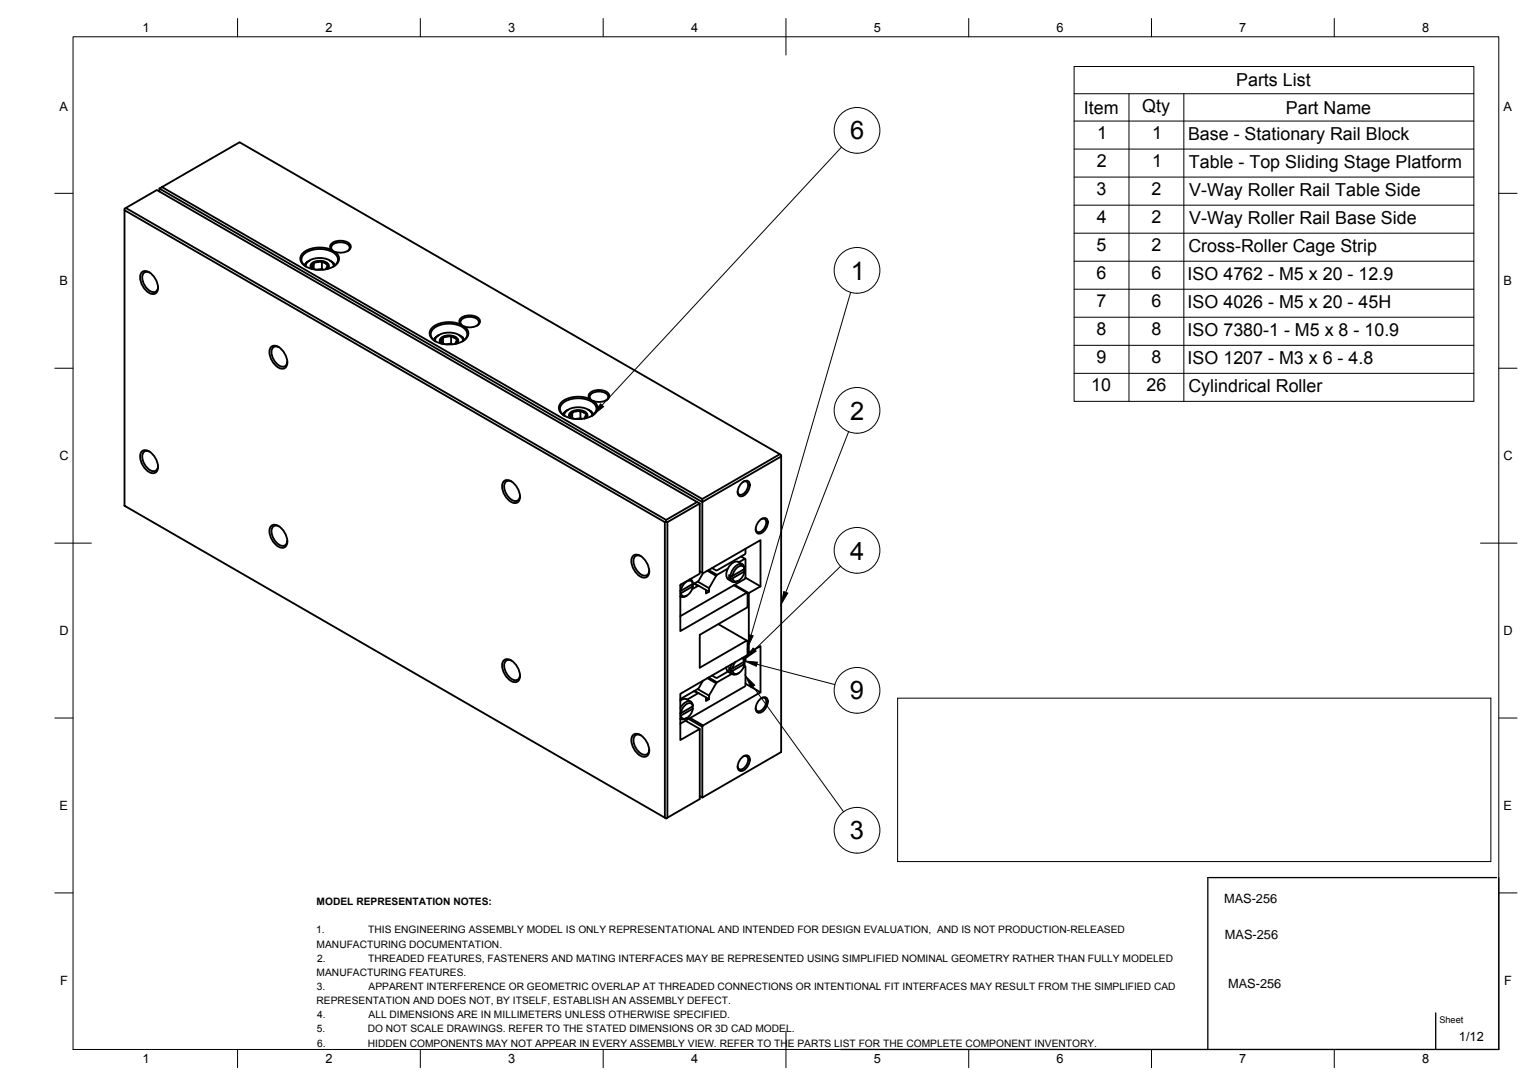
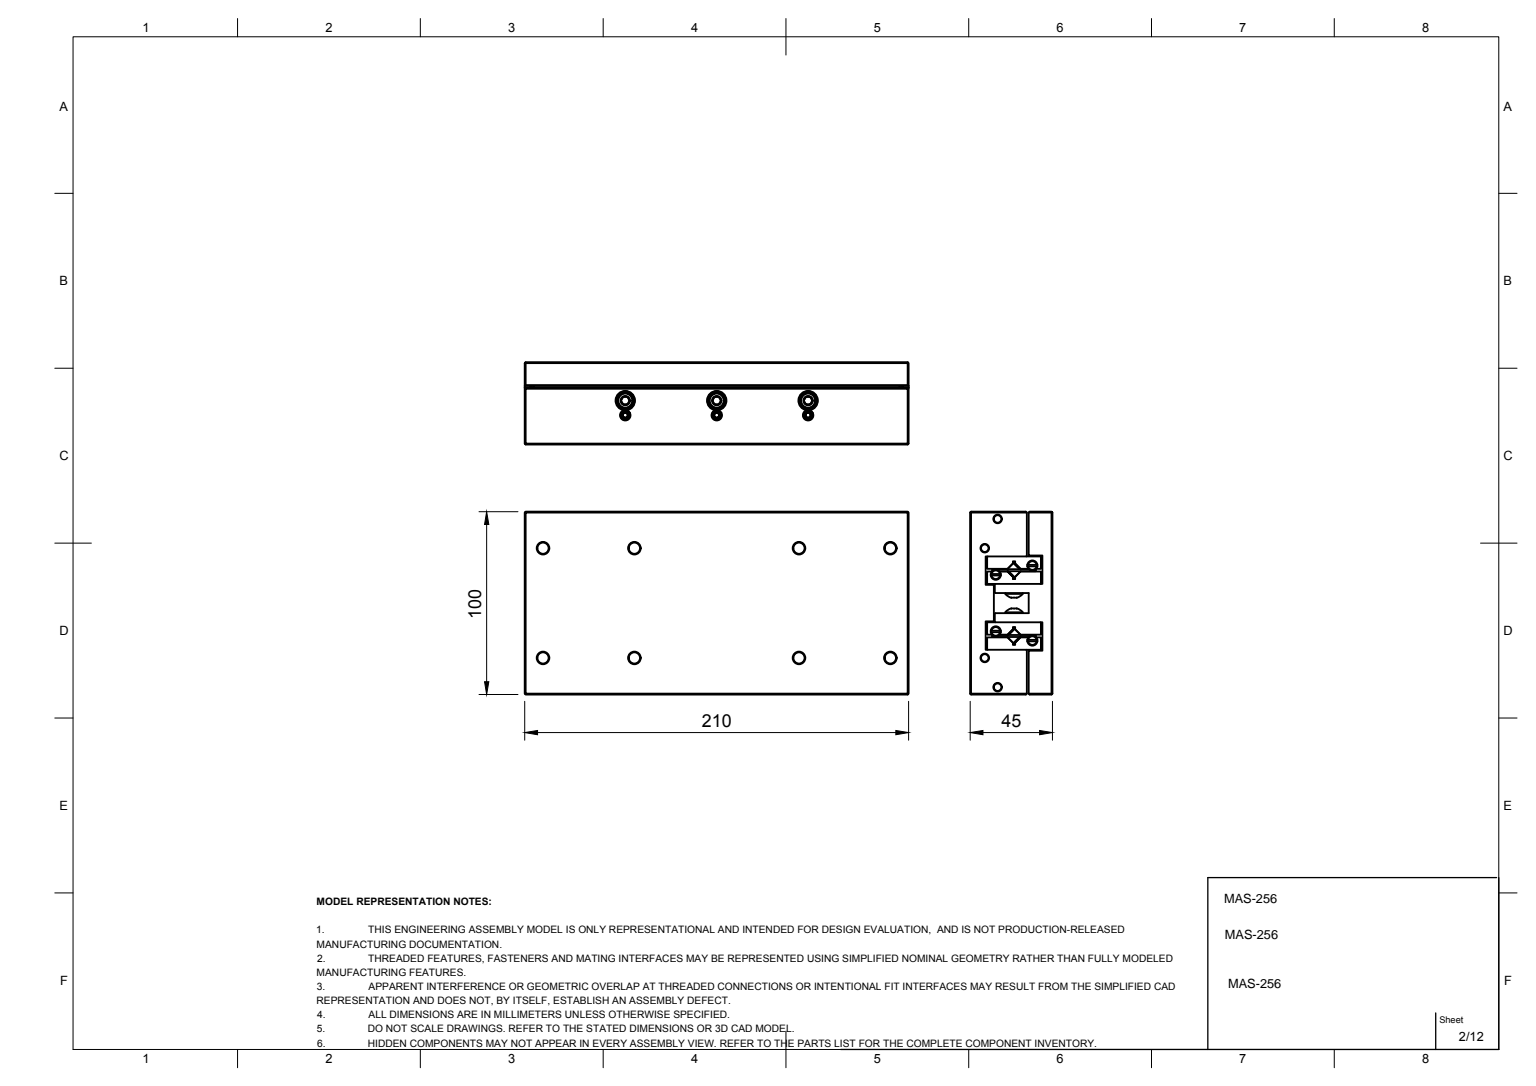
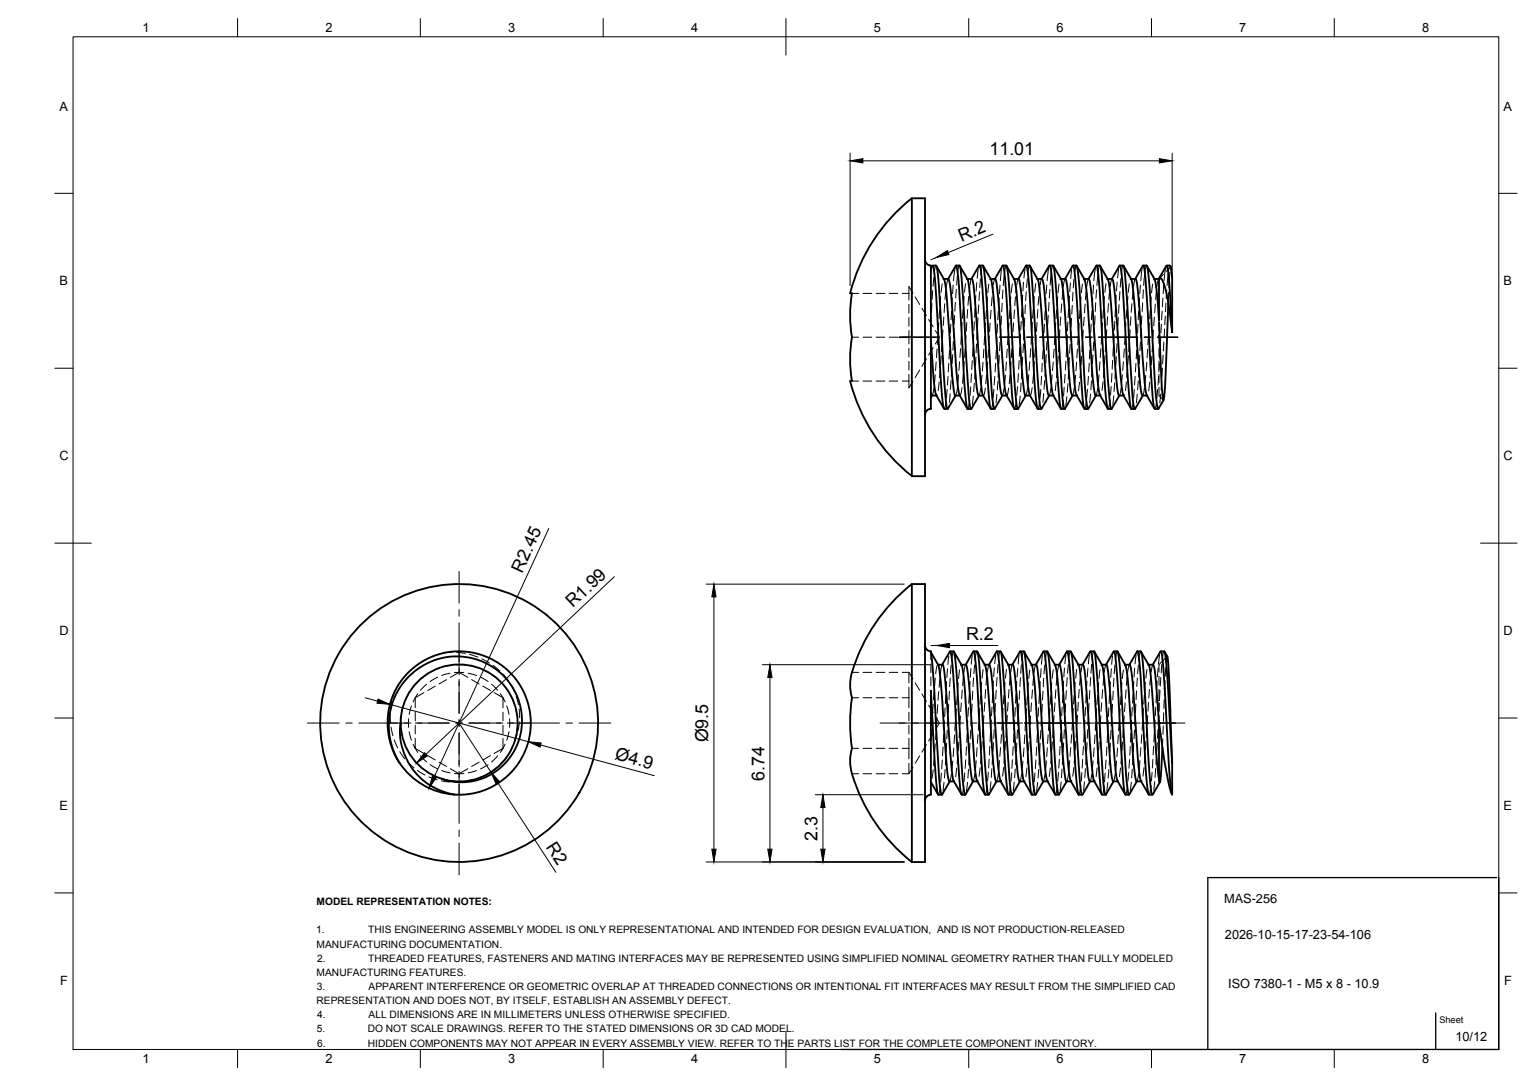
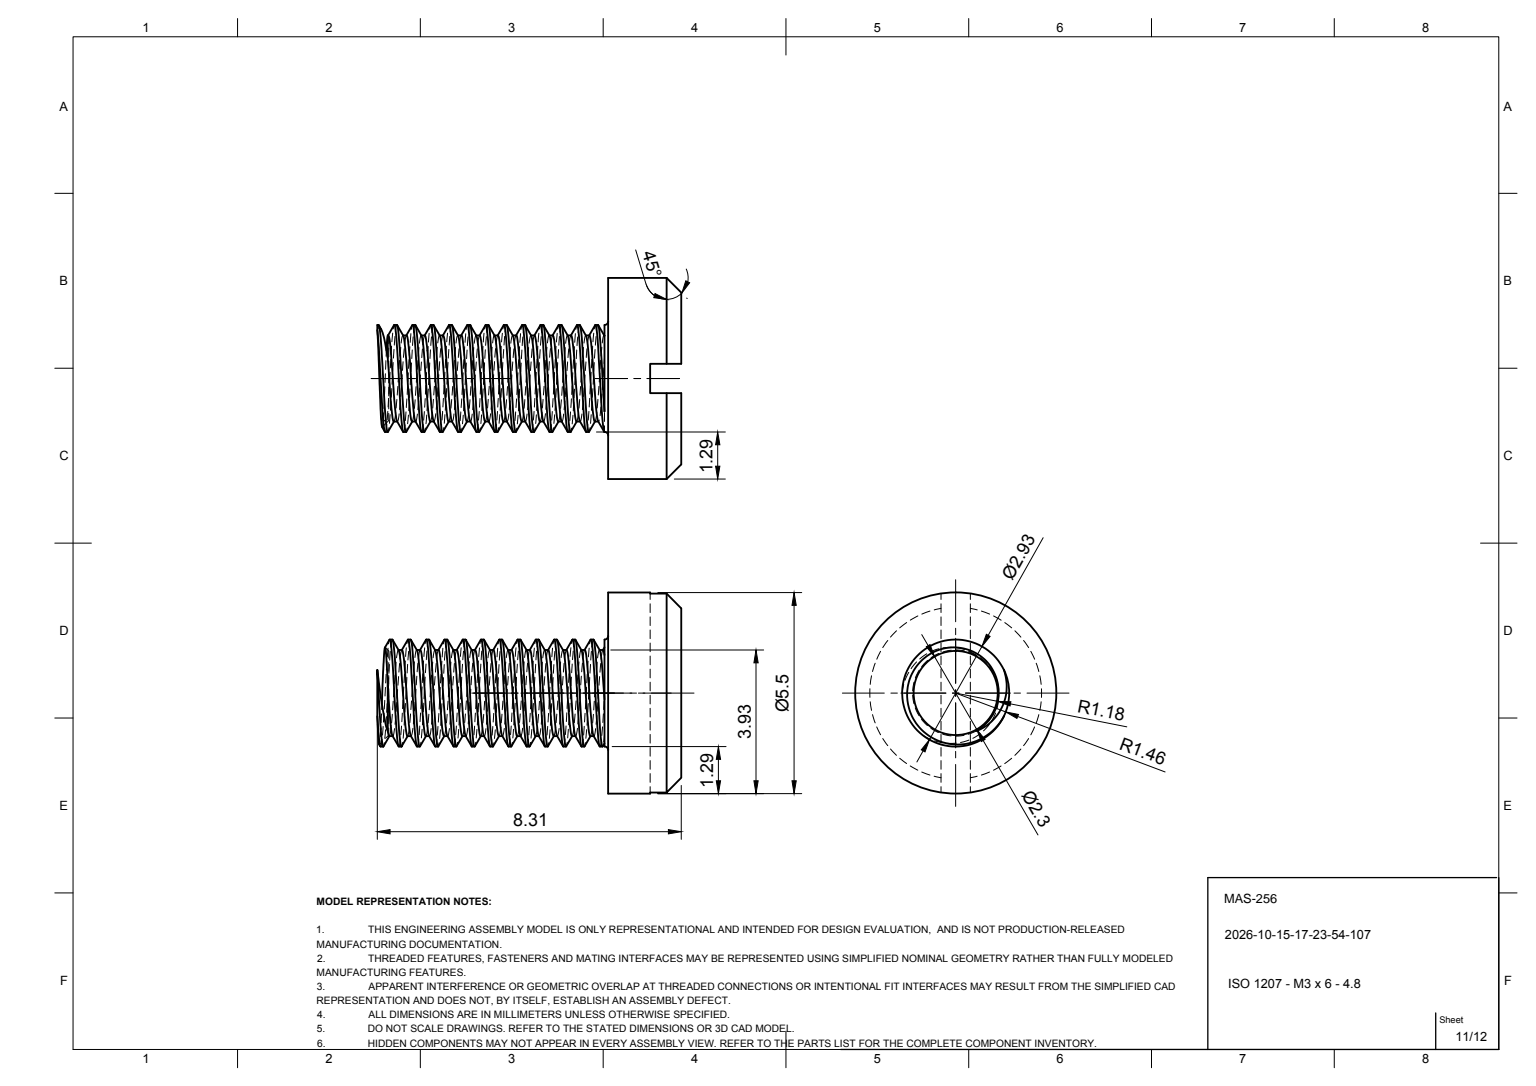
ISO-10303-21;
HEADER;
/* Generated by software containing ST-Developer
 * from STEP Tools, Inc. (www.steptools.com) 
 */

FILE_DESCRIPTION(
/* description */ (''),
/* implementation_level */ '2;1');

FILE_NAME(
/* name */ 'MAS-256',
/* time_stamp */ '2026-10-14T18:40:07-07:00',
/* author */ (''),
/* organization */ (''),
/* preprocessor_version */ 'ST-DEVELOPER v20.2',
/* originating_system */ 'Autodesk Translation Framework v15.15.0.0',
/* authorisation */ '');

FILE_SCHEMA (('AUTOMOTIVE_DESIGN { 1 0 10303 214 3 1 1 }'));
ENDSEC;

DATA;
#10=MECHANICAL_DESIGN_GEOMETRIC_PRESENTATION_REPRESENTATION('',(#831,#832,
#833,#834,#835,#836,#837,#838,#839,#840),#81040);
#11=ITEM_DEFINED_TRANSFORMATION($,$,#15206,#16558);
#12=ITEM_DEFINED_TRANSFORMATION($,$,#15327,#16559);
#13=ITEM_DEFINED_TRANSFORMATION($,$,#15614,#16560);
#14=ITEM_DEFINED_TRANSFORMATION($,$,#15705,#16561);
#15=ITEM_DEFINED_TRANSFORMATION($,$,#15816,#16562);
#16=ITEM_DEFINED_TRANSFORMATION($,$,#16085,#16563);
#17=ITEM_DEFINED_TRANSFORMATION($,$,#16363,#16564);
#18=ITEM_DEFINED_TRANSFORMATION($,$,#16450,#16565);
#19=ITEM_DEFINED_TRANSFORMATION($,$,#16512,#16566);
#20=ITEM_DEFINED_TRANSFORMATION($,$,#16075,#16567);
#21=ITEM_DEFINED_TRANSFORMATION($,$,#15614,#16568);
#22=ITEM_DEFINED_TRANSFORMATION($,$,#15705,#16569);
#23=ITEM_DEFINED_TRANSFORMATION($,$,#15816,#16570);
#24=ITEM_DEFINED_TRANSFORMATION($,$,#16075,#16571);
#25=ITEM_DEFINED_TRANSFORMATION($,$,#16075,#16572);
#26=ITEM_DEFINED_TRANSFORMATION($,$,#16075,#16573);
#27=ITEM_DEFINED_TRANSFORMATION($,$,#16075,#16574);
#28=ITEM_DEFINED_TRANSFORMATION($,$,#16075,#16575);
#29=ITEM_DEFINED_TRANSFORMATION($,$,#16075,#16576);
#30=ITEM_DEFINED_TRANSFORMATION($,$,#16075,#16577);
#31=ITEM_DEFINED_TRANSFORMATION($,$,#16075,#16578);
#32=ITEM_DEFINED_TRANSFORMATION($,$,#16075,#16579);
#33=ITEM_DEFINED_TRANSFORMATION($,$,#16075,#16580);
#34=ITEM_DEFINED_TRANSFORMATION($,$,#16075,#16581);
#35=ITEM_DEFINED_TRANSFORMATION($,$,#16075,#16582);
#36=ITEM_DEFINED_TRANSFORMATION($,$,#16075,#16583);
#37=ITEM_DEFINED_TRANSFORMATION($,$,#16075,#16584);
#38=ITEM_DEFINED_TRANSFORMATION($,$,#16075,#16585);
#39=ITEM_DEFINED_TRANSFORMATION($,$,#16075,#16586);
#40=ITEM_DEFINED_TRANSFORMATION($,$,#16075,#16587);
#41=ITEM_DEFINED_TRANSFORMATION($,$,#16075,#16588);
#42=ITEM_DEFINED_TRANSFORMATION($,$,#16075,#16589);
#43=ITEM_DEFINED_TRANSFORMATION($,$,#16075,#16590);
#44=ITEM_DEFINED_TRANSFORMATION($,$,#16075,#16591);
#45=ITEM_DEFINED_TRANSFORMATION($,$,#16075,#16592);
#46=ITEM_DEFINED_TRANSFORMATION($,$,#16075,#16593);
#47=ITEM_DEFINED_TRANSFORMATION($,$,#16075,#16594);
#48=ITEM_DEFINED_TRANSFORMATION($,$,#16075,#16595);
#49=ITEM_DEFINED_TRANSFORMATION($,$,#16085,#16596);
#50=ITEM_DEFINED_TRANSFORMATION($,$,#16085,#16597);
#51=ITEM_DEFINED_TRANSFORMATION($,$,#16085,#16598);
#52=ITEM_DEFINED_TRANSFORMATION($,$,#16085,#16599);
#53=ITEM_DEFINED_TRANSFORMATION($,$,#16085,#16600);
#54=ITEM_DEFINED_TRANSFORMATION($,$,#16363,#16601);
#55=ITEM_DEFINED_TRANSFORMATION($,$,#16363,#16602);
#56=ITEM_DEFINED_TRANSFORMATION($,$,#16363,#16603);
#57=ITEM_DEFINED_TRANSFORMATION($,$,#16363,#16604);
#58=ITEM_DEFINED_TRANSFORMATION($,$,#16363,#16605);
#59=ITEM_DEFINED_TRANSFORMATION($,$,#16450,#16606);
#60=ITEM_DEFINED_TRANSFORMATION($,$,#16450,#16607);
#61=ITEM_DEFINED_TRANSFORMATION($,$,#16450,#16608);
#62=ITEM_DEFINED_TRANSFORMATION($,$,#16450,#16609);
#63=ITEM_DEFINED_TRANSFORMATION($,$,#16450,#16610);
#64=ITEM_DEFINED_TRANSFORMATION($,$,#16450,#16611);
#65=ITEM_DEFINED_TRANSFORMATION($,$,#16450,#16612);
#66=ITEM_DEFINED_TRANSFORMATION($,$,#16512,#16613);
#67=ITEM_DEFINED_TRANSFORMATION($,$,#16512,#16614);
#68=ITEM_DEFINED_TRANSFORMATION($,$,#16512,#16615);
#69=ITEM_DEFINED_TRANSFORMATION($,$,#16512,#16616);
#70=ITEM_DEFINED_TRANSFORMATION($,$,#16512,#16617);
#71=ITEM_DEFINED_TRANSFORMATION($,$,#16512,#16618);
#72=ITEM_DEFINED_TRANSFORMATION($,$,#16512,#16619);
#73=(
REPRESENTATION_RELATIONSHIP($,$,#81130,#81129)
REPRESENTATION_RELATIONSHIP_WITH_TRANSFORMATION(#11)
SHAPE_REPRESENTATION_RELATIONSHIP()
);
#74=(
REPRESENTATION_RELATIONSHIP($,$,#81131,#81129)
REPRESENTATION_RELATIONSHIP_WITH_TRANSFORMATION(#12)
SHAPE_REPRESENTATION_RELATIONSHIP()
);
#75=(
REPRESENTATION_RELATIONSHIP($,$,#81132,#81129)
REPRESENTATION_RELATIONSHIP_WITH_TRANSFORMATION(#13)
SHAPE_REPRESENTATION_RELATIONSHIP()
);
#76=(
REPRESENTATION_RELATIONSHIP($,$,#81133,#81129)
REPRESENTATION_RELATIONSHIP_WITH_TRANSFORMATION(#14)
SHAPE_REPRESENTATION_RELATIONSHIP()
);
#77=(
REPRESENTATION_RELATIONSHIP($,$,#81134,#81129)
REPRESENTATION_RELATIONSHIP_WITH_TRANSFORMATION(#15)
SHAPE_REPRESENTATION_RELATIONSHIP()
);
#78=(
REPRESENTATION_RELATIONSHIP($,$,#81136,#81129)
REPRESENTATION_RELATIONSHIP_WITH_TRANSFORMATION(#16)
SHAPE_REPRESENTATION_RELATIONSHIP()
);
#79=(
REPRESENTATION_RELATIONSHIP($,$,#81137,#81129)
REPRESENTATION_RELATIONSHIP_WITH_TRANSFORMATION(#17)
SHAPE_REPRESENTATION_RELATIONSHIP()
);
#80=(
REPRESENTATION_RELATIONSHIP($,$,#81138,#81129)
REPRESENTATION_RELATIONSHIP_WITH_TRANSFORMATION(#18)
SHAPE_REPRESENTATION_RELATIONSHIP()
);
#81=(
REPRESENTATION_RELATIONSHIP($,$,#81139,#81129)
REPRESENTATION_RELATIONSHIP_WITH_TRANSFORMATION(#19)
SHAPE_REPRESENTATION_RELATIONSHIP()
);
#82=(
REPRESENTATION_RELATIONSHIP($,$,#81135,#81129)
REPRESENTATION_RELATIONSHIP_WITH_TRANSFORMATION(#20)
SHAPE_REPRESENTATION_RELATIONSHIP()
);
#83=(
REPRESENTATION_RELATIONSHIP($,$,#81132,#81129)
REPRESENTATION_RELATIONSHIP_WITH_TRANSFORMATION(#21)
SHAPE_REPRESENTATION_RELATIONSHIP()
);
#84=(
REPRESENTATION_RELATIONSHIP($,$,#81133,#81129)
REPRESENTATION_RELATIONSHIP_WITH_TRANSFORMATION(#22)
SHAPE_REPRESENTATION_RELATIONSHIP()
);
#85=(
REPRESENTATION_RELATIONSHIP($,$,#81134,#81129)
REPRESENTATION_RELATIONSHIP_WITH_TRANSFORMATION(#23)
SHAPE_REPRESENTATION_RELATIONSHIP()
);
#86=(
REPRESENTATION_RELATIONSHIP($,$,#81135,#81129)
REPRESENTATION_RELATIONSHIP_WITH_TRANSFORMATION(#24)
SHAPE_REPRESENTATION_RELATIONSHIP()
);
#87=(
REPRESENTATION_RELATIONSHIP($,$,#81135,#81129)
REPRESENTATION_RELATIONSHIP_WITH_TRANSFORMATION(#25)
SHAPE_REPRESENTATION_RELATIONSHIP()
);
#88=(
REPRESENTATION_RELATIONSHIP($,$,#81135,#81129)
REPRESENTATION_RELATIONSHIP_WITH_TRANSFORMATION(#26)
SHAPE_REPRESENTATION_RELATIONSHIP()
);
#89=(
REPRESENTATION_RELATIONSHIP($,$,#81135,#81129)
REPRESENTATION_RELATIONSHIP_WITH_TRANSFORMATION(#27)
SHAPE_REPRESENTATION_RELATIONSHIP()
);
#90=(
REPRESENTATION_RELATIONSHIP($,$,#81135,#81129)
REPRESENTATION_RELATIONSHIP_WITH_TRANSFORMATION(#28)
SHAPE_REPRESENTATION_RELATIONSHIP()
);
#91=(
REPRESENTATION_RELATIONSHIP($,$,#81135,#81129)
REPRESENTATION_RELATIONSHIP_WITH_TRANSFORMATION(#29)
SHAPE_REPRESENTATION_RELATIONSHIP()
);
#92=(
REPRESENTATION_RELATIONSHIP($,$,#81135,#81129)
REPRESENTATION_RELATIONSHIP_WITH_TRANSFORMATION(#30)
SHAPE_REPRESENTATION_RELATIONSHIP()
);
#93=(
REPRESENTATION_RELATIONSHIP($,$,#81135,#81129)
REPRESENTATION_RELATIONSHIP_WITH_TRANSFORMATION(#31)
SHAPE_REPRESENTATION_RELATIONSHIP()
);
#94=(
REPRESENTATION_RELATIONSHIP($,$,#81135,#81129)
REPRESENTATION_RELATIONSHIP_WITH_TRANSFORMATION(#32)
SHAPE_REPRESENTATION_RELATIONSHIP()
);
#95=(
REPRESENTATION_RELATIONSHIP($,$,#81135,#81129)
REPRESENTATION_RELATIONSHIP_WITH_TRANSFORMATION(#33)
SHAPE_REPRESENTATION_RELATIONSHIP()
);
#96=(
REPRESENTATION_RELATIONSHIP($,$,#81135,#81129)
REPRESENTATION_RELATIONSHIP_WITH_TRANSFORMATION(#34)
SHAPE_REPRESENTATION_RELATIONSHIP()
);
#97=(
REPRESENTATION_RELATIONSHIP($,$,#81135,#81129)
REPRESENTATION_RELATIONSHIP_WITH_TRANSFORMATION(#35)
SHAPE_REPRESENTATION_RELATIONSHIP()
);
#98=(
REPRESENTATION_RELATIONSHIP($,$,#81135,#81129)
REPRESENTATION_RELATIONSHIP_WITH_TRANSFORMATION(#36)
SHAPE_REPRESENTATION_RELATIONSHIP()
);
#99=(
REPRESENTATION_RELATIONSHIP($,$,#81135,#81129)
REPRESENTATION_RELATIONSHIP_WITH_TRANSFORMATION(#37)
SHAPE_REPRESENTATION_RELATIONSHIP()
);
#100=(
REPRESENTATION_RELATIONSHIP($,$,#81135,#81129)
REPRESENTATION_RELATIONSHIP_WITH_TRANSFORMATION(#38)
SHAPE_REPRESENTATION_RELATIONSHIP()
);
#101=(
REPRESENTATION_RELATIONSHIP($,$,#81135,#81129)
REPRESENTATION_RELATIONSHIP_WITH_TRANSFORMATION(#39)
SHAPE_REPRESENTATION_RELATIONSHIP()
);
#102=(
REPRESENTATION_RELATIONSHIP($,$,#81135,#81129)
REPRESENTATION_RELATIONSHIP_WITH_TRANSFORMATION(#40)
SHAPE_REPRESENTATION_RELATIONSHIP()
);
#103=(
REPRESENTATION_RELATIONSHIP($,$,#81135,#81129)
REPRESENTATION_RELATIONSHIP_WITH_TRANSFORMATION(#41)
SHAPE_REPRESENTATION_RELATIONSHIP()
);
#104=(
REPRESENTATION_RELATIONSHIP($,$,#81135,#81129)
REPRESENTATION_RELATIONSHIP_WITH_TRANSFORMATION(#42)
SHAPE_REPRESENTATION_RELATIONSHIP()
);
#105=(
REPRESENTATION_RELATIONSHIP($,$,#81135,#81129)
REPRESENTATION_RELATIONSHIP_WITH_TRANSFORMATION(#43)
SHAPE_REPRESENTATION_RELATIONSHIP()
);
#106=(
REPRESENTATION_RELATIONSHIP($,$,#81135,#81129)
REPRESENTATION_RELATIONSHIP_WITH_TRANSFORMATION(#44)
SHAPE_REPRESENTATION_RELATIONSHIP()
);
#107=(
REPRESENTATION_RELATIONSHIP($,$,#81135,#81129)
REPRESENTATION_RELATIONSHIP_WITH_TRANSFORMATION(#45)
SHAPE_REPRESENTATION_RELATIONSHIP()
);
#108=(
REPRESENTATION_RELATIONSHIP($,$,#81135,#81129)
REPRESENTATION_RELATIONSHIP_WITH_TRANSFORMATION(#46)
SHAPE_REPRESENTATION_RELATIONSHIP()
);
#109=(
REPRESENTATION_RELATIONSHIP($,$,#81135,#81129)
REPRESENTATION_RELATIONSHIP_WITH_TRANSFORMATION(#47)
SHAPE_REPRESENTATION_RELATIONSHIP()
);
#110=(
REPRESENTATION_RELATIONSHIP($,$,#81135,#81129)
REPRESENTATION_RELATIONSHIP_WITH_TRANSFORMATION(#48)
SHAPE_REPRESENTATION_RELATIONSHIP()
);
#111=(
REPRESENTATION_RELATIONSHIP($,$,#81136,#81129)
REPRESENTATION_RELATIONSHIP_WITH_TRANSFORMATION(#49)
SHAPE_REPRESENTATION_RELATIONSHIP()
);
#112=(
REPRESENTATION_RELATIONSHIP($,$,#81136,#81129)
REPRESENTATION_RELATIONSHIP_WITH_TRANSFORMATION(#50)
SHAPE_REPRESENTATION_RELATIONSHIP()
);
#113=(
REPRESENTATION_RELATIONSHIP($,$,#81136,#81129)
REPRESENTATION_RELATIONSHIP_WITH_TRANSFORMATION(#51)
SHAPE_REPRESENTATION_RELATIONSHIP()
);
#114=(
REPRESENTATION_RELATIONSHIP($,$,#81136,#81129)
REPRESENTATION_RELATIONSHIP_WITH_TRANSFORMATION(#52)
SHAPE_REPRESENTATION_RELATIONSHIP()
);
#115=(
REPRESENTATION_RELATIONSHIP($,$,#81136,#81129)
REPRESENTATION_RELATIONSHIP_WITH_TRANSFORMATION(#53)
SHAPE_REPRESENTATION_RELATIONSHIP()
);
#116=(
REPRESENTATION_RELATIONSHIP($,$,#81137,#81129)
REPRESENTATION_RELATIONSHIP_WITH_TRANSFORMATION(#54)
SHAPE_REPRESENTATION_RELATIONSHIP()
);
#117=(
REPRESENTATION_RELATIONSHIP($,$,#81137,#81129)
REPRESENTATION_RELATIONSHIP_WITH_TRANSFORMATION(#55)
SHAPE_REPRESENTATION_RELATIONSHIP()
);
#118=(
REPRESENTATION_RELATIONSHIP($,$,#81137,#81129)
REPRESENTATION_RELATIONSHIP_WITH_TRANSFORMATION(#56)
SHAPE_REPRESENTATION_RELATIONSHIP()
);
#119=(
REPRESENTATION_RELATIONSHIP($,$,#81137,#81129)
REPRESENTATION_RELATIONSHIP_WITH_TRANSFORMATION(#57)
SHAPE_REPRESENTATION_RELATIONSHIP()
);
#120=(
REPRESENTATION_RELATIONSHIP($,$,#81137,#81129)
REPRESENTATION_RELATIONSHIP_WITH_TRANSFORMATION(#58)
SHAPE_REPRESENTATION_RELATIONSHIP()
);
#121=(
REPRESENTATION_RELATIONSHIP($,$,#81138,#81129)
REPRESENTATION_RELATIONSHIP_WITH_TRANSFORMATION(#59)
SHAPE_REPRESENTATION_RELATIONSHIP()
);
#122=(
REPRESENTATION_RELATIONSHIP($,$,#81138,#81129)
REPRESENTATION_RELATIONSHIP_WITH_TRANSFORMATION(#60)
SHAPE_REPRESENTATION_RELATIONSHIP()
);
#123=(
REPRESENTATION_RELATIONSHIP($,$,#81138,#81129)
REPRESENTATION_RELATIONSHIP_WITH_TRANSFORMATION(#61)
SHAPE_REPRESENTATION_RELATIONSHIP()
);
#124=(
REPRESENTATION_RELATIONSHIP($,$,#81138,#81129)
REPRESENTATION_RELATIONSHIP_WITH_TRANSFORMATION(#62)
SHAPE_REPRESENTATION_RELATIONSHIP()
);
#125=(
REPRESENTATION_RELATIONSHIP($,$,#81138,#81129)
REPRESENTATION_RELATIONSHIP_WITH_TRANSFORMATION(#63)
SHAPE_REPRESENTATION_RELATIONSHIP()
);
#126=(
REPRESENTATION_RELATIONSHIP($,$,#81138,#81129)
REPRESENTATION_RELATIONSHIP_WITH_TRANSFORMATION(#64)
SHAPE_REPRESENTATION_RELATIONSHIP()
);
#127=(
REPRESENTATION_RELATIONSHIP($,$,#81138,#81129)
REPRESENTATION_RELATIONSHIP_WITH_TRANSFORMATION(#65)
SHAPE_REPRESENTATION_RELATIONSHIP()
);
#128=(
REPRESENTATION_RELATIONSHIP($,$,#81139,#81129)
REPRESENTATION_RELATIONSHIP_WITH_TRANSFORMATION(#66)
SHAPE_REPRESENTATION_RELATIONSHIP()
);
#129=(
REPRESENTATION_RELATIONSHIP($,$,#81139,#81129)
REPRESENTATION_RELATIONSHIP_WITH_TRANSFORMATION(#67)
SHAPE_REPRESENTATION_RELATIONSHIP()
);
#130=(
REPRESENTATION_RELATIONSHIP($,$,#81139,#81129)
REPRESENTATION_RELATIONSHIP_WITH_TRANSFORMATION(#68)
SHAPE_REPRESENTATION_RELATIONSHIP()
);
#131=(
REPRESENTATION_RELATIONSHIP($,$,#81139,#81129)
REPRESENTATION_RELATIONSHIP_WITH_TRANSFORMATION(#69)
SHAPE_REPRESENTATION_RELATIONSHIP()
);
#132=(
REPRESENTATION_RELATIONSHIP($,$,#81139,#81129)
REPRESENTATION_RELATIONSHIP_WITH_TRANSFORMATION(#70)
SHAPE_REPRESENTATION_RELATIONSHIP()
);
#133=(
REPRESENTATION_RELATIONSHIP($,$,#81139,#81129)
REPRESENTATION_RELATIONSHIP_WITH_TRANSFORMATION(#71)
SHAPE_REPRESENTATION_RELATIONSHIP()
);
#134=(
REPRESENTATION_RELATIONSHIP($,$,#81139,#81129)
REPRESENTATION_RELATIONSHIP_WITH_TRANSFORMATION(#72)
SHAPE_REPRESENTATION_RELATIONSHIP()
);
#135=CONTEXT_DEPENDENT_SHAPE_REPRESENTATION(#73,#81067);
#136=CONTEXT_DEPENDENT_SHAPE_REPRESENTATION(#74,#81068);
#137=CONTEXT_DEPENDENT_SHAPE_REPRESENTATION(#75,#81069);
#138=CONTEXT_DEPENDENT_SHAPE_REPRESENTATION(#76,#81070);
#139=CONTEXT_DEPENDENT_SHAPE_REPRESENTATION(#77,#81071);
#140=CONTEXT_DEPENDENT_SHAPE_REPRESENTATION(#78,#81072);
#141=CONTEXT_DEPENDENT_SHAPE_REPRESENTATION(#79,#81073);
#142=CONTEXT_DEPENDENT_SHAPE_REPRESENTATION(#80,#81074);
#143=CONTEXT_DEPENDENT_SHAPE_REPRESENTATION(#81,#81075);
#144=CONTEXT_DEPENDENT_SHAPE_REPRESENTATION(#82,#81076);
#145=CONTEXT_DEPENDENT_SHAPE_REPRESENTATION(#83,#81077);
#146=CONTEXT_DEPENDENT_SHAPE_REPRESENTATION(#84,#81078);
#147=CONTEXT_DEPENDENT_SHAPE_REPRESENTATION(#85,#81079);
#148=CONTEXT_DEPENDENT_SHAPE_REPRESENTATION(#86,#81080);
#149=CONTEXT_DEPENDENT_SHAPE_REPRESENTATION(#87,#81081);
#150=CONTEXT_DEPENDENT_SHAPE_REPRESENTATION(#88,#81082);
#151=CONTEXT_DEPENDENT_SHAPE_REPRESENTATION(#89,#81083);
#152=CONTEXT_DEPENDENT_SHAPE_REPRESENTATION(#90,#81084);
#153=CONTEXT_DEPENDENT_SHAPE_REPRESENTATION(#91,#81085);
#154=CONTEXT_DEPENDENT_SHAPE_REPRESENTATION(#92,#81086);
#155=CONTEXT_DEPENDENT_SHAPE_REPRESENTATION(#93,#81087);
#156=CONTEXT_DEPENDENT_SHAPE_REPRESENTATION(#94,#81088);
#157=CONTEXT_DEPENDENT_SHAPE_REPRESENTATION(#95,#81089);
#158=CONTEXT_DEPENDENT_SHAPE_REPRESENTATION(#96,#81090);
#159=CONTEXT_DEPENDENT_SHAPE_REPRESENTATION(#97,#81091);
#160=CONTEXT_DEPENDENT_SHAPE_REPRESENTATION(#98,#81092);
#161=CONTEXT_DEPENDENT_SHAPE_REPRESENTATION(#99,#81093);
#162=CONTEXT_DEPENDENT_SHAPE_REPRESENTATION(#100,#81094);
#163=CONTEXT_DEPENDENT_SHAPE_REPRESENTATION(#101,#81095);
#164=CONTEXT_DEPENDENT_SHAPE_REPRESENTATION(#102,#81096);
#165=CONTEXT_DEPENDENT_SHAPE_REPRESENTATION(#103,#81097);
#166=CONTEXT_DEPENDENT_SHAPE_REPRESENTATION(#104,#81098);
#167=CONTEXT_DEPENDENT_SHAPE_REPRESENTATION(#105,#81099);
#168=CONTEXT_DEPENDENT_SHAPE_REPRESENTATION(#106,#81100);
#169=CONTEXT_DEPENDENT_SHAPE_REPRESENTATION(#107,#81101);
#170=CONTEXT_DEPENDENT_SHAPE_REPRESENTATION(#108,#81102);
#171=CONTEXT_DEPENDENT_SHAPE_REPRESENTATION(#109,#81103);
#172=CONTEXT_DEPENDENT_SHAPE_REPRESENTATION(#110,#81104);
#173=CONTEXT_DEPENDENT_SHAPE_REPRESENTATION(#111,#81105);
#174=CONTEXT_DEPENDENT_SHAPE_REPRESENTATION(#112,#81106);
#175=CONTEXT_DEPENDENT_SHAPE_REPRESENTATION(#113,#81107);
#176=CONTEXT_DEPENDENT_SHAPE_REPRESENTATION(#114,#81108);
#177=CONTEXT_DEPENDENT_SHAPE_REPRESENTATION(#115,#81109);
#178=CONTEXT_DEPENDENT_SHAPE_REPRESENTATION(#116,#81110);
#179=CONTEXT_DEPENDENT_SHAPE_REPRESENTATION(#117,#81111);
#180=CONTEXT_DEPENDENT_SHAPE_REPRESENTATION(#118,#81112);
#181=CONTEXT_DEPENDENT_SHAPE_REPRESENTATION(#119,#81113);
#182=CONTEXT_DEPENDENT_SHAPE_REPRESENTATION(#120,#81114);
#183=CONTEXT_DEPENDENT_SHAPE_REPRESENTATION(#121,#81115);
#184=CONTEXT_DEPENDENT_SHAPE_REPRESENTATION(#122,#81116);
#185=CONTEXT_DEPENDENT_SHAPE_REPRESENTATION(#123,#81117);
#186=CONTEXT_DEPENDENT_SHAPE_REPRESENTATION(#124,#81118);
#187=CONTEXT_DEPENDENT_SHAPE_REPRESENTATION(#125,#81119);
#188=CONTEXT_DEPENDENT_SHAPE_REPRESENTATION(#126,#81120);
#189=CONTEXT_DEPENDENT_SHAPE_REPRESENTATION(#127,#81121);
#190=CONTEXT_DEPENDENT_SHAPE_REPRESENTATION(#128,#81122);
#191=CONTEXT_DEPENDENT_SHAPE_REPRESENTATION(#129,#81123);
#192=CONTEXT_DEPENDENT_SHAPE_REPRESENTATION(#130,#81124);
#193=CONTEXT_DEPENDENT_SHAPE_REPRESENTATION(#131,#81125);
#194=CONTEXT_DEPENDENT_SHAPE_REPRESENTATION(#132,#81126);
#195=CONTEXT_DEPENDENT_SHAPE_REPRESENTATION(#133,#81127);
#196=CONTEXT_DEPENDENT_SHAPE_REPRESENTATION(#134,#81128);
#197=NEXT_ASSEMBLY_USAGE_OCCURRENCE('Base - Stationary Rail Block:1',
'Base - Stationary Rail Block:1','Base - Stationary Rail Block:1',#81141,
#81142,'Base - Stationary Rail Block:1');
#198=NEXT_ASSEMBLY_USAGE_OCCURRENCE(
'Table - Top Sliding Stage Platform:1',
'Table - Top Sliding Stage Platform:1',
'Table - Top Sliding Stage Platform:1',#81141,#81143,
'Table - Top Sliding Stage Platform:1');
#199=NEXT_ASSEMBLY_USAGE_OCCURRENCE('V-Way Roller Rail Table Side:1',
'V-Way Roller Rail Table Side:1','V-Way Roller Rail Table Side:1',#81141,
#81144,'V-Way Roller Rail Table Side:1');
#200=NEXT_ASSEMBLY_USAGE_OCCURRENCE('V-Way Roller Rail Base Side:1',
'V-Way Roller Rail Base Side:1','V-Way Roller Rail Base Side:1',#81141,
#81145,'V-Way Roller Rail Base Side:1');
#201=NEXT_ASSEMBLY_USAGE_OCCURRENCE('Cross-Roller Cage Strip:1',
'Cross-Roller Cage Strip:1','Cross-Roller Cage Strip:1',#81141,#81146,
'Cross-Roller Cage Strip:1');
#202=NEXT_ASSEMBLY_USAGE_OCCURRENCE('ISO 4762 - M5 x 20 - 12.9:1',
'ISO 4762 - M5 x 20 - 12.9:1','ISO 4762 - M5 x 20 - 12.9:1',#81141,#81148,
'ISO 4762 - M5 x 20 - 12.9:1');
#203=NEXT_ASSEMBLY_USAGE_OCCURRENCE('ISO 4026 - M5 x 20 - 45H:1',
'ISO 4026 - M5 x 20 - 45H:1','ISO 4026 - M5 x 20 - 45H:1',#81141,#81149,
'ISO 4026 - M5 x 20 - 45H:1');
#204=NEXT_ASSEMBLY_USAGE_OCCURRENCE('ISO 7380-1 - M5 x 8 - 10.9:1',
'ISO 7380-1 - M5 x 8 - 10.9:1','ISO 7380-1 - M5 x 8 - 10.9:1',#81141,#81150,
'ISO 7380-1 - M5 x 8 - 10.9:1');
#205=NEXT_ASSEMBLY_USAGE_OCCURRENCE('ISO 1207 - M3 x 6 - 4.8:1',
'ISO 1207 - M3 x 6 - 4.8:1','ISO 1207 - M3 x 6 - 4.8:1',#81141,#81151,
'ISO 1207 - M3 x 6 - 4.8:1');
#206=NEXT_ASSEMBLY_USAGE_OCCURRENCE('Cylindrical Roller:1',
'Cylindrical Roller:1','Cylindrical Roller:1',#81141,#81147,
'Cylindrical Roller:1');
#207=NEXT_ASSEMBLY_USAGE_OCCURRENCE('V-Way Roller Rail Table Side:2',
'V-Way Roller Rail Table Side:2','V-Way Roller Rail Table Side:2',#81141,
#81144,'V-Way Roller Rail Table Side:2');
#208=NEXT_ASSEMBLY_USAGE_OCCURRENCE('V-Way Roller Rail Base Side:2',
'V-Way Roller Rail Base Side:2','V-Way Roller Rail Base Side:2',#81141,
#81145,'V-Way Roller Rail Base Side:2');
#209=NEXT_ASSEMBLY_USAGE_OCCURRENCE('Cross-Roller Cage Strip:2',
'Cross-Roller Cage Strip:2','Cross-Roller Cage Strip:2',#81141,#81146,
'Cross-Roller Cage Strip:2');
#210=NEXT_ASSEMBLY_USAGE_OCCURRENCE('Cylindrical Roller:2',
'Cylindrical Roller:2','Cylindrical Roller:2',#81141,#81147,
'Cylindrical Roller:2');
#211=NEXT_ASSEMBLY_USAGE_OCCURRENCE('Cylindrical Roller:3',
'Cylindrical Roller:3','Cylindrical Roller:3',#81141,#81147,
'Cylindrical Roller:3');
#212=NEXT_ASSEMBLY_USAGE_OCCURRENCE('Cylindrical Roller:4',
'Cylindrical Roller:4','Cylindrical Roller:4',#81141,#81147,
'Cylindrical Roller:4');
#213=NEXT_ASSEMBLY_USAGE_OCCURRENCE('Cylindrical Roller:5',
'Cylindrical Roller:5','Cylindrical Roller:5',#81141,#81147,
'Cylindrical Roller:5');
#214=NEXT_ASSEMBLY_USAGE_OCCURRENCE('Cylindrical Roller:6',
'Cylindrical Roller:6','Cylindrical Roller:6',#81141,#81147,
'Cylindrical Roller:6');
#215=NEXT_ASSEMBLY_USAGE_OCCURRENCE('Cylindrical Roller:7',
'Cylindrical Roller:7','Cylindrical Roller:7',#81141,#81147,
'Cylindrical Roller:7');
#216=NEXT_ASSEMBLY_USAGE_OCCURRENCE('Cylindrical Roller:8',
'Cylindrical Roller:8','Cylindrical Roller:8',#81141,#81147,
'Cylindrical Roller:8');
#217=NEXT_ASSEMBLY_USAGE_OCCURRENCE('Cylindrical Roller:9',
'Cylindrical Roller:9','Cylindrical Roller:9',#81141,#81147,
'Cylindrical Roller:9');
#218=NEXT_ASSEMBLY_USAGE_OCCURRENCE('Cylindrical Roller:10',
'Cylindrical Roller:10','Cylindrical Roller:10',#81141,#81147,
'Cylindrical Roller:10');
#219=NEXT_ASSEMBLY_USAGE_OCCURRENCE('Cylindrical Roller:11',
'Cylindrical Roller:11','Cylindrical Roller:11',#81141,#81147,
'Cylindrical Roller:11');
#220=NEXT_ASSEMBLY_USAGE_OCCURRENCE('Cylindrical Roller:12',
'Cylindrical Roller:12','Cylindrical Roller:12',#81141,#81147,
'Cylindrical Roller:12');
#221=NEXT_ASSEMBLY_USAGE_OCCURRENCE('Cylindrical Roller:13',
'Cylindrical Roller:13','Cylindrical Roller:13',#81141,#81147,
'Cylindrical Roller:13');
#222=NEXT_ASSEMBLY_USAGE_OCCURRENCE('Cylindrical Roller:14',
'Cylindrical Roller:14','Cylindrical Roller:14',#81141,#81147,
'Cylindrical Roller:14');
#223=NEXT_ASSEMBLY_USAGE_OCCURRENCE('Cylindrical Roller:15',
'Cylindrical Roller:15','Cylindrical Roller:15',#81141,#81147,
'Cylindrical Roller:15');
#224=NEXT_ASSEMBLY_USAGE_OCCURRENCE('Cylindrical Roller:16',
'Cylindrical Roller:16','Cylindrical Roller:16',#81141,#81147,
'Cylindrical Roller:16');
#225=NEXT_ASSEMBLY_USAGE_OCCURRENCE('Cylindrical Roller:17',
'Cylindrical Roller:17','Cylindrical Roller:17',#81141,#81147,
'Cylindrical Roller:17');
#226=NEXT_ASSEMBLY_USAGE_OCCURRENCE('Cylindrical Roller:18',
'Cylindrical Roller:18','Cylindrical Roller:18',#81141,#81147,
'Cylindrical Roller:18');
#227=NEXT_ASSEMBLY_USAGE_OCCURRENCE('Cylindrical Roller:19',
'Cylindrical Roller:19','Cylindrical Roller:19',#81141,#81147,
'Cylindrical Roller:19');
#228=NEXT_ASSEMBLY_USAGE_OCCURRENCE('Cylindrical Roller:20',
'Cylindrical Roller:20','Cylindrical Roller:20',#81141,#81147,
'Cylindrical Roller:20');
#229=NEXT_ASSEMBLY_USAGE_OCCURRENCE('Cylindrical Roller:21',
'Cylindrical Roller:21','Cylindrical Roller:21',#81141,#81147,
'Cylindrical Roller:21');
#230=NEXT_ASSEMBLY_USAGE_OCCURRENCE('Cylindrical Roller:22',
'Cylindrical Roller:22','Cylindrical Roller:22',#81141,#81147,
'Cylindrical Roller:22');
#231=NEXT_ASSEMBLY_USAGE_OCCURRENCE('Cylindrical Roller:23',
'Cylindrical Roller:23','Cylindrical Roller:23',#81141,#81147,
'Cylindrical Roller:23');
#232=NEXT_ASSEMBLY_USAGE_OCCURRENCE('Cylindrical Roller:24',
'Cylindrical Roller:24','Cylindrical Roller:24',#81141,#81147,
'Cylindrical Roller:24');
#233=NEXT_ASSEMBLY_USAGE_OCCURRENCE('Cylindrical Roller:25',
'Cylindrical Roller:25','Cylindrical Roller:25',#81141,#81147,
'Cylindrical Roller:25');
#234=NEXT_ASSEMBLY_USAGE_OCCURRENCE('Cylindrical Roller:26',
'Cylindrical Roller:26','Cylindrical Roller:26',#81141,#81147,
'Cylindrical Roller:26');
#235=NEXT_ASSEMBLY_USAGE_OCCURRENCE('ISO 4762 - M5 x 20 - 12.9:2',
'ISO 4762 - M5 x 20 - 12.9:2','ISO 4762 - M5 x 20 - 12.9:2',#81141,#81148,
'ISO 4762 - M5 x 20 - 12.9:2');
#236=NEXT_ASSEMBLY_USAGE_OCCURRENCE('ISO 4762 - M5 x 20 - 12.9:3',
'ISO 4762 - M5 x 20 - 12.9:3','ISO 4762 - M5 x 20 - 12.9:3',#81141,#81148,
'ISO 4762 - M5 x 20 - 12.9:3');
#237=NEXT_ASSEMBLY_USAGE_OCCURRENCE('ISO 4762 - M5 x 20 - 12.9:4',
'ISO 4762 - M5 x 20 - 12.9:4','ISO 4762 - M5 x 20 - 12.9:4',#81141,#81148,
'ISO 4762 - M5 x 20 - 12.9:4');
#238=NEXT_ASSEMBLY_USAGE_OCCURRENCE('ISO 4762 - M5 x 20 - 12.9:5',
'ISO 4762 - M5 x 20 - 12.9:5','ISO 4762 - M5 x 20 - 12.9:5',#81141,#81148,
'ISO 4762 - M5 x 20 - 12.9:5');
#239=NEXT_ASSEMBLY_USAGE_OCCURRENCE('ISO 4762 - M5 x 20 - 12.9:6',
'ISO 4762 - M5 x 20 - 12.9:6','ISO 4762 - M5 x 20 - 12.9:6',#81141,#81148,
'ISO 4762 - M5 x 20 - 12.9:6');
#240=NEXT_ASSEMBLY_USAGE_OCCURRENCE('ISO 4026 - M5 x 20 - 45H:2',
'ISO 4026 - M5 x 20 - 45H:2','ISO 4026 - M5 x 20 - 45H:2',#81141,#81149,
'ISO 4026 - M5 x 20 - 45H:2');
#241=NEXT_ASSEMBLY_USAGE_OCCURRENCE('ISO 4026 - M5 x 20 - 45H:3',
'ISO 4026 - M5 x 20 - 45H:3','ISO 4026 - M5 x 20 - 45H:3',#81141,#81149,
'ISO 4026 - M5 x 20 - 45H:3');
#242=NEXT_ASSEMBLY_USAGE_OCCURRENCE('ISO 4026 - M5 x 20 - 45H:4',
'ISO 4026 - M5 x 20 - 45H:4','ISO 4026 - M5 x 20 - 45H:4',#81141,#81149,
'ISO 4026 - M5 x 20 - 45H:4');
#243=NEXT_ASSEMBLY_USAGE_OCCURRENCE('ISO 4026 - M5 x 20 - 45H:5',
'ISO 4026 - M5 x 20 - 45H:5','ISO 4026 - M5 x 20 - 45H:5',#81141,#81149,
'ISO 4026 - M5 x 20 - 45H:5');
#244=NEXT_ASSEMBLY_USAGE_OCCURRENCE('ISO 4026 - M5 x 20 - 45H:6',
'ISO 4026 - M5 x 20 - 45H:6','ISO 4026 - M5 x 20 - 45H:6',#81141,#81149,
'ISO 4026 - M5 x 20 - 45H:6');
#245=NEXT_ASSEMBLY_USAGE_OCCURRENCE('ISO 7380-1 - M5 x 8 - 10.9:2',
'ISO 7380-1 - M5 x 8 - 10.9:2','ISO 7380-1 - M5 x 8 - 10.9:2',#81141,#81150,
'ISO 7380-1 - M5 x 8 - 10.9:2');
#246=NEXT_ASSEMBLY_USAGE_OCCURRENCE('ISO 7380-1 - M5 x 8 - 10.9:3',
'ISO 7380-1 - M5 x 8 - 10.9:3','ISO 7380-1 - M5 x 8 - 10.9:3',#81141,#81150,
'ISO 7380-1 - M5 x 8 - 10.9:3');
#247=NEXT_ASSEMBLY_USAGE_OCCURRENCE('ISO 7380-1 - M5 x 8 - 10.9:4',
'ISO 7380-1 - M5 x 8 - 10.9:4','ISO 7380-1 - M5 x 8 - 10.9:4',#81141,#81150,
'ISO 7380-1 - M5 x 8 - 10.9:4');
#248=NEXT_ASSEMBLY_USAGE_OCCURRENCE('ISO 7380-1 - M5 x 8 - 10.9:5',
'ISO 7380-1 - M5 x 8 - 10.9:5','ISO 7380-1 - M5 x 8 - 10.9:5',#81141,#81150,
'ISO 7380-1 - M5 x 8 - 10.9:5');
#249=NEXT_ASSEMBLY_USAGE_OCCURRENCE('ISO 7380-1 - M5 x 8 - 10.9:6',
'ISO 7380-1 - M5 x 8 - 10.9:6','ISO 7380-1 - M5 x 8 - 10.9:6',#81141,#81150,
'ISO 7380-1 - M5 x 8 - 10.9:6');
#250=NEXT_ASSEMBLY_USAGE_OCCURRENCE('ISO 7380-1 - M5 x 8 - 10.9:7',
'ISO 7380-1 - M5 x 8 - 10.9:7','ISO 7380-1 - M5 x 8 - 10.9:7',#81141,#81150,
'ISO 7380-1 - M5 x 8 - 10.9:7');
#251=NEXT_ASSEMBLY_USAGE_OCCURRENCE('ISO 7380-1 - M5 x 8 - 10.9:8',
'ISO 7380-1 - M5 x 8 - 10.9:8','ISO 7380-1 - M5 x 8 - 10.9:8',#81141,#81150,
'ISO 7380-1 - M5 x 8 - 10.9:8');
#252=NEXT_ASSEMBLY_USAGE_OCCURRENCE('ISO 1207 - M3 x 6 - 4.8:2',
'ISO 1207 - M3 x 6 - 4.8:2','ISO 1207 - M3 x 6 - 4.8:2',#81141,#81151,
'ISO 1207 - M3 x 6 - 4.8:2');
#253=NEXT_ASSEMBLY_USAGE_OCCURRENCE('ISO 1207 - M3 x 6 - 4.8:3',
'ISO 1207 - M3 x 6 - 4.8:3','ISO 1207 - M3 x 6 - 4.8:3',#81141,#81151,
'ISO 1207 - M3 x 6 - 4.8:3');
#254=NEXT_ASSEMBLY_USAGE_OCCURRENCE('ISO 1207 - M3 x 6 - 4.8:4',
'ISO 1207 - M3 x 6 - 4.8:4','ISO 1207 - M3 x 6 - 4.8:4',#81141,#81151,
'ISO 1207 - M3 x 6 - 4.8:4');
#255=NEXT_ASSEMBLY_USAGE_OCCURRENCE('ISO 1207 - M3 x 6 - 4.8:5',
'ISO 1207 - M3 x 6 - 4.8:5','ISO 1207 - M3 x 6 - 4.8:5',#81141,#81151,
'ISO 1207 - M3 x 6 - 4.8:5');
#256=NEXT_ASSEMBLY_USAGE_OCCURRENCE('ISO 1207 - M3 x 6 - 4.8:6',
'ISO 1207 - M3 x 6 - 4.8:6','ISO 1207 - M3 x 6 - 4.8:6',#81141,#81151,
'ISO 1207 - M3 x 6 - 4.8:6');
#257=NEXT_ASSEMBLY_USAGE_OCCURRENCE('ISO 1207 - M3 x 6 - 4.8:7',
'ISO 1207 - M3 x 6 - 4.8:7','ISO 1207 - M3 x 6 - 4.8:7',#81141,#81151,
'ISO 1207 - M3 x 6 - 4.8:7');
#258=NEXT_ASSEMBLY_USAGE_OCCURRENCE('ISO 1207 - M3 x 6 - 4.8:8',
'ISO 1207 - M3 x 6 - 4.8:8','ISO 1207 - M3 x 6 - 4.8:8',#81141,#81151,
'ISO 1207 - M3 x 6 - 4.8:8');
#259=SPHERICAL_SURFACE('',#16510,6.05489130434781);
#260=(
BOUNDED_CURVE()
B_SPLINE_CURVE(2,(#42262,#42263,#42264),.UNSPECIFIED.,.F.,.F.)
B_SPLINE_CURVE_WITH_KNOTS((3,3),(0.,0.0216285523885327),.UNSPECIFIED.)
CURVE()
GEOMETRIC_REPRESENTATION_ITEM()
RATIONAL_B_SPLINE_CURVE((1.,1.000549833114,1.00070303138813))
REPRESENTATION_ITEM('')
);
#261=(
BOUNDED_CURVE()
B_SPLINE_CURVE(2,(#42268,#42269,#42270),.UNSPECIFIED.,.F.,.F.)
B_SPLINE_CURVE_WITH_KNOTS((3,3),(0.0383363983196538,0.0599649507081082),
 .UNSPECIFIED.)
CURVE()
GEOMETRIC_REPRESENTATION_ITEM()
RATIONAL_B_SPLINE_CURVE((1.00070303139789,1.00054983312164,1.))
REPRESENTATION_ITEM('')
);
#262=(
BOUNDED_CURVE()
B_SPLINE_CURVE(2,(#42563,#42564,#42565),.UNSPECIFIED.,.F.,.F.)
B_SPLINE_CURVE_WITH_KNOTS((3,3),(0.,0.0216285523885616),.UNSPECIFIED.)
CURVE()
GEOMETRIC_REPRESENTATION_ITEM()
RATIONAL_B_SPLINE_CURVE((1.,1.00054983311705,1.00070303139203))
REPRESENTATION_ITEM('')
);
#263=(
BOUNDED_CURVE()
B_SPLINE_CURVE(2,(#42567,#42568,#42569),.UNSPECIFIED.,.F.,.F.)
B_SPLINE_CURVE_WITH_KNOTS((3,3),(0.0383363983195465,0.0599649507081086),
 .UNSPECIFIED.)
CURVE()
GEOMETRIC_REPRESENTATION_ITEM()
RATIONAL_B_SPLINE_CURVE((1.00070303139079,1.00054983311608,1.))
REPRESENTATION_ITEM('')
);
#264=(
BOUNDED_CURVE()
B_SPLINE_CURVE(2,(#42574,#42575,#42576),.UNSPECIFIED.,.F.,.F.)
B_SPLINE_CURVE_WITH_KNOTS((3,3),(0.0383363983195738,0.0599649507081061),
 .UNSPECIFIED.)
CURVE()
GEOMETRIC_REPRESENTATION_ITEM()
RATIONAL_B_SPLINE_CURVE((1.00070303139411,1.00054983311868,1.))
REPRESENTATION_ITEM('')
);
#265=(
BOUNDED_CURVE()
B_SPLINE_CURVE(2,(#42578,#42579,#42580),.UNSPECIFIED.,.F.,.F.)
B_SPLINE_CURVE_WITH_KNOTS((3,3),(0.,0.0216285523884906),.UNSPECIFIED.)
CURVE()
GEOMETRIC_REPRESENTATION_ITEM()
RATIONAL_B_SPLINE_CURVE((1.,1.00054983311838,1.00070303139373))
REPRESENTATION_ITEM('')
);
#266=(
BOUNDED_CURVE()
B_SPLINE_CURVE(2,(#42581,#42582,#42583),.UNSPECIFIED.,.F.,.F.)
B_SPLINE_CURVE_WITH_KNOTS((3,3),(0.0383363983195406,0.0599649507081063),
 .UNSPECIFIED.)
CURVE()
GEOMETRIC_REPRESENTATION_ITEM()
RATIONAL_B_SPLINE_CURVE((1.00070303138964,1.00054983311518,1.))
REPRESENTATION_ITEM('')
);
#267=(
BOUNDED_CURVE()
B_SPLINE_CURVE(2,(#42585,#42586,#42587),.UNSPECIFIED.,.F.,.F.)
B_SPLINE_CURVE_WITH_KNOTS((3,3),(0.,0.0216285523884772),.UNSPECIFIED.)
CURVE()
GEOMETRIC_REPRESENTATION_ITEM()
RATIONAL_B_SPLINE_CURVE((1.,1.00054983312122,1.00070303139736))
REPRESENTATION_ITEM('')
);
#268=(
BOUNDED_CURVE()
B_SPLINE_CURVE(2,(#42588,#42589,#42590),.UNSPECIFIED.,.F.,.F.)
B_SPLINE_CURVE_WITH_KNOTS((3,3),(0.0383363983195954,0.0599649507081057),
 .UNSPECIFIED.)
CURVE()
GEOMETRIC_REPRESENTATION_ITEM()
RATIONAL_B_SPLINE_CURVE((1.00070303139538,1.00054983311967,1.))
REPRESENTATION_ITEM('')
);
#269=(
BOUNDED_CURVE()
B_SPLINE_CURVE(2,(#42592,#42593,#42594),.UNSPECIFIED.,.F.,.F.)
B_SPLINE_CURVE_WITH_KNOTS((3,3),(0.,0.0216285523885691),.UNSPECIFIED.)
CURVE()
GEOMETRIC_REPRESENTATION_ITEM()
RATIONAL_B_SPLINE_CURVE((1.,1.00054983311357,1.00070303138758))
REPRESENTATION_ITEM('')
);
#270=(
BOUNDED_CURVE()
B_SPLINE_CURVE(2,(#42595,#42596,#42597),.UNSPECIFIED.,.F.,.F.)
B_SPLINE_CURVE_WITH_KNOTS((3,3),(0.0383363983195734,0.0599649507081057),
 .UNSPECIFIED.)
CURVE()
GEOMETRIC_REPRESENTATION_ITEM()
RATIONAL_B_SPLINE_CURVE((1.00070303138924,1.00054983311487,1.))
REPRESENTATION_ITEM('')
);
#271=(
BOUNDED_CURVE()
B_SPLINE_CURVE(2,(#42599,#42600,#42601),.UNSPECIFIED.,.F.,.F.)
B_SPLINE_CURVE_WITH_KNOTS((3,3),(0.,0.021628552388544),.UNSPECIFIED.)
CURVE()
GEOMETRIC_REPRESENTATION_ITEM()
RATIONAL_B_SPLINE_CURVE((1.,1.00054983311579,1.00070303139042))
REPRESENTATION_ITEM('')
);
#272=(
BOUNDED_CURVE()
B_SPLINE_CURVE(2,(#42602,#42603,#42604),.UNSPECIFIED.,.F.,.F.)
B_SPLINE_CURVE_WITH_KNOTS((3,3),(0.0383363983195219,0.0599649507081056),
 .UNSPECIFIED.)
CURVE()
GEOMETRIC_REPRESENTATION_ITEM()
RATIONAL_B_SPLINE_CURVE((1.00070303138672,1.0005498331129,1.))
REPRESENTATION_ITEM('')
);
#273=(
BOUNDED_CURVE()
B_SPLINE_CURVE(2,(#42606,#42607,#42608),.UNSPECIFIED.,.F.,.F.)
B_SPLINE_CURVE_WITH_KNOTS((3,3),(0.,0.0216285523886276),.UNSPECIFIED.)
CURVE()
GEOMETRIC_REPRESENTATION_ITEM()
RATIONAL_B_SPLINE_CURVE((1.,1.00054983311002,1.00070303138303))
REPRESENTATION_ITEM('')
);
#274=(
BOUNDED_CURVE()
B_SPLINE_CURVE(2,(#42609,#42610,#42611),.UNSPECIFIED.,.F.,.F.)
B_SPLINE_CURVE_WITH_KNOTS((3,3),(0.0383363983195948,0.0599649507081057),
 .UNSPECIFIED.)
CURVE()
GEOMETRIC_REPRESENTATION_ITEM()
RATIONAL_B_SPLINE_CURVE((1.00070303139332,1.00054983311806,1.))
REPRESENTATION_ITEM('')
);
#275=(
BOUNDED_CURVE()
B_SPLINE_CURVE(2,(#42613,#42614,#42615),.UNSPECIFIED.,.F.,.F.)
B_SPLINE_CURVE_WITH_KNOTS((3,3),(0.,0.0216285523885387),.UNSPECIFIED.)
CURVE()
GEOMETRIC_REPRESENTATION_ITEM()
RATIONAL_B_SPLINE_CURVE((1.,1.00054983311459,1.00070303138888))
REPRESENTATION_ITEM('')
);
#276=(
BOUNDED_CURVE()
B_SPLINE_CURVE(2,(#42616,#42617,#42618),.UNSPECIFIED.,.F.,.F.)
B_SPLINE_CURVE_WITH_KNOTS((3,3),(0.0383363983195453,0.0599649507081048),
 .UNSPECIFIED.)
CURVE()
GEOMETRIC_REPRESENTATION_ITEM()
RATIONAL_B_SPLINE_CURVE((1.00070303138923,1.00054983311486,1.))
REPRESENTATION_ITEM('')
);
#277=(
BOUNDED_CURVE()
B_SPLINE_CURVE(2,(#42620,#42621,#42622),.UNSPECIFIED.,.F.,.F.)
B_SPLINE_CURVE_WITH_KNOTS((3,3),(0.,0.0216285523885327),.UNSPECIFIED.)
CURVE()
GEOMETRIC_REPRESENTATION_ITEM()
RATIONAL_B_SPLINE_CURVE((1.,1.000549833118,1.00070303139324))
REPRESENTATION_ITEM('')
);
#278=(
BOUNDED_CURVE()
B_SPLINE_CURVE(2,(#42623,#42624,#42625),.UNSPECIFIED.,.F.,.F.)
B_SPLINE_CURVE_WITH_KNOTS((3,3),(0.038336398319501,0.0599649507081059),
 .UNSPECIFIED.)
CURVE()
GEOMETRIC_REPRESENTATION_ITEM()
RATIONAL_B_SPLINE_CURVE((1.00070303138577,1.00054983311216,1.))
REPRESENTATION_ITEM('')
);
#279=(
BOUNDED_CURVE()
B_SPLINE_CURVE(2,(#42627,#42628,#42629),.UNSPECIFIED.,.F.,.F.)
B_SPLINE_CURVE_WITH_KNOTS((3,3),(0.,0.0216285523885216),.UNSPECIFIED.)
CURVE()
GEOMETRIC_REPRESENTATION_ITEM()
RATIONAL_B_SPLINE_CURVE((1.,1.0005498331148,1.00070303138915))
REPRESENTATION_ITEM('')
);
#280=(
BOUNDED_CURVE()
B_SPLINE_CURVE(2,(#42630,#42631,#42632),.UNSPECIFIED.,.F.,.F.)
B_SPLINE_CURVE_WITH_KNOTS((3,3),(0.0383363983195421,0.0599649507081054),
 .UNSPECIFIED.)
CURVE()
GEOMETRIC_REPRESENTATION_ITEM()
RATIONAL_B_SPLINE_CURVE((1.00070303139029,1.00054983311569,1.))
REPRESENTATION_ITEM('')
);
#281=(
BOUNDED_CURVE()
B_SPLINE_CURVE(2,(#42634,#42635,#42636),.UNSPECIFIED.,.F.,.F.)
B_SPLINE_CURVE_WITH_KNOTS((3,3),(0.,0.0216285523885795),.UNSPECIFIED.)
CURVE()
GEOMETRIC_REPRESENTATION_ITEM()
RATIONAL_B_SPLINE_CURVE((1.,1.0005498331127,1.00070303138646))
REPRESENTATION_ITEM('')
);
#282=(
BOUNDED_CURVE()
B_SPLINE_CURVE(2,(#42637,#42638,#42639),.UNSPECIFIED.,.F.,.F.)
B_SPLINE_CURVE_WITH_KNOTS((3,3),(0.0383363983195796,0.0599649507081049),
 .UNSPECIFIED.)
CURVE()
GEOMETRIC_REPRESENTATION_ITEM()
RATIONAL_B_SPLINE_CURVE((1.00070303139298,1.00054983311779,1.))
REPRESENTATION_ITEM('')
);
#283=(
BOUNDED_CURVE()
B_SPLINE_CURVE(2,(#42641,#42642,#42643),.UNSPECIFIED.,.F.,.F.)
B_SPLINE_CURVE_WITH_KNOTS((3,3),(0.,0.0216285523885516),.UNSPECIFIED.)
CURVE()
GEOMETRIC_REPRESENTATION_ITEM()
RATIONAL_B_SPLINE_CURVE((1.,1.00054983311626,1.00070303139102))
REPRESENTATION_ITEM('')
);
#284=(
BOUNDED_CURVE()
B_SPLINE_CURVE(2,(#42644,#42645,#42646),.UNSPECIFIED.,.F.,.F.)
B_SPLINE_CURVE_WITH_KNOTS((3,3),(0.0383363983195596,0.059964950708105),
 .UNSPECIFIED.)
CURVE()
GEOMETRIC_REPRESENTATION_ITEM()
RATIONAL_B_SPLINE_CURVE((1.00070303138868,1.00054983311444,1.))
REPRESENTATION_ITEM('')
);
#285=(
BOUNDED_CURVE()
B_SPLINE_CURVE(2,(#42648,#42649,#42650),.UNSPECIFIED.,.F.,.F.)
B_SPLINE_CURVE_WITH_KNOTS((3,3),(0.,0.0216285523885783),.UNSPECIFIED.)
CURVE()
GEOMETRIC_REPRESENTATION_ITEM()
RATIONAL_B_SPLINE_CURVE((1.,1.00054983311312,1.000703031387))
REPRESENTATION_ITEM('')
);
#286=(
BOUNDED_CURVE()
B_SPLINE_CURVE(2,(#42651,#42652,#42653),.UNSPECIFIED.,.F.,.F.)
B_SPLINE_CURVE_WITH_KNOTS((3,3),(0.0383363983195159,0.0599649507081054),
 .UNSPECIFIED.)
CURVE()
GEOMETRIC_REPRESENTATION_ITEM()
RATIONAL_B_SPLINE_CURVE((1.00070303138659,1.0005498331128,1.))
REPRESENTATION_ITEM('')
);
#287=(
BOUNDED_CURVE()
B_SPLINE_CURVE(2,(#42655,#42656,#42657),.UNSPECIFIED.,.F.,.F.)
B_SPLINE_CURVE_WITH_KNOTS((3,3),(0.,0.0216285523885604),.UNSPECIFIED.)
CURVE()
GEOMETRIC_REPRESENTATION_ITEM()
RATIONAL_B_SPLINE_CURVE((1.,1.00054983311293,1.00070303138676))
REPRESENTATION_ITEM('')
);
#288=(
BOUNDED_CURVE()
B_SPLINE_CURVE(2,(#42658,#42659,#42660),.UNSPECIFIED.,.F.,.F.)
B_SPLINE_CURVE_WITH_KNOTS((3,3),(0.0383363983195082,0.0599649507081046),
 .UNSPECIFIED.)
CURVE()
GEOMETRIC_REPRESENTATION_ITEM()
RATIONAL_B_SPLINE_CURVE((1.00070303138548,1.00054983311193,1.))
REPRESENTATION_ITEM('')
);
#289=(
BOUNDED_CURVE()
B_SPLINE_CURVE(2,(#42662,#42663,#42664),.UNSPECIFIED.,.F.,.F.)
B_SPLINE_CURVE_WITH_KNOTS((3,3),(0.,0.0216285523886338),.UNSPECIFIED.)
CURVE()
GEOMETRIC_REPRESENTATION_ITEM()
RATIONAL_B_SPLINE_CURVE((1.,1.00054983310968,1.00070303138259))
REPRESENTATION_ITEM('')
);
#290=(
BOUNDED_CURVE()
B_SPLINE_CURVE(2,(#42665,#42666,#42667),.UNSPECIFIED.,.F.,.F.)
B_SPLINE_CURVE_WITH_KNOTS((3,3),(0.0383363983196053,0.0599649507081053),
 .UNSPECIFIED.)
CURVE()
GEOMETRIC_REPRESENTATION_ITEM()
RATIONAL_B_SPLINE_CURVE((1.00070303139687,1.00054983312084,1.))
REPRESENTATION_ITEM('')
);
#291=(
BOUNDED_CURVE()
B_SPLINE_CURVE(2,(#42669,#42670,#42671),.UNSPECIFIED.,.F.,.F.)
B_SPLINE_CURVE_WITH_KNOTS((3,3),(0.,0.0216285523885115),.UNSPECIFIED.)
CURVE()
GEOMETRIC_REPRESENTATION_ITEM()
RATIONAL_B_SPLINE_CURVE((1.,1.00054983312007,1.00070303139589))
REPRESENTATION_ITEM('')
);
#292=(
BOUNDED_CURVE()
B_SPLINE_CURVE(2,(#42672,#42673,#42674),.UNSPECIFIED.,.F.,.F.)
B_SPLINE_CURVE_WITH_KNOTS((3,3),(0.0383363983195966,0.0599649507081041),
 .UNSPECIFIED.)
CURVE()
GEOMETRIC_REPRESENTATION_ITEM()
RATIONAL_B_SPLINE_CURVE((1.00070303139314,1.00054983311792,1.))
REPRESENTATION_ITEM('')
);
#293=(
BOUNDED_CURVE()
B_SPLINE_CURVE(2,(#42676,#42677,#42678),.UNSPECIFIED.,.F.,.F.)
B_SPLINE_CURVE_WITH_KNOTS((3,3),(0.,0.0216285523885745),.UNSPECIFIED.)
CURVE()
GEOMETRIC_REPRESENTATION_ITEM()
RATIONAL_B_SPLINE_CURVE((1.,1.00054983311169,1.00070303138517))
REPRESENTATION_ITEM('')
);
#294=(
BOUNDED_CURVE()
B_SPLINE_CURVE(2,(#42679,#42680,#42681),.UNSPECIFIED.,.F.,.F.)
B_SPLINE_CURVE_WITH_KNOTS((3,3),(0.0383363983195842,0.0599649507081042),
 .UNSPECIFIED.)
CURVE()
GEOMETRIC_REPRESENTATION_ITEM()
RATIONAL_B_SPLINE_CURVE((1.00070303139113,1.00054983311635,1.))
REPRESENTATION_ITEM('')
);
#295=(
BOUNDED_CURVE()
B_SPLINE_CURVE(2,(#42683,#42684,#42685),.UNSPECIFIED.,.F.,.F.)
B_SPLINE_CURVE_WITH_KNOTS((3,3),(0.,0.0216285523885027),.UNSPECIFIED.)
CURVE()
GEOMETRIC_REPRESENTATION_ITEM()
RATIONAL_B_SPLINE_CURVE((1.,1.00054983311917,1.00070303139474))
REPRESENTATION_ITEM('')
);
#296=(
BOUNDED_CURVE()
B_SPLINE_CURVE(2,(#42686,#42687,#42688),.UNSPECIFIED.,.F.,.F.)
B_SPLINE_CURVE_WITH_KNOTS((3,3),(0.0383363983195908,0.0599649507081052),
 .UNSPECIFIED.)
CURVE()
GEOMETRIC_REPRESENTATION_ITEM()
RATIONAL_B_SPLINE_CURVE((1.00070303139353,1.00054983311823,1.))
REPRESENTATION_ITEM('')
);
#297=(
BOUNDED_CURVE()
B_SPLINE_CURVE(2,(#42690,#42691,#42692),.UNSPECIFIED.,.F.,.F.)
B_SPLINE_CURVE_WITH_KNOTS((3,3),(0.,0.0216285523885997),.UNSPECIFIED.)
CURVE()
GEOMETRIC_REPRESENTATION_ITEM()
RATIONAL_B_SPLINE_CURVE((1.,1.00054983311374,1.00070303138779))
REPRESENTATION_ITEM('')
);
#298=(
BOUNDED_CURVE()
B_SPLINE_CURVE(2,(#42693,#42694,#42695),.UNSPECIFIED.,.F.,.F.)
B_SPLINE_CURVE_WITH_KNOTS((3,3),(0.0383363983195373,0.0599649507081046),
 .UNSPECIFIED.)
CURVE()
GEOMETRIC_REPRESENTATION_ITEM()
RATIONAL_B_SPLINE_CURVE((1.00070303138796,1.00054983311387,1.))
REPRESENTATION_ITEM('')
);
#299=(
BOUNDED_CURVE()
B_SPLINE_CURVE(2,(#42697,#42698,#42699),.UNSPECIFIED.,.F.,.F.)
B_SPLINE_CURVE_WITH_KNOTS((3,3),(0.,0.0216285523885614),.UNSPECIFIED.)
CURVE()
GEOMETRIC_REPRESENTATION_ITEM()
RATIONAL_B_SPLINE_CURVE((1.,1.00054983311414,1.00070303138831))
REPRESENTATION_ITEM('')
);
#300=(
BOUNDED_CURVE()
B_SPLINE_CURVE(2,(#42700,#42701,#42702),.UNSPECIFIED.,.F.,.F.)
B_SPLINE_CURVE_WITH_KNOTS((3,3),(0.0383363983195286,0.0599649507081044),
 .UNSPECIFIED.)
CURVE()
GEOMETRIC_REPRESENTATION_ITEM()
RATIONAL_B_SPLINE_CURVE((1.00070303139035,1.00054983311574,1.))
REPRESENTATION_ITEM('')
);
#301=(
BOUNDED_CURVE()
B_SPLINE_CURVE(2,(#42704,#42705,#42706),.UNSPECIFIED.,.F.,.F.)
B_SPLINE_CURVE_WITH_KNOTS((3,3),(0.,0.0216285523885108),.UNSPECIFIED.)
CURVE()
GEOMETRIC_REPRESENTATION_ITEM()
RATIONAL_B_SPLINE_CURVE((1.,1.00054983311702,1.00070303139198))
REPRESENTATION_ITEM('')
);
#302=(
BOUNDED_CURVE()
B_SPLINE_CURVE(2,(#42707,#42708,#42709),.UNSPECIFIED.,.F.,.F.)
B_SPLINE_CURVE_WITH_KNOTS((3,3),(0.0383363983195893,0.0599649507081084),
 .UNSPECIFIED.)
CURVE()
GEOMETRIC_REPRESENTATION_ITEM()
RATIONAL_B_SPLINE_CURVE((1.00070303139496,1.00054983311935,1.))
REPRESENTATION_ITEM('')
);
#303=(
BOUNDED_CURVE()
B_SPLINE_CURVE(2,(#42711,#42712,#42713),.UNSPECIFIED.,.F.,.F.)
B_SPLINE_CURVE_WITH_KNOTS((3,3),(0.,0.021628552388581),.UNSPECIFIED.)
CURVE()
GEOMETRIC_REPRESENTATION_ITEM()
RATIONAL_B_SPLINE_CURVE((1.,1.00054983311652,1.00070303139135))
REPRESENTATION_ITEM('')
);
#304=(
BOUNDED_CURVE()
B_SPLINE_CURVE(2,(#42714,#42715,#42716),.UNSPECIFIED.,.F.,.F.)
B_SPLINE_CURVE_WITH_KNOTS((3,3),(0.0383363983195303,0.059964950708108),
 .UNSPECIFIED.)
CURVE()
GEOMETRIC_REPRESENTATION_ITEM()
RATIONAL_B_SPLINE_CURVE((1.00070303138822,1.00054983311407,1.))
REPRESENTATION_ITEM('')
);
#305=(
BOUNDED_CURVE()
B_SPLINE_CURVE(2,(#42718,#42719,#42720),.UNSPECIFIED.,.F.,.F.)
B_SPLINE_CURVE_WITH_KNOTS((3,3),(0.,0.0216285523886002),.UNSPECIFIED.)
CURVE()
GEOMETRIC_REPRESENTATION_ITEM()
RATIONAL_B_SPLINE_CURVE((1.,1.00054983311286,1.00070303138666))
REPRESENTATION_ITEM('')
);
#306=(
BOUNDED_CURVE()
B_SPLINE_CURVE(2,(#42721,#42722,#42723),.UNSPECIFIED.,.F.,.F.)
B_SPLINE_CURVE_WITH_KNOTS((3,3),(0.0383363983195208,0.059964950708108),
 .UNSPECIFIED.)
CURVE()
GEOMETRIC_REPRESENTATION_ITEM()
RATIONAL_B_SPLINE_CURVE((1.00070303138903,1.00054983311471,1.))
REPRESENTATION_ITEM('')
);
#307=(
BOUNDED_CURVE()
B_SPLINE_CURVE(2,(#42725,#42726,#42727),.UNSPECIFIED.,.F.,.F.)
B_SPLINE_CURVE_WITH_KNOTS((3,3),(0.,0.0216285523885397),.UNSPECIFIED.)
CURVE()
GEOMETRIC_REPRESENTATION_ITEM()
RATIONAL_B_SPLINE_CURVE((1.,1.00054983311497,1.00070303138936))
REPRESENTATION_ITEM('')
);
#308=(
BOUNDED_CURVE()
B_SPLINE_CURVE(2,(#42728,#42729,#42730),.UNSPECIFIED.,.F.,.F.)
B_SPLINE_CURVE_WITH_KNOTS((3,3),(0.0383363983195002,0.0599649507081073),
 .UNSPECIFIED.)
CURVE()
GEOMETRIC_REPRESENTATION_ITEM()
RATIONAL_B_SPLINE_CURVE((1.00070303138446,1.00054983311114,1.))
REPRESENTATION_ITEM('')
);
#309=(
BOUNDED_CURVE()
B_SPLINE_CURVE(2,(#42732,#42733,#42734),.UNSPECIFIED.,.F.,.F.)
B_SPLINE_CURVE_WITH_KNOTS((3,3),(0.,0.0216285523885717),.UNSPECIFIED.)
CURVE()
GEOMETRIC_REPRESENTATION_ITEM()
RATIONAL_B_SPLINE_CURVE((1.,1.00054983311286,1.00070303138667))
REPRESENTATION_ITEM('')
);
#310=(
BOUNDED_CURVE()
B_SPLINE_CURVE(2,(#42735,#42736,#42737),.UNSPECIFIED.,.F.,.F.)
B_SPLINE_CURVE_WITH_KNOTS((3,3),(0.0383363983195212,0.0599649507081082),
 .UNSPECIFIED.)
CURVE()
GEOMETRIC_REPRESENTATION_ITEM()
RATIONAL_B_SPLINE_CURVE((1.00070303138591,1.00054983311226,1.))
REPRESENTATION_ITEM('')
);
#311=(
BOUNDED_CURVE()
B_SPLINE_CURVE(2,(#42739,#42740,#42741),.UNSPECIFIED.,.F.,.F.)
B_SPLINE_CURVE_WITH_KNOTS((3,3),(0.,0.0216285523885764),.UNSPECIFIED.)
CURVE()
GEOMETRIC_REPRESENTATION_ITEM()
RATIONAL_B_SPLINE_CURVE((1.,1.0005498331135,1.00070303138749))
REPRESENTATION_ITEM('')
);
#312=(
BOUNDED_CURVE()
B_SPLINE_CURVE(2,(#42742,#42743,#42744),.UNSPECIFIED.,.F.,.F.)
B_SPLINE_CURVE_WITH_KNOTS((3,3),(0.0383363983195505,0.059964950708108),
 .UNSPECIFIED.)
CURVE()
GEOMETRIC_REPRESENTATION_ITEM()
RATIONAL_B_SPLINE_CURVE((1.00070303138856,1.00054983311434,1.))
REPRESENTATION_ITEM('')
);
#313=(
BOUNDED_CURVE()
B_SPLINE_CURVE(2,(#42746,#42747,#42748),.UNSPECIFIED.,.F.,.F.)
B_SPLINE_CURVE_WITH_KNOTS((3,3),(0.,0.0216285523885379),.UNSPECIFIED.)
CURVE()
GEOMETRIC_REPRESENTATION_ITEM()
RATIONAL_B_SPLINE_CURVE((1.,1.00054983311513,1.00070303138957))
REPRESENTATION_ITEM('')
);
#314=(
BOUNDED_CURVE()
B_SPLINE_CURVE(2,(#42749,#42750,#42751),.UNSPECIFIED.,.F.,.F.)
B_SPLINE_CURVE_WITH_KNOTS((3,3),(0.0383363983195525,0.0599649507081075),
 .UNSPECIFIED.)
CURVE()
GEOMETRIC_REPRESENTATION_ITEM()
RATIONAL_B_SPLINE_CURVE((1.00070303138821,1.00054983311407,1.))
REPRESENTATION_ITEM('')
);
#315=(
BOUNDED_CURVE()
B_SPLINE_CURVE(2,(#42753,#42754,#42755),.UNSPECIFIED.,.F.,.F.)
B_SPLINE_CURVE_WITH_KNOTS((3,3),(0.,0.0216285523885421),.UNSPECIFIED.)
CURVE()
GEOMETRIC_REPRESENTATION_ITEM()
RATIONAL_B_SPLINE_CURVE((1.,1.00054983311399,1.00070303138812))
REPRESENTATION_ITEM('')
);
#316=(
BOUNDED_CURVE()
B_SPLINE_CURVE(2,(#42756,#42757,#42758),.UNSPECIFIED.,.F.,.F.)
B_SPLINE_CURVE_WITH_KNOTS((3,3),(0.0383363983195263,0.0599649507081077),
 .UNSPECIFIED.)
CURVE()
GEOMETRIC_REPRESENTATION_ITEM()
RATIONAL_B_SPLINE_CURVE((1.00070303138823,1.00054983311409,1.))
REPRESENTATION_ITEM('')
);
#317=(
BOUNDED_CURVE()
B_SPLINE_CURVE(2,(#42760,#42761,#42762),.UNSPECIFIED.,.F.,.F.)
B_SPLINE_CURVE_WITH_KNOTS((3,3),(0.,0.0216285523886281),.UNSPECIFIED.)
CURVE()
GEOMETRIC_REPRESENTATION_ITEM()
RATIONAL_B_SPLINE_CURVE((1.,1.00054983311262,1.00070303138635))
REPRESENTATION_ITEM('')
);
#318=(
BOUNDED_CURVE()
B_SPLINE_CURVE(2,(#42763,#42764,#42765),.UNSPECIFIED.,.F.,.F.)
B_SPLINE_CURVE_WITH_KNOTS((3,3),(0.0383363983195607,0.0599649507081075),
 .UNSPECIFIED.)
CURVE()
GEOMETRIC_REPRESENTATION_ITEM()
RATIONAL_B_SPLINE_CURVE((1.00070303139002,1.00054983311548,1.))
REPRESENTATION_ITEM('')
);
#319=(
BOUNDED_CURVE()
B_SPLINE_CURVE(2,(#42767,#42768,#42769),.UNSPECIFIED.,.F.,.F.)
B_SPLINE_CURVE_WITH_KNOTS((3,3),(0.,0.0216285523885411),.UNSPECIFIED.)
CURVE()
GEOMETRIC_REPRESENTATION_ITEM()
RATIONAL_B_SPLINE_CURVE((1.,1.00054983311589,1.00070303139054))
REPRESENTATION_ITEM('')
);
#320=(
BOUNDED_CURVE()
B_SPLINE_CURVE(2,(#42770,#42771,#42772),.UNSPECIFIED.,.F.,.F.)
B_SPLINE_CURVE_WITH_KNOTS((3,3),(0.0383363983195253,0.0599649507081071),
 .UNSPECIFIED.)
CURVE()
GEOMETRIC_REPRESENTATION_ITEM()
RATIONAL_B_SPLINE_CURVE((1.0007030313902,1.00054983311562,1.))
REPRESENTATION_ITEM('')
);
#321=(
BOUNDED_CURVE()
B_SPLINE_CURVE(2,(#42774,#42775,#42776),.UNSPECIFIED.,.F.,.F.)
B_SPLINE_CURVE_WITH_KNOTS((3,3),(0.,0.0216285523886145),.UNSPECIFIED.)
CURVE()
GEOMETRIC_REPRESENTATION_ITEM()
RATIONAL_B_SPLINE_CURVE((1.,1.00054983311291,1.00070303138673))
REPRESENTATION_ITEM('')
);
#322=(
BOUNDED_CURVE()
B_SPLINE_CURVE(2,(#42777,#42778,#42779),.UNSPECIFIED.,.F.,.F.)
B_SPLINE_CURVE_WITH_KNOTS((3,3),(0.0383363983195111,0.0599649507081069),
 .UNSPECIFIED.)
CURVE()
GEOMETRIC_REPRESENTATION_ITEM()
RATIONAL_B_SPLINE_CURVE((1.00070303138553,1.00054983311197,1.))
REPRESENTATION_ITEM('')
);
#323=(
BOUNDED_CURVE()
B_SPLINE_CURVE(2,(#42781,#42782,#42783),.UNSPECIFIED.,.F.,.F.)
B_SPLINE_CURVE_WITH_KNOTS((3,3),(0.,0.0216285523885865),.UNSPECIFIED.)
CURVE()
GEOMETRIC_REPRESENTATION_ITEM()
RATIONAL_B_SPLINE_CURVE((1.,1.00054983311348,1.00070303138746))
REPRESENTATION_ITEM('')
);
#324=(
BOUNDED_CURVE()
B_SPLINE_CURVE(2,(#42784,#42785,#42786),.UNSPECIFIED.,.F.,.F.)
B_SPLINE_CURVE_WITH_KNOTS((3,3),(0.0383363983194927,0.0599649507081069),
 .UNSPECIFIED.)
CURVE()
GEOMETRIC_REPRESENTATION_ITEM()
RATIONAL_B_SPLINE_CURVE((1.00070303138451,1.00054983311118,1.))
REPRESENTATION_ITEM('')
);
#325=(
BOUNDED_CURVE()
B_SPLINE_CURVE(2,(#42788,#42789,#42790),.UNSPECIFIED.,.F.,.F.)
B_SPLINE_CURVE_WITH_KNOTS((3,3),(0.,0.0216285523884905),.UNSPECIFIED.)
CURVE()
GEOMETRIC_REPRESENTATION_ITEM()
RATIONAL_B_SPLINE_CURVE((1.,1.00054983311838,1.00070303139373))
REPRESENTATION_ITEM('')
);
#326=(
BOUNDED_CURVE()
B_SPLINE_CURVE(2,(#42791,#42792,#42793),.UNSPECIFIED.,.F.,.F.)
B_SPLINE_CURVE_WITH_KNOTS((3,3),(0.0383363983196131,0.0599649507081062),
 .UNSPECIFIED.)
CURVE()
GEOMETRIC_REPRESENTATION_ITEM()
RATIONAL_B_SPLINE_CURVE((1.00070303139756,1.00054983312138,1.))
REPRESENTATION_ITEM('')
);
#327=(
BOUNDED_CURVE()
B_SPLINE_CURVE(2,(#42795,#42796,#42797),.UNSPECIFIED.,.F.,.F.)
B_SPLINE_CURVE_WITH_KNOTS((3,3),(0.,0.0216285523886255),.UNSPECIFIED.)
CURVE()
GEOMETRIC_REPRESENTATION_ITEM()
RATIONAL_B_SPLINE_CURVE((1.,1.00054983311094,1.00070303138421))
REPRESENTATION_ITEM('')
);
#328=(
BOUNDED_CURVE()
B_SPLINE_CURVE(2,(#42798,#42799,#42800),.UNSPECIFIED.,.F.,.F.)
B_SPLINE_CURVE_WITH_KNOTS((3,3),(0.0383363983195603,0.0599649507081068),
 .UNSPECIFIED.)
CURVE()
GEOMETRIC_REPRESENTATION_ITEM()
RATIONAL_B_SPLINE_CURVE((1.0007030313936,1.00054983311828,1.))
REPRESENTATION_ITEM('')
);
#329=(
BOUNDED_CURVE()
B_SPLINE_CURVE(2,(#42802,#42803,#42804),.UNSPECIFIED.,.F.,.F.)
B_SPLINE_CURVE_WITH_KNOTS((3,3),(0.,0.021628552388625),.UNSPECIFIED.)
CURVE()
GEOMETRIC_REPRESENTATION_ITEM()
RATIONAL_B_SPLINE_CURVE((1.,1.00054983311264,1.00070303138639))
REPRESENTATION_ITEM('')
);
#330=(
BOUNDED_CURVE()
B_SPLINE_CURVE(2,(#42805,#42806,#42807),.UNSPECIFIED.,.F.,.F.)
B_SPLINE_CURVE_WITH_KNOTS((3,3),(0.0383363983195806,0.059964950708106),
 .UNSPECIFIED.)
CURVE()
GEOMETRIC_REPRESENTATION_ITEM()
RATIONAL_B_SPLINE_CURVE((1.00070303139255,1.00054983311746,1.))
REPRESENTATION_ITEM('')
);
#331=(
BOUNDED_CURVE()
B_SPLINE_CURVE(2,(#42808,#42809,#42810),.UNSPECIFIED.,.F.,.F.)
B_SPLINE_CURVE_WITH_KNOTS((3,3),(0.,0.0216285523884755),.UNSPECIFIED.)
CURVE()
GEOMETRIC_REPRESENTATION_ITEM()
RATIONAL_B_SPLINE_CURVE((1.,1.00054983312103,1.00070303139712))
REPRESENTATION_ITEM('')
);
#332=(
BOUNDED_CURVE()
B_SPLINE_CURVE(2,(#43060,#43061,#43062),.UNSPECIFIED.,.F.,.F.)
B_SPLINE_CURVE_WITH_KNOTS((3,3),(0.,0.0124050518656677),.UNSPECIFIED.)
CURVE()
GEOMETRIC_REPRESENTATION_ITEM()
RATIONAL_B_SPLINE_CURVE((1.,1.00128973373368,1.00206600698525))
REPRESENTATION_ITEM('')
);
#333=(
BOUNDED_CURVE()
B_SPLINE_CURVE(2,(#43066,#43067,#43068),.UNSPECIFIED.,.F.,.F.)
B_SPLINE_CURVE_WITH_KNOTS((3,3),(0.0499141116010052,0.0623191634666637),
 .UNSPECIFIED.)
CURVE()
GEOMETRIC_REPRESENTATION_ITEM()
RATIONAL_B_SPLINE_CURVE((1.00206600698578,1.00128973373401,1.))
REPRESENTATION_ITEM('')
);
#334=(
BOUNDED_CURVE()
B_SPLINE_CURVE(2,(#43070,#43071,#43072),.UNSPECIFIED.,.F.,.F.)
B_SPLINE_CURVE_WITH_KNOTS((3,3),(0.,0.0124050518656597),.UNSPECIFIED.)
CURVE()
GEOMETRIC_REPRESENTATION_ITEM()
RATIONAL_B_SPLINE_CURVE((1.,1.00128973373396,1.00206600698569))
REPRESENTATION_ITEM('')
);
#335=(
BOUNDED_CURVE()
B_SPLINE_CURVE(2,(#43076,#43077,#43078),.UNSPECIFIED.,.F.,.F.)
B_SPLINE_CURVE_WITH_KNOTS((3,3),(0.049914111601003,0.0623191634666626),
 .UNSPECIFIED.)
CURVE()
GEOMETRIC_REPRESENTATION_ITEM()
RATIONAL_B_SPLINE_CURVE((1.00206600698569,1.00128973373396,1.))
REPRESENTATION_ITEM('')
);
#336=(
BOUNDED_CURVE()
B_SPLINE_CURVE(2,(#43080,#43081,#43082),.UNSPECIFIED.,.F.,.F.)
B_SPLINE_CURVE_WITH_KNOTS((3,3),(0.,0.0124050518656559),.UNSPECIFIED.)
CURVE()
GEOMETRIC_REPRESENTATION_ITEM()
RATIONAL_B_SPLINE_CURVE((1.,1.00128973373402,1.0020660069858))
REPRESENTATION_ITEM('')
);
#337=(
BOUNDED_CURVE()
B_SPLINE_CURVE(2,(#43086,#43087,#43088),.UNSPECIFIED.,.F.,.F.)
B_SPLINE_CURVE_WITH_KNOTS((3,3),(0.0499141116009975,0.062319163466664),
 .UNSPECIFIED.)
CURVE()
GEOMETRIC_REPRESENTATION_ITEM()
RATIONAL_B_SPLINE_CURVE((1.00206600698527,1.0012897337337,1.))
REPRESENTATION_ITEM('')
);
#338=(
BOUNDED_CURVE()
B_SPLINE_CURVE(2,(#43090,#43091,#43092),.UNSPECIFIED.,.F.,.F.)
B_SPLINE_CURVE_WITH_KNOTS((3,3),(0.,0.0124050518656685),.UNSPECIFIED.)
CURVE()
GEOMETRIC_REPRESENTATION_ITEM()
RATIONAL_B_SPLINE_CURVE((1.,1.00128973373364,1.00206600698518))
REPRESENTATION_ITEM('')
);
#339=(
BOUNDED_CURVE()
B_SPLINE_CURVE(2,(#43096,#43097,#43098),.UNSPECIFIED.,.F.,.F.)
B_SPLINE_CURVE_WITH_KNOTS((3,3),(0.049914111600997,0.0623191634666649),
 .UNSPECIFIED.)
CURVE()
GEOMETRIC_REPRESENTATION_ITEM()
RATIONAL_B_SPLINE_CURVE((1.00206600698519,1.00128973373364,1.))
REPRESENTATION_ITEM('')
);
#340=(
BOUNDED_CURVE()
B_SPLINE_CURVE(2,(#43100,#43101,#43102),.UNSPECIFIED.,.F.,.F.)
B_SPLINE_CURVE_WITH_KNOTS((3,3),(0.,0.0124050518656616),.UNSPECIFIED.)
CURVE()
GEOMETRIC_REPRESENTATION_ITEM()
RATIONAL_B_SPLINE_CURVE((1.,1.0012897337338,1.00206600698545))
REPRESENTATION_ITEM('')
);
#341=(
BOUNDED_CURVE()
B_SPLINE_CURVE(2,(#43106,#43107,#43108),.UNSPECIFIED.,.F.,.F.)
B_SPLINE_CURVE_WITH_KNOTS((3,3),(0.049914111601002,0.0623191634666634),
 .UNSPECIFIED.)
CURVE()
GEOMETRIC_REPRESENTATION_ITEM()
RATIONAL_B_SPLINE_CURVE((1.00206600698545,1.0012897337338,1.))
REPRESENTATION_ITEM('')
);
#342=(
BOUNDED_CURVE()
B_SPLINE_CURVE(2,(#43110,#43111,#43112),.UNSPECIFIED.,.F.,.F.)
B_SPLINE_CURVE_WITH_KNOTS((3,3),(0.,0.0124050518656481),.UNSPECIFIED.)
CURVE()
GEOMETRIC_REPRESENTATION_ITEM()
RATIONAL_B_SPLINE_CURVE((1.,1.00128973373427,1.0020660069862))
REPRESENTATION_ITEM('')
);
#343=(
BOUNDED_CURVE()
B_SPLINE_CURVE(2,(#43115,#43116,#43117),.UNSPECIFIED.,.F.,.F.)
B_SPLINE_CURVE_WITH_KNOTS((3,3),(0.0499141116009961,0.0623191634666644),
 .UNSPECIFIED.)
CURVE()
GEOMETRIC_REPRESENTATION_ITEM()
RATIONAL_B_SPLINE_CURVE((1.0020660069852,1.00128973373365,1.))
REPRESENTATION_ITEM('')
);
#344=(
BOUNDED_CURVE()
B_SPLINE_CURVE(2,(#63186,#63187,#63188),.UNSPECIFIED.,.F.,.F.)
B_SPLINE_CURVE_WITH_KNOTS((3,3),(0.,0.0126130588257634),.UNSPECIFIED.)
CURVE()
GEOMETRIC_REPRESENTATION_ITEM()
RATIONAL_B_SPLINE_CURVE((1.,1.00234596681246,1.00329298027559))
REPRESENTATION_ITEM('')
);
#345=(
BOUNDED_CURVE()
B_SPLINE_CURVE(2,(#63192,#63193,#63194),.UNSPECIFIED.,.F.,.F.)
B_SPLINE_CURVE_WITH_KNOTS((3,3),(0.0296897347922137,0.0423027936179765),
 .UNSPECIFIED.)
CURVE()
GEOMETRIC_REPRESENTATION_ITEM()
RATIONAL_B_SPLINE_CURVE((1.00329298027598,1.00234596681273,1.))
REPRESENTATION_ITEM('')
);
#346=(
BOUNDED_CURVE()
B_SPLINE_CURVE(2,(#63196,#63197,#63198),.UNSPECIFIED.,.F.,.F.)
B_SPLINE_CURVE_WITH_KNOTS((3,3),(0.,0.0126130588257622),.UNSPECIFIED.)
CURVE()
GEOMETRIC_REPRESENTATION_ITEM()
RATIONAL_B_SPLINE_CURVE((1.,1.00234596681263,1.00329298027583))
REPRESENTATION_ITEM('')
);
#347=(
BOUNDED_CURVE()
B_SPLINE_CURVE(2,(#63202,#63203,#63204),.UNSPECIFIED.,.F.,.F.)
B_SPLINE_CURVE_WITH_KNOTS((3,3),(0.0296897347922138,0.0423027936179762),
 .UNSPECIFIED.)
CURVE()
GEOMETRIC_REPRESENTATION_ITEM()
RATIONAL_B_SPLINE_CURVE((1.00329298027583,1.00234596681263,1.))
REPRESENTATION_ITEM('')
);
#348=(
BOUNDED_CURVE()
B_SPLINE_CURVE(2,(#63206,#63207,#63208),.UNSPECIFIED.,.F.,.F.)
B_SPLINE_CURVE_WITH_KNOTS((3,3),(0.,0.0126130588257628),.UNSPECIFIED.)
CURVE()
GEOMETRIC_REPRESENTATION_ITEM()
RATIONAL_B_SPLINE_CURVE((1.,1.00234596681273,1.00329298027598))
REPRESENTATION_ITEM('')
);
#349=(
BOUNDED_CURVE()
B_SPLINE_CURVE(2,(#63212,#63213,#63214),.UNSPECIFIED.,.F.,.F.)
B_SPLINE_CURVE_WITH_KNOTS((3,3),(0.0296897347922133,0.0423027936179766),
 .UNSPECIFIED.)
CURVE()
GEOMETRIC_REPRESENTATION_ITEM()
RATIONAL_B_SPLINE_CURVE((1.00329298027559,1.00234596681246,1.))
REPRESENTATION_ITEM('')
);
#350=(
BOUNDED_CURVE()
B_SPLINE_CURVE(2,(#63216,#63217,#63218),.UNSPECIFIED.,.F.,.F.)
B_SPLINE_CURVE_WITH_KNOTS((3,3),(0.,0.0126130588257654),.UNSPECIFIED.)
CURVE()
GEOMETRIC_REPRESENTATION_ITEM()
RATIONAL_B_SPLINE_CURVE((1.,1.00234596681226,1.00329298027532))
REPRESENTATION_ITEM('')
);
#351=(
BOUNDED_CURVE()
B_SPLINE_CURVE(2,(#63222,#63223,#63224),.UNSPECIFIED.,.F.,.F.)
B_SPLINE_CURVE_WITH_KNOTS((3,3),(0.029689734792212,0.0423027936179753),
 .UNSPECIFIED.)
CURVE()
GEOMETRIC_REPRESENTATION_ITEM()
RATIONAL_B_SPLINE_CURVE((1.00329298027571,1.00234596681254,1.))
REPRESENTATION_ITEM('')
);
#352=(
BOUNDED_CURVE()
B_SPLINE_CURVE(2,(#63226,#63227,#63228),.UNSPECIFIED.,.F.,.F.)
B_SPLINE_CURVE_WITH_KNOTS((3,3),(0.,0.0126130588257619),.UNSPECIFIED.)
CURVE()
GEOMETRIC_REPRESENTATION_ITEM()
RATIONAL_B_SPLINE_CURVE((1.,1.00234596681263,1.00329298027583))
REPRESENTATION_ITEM('')
);
#353=(
BOUNDED_CURVE()
B_SPLINE_CURVE(2,(#63232,#63233,#63234),.UNSPECIFIED.,.F.,.F.)
B_SPLINE_CURVE_WITH_KNOTS((3,3),(0.0296897347922146,0.0423027936179762),
 .UNSPECIFIED.)
CURVE()
GEOMETRIC_REPRESENTATION_ITEM()
RATIONAL_B_SPLINE_CURVE((1.00329298027583,1.00234596681263,1.))
REPRESENTATION_ITEM('')
);
#354=(
BOUNDED_CURVE()
B_SPLINE_CURVE(2,(#63236,#63237,#63238),.UNSPECIFIED.,.F.,.F.)
B_SPLINE_CURVE_WITH_KNOTS((3,3),(0.,0.0126130588257574),.UNSPECIFIED.)
CURVE()
GEOMETRIC_REPRESENTATION_ITEM()
RATIONAL_B_SPLINE_CURVE((1.,1.002345966813,1.00329298027635))
REPRESENTATION_ITEM('')
);
#355=(
BOUNDED_CURVE()
B_SPLINE_CURVE(2,(#63241,#63242,#63243),.UNSPECIFIED.,.F.,.F.)
B_SPLINE_CURVE_WITH_KNOTS((3,3),(0.029689734792213,0.0423027936179761),
 .UNSPECIFIED.)
CURVE()
GEOMETRIC_REPRESENTATION_ITEM()
RATIONAL_B_SPLINE_CURVE((1.00329298027557,1.00234596681244,1.))
REPRESENTATION_ITEM('')
);
#356=(
BOUNDED_CURVE()
B_SPLINE_CURVE(2,(#80918,#80919,#80920),.UNSPECIFIED.,.F.,.F.)
B_SPLINE_CURVE_WITH_KNOTS((3,3),(0.,0.0569264978342637),.UNSPECIFIED.)
CURVE()
GEOMETRIC_REPRESENTATION_ITEM()
RATIONAL_B_SPLINE_CURVE((1.,1.00316883460161,1.))
REPRESENTATION_ITEM('')
);
#357=(
BOUNDED_CURVE()
B_SPLINE_CURVE(2,(#80923,#80924,#80925),.UNSPECIFIED.,.F.,.F.)
B_SPLINE_CURVE_WITH_KNOTS((3,3),(0.,0.0569264978342636),.UNSPECIFIED.)
CURVE()
GEOMETRIC_REPRESENTATION_ITEM()
RATIONAL_B_SPLINE_CURVE((1.,1.00316883454694,1.))
REPRESENTATION_ITEM('')
);
#358=(
BOUNDED_CURVE()
B_SPLINE_CURVE(2,(#80930,#80931,#80932),.UNSPECIFIED.,.F.,.F.)
B_SPLINE_CURVE_WITH_KNOTS((3,3),(0.,0.0569264978342637),.UNSPECIFIED.)
CURVE()
GEOMETRIC_REPRESENTATION_ITEM()
RATIONAL_B_SPLINE_CURVE((1.,1.00316883459387,1.))
REPRESENTATION_ITEM('')
);
#359=(
BOUNDED_CURVE()
B_SPLINE_CURVE(2,(#80936,#80937,#80938),.UNSPECIFIED.,.F.,.F.)
B_SPLINE_CURVE_WITH_KNOTS((3,3),(0.,0.0569264978342637),.UNSPECIFIED.)
CURVE()
GEOMETRIC_REPRESENTATION_ITEM()
RATIONAL_B_SPLINE_CURVE((1.,1.00316883460998,1.))
REPRESENTATION_ITEM('')
);
#360=TOROIDAL_SURFACE('',#16122,2.6505,0.2);
#361=TOROIDAL_SURFACE('',#16315,4.05,0.2);
#362=TOROIDAL_SURFACE('',#16478,2.6505,0.2);
#363=TOROIDAL_SURFACE('',#16535,1.5635,0.1);
#364=B_SPLINE_SURFACE_WITH_KNOTS('',3,3,((#40791,#40792,#40793,#40794,#40795,
#40796,#40797,#40798,#40799,#40800,#40801,#40802,#40803,#40804,#40805,#40806,
#40807,#40808,#40809,#40810,#40811,#40812,#40813,#40814,#40815,#40816,#40817,
#40818,#40819,#40820,#40821,#40822,#40823,#40824,#40825,#40826,#40827,#40828,
#40829,#40830,#40831,#40832,#40833,#40834,#40835,#40836,#40837,#40838,#40839,
#40840,#40841,#40842,#40843,#40844,#40845,#40846,#40847,#40848,#40849,#40850,
#40851,#40852,#40853,#40854,#40855,#40856,#40857,#40858,#40859,#40860,#40861,
#40862,#40863,#40864,#40865,#40866,#40867,#40868,#40869,#40870,#40871,#40872,
#40873,#40874,#40875,#40876,#40877,#40878,#40879,#40880,#40881,#40882,#40883,
#40884,#40885,#40886,#40887,#40888,#40889,#40890,#40891,#40892,#40893,#40894,
#40895,#40896,#40897,#40898,#40899,#40900,#40901,#40902,#40903,#40904,#40905,
#40906,#40907,#40908,#40909,#40910,#40911,#40912,#40913,#40914,#40915,#40916,
#40917,#40918,#40919,#40920,#40921,#40922,#40923,#40924,#40925,#40926,#40927,
#40928,#40929,#40930,#40931,#40932,#40933,#40934,#40935,#40936,#40937,#40938,
#40939,#40940,#40941,#40942,#40943,#40944,#40945,#40946,#40947),(#40948,
#40949,#40950,#40951,#40952,#40953,#40954,#40955,#40956,#40957,#40958,#40959,
#40960,#40961,#40962,#40963,#40964,#40965,#40966,#40967,#40968,#40969,#40970,
#40971,#40972,#40973,#40974,#40975,#40976,#40977,#40978,#40979,#40980,#40981,
#40982,#40983,#40984,#40985,#40986,#40987,#40988,#40989,#40990,#40991,#40992,
#40993,#40994,#40995,#40996,#40997,#40998,#40999,#41000,#41001,#41002,#41003,
#41004,#41005,#41006,#41007,#41008,#41009,#41010,#41011,#41012,#41013,#41014,
#41015,#41016,#41017,#41018,#41019,#41020,#41021,#41022,#41023,#41024,#41025,
#41026,#41027,#41028,#41029,#41030,#41031,#41032,#41033,#41034,#41035,#41036,
#41037,#41038,#41039,#41040,#41041,#41042,#41043,#41044,#41045,#41046,#41047,
#41048,#41049,#41050,#41051,#41052,#41053,#41054,#41055,#41056,#41057,#41058,
#41059,#41060,#41061,#41062,#41063,#41064,#41065,#41066,#41067,#41068,#41069,
#41070,#41071,#41072,#41073,#41074,#41075,#41076,#41077,#41078,#41079,#41080,
#41081,#41082,#41083,#41084,#41085,#41086,#41087,#41088,#41089,#41090,#41091,
#41092,#41093,#41094,#41095,#41096,#41097,#41098,#41099,#41100,#41101,#41102,
#41103,#41104),(#41105,#41106,#41107,#41108,#41109,#41110,#41111,#41112,
#41113,#41114,#41115,#41116,#41117,#41118,#41119,#41120,#41121,#41122,#41123,
#41124,#41125,#41126,#41127,#41128,#41129,#41130,#41131,#41132,#41133,#41134,
#41135,#41136,#41137,#41138,#41139,#41140,#41141,#41142,#41143,#41144,#41145,
#41146,#41147,#41148,#41149,#41150,#41151,#41152,#41153,#41154,#41155,#41156,
#41157,#41158,#41159,#41160,#41161,#41162,#41163,#41164,#41165,#41166,#41167,
#41168,#41169,#41170,#41171,#41172,#41173,#41174,#41175,#41176,#41177,#41178,
#41179,#41180,#41181,#41182,#41183,#41184,#41185,#41186,#41187,#41188,#41189,
#41190,#41191,#41192,#41193,#41194,#41195,#41196,#41197,#41198,#41199,#41200,
#41201,#41202,#41203,#41204,#41205,#41206,#41207,#41208,#41209,#41210,#41211,
#41212,#41213,#41214,#41215,#41216,#41217,#41218,#41219,#41220,#41221,#41222,
#41223,#41224,#41225,#41226,#41227,#41228,#41229,#41230,#41231,#41232,#41233,
#41234,#41235,#41236,#41237,#41238,#41239,#41240,#41241,#41242,#41243,#41244,
#41245,#41246,#41247,#41248,#41249,#41250,#41251,#41252,#41253,#41254,#41255,
#41256,#41257,#41258,#41259,#41260,#41261),(#41262,#41263,#41264,#41265,
#41266,#41267,#41268,#41269,#41270,#41271,#41272,#41273,#41274,#41275,#41276,
#41277,#41278,#41279,#41280,#41281,#41282,#41283,#41284,#41285,#41286,#41287,
#41288,#41289,#41290,#41291,#41292,#41293,#41294,#41295,#41296,#41297,#41298,
#41299,#41300,#41301,#41302,#41303,#41304,#41305,#41306,#41307,#41308,#41309,
#41310,#41311,#41312,#41313,#41314,#41315,#41316,#41317,#41318,#41319,#41320,
#41321,#41322,#41323,#41324,#41325,#41326,#41327,#41328,#41329,#41330,#41331,
#41332,#41333,#41334,#41335,#41336,#41337,#41338,#41339,#41340,#41341,#41342,
#41343,#41344,#41345,#41346,#41347,#41348,#41349,#41350,#41351,#41352,#41353,
#41354,#41355,#41356,#41357,#41358,#41359,#41360,#41361,#41362,#41363,#41364,
#41365,#41366,#41367,#41368,#41369,#41370,#41371,#41372,#41373,#41374,#41375,
#41376,#41377,#41378,#41379,#41380,#41381,#41382,#41383,#41384,#41385,#41386,
#41387,#41388,#41389,#41390,#41391,#41392,#41393,#41394,#41395,#41396,#41397,
#41398,#41399,#41400,#41401,#41402,#41403,#41404,#41405,#41406,#41407,#41408,
#41409,#41410,#41411,#41412,#41413,#41414,#41415,#41416,#41417,#41418)),
 .UNSPECIFIED.,.F.,.F.,.F.,(4,4),(4,1,1,1,1,1,1,1,1,1,1,1,1,1,1,1,1,1,1,
1,1,1,1,1,1,1,1,1,1,1,1,1,1,1,1,1,1,1,1,1,1,1,1,1,1,1,1,1,1,1,1,1,1,1,1,
1,1,1,1,1,1,1,1,1,1,1,1,1,1,1,1,1,1,1,1,1,1,1,1,1,1,1,1,1,1,1,1,1,1,1,1,
1,1,1,1,1,1,1,1,1,1,1,1,1,1,1,1,1,1,1,1,1,1,1,1,1,1,1,1,1,1,1,1,1,1,1,1,
1,1,1,1,1,1,1,1,1,1,1,1,1,1,1,1,1,1,1,1,1,1,1,1,1,1,1,4),(-0.000414828532079457,
0.0529939397069977),(8.30815772716272,9.30587489071033,10.3035920542579,
11.3013092178055,12.2990263813532,13.2967435449008,14.2944607084484,15.292177871996,
16.2898950355436,17.2876121990912,18.2853293626388,19.2830465261864,20.280763689734,
21.2784808532816,22.2761980168293,23.2739151803769,24.2716323439245,25.2693495074721,
26.2670666710197,27.2647838345673,28.2625009981149,29.2602181616625,30.2579353252101,
31.2556524887577,32.2533696523054,33.251086815853,34.2488039794006,35.2465211429482,
36.2442383064958,37.2419554700434,38.239672633591,39.2373897971386,40.2351069606862,
41.2328241242338,42.2305412877814,43.2282584513291,44.2259756148767,45.2236927784243,
46.2214099419719,47.2191271055195,48.2168442690671,49.2145614326147,50.2122785961623,
51.2099957597099,52.2077129232575,53.2054300868052,54.2031472503528,55.2008644139004,
56.198581577448,57.1962987409956,58.1940159045432,59.1917330680908,60.1894502316384,
61.187167395186,62.1848845587336,63.1826017222812,64.1803188858289,65.1780360493765,
66.1757532129241,67.1734703764717,68.1711875400193,69.1689047035669,70.1666218671145,
71.1643390306621,72.1620561942097,73.1597733577573,74.157490521305,75.1552076848526,
76.1529248484002,77.1506420119478,78.1483591754954,79.146076339043,80.1437935025906,
81.1415106661382,82.1392278296858,83.1369449932334,84.1346621567811,85.1323793203287,
86.1300964838763,87.1278136474239,88.1255308109715,89.1232479745191,90.1209651380667,
91.1186823016143,92.1163994651619,93.1141166287095,94.1118337922572,95.1095509558048,
96.1072681193524,97.1049852829,98.1027024464476,99.1004196099952,100.098136773543,
101.09585393709,102.093571100638,103.091288264186,104.089005427733,105.086722591281,
106.084439754828,107.082156918376,108.079874081924,109.077591245471,110.075308409019,
111.073025572567,112.070742736114,113.068459899662,114.066177063209,115.063894226757,
116.061611390305,117.059328553852,118.0570457174,119.054762880947,120.052480044495,
121.050197208043,122.04791437159,123.045631535138,124.043348698685,125.041065862233,
126.038783025781,127.036500189328,128.034217352876,129.031934516423,130.029651679971,
131.027368843519,132.025086007066,133.022803170614,134.020520334162,135.018237497709,
136.015954661257,137.013671824804,138.011388988352,139.0091061519,140.006823315447,
141.004540478995,142.002257642542,142.99997480609,143.997691969638,144.995409133185,
145.993126296733,146.99084346028,147.988560623828,148.986277787376,149.983994950923,
150.981712114471,151.979429278019,152.977146441566,153.974863605114,154.972580768661,
155.970297932209,156.968015095757,157.965732259304,158.963449422852,159.961166586399,
160.958883749947,161.957015742027),.UNSPECIFIED.);
#365=B_SPLINE_SURFACE_WITH_KNOTS('',3,3,((#41606,#41607,#41608,#41609,#41610,
#41611,#41612,#41613,#41614,#41615,#41616,#41617,#41618,#41619,#41620,#41621,
#41622,#41623,#41624,#41625,#41626,#41627,#41628,#41629,#41630,#41631,#41632,
#41633,#41634,#41635,#41636,#41637,#41638,#41639,#41640,#41641,#41642,#41643,
#41644,#41645,#41646,#41647,#41648,#41649,#41650,#41651,#41652,#41653,#41654,
#41655,#41656,#41657,#41658,#41659,#41660,#41661,#41662,#41663,#41664,#41665,
#41666,#41667,#41668,#41669,#41670,#41671,#41672,#41673,#41674,#41675,#41676,
#41677,#41678,#41679,#41680,#41681,#41682,#41683,#41684,#41685,#41686,#41687,
#41688,#41689,#41690,#41691,#41692,#41693,#41694,#41695,#41696,#41697,#41698,
#41699,#41700,#41701,#41702,#41703,#41704,#41705,#41706,#41707,#41708,#41709,
#41710,#41711,#41712,#41713,#41714,#41715,#41716,#41717,#41718,#41719,#41720,
#41721,#41722,#41723,#41724,#41725,#41726,#41727,#41728,#41729,#41730,#41731,
#41732,#41733,#41734,#41735,#41736,#41737,#41738,#41739,#41740,#41741,#41742,
#41743,#41744,#41745,#41746,#41747,#41748,#41749,#41750,#41751,#41752,#41753,
#41754,#41755,#41756,#41757,#41758,#41759,#41760,#41761,#41762),(#41763,
#41764,#41765,#41766,#41767,#41768,#41769,#41770,#41771,#41772,#41773,#41774,
#41775,#41776,#41777,#41778,#41779,#41780,#41781,#41782,#41783,#41784,#41785,
#41786,#41787,#41788,#41789,#41790,#41791,#41792,#41793,#41794,#41795,#41796,
#41797,#41798,#41799,#41800,#41801,#41802,#41803,#41804,#41805,#41806,#41807,
#41808,#41809,#41810,#41811,#41812,#41813,#41814,#41815,#41816,#41817,#41818,
#41819,#41820,#41821,#41822,#41823,#41824,#41825,#41826,#41827,#41828,#41829,
#41830,#41831,#41832,#41833,#41834,#41835,#41836,#41837,#41838,#41839,#41840,
#41841,#41842,#41843,#41844,#41845,#41846,#41847,#41848,#41849,#41850,#41851,
#41852,#41853,#41854,#41855,#41856,#41857,#41858,#41859,#41860,#41861,#41862,
#41863,#41864,#41865,#41866,#41867,#41868,#41869,#41870,#41871,#41872,#41873,
#41874,#41875,#41876,#41877,#41878,#41879,#41880,#41881,#41882,#41883,#41884,
#41885,#41886,#41887,#41888,#41889,#41890,#41891,#41892,#41893,#41894,#41895,
#41896,#41897,#41898,#41899,#41900,#41901,#41902,#41903,#41904,#41905,#41906,
#41907,#41908,#41909,#41910,#41911,#41912,#41913,#41914,#41915,#41916,#41917,
#41918,#41919),(#41920,#41921,#41922,#41923,#41924,#41925,#41926,#41927,
#41928,#41929,#41930,#41931,#41932,#41933,#41934,#41935,#41936,#41937,#41938,
#41939,#41940,#41941,#41942,#41943,#41944,#41945,#41946,#41947,#41948,#41949,
#41950,#41951,#41952,#41953,#41954,#41955,#41956,#41957,#41958,#41959,#41960,
#41961,#41962,#41963,#41964,#41965,#41966,#41967,#41968,#41969,#41970,#41971,
#41972,#41973,#41974,#41975,#41976,#41977,#41978,#41979,#41980,#41981,#41982,
#41983,#41984,#41985,#41986,#41987,#41988,#41989,#41990,#41991,#41992,#41993,
#41994,#41995,#41996,#41997,#41998,#41999,#42000,#42001,#42002,#42003,#42004,
#42005,#42006,#42007,#42008,#42009,#42010,#42011,#42012,#42013,#42014,#42015,
#42016,#42017,#42018,#42019,#42020,#42021,#42022,#42023,#42024,#42025,#42026,
#42027,#42028,#42029,#42030,#42031,#42032,#42033,#42034,#42035,#42036,#42037,
#42038,#42039,#42040,#42041,#42042,#42043,#42044,#42045,#42046,#42047,#42048,
#42049,#42050,#42051,#42052,#42053,#42054,#42055,#42056,#42057,#42058,#42059,
#42060,#42061,#42062,#42063,#42064,#42065,#42066,#42067,#42068,#42069,#42070,
#42071,#42072,#42073,#42074,#42075,#42076),(#42077,#42078,#42079,#42080,
#42081,#42082,#42083,#42084,#42085,#42086,#42087,#42088,#42089,#42090,#42091,
#42092,#42093,#42094,#42095,#42096,#42097,#42098,#42099,#42100,#42101,#42102,
#42103,#42104,#42105,#42106,#42107,#42108,#42109,#42110,#42111,#42112,#42113,
#42114,#42115,#42116,#42117,#42118,#42119,#42120,#42121,#42122,#42123,#42124,
#42125,#42126,#42127,#42128,#42129,#42130,#42131,#42132,#42133,#42134,#42135,
#42136,#42137,#42138,#42139,#42140,#42141,#42142,#42143,#42144,#42145,#42146,
#42147,#42148,#42149,#42150,#42151,#42152,#42153,#42154,#42155,#42156,#42157,
#42158,#42159,#42160,#42161,#42162,#42163,#42164,#42165,#42166,#42167,#42168,
#42169,#42170,#42171,#42172,#42173,#42174,#42175,#42176,#42177,#42178,#42179,
#42180,#42181,#42182,#42183,#42184,#42185,#42186,#42187,#42188,#42189,#42190,
#42191,#42192,#42193,#42194,#42195,#42196,#42197,#42198,#42199,#42200,#42201,
#42202,#42203,#42204,#42205,#42206,#42207,#42208,#42209,#42210,#42211,#42212,
#42213,#42214,#42215,#42216,#42217,#42218,#42219,#42220,#42221,#42222,#42223,
#42224,#42225,#42226,#42227,#42228,#42229,#42230,#42231,#42232,#42233)),
 .UNSPECIFIED.,.F.,.F.,.F.,(4,4),(4,1,1,1,1,1,1,1,1,1,1,1,1,1,1,1,1,1,1,
1,1,1,1,1,1,1,1,1,1,1,1,1,1,1,1,1,1,1,1,1,1,1,1,1,1,1,1,1,1,1,1,1,1,1,1,
1,1,1,1,1,1,1,1,1,1,1,1,1,1,1,1,1,1,1,1,1,1,1,1,1,1,1,1,1,1,1,1,1,1,1,1,
1,1,1,1,1,1,1,1,1,1,1,1,1,1,1,1,1,1,1,1,1,1,1,1,1,1,1,1,1,1,1,1,1,1,1,1,
1,1,1,1,1,1,1,1,1,1,1,1,1,1,1,1,1,1,1,1,1,1,1,1,1,1,1,4),(-0.000352467397055627,
0.053040310820889),(11.6159783635572,12.6141103608891,13.6118275244367,
14.6095446879844,15.607261851532,16.6049790150796,17.6026961786272,18.6004133421748,
19.5981305057224,20.59584766927,21.5935648328176,22.5912819963652,23.5889991599128,
24.5867163234605,25.5844334870081,26.5821506505557,27.5798678141033,28.5775849776509,
29.5753021411985,30.5730193047461,31.5707364682937,32.5684536318413,33.5661707953889,
34.5638879589366,35.5616051224842,36.5593222860318,37.5570394495794,38.554756613127,
39.5524737766746,40.5501909402222,41.5479081037698,42.5456252673174,43.543342430865,
44.5410595944127,45.5387767579603,46.5364939215079,47.5342110850555,48.5319282486031,
49.5296454121507,50.5273625756983,51.5250797392459,52.5227969027935,53.5205140663411,
54.5182312298887,55.5159483934364,56.513665556984,57.5113827205316,58.5090998840792,
59.5068170476268,60.5045342111744,61.502251374722,62.4999685382696,63.4976857018172,
64.4954028653649,65.4931200289125,66.4908371924601,67.4885543560077,68.4862715195553,
69.4839886831029,70.4817058466505,71.4794230101981,72.4771401737457,73.4748573372933,
74.4725745008409,75.4702916643886,76.4680088279362,77.4657259914838,78.4634431550314,
79.461160318579,80.4588774821266,81.4565946456742,82.4543118092218,83.4520289727694,
84.449746136317,85.4474632998647,86.4451804634123,87.4428976269599,88.4406147905075,
89.4383319540551,90.4360491176027,91.4337662811503,92.4314834446979,93.4292006082455,
94.4269177717931,95.4246349353407,96.4223520988884,97.420069262436,98.4177864259836,
99.4155035895312,100.413220753079,101.410937916626,102.408655080174,103.406372243722,
104.404089407269,105.401806570817,106.399523734364,107.397240897912,108.39495806146,
109.392675225007,110.390392388555,111.388109552103,112.38582671565,113.383543879198,
114.381261042745,115.378978206293,116.376695369841,117.374412533388,118.372129696936,
119.369846860483,120.367564024031,121.365281187579,122.362998351126,123.360715514674,
124.358432678221,125.356149841769,126.353867005317,127.351584168864,128.349301332412,
129.34701849596,130.344735659507,131.342452823055,132.340169986602,133.33788715015,
134.335604313698,135.333321477245,136.331038640793,137.32875580434,138.326472967888,
139.324190131436,140.321907294983,141.319624458531,142.317341622078,143.315058785626,
144.312775949174,145.310493112721,146.308210276269,147.305927439816,148.303644603364,
149.301361766912,150.299078930459,151.296796094007,152.294513257555,153.292230421102,
154.28994758465,155.287664748197,156.285381911745,157.283099075293,158.28081623884,
159.278533402388,160.276250565935,161.273967729483,162.271684893031,163.269402056578,
164.267119220126,165.264836383673),.UNSPECIFIED.);
#366=B_SPLINE_SURFACE_WITH_KNOTS('',3,3,((#61760,#61761,#61762,#61763,#61764,
#61765,#61766,#61767,#61768,#61769,#61770,#61771,#61772,#61773,#61774,#61775,
#61776,#61777,#61778,#61779,#61780,#61781,#61782,#61783,#61784,#61785,#61786,
#61787,#61788,#61789,#61790,#61791,#61792,#61793,#61794,#61795,#61796,#61797,
#61798,#61799,#61800,#61801,#61802,#61803,#61804,#61805,#61806,#61807,#61808,
#61809,#61810,#61811,#61812,#61813,#61814,#61815,#61816,#61817,#61818,#61819,
#61820,#61821,#61822,#61823,#61824,#61825,#61826,#61827,#61828,#61829,#61830,
#61831,#61832,#61833,#61834,#61835,#61836,#61837,#61838,#61839,#61840,#61841,
#61842,#61843,#61844,#61845,#61846,#61847,#61848,#61849,#61850,#61851,#61852,
#61853,#61854,#61855,#61856,#61857,#61858,#61859,#61860,#61861,#61862,#61863,
#61864,#61865,#61866,#61867,#61868,#61869,#61870,#61871,#61872,#61873,#61874,
#61875,#61876,#61877,#61878,#61879,#61880,#61881,#61882,#61883,#61884,#61885,
#61886,#61887,#61888,#61889,#61890,#61891,#61892,#61893,#61894,#61895,#61896,
#61897,#61898,#61899,#61900,#61901,#61902,#61903,#61904,#61905,#61906,#61907,
#61908,#61909,#61910,#61911,#61912,#61913),(#61914,#61915,#61916,#61917,
#61918,#61919,#61920,#61921,#61922,#61923,#61924,#61925,#61926,#61927,#61928,
#61929,#61930,#61931,#61932,#61933,#61934,#61935,#61936,#61937,#61938,#61939,
#61940,#61941,#61942,#61943,#61944,#61945,#61946,#61947,#61948,#61949,#61950,
#61951,#61952,#61953,#61954,#61955,#61956,#61957,#61958,#61959,#61960,#61961,
#61962,#61963,#61964,#61965,#61966,#61967,#61968,#61969,#61970,#61971,#61972,
#61973,#61974,#61975,#61976,#61977,#61978,#61979,#61980,#61981,#61982,#61983,
#61984,#61985,#61986,#61987,#61988,#61989,#61990,#61991,#61992,#61993,#61994,
#61995,#61996,#61997,#61998,#61999,#62000,#62001,#62002,#62003,#62004,#62005,
#62006,#62007,#62008,#62009,#62010,#62011,#62012,#62013,#62014,#62015,#62016,
#62017,#62018,#62019,#62020,#62021,#62022,#62023,#62024,#62025,#62026,#62027,
#62028,#62029,#62030,#62031,#62032,#62033,#62034,#62035,#62036,#62037,#62038,
#62039,#62040,#62041,#62042,#62043,#62044,#62045,#62046,#62047,#62048,#62049,
#62050,#62051,#62052,#62053,#62054,#62055,#62056,#62057,#62058,#62059,#62060,
#62061,#62062,#62063,#62064,#62065,#62066,#62067),(#62068,#62069,#62070,
#62071,#62072,#62073,#62074,#62075,#62076,#62077,#62078,#62079,#62080,#62081,
#62082,#62083,#62084,#62085,#62086,#62087,#62088,#62089,#62090,#62091,#62092,
#62093,#62094,#62095,#62096,#62097,#62098,#62099,#62100,#62101,#62102,#62103,
#62104,#62105,#62106,#62107,#62108,#62109,#62110,#62111,#62112,#62113,#62114,
#62115,#62116,#62117,#62118,#62119,#62120,#62121,#62122,#62123,#62124,#62125,
#62126,#62127,#62128,#62129,#62130,#62131,#62132,#62133,#62134,#62135,#62136,
#62137,#62138,#62139,#62140,#62141,#62142,#62143,#62144,#62145,#62146,#62147,
#62148,#62149,#62150,#62151,#62152,#62153,#62154,#62155,#62156,#62157,#62158,
#62159,#62160,#62161,#62162,#62163,#62164,#62165,#62166,#62167,#62168,#62169,
#62170,#62171,#62172,#62173,#62174,#62175,#62176,#62177,#62178,#62179,#62180,
#62181,#62182,#62183,#62184,#62185,#62186,#62187,#62188,#62189,#62190,#62191,
#62192,#62193,#62194,#62195,#62196,#62197,#62198,#62199,#62200,#62201,#62202,
#62203,#62204,#62205,#62206,#62207,#62208,#62209,#62210,#62211,#62212,#62213,
#62214,#62215,#62216,#62217,#62218,#62219,#62220,#62221),(#62222,#62223,
#62224,#62225,#62226,#62227,#62228,#62229,#62230,#62231,#62232,#62233,#62234,
#62235,#62236,#62237,#62238,#62239,#62240,#62241,#62242,#62243,#62244,#62245,
#62246,#62247,#62248,#62249,#62250,#62251,#62252,#62253,#62254,#62255,#62256,
#62257,#62258,#62259,#62260,#62261,#62262,#62263,#62264,#62265,#62266,#62267,
#62268,#62269,#62270,#62271,#62272,#62273,#62274,#62275,#62276,#62277,#62278,
#62279,#62280,#62281,#62282,#62283,#62284,#62285,#62286,#62287,#62288,#62289,
#62290,#62291,#62292,#62293,#62294,#62295,#62296,#62297,#62298,#62299,#62300,
#62301,#62302,#62303,#62304,#62305,#62306,#62307,#62308,#62309,#62310,#62311,
#62312,#62313,#62314,#62315,#62316,#62317,#62318,#62319,#62320,#62321,#62322,
#62323,#62324,#62325,#62326,#62327,#62328,#62329,#62330,#62331,#62332,#62333,
#62334,#62335,#62336,#62337,#62338,#62339,#62340,#62341,#62342,#62343,#62344,
#62345,#62346,#62347,#62348,#62349,#62350,#62351,#62352,#62353,#62354,#62355,
#62356,#62357,#62358,#62359,#62360,#62361,#62362,#62363,#62364,#62365,#62366,
#62367,#62368,#62369,#62370,#62371,#62372,#62373,#62374,#62375)),
 .UNSPECIFIED.,.F.,.F.,.F.,(4,4),(4,1,1,1,1,1,1,1,1,1,1,1,1,1,1,1,1,1,1,
1,1,1,1,1,1,1,1,1,1,1,1,1,1,1,1,1,1,1,1,1,1,1,1,1,1,1,1,1,1,1,1,1,1,1,1,
1,1,1,1,1,1,1,1,1,1,1,1,1,1,1,1,1,1,1,1,1,1,1,1,1,1,1,1,1,1,1,1,1,1,1,1,
1,1,1,1,1,1,1,1,1,1,1,1,1,1,1,1,1,1,1,1,1,1,1,1,1,1,1,1,1,1,1,1,1,1,1,1,
1,1,1,1,1,1,1,1,1,1,1,1,1,1,1,1,1,1,1,1,1,1,1,1,4),(-0.000410693813861421,
0.0529897430905959),(8.30815772716268,9.30327942982552,10.2984011324884,
11.2935228351512,12.288644537814,13.2837662404769,14.2788879431397,15.2740096458026,
16.2691313484654,17.2642530511282,18.2593747537911,19.2544964564539,20.2496181591168,
21.2447398617796,22.2398615644424,23.2349832671053,24.2301049697681,25.225226672431,
26.2203483750938,27.2154700777567,28.2105917804195,29.2057134830823,30.2008351857452,
31.195956888408,32.1910785910709,33.1862002937337,34.1813219963965,35.1764436990594,
36.1715654017222,37.1666871043851,38.1618088070479,39.1569305097107,40.1520522123736,
41.1471739150364,42.1422956176993,43.1374173203621,44.132539023025,45.1276607256878,
46.1227824283506,47.1179041310135,48.1130258336763,49.1081475363392,50.103269239002,
51.0983909416648,52.0935126443277,53.0886343469905,54.0837560496534,55.0788777523162,
56.073999454979,57.0691211576419,58.0642428603047,59.0593645629676,60.0544862656304,
61.0496079682933,62.0447296709561,63.0398513736189,64.0349730762818,65.0300947789446,
66.0252164816075,67.0203381842703,68.0154598869331,69.010581589596,70.0057032922588,
71.0008249949217,71.9959466975845,72.9910684002473,73.9861901029102,74.981311805573,
75.9764335082359,76.9715552108987,77.9666769135615,78.9617986162244,79.9569203188872,
80.9520420215501,81.9471637242129,82.9422854268758,83.9374071295386,84.9325288322014,
85.9276505348643,86.9227722375271,87.91789394019,88.9130156428528,89.9081373455156,
90.9032590481785,91.8983807508413,92.8935024535042,93.888624156167,94.8837458588298,
95.8788675614927,96.8739892641555,97.8691109668184,98.8642326694812,99.859354372144,
100.854476074807,101.84959777747,102.844719480133,103.839841182795,104.834962885458,
105.830084588121,106.825206290784,107.820327993447,108.81544969611,109.810571398772,
110.805693101435,111.800814804098,112.795936506761,113.791058209424,114.786179912087,
115.781301614749,116.776423317412,117.771545020075,118.766666722738,119.761788425401,
120.756910128064,121.752031830727,122.747153533389,123.742275236052,124.737396938715,
125.732518641378,126.727640344041,127.722762046704,128.717883749366,129.713005452029,
130.708127154692,131.703248857355,132.698370560018,133.693492262681,134.688613965343,
135.683735668006,136.678857370669,137.673979073332,138.669100775995,139.664222478658,
140.659344181321,141.654465883983,142.649587586646,143.644709289309,144.639830991972,
145.634952694635,146.630074397298,147.62519609996,148.620317802623,149.615439505286,
150.610561207949,151.605682910612,152.600804613275,153.595926315937,154.5910480186,
155.586169721263,156.581291423926,157.576413126589,158.571945523066),
 .UNSPECIFIED.);
#367=B_SPLINE_SURFACE_WITH_KNOTS('',3,3,((#62563,#62564,#62565,#62566,#62567,
#62568,#62569,#62570,#62571,#62572,#62573,#62574,#62575,#62576,#62577,#62578,
#62579,#62580,#62581,#62582,#62583,#62584,#62585,#62586,#62587,#62588,#62589,
#62590,#62591,#62592,#62593,#62594,#62595,#62596,#62597,#62598,#62599,#62600,
#62601,#62602,#62603,#62604,#62605,#62606,#62607,#62608,#62609,#62610,#62611,
#62612,#62613,#62614,#62615,#62616,#62617,#62618,#62619,#62620,#62621,#62622,
#62623,#62624,#62625,#62626,#62627,#62628,#62629,#62630,#62631,#62632,#62633,
#62634,#62635,#62636,#62637,#62638,#62639,#62640,#62641,#62642,#62643,#62644,
#62645,#62646,#62647,#62648,#62649,#62650,#62651,#62652,#62653,#62654,#62655,
#62656,#62657,#62658,#62659,#62660,#62661,#62662,#62663,#62664,#62665,#62666,
#62667,#62668,#62669,#62670,#62671,#62672,#62673,#62674,#62675,#62676,#62677,
#62678,#62679,#62680,#62681,#62682,#62683,#62684,#62685,#62686,#62687,#62688,
#62689,#62690,#62691,#62692,#62693,#62694,#62695,#62696,#62697,#62698,#62699,
#62700,#62701,#62702,#62703,#62704,#62705,#62706,#62707,#62708,#62709,#62710,
#62711,#62712,#62713,#62714,#62715,#62716),(#62717,#62718,#62719,#62720,
#62721,#62722,#62723,#62724,#62725,#62726,#62727,#62728,#62729,#62730,#62731,
#62732,#62733,#62734,#62735,#62736,#62737,#62738,#62739,#62740,#62741,#62742,
#62743,#62744,#62745,#62746,#62747,#62748,#62749,#62750,#62751,#62752,#62753,
#62754,#62755,#62756,#62757,#62758,#62759,#62760,#62761,#62762,#62763,#62764,
#62765,#62766,#62767,#62768,#62769,#62770,#62771,#62772,#62773,#62774,#62775,
#62776,#62777,#62778,#62779,#62780,#62781,#62782,#62783,#62784,#62785,#62786,
#62787,#62788,#62789,#62790,#62791,#62792,#62793,#62794,#62795,#62796,#62797,
#62798,#62799,#62800,#62801,#62802,#62803,#62804,#62805,#62806,#62807,#62808,
#62809,#62810,#62811,#62812,#62813,#62814,#62815,#62816,#62817,#62818,#62819,
#62820,#62821,#62822,#62823,#62824,#62825,#62826,#62827,#62828,#62829,#62830,
#62831,#62832,#62833,#62834,#62835,#62836,#62837,#62838,#62839,#62840,#62841,
#62842,#62843,#62844,#62845,#62846,#62847,#62848,#62849,#62850,#62851,#62852,
#62853,#62854,#62855,#62856,#62857,#62858,#62859,#62860,#62861,#62862,#62863,
#62864,#62865,#62866,#62867,#62868,#62869,#62870),(#62871,#62872,#62873,
#62874,#62875,#62876,#62877,#62878,#62879,#62880,#62881,#62882,#62883,#62884,
#62885,#62886,#62887,#62888,#62889,#62890,#62891,#62892,#62893,#62894,#62895,
#62896,#62897,#62898,#62899,#62900,#62901,#62902,#62903,#62904,#62905,#62906,
#62907,#62908,#62909,#62910,#62911,#62912,#62913,#62914,#62915,#62916,#62917,
#62918,#62919,#62920,#62921,#62922,#62923,#62924,#62925,#62926,#62927,#62928,
#62929,#62930,#62931,#62932,#62933,#62934,#62935,#62936,#62937,#62938,#62939,
#62940,#62941,#62942,#62943,#62944,#62945,#62946,#62947,#62948,#62949,#62950,
#62951,#62952,#62953,#62954,#62955,#62956,#62957,#62958,#62959,#62960,#62961,
#62962,#62963,#62964,#62965,#62966,#62967,#62968,#62969,#62970,#62971,#62972,
#62973,#62974,#62975,#62976,#62977,#62978,#62979,#62980,#62981,#62982,#62983,
#62984,#62985,#62986,#62987,#62988,#62989,#62990,#62991,#62992,#62993,#62994,
#62995,#62996,#62997,#62998,#62999,#63000,#63001,#63002,#63003,#63004,#63005,
#63006,#63007,#63008,#63009,#63010,#63011,#63012,#63013,#63014,#63015,#63016,
#63017,#63018,#63019,#63020,#63021,#63022,#63023,#63024),(#63025,#63026,
#63027,#63028,#63029,#63030,#63031,#63032,#63033,#63034,#63035,#63036,#63037,
#63038,#63039,#63040,#63041,#63042,#63043,#63044,#63045,#63046,#63047,#63048,
#63049,#63050,#63051,#63052,#63053,#63054,#63055,#63056,#63057,#63058,#63059,
#63060,#63061,#63062,#63063,#63064,#63065,#63066,#63067,#63068,#63069,#63070,
#63071,#63072,#63073,#63074,#63075,#63076,#63077,#63078,#63079,#63080,#63081,
#63082,#63083,#63084,#63085,#63086,#63087,#63088,#63089,#63090,#63091,#63092,
#63093,#63094,#63095,#63096,#63097,#63098,#63099,#63100,#63101,#63102,#63103,
#63104,#63105,#63106,#63107,#63108,#63109,#63110,#63111,#63112,#63113,#63114,
#63115,#63116,#63117,#63118,#63119,#63120,#63121,#63122,#63123,#63124,#63125,
#63126,#63127,#63128,#63129,#63130,#63131,#63132,#63133,#63134,#63135,#63136,
#63137,#63138,#63139,#63140,#63141,#63142,#63143,#63144,#63145,#63146,#63147,
#63148,#63149,#63150,#63151,#63152,#63153,#63154,#63155,#63156,#63157,#63158,
#63159,#63160,#63161,#63162,#63163,#63164,#63165,#63166,#63167,#63168,#63169,
#63170,#63171,#63172,#63173,#63174,#63175,#63176,#63177,#63178)),
 .UNSPECIFIED.,.F.,.F.,.F.,(4,4),(4,1,1,1,1,1,1,1,1,1,1,1,1,1,1,1,1,1,1,
1,1,1,1,1,1,1,1,1,1,1,1,1,1,1,1,1,1,1,1,1,1,1,1,1,1,1,1,1,1,1,1,1,1,1,1,
1,1,1,1,1,1,1,1,1,1,1,1,1,1,1,1,1,1,1,1,1,1,1,1,1,1,1,1,1,1,1,1,1,1,1,1,
1,1,1,1,1,1,1,1,1,1,1,1,1,1,1,1,1,1,1,1,1,1,1,1,1,1,1,1,1,1,1,1,1,1,1,1,
1,1,1,1,1,1,1,1,1,1,1,1,1,1,1,1,1,1,1,1,1,1,1,1,4),(-0.000364258179702487,
0.0530361410367657),(11.6159825333414,12.6115149000043,13.6066366026672,
14.60175830533,15.5968800079929,16.5920017106557,17.5871234133185,18.5822451159814,
19.5773668186442,20.5724885213071,21.5676102239699,22.5627319266327,23.5578536292956,
24.5529753319584,25.5480970346213,26.5432187372841,27.5383404399469,28.5334621426098,
29.5285838452726,30.5237055479355,31.5188272505983,32.5139489532611,33.509070655924,
34.5041923585868,35.4993140612497,36.4944357639125,37.4895574665754,38.4846791692382,
39.479800871901,40.4749225745639,41.4700442772267,42.4651659798896,43.4602876825524,
44.4554093852152,45.4505310878781,46.4456527905409,47.4407744932038,48.4358961958666,
49.4310178985294,50.4261396011923,51.4212613038551,52.416383006518,53.4115047091808,
54.4066264118436,55.4017481145065,56.3968698171693,57.3919915198322,58.387113222495,
59.3822349251579,60.3773566278207,61.3724783304835,62.3676000331464,63.3627217358092,
64.3578434384721,65.3529651411349,66.3480868437977,67.3432085464606,68.3383302491234,
69.3334519517863,70.3285736544491,71.3236953571119,72.3188170597748,73.3139387624376,
74.3090604651005,75.3041821677633,76.2993038704262,77.294425573089,78.2895472757518,
79.2846689784147,80.2797906810775,81.2749123837404,82.2700340864032,83.265155789066,
84.2602774917289,85.2553991943917,86.2505208970546,87.2456425997174,88.2407643023802,
89.2358860050431,90.2310077077059,91.2261294103688,92.2212511130316,93.2163728156945,
94.2114945183573,95.2066162210201,96.201737923683,97.1968596263458,98.1919813290087,
99.1871030316715,100.182224734334,101.177346436997,102.17246813966,103.167589842323,
104.162711544986,105.157833247649,106.152954950311,107.148076652974,108.143198355637,
109.1383200583,110.133441760963,111.128563463626,112.123685166288,113.118806868951,
114.113928571614,115.109050274277,116.10417197694,117.099293679603,118.094415382265,
119.089537084928,120.084658787591,121.079780490254,122.074902192917,123.07002389558,
124.065145598243,125.060267300905,126.055389003568,127.050510706231,128.045632408894,
129.040754111557,130.03587581422,131.030997516882,132.026119219545,133.021240922208,
134.016362624871,135.011484327534,136.006606030197,137.001727732859,137.996849435522,
138.991971138185,139.987092840848,140.982214543511,141.977336246174,142.972457948837,
143.967579651499,144.962701354162,145.957823056825,146.952944759488,147.948066462151,
148.943188164814,149.938309867476,150.933431570139,151.928553272802,152.923674975465,
153.918796678128,154.913918380791,155.909040083453,156.904161786116,157.899283488779,
158.894405191442,159.889526894105,160.884648596768,161.87977029943),
 .UNSPECIFIED.);
#368=B_SPLINE_SURFACE_WITH_KNOTS('',3,3,((#70659,#70660,#70661,#70662,#70663,
#70664,#70665,#70666,#70667,#70668,#70669,#70670,#70671,#70672,#70673,#70674,
#70675,#70676,#70677,#70678,#70679,#70680,#70681,#70682,#70683,#70684,#70685,
#70686,#70687,#70688,#70689,#70690,#70691,#70692,#70693,#70694,#70695,#70696,
#70697,#70698,#70699,#70700,#70701,#70702,#70703,#70704,#70705,#70706,#70707,
#70708,#70709,#70710,#70711,#70712,#70713,#70714,#70715,#70716,#70717,#70718,
#70719,#70720,#70721,#70722,#70723,#70724,#70725,#70726),(#70727,#70728,
#70729,#70730,#70731,#70732,#70733,#70734,#70735,#70736,#70737,#70738,#70739,
#70740,#70741,#70742,#70743,#70744,#70745,#70746,#70747,#70748,#70749,#70750,
#70751,#70752,#70753,#70754,#70755,#70756,#70757,#70758,#70759,#70760,#70761,
#70762,#70763,#70764,#70765,#70766,#70767,#70768,#70769,#70770,#70771,#70772,
#70773,#70774,#70775,#70776,#70777,#70778,#70779,#70780,#70781,#70782,#70783,
#70784,#70785,#70786,#70787,#70788,#70789,#70790,#70791,#70792,#70793,#70794),
(#70795,#70796,#70797,#70798,#70799,#70800,#70801,#70802,#70803,#70804,
#70805,#70806,#70807,#70808,#70809,#70810,#70811,#70812,#70813,#70814,#70815,
#70816,#70817,#70818,#70819,#70820,#70821,#70822,#70823,#70824,#70825,#70826,
#70827,#70828,#70829,#70830,#70831,#70832,#70833,#70834,#70835,#70836,#70837,
#70838,#70839,#70840,#70841,#70842,#70843,#70844,#70845,#70846,#70847,#70848,
#70849,#70850,#70851,#70852,#70853,#70854,#70855,#70856,#70857,#70858,#70859,
#70860,#70861,#70862),(#70863,#70864,#70865,#70866,#70867,#70868,#70869,
#70870,#70871,#70872,#70873,#70874,#70875,#70876,#70877,#70878,#70879,#70880,
#70881,#70882,#70883,#70884,#70885,#70886,#70887,#70888,#70889,#70890,#70891,
#70892,#70893,#70894,#70895,#70896,#70897,#70898,#70899,#70900,#70901,#70902,
#70903,#70904,#70905,#70906,#70907,#70908,#70909,#70910,#70911,#70912,#70913,
#70914,#70915,#70916,#70917,#70918,#70919,#70920,#70921,#70922,#70923,#70924,
#70925,#70926,#70927,#70928,#70929,#70930)),.UNSPECIFIED.,.F.,.F.,.F.,(4,
4),(4,1,1,1,1,1,1,1,1,1,1,1,1,1,1,1,1,1,1,1,1,1,1,1,1,1,1,1,1,1,1,1,1,1,
1,1,1,1,1,1,1,1,1,1,1,1,1,1,1,1,1,1,1,1,1,1,1,1,1,1,1,1,1,1,1,4),(-0.000353530926813993,
0.0529178421063444),(13.6829908479658,14.6799027782905,15.6768147086152,
16.67372663894,17.6706385692647,18.6675504995894,19.6644624299141,20.6613743602388,
21.6582862905635,22.6551982208882,23.652110151213,24.6490220815377,25.6459340118624,
26.6428459421871,27.6397578725118,28.6366698028365,29.6335817331613,30.630493663486,
31.6274055938107,32.6243175241354,33.6212294544601,34.6181413847848,35.6150533151095,
36.6119652454343,37.608877175759,38.6057891060837,39.6027010364084,40.5996129667331,
41.5965248970578,42.5934368273825,43.5903487577073,44.587260688032,45.5841726183567,
46.5810845486814,47.5779964790061,48.5749084093308,49.5718203396556,50.5687322699803,
51.565644200305,52.5625561306297,53.5594680609544,54.5563799912791,55.5532919216039,
56.5502038519286,57.5471157822533,58.544027712578,59.5409396429027,60.5378515732274,
61.5347635035521,62.5316754338769,63.5285873642016,64.5254992945263,65.522411224851,
66.5193231551757,67.5162350855004,68.5131470158251,69.5100589461499,70.5069708764746,
71.5038828067993,72.500794737124,73.4977066674487,74.4946185977734,75.4915305280982,
76.4884424584229,77.4853543887476,78.4822663190723),.UNSPECIFIED.);
#369=B_SPLINE_SURFACE_WITH_KNOTS('',3,3,((#71108,#71109,#71110,#71111,#71112,
#71113,#71114,#71115,#71116,#71117,#71118,#71119,#71120,#71121,#71122,#71123,
#71124,#71125,#71126,#71127,#71128,#71129,#71130,#71131,#71132,#71133,#71134,
#71135,#71136,#71137,#71138,#71139,#71140,#71141,#71142,#71143,#71144,#71145,
#71146,#71147,#71148,#71149,#71150,#71151,#71152,#71153,#71154,#71155,#71156,
#71157,#71158,#71159,#71160,#71161,#71162,#71163,#71164,#71165,#71166,#71167,
#71168,#71169,#71170,#71171,#71172,#71173,#71174,#71175,#71176,#71177),
(#71178,#71179,#71180,#71181,#71182,#71183,#71184,#71185,#71186,#71187,
#71188,#71189,#71190,#71191,#71192,#71193,#71194,#71195,#71196,#71197,#71198,
#71199,#71200,#71201,#71202,#71203,#71204,#71205,#71206,#71207,#71208,#71209,
#71210,#71211,#71212,#71213,#71214,#71215,#71216,#71217,#71218,#71219,#71220,
#71221,#71222,#71223,#71224,#71225,#71226,#71227,#71228,#71229,#71230,#71231,
#71232,#71233,#71234,#71235,#71236,#71237,#71238,#71239,#71240,#71241,#71242,
#71243,#71244,#71245,#71246,#71247),(#71248,#71249,#71250,#71251,#71252,
#71253,#71254,#71255,#71256,#71257,#71258,#71259,#71260,#71261,#71262,#71263,
#71264,#71265,#71266,#71267,#71268,#71269,#71270,#71271,#71272,#71273,#71274,
#71275,#71276,#71277,#71278,#71279,#71280,#71281,#71282,#71283,#71284,#71285,
#71286,#71287,#71288,#71289,#71290,#71291,#71292,#71293,#71294,#71295,#71296,
#71297,#71298,#71299,#71300,#71301,#71302,#71303,#71304,#71305,#71306,#71307,
#71308,#71309,#71310,#71311,#71312,#71313,#71314,#71315,#71316,#71317),
(#71318,#71319,#71320,#71321,#71322,#71323,#71324,#71325,#71326,#71327,
#71328,#71329,#71330,#71331,#71332,#71333,#71334,#71335,#71336,#71337,#71338,
#71339,#71340,#71341,#71342,#71343,#71344,#71345,#71346,#71347,#71348,#71349,
#71350,#71351,#71352,#71353,#71354,#71355,#71356,#71357,#71358,#71359,#71360,
#71361,#71362,#71363,#71364,#71365,#71366,#71367,#71368,#71369,#71370,#71371,
#71372,#71373,#71374,#71375,#71376,#71377,#71378,#71379,#71380,#71381,#71382,
#71383,#71384,#71385,#71386,#71387)),.UNSPECIFIED.,.F.,.F.,.F.,(4,4),(4,
1,1,1,1,1,1,1,1,1,1,1,1,1,1,1,1,1,1,1,1,1,1,1,1,1,1,1,1,1,1,1,1,1,1,1,1,
1,1,1,1,1,1,1,1,1,1,1,1,1,1,1,1,1,1,1,1,1,1,1,1,1,1,1,1,1,1,4),(-0.000420248331794808,
0.0529960453941712),(8.30815772716266,9.30615583345715,10.3041539397516,
11.3021520460461,12.3001501523406,13.2981482586351,14.2961463649296,15.2941444712241,
16.2921425775186,17.2901406838131,18.2881387901076,19.286136896402,20.2841350026965,
21.282133108991,22.2801312152855,23.27812932158,24.2761274278745,25.274125534169,
26.2721236404635,27.270121746758,28.2681198530525,29.2661179593469,30.2641160656414,
31.2621141719359,32.2601122782304,33.2581103845249,34.2561084908194,35.2541065971139,
36.2521047034084,37.2501028097029,38.2481009159974,39.2460990222918,40.2440971285863,
41.2420952348808,42.2400933411753,43.2380914474698,44.2360895537643,45.2340876600588,
46.2320857663533,47.2300838726478,48.2280819789423,49.2260800852367,50.2240781915312,
51.2220762978257,52.2200744041202,53.2180725104147,54.2160706167092,55.2140687230037,
56.2120668292982,57.2100649355927,58.2080630418872,59.2060611481816,60.2040592544761,
61.2020573607706,62.2000554670651,63.1980535733596,64.1960516796541,65.1940497859486,
66.1920478922431,67.1900459985376,68.188044104832,69.1860422111265,70.184040317421,
71.1820384237155,72.18003653001,73.1780346363045,74.176032742599,75.1744510972253),
 .UNSPECIFIED.);
#370=B_SPLINE_SURFACE_WITH_KNOTS('',3,3,((#80001,#80002,#80003,#80004,#80005,
#80006,#80007,#80008,#80009,#80010,#80011,#80012,#80013,#80014,#80015,#80016,
#80017,#80018,#80019,#80020,#80021,#80022,#80023,#80024,#80025,#80026,#80027,
#80028,#80029,#80030,#80031,#80032,#80033,#80034,#80035,#80036,#80037,#80038,
#80039,#80040,#80041,#80042,#80043,#80044,#80045,#80046,#80047,#80048,#80049,
#80050,#80051,#80052,#80053,#80054,#80055,#80056,#80057,#80058,#80059,#80060,
#80061,#80062,#80063,#80064,#80065,#80066,#80067,#80068,#80069,#80070,#80071,
#80072,#80073,#80074,#80075,#80076,#80077,#80078,#80079,#80080,#80081,#80082,
#80083,#80084),(#80085,#80086,#80087,#80088,#80089,#80090,#80091,#80092,
#80093,#80094,#80095,#80096,#80097,#80098,#80099,#80100,#80101,#80102,#80103,
#80104,#80105,#80106,#80107,#80108,#80109,#80110,#80111,#80112,#80113,#80114,
#80115,#80116,#80117,#80118,#80119,#80120,#80121,#80122,#80123,#80124,#80125,
#80126,#80127,#80128,#80129,#80130,#80131,#80132,#80133,#80134,#80135,#80136,
#80137,#80138,#80139,#80140,#80141,#80142,#80143,#80144,#80145,#80146,#80147,
#80148,#80149,#80150,#80151,#80152,#80153,#80154,#80155,#80156,#80157,#80158,
#80159,#80160,#80161,#80162,#80163,#80164,#80165,#80166,#80167,#80168),
(#80169,#80170,#80171,#80172,#80173,#80174,#80175,#80176,#80177,#80178,
#80179,#80180,#80181,#80182,#80183,#80184,#80185,#80186,#80187,#80188,#80189,
#80190,#80191,#80192,#80193,#80194,#80195,#80196,#80197,#80198,#80199,#80200,
#80201,#80202,#80203,#80204,#80205,#80206,#80207,#80208,#80209,#80210,#80211,
#80212,#80213,#80214,#80215,#80216,#80217,#80218,#80219,#80220,#80221,#80222,
#80223,#80224,#80225,#80226,#80227,#80228,#80229,#80230,#80231,#80232,#80233,
#80234,#80235,#80236,#80237,#80238,#80239,#80240,#80241,#80242,#80243,#80244,
#80245,#80246,#80247,#80248,#80249,#80250,#80251,#80252),(#80253,#80254,
#80255,#80256,#80257,#80258,#80259,#80260,#80261,#80262,#80263,#80264,#80265,
#80266,#80267,#80268,#80269,#80270,#80271,#80272,#80273,#80274,#80275,#80276,
#80277,#80278,#80279,#80280,#80281,#80282,#80283,#80284,#80285,#80286,#80287,
#80288,#80289,#80290,#80291,#80292,#80293,#80294,#80295,#80296,#80297,#80298,
#80299,#80300,#80301,#80302,#80303,#80304,#80305,#80306,#80307,#80308,#80309,
#80310,#80311,#80312,#80313,#80314,#80315,#80316,#80317,#80318,#80319,#80320,
#80321,#80322,#80323,#80324,#80325,#80326,#80327,#80328,#80329,#80330,#80331,
#80332,#80333,#80334,#80335,#80336)),.UNSPECIFIED.,.F.,.F.,.F.,(4,4),(4,
1,1,1,1,1,1,1,1,1,1,1,1,1,1,1,1,1,1,1,1,1,1,1,1,1,1,1,1,1,1,1,1,1,1,1,1,
1,1,1,1,1,1,1,1,1,1,1,1,1,1,1,1,1,1,1,1,1,1,1,1,1,1,1,1,1,1,1,1,1,1,1,1,
1,1,1,1,1,1,1,1,4),(-0.000243720225400152,0.0332111771674427),(8.30203615430888,
9.29159561709456,10.2811550798802,11.2707145426659,12.2602740054516,13.2498334682373,
14.2393929310229,15.2289523938086,16.2185118565943,17.20807131938,18.1976307821657,
19.1871902449513,20.176749707737,21.1663091705227,22.1558686333084,23.145428096094,
24.1349875588797,25.1245470216654,26.1141064844511,27.1036659472367,28.0932254100224,
29.0827848728081,30.0723443355938,31.0619037983795,32.0514632611651,33.0410227239508,
34.0305821867365,35.0201416495222,36.0097011123078,36.9992605750935,37.9888200378792,
38.9783795006649,39.9679389634505,40.9574984262362,41.9470578890219,42.9366173518076,
43.9261768145933,44.9157362773789,45.9052957401646,46.8948552029503,47.884414665736,
48.8739741285216,49.8635335913073,50.853093054093,51.8426525168787,52.8322119796644,
53.82177144245,54.8113309052357,55.8008903680214,56.7904498308071,57.7800092935927,
58.7695687563784,59.7591282191641,60.7486876819498,61.7382471447354,62.7278066075211,
63.7173660703068,64.7069255330925,65.6964849958782,66.6860444586638,67.6756039214495,
68.6651633842352,69.6547228470209,70.6442823098065,71.6338417725922,72.6234012353779,
73.6129606981636,74.6025201609492,75.5920796237349,76.5816390865206,77.5711985493063,
78.560758012092,79.5503174748776,80.5398769376633,81.529436400449,82.5189958632347,
83.5085553260203,84.498114788806,85.4876742515917,86.4772337143774,87.466793177163,
88.4565963601741),.UNSPECIFIED.);
#371=B_SPLINE_SURFACE_WITH_KNOTS('',3,3,((#80552,#80553,#80554,#80555,#80556,
#80557,#80558,#80559,#80560,#80561,#80562,#80563,#80564,#80565,#80566,#80567,
#80568,#80569,#80570,#80571,#80572,#80573,#80574,#80575,#80576,#80577,#80578,
#80579,#80580,#80581,#80582,#80583,#80584,#80585,#80586,#80587,#80588,#80589,
#80590,#80591,#80592,#80593,#80594,#80595,#80596,#80597,#80598,#80599,#80600,
#80601,#80602,#80603,#80604,#80605,#80606,#80607,#80608,#80609,#80610,#80611,
#80612,#80613,#80614,#80615,#80616,#80617,#80618,#80619,#80620,#80621,#80622,
#80623,#80624,#80625,#80626,#80627,#80628,#80629,#80630,#80631,#80632,#80633),
(#80634,#80635,#80636,#80637,#80638,#80639,#80640,#80641,#80642,#80643,
#80644,#80645,#80646,#80647,#80648,#80649,#80650,#80651,#80652,#80653,#80654,
#80655,#80656,#80657,#80658,#80659,#80660,#80661,#80662,#80663,#80664,#80665,
#80666,#80667,#80668,#80669,#80670,#80671,#80672,#80673,#80674,#80675,#80676,
#80677,#80678,#80679,#80680,#80681,#80682,#80683,#80684,#80685,#80686,#80687,
#80688,#80689,#80690,#80691,#80692,#80693,#80694,#80695,#80696,#80697,#80698,
#80699,#80700,#80701,#80702,#80703,#80704,#80705,#80706,#80707,#80708,#80709,
#80710,#80711,#80712,#80713,#80714,#80715),(#80716,#80717,#80718,#80719,
#80720,#80721,#80722,#80723,#80724,#80725,#80726,#80727,#80728,#80729,#80730,
#80731,#80732,#80733,#80734,#80735,#80736,#80737,#80738,#80739,#80740,#80741,
#80742,#80743,#80744,#80745,#80746,#80747,#80748,#80749,#80750,#80751,#80752,
#80753,#80754,#80755,#80756,#80757,#80758,#80759,#80760,#80761,#80762,#80763,
#80764,#80765,#80766,#80767,#80768,#80769,#80770,#80771,#80772,#80773,#80774,
#80775,#80776,#80777,#80778,#80779,#80780,#80781,#80782,#80783,#80784,#80785,
#80786,#80787,#80788,#80789,#80790,#80791,#80792,#80793,#80794,#80795,#80796,
#80797),(#80798,#80799,#80800,#80801,#80802,#80803,#80804,#80805,#80806,
#80807,#80808,#80809,#80810,#80811,#80812,#80813,#80814,#80815,#80816,#80817,
#80818,#80819,#80820,#80821,#80822,#80823,#80824,#80825,#80826,#80827,#80828,
#80829,#80830,#80831,#80832,#80833,#80834,#80835,#80836,#80837,#80838,#80839,
#80840,#80841,#80842,#80843,#80844,#80845,#80846,#80847,#80848,#80849,#80850,
#80851,#80852,#80853,#80854,#80855,#80856,#80857,#80858,#80859,#80860,#80861,
#80862,#80863,#80864,#80865,#80866,#80867,#80868,#80869,#80870,#80871,#80872,
#80873,#80874,#80875,#80876,#80877,#80878,#80879)),.UNSPECIFIED.,.F.,.F.,
 .F.,(4,4),(4,1,1,1,1,1,1,1,1,1,1,1,1,1,1,1,1,1,1,1,1,1,1,1,1,1,1,1,1,1,
1,1,1,1,1,1,1,1,1,1,1,1,1,1,1,1,1,1,1,1,1,1,1,1,1,1,1,1,1,1,1,1,1,1,1,1,
1,1,1,1,1,1,1,1,1,1,1,1,1,4),(-0.000214583729420464,0.0331596015900255),
(13.6891124208198,14.6774813298366,15.6658502388533,16.65421914787,17.6425880568867,
18.6309569659034,19.6193258749201,20.6076947839369,21.5960636929536,22.5844326019703,
23.572801510987,24.5611704200037,25.5495393290204,26.5379082380372,27.5262771470539,
28.5146460560706,29.5030149650873,30.491383874104,31.4797527831207,32.4681216921375,
33.4564906011542,34.4448595101709,35.4332284191876,36.4215973282043,37.409966237221,
38.3983351462378,39.3867040552545,40.3750729642712,41.3634418732879,42.3518107823046,
43.3401796913213,44.3285486003381,45.3169175093548,46.3052864183715,47.2936553273882,
48.2820242364049,49.2703931454216,50.2587620544383,51.2471309634551,52.2354998724718,
53.2238687814885,54.2122376905052,55.2006065995219,56.1889755085386,57.1773444175554,
58.1657133265721,59.1540822355888,60.1424511446055,61.1308200536222,62.119188962639,
63.1075578716557,64.0959267806724,65.0842956896891,66.0726645987058,67.0610335077225,
68.0494024167392,69.037771325756,70.0261402347727,71.0145091437894,72.0028780528061,
72.9912469618228,73.9796158708395,74.9679847798563,75.956353688873,76.9447225978897,
77.9330915069064,78.9214604159231,79.9098293249398,80.8981982339565,81.8865671429733,
82.87493605199,83.8633049610067,84.8516738700234,85.8400427790401,86.8284116880568,
87.8167805970736,88.8051495060903,89.793518415107,90.7818873241237,91.7702562331404),
 .UNSPECIFIED.);
#372=ELLIPSE('',#15639,3.6062445840514,2.55000000000001);
#373=ELLIPSE('',#15641,3.6062445840514,2.55000000000001);
#374=ELLIPSE('',#15643,3.6062445840514,2.55000000000001);
#375=ELLIPSE('',#15645,3.6062445840514,2.55000000000001);
#376=ELLIPSE('',#15651,3.6062445840514,2.55000000000001);
#377=ELLIPSE('',#15653,3.6062445840514,2.55000000000001);
#378=ELLIPSE('',#15655,3.6062445840514,2.55000000000001);
#379=ELLIPSE('',#15657,3.6062445840514,2.55000000000001);
#380=ELLIPSE('',#15663,3.60624458405139,2.55);
#381=ELLIPSE('',#15665,3.60624458405139,2.55);
#382=ELLIPSE('',#15667,3.60624458405139,2.55);
#383=ELLIPSE('',#15669,3.60624458405139,2.55);
#384=ELLIPSE('',#15733,3.60624458405138,2.54999999999999);
#385=ELLIPSE('',#15735,3.60624458405138,2.54999999999999);
#386=ELLIPSE('',#15737,3.60624458405138,2.54999999999999);
#387=ELLIPSE('',#15739,3.60624458405138,2.54999999999999);
#388=ELLIPSE('',#15745,3.60624458405139,2.55);
#389=ELLIPSE('',#15747,3.60624458405139,2.55);
#390=ELLIPSE('',#15749,3.60624458405139,2.55);
#391=ELLIPSE('',#15751,3.60624458405139,2.55);
#392=ELLIPSE('',#15757,3.60624458405141,2.55000000000001);
#393=ELLIPSE('',#15759,3.60624458405141,2.55000000000001);
#394=ELLIPSE('',#15761,3.6062445840514,2.55000000000001);
#395=ELLIPSE('',#15763,3.6062445840514,2.55000000000001);
#396=ELLIPSE('',#15769,3.60624458405141,2.55000000000001);
#397=ELLIPSE('',#15771,3.60624458405141,2.55000000000001);
#398=ELLIPSE('',#15773,3.6062445840514,2.55000000000001);
#399=ELLIPSE('',#15775,3.6062445840514,2.55000000000001);
#400=ELLIPSE('',#16473,1.70248048578179,1.37104286127159);
#401=ELLIPSE('',#16476,1.73906534450511,1.41773226323344);
#402=B_SPLINE_CURVE_WITH_KNOTS('',3,(#20931,#20932,#20933,#20934,#20935,
#20936),.UNSPECIFIED.,.F.,.F.,(4,2,4),(1.66095691430957,1.73342009736541,
1.80588328042126),.UNSPECIFIED.);
#403=B_SPLINE_CURVE_WITH_KNOTS('',3,(#20957,#20958,#20959,#20960,#20961,
#20962),.UNSPECIFIED.,.F.,.F.,(4,2,4),(1.66095691430954,1.73342009736538,
1.80588328042123),.UNSPECIFIED.);
#404=B_SPLINE_CURVE_WITH_KNOTS('',3,(#20983,#20984,#20985,#20986,#20987,
#20988),.UNSPECIFIED.,.F.,.F.,(4,2,4),(1.66095691430954,1.73342009736541,
1.80588328042128),.UNSPECIFIED.);
#405=B_SPLINE_CURVE_WITH_KNOTS('',3,(#21051,#21052,#21053,#21054,#21055,
#21056),.UNSPECIFIED.,.F.,.F.,(4,2,4),(1.66095691430955,1.73342009736539,
1.80588328042123),.UNSPECIFIED.);
#406=B_SPLINE_CURVE_WITH_KNOTS('',3,(#21077,#21078,#21079,#21080,#21081,
#21082),.UNSPECIFIED.,.F.,.F.,(4,2,4),(1.66095691430953,1.73342009736537,
1.80588328042121),.UNSPECIFIED.);
#407=B_SPLINE_CURVE_WITH_KNOTS('',3,(#21103,#21104,#21105,#21106,#21107,
#21108),.UNSPECIFIED.,.F.,.F.,(4,2,4),(1.66095691430952,1.73342009736539,
1.80588328042126),.UNSPECIFIED.);
#408=B_SPLINE_CURVE_WITH_KNOTS('',3,(#23040,#23041,#23042,#23043,#23044,
#23045,#23046,#23047,#23048,#23049,#23050,#23051,#23052,#23053,#23054,#23055,
#23056,#23057,#23058,#23059,#23060,#23061,#23062,#23063,#23064,#23065,#23066,
#23067,#23068,#23069,#23070,#23071,#23072,#23073,#23074,#23075,#23076,#23077,
#23078,#23079,#23080,#23081,#23082,#23083,#23084,#23085,#23086,#23087,#23088,
#23089,#23090,#23091,#23092,#23093,#23094,#23095,#23096,#23097,#23098,#23099,
#23100,#23101,#23102,#23103,#23104,#23105,#23106,#23107,#23108,#23109,#23110,
#23111,#23112,#23113,#23114,#23115,#23116,#23117,#23118,#23119,#23120,#23121,
#23122,#23123,#23124,#23125,#23126,#23127,#23128,#23129,#23130,#23131,#23132,
#23133,#23134,#23135,#23136,#23137,#23138,#23139,#23140,#23141,#23142,#23143,
#23144,#23145,#23146,#23147,#23148,#23149,#23150,#23151,#23152,#23153,#23154,
#23155,#23156,#23157,#23158,#23159,#23160,#23161,#23162,#23163,#23164,#23165,
#23166,#23167,#23168,#23169,#23170,#23171,#23172,#23173,#23174,#23175,#23176,
#23177,#23178,#23179,#23180,#23181,#23182,#23183,#23184,#23185,#23186,#23187,
#23188,#23189,#23190,#23191,#23192,#23193,#23194,#23195,#23196,#23197),
 .UNSPECIFIED.,.F.,.F.,(4,2,2,2,2,2,2,2,2,2,2,2,2,2,2,2,2,2,2,2,2,2,2,2,
2,2,2,2,2,2,2,2,2,2,2,2,2,2,2,2,2,2,2,2,2,2,2,2,2,2,2,2,2,2,2,2,2,2,2,2,
2,2,2,2,2,2,2,2,2,2,2,2,2,2,2,2,2,2,4),(-0.736675210638058,-0.733821596808743,
-0.694292033914328,-0.689636306082269,-0.686738441869285,-0.684478224512377,
-0.68197459732431,-0.677843159020972,-0.662315926433236,-0.609673816667036,
-0.60542480610492,-0.590249017300808,-0.587646734993429,-0.58603249381003,
-0.584775927897407,-0.583320803513858,-0.580700810859027,-0.567619048230907,
-0.498749414458695,-0.490687875993121,-0.487355526501576,-0.485269466399629,
-0.482983111861107,-0.47981466001079,-0.472190340759041,-0.461503343415649,
-0.402687458406344,-0.390008334220899,-0.387544858158691,-0.385977168728162,
-0.38472244088543,-0.383223865036566,-0.380442637090082,-0.364403892819621,
-0.310894446169308,-0.293090695693202,-0.288631625129639,-0.286024966281755,
-0.283770737027648,-0.281009047858853,-0.27569948623136,-0.268986738050613,
-0.253669224173961,-0.215639415702403,-0.191097914207698,-0.187984675517241,
-0.186403617887784,-0.185150735660367,-0.185140371720751,-0.185130377235419,
-0.185120735762252,-0.185111431649632,-0.185102450266112,-0.185093777770031,
-0.185085401014474,-0.185077307521438,-0.185069485549634,-0.185061923946848,
-0.185054612044751,-0.185047539936342,-0.1850406980958,-0.185032579111707,
-0.185024517471098,-0.185016512188063,-0.185008562278368,-0.185000666664865,
-0.184992824418986,-0.183459446820892,-0.180515474988828,-0.161220776772221,
-0.119046916699663,-0.0967044542819805,-0.0923424843568188,-0.0895154180428306,
-0.087237298885081,-0.0846349927311359,-0.0801453807302738,-0.0602832274206637,
-0.00330615950253142),.UNSPECIFIED.);
#409=B_SPLINE_CURVE_WITH_KNOTS('',3,(#23200,#23201,#23202,#23203,#23204,
#23205,#23206,#23207,#23208,#23209,#23210,#23211,#23212,#23213,#23214,#23215,
#23216,#23217,#23218,#23219,#23220,#23221,#23222,#23223,#23224,#23225,#23226,
#23227,#23228,#23229,#23230,#23231,#23232,#23233,#23234,#23235,#23236,#23237,
#23238,#23239,#23240,#23241,#23242,#23243,#23244,#23245,#23246,#23247,#23248,
#23249,#23250,#23251,#23252,#23253,#23254,#23255,#23256,#23257,#23258,#23259,
#23260,#23261,#23262,#23263,#23264,#23265,#23266,#23267,#23268,#23269,#23270,
#23271,#23272,#23273,#23274,#23275),.UNSPECIFIED.,.F.,.F.,(4,3,3,3,3,3,
3,3,3,3,3,3,3,3,3,3,3,3,3,3,3,3,3,3,3,4),(11.6163931973415,11.7237492295633,
11.835044370979,11.9423196466468,12.049596139851,12.156902775469,12.2642685060456,
12.371800331433,12.4794284226994,12.5872559860832,12.6141103608891,12.7180831030621,
12.8218829433769,12.9255411761381,13.0291226045906,13.1326641607794,13.2362027194087,
13.3398462288228,13.4435459699825,13.5474312704339,13.6118275244367,13.7169098947458,
13.8218092643123,13.9266035018259,14.0313222763496,14.054777935193),
 .UNSPECIFIED.);
#410=B_SPLINE_CURVE_WITH_KNOTS('',3,(#23280,#23281,#23282,#23283,#23284,
#23285,#23286,#23287,#23288,#23289,#23290,#23291,#23292,#23293,#23294,#23295,
#23296,#23297,#23298,#23299,#23300,#23301,#23302,#23303,#23304,#23305,#23306,
#23307,#23308,#23309,#23310,#23311,#23312,#23313,#23314,#23315,#23316,#23317,
#23318,#23319,#23320,#23321,#23322,#23323,#23324,#23325,#23326,#23327,#23328,
#23329,#23330,#23331,#23332,#23333,#23334,#23335,#23336,#23337,#23338,#23339,
#23340,#23341,#23342,#23343,#23344,#23345,#23346,#23347,#23348,#23349,#23350,
#23351,#23352,#23353,#23354,#23355,#23356,#23357,#23358,#23359,#23360,#23361,
#23362,#23363,#23364,#23365,#23366,#23367,#23368,#23369,#23370,#23371,#23372,
#23373,#23374,#23375,#23376,#23377,#23378,#23379,#23380,#23381,#23382,#23383,
#23384,#23385,#23386,#23387,#23388,#23389,#23390,#23391,#23392,#23393,#23394,
#23395,#23396,#23397,#23398,#23399,#23400,#23401,#23402,#23403,#23404,#23405,
#23406,#23407,#23408,#23409,#23410,#23411,#23412,#23413,#23414,#23415,#23416,
#23417,#23418,#23419,#23420,#23421,#23422,#23423,#23424,#23425,#23426,#23427,
#23428,#23429,#23430,#23431,#23432,#23433,#23434,#23435,#23436,#23437,#23438,
#23439,#23440,#23441,#23442,#23443,#23444,#23445,#23446,#23447,#23448,#23449,
#23450,#23451,#23452,#23453,#23454,#23455,#23456,#23457,#23458,#23459,#23460,
#23461,#23462,#23463,#23464,#23465,#23466,#23467,#23468,#23469,#23470,#23471,
#23472,#23473,#23474,#23475,#23476,#23477,#23478,#23479,#23480,#23481,#23482,
#23483,#23484,#23485,#23486,#23487,#23488,#23489,#23490,#23491,#23492,#23493,
#23494,#23495,#23496,#23497,#23498,#23499,#23500,#23501),.UNSPECIFIED.,
 .F.,.F.,(4,2,2,2,2,2,2,2,2,2,2,2,2,2,2,2,2,2,2,2,2,2,2,2,2,2,2,2,2,2,2,
2,2,2,2,2,2,2,2,2,2,2,2,2,2,2,2,2,2,2,2,2,2,2,2,2,2,2,2,2,2,2,2,2,2,2,2,
2,2,2,2,2,2,2,2,2,2,2,2,2,2,2,2,2,2,2,2,2,2,2,2,2,2,2,2,2,2,2,2,2,2,2,2,
2,2,2,2,2,2,2,4),(-1.99319254965038,-1.98653737002634,-1.98379876219187,
-1.98231127336989,-1.98105390575671,-1.97946774020603,-1.97695764114924,
-1.96358609747753,-1.95947365261895,-1.91009979267965,-1.88997447752518,
-1.8855124399241,-1.88293983892923,-1.88069627497894,-1.87792368335606,
-1.87366964594137,-1.85263256574772,-1.80271668913237,-1.79220829787831,
-1.7878977864728,-1.78462777973597,-1.78303063756752,-1.78177262317214,
-1.78029379898174,-1.77766847778042,-1.76624504842418,-1.72805574524784,
-1.69152579643256,-1.68645760565609,-1.68375522131271,-1.68173376564286,
-1.67918575318431,-1.67483532908617,-1.65877935779111,-1.6037048732393,
-1.58756341620945,-1.5847825791044,-1.583286052845,-1.58202929210908,-1.58045430170204,
-1.57798093406084,-1.56527370394193,-1.55688098194784,-1.50556565384859,
-1.49022978933833,-1.48612066592295,-1.48362540409227,-1.48136947813647,
-1.47847265369504,-1.47380975113612,-1.44015465221223,-1.41430436279017,
-1.3907709908021,-1.38618570486933,-1.38435473181944,-1.383063591166,-1.38186692765178,
-1.38018734647392,-1.37572966665698,-1.33404109191877,-1.29299639046651,
-1.28762830059024,-1.28486300891597,-1.28261920610225,-1.28003953442239,
-1.27566305997605,-1.25870238180554,-1.20068310336964,-1.18819100667183,
-1.18559107374171,-1.18413335063411,-1.18287330707974,-1.18124711843356,
-1.17860182329707,-1.16243375888946,-1.10376929772002,-1.09093020651619,
-1.08691406550062,-1.08444070426442,-1.08218190750236,-1.07924926338534,
-1.07302093646664,-1.03972953816717,-1.0098835930594,-1.00216406863422,
-0.988916655393418,-0.986414427156384,-0.984831290152103,-0.983574602856247,
-0.982085784279071,-0.979340969979418,-0.964033763220833,-0.917227233395081,
-0.892981609427976,-0.888570353940284,-0.885748892048188,-0.883500284903431,
-0.880958973937785,-0.876643557614502,-0.858725039011845,-0.8120316403843,
-0.810317698066935,-0.80146037094138,-0.789266527434246,-0.786821851193486,
-0.785254625932403,-0.783995157677338,-0.782484136198523,-0.779651271266861,
-0.762365581868955,-0.736675210638058),.UNSPECIFIED.);
#411=B_SPLINE_CURVE_WITH_KNOTS('',3,(#23503,#23504,#23505,#23506,#23507,
#23508,#23509,#23510,#23511,#23512,#23513,#23514,#23515,#23516,#23517,#23518,
#23519,#23520,#23521,#23522,#23523,#23524,#23525,#23526,#23527,#23528,#23529,
#23530,#23531,#23532,#23533,#23534,#23535,#23536,#23537,#23538,#23539,#23540,
#23541,#23542,#23543,#23544,#23545,#23546,#23547,#23548,#23549,#23550,#23551,
#23552,#23553,#23554),.UNSPECIFIED.,.F.,.F.,(4,3,3,3,3,3,3,3,3,3,3,3,3,
3,3,3,3,4),(14.054777935193,14.1594700099767,14.2641741224379,14.3689912503651,
14.4738754371146,14.5789317449399,14.6095446879844,14.7146790594763,14.8196597064566,
14.9245217842077,15.0293208169872,15.1340920802013,15.2388708079724,15.3437622025241,
15.4487162544608,15.5538525389373,15.607261851532,15.707963267949),
 .UNSPECIFIED.);
#412=B_SPLINE_CURVE_WITH_KNOTS('',3,(#23555,#23556,#23557,#23558,#23559,
#23560,#23561,#23562,#23563,#23564,#23565,#23566,#23567,#23568,#23569,#23570,
#23571,#23572,#23573,#23574,#23575,#23576,#23577,#23578,#23579,#23580,#23581,
#23582,#23583,#23584,#23585,#23586,#23587,#23588,#23589,#23590,#23591,#23592,
#23593,#23594,#23595,#23596,#23597,#23598,#23599,#23600,#23601,#23602,#23603,
#23604,#23605,#23606,#23607,#23608,#23609,#23610,#23611,#23612,#23613,#23614,
#23615,#23616,#23617,#23618,#23619,#23620,#23621,#23622,#23623,#23624,#23625,
#23626,#23627,#23628,#23629,#23630,#23631,#23632,#23633,#23634,#23635,#23636,
#23637,#23638,#23639,#23640,#23641,#23642,#23643,#23644,#23645,#23646,#23647,
#23648,#23649,#23650,#23651,#23652,#23653,#23654,#23655,#23656,#23657,#23658,
#23659,#23660,#23661,#23662,#23663,#23664,#23665,#23666,#23667,#23668,#23669,
#23670,#23671,#23672,#23673,#23674,#23675,#23676,#23677,#23678,#23679,#23680,
#23681,#23682,#23683,#23684,#23685,#23686,#23687,#23688,#23689,#23690,#23691,
#23692,#23693,#23694,#23695,#23696,#23697,#23698,#23699,#23700,#23701,#23702,
#23703,#23704,#23705,#23706,#23707,#23708,#23709,#23710,#23711,#23712,#23713,
#23714),.UNSPECIFIED.,.F.,.F.,(4,2,2,2,2,2,2,2,2,2,2,2,2,2,2,2,2,2,2,2,
2,2,2,2,2,2,2,2,2,2,2,2,2,2,2,2,2,2,2,2,2,2,2,2,2,2,2,2,2,2,2,2,2,2,2,2,
2,2,2,2,2,2,2,2,2,2,2,2,2,2,2,2,2,2,2,2,2,2,2,4),(-2.51428340140175,-2.5075761767229,
-2.45683770840886,-2.44694558480235,-2.43976138139802,-2.43666717087808,
-2.43439424280313,-2.43229232245576,-2.42942596561606,-2.42222426557208,
-2.37875002873089,-2.35254832993181,-2.34360277058353,-2.33975515706998,
-2.33763316598838,-2.33579391733833,-2.33452171846559,-2.33334371170081,
-2.33142428110962,-2.32662747627728,-2.29536552386702,-2.26894776642379,
-2.24547788033084,-2.23934453969068,-2.23642506127349,-2.23416264487136,
-2.23167141480239,-2.22759445232846,-2.21427158911533,-2.1564453148252,
-2.14010421221288,-2.13730832658454,-2.13580526270536,-2.13454558661861,
-2.13296942338265,-2.12990975131705,-2.10887285789977,-2.05788040819895,
-2.04275310843614,-2.03866156407082,-2.03616971049145,-2.03391216218611,
-2.03100666744326,-2.02631629293022,-1.98971337666585,-1.95395538417286,
-1.94029352616069,-1.93762888225658,-1.93615744135929,-1.93489938813596,
-1.93329387424094,-1.93071738003684,-1.9161173043658,-1.8943178333712,-1.86074202471722,
-1.84349754275835,-1.83923594398317,-1.83670871473161,-1.83446173565513,
-1.83162783997351,-1.82716877083037,-1.8015579920678,-1.76511576577924,
-1.74342876761541,-1.73902692727964,-1.73722685757312,-1.73594237209019,
-1.73457089489806,-1.7323601738389,-1.72554131716868,-1.68365381660965,
-1.66232755257428,-1.64407877699645,-1.63974031220367,-1.63719430830286,
-1.63494695966009,-1.63213425033871,-1.62775052475623,-1.60421127678611,
-1.58825468741526),.UNSPECIFIED.);
#413=B_SPLINE_CURVE_WITH_KNOTS('',3,(#23720,#23721,#23722,#23723,#23724,
#23725,#23726,#23727,#23728,#23729,#23730,#23731,#23732,#23733,#23734,#23735,
#23736,#23737,#23738,#23739,#23740,#23741,#23742,#23743,#23744,#23745,#23746,
#23747,#23748,#23749,#23750,#23751,#23752,#23753,#23754,#23755,#23756,#23757,
#23758,#23759,#23760,#23761,#23762,#23763,#23764,#23765,#23766,#23767,#23768,
#23769,#23770,#23771,#23772,#23773,#23774,#23775,#23776,#23777,#23778,#23779,
#23780,#23781,#23782,#23783,#23784,#23785,#23786,#23787,#23788,#23789,#23790,
#23791,#23792,#23793,#23794,#23795,#23796,#23797,#23798,#23799,#23800,#23801,
#23802,#23803,#23804,#23805,#23806,#23807,#23808,#23809,#23810,#23811,#23812,
#23813,#23814,#23815,#23816,#23817,#23818,#23819,#23820,#23821,#23822,#23823,
#23824,#23825,#23826,#23827,#23828,#23829,#23830,#23831,#23832,#23833,#23834,
#23835,#23836,#23837,#23838,#23839,#23840,#23841,#23842,#23843,#23844,#23845,
#23846,#23847,#23848,#23849,#23850,#23851,#23852,#23853,#23854,#23855,#23856,
#23857,#23858,#23859,#23860,#23861,#23862,#23863,#23864,#23865,#23866,#23867,
#23868,#23869,#23870,#23871,#23872,#23873,#23874,#23875,#23876,#23877,#23878,
#23879),.UNSPECIFIED.,.F.,.F.,(4,2,2,2,2,2,2,2,2,2,2,2,2,2,2,2,2,2,2,2,
2,2,2,2,2,2,2,2,2,2,2,2,2,2,2,2,2,2,2,2,2,2,2,2,2,2,2,2,2,2,2,2,2,2,2,2,
2,2,2,2,2,2,2,2,2,2,2,2,2,2,2,2,2,2,2,2,2,2,2,4),(-0.926471073029744,-0.901398759294761,
-0.863449560271604,-0.8587761697636,-0.856877258545011,-0.85570281277469,
-0.854390777529996,-0.852453661213017,-0.847162662369924,-0.839085288849207,
-0.785971877562881,-0.777057598575648,-0.763193976411606,-0.75906279309083,
-0.75656269366143,-0.75430788109391,-0.751420113184561,-0.745434473064014,
-0.701439480574167,-0.663919966451118,-0.65922739160026,-0.657325276204849,
-0.656150248169787,-0.654838926037188,-0.652905234628083,-0.647638216958983,
-0.639610055216725,-0.58732950151616,-0.578277266020182,-0.563770046930224,
-0.559571489157056,-0.557056546905337,-0.555029930440796,-0.552279559627591,
-0.546982047577972,-0.540281886959943,-0.524985634153146,-0.487492707266087,
-0.462041993179969,-0.458914167666053,-0.45732445647121,-0.456066807200957,
-0.45458193471129,-0.451855905147516,-0.436961198923767,-0.393353239812336,
-0.365760600957839,-0.361234075326173,-0.358378298953241,-0.356127120693537,
-0.353608895514417,-0.349395326665183,-0.332804041632327,-0.269379222595975,
-0.261094679575136,-0.258714976427778,-0.257305711512071,-0.256034303932594,
-0.254320957608614,-0.250434290240936,-0.245054712240226,-0.230482217332864,
-0.180040824463748,-0.164788409045415,-0.160515653588025,-0.157984118036114,
-0.155959670457389,-0.153814290875608,-0.149684335246355,-0.132747892627418,
-0.104663709423388,-0.0651145466777724,-0.0605245248097448,-0.0586393776065246,
-0.0573507265026836,-0.0560085391993869,-0.0539314083632888,-0.0514996293803942,
-0.046843274153505,-0.000589973186885262),.UNSPECIFIED.);
#414=B_SPLINE_CURVE_WITH_KNOTS('',3,(#23880,#23881,#23882,#23883,#23884,
#23885,#23886,#23887,#23888,#23889,#23890,#23891,#23892,#23893,#23894,#23895,
#23896,#23897,#23898,#23899,#23900,#23901,#23902,#23903,#23904,#23905,#23906,
#23907,#23908,#23909,#23910,#23911,#23912,#23913,#23914,#23915,#23916,#23917,
#23918,#23919,#23920,#23921,#23922,#23923,#23924,#23925,#23926,#23927,#23928,
#23929,#23930,#23931,#23932,#23933,#23934,#23935,#23936,#23937,#23938,#23939),
 .UNSPECIFIED.,.F.,.F.,(4,2,2,2,2,2,2,2,2,2,2,2,2,2,2,2,2,2,2,2,2,2,2,2,
2,2,2,2,2,4),(-2.32386902743845,-2.30024041246414,-2.28982706294607,-2.28626771725673,
-2.28379755546917,-2.28169323369155,-2.27944215589424,-2.27658444578319,
-2.27205069880471,-2.24420995510776,-2.22185146770358,-2.20084557525772,
-2.18598778828631,-2.18325338576836,-2.18176690229588,-2.18050966000605,
-2.17892272561299,-2.17580707699489,-2.15134499037956,-2.1195743325545,
-2.1000265239033,-2.08816509482076,-2.0844248315671,-2.08231862587725,-2.0800700710637,
-2.07723710407267,-2.07278513444405,-2.04741796436327,-2.00170747490439,
-1.99319254965038),.UNSPECIFIED.);
#415=B_SPLINE_CURVE_WITH_KNOTS('',3,(#23940,#23941,#23942,#23943,#23944,
#23945,#23946,#23947,#23948,#23949,#23950,#23951,#23952,#23953,#23954,#23955,
#23956,#23957,#23958,#23959,#23960,#23961,#23962,#23963,#23964,#23965,#23966,
#23967,#23968,#23969,#23970,#23971,#23972,#23973,#23974,#23975,#23976,#23977,
#23978,#23979,#23980,#23981,#23982,#23983,#23984,#23985,#23986,#23987,#23988,
#23989,#23990,#23991,#23992,#23993,#23994,#23995,#23996,#23997,#23998,#23999,
#24000,#24001,#24002,#24003,#24004,#24005,#24006,#24007,#24008,#24009,#24010,
#24011,#24012,#24013,#24014,#24015,#24016,#24017,#24018,#24019,#24020,#24021,
#24022,#24023,#24024,#24025,#24026,#24027,#24028,#24029,#24030,#24031,#24032,
#24033,#24034,#24035,#24036,#24037,#24038,#24039,#24040,#24041,#24042,#24043,
#24044,#24045,#24046,#24047,#24048,#24049,#24050,#24051,#24052,#24053,#24054,
#24055,#24056,#24057,#24058,#24059,#24060,#24061,#24062,#24063,#24064,#24065,
#24066,#24067,#24068,#24069,#24070,#24071,#24072,#24073,#24074,#24075,#24076,
#24077,#24078,#24079,#24080,#24081,#24082,#24083,#24084,#24085,#24086,#24087,
#24088,#24089,#24090,#24091,#24092,#24093,#24094,#24095,#24096,#24097,#24098,
#24099,#24100,#24101,#24102,#24103,#24104,#24105,#24106,#24107,#24108,#24109,
#24110,#24111,#24112,#24113,#24114,#24115,#24116,#24117,#24118,#24119,#24120,
#24121,#24122,#24123,#24124,#24125,#24126,#24127,#24128,#24129,#24130,#24131,
#24132,#24133,#24134,#24135,#24136,#24137,#24138,#24139,#24140,#24141,#24142,
#24143,#24144,#24145,#24146,#24147,#24148,#24149,#24150,#24151),
 .UNSPECIFIED.,.F.,.F.,(4,2,2,2,2,2,2,2,2,2,2,2,2,2,2,2,2,2,2,2,2,2,2,2,
2,2,2,2,2,2,2,2,2,2,2,2,2,2,2,2,2,2,2,2,2,2,2,2,2,2,2,2,2,2,2,2,2,2,2,2,
2,2,2,2,2,2,2,2,2,2,2,2,2,2,2,2,2,2,2,2,2,2,2,2,2,2,2,2,2,2,2,2,2,2,2,2,
2,2,2,2,2,2,2,2,2,4),(-1.58825468741526,-1.55677506762686,-1.54139479875759,
-1.53864569877202,-1.53715547627514,-1.53589789844193,-1.53431399719557,
-1.53181158703341,-1.51858553333341,-1.46036439035829,-1.44421639674659,
-1.44003904369588,-1.43752901255672,-1.4352766705218,-1.43240780443973,
-1.42783719397291,-1.39873623119091,-1.35645497139845,-1.34174254908841,
-1.33902537677097,-1.33754258912259,-1.33628509220085,-1.33469355133465,
-1.33155601228223,-1.30476527817291,-1.25760534437154,-1.24442306199696,
-1.24036672110512,-1.23788355567592,-1.23562557886839,-1.23270783868223,
-1.22656355135345,-1.2029636011212,-1.17666026239359,-1.1454594412336,-1.14066498106173,
-1.13874619950042,-1.13756839240883,-1.13626106863574,-1.13434584666061,
-1.12920515949249,-1.099335148626,-1.04964048219559,-1.04338318364314,-1.04003650932242,
-1.03793804377308,-1.03563519696388,-1.0324382829047,-1.02471587082062,
-1.01386799284532,-0.952496209407458,-0.942316435553413,-0.939786839112411,
-0.938329715197559,-0.937080962753366,-0.935459307712926,-0.932064270962055,
-0.902850075623865,-0.851083944835811,-0.843539045504256,-0.840604468987905,
-0.838475751765444,-0.836195552509475,-0.833129397117509,-0.826177351757518,
-0.796164195035236,-0.765251952016309,-0.743697803607661,-0.740614769775796,
-0.739034717233685,-0.737777777429725,-0.736285594195263,-0.733524951392105,
-0.717856561959718,-0.667803722517626,-0.646912657506546,-0.642668709759187,
-0.639899310754679,-0.63765612011023,-0.63508152058239,-0.630609816994546,
-0.610327666667982,-0.559925052734969,-0.543811958200507,-0.541167496046246,
-0.539540907412971,-0.53828042250701,-0.536822407231302,-0.534220187814012,
-0.521681642425395,-0.462957025843696,-0.446684494953387,-0.442359922472271,
-0.439792878570727,-0.437548984029459,-0.434769297797808,-0.429327067146504,
-0.39206335072283,-0.3510844558689,-0.343160369793844,-0.340819935367345,
-0.339419677534822,-0.3381459957407,-0.33641512250523,-0.332427443485893,
-0.331363008767816),.UNSPECIFIED.);
#416=B_SPLINE_CURVE_WITH_KNOTS('',3,(#24156,#24157,#24158,#24159,#24160,
#24161,#24162,#24163,#24164,#24165,#24166,#24167,#24168,#24169,#24170,#24171,
#24172,#24173,#24174,#24175,#24176,#24177,#24178,#24179,#24180,#24181,#24182,
#24183,#24184,#24185,#24186,#24187,#24188,#24189,#24190,#24191,#24192,#24193,
#24194,#24195,#24196,#24197,#24198,#24199,#24200,#24201,#24202,#24203,#24204,
#24205,#24206,#24207,#24208,#24209,#24210,#24211,#24212,#24213,#24214,#24215,
#24216,#24217,#24218,#24219,#24220,#24221,#24222,#24223,#24224,#24225,#24226,
#24227,#24228,#24229,#24230,#24231,#24232,#24233,#24234,#24235,#24236,#24237,
#24238,#24239,#24240,#24241,#24242,#24243,#24244,#24245,#24246,#24247,#24248,
#24249,#24250,#24251,#24252,#24253,#24254,#24255,#24256,#24257,#24258,#24259,
#24260,#24261,#24262,#24263,#24264,#24265,#24266,#24267,#24268,#24269,#24270,
#24271,#24272,#24273,#24274,#24275,#24276,#24277,#24278,#24279,#24280,#24281,
#24282,#24283,#24284,#24285,#24286,#24287,#24288,#24289,#24290,#24291,#24292,
#24293,#24294,#24295,#24296,#24297,#24298,#24299,#24300,#24301,#24302,#24303,
#24304,#24305,#24306,#24307,#24308,#24309,#24310,#24311,#24312,#24313,#24314,
#24315,#24316,#24317,#24318,#24319,#24320,#24321,#24322,#24323,#24324,#24325,
#24326,#24327,#24328,#24329,#24330,#24331,#24332,#24333,#24334,#24335,#24336,
#24337,#24338,#24339,#24340,#24341,#24342,#24343,#24344,#24345,#24346,#24347,
#24348,#24349,#24350,#24351,#24352,#24353,#24354,#24355,#24356,#24357,#24358,
#24359,#24360,#24361,#24362,#24363,#24364,#24365,#24366,#24367,#24368,#24369,
#24370,#24371),.UNSPECIFIED.,.F.,.F.,(4,2,2,2,2,2,2,2,2,2,2,2,2,2,2,2,2,
2,2,2,2,2,2,2,2,2,2,2,2,2,2,2,2,2,2,2,2,2,2,2,2,2,2,2,2,2,2,2,2,2,2,2,2,
2,2,2,2,2,2,2,2,2,2,2,2,2,2,2,2,2,2,2,2,2,2,2,2,2,2,2,2,2,2,2,2,2,2,2,2,
2,2,2,2,2,2,2,2,2,2,2,2,2,2,2,2,2,2,4),(-2.18288930522275,-2.17834301383946,
-2.16020040172271,-2.15587072988079,-2.15332731439035,-2.1510806879597,
-2.14826681747001,-2.14387730153829,-2.1201523076371,-2.07288484499641,
-2.05752614137735,-2.05477918087068,-2.05328996736556,-2.05203287237048,
-2.05044923516515,-2.04794710130817,-2.03471863569996,-1.97652329525705,
-1.96038039200939,-1.95620379391468,-1.95369409432431,-1.9514419666657,
-1.94857325213857,-1.94400261283041,-1.91487487853451,-1.87265683400618,
-1.85795633725304,-1.85523983324506,-1.85375720853212,-1.85249967531851,
-1.85090784074904,-1.84776905670891,-1.82053844454068,-1.80702176300512,
-1.762770457098,-1.75754620130744,-1.75481133108086,-1.75278677223426,-1.75026235437542,
-1.74601912725718,-1.73107638943766,-1.72277035561684,-1.67406462991704,
-1.6585415000374,-1.65578724851468,-1.65429647179162,-1.65303948404066,
-1.65145778811473,-1.64836688534275,-1.61499255657007,-1.6073174439316,
-1.56316058746397,-1.55800618092379,-1.55528573064452,-1.55326253842361,
-1.55072773351432,-1.54643765807058,-1.53099284876732,-1.52359312990677,
-1.47079345239254,-1.46273356700672,-1.45745170533687,-1.4555160347539,
-1.45420441800844,-1.45302991697515,-1.45113012579219,-1.44645060936936,
-1.40879652980982,-1.37789096259205,-1.36733124129625,-1.35976588672558,
-1.35659469999181,-1.35429635296919,-1.35219233198252,-1.34935546633975,
-1.34239240660485,-1.29454086604358,-1.26039285948415,-1.25710430676926,
-1.25550345953941,-1.2542450605592,-1.2527686867682,-1.25008208414243,-1.23599879538802,
-1.20020177073284,-1.16420873192039,-1.15953052808974,-1.15662915048781,
-1.15437271942564,-1.15187998748226,-1.14778215559761,-1.13257488419503,
-1.08167177164236,-1.06058446385204,-1.05751334261323,-1.055935687434,-1.05467867073207,
-1.05318402170262,-1.05041255344463,-1.03449880251862,-0.981965032847736,
-0.963518796284954,-0.959029969321492,-0.956424982584346,-0.954183684597177,
-0.951452370623684,-0.946247010678033,-0.926471073029744),.UNSPECIFIED.);
#417=B_SPLINE_CURVE_WITH_KNOTS('',3,(#24373,#24374,#24375,#24376,#24377,
#24378,#24379,#24380,#24381,#24382,#24383,#24384,#24385,#24386,#24387,#24388,
#24389,#24390,#24391,#24392,#24393,#24394,#24395,#24396,#24397,#24398,#24399,
#24400,#24401,#24402,#24403,#24404,#24405,#24406,#24407,#24408,#24409,#24410,
#24411,#24412,#24413,#24414,#24415,#24416,#24417,#24418,#24419,#24420,#24421,
#24422,#24423,#24424,#24425,#24426,#24427,#24428,#24429,#24430,#24431,#24432),
 .UNSPECIFIED.,.F.,.F.,(4,2,2,2,2,2,2,2,2,2,2,2,2,2,2,2,2,2,2,2,2,2,2,2,
2,2,2,2,2,4),(-0.331363008767816,-0.314613325869936,-0.263867340288622,
-0.247176462282809,-0.242822084074471,-0.240248181884976,-0.238004959710724,
-0.235289894837674,-0.230105687478555,-0.223506425722653,-0.208541152356611,
-0.174691666715924,-0.145069412420928,-0.141929844389683,-0.140337806477531,
-0.139080220156367,-0.137597676101777,-0.13488172883738,-0.120193948897179,
-0.102666300485983,-0.0745907170427717,-0.0667114523857546,-0.0479811673334748,
-0.0434728312697193,-0.0408636002469527,-0.0386228621979387,-0.0364783822061139,
-0.0338123195932177,-0.0297771153707352,-0.000589579587611316),
 .UNSPECIFIED.);
#418=B_SPLINE_CURVE_WITH_KNOTS('',3,(#24433,#24434,#24435,#24436,#24437,
#24438,#24439,#24440,#24441,#24442,#24443,#24444,#24445,#24446,#24447,#24448,
#24449,#24450,#24451,#24452,#24453,#24454,#24455,#24456,#24457,#24458,#24459,
#24460,#24461,#24462,#24463,#24464,#24465,#24466,#24467,#24468,#24469,#24470,
#24471,#24472,#24473,#24474,#24475,#24476,#24477,#24478,#24479,#24480,#24481,
#24482,#24483,#24484,#24485,#24486,#24487,#24488,#24489,#24490,#24491,#24492,
#24493,#24494,#24495,#24496,#24497,#24498,#24499,#24500,#24501,#24502,#24503,
#24504,#24505,#24506,#24507,#24508,#24509,#24510,#24511,#24512,#24513,#24514,
#24515,#24516,#24517,#24518,#24519,#24520,#24521,#24522,#24523,#24524,#24525,
#24526,#24527,#24528,#24529,#24530,#24531,#24532,#24533,#24534,#24535,#24536,
#24537,#24538,#24539,#24540,#24541,#24542,#24543,#24544,#24545,#24546,#24547,
#24548,#24549,#24550,#24551,#24552,#24553,#24554,#24555,#24556,#24557,#24558,
#24559,#24560,#24561,#24562,#24563,#24564,#24565,#24566,#24567,#24568,#24569,
#24570,#24571,#24572,#24573,#24574,#24575,#24576,#24577,#24578,#24579,#24580,
#24581,#24582,#24583,#24584,#24585,#24586,#24587,#24588,#24589,#24590,#24591,
#24592),.UNSPECIFIED.,.F.,.F.,(4,2,2,2,2,2,2,2,2,2,2,2,2,2,2,2,2,2,2,2,
2,2,2,2,2,2,2,2,2,2,2,2,2,2,2,2,2,2,2,2,2,2,2,2,2,2,2,2,2,2,2,2,2,2,2,2,
2,2,2,2,2,2,2,2,2,2,2,2,2,2,2,2,2,2,2,2,2,2,2,4),(-2.51358401917516,-2.46703860870495,
-2.46051812019456,-2.45601462776875,-2.45419725742886,-2.45290914450858,
-2.45171041740422,-2.45002073159288,-2.44548318021959,-2.40464700529405,
-2.37779981793696,-2.36090169562812,-2.35677388468954,-2.35462965872032,
-2.35238935779344,-2.3497816367392,-2.34527840742169,-2.32661282921734,
-2.29323509950433,-2.26204653145543,-2.25680265662964,-2.25487274654001,
-2.25356258071575,-2.25238753313668,-2.25048344397783,-2.24577632722571,
-2.20858866072298,-2.17736326057625,-2.16674123678549,-2.15914203105175,
-2.15596576186363,-2.15366699020086,-2.15156482532594,-2.14873385523847,
-2.14180236408896,-2.09357101040751,-2.06252505115547,-2.05729207703341,
-2.05536366441566,-2.05405375605734,-2.05287836137734,-2.05097263444841,
-2.04625610368035,-2.00958269215844,-2.00827377236082,-1.96357062935181,
-1.95836210175496,-1.95563066737396,-1.95360665753113,-1.95108035445126,
-1.94682777536967,-1.93178326394824,-1.92412774371613,-1.87492927438097,
-1.85935091895692,-1.85659442034959,-1.85510325700639,-1.85384644525813,
-1.85226563405835,-1.84917842462162,-1.82743592732228,-1.7933232899625,
-1.7734818379219,-1.76145754600471,-1.75767679399282,-1.75525400601117,
-1.75297560363687,-1.74997200248425,-1.74318546755197,-1.69190450788205,
-1.66983204042916,-1.66282779437516,-1.65807321130845,-1.65621599499858,
-1.65492022064735,-1.65373063107379,-1.65174984896922,-1.64657571147666,
-1.60316397744653,-1.58790776972358),.UNSPECIFIED.);
#419=B_SPLINE_CURVE_WITH_KNOTS('',3,(#24598,#24599,#24600,#24601,#24602,
#24603,#24604,#24605,#24606,#24607,#24608,#24609,#24610,#24611,#24612,#24613,
#24614,#24615,#24616,#24617,#24618,#24619,#24620,#24621,#24622,#24623,#24624,
#24625,#24626,#24627,#24628,#24629,#24630,#24631,#24632,#24633,#24634,#24635,
#24636,#24637,#24638,#24639,#24640,#24641,#24642,#24643,#24644,#24645,#24646,
#24647,#24648,#24649,#24650,#24651,#24652,#24653,#24654,#24655,#24656,#24657,
#24658,#24659,#24660,#24661,#24662,#24663,#24664,#24665,#24666,#24667,#24668,
#24669,#24670,#24671,#24672,#24673,#24674,#24675,#24676,#24677,#24678,#24679,
#24680,#24681,#24682,#24683,#24684,#24685,#24686,#24687,#24688,#24689,#24690,
#24691,#24692,#24693,#24694,#24695,#24696,#24697,#24698,#24699,#24700,#24701,
#24702,#24703,#24704,#24705,#24706,#24707,#24708,#24709,#24710,#24711,#24712,
#24713,#24714,#24715,#24716,#24717,#24718,#24719,#24720,#24721,#24722,#24723,
#24724,#24725,#24726,#24727,#24728,#24729,#24730,#24731,#24732,#24733,#24734,
#24735,#24736,#24737,#24738,#24739,#24740,#24741,#24742,#24743,#24744,#24745,
#24746,#24747,#24748,#24749,#24750,#24751,#24752,#24753,#24754,#24755,#24756,
#24757,#24758,#24759,#24760,#24761,#24762,#24763,#24764,#24765,#24766,#24767,
#24768,#24769,#24770,#24771,#24772,#24773,#24774,#24775,#24776,#24777,#24778,
#24779,#24780,#24781,#24782,#24783,#24784,#24785,#24786,#24787,#24788,#24789,
#24790,#24791,#24792,#24793,#24794,#24795,#24796,#24797,#24798,#24799),
 .UNSPECIFIED.,.F.,.F.,(4,2,2,2,2,2,2,2,2,2,2,2,2,2,2,2,2,2,2,2,2,2,2,2,
2,2,2,2,2,2,2,2,2,2,2,2,2,2,2,2,2,2,2,2,2,2,2,2,2,2,2,2,2,2,2,2,2,2,2,2,
2,2,2,2,2,2,2,2,2,2,2,2,2,2,2,2,2,2,2,2,2,2,2,2,2,2,2,2,2,2,2,2,2,2,2,2,
2,2,2,2,4),(-0.926590849584021,-0.895705628617206,-0.849097035878392,-0.84205238580067,
-0.839201487858656,-0.837093933251416,-0.834798394542621,-0.831643261401205,
-0.824174518738562,-0.813788802669523,-0.7837535010908,-0.777232071165272,
-0.774946725784697,-0.756916936181162,-0.742064214596665,-0.739479374222173,
-0.737870647314892,-0.736611704772934,-0.735141235364103,-0.732481715790049,
-0.718919058633716,-0.685782092130831,-0.646498652233088,-0.641855846977377,
-0.638965158103643,-0.636710135130437,-0.634211917532468,-0.630088762293131,
-0.614588451309749,-0.562036459205467,-0.557273586525968,-0.542536259699213,
-0.539956820168759,-0.53834966162718,-0.537090765311508,-0.535618981590008,
-0.532953677846819,-0.519284180896549,-0.483463864555616,-0.479834864333695,
-0.447003099826601,-0.442349011651426,-0.43945481891684,-0.437199219675766,
-0.434702563613216,-0.430587084483246,-0.415178318239458,-0.363324761820432,
-0.356756312954078,-0.342930448248988,-0.340396089552481,-0.338802484965043,
-0.337544493127627,-0.336062417776771,-0.333349724848171,-0.318740074634343,
-0.287948673622923,-0.247447086897912,-0.242803199030523,-0.239911966447855,
-0.237656599298613,-0.2376061950838,-0.237560501009073,-0.237519066148853,
-0.237481482031868,-0.237447381287586,-0.237416432763583,-0.237388337869124,
-0.237362827247346,-0.237339657852027,-0.237318610250785,-0.237299486247105,
-0.237272793681814,-0.237246662466461,-0.237221077810542,-0.237196025360201,
-0.237171491207558,-0.237147461813345,-0.237123924063153,-0.234481204273956,
-0.229639135778107,-0.223576755855529,-0.172049741676069,-0.143982609666729,
-0.140842202158548,-0.139249695289737,-0.137991710515435,-0.136508637639563,
-0.13379154507168,-0.1190922253451,-0.0836875128642156,-0.0677007568617229,
-0.0578862961661651,-0.045709236361506,-0.0417684314047173,-0.0393099850987222,
-0.0370436444585214,-0.0348306661534586,-0.0319439022230871,-0.0273777962145406,
-0.000589178997369609),.UNSPECIFIED.);
#420=B_SPLINE_CURVE_WITH_KNOTS('',3,(#24800,#24801,#24802,#24803,#24804,
#24805,#24806,#24807,#24808,#24809,#24810,#24811,#24812,#24813,#24814,#24815,
#24816,#24817,#24818,#24819,#24820,#24821,#24822,#24823,#24824,#24825,#24826,
#24827,#24828,#24829,#24830,#24831,#24832,#24833,#24834,#24835,#24836,#24837,
#24838,#24839,#24840,#24841,#24842,#24843,#24844,#24845,#24846,#24847,#24848,
#24849,#24850,#24851,#24852,#24853),.UNSPECIFIED.,.F.,.F.,(4,2,2,2,2,2,
2,2,2,2,2,2,2,2,2,2,2,2,2,2,2,2,2,2,2,2,4),(-2.51327171715581,-2.48216238508032,
-2.45919088034406,-2.45466062409862,-2.45283886646618,-2.4515498705018,
-2.45035209269732,-2.44866616191491,-2.44415559962663,-2.40283336804128,
-2.37572130933742,-2.35946289330924,-2.35538592518744,-2.35324585131935,
-2.35102717896767,-2.34841220047479,-2.34387768404516,-2.32476294411026,
-2.27290024661368,-2.25704996916575,-2.25428163299295,-2.25278787855367,
-2.25153113879486,-2.24995323829489,-2.24687991493532,-2.22570759015456,
-2.18288930522275),.UNSPECIFIED.);
#421=B_SPLINE_CURVE_WITH_KNOTS('',3,(#24854,#24855,#24856,#24857,#24858,
#24859,#24860,#24861,#24862,#24863,#24864,#24865,#24866,#24867,#24868,#24869,
#24870,#24871,#24872,#24873,#24874,#24875,#24876,#24877,#24878,#24879,#24880,
#24881,#24882,#24883,#24884,#24885,#24886,#24887,#24888,#24889,#24890,#24891,
#24892,#24893,#24894,#24895,#24896,#24897,#24898,#24899,#24900,#24901,#24902,
#24903,#24904,#24905,#24906,#24907,#24908,#24909,#24910,#24911,#24912,#24913,
#24914,#24915,#24916,#24917,#24918,#24919,#24920,#24921,#24922,#24923,#24924,
#24925,#24926,#24927,#24928,#24929,#24930,#24931,#24932,#24933,#24934,#24935,
#24936,#24937,#24938,#24939,#24940,#24941,#24942,#24943,#24944,#24945,#24946,
#24947,#24948,#24949,#24950,#24951,#24952,#24953,#24954,#24955,#24956,#24957,
#24958,#24959,#24960,#24961,#24962,#24963,#24964,#24965,#24966,#24967,#24968,
#24969,#24970,#24971,#24972,#24973,#24974,#24975,#24976,#24977,#24978,#24979,
#24980,#24981,#24982,#24983,#24984,#24985,#24986,#24987,#24988,#24989,#24990,
#24991,#24992,#24993,#24994,#24995,#24996,#24997,#24998,#24999,#25000,#25001,
#25002,#25003,#25004,#25005,#25006,#25007,#25008,#25009,#25010,#25011,#25012,
#25013,#25014,#25015,#25016,#25017,#25018,#25019,#25020,#25021,#25022,#25023,
#25024,#25025,#25026,#25027,#25028,#25029,#25030,#25031,#25032,#25033,#25034,
#25035,#25036,#25037,#25038,#25039,#25040,#25041,#25042,#25043,#25044,#25045,
#25046,#25047,#25048,#25049,#25050,#25051,#25052,#25053,#25054,#25055,#25056,
#25057,#25058,#25059,#25060,#25061,#25062,#25063,#25064,#25065,#25066,#25067,
#25068,#25069,#25070,#25071,#25072,#25073,#25074,#25075),.UNSPECIFIED.,
 .F.,.F.,(4,2,2,2,2,2,2,2,2,2,2,2,2,2,2,2,2,2,2,2,2,2,2,2,2,2,2,2,2,2,2,
2,2,2,2,2,2,2,2,2,2,2,2,2,2,2,2,2,2,2,2,2,2,2,2,2,2,2,2,2,2,2,2,2,2,2,2,
2,2,2,2,2,2,2,2,2,2,2,2,2,2,2,2,2,2,2,2,2,2,2,2,2,2,2,2,2,2,2,2,2,2,2,2,
2,2,2,2,2,2,2,4),(-1.58790776972358,-1.56433038537726,-1.55922552834473,
-1.55651550855986,-1.55429663836922,-1.55168292212814,-1.54715436724346,
-1.52813037922064,-1.47614614877465,-1.46028109451036,-1.45751195575631,
-1.45601797405431,-1.45476117260214,-1.45318338617889,-1.4501108637531,
-1.42896988838759,-1.37803958926502,-1.36805226866343,-1.36080496724478,
-1.3576876652133,-1.35539902472085,-1.35328333181485,-1.35039917994523,
-1.34315648021733,-1.30169838395921,-1.27269464144579,-1.26449670339422,
-1.25914786400453,-1.25720279984552,-1.25601998818139,-1.25471780634858,
-1.25282809331194,-1.24786016457302,-1.24043607544603,-1.21609426764117,
-1.16831833072192,-1.16135110661376,-1.15851372473321,-1.15640974861023,
-1.15411187187234,-1.15094212745578,-1.14338416094597,-1.13283645927949,
-1.10199248833042,-1.06418610726124,-1.05951055055522,-1.05761151373998,
-1.05643722499709,-1.05512561058081,-1.05318956827674,-1.04790434174775,
-1.03983840816093,-0.986921597734203,-0.979849263367743,-0.96424914910678,
-0.959944356115374,-0.957406397205592,-0.955383753702977,-0.952667993201792,
-0.947535709764712,-0.906442000049919,-0.864311606286453,-0.859854417102353,
-0.858175525700282,-0.856979535409336,-0.855688908569718,-0.853859037279309,
-0.849278918784948,-0.825798522273947,-0.799834300346273,-0.766250011593278,
-0.761588242008963,-0.758691938877223,-0.756436334221659,-0.753941347516222,
-0.74983251145566,-0.73449664720544,-0.683187480161499,-0.674762776190746,
-0.662035645267422,-0.659561113628769,-0.657985800836894,-0.656729035787356,
-0.655232800303313,-0.652453434985366,-0.636347181587834,-0.581669316826979,
-0.565263035664434,-0.560927233560201,-0.558357533134028,-0.556113792558436,
-0.553337497964581,-0.547912321027593,-0.504863377490104,-0.465348547109447,
-0.460756767152621,-0.458871617368697,-0.457583207893888,-0.456241511823363,
-0.454165620251658,-0.447820358056242,-0.437464068155186,-0.389527692327158,
-0.366507039381414,-0.362143755338416,-0.35933772025724,-0.357091582241529,
-0.354542529520285,-0.35018792614072,-0.331697579609663,-0.331164696783045),
 .UNSPECIFIED.);
#422=B_SPLINE_CURVE_WITH_KNOTS('',3,(#25080,#25081,#25082,#25083,#25084,
#25085,#25086,#25087,#25088,#25089,#25090,#25091,#25092,#25093,#25094,#25095,
#25096,#25097,#25098,#25099,#25100,#25101,#25102,#25103,#25104,#25105,#25106,
#25107,#25108,#25109,#25110,#25111,#25112,#25113,#25114,#25115,#25116,#25117,
#25118,#25119,#25120,#25121,#25122,#25123,#25124,#25125,#25126,#25127,#25128,
#25129,#25130,#25131,#25132,#25133,#25134,#25135,#25136,#25137,#25138,#25139,
#25140,#25141,#25142,#25143,#25144,#25145,#25146,#25147,#25148,#25149,#25150,
#25151,#25152,#25153,#25154,#25155,#25156,#25157,#25158,#25159,#25160,#25161,
#25162,#25163,#25164,#25165,#25166,#25167,#25168,#25169,#25170,#25171,#25172,
#25173,#25174,#25175,#25176,#25177,#25178,#25179,#25180,#25181,#25182,#25183,
#25184,#25185,#25186,#25187,#25188,#25189,#25190,#25191,#25192,#25193,#25194,
#25195,#25196,#25197,#25198,#25199,#25200,#25201,#25202,#25203,#25204,#25205,
#25206,#25207,#25208,#25209,#25210,#25211,#25212,#25213,#25214,#25215,#25216,
#25217,#25218,#25219,#25220,#25221,#25222,#25223,#25224,#25225,#25226,#25227,
#25228,#25229,#25230,#25231,#25232,#25233,#25234,#25235,#25236,#25237,#25238,
#25239,#25240,#25241,#25242,#25243,#25244,#25245,#25246,#25247,#25248,#25249,
#25250,#25251,#25252,#25253,#25254,#25255,#25256,#25257,#25258,#25259,#25260,
#25261,#25262,#25263,#25264,#25265,#25266,#25267,#25268,#25269,#25270,#25271,
#25272,#25273,#25274,#25275,#25276,#25277,#25278,#25279,#25280,#25281,#25282,
#25283,#25284,#25285,#25286,#25287,#25288,#25289,#25290,#25291,#25292,#25293),
 .UNSPECIFIED.,.F.,.F.,(4,2,2,2,2,2,2,2,2,2,2,2,2,2,2,2,2,2,2,2,2,2,2,2,
2,2,2,2,2,2,2,2,2,2,2,2,2,2,2,2,2,2,2,2,2,2,2,2,2,2,2,2,2,2,2,2,2,2,2,2,
2,2,2,2,2,2,2,2,2,2,2,2,2,2,2,2,2,2,2,2,2,2,2,2,2,2,2,2,2,2,2,2,2,2,2,2,
2,2,2,2,2,2,2,2,2,2,4),(-2.18303470285366,-2.15323070742354,-2.13838275441974,
-2.13565920080161,-2.13417502276345,-2.13291756089068,-2.13132758505621,
-2.12819774145529,-2.09732430128089,-2.05947037596656,-2.04158971387745,
-2.03727871475553,-2.03473931492364,-2.03249198606179,-2.02967158806749,
-2.02526089969832,-2.00098170680169,-1.95423868863094,-1.9389419007886,
-1.93619761165177,-1.93470892585,-1.93345172481894,-1.93186725469224,-1.92936251419912,
-1.91608774371415,-1.8579349067261,-1.84179569422143,-1.83761925732135,
-1.83510951416174,-1.83285725855118,-1.8299882590998,-1.82541692029795,
-1.79627084060417,-1.75406610782806,-1.73936708878227,-1.73665055484494,
-1.73516787905997,-1.73391028142891,-1.73231833842737,-1.72917926022242,
-1.70187761255867,-1.68842486591373,-1.65811051600642,-1.64766888773947,
-1.64016876818698,-1.63700858717922,-1.6347123316985,-1.6326061581937,-1.62976022503272,
-1.62274365673674,-1.57566490710204,-1.54073000057352,-1.5375055302525,
-1.53591745204772,-1.53465999739472,-1.53317406646495,-1.5305178873319,
-1.51865850714293,-1.45907989559261,-1.44280473715374,-1.43861714468706,
-1.43610491853278,-1.4338530992537,-1.43098830552653,-1.42643100233579,
-1.39778419182389,-1.35512210007525,-1.34035792101552,-1.33763825993884,
-1.33615489535833,-1.33489733058598,-1.33330621547456,-1.33017111859939,
-1.30379552089089,-1.25734096698368,-1.24325615154456,-1.23910203776784,
-1.23659716011384,-1.23434383637724,-1.23146598879311,-1.22552999347426,
-1.18770298528498,-1.14331160636109,-1.13908645869486,-1.13744080414567,
-1.13625357555316,-1.13495547125603,-1.13308668699463,-1.12825750268597,
-1.12110796042993,-1.09826765738807,-1.04825527587019,-1.04134067265296,
-1.03858686777589,-1.03629453433488,-1.03393894020954,-1.0304741371515,
-1.0209779822248,-1.0067028198717,-0.950036471996001,-0.940858628873664,
-0.938389628295971,-0.936960772696591,-0.935821787841959,-0.934218751633752,
-0.930919155436449,-0.926590849584021),.UNSPECIFIED.);
#423=B_SPLINE_CURVE_WITH_KNOTS('',3,(#25295,#25296,#25297,#25298,#25299,
#25300,#25301,#25302,#25303,#25304,#25305,#25306,#25307,#25308,#25309,#25310,
#25311,#25312,#25313,#25314,#25315,#25316,#25317,#25318,#25319,#25320,#25321,
#25322,#25323,#25324,#25325,#25326,#25327,#25328,#25329,#25330,#25331,#25332,
#25333,#25334,#25335,#25336,#25337,#25338,#25339,#25340,#25341,#25342,#25343,
#25344,#25345,#25346),.UNSPECIFIED.,.F.,.F.,(4,2,2,2,2,2,2,2,2,2,2,2,2,
2,2,2,2,2,2,2,2,2,2,2,2,4),(-0.331164696783045,-0.284340024328848,-0.263458405458446,
-0.260394021052475,-0.258817921732811,-0.25756113203129,-0.256065580756608,
-0.253289371421596,-0.237388738728392,-0.184912682781884,-0.166395205030571,
-0.161901670623027,-0.159295798848285,-0.157054846381753,-0.154909335325312,
-0.150771729368069,-0.13373600435653,-0.106159192349091,-0.0661893748728856,
-0.061617829780471,-0.0597360883543101,-0.0584483707546459,-0.0571057808163933,
-0.0550256913502012,-0.0486456322016143,-0.00058995120662514),
 .UNSPECIFIED.);
#424=B_SPLINE_CURVE_WITH_KNOTS('',3,(#25347,#25348,#25349,#25350,#25351,
#25352,#25353,#25354,#25355,#25356,#25357,#25358,#25359,#25360,#25361,#25362,
#25363,#25364,#25365,#25366,#25367,#25368,#25369,#25370,#25371,#25372,#25373,
#25374,#25375,#25376,#25377,#25378,#25379,#25380,#25381,#25382,#25383,#25384,
#25385,#25386,#25387,#25388,#25389,#25390,#25391,#25392,#25393,#25394,#25395,
#25396,#25397,#25398,#25399,#25400,#25401,#25402,#25403,#25404,#25405,#25406,
#25407,#25408,#25409,#25410,#25411,#25412,#25413,#25414,#25415,#25416,#25417,
#25418,#25419,#25420,#25421,#25422,#25423,#25424,#25425,#25426,#25427,#25428,
#25429,#25430,#25431,#25432,#25433,#25434,#25435,#25436,#25437,#25438,#25439,
#25440,#25441,#25442,#25443,#25444,#25445,#25446,#25447,#25448,#25449,#25450,
#25451,#25452,#25453,#25454,#25455,#25456,#25457,#25458,#25459,#25460,#25461,
#25462,#25463,#25464,#25465,#25466,#25467,#25468,#25469,#25470,#25471,#25472,
#25473,#25474,#25475,#25476,#25477,#25478,#25479,#25480,#25481,#25482,#25483,
#25484,#25485,#25486,#25487,#25488,#25489,#25490,#25491,#25492,#25493,#25494,
#25495,#25496,#25497,#25498,#25499,#25500,#25501,#25502,#25503,#25504,#25505,
#25506),.UNSPECIFIED.,.F.,.F.,(4,2,2,2,2,2,2,2,2,2,2,2,2,2,2,2,2,2,2,2,
2,2,2,2,2,2,2,2,2,2,2,2,2,2,2,2,2,2,2,2,2,2,2,2,2,2,2,2,2,2,2,2,2,2,2,2,
2,2,2,2,2,2,2,2,2,2,2,2,2,2,2,2,2,2,2,2,2,2,2,4),(-2.51410445116209,-2.48115962050804,
-2.4775909854511,-2.47511710807547,-2.47301244678002,-2.47076222930669,
-2.46791145153916,-2.46340035413433,-2.43629515448796,-2.41345917543091,
-2.3918711866273,-2.37725269550936,-2.37452995355423,-2.37304602537111,
-2.37178866658817,-2.37019871104166,-2.36706860085179,-2.34130238490027,
-2.28778461265617,-2.28158674873041,-2.27666077349263,-2.27399903801622,
-2.27197657063979,-2.26943915158629,-2.26513604710984,-2.24955080300122,
-2.2424050734882,-2.20341756298698,-2.18046744818344,-2.17593920896639,
-2.1741178163007,-2.17282892763191,-2.17163114411436,-2.16994507729867,
-2.16543325549935,-2.12410635948414,-2.08265470442655,-2.07733252077868,
-2.07457767069645,-2.07255116461594,-2.07004071453089,-2.06585997657549,
-2.05151614598836,-2.04212252185987,-1.99373447131584,-1.98334167469653,
-1.97698131906251,-1.97490385701313,-1.97356201090889,-1.97227418791932,
-1.97039103713779,-1.96580976647041,-1.92614628363177,-1.88300627035365,
-1.87775431228586,-1.87501386675412,-1.87298888623818,-1.87046871175628,
-1.86624407825216,-1.85147730278375,-1.84284309777178,-1.79042690555159,
-1.78238945657257,-1.7771186455345,-1.77518472927491,-1.77387361724298,
-1.77269906382288,-1.77079827600718,-1.76611178981052,-1.72855070920642,
-1.6844844865033,-1.67858935215021,-1.67571960484346,-1.67346737213277,
-1.67095829089961,-1.66678447810119,-1.652509791412,-1.64298838599048,-1.59084016524227,
-1.58799807313078),.UNSPECIFIED.);
#425=B_SPLINE_CURVE_WITH_KNOTS('',3,(#25512,#25513,#25514,#25515,#25516,
#25517,#25518,#25519,#25520),.UNSPECIFIED.,.F.,.F.,(4,1,1,1,1,1,4),(47.1238898038469,
47.2191271055195,48.2168442690671,49.2145614326147,50.2122785961623,51.2099957597099,
51.753505798748),.UNSPECIFIED.);
#426=B_SPLINE_CURVE_WITH_KNOTS('',3,(#25521,#25522,#25523,#25524,#25525,
#25526,#25527,#25528,#25529,#25530,#25531,#25532,#25533,#25534,#25535,#25536,
#25537,#25538,#25539,#25540,#25541,#25542,#25543,#25544,#25545,#25546,#25547,
#25548,#25549,#25550,#25551,#25552,#25553,#25554,#25555,#25556,#25557,#25558,
#25559,#25560,#25561,#25562,#25563,#25564,#25565,#25566,#25567,#25568,#25569,
#25570,#25571,#25572,#25573,#25574),.UNSPECIFIED.,.F.,.F.,(4,2,2,2,2,2,
2,2,2,2,2,2,2,2,2,2,2,2,2,2,2,2,2,2,2,2,4),(-2.51382926221767,-2.45903949326626,
-2.44068235929343,-2.43633727043439,-2.4337903419711,-2.43154397812033,
-2.42873488528968,-2.42436142953249,-2.40107333404785,-2.35338312683811,
-2.34304546170578,-2.33878344098341,-2.33559364184831,-2.33400554447704,
-2.33278162207138,-2.33133353937978,-2.32884275385845,-2.31910991204386,
-2.25731393916809,-2.24084993657796,-2.23664717385184,-2.23413165225028,
-2.23188053067103,-2.22902160968702,-2.22448363042851,-2.19649575545307,
-2.18303470285366),.UNSPECIFIED.);
#427=B_SPLINE_CURVE_WITH_KNOTS('',3,(#25575,#25576,#25577,#25578,#25579,
#25580,#25581,#25582,#25583,#25584,#25585,#25586,#25587,#25588,#25589,#25590,
#25591,#25592,#25593,#25594,#25595,#25596,#25597,#25598,#25599,#25600,#25601,
#25602,#25603,#25604,#25605,#25606,#25607,#25608,#25609,#25610,#25611,#25612,
#25613,#25614,#25615,#25616,#25617,#25618,#25619,#25620,#25621,#25622,#25623,
#25624,#25625,#25626,#25627,#25628,#25629,#25630,#25631,#25632,#25633,#25634,
#25635,#25636,#25637,#25638,#25639,#25640,#25641,#25642,#25643,#25644,#25645,
#25646,#25647,#25648,#25649,#25650,#25651,#25652,#25653,#25654,#25655,#25656,
#25657,#25658,#25659,#25660,#25661,#25662,#25663,#25664,#25665,#25666,#25667,
#25668,#25669,#25670,#25671,#25672,#25673,#25674,#25675,#25676,#25677,#25678,
#25679,#25680,#25681,#25682,#25683,#25684,#25685,#25686,#25687,#25688,#25689,
#25690,#25691,#25692,#25693,#25694,#25695,#25696,#25697,#25698,#25699,#25700,
#25701,#25702,#25703,#25704,#25705,#25706,#25707,#25708,#25709,#25710,#25711,
#25712,#25713,#25714,#25715,#25716,#25717,#25718,#25719,#25720,#25721,#25722,
#25723,#25724,#25725,#25726,#25727,#25728,#25729,#25730,#25731,#25732,#25733,
#25734,#25735,#25736,#25737,#25738,#25739,#25740,#25741,#25742,#25743,#25744,
#25745,#25746,#25747,#25748,#25749,#25750,#25751,#25752,#25753,#25754,#25755,
#25756,#25757,#25758,#25759,#25760,#25761,#25762,#25763,#25764,#25765,#25766,
#25767,#25768,#25769,#25770,#25771,#25772,#25773,#25774,#25775,#25776,#25777,
#25778,#25779,#25780,#25781,#25782,#25783,#25784,#25785,#25786,#25787,#25788,
#25789,#25790,#25791,#25792,#25793,#25794),.UNSPECIFIED.,.F.,.F.,(4,2,2,
2,2,2,2,2,2,2,2,2,2,2,2,2,2,2,2,2,2,2,2,2,2,2,2,2,2,2,2,2,2,2,2,2,2,2,2,
2,2,2,2,2,2,2,2,2,2,2,2,2,2,2,2,2,2,2,2,2,2,2,2,2,2,2,2,2,2,2,2,2,2,2,2,
2,2,2,2,2,2,2,2,2,2,2,2,2,2,2,2,2,2,2,2,2,2,2,2,2,2,2,2,2,2,2,2,2,2,4),
(-1.58799807313078,-1.58281854779097,-1.57755537961493,-1.5756224874594,
-1.57431153510487,-1.57313671950623,-1.57123475362205,-1.56654160087626,
-1.52906351136109,-1.49802699439358,-1.48199304797864,-1.47782511396363,
-1.47531717555945,-1.47306445112747,-1.47019199152731,-1.46560938630689,
-1.43669924933499,-1.39428106696778,-1.37954944304334,-1.37683123410999,
-1.37534815887241,-1.37409054249698,-1.3724990119409,-1.36936207201397,
-1.34274183254778,-1.28674100229136,-1.27993345901643,-1.27689317464382,
-1.27461735267793,-1.2721882306633,-1.26837862871245,-1.25723710660705,
-1.23894332830876,-1.21377157079921,-1.20269944921508,-1.20183196487044,
-1.1806593824426,-1.17758610323861,-1.17600826057003,-1.174751591428,-1.17325796937191,
-1.17049004405378,-1.15464591426987,-1.10283366266568,-1.08368075910792,
-1.0791439567425,-1.07652848512044,-1.07430988584095,-1.07160236463613,
-1.06650883198453,-1.02845631994496,-0.98703199366014,-0.979653981653059,
-0.977375689492475,-0.975989358952021,-0.974710736414749,-0.972948252382905,
-0.968776938777643,-0.949308591445746,-0.898213513488314,-0.883458187345647,
-0.879234678108117,-0.876714705181225,-0.874689625715152,-0.871948694274047,
-0.866694631378739,-0.823439680357804,-0.783858298084751,-0.779271076918284,
-0.777386865775199,-0.776098786118058,-0.774757126591892,-0.772680757375622,
-0.766329880626308,-0.755960188204414,-0.707840955538581,-0.697561859977648,
-0.683732683711984,-0.679605829781044,-0.677107111653054,-0.674852757496159,
-0.671964490956605,-0.665973890678441,-0.62125639897922,-0.584495431343864,
-0.579779286833981,-0.577873528946357,-0.576698059128757,-0.575388009606254,
-0.57345929734738,-0.568224880184591,-0.537165905962623,-0.488987914889991,
-0.482052090544821,-0.479220220913931,-0.477117698220485,-0.474818838034934,
-0.471643015508458,-0.464047682685806,-0.453431819894759,-0.42224030535768,
-0.384950837732984,-0.380245214903167,-0.378341230681134,-0.377166096588368,
-0.375855686179772,-0.373925163426813,-0.368678008366101,-0.360689937409051,
-0.331376765677369),.UNSPECIFIED.);
#428=B_SPLINE_CURVE_WITH_KNOTS('',3,(#25800,#25801,#25802,#25803,#25804,
#25805,#25806,#25807,#25808,#25809,#25810,#25811,#25812,#25813,#25814,#25815,
#25816,#25817,#25818,#25819,#25820,#25821,#25822,#25823,#25824,#25825,#25826,
#25827,#25828,#25829,#25830,#25831,#25832,#25833,#25834,#25835,#25836,#25837,
#25838,#25839,#25840,#25841,#25842,#25843,#25844,#25845,#25846,#25847,#25848,
#25849,#25850,#25851,#25852,#25853,#25854,#25855,#25856,#25857,#25858,#25859,
#25860,#25861,#25862,#25863,#25864,#25865,#25866,#25867,#25868,#25869,#25870,
#25871,#25872,#25873,#25874,#25875,#25876,#25877,#25878,#25879,#25880,#25881,
#25882,#25883,#25884,#25885,#25886,#25887,#25888,#25889,#25890,#25891,#25892,
#25893,#25894,#25895,#25896,#25897,#25898,#25899,#25900,#25901,#25902,#25903,
#25904,#25905,#25906,#25907,#25908,#25909,#25910,#25911,#25912,#25913,#25914,
#25915,#25916,#25917,#25918,#25919,#25920,#25921,#25922,#25923,#25924,#25925,
#25926,#25927,#25928,#25929,#25930,#25931,#25932,#25933,#25934,#25935,#25936,
#25937,#25938,#25939,#25940,#25941,#25942,#25943,#25944,#25945,#25946,#25947,
#25948,#25949,#25950,#25951,#25952,#25953),.UNSPECIFIED.,.F.,.F.,(4,2,2,
2,2,2,2,2,2,2,2,2,2,2,2,2,2,2,2,2,2,2,2,2,2,2,2,2,2,2,2,2,2,2,2,2,2,2,2,
2,2,2,2,2,2,2,2,2,2,2,2,2,2,2,2,2,2,2,2,2,2,2,2,2,2,2,2,2,2,2,2,2,2,2,2,
2,4),(-0.926782221294469,-0.896569100631809,-0.867447118673057,-0.862876094611461,
-0.860006951553309,-0.857754387215146,-0.855244096965053,-0.851066274682072,
-0.834916065147125,-0.776686390209619,-0.763443585714247,-0.760940167704961,
-0.759355947067707,-0.758098536432829,-0.756609114835076,-0.753862217391411,
-0.738514391918759,-0.691339421288076,-0.667534478572589,-0.663141365188601,
-0.660325983629374,-0.658078676370874,-0.655535052155691,-0.651206417428453,
-0.6330909157989,-0.585626792600053,-0.564456624116818,-0.561382686323562,
-0.559804384165768,-0.558547278484847,-0.557053027733001,-0.554283624801016,
-0.53842083286486,-0.486429462491141,-0.467451549432601,-0.46292553704893,
-0.460311979787076,-0.458092471214793,-0.455380709575718,-0.450269616839376,
-0.411074460894452,-0.366679149602077,-0.362463768482037,-0.360819511930875,
-0.359632481435553,-0.358333666825421,-0.356462303850262,-0.351617877119955,
-0.344438872658291,-0.32144410179083,-0.271648037273247,-0.264711303041573,
-0.261953609145812,-0.25965992714859,-0.257304879895282,-0.253844487590635,
-0.244586799371763,-0.23069623817164,-0.182930715482505,-0.179584128800173,
-0.164918984744038,-0.162342767911905,-0.160736473467934,-0.159477499261556,
-0.158004749467612,-0.155523551248057,-0.143761124602971,-0.116923019618865,
-0.0726531924634352,-0.0654919159067642,-0.0626209873586662,-0.0605082243338179,
-0.0582162528217251,-0.0550827265177684,-0.0516124903134288,-0.0403488636777721,
-0.000589815695671829),.UNSPECIFIED.);
#429=B_SPLINE_CURVE_WITH_KNOTS('',3,(#25954,#25955,#25956,#25957,#25958,
#25959),.UNSPECIFIED.,.F.,.F.,(4,1,1,4),(51.753505798748,52.2077129232575,
53.2054300868052,53.4070751110265),.UNSPECIFIED.);
#430=B_SPLINE_CURVE_WITH_KNOTS('',3,(#25961,#25962,#25963,#25964,#25965,
#25966,#25967,#25968,#25969,#25970,#25971,#25972,#25973,#25974,#25975,#25976,
#25977,#25978,#25979,#25980,#25981,#25982,#25983,#25984,#25985,#25986,#25987,
#25988,#25989,#25990,#25991,#25992,#25993,#25994,#25995,#25996,#25997,#25998,
#25999,#26000,#26001,#26002,#26003,#26004,#26005,#26006,#26007,#26008,#26009,
#26010,#26011,#26012,#26013,#26014,#26015,#26016,#26017,#26018,#26019,#26020,
#26021,#26022,#26023,#26024,#26025,#26026,#26027,#26028,#26029,#26030,#26031,
#26032),.UNSPECIFIED.,.F.,.F.,(4,2,2,2,2,2,2,2,2,2,2,2,2,2,2,2,2,2,2,2,
2,2,2,2,2,2,2,2,2,2,2,2,2,2,2,4),(-0.331376765677369,-0.309063892239683,
-0.285958208367855,-0.281592278087566,-0.278785677343909,-0.276539819396871,
-0.273991872497997,-0.269641116675965,-0.251198764775781,-0.210921638042901,
-0.183051994460163,-0.179916331687803,-0.178325200630787,-0.177067771202634,
-0.177060482826282,-0.177053263815713,-0.177046112922922,-0.177039028893918,
-0.177032010767957,-0.177025057373861,-0.177018167626151,-0.177011340628512,
-0.175534301229271,-0.172876503285918,-0.169474827828848,-0.16198886748036,
-0.137296419888448,-0.0900392263524134,-0.0830363294569277,-0.0801930047857767,
-0.0780877085930016,-0.0757913910703241,-0.0726292855006604,-0.0651159049661456,
-0.0546487482589572,-0.000590208984640202),.UNSPECIFIED.);
#431=B_SPLINE_CURVE_WITH_KNOTS('',3,(#26033,#26034,#26035,#26036,#26037,
#26038,#26039,#26040,#26041,#26042,#26043,#26044,#26045,#26046,#26047,#26048,
#26049,#26050,#26051,#26052,#26053,#26054,#26055,#26056,#26057,#26058,#26059,
#26060,#26061,#26062,#26063,#26064,#26065,#26066,#26067,#26068,#26069,#26070,
#26071,#26072,#26073,#26074,#26075,#26076,#26077,#26078,#26079,#26080,#26081,
#26082,#26083,#26084,#26085,#26086,#26087,#26088,#26089,#26090,#26091,#26092,
#26093,#26094,#26095,#26096,#26097,#26098,#26099,#26100,#26101,#26102,#26103,
#26104,#26105,#26106,#26107,#26108,#26109,#26110,#26111,#26112,#26113,#26114,
#26115,#26116,#26117,#26118,#26119,#26120,#26121,#26122,#26123,#26124,#26125,
#26126,#26127,#26128,#26129,#26130,#26131,#26132,#26133,#26134,#26135,#26136,
#26137,#26138,#26139,#26140,#26141,#26142,#26143,#26144,#26145,#26146,#26147,
#26148,#26149,#26150,#26151,#26152,#26153,#26154,#26155,#26156,#26157,#26158,
#26159,#26160,#26161,#26162,#26163,#26164,#26165,#26166,#26167,#26168,#26169,
#26170,#26171,#26172,#26173,#26174,#26175,#26176,#26177,#26178,#26179,#26180,
#26181,#26182,#26183,#26184,#26185,#26186,#26187,#26188,#26189,#26190,#26191,
#26192,#26193,#26194,#26195,#26196,#26197,#26198,#26199,#26200,#26201,#26202,
#26203,#26204,#26205,#26206,#26207,#26208,#26209,#26210,#26211,#26212,#26213,
#26214,#26215,#26216,#26217,#26218,#26219,#26220,#26221,#26222,#26223,#26224,
#26225,#26226,#26227,#26228,#26229,#26230,#26231,#26232,#26233,#26234,#26235,
#26236,#26237,#26238,#26239,#26240,#26241,#26242,#26243,#26244,#26245,#26246,
#26247,#26248,#26249,#26250,#26251,#26252,#26253,#26254,#26255,#26256,#26257,
#26258,#26259,#26260,#26261,#26262),.UNSPECIFIED.,.F.,.F.,(4,2,2,2,2,2,
2,2,2,2,2,2,2,2,2,2,2,2,2,2,2,2,2,2,2,2,2,2,2,2,2,2,2,2,2,2,2,2,2,2,2,2,
2,2,2,2,2,2,2,2,2,2,2,2,2,2,2,2,2,2,2,2,2,2,2,2,2,2,2,2,2,2,2,2,2,2,2,2,
2,2,2,2,2,2,2,2,2,2,2,2,2,2,2,2,2,2,2,2,2,2,2,2,2,2,2,2,2,2,2,2,2,2,2,2,
4),(-2.51346753526968,-2.49656179228236,-2.49424723594855,-2.49273616890078,
-2.49153253300303,-2.4904003041141,-2.48891890748557,-2.48628092833495,
-2.47467461223247,-2.46438953224031,-2.41344210935815,-2.40349461615151,
-2.39627032435406,-2.39315773071129,-2.39087061291293,-2.38875496529178,
-2.38586876956187,-2.37860980224731,-2.34044838303393,-2.30883856078443,
-2.3002571234992,-2.29651339291565,-2.29361521200013,-2.29210067622909,
-2.29209676840992,-2.29209284763182,-2.29208891390529,-2.29208496724888,
-2.292081007472,-2.29207703453806,-2.29207304832167,-2.29206904876174,-2.2920650358846,
-2.29206100947057,-2.29205696947747,-2.29205291583333,-2.29204884855905,
-2.29204476735244,-2.29204067231708,-2.29203656334953,-2.29203244024959,
-2.29202830317416,-2.29202415190499,-2.29201998627501,-2.2920158061623,
-2.29201161171023,-2.29200735585989,-2.29200303220012,-2.29199863949181,
-2.29199417644603,-2.29198964205109,-2.29198503500484,-2.29198035405605,
-2.29072396623304,-2.28914406122872,-2.28605971234948,-2.25313701549437,
-2.22819669415689,-2.20033728864931,-2.19550277604362,-2.19285044322371,
-2.19083341211432,-2.18824620332314,-2.18383126039513,-2.16634169349974,
-2.11751650752112,-2.10362146207841,-2.09841081189956,-2.0946197886711,
-2.09292436995261,-2.09165624682317,-2.09023965806498,-2.08782411721593,
-2.07918227157483,-2.06467469556245,-2.03652651853766,-2.00123953520626,
-1.99619631574526,-1.99349966870737,-1.99128187958603,-1.98865784365498,
-1.98408208799893,-1.9643599454585,-1.9131083739074,-1.89731800110081,-1.89455263350775,
-1.89305970821891,-1.89180321516825,-1.89022508306611,-1.88714975356278,
-1.86590431340644,-1.81848083834169,-1.8004494510167,-1.79612832339647,
-1.79358712837836,-1.7913407632741,-1.78852497205372,-1.78412811281269,
-1.7601943684581,-1.71311724953864,-1.69778110606826,-1.69503556125834,
-1.69354684698124,-1.69229002049101,-1.69070655582423,-1.68760642285652,
-1.66434293455431,-1.62354861643047,-1.60893761960786,-1.60244718966934,
-1.59728205236897,-1.59455970113808,-1.59231958379201,-1.58970895658841,
-1.58797213626332),.UNSPECIFIED.);
#432=B_SPLINE_CURVE_WITH_KNOTS('',3,(#26267,#26268,#26269,#26270,#26271,
#26272,#26273,#26274,#26275,#26276,#26277,#26278,#26279,#26280,#26281,#26282,
#26283,#26284,#26285,#26286,#26287,#26288,#26289,#26290,#26291,#26292,#26293,
#26294,#26295,#26296,#26297,#26298,#26299,#26300,#26301,#26302,#26303,#26304,
#26305,#26306,#26307,#26308,#26309,#26310,#26311,#26312,#26313,#26314,#26315,
#26316,#26317,#26318,#26319,#26320,#26321,#26322,#26323,#26324,#26325,#26326,
#26327,#26328,#26329,#26330,#26331,#26332,#26333,#26334,#26335,#26336,#26337,
#26338,#26339,#26340,#26341,#26342,#26343,#26344,#26345,#26346,#26347,#26348,
#26349,#26350,#26351,#26352,#26353,#26354,#26355,#26356,#26357,#26358,#26359,
#26360,#26361,#26362,#26363,#26364,#26365,#26366,#26367,#26368,#26369,#26370,
#26371,#26372,#26373,#26374,#26375,#26376,#26377,#26378,#26379,#26380,#26381,
#26382,#26383,#26384,#26385,#26386,#26387,#26388,#26389,#26390,#26391,#26392,
#26393,#26394,#26395,#26396,#26397,#26398,#26399,#26400,#26401,#26402,#26403,
#26404,#26405,#26406,#26407,#26408,#26409,#26410,#26411,#26412,#26413,#26414,
#26415,#26416,#26417,#26418,#26419,#26420,#26421,#26422,#26423,#26424,#26425,
#26426,#26427,#26428,#26429,#26430,#26431,#26432,#26433,#26434,#26435,#26436,
#26437,#26438,#26439,#26440,#26441,#26442,#26443,#26444,#26445,#26446,#26447,
#26448,#26449,#26450,#26451,#26452,#26453,#26454,#26455,#26456,#26457,#26458,
#26459,#26460,#26461,#26462,#26463,#26464,#26465,#26466,#26467,#26468,#26469,
#26470,#26471,#26472,#26473,#26474,#26475,#26476,#26477,#26478,#26479,#26480,
#26481,#26482,#26483,#26484,#26485,#26486),.UNSPECIFIED.,.F.,.F.,(4,2,2,
2,2,2,2,2,2,2,2,2,2,2,2,2,2,2,2,2,2,2,2,2,2,2,2,2,2,2,2,2,2,2,2,2,2,2,2,
2,2,2,2,2,2,2,2,2,2,2,2,2,2,2,2,2,2,2,2,2,2,2,2,2,2,2,2,2,2,2,2,2,2,2,2,
2,2,2,2,2,2,2,2,2,2,2,2,2,2,2,2,2,2,2,2,2,2,2,2,2,2,2,2,2,2,2,2,2,2,4),
(-2.18319200174337,-2.16359838216707,-2.1584116001934,-2.15648969410656,
-2.15518100271013,-2.15400424566726,-2.15209168910771,-2.14733515781527,
-2.1117026065375,-2.06598685646796,-2.05998912749124,-2.05709937449685,
-2.05484471035047,-2.05234651101395,-2.04822250514987,-2.03442145243029,
-2.02543629577283,-1.97610993079422,-1.96051859735302,-1.95776130709681,
-1.95626985859612,-1.95501288431121,-1.95343193894711,-1.95093872828567,
-1.93786949853894,-1.93007531197245,-1.87860936625802,-1.86846603671781,
-1.86113158605661,-1.85799942688707,-1.85570820926452,-1.85359596284519,
-1.85072546270073,-1.84356386857095,-1.79931583588026,-1.76201427868664,
-1.75863540324206,-1.75701699140117,-1.75575730520372,-1.75429383070465,
-1.75173592666085,-1.74120938965973,-1.68599124027133,-1.67182058774856,
-1.66237510029339,-1.65891752477938,-1.65656353706547,-1.65427022678671,
-1.65151217240877,-1.64457021923226,-1.59480995628112,-1.56498014999898,
-1.55984312005975,-1.55792842001342,-1.55662118878533,-1.55544310789001,
-1.55352343947155,-1.54872459774506,-1.51607767614575,-1.48675320837772,
-1.47243778484153,-1.4629208941717,-1.45945320627041,-1.45709700459764,
-1.45480511416044,-1.45205307667352,-1.44514971648253,-1.39499021934369,
-1.37221643280129,-1.36507931473656,-1.36025683228186,-1.35838905648669,
-1.35709114121835,-1.35590368006945,-1.35425717660693,-1.35002685272821,
-1.3057114569128,-1.27140333647857,-1.26302142366455,-1.25971968882476,
-1.25739687609636,-1.25504560822842,-1.25160198491647,-1.24225736039381,
-1.22828929603157,-1.17569161707384,-1.16249594593501,-1.1599952910368,
-1.1584119989668,-1.15715476730923,-1.15566490053829,-1.15291547138757,
-1.13750586590118,-1.08979268683339,-1.06655946222934,-1.06218820417152,
-1.05937965125502,-1.05713317268694,-1.05458552700571,-1.05023776279689,
-1.03184699280381,-0.991802722515877,-0.963657384518453,-0.96051761509897,
-0.958925407794182,-0.957667647150966,-0.956184823873192,-0.953468151099108,
-0.938770136960093,-0.926782221294469),.UNSPECIFIED.);
#433=B_SPLINE_CURVE_WITH_KNOTS('',3,(#26487,#26488,#26489,#26490,#26491,
#26492,#26493,#26494,#26495,#26496,#26497,#26498,#26499,#26500,#26501,#26502,
#26503,#26504,#26505,#26506,#26507,#26508,#26509,#26510,#26511,#26512,#26513,
#26514,#26515,#26516,#26517,#26518,#26519,#26520,#26521,#26522,#26523,#26524,
#26525,#26526,#26527,#26528,#26529,#26530,#26531,#26532,#26533,#26534,#26535,
#26536,#26537,#26538,#26539,#26540,#26541,#26542,#26543,#26544,#26545,#26546,
#26547,#26548,#26549,#26550,#26551,#26552,#26553,#26554,#26555,#26556,#26557,
#26558,#26559,#26560,#26561,#26562,#26563,#26564,#26565,#26566,#26567,#26568,
#26569,#26570,#26571,#26572,#26573,#26574,#26575,#26576,#26577,#26578,#26579,
#26580,#26581,#26582,#26583,#26584,#26585,#26586,#26587,#26588,#26589,#26590,
#26591,#26592,#26593,#26594,#26595,#26596,#26597,#26598,#26599,#26600,#26601,
#26602,#26603,#26604,#26605,#26606,#26607,#26608,#26609,#26610,#26611,#26612,
#26613,#26614,#26615,#26616,#26617,#26618,#26619,#26620,#26621,#26622,#26623,
#26624,#26625,#26626,#26627,#26628,#26629,#26630,#26631,#26632,#26633,#26634,
#26635,#26636,#26637,#26638,#26639,#26640,#26641,#26642,#26643,#26644,#26645,
#26646,#26647,#26648,#26649,#26650,#26651,#26652,#26653,#26654,#26655,#26656,
#26657,#26658,#26659,#26660,#26661,#26662,#26663,#26664,#26665,#26666,#26667,
#26668,#26669,#26670,#26671,#26672,#26673,#26674,#26675,#26676,#26677,#26678,
#26679,#26680,#26681,#26682,#26683,#26684,#26685,#26686,#26687,#26688,#26689,
#26690,#26691,#26692,#26693,#26694,#26695,#26696),.UNSPECIFIED.,.F.,.F.,
(4,2,2,2,2,2,2,2,2,2,2,2,2,2,2,2,2,2,2,2,2,2,2,2,2,2,2,2,2,2,2,2,2,2,2,
2,2,2,2,2,2,2,2,2,2,2,2,2,2,2,2,2,2,2,2,2,2,2,2,2,2,2,2,2,2,2,2,2,2,2,2,
2,2,2,2,2,2,2,2,2,2,2,2,2,2,2,2,2,2,2,2,2,2,2,2,2,2,2,2,2,2,2,2,2,4),(-1.58797213626332,
-1.5851929007491,-1.5663422844173,-1.51419113504517,-1.49831169608799,-1.49554225745563,
-1.49404834616904,-1.49279174156747,-1.49121437593086,-1.48814317787937,
-1.46703177656211,-1.41614769494923,-1.40097955905269,-1.39688603160707,
-1.39439474632506,-1.39213887207933,-1.38923716471809,-1.38455625656101,
-1.34767100094664,-1.31220497116264,-1.29859999805051,-1.2959386080392,
-1.29446795206325,-1.29320937908204,-1.29160184711831,-1.28902033922292,
-1.27422728704706,-1.2704075810326,-1.25750066205839,-1.20583112652477,
-1.19976368995687,-1.19646809061598,-1.19417002883725,-1.19182259665336,
-1.18839578697113,-1.17916635650738,-1.12562321929112,-1.09988575134419,
-1.09675565798519,-1.09516571459432,-1.09390836805184,-1.09242444874957,
-1.08970172541419,-1.07486675030426,-1.03169035384809,-1.00362467498763,
-0.999084627258315,-0.996225166722573,-0.993974121173912,-0.991459211339525,
-0.98725874516619,-0.970822265571422,-0.909425777807314,-0.899269227848342,
-0.896741808908697,-0.895285306637434,-0.894036620311793,-0.892414479487631,
-0.889016543084278,-0.859688219414146,-0.806342908280219,-0.79989390930073,
-0.796904624741144,-0.794628474582261,-0.792199789842373,-0.788392523505356,
-0.776131794161726,-0.755719113906674,-0.723641362493661,-0.717161664297247,
-0.710306326389501,-0.699775968838783,-0.697217776842032,-0.695754280985651,
-0.694494670686153,-0.692876520728066,-0.689498760586868,-0.65523219478018,
-0.607696342518147,-0.600711970852484,-0.597871687747316,-0.595767030877307,
-0.59346984196221,-0.590303667014539,-0.582766833567633,-0.572257412688759,
-0.5416056563801,-0.52126461190133,-0.514076782525264,-0.500608793142929,
-0.498093774263695,-0.496506300997038,-0.495249084389736,-0.493763178101448,
-0.491031291730914,-0.476000215818838,-0.431365170330414,-0.404886988352848,
-0.400388542027565,-0.397541633132385,-0.395291889687219,-0.39276946027005,
-0.388534951295831,-0.371669015387297,-0.331262636501411),.UNSPECIFIED.);
#434=B_SPLINE_CURVE_WITH_KNOTS('',3,(#26702,#26703,#26704,#26705,#26706,
#26707,#26708,#26709,#26710),.UNSPECIFIED.,.F.,.F.,(4,1,1,1,1,1,4),(65.9734457253857,
66.1757532129241,67.1734703764717,68.1711875400193,69.1689047035669,70.1666218671145,
70.6036277493768),.UNSPECIFIED.);
#435=B_SPLINE_CURVE_WITH_KNOTS('',3,(#26711,#26712,#26713,#26714,#26715,
#26716,#26717,#26718,#26719,#26720,#26721,#26722,#26723,#26724,#26725,#26726,
#26727,#26728,#26729,#26730,#26731,#26732,#26733,#26734,#26735,#26736,#26737,
#26738,#26739,#26740,#26741,#26742,#26743,#26744,#26745,#26746,#26747,#26748,
#26749,#26750,#26751,#26752,#26753,#26754,#26755,#26756,#26757,#26758,#26759,
#26760,#26761,#26762,#26763,#26764,#26765,#26766),.UNSPECIFIED.,.F.,.F.,
(4,2,2,2,2,2,2,2,2,2,2,2,2,2,2,2,2,2,2,2,2,2,2,2,2,2,2,4),(-2.51394155306699,
-2.466637600994,-2.4617427397929,-2.45762045848769,-2.45512266136964,-2.45286794636516,
-2.44997755319159,-2.44533497805284,-2.40601539242209,-2.38392710713627,
-2.36049431156025,-2.35724775535317,-2.35593199396106,-2.3546288135796,
-2.35344713167725,-2.35150779911278,-2.34659141335136,-2.30853132004468,
-2.27817622236129,-2.26772679171622,-2.2602956332158,-2.25710544234426,
-2.25480391126825,-2.25270422506788,-2.24988409942968,-2.2430165150615,
-2.19405343286759,-2.18319200174337),.UNSPECIFIED.);
#436=B_SPLINE_CURVE_WITH_KNOTS('',3,(#26768,#26769,#26770,#26771,#26772,
#26773,#26774,#26775,#26776,#26777,#26778,#26779,#26780,#26781,#26782,#26783,
#26784,#26785,#26786,#26787,#26788,#26789,#26790,#26791,#26792,#26793,#26794,
#26795,#26796,#26797,#26798,#26799,#26800,#26801,#26802,#26803,#26804,#26805,
#26806,#26807,#26808,#26809,#26810,#26811,#26812,#26813,#26814,#26815,#26816,
#26817,#26818,#26819,#26820,#26821,#26822,#26823,#26824,#26825,#26826,#26827,
#26828,#26829,#26830,#26831,#26832,#26833,#26834,#26835,#26836,#26837,#26838,
#26839,#26840,#26841,#26842,#26843,#26844,#26845,#26846,#26847,#26848,#26849,
#26850,#26851,#26852,#26853,#26854,#26855,#26856,#26857,#26858,#26859),
 .UNSPECIFIED.,.F.,.F.,(4,2,2,2,2,2,2,2,2,2,2,2,2,2,2,2,2,2,2,2,2,2,2,2,
2,2,2,2,2,2,2,2,2,2,2,2,2,2,2,2,2,2,2,2,2,4),(-0.331262636501411,-0.312537078033625,
-0.300832996363419,-0.298187411773189,-0.296703916745071,-0.295446313583396,
-0.293855270118835,-0.290615749906918,-0.286356679162698,-0.276030209491528,
-0.228465125088051,-0.205056141648706,-0.200292075512775,-0.197657880779281,
-0.195582052980325,-0.195490067650667,-0.195407293701803,-0.195331674364844,
-0.195261724972701,-0.195196335329914,-0.195134650617439,-0.195075995992206,
-0.195019826822999,-0.194965694784247,-0.194913223937621,-0.194862093538244,
-0.194812025352817,-0.194762774111738,-0.19471412011704,-0.194665863532038,
-0.191834663234259,-0.185628295894901,-0.161570327181278,-0.120953101159568,
-0.116450037651974,-0.101616979484438,-0.099033135339379,-0.0974247572295934,
-0.096165915090873,-0.0946953889985359,-0.0920353584835478,-0.0784614972025078,
-0.0467598687421659,-0.00940609176814624,-0.00362882690152282,-0.000621359024833994),
 .UNSPECIFIED.);
#437=B_SPLINE_CURVE_WITH_KNOTS('',3,(#26860,#26861,#26862,#26863,#26864,
#26865,#26866,#26867,#26868),.UNSPECIFIED.,.F.,.F.,(4,1,1,1,1,1,4),(65.9734457253857,
66.4908371924601,67.4885543560077,68.4862715195553,69.4839886831029,70.4817058466505,
70.6039745846252),.UNSPECIFIED.);
#438=B_SPLINE_CURVE_WITH_KNOTS('',3,(#26874,#26875,#26876,#26877,#26878,
#26879,#26880,#26881,#26882,#26883,#26884,#26885,#26886,#26887,#26888,#26889,
#26890,#26891,#26892,#26893,#26894,#26895,#26896,#26897,#26898,#26899,#26900,
#26901,#26902,#26903,#26904,#26905,#26906,#26907,#26908,#26909,#26910,#26911,
#26912,#26913,#26914,#26915,#26916,#26917,#26918,#26919,#26920,#26921,#26922,
#26923,#26924,#26925,#26926,#26927,#26928,#26929,#26930,#26931,#26932,#26933,
#26934,#26935,#26936,#26937,#26938,#26939,#26940,#26941,#26942,#26943,#26944,
#26945,#26946,#26947,#26948,#26949,#26950,#26951,#26952,#26953,#26954,#26955,
#26956,#26957,#26958,#26959,#26960,#26961,#26962,#26963,#26964,#26965,#26966,
#26967,#26968,#26969,#26970,#26971,#26972,#26973,#26974,#26975,#26976,#26977,
#26978,#26979,#26980,#26981,#26982,#26983,#26984,#26985,#26986,#26987,#26988,
#26989,#26990,#26991,#26992,#26993,#26994,#26995,#26996,#26997,#26998,#26999,
#27000,#27001,#27002,#27003,#27004,#27005,#27006,#27007,#27008,#27009,#27010,
#27011,#27012),.UNSPECIFIED.,.F.,.F.,(4,3,3,3,3,3,3,3,3,3,3,3,3,3,3,3,3,
3,3,3,3,3,3,3,3,3,3,3,3,3,3,3,3,3,3,3,3,3,3,3,3,3,3,3,3,3,4),(72.2566313142932,
72.3602645627545,72.4637412961988,72.567131952733,72.670473758299,72.7738038687084,
72.8772298862312,72.9807049395385,73.0843641198611,73.1597733577573,73.2647320310558,
73.3695332432659,73.474211236588,73.5788234142111,73.6834053394952,73.7879925318276,
73.8926903737461,73.9974494450646,74.1023905972613,74.157490521305,74.2624491946034,
74.3672504068134,74.4719284001355,74.5765405777585,74.6811225030425,74.7857096953747,
74.8904075372932,74.9951666086117,75.1001077608083,75.1552076848526,75.2601663581511,
75.3649675703609,75.469645563683,75.5742577413061,75.6788396665902,75.783426858922,
75.8881247008404,75.9928837721588,76.0978249243555,76.1529248484002,76.2578569199746,
76.3626439379309,76.4673216974341,76.5719713509118,76.6765579426452,76.7812391269951,
76.8859203113449),.UNSPECIFIED.);
#439=B_SPLINE_CURVE_WITH_KNOTS('',3,(#27013,#27014,#27015,#27016,#27017,
#27018),.UNSPECIFIED.,.F.,.F.,(4,1,1,4),(70.6036277493768,71.1643390306621,
72.1620561942097,72.2566310325653),.UNSPECIFIED.);
#440=B_SPLINE_CURVE_WITH_KNOTS('',3,(#27020,#27021,#27022,#27023,#27024),
 .UNSPECIFIED.,.F.,.F.,(4,1,4),(70.6039745846252,71.4794230101981,72.2566298138773),
 .UNSPECIFIED.);
#441=B_SPLINE_CURVE_WITH_KNOTS('',3,(#27025,#27026,#27027,#27028,#27029,
#27030,#27031,#27032,#27033,#27034,#27035,#27036,#27037,#27038,#27039,#27040,
#27041,#27042,#27043,#27044,#27045,#27046,#27047,#27048,#27049,#27050,#27051,
#27052,#27053,#27054,#27055,#27056,#27057,#27058,#27059,#27060,#27061,#27062,
#27063,#27064,#27065,#27066,#27067,#27068,#27069,#27070,#27071,#27072,#27073,
#27074,#27075,#27076,#27077,#27078,#27079,#27080,#27081,#27082,#27083,#27084,
#27085,#27086,#27087,#27088,#27089,#27090,#27091,#27092,#27093,#27094,#27095,
#27096,#27097,#27098,#27099,#27100,#27101,#27102,#27103,#27104,#27105,#27106,
#27107,#27108,#27109,#27110,#27111,#27112,#27113,#27114,#27115,#27116,#27117,
#27118,#27119,#27120,#27121,#27122,#27123,#27124,#27125,#27126,#27127,#27128,
#27129,#27130,#27131,#27132,#27133,#27134,#27135,#27136,#27137,#27138,#27139,
#27140,#27141,#27142,#27143,#27144,#27145,#27146,#27147,#27148,#27149,#27150,
#27151,#27152,#27153,#27154,#27155,#27156,#27157,#27158,#27159,#27160,#27161,
#27162,#27163,#27164,#27165,#27166,#27167,#27168,#27169,#27170,#27171,#27172,
#27173,#27174,#27175,#27176,#27177,#27178,#27179,#27180,#27181,#27182,#27183,
#27184,#27185,#27186,#27187,#27188,#27189,#27190),.UNSPECIFIED.,.F.,.F.,
(4,2,2,2,2,2,2,2,2,2,2,2,2,2,2,2,2,2,2,2,2,2,2,2,2,2,2,2,2,2,2,2,2,2,2,
2,2,2,2,2,2,2,2,2,2,2,2,2,2,2,2,2,2,2,2,2,2,2,2,2,2,2,2,2,2,2,2,2,2,2,2,
2,2,2,2,2,2,2,2,2,2,2,4),(-2.51330016705752,-2.47991256274182,-2.47529421864695,
-2.4728770419069,-2.47132370811844,-2.4698596046738,-2.46860064517186,-2.4669848530403,
-2.46437511981821,-2.44905909909445,-2.43145075979571,-2.40980862070163,
-2.38441020802264,-2.37554419845501,-2.37294406094825,-2.37043126395865,
-2.36818048880956,-2.36531915807952,-2.36077166539362,-2.33242979206749,
-2.29028115258029,-2.27985543836915,-2.27556886743201,-2.27238212011941,
-2.27076428981524,-2.26951646673672,-2.26805808971772,-2.26552097690678,
-2.25524029574819,-2.19403330477267,-2.18319928172661,-2.17548453064293,
-2.17228976555339,-2.16998810430565,-2.16789046670598,-2.16454458651877,
-2.15828727472907,-2.10862815690352,-2.07872439634806,-2.07358234294318,
-2.07166740114468,-2.07036050990824,-2.06918313579971,-2.06726539847066,
-2.0624752654823,-2.03120494517,-2.00474676260167,-1.98139779817127,-1.97528812501293,
-1.97237746645103,-1.97012089964132,-1.96763517933785,-1.96356529556603,
-1.95025468714898,-1.94074376402126,-1.89135754142829,-1.87576111808876,
-1.8730042864536,-1.87151325004914,-1.87025672840254,-1.86867651365306,
-1.86559114622134,-1.84390124485284,-1.80799875526818,-1.78930432285737,
-1.78162123549416,-1.77571718100365,-1.77284603762069,-1.77059403159059,
-1.76808656862234,-1.76391866536552,-1.74969554545172,-1.74008836109247,
-1.69176924791012,-1.68138250321778,-1.67502498943512,-1.67294800552402,
-1.67160635405697,-1.67031862047412,-1.66843544979252,-1.66385338009683,
-1.62422138514652,-1.58784062522319),.UNSPECIFIED.);
#442=B_SPLINE_CURVE_WITH_KNOTS('',3,(#27196,#27197,#27198,#27199,#27200,
#27201,#27202,#27203,#27204,#27205,#27206,#27207,#27208,#27209,#27210,#27211,
#27212,#27213,#27214,#27215,#27216,#27217,#27218,#27219,#27220,#27221,#27222,
#27223,#27224,#27225,#27226,#27227,#27228,#27229,#27230,#27231,#27232,#27233,
#27234,#27235,#27236,#27237,#27238,#27239,#27240,#27241,#27242,#27243,#27244,
#27245,#27246,#27247,#27248,#27249,#27250,#27251,#27252,#27253,#27254,#27255,
#27256,#27257,#27258,#27259,#27260,#27261,#27262,#27263,#27264,#27265,#27266,
#27267,#27268,#27269,#27270,#27271,#27272,#27273,#27274,#27275,#27276,#27277,
#27278,#27279,#27280,#27281,#27282,#27283,#27284,#27285,#27286,#27287,#27288,
#27289,#27290,#27291,#27292,#27293,#27294,#27295,#27296,#27297,#27298,#27299,
#27300,#27301,#27302,#27303,#27304,#27305,#27306,#27307,#27308,#27309,#27310,
#27311,#27312,#27313,#27314,#27315,#27316,#27317,#27318,#27319,#27320,#27321,
#27322,#27323,#27324,#27325,#27326,#27327,#27328,#27329,#27330,#27331,#27332,
#27333,#27334,#27335,#27336,#27337,#27338,#27339,#27340,#27341,#27342,#27343,
#27344,#27345,#27346,#27347,#27348,#27349,#27350,#27351,#27352,#27353,#27354,
#27355,#27356,#27357,#27358,#27359,#27360,#27361,#27362,#27363,#27364,#27365,
#27366,#27367),.UNSPECIFIED.,.F.,.F.,(4,2,2,2,2,2,2,2,2,2,2,2,2,2,2,2,2,
2,2,2,2,2,2,2,2,2,2,2,2,2,2,2,2,2,2,2,2,2,2,2,2,2,2,2,2,2,2,2,2,2,2,2,2,
2,2,2,2,2,2,2,2,2,2,2,2,2,2,2,2,2,2,2,2,2,2,2,2,2,2,2,2,2,2,2,2,4),(-0.926807318156856,
-0.925373376894712,-0.922713571027084,-0.921082197429211,-0.919820983452259,
-0.918365503869921,-0.915775850211289,-0.90345491509868,-0.874298322310961,
-0.833079534301998,-0.825834080675445,-0.822948939119945,-0.820832544766051,
-0.818543164258394,-0.815424891538882,-0.80817547098942,-0.798184089328335,
-0.747211001922924,-0.726077872881513,-0.723004874505717,-0.721426667831066,
-0.720169431854571,-0.718674782275535,-0.715903998226448,-0.700014398287469,
-0.647755460227258,-0.6290304993301,-0.624521689505782,-0.621911878994728,
-0.619670455078301,-0.61694400867495,-0.611763386103654,-0.566763233892935,
-0.528911052604525,-0.524235744475249,-0.522336329847796,-0.521161656910474,
-0.519849451286753,-0.517912226725937,-0.512621818685951,-0.504546114369096,
-0.451475453742175,-0.443037867787702,-0.428727097014748,-0.424548478078506,
-0.422037670582143,-0.419784616041472,-0.416914813247638,-0.41102309633798,
-0.369520376990956,-0.329162402132365,-0.324603233221116,-0.322909765846531,
-0.32170959020882,-0.320421249380948,-0.318605707999499,-0.314117460590152,
-0.291589075693152,-0.282497019545978,-0.233799987062063,-0.226907837373905,
-0.22408277986961,-0.221981296203417,-0.219725598053063,-0.21664096372067,
-0.213179056558184,-0.207203429930074,-0.1942258004651,-0.147710486661316,
-0.139797729375172,-0.126759667223844,-0.124267477631899,-0.122686546961463,
-0.121429143446021,-0.119936657983165,-0.117176084710195,-0.101525116676944,
-0.0480775700168125,-0.0330517577391862,-0.0268002465373971,-0.0238929708442883,
-0.0216289297483238,-0.019528173283468,-0.0171074106056456,-0.0136712472908266,
-0.000589101730667486),.UNSPECIFIED.);
#443=B_SPLINE_CURVE_WITH_KNOTS('',3,(#27368,#27369,#27370,#27371,#27372,
#27373,#27374,#27375,#27376,#27377,#27378,#27379,#27380,#27381,#27382,#27383,
#27384,#27385,#27386,#27387,#27388,#27389,#27390,#27391,#27392,#27393,#27394,
#27395,#27396,#27397,#27398,#27399,#27400,#27401,#27402,#27403,#27404,#27405,
#27406,#27407,#27408,#27409,#27410,#27411,#27412,#27413,#27414,#27415,#27416,
#27417,#27418,#27419),.UNSPECIFIED.,.F.,.F.,(4,3,3,3,3,3,3,3,3,3,3,3,3,
3,3,3,3,4),(76.8859203113449,76.9906794404996,77.095620626684,77.1506420119478,
77.2556006852461,77.3604018974561,77.4650798907783,77.5696920684015,77.6742739936856,
77.7788611860176,77.8835590279362,77.9883180992548,78.0932592514514,78.1483591754954,
78.2655869204099,78.382405937241,78.4985506711647,78.5398163393789),
 .UNSPECIFIED.);
#444=B_SPLINE_CURVE_WITH_KNOTS('',3,(#27420,#27421,#27422,#27423,#27424,
#27425,#27426,#27427,#27428,#27429,#27430,#27431,#27432,#27433,#27434,#27435,
#27436,#27437,#27438,#27439,#27440,#27441,#27442,#27443,#27444,#27445,#27446,
#27447,#27448,#27449,#27450,#27451,#27452,#27453,#27454,#27455,#27456,#27457,
#27458,#27459,#27460,#27461,#27462,#27463,#27464,#27465,#27466,#27467,#27468,
#27469,#27470,#27471,#27472,#27473,#27474,#27475,#27476,#27477,#27478,#27479,
#27480,#27481,#27482,#27483,#27484,#27485,#27486,#27487,#27488,#27489,#27490,
#27491,#27492,#27493,#27494,#27495,#27496,#27497,#27498,#27499,#27500,#27501,
#27502,#27503,#27504,#27505,#27506,#27507,#27508,#27509,#27510,#27511,#27512,
#27513,#27514,#27515,#27516,#27517,#27518,#27519,#27520,#27521,#27522,#27523,
#27524,#27525,#27526,#27527,#27528,#27529,#27530,#27531,#27532,#27533,#27534,
#27535,#27536,#27537,#27538,#27539,#27540,#27541,#27542,#27543,#27544,#27545,
#27546,#27547,#27548,#27549,#27550,#27551,#27552,#27553,#27554,#27555,#27556,
#27557,#27558,#27559,#27560,#27561,#27562,#27563,#27564,#27565,#27566,#27567,
#27568,#27569,#27570,#27571,#27572,#27573,#27574,#27575,#27576,#27577,#27578,
#27579,#27580,#27581,#27582,#27583,#27584,#27585,#27586,#27587,#27588,#27589,
#27590,#27591,#27592,#27593,#27594,#27595,#27596,#27597,#27598,#27599,#27600,
#27601,#27602,#27603,#27604,#27605,#27606,#27607,#27608,#27609,#27610,#27611,
#27612,#27613,#27614,#27615,#27616,#27617,#27618,#27619,#27620,#27621,#27622,
#27623,#27624,#27625,#27626,#27627,#27628,#27629,#27630,#27631,#27632,#27633,
#27634,#27635,#27636,#27637,#27638,#27639,#27640,#27641,#27642,#27643),
 .UNSPECIFIED.,.F.,.F.,(4,2,2,2,2,2,2,2,2,2,2,2,2,2,2,2,2,2,2,2,2,2,2,2,
2,2,2,2,2,2,2,2,2,2,2,2,2,2,2,2,2,2,2,2,2,2,2,2,2,2,2,2,2,2,2,2,2,2,2,2,
2,2,2,2,2,2,2,2,2,2,2,2,2,2,2,2,2,2,2,2,2,2,2,2,2,2,2,2,2,2,2,2,2,2,2,2,
2,2,2,2,2,2,2,2,2,2,2,2,2,2,2,4),(-1.58784062522319,-1.58221103954342,-1.57624379253658,
-1.57336030004944,-1.57110678889273,-1.5686060511992,-1.56446898299355,
-1.55054031333842,-1.5403996123742,-1.48844940522033,-1.48044057016584,
-1.47518385362657,-1.47325207147764,-1.47194149333888,-1.47076672597767,
-1.4688643037845,-1.46416735823224,-1.42685748453031,-1.39571037012948,
-1.3796441492217,-1.37547399866116,-1.37296582418165,-1.3707135833922,-1.36784269676348,
-1.36326452976911,-1.3338661568848,-1.28269358222039,-1.27823077797614,
-1.27487063935757,-1.2732559658949,-1.27199671755082,-1.27053092911233,
-1.26796255187546,-1.25730409551706,-1.23402934605179,-1.18466678326279,
-1.17768802828592,-1.17492424917217,-1.1726295664007,-1.17027763960127,
-1.16682955455234,-1.15745100760379,-1.14341407555502,-1.09000305083113,
-1.07762655782137,-1.07517309973763,-1.07360431720513,-1.07234799098609,
-1.07084660405032,-1.06804254251476,-1.05131907054971,-1.02219495066418,
-0.9823059764507,-0.977656020347348,-0.974763331421145,-0.972508259456574,
-0.970011535578737,-0.965894451670222,-0.950461926067842,-0.898434063152091,
-0.892358085407629,-0.878254646857698,-0.875706396014921,-0.874108733593552,
-0.872850670815167,-0.871372190868561,-0.868675453697037,-0.854386645095842,
-0.83379807270375,-0.785706357108745,-0.77876249055942,-0.775929036702919,
-0.773825952992545,-0.771527079904415,-0.768352342853144,-0.760764958496427,
-0.750163951228377,-0.71905093550358,-0.681637270713771,-0.676937307973491,
-0.67503413336087,-0.673859046308614,-0.672548249224625,-0.670616392034461,
-0.665360920851439,-0.657356160705935,-0.605467264792169,-0.595107241660825,
-0.581320178577621,-0.577197514745334,-0.574699536054711,-0.572444695775254,
-0.569554203330038,-0.563553117135836,-0.519029241755175,-0.482077028959812,
-0.477362993831511,-0.475457459290951,-0.474281934789479,-0.472971637895728,
-0.471042237212878,-0.465803971318245,-0.434699629213652,-0.386567694011509,
-0.379627406296936,-0.376794578242346,-0.374691656841344,-0.372392666182983,
-0.369217224770673,-0.361625527917048,-0.351016654667816,-0.331163854026367),
 .UNSPECIFIED.);
#445=B_SPLINE_CURVE_WITH_KNOTS('',3,(#27648,#27649,#27650,#27651,#27652,
#27653,#27654,#27655,#27656,#27657,#27658,#27659,#27660,#27661,#27662,#27663,
#27664,#27665,#27666,#27667,#27668,#27669,#27670,#27671,#27672,#27673,#27674,
#27675,#27676,#27677,#27678,#27679,#27680,#27681,#27682,#27683,#27684,#27685,
#27686,#27687,#27688,#27689,#27690,#27691,#27692,#27693,#27694,#27695,#27696,
#27697,#27698,#27699,#27700,#27701,#27702,#27703,#27704,#27705,#27706,#27707,
#27708,#27709,#27710,#27711,#27712,#27713,#27714,#27715,#27716,#27717,#27718,
#27719,#27720,#27721,#27722,#27723,#27724,#27725,#27726,#27727,#27728,#27729,
#27730,#27731,#27732,#27733,#27734,#27735,#27736,#27737,#27738,#27739,#27740,
#27741,#27742,#27743,#27744,#27745,#27746,#27747,#27748,#27749,#27750,#27751,
#27752,#27753,#27754,#27755,#27756,#27757,#27758,#27759,#27760,#27761,#27762,
#27763,#27764,#27765,#27766,#27767,#27768,#27769,#27770,#27771,#27772,#27773,
#27774,#27775,#27776,#27777,#27778,#27779,#27780,#27781,#27782,#27783,#27784,
#27785,#27786,#27787,#27788,#27789,#27790,#27791,#27792,#27793,#27794,#27795,
#27796,#27797,#27798,#27799,#27800,#27801,#27802,#27803,#27804,#27805,#27806,
#27807,#27808,#27809,#27810,#27811,#27812,#27813,#27814,#27815,#27816,#27817,
#27818,#27819,#27820,#27821,#27822,#27823,#27824,#27825,#27826,#27827,#27828,
#27829,#27830,#27831,#27832,#27833,#27834,#27835,#27836,#27837,#27838,#27839,
#27840,#27841,#27842,#27843,#27844,#27845,#27846,#27847,#27848,#27849,#27850,
#27851),.UNSPECIFIED.,.F.,.F.,(4,2,2,2,2,2,2,2,2,2,2,2,2,2,2,2,2,2,2,2,
2,2,2,2,2,2,2,2,2,2,2,2,2,2,2,2,2,2,2,2,2,2,2,2,2,2,2,2,2,2,2,2,2,2,2,2,
2,2,2,2,2,2,2,2,2,2,2,2,2,2,2,2,2,2,2,2,2,2,2,2,2,2,2,2,2,2,2,2,2,2,2,2,
2,2,2,2,2,2,2,2,2,4),(-2.18351281682041,-2.18101681610237,-2.1372290852562,
-2.12230855412162,-2.11958131522797,-2.11809621566542,-2.11683862965526,
-2.11524933235074,-2.11212331065142,-2.08108951867406,-2.04334702308628,
-2.02549204063445,-2.02118247014029,-2.01864315334134,-2.01639543379035,
-2.01357392767378,-2.00916030230868,-1.98481735473266,-1.94652470527624,
-1.92531954767722,-1.9209651494158,-1.91917173531293,-1.91788759929618,
-1.91668201002598,-1.9146197520273,-1.90890717017128,-1.86602816708059,
-1.82738618997019,-1.82228356652633,-1.81957374242647,-1.81735452457443,
-1.81473979965965,-1.81020797347806,-1.79114276621091,-1.73921311664175,
-1.723353900045,-1.720584705783,-1.7190905623037,-1.7178335390829,-1.71625533803371,
-1.71318159035454,-1.69201279303018,-1.64100155323564,-1.63108288676515,
-1.62387392809614,-1.62076290641904,-1.61847505178503,-1.61635738373742,
-1.61290670811308,-1.6042227764439,-1.54679198967744,-1.5313036791489,-1.52570400233818,
-1.5216955570262,-1.51996082054256,-1.51868632399239,-1.51728732222685,
-1.51495338261783,-1.5070907376698,-1.44322790731788,-1.42660968236939,
-1.42239416762734,-1.41987559198117,-1.41762460781561,-1.41476976814698,
-1.41024606415742,-1.38274738846111,-1.33902026916804,-1.32410781823506,
-1.32138092997059,-1.31989589425515,-1.31863828554251,-1.3170488618652,
-1.31452805404872,-1.30095653388421,-1.294006931938,-1.25769731442286,-1.22865277151619,
-1.22408373627076,-1.22121511994126,-1.2189625206458,-1.21645172735011,
-1.21227197191485,-1.19609988066308,-1.13765288145582,-1.12462434190597,
-1.12213286299651,-1.12055223188168,-1.11929496323575,-1.11780251585233,
-1.1150416935152,-1.0993801385356,-1.04939480462388,-1.02844500712769,-1.02419649919778,
-1.02142533428652,-1.0191815040607,-1.016607034876,-1.0121377570243,-0.991906648634121,
-0.941860362376527,-0.926807318156856),.UNSPECIFIED.);
#446=B_SPLINE_CURVE_WITH_KNOTS('',3,(#27853,#27854,#27855,#27856,#27857,
#27858,#27859,#27860,#27861,#27862,#27863,#27864,#27865,#27866,#27867,#27868,
#27869,#27870,#27871,#27872,#27873,#27874,#27875,#27876,#27877,#27878,#27879,
#27880,#27881,#27882,#27883,#27884,#27885,#27886,#27887,#27888,#27889,#27890,
#27891,#27892,#27893,#27894,#27895,#27896,#27897,#27898,#27899,#27900,#27901,
#27902,#27903,#27904,#27905,#27906,#27907,#27908,#27909,#27910),
 .UNSPECIFIED.,.F.,.F.,(4,2,2,2,2,2,2,2,2,2,2,2,2,2,2,2,2,2,2,2,2,2,2,2,
2,2,2,2,4),(-0.331163854026367,-0.319863441156325,-0.282506835646621,-0.277805204671239,
-0.275901757877679,-0.274726626002702,-0.273415898471444,-0.271484352001104,
-0.26623100329555,-0.258230573221689,-0.206412150061396,-0.183470942609572,
-0.179123961518021,-0.176322980558378,-0.174077374758578,-0.171620148404089,
-0.167481878800948,-0.162478015590372,-0.152386304442785,-0.125059925231917,
-0.0825698578329224,-0.0781441494796792,-0.0764693740893651,-0.0752744619194422,
-0.0739829355785006,-0.0721483906077727,-0.0675390301218784,-0.0437529782176269,
-0.000590121595483474),.UNSPECIFIED.);
#447=B_SPLINE_CURVE_WITH_KNOTS('',3,(#27911,#27912,#27913,#27914,#27915,
#27916,#27917,#27918,#27919,#27920,#27921,#27922,#27923,#27924,#27925,#27926,
#27927,#27928,#27929,#27930,#27931,#27932,#27933,#27934,#27935,#27936,#27937,
#27938,#27939,#27940,#27941,#27942,#27943,#27944,#27945,#27946,#27947,#27948,
#27949,#27950,#27951,#27952,#27953,#27954,#27955,#27956,#27957,#27958,#27959,
#27960,#27961,#27962,#27963,#27964,#27965,#27966,#27967,#27968,#27969,#27970,
#27971,#27972,#27973,#27974,#27975,#27976,#27977,#27978,#27979,#27980,#27981,
#27982,#27983,#27984,#27985,#27986,#27987,#27988,#27989,#27990,#27991,#27992,
#27993,#27994,#27995,#27996,#27997,#27998,#27999,#28000,#28001,#28002,#28003,
#28004,#28005,#28006,#28007,#28008,#28009,#28010,#28011,#28012,#28013,#28014,
#28015,#28016,#28017,#28018,#28019,#28020,#28021,#28022,#28023,#28024,#28025,
#28026,#28027,#28028,#28029,#28030,#28031,#28032,#28033,#28034,#28035,#28036,
#28037,#28038,#28039,#28040,#28041,#28042,#28043,#28044,#28045,#28046,#28047,
#28048,#28049,#28050,#28051,#28052,#28053,#28054,#28055,#28056,#28057,#28058,
#28059,#28060,#28061,#28062,#28063,#28064,#28065,#28066,#28067,#28068,#28069,
#28070,#28071,#28072,#28073,#28074,#28075,#28076,#28077,#28078,#28079,#28080,
#28081,#28082,#28083,#28084,#28085,#28086,#28087,#28088,#28089,#28090,#28091,
#28092),.UNSPECIFIED.,.F.,.F.,(4,2,2,2,2,2,2,2,2,2,2,2,2,2,2,2,2,2,2,2,
2,2,2,2,2,2,2,2,2,2,2,2,2,2,2,2,2,2,2,2,2,2,2,2,2,2,2,2,2,2,2,2,2,2,2,2,
2,2,2,2,2,2,2,2,2,2,2,2,2,2,2,2,2,2,2,2,2,2,2,2,2,2,2,2,2,2,2,2,2,2,4),
(-2.51353945094856,-2.50220186507432,-2.49527542065432,-2.4923592038255,
-2.4901372269883,-2.48799464166275,-2.48587512033717,-2.48240866365923,
-2.47361280374915,-2.45880492184982,-2.40618900205649,-2.39313758226095,
-2.3905069447287,-2.38904325567487,-2.38778433848214,-2.38616819344917,
-2.38355710255715,-2.36822767398951,-2.31716309211462,-2.30372540991668,
-2.2976034428148,-2.29271602857679,-2.29006856305797,-2.29004487329658,
-2.2900206881505,-2.28999599511909,-2.28997078131414,-2.28994503347818,
-2.28991873800238,-2.28789976666376,-2.28529951635349,-2.28082673225287,
-2.26259338861597,-2.20983409160828,-2.1939004978952,-2.19112940705993,
-2.18963541990004,-2.18837923418689,-2.18680300330163,-2.1837357838108,
-2.16272443384726,-2.11187846482913,-2.09661162278341,-2.09251027500257,
-2.0900177539398,-2.08776303461586,-2.08486599196874,-2.08019913913287,
-2.04067387747045,-2.00775269183138,-1.99423646712642,-1.99158039115654,
-1.99011116142325,-1.98885286758129,-1.98724447781428,-1.98465927006454,
-1.96977723397764,-1.9657112920977,-1.92484159572174,-1.90074633741755,
-1.89453602685366,-1.89160633467944,-1.88934741998761,-1.88687152921894,
-1.88284584064097,-1.86992814297236,-1.86106762445878,-1.81066778903153,
-1.79496500775627,-1.7922036682246,-1.79071171582063,-1.78945532751888,
-1.78787642461829,-1.78538884343792,-1.77240851787872,-1.7644681380549,
-1.71798280984101,-1.69832496422443,-1.6938938206752,-1.69132871223749,
-1.68908556850196,-1.68630559324293,-1.68202529533571,-1.66054121399684,
-1.61108208154023,-1.59547781481612,-1.59272064160989,-1.59122953241725,
-1.58997301610867,-1.58839289240738,-1.58779384257567),.UNSPECIFIED.);
#448=B_SPLINE_CURVE_WITH_KNOTS('',3,(#28098,#28099,#28100,#28101,#28102,
#28103,#28104,#28105,#28106,#28107,#28108,#28109,#28110,#28111,#28112,#28113,
#28114,#28115,#28116,#28117,#28118,#28119,#28120,#28121,#28122,#28123,#28124,
#28125,#28126,#28127,#28128,#28129,#28130,#28131,#28132,#28133,#28134,#28135,
#28136,#28137,#28138,#28139,#28140,#28141,#28142,#28143,#28144,#28145,#28146,
#28147,#28148,#28149,#28150,#28151,#28152,#28153,#28154,#28155,#28156,#28157,
#28158,#28159,#28160,#28161,#28162,#28163,#28164,#28165,#28166,#28167,#28168,
#28169,#28170,#28171,#28172,#28173,#28174,#28175,#28176,#28177,#28178,#28179,
#28180,#28181,#28182,#28183,#28184,#28185,#28186,#28187,#28188,#28189,#28190,
#28191,#28192,#28193,#28194,#28195,#28196,#28197,#28198,#28199,#28200,#28201,
#28202,#28203,#28204,#28205,#28206,#28207,#28208,#28209,#28210,#28211,#28212,
#28213,#28214,#28215,#28216,#28217,#28218,#28219,#28220,#28221,#28222,#28223,
#28224,#28225,#28226,#28227,#28228,#28229,#28230,#28231,#28232,#28233,#28234,
#28235,#28236,#28237,#28238,#28239,#28240,#28241,#28242,#28243,#28244,#28245,
#28246,#28247,#28248,#28249,#28250,#28251,#28252,#28253,#28254,#28255,#28256,
#28257,#28258,#28259,#28260,#28261,#28262,#28263,#28264,#28265,#28266,#28267),
 .UNSPECIFIED.,.F.,.F.,(4,2,2,2,2,2,2,2,2,2,2,2,2,2,2,2,2,2,2,2,2,2,2,2,
2,2,2,2,2,2,2,2,2,2,2,2,2,2,2,2,2,2,2,2,2,2,2,2,2,2,2,2,2,2,2,2,2,2,2,2,
2,2,2,2,2,2,2,2,2,2,2,2,2,2,2,2,2,2,2,2,2,2,2,2,4),(-0.926452780362809,
-0.909637390829123,-0.905229033347337,-0.902409538782332,-0.900162569554983,
-0.897623191808063,-0.893311291056809,-0.875413314360576,-0.828683561839237,
-0.826602189992789,-0.819658396293833,-0.806054498526084,-0.803532363268601,
-0.801942752075319,-0.800685424975685,-0.799201217319981,-0.796477140805644,
-0.781612357380261,-0.738205760173885,-0.71041582483058,-0.705884297560961,
-0.703027417811861,-0.700776653718294,-0.698260229705421,-0.69405286355535,
-0.67752947311056,-0.614988949722869,-0.605919794125388,-0.603461365362065,
-0.602034923473083,-0.600895576046197,-0.599289021167143,-0.595971085594238,
-0.562732826372065,-0.513945411207184,-0.507061002043918,-0.504237813121291,
-0.502137243919294,-0.499836115548513,-0.496649028056098,-0.488986935526028,
-0.478249535149239,-0.418807071527379,-0.4067760496548,-0.404108058120974,
-0.402619354801629,-0.401361957695237,-0.399777010521043,-0.396568755446391,
-0.392362061495167,-0.382219182975904,-0.336833320660837,-0.311146559031905,
-0.306682433989072,-0.303845509941163,-0.301596223973575,-0.29906647174904,
-0.294800719127599,-0.277538402984045,-0.243906241970156,-0.210539914062049,
-0.205761662800579,-0.203876827853335,-0.202607846560628,-0.20131699883905,
-0.199985948362352,-0.198115467943968,-0.185932207224183,-0.157374934046016,
-0.11539442927958,-0.108162898220615,-0.105280301336457,-0.103164725556191,
-0.100875228828571,-0.0977550038494009,-0.0904928011869399,-0.0804782340822814,
-0.0295372784663833,-0.0132637756828869,-0.00675812967874559,-0.00463040526874976,
-0.00325817851213518,-0.00205816246604583,-0.00108891780732919,-0.000589454289888855),
 .UNSPECIFIED.);
#449=B_SPLINE_CURVE_WITH_KNOTS('',3,(#28268,#28269,#28270,#28271,#28272,
#28273,#28274,#28275,#28276,#28277,#28278,#28279,#28280,#28281,#28282,#28283,
#28284,#28285,#28286,#28287,#28288,#28289,#28290,#28291,#28292,#28293,#28294,
#28295,#28296,#28297,#28298,#28299,#28300,#28301,#28302,#28303,#28304,#28305,
#28306,#28307,#28308,#28309,#28310,#28311,#28312,#28313,#28314,#28315,#28316,
#28317,#28318,#28319,#28320,#28321,#28322,#28323,#28324,#28325),
 .UNSPECIFIED.,.F.,.F.,(4,2,2,2,2,2,2,2,2,2,2,2,2,2,2,2,2,2,2,2,2,2,2,2,
2,2,2,2,4),(-2.51424347129331,-2.51298909616975,-2.50974297696382,-2.49086577269954,
-2.43953947552916,-2.42420230201702,-2.42009286305575,-2.41759741122848,
-2.41534131430693,-2.41244427175551,-2.40778102725624,-2.36861356833193,
-2.34088994770667,-2.32822021179079,-2.32332203447788,-2.31970836324781,
-2.3180661535042,-2.31684531340443,-2.31546990813453,-2.31321238005377,
-2.30562425205202,-2.24145067854674,-2.22481168872888,-2.22059456534028,
-2.21807565631282,-2.21582476734007,-2.21297058292729,-2.2084489828068,
-2.18351281682041),.UNSPECIFIED.);
#450=B_SPLINE_CURVE_WITH_KNOTS('',3,(#28326,#28327,#28328,#28329,#28330,
#28331,#28332,#28333,#28334,#28335,#28336,#28337,#28338,#28339,#28340,#28341,
#28342,#28343,#28344,#28345,#28346,#28347,#28348,#28349,#28350,#28351,#28352,
#28353,#28354,#28355,#28356,#28357,#28358,#28359,#28360,#28361,#28362,#28363,
#28364,#28365,#28366,#28367,#28368,#28369,#28370,#28371,#28372,#28373,#28374,
#28375,#28376,#28377,#28378,#28379,#28380,#28381,#28382,#28383,#28384,#28385,
#28386,#28387,#28388,#28389,#28390,#28391,#28392,#28393,#28394,#28395,#28396,
#28397,#28398,#28399,#28400,#28401,#28402,#28403,#28404,#28405,#28406,#28407,
#28408,#28409,#28410,#28411,#28412,#28413,#28414,#28415,#28416,#28417,#28418,
#28419,#28420,#28421,#28422,#28423,#28424,#28425,#28426,#28427,#28428,#28429,
#28430,#28431,#28432,#28433,#28434,#28435,#28436,#28437,#28438,#28439,#28440,
#28441,#28442,#28443,#28444,#28445,#28446,#28447,#28448,#28449,#28450,#28451,
#28452,#28453,#28454,#28455,#28456,#28457,#28458,#28459,#28460,#28461,#28462,
#28463,#28464,#28465,#28466,#28467,#28468,#28469,#28470,#28471,#28472,#28473,
#28474,#28475,#28476,#28477,#28478,#28479,#28480,#28481,#28482,#28483,#28484,
#28485,#28486,#28487,#28488,#28489,#28490,#28491,#28492,#28493,#28494,#28495,
#28496,#28497,#28498,#28499,#28500,#28501,#28502,#28503,#28504,#28505,#28506,
#28507,#28508,#28509,#28510,#28511,#28512,#28513,#28514,#28515,#28516,#28517,
#28518,#28519,#28520,#28521,#28522,#28523,#28524,#28525,#28526,#28527),
 .UNSPECIFIED.,.F.,.F.,(4,2,2,2,2,2,2,2,2,2,2,2,2,2,2,2,2,2,2,2,2,2,2,2,
2,2,2,2,2,2,2,2,2,2,2,2,2,2,2,2,2,2,2,2,2,2,2,2,2,2,2,2,2,2,2,2,2,2,2,2,
2,2,2,2,2,2,2,2,2,2,2,2,2,2,2,2,2,2,2,2,2,2,2,2,2,2,2,2,2,2,2,2,2,2,2,2,
2,2,2,2,4),(-1.58779384257567,-1.58530794947241,-1.56363531377009,-1.5277173334975,
-1.502108239085,-1.4956983741498,-1.49273101241254,-1.49046665410613,-1.48800798875912,
-1.48406165264793,-1.47182624559535,-1.42947772403734,-1.39953940009233,
-1.39439420386491,-1.39247864574392,-1.39117150395504,-1.38999403421244,
-1.38807638593596,-1.38328768519082,-1.35003123001768,-1.3163578787736,
-1.2990850221524,-1.29481979239473,-1.29229086757762,-1.2900426420838,-1.28720749980552,
-1.28274703433158,-1.25712946427265,-1.2309016158967,-1.19974792762863,
-1.19495386378932,-1.19303530967686,-1.19185766863045,-1.19055070335237,
-1.18863604401668,-1.1834970163045,-1.15363841567152,-1.10395251088246,
-1.0976974001608,-1.09435182250629,-1.09225401353284,-1.08995186341681,
-1.08675587422493,-1.07903550863753,-1.06819045349403,-1.00684065986656,
-0.996653163768813,-0.994123460804956,-0.992666602774408,-0.991418250122011,
-0.989797372338245,-0.986404993373701,-0.957262671062231,-0.905738153423709,
-0.897985897829439,-0.894690400011276,-0.892392346577639,-0.890044870833402,
-0.886617901687495,-0.87738745063311,-0.823843874675645,-0.798107568135285,
-0.794977466447497,-0.793387515135325,-0.792130160400013,-0.790646229167718,
-0.787923478132749,-0.773088200049362,-0.729910036825996,-0.70184577967035,
-0.69730574949192,-0.694446284358185,-0.692195225413299,-0.689680290444027,
-0.685479758113578,-0.669042693550401,-0.607639976093929,-0.597488851031956,
-0.594961878846494,-0.593505473381675,-0.592256763100708,-0.590634452145934,
-0.587235670757584,-0.557876756830801,-0.504570747755453,-0.498116529623879,
-0.495126226002401,-0.49284989523288,-0.490421592138919,-0.486616126413661,
-0.474371876822789,-0.453999217792585,-0.422879830155066,-0.398939084188236,
-0.395825093693884,-0.394238486223362,-0.392981235825957,-0.391494444456293,
-0.388758746054412,-0.373647931397671,-0.331223639443211),.UNSPECIFIED.);
#451=B_SPLINE_CURVE_WITH_KNOTS('',3,(#28532,#28533,#28534,#28535,#28536,
#28537,#28538,#28539,#28540,#28541,#28542,#28543,#28544,#28545,#28546,#28547,
#28548,#28549,#28550,#28551,#28552,#28553,#28554,#28555,#28556,#28557,#28558,
#28559,#28560,#28561,#28562,#28563,#28564,#28565,#28566,#28567,#28568,#28569,
#28570,#28571,#28572,#28573,#28574,#28575,#28576,#28577,#28578,#28579,#28580,
#28581,#28582,#28583,#28584,#28585,#28586,#28587,#28588,#28589,#28590,#28591,
#28592,#28593,#28594,#28595,#28596,#28597,#28598,#28599,#28600,#28601,#28602,
#28603,#28604,#28605,#28606,#28607,#28608,#28609,#28610,#28611,#28612,#28613,
#28614,#28615,#28616,#28617,#28618,#28619,#28620,#28621,#28622,#28623,#28624,
#28625,#28626,#28627,#28628,#28629,#28630,#28631,#28632,#28633,#28634,#28635,
#28636,#28637,#28638,#28639,#28640,#28641,#28642,#28643,#28644,#28645,#28646,
#28647,#28648,#28649,#28650,#28651,#28652,#28653,#28654,#28655,#28656,#28657,
#28658,#28659,#28660,#28661,#28662,#28663,#28664,#28665,#28666,#28667,#28668,
#28669,#28670,#28671,#28672,#28673,#28674,#28675,#28676,#28677,#28678,#28679,
#28680,#28681,#28682,#28683,#28684,#28685,#28686,#28687,#28688,#28689,#28690,
#28691,#28692,#28693,#28694,#28695,#28696,#28697,#28698,#28699,#28700,#28701,
#28702,#28703,#28704,#28705,#28706,#28707,#28708,#28709,#28710,#28711,#28712,
#28713,#28714,#28715,#28716,#28717,#28718,#28719,#28720,#28721,#28722,#28723,
#28724,#28725,#28726,#28727,#28728,#28729,#28730,#28731,#28732,#28733),
 .UNSPECIFIED.,.F.,.F.,(4,2,2,2,2,2,2,2,2,2,2,2,2,2,2,2,2,2,2,2,2,2,2,2,
2,2,2,2,2,2,2,2,2,2,2,2,2,2,2,2,2,2,2,2,2,2,2,2,2,2,2,2,2,2,2,2,2,2,2,2,
2,2,2,2,2,2,2,2,2,2,2,2,2,2,2,2,2,2,2,2,2,2,2,2,2,2,2,2,2,2,2,2,2,2,2,2,
2,2,2,2,4),(-2.18264003139251,-2.14598451708076,-2.10816324425232,-2.10222939614988,
-2.0993523865971,-2.09709962472545,-2.09459527428191,-2.09044181082173,
-2.07635722326331,-2.06768237234159,-2.01458815009102,-2.00651223311199,
-2.00122290088457,-1.99928645620989,-1.9979749021351,-1.99680090168871,
-1.99490274494027,-1.99023136912594,-1.95231774782686,-1.90753000941557,
-1.90231067993299,-1.89957704643358,-1.89733637115704,-1.8947349626996,
-1.89025938272062,-1.87198742392528,-1.81926721632703,-1.8033360604423,
-1.80056442705413,-1.79907002736022,-1.797813416199,-1.79623652430868,-1.79316762776359,
-1.7721257845726,-1.72130604146506,-1.70604383032626,-1.70194202418997,
-1.69944887860977,-1.69719336477275,-1.69429497280168,-1.68962524999063,
-1.65465448426018,-1.62954044403999,-1.60654603379918,-1.60201364758044,
-1.60019159491186,-1.59890258516541,-1.59770495083073,-1.59601943672233,
-1.59151154759564,-1.55015084884505,-1.50844831044497,-1.50331178188857,
-1.50059537565022,-1.49857291477652,-1.49603605541585,-1.49173523329185,
-1.47617214165339,-1.42057980179783,-1.40439869897935,-1.40161658903259,
-1.40011994170544,-1.39886344698385,-1.39728922798726,-1.39423284770309,
-1.37359207520142,-1.32240919203572,-1.30709484263055,-1.30298844807667,
-1.30049427226178,-1.29823895994862,-1.29534240983719,-1.29067890181161,
-1.25678765109242,-1.2202430768001,-1.20510121321782,-1.20250176290395,
-1.20088882445463,-1.19962978186435,-1.19816288368014,-1.19551894024778,
-1.18223748360061,-1.15043463924379,-1.10948361271134,-1.10486482500918,
-1.10198167533799,-1.09972796941844,-1.09722653510611,-1.09308717663254,
-1.07738987906207,-1.04744044205406,-1.00837454542915,-1.00375780977525,
-1.00186871928028,-1.00057971673414,-0.99923944727864,-0.997169282320156,
-0.990868671238765,-0.980612478789826,-0.933876250565931,-0.926452780362809),
 .UNSPECIFIED.);
#452=B_SPLINE_CURVE_WITH_KNOTS('',3,(#28735,#28736,#28737,#28738,#28739,
#28740,#28741,#28742,#28743,#28744,#28745,#28746,#28747,#28748,#28749,#28750,
#28751,#28752,#28753,#28754,#28755,#28756,#28757,#28758,#28759,#28760,#28761,
#28762,#28763,#28764,#28765,#28766,#28767,#28768,#28769,#28770,#28771,#28772,
#28773,#28774,#28775,#28776,#28777,#28778,#28779,#28780,#28781,#28782,#28783,
#28784,#28785,#28786,#28787,#28788,#28789,#28790,#28791,#28792,#28793,#28794,
#28795,#28796,#28797,#28798,#28799,#28800,#28801,#28802,#28803,#28804,#28805,
#28806,#28807,#28808,#28809,#28810,#28811,#28812,#28813,#28814,#28815,#28816,
#28817,#28818),.UNSPECIFIED.,.F.,.F.,(4,2,2,2,2,2,2,2,2,2,2,2,2,2,2,2,2,
2,2,2,2,2,2,2,2,2,2,2,2,2,2,2,2,2,2,2,2,2,2,2,2,4),(-0.331223639443211,
-0.328400283237573,-0.318230345971041,-0.301571799019314,-0.297219577159239,
-0.294646191467861,-0.29240295333943,-0.289632073593904,-0.284232991031098,
-0.277370440987669,-0.261533147621455,-0.221660235473837,-0.19938299995667,
-0.196293789654357,-0.194712475032134,-0.193490616217635,-0.193482886691718,
-0.193475217914417,-0.193467608531236,-0.1934600574321,-0.193452563300397,
-0.193445124781644,-0.19343774067915,-0.193430409979487,-0.19342313169482,
-0.193415904542959,-0.193408727497731,-0.1919276918568,-0.190320685315479,
-0.187773706910874,-0.18280122812995,-0.169845147164471,-0.128787708133948,
-0.103050212938598,-0.0985848410198022,-0.0957478779548156,-0.0934990459870276,
-0.0909703220249327,-0.0867075750181842,-0.0694766656570718,-0.0373212317703668,
-0.000589895100449732),.UNSPECIFIED.);
#453=B_SPLINE_CURVE_WITH_KNOTS('',3,(#28819,#28820,#28821,#28822,#28823,
#28824,#28825,#28826,#28827,#28828,#28829,#28830,#28831,#28832,#28833,#28834,
#28835,#28836,#28837,#28838,#28839,#28840,#28841,#28842,#28843,#28844,#28845,
#28846,#28847,#28848,#28849,#28850,#28851,#28852,#28853,#28854,#28855,#28856,
#28857,#28858,#28859,#28860,#28861,#28862,#28863,#28864,#28865,#28866,#28867,
#28868,#28869,#28870,#28871,#28872,#28873,#28874,#28875,#28876,#28877,#28878,
#28879,#28880,#28881,#28882,#28883,#28884,#28885,#28886,#28887,#28888,#28889,
#28890,#28891,#28892,#28893,#28894,#28895,#28896,#28897,#28898,#28899,#28900,
#28901,#28902,#28903,#28904,#28905,#28906,#28907,#28908,#28909,#28910,#28911,
#28912,#28913,#28914,#28915,#28916,#28917,#28918,#28919,#28920,#28921,#28922,
#28923,#28924,#28925,#28926,#28927,#28928,#28929,#28930,#28931,#28932,#28933,
#28934,#28935,#28936,#28937,#28938,#28939,#28940,#28941,#28942,#28943,#28944,
#28945,#28946,#28947,#28948,#28949,#28950,#28951,#28952,#28953,#28954,#28955,
#28956,#28957,#28958,#28959,#28960,#28961,#28962,#28963,#28964,#28965,#28966,
#28967,#28968,#28969,#28970,#28971,#28972,#28973,#28974,#28975,#28976,#28977,
#28978,#28979,#28980,#28981,#28982,#28983,#28984,#28985,#28986),
 .UNSPECIFIED.,.F.,.F.,(4,2,2,2,2,2,2,2,2,2,2,2,2,2,2,2,2,2,2,2,2,2,2,2,
2,2,2,2,2,2,2,2,2,2,2,2,2,2,2,2,2,2,2,2,2,2,2,2,2,2,2,2,2,2,2,2,2,2,2,2,
2,2,2,2,2,2,2,2,2,2,2,2,2,2,2,2,2,2,2,2,2,2,2,4),(-2.51455855929107,-2.51267182880103,
-2.51070992938911,-2.50944404317543,-2.50824341760209,-2.50686998312504,
-2.5046508170838,-2.49776268037399,-2.48328141238618,-2.43134975919785,
-2.41592979517343,-2.41181344669691,-2.40931665937358,-2.40706120102442,
-2.40416755859932,-2.399515090484,-2.35967307239754,-2.33087137330689,-2.31934138430718,
-2.31474724717373,-2.31233861907934,-2.31078850070573,-2.30934995365382,
-2.30813825193173,-2.3065556437761,-2.30346104587939,-2.27105233106817,
-2.23432188999498,-2.21671480519106,-2.212423325102,-2.20988796821129,-2.20763964562131,
-2.20481190507332,-2.20037783686281,-2.17550534314661,-2.12929179002068,
-2.11907402644167,-2.11279029264204,-2.1107217758433,-2.10938159027269,
-2.1080918321381,-2.10620037573726,-2.10157158395456,-2.06272787620119,
-2.01882008688869,-2.01355659330931,-2.01081321545647,-2.0087873446844,
-2.00626769959418,-2.00204787052256,-1.9873360563847,-1.93617665552517,
-1.9166595416907,-1.91248251071885,-1.91071870976273,-1.90943955011861,
-1.9080530718869,-1.90577541100855,-1.89840660830998,-1.85698225723775,
-1.83578842024898,-1.81760633237194,-1.81327287723171,-1.81072815510037,
-1.80848093849328,-1.80566708304984,-1.80127907173016,-1.77762856658772,
-1.73981116668979,-1.71684754745087,-1.71284628666751,-1.71111281516262,
-1.70983852640525,-1.7084390022998,-1.70610267362239,-1.6982184297288,-1.63435668719908,
-1.61773550055021,-1.61351972240989,-1.61100110385319,-1.60875015954643,
-1.60589548422185,-1.60137228783183,-1.58839498599662),.UNSPECIFIED.);
#454=B_SPLINE_CURVE_WITH_KNOTS('',3,(#28992,#28993,#28994,#28995,#28996,
#28997,#28998,#28999,#29000,#29001,#29002,#29003,#29004,#29005,#29006,#29007,
#29008,#29009,#29010,#29011,#29012,#29013,#29014,#29015,#29016,#29017,#29018,
#29019,#29020,#29021,#29022,#29023,#29024,#29025,#29026,#29027,#29028,#29029,
#29030,#29031,#29032,#29033,#29034,#29035,#29036,#29037,#29038,#29039,#29040,
#29041,#29042,#29043,#29044,#29045,#29046,#29047,#29048,#29049,#29050,#29051,
#29052,#29053,#29054,#29055,#29056,#29057,#29058,#29059,#29060,#29061,#29062,
#29063,#29064,#29065,#29066,#29067,#29068,#29069,#29070,#29071,#29072,#29073,
#29074,#29075,#29076,#29077,#29078,#29079,#29080,#29081,#29082,#29083,#29084,
#29085,#29086,#29087,#29088,#29089,#29090,#29091,#29092,#29093,#29094,#29095,
#29096,#29097,#29098,#29099,#29100,#29101,#29102,#29103,#29104,#29105,#29106,
#29107,#29108,#29109,#29110,#29111,#29112,#29113,#29114,#29115,#29116,#29117,
#29118,#29119,#29120,#29121,#29122,#29123,#29124,#29125,#29126,#29127,#29128,
#29129,#29130,#29131,#29132,#29133,#29134,#29135,#29136,#29137,#29138,#29139,
#29140,#29141,#29142,#29143,#29144,#29145,#29146,#29147,#29148,#29149,#29150,
#29151,#29152,#29153,#29154,#29155),.UNSPECIFIED.,.F.,.F.,(4,2,2,2,2,2,
2,2,2,2,2,2,2,2,2,2,2,2,2,2,2,2,2,2,2,2,2,2,2,2,2,2,2,2,2,2,2,2,2,2,2,2,
2,2,2,2,2,2,2,2,2,2,2,2,2,2,2,2,2,2,2,2,2,2,2,2,2,2,2,2,2,2,2,2,2,2,2,2,
2,2,2,4),(-0.92677959358465,-0.913956461130793,-0.887738891672986,-0.88460392692942,
-0.883012622282303,-0.88175477462299,-0.880270911707597,-0.877549931281789,
-0.862766394361419,-0.819969429023721,-0.79148963880891,-0.786936396563254,
-0.784072428199227,-0.78182019700041,-0.779306410335309,-0.775113611790413,
-0.758784126405556,-0.698657199786042,-0.687281807858335,-0.684659282558548,
-0.683180723310601,-0.681922185656012,-0.680323380708066,-0.67704636708009,
-0.672724771099001,-0.62415063732743,-0.592032702904539,-0.587387979671654,
-0.584496297058608,-0.582240621835037,-0.579741807221744,-0.575617958157782,
-0.560118639868694,-0.507592837897413,-0.502745404443118,-0.488037317593654,
-0.485458757510819,-0.48385163229742,-0.482592422724597,-0.481119879474698,
-0.478452219407395,-0.464748199372748,-0.428746998202478,-0.392514894443486,
-0.387837323526096,-0.384935697135191,-0.38267868134251,-0.380184906170556,
-0.37608444400125,-0.360856403997985,-0.30994950409805,-0.288863758069141,
-0.285791990872181,-0.284213929083897,-0.282956548399099,-0.281461419176586,
-0.278688936006906,-0.262765672654064,-0.210164493371885,-0.191771762761121,
-0.187280697736259,-0.184674739580836,-0.182516231652231,-0.182476324449123,
-0.182438033032951,-0.182401247586332,-0.182365867957033,-0.18233180268593,
-0.182298968078676,-0.179559949958377,-0.176588839186943,-0.171819231333473,
-0.162389840194946,-0.115810719314727,-0.089364706251363,-0.0862274145327824,
-0.0846353913761449,-0.0833772170991153,-0.081893251484031,-0.0791728076642042,
-0.0644110085413288,-0.000590038431533063),.UNSPECIFIED.);
#455=B_SPLINE_CURVE_WITH_KNOTS('',3,(#29156,#29157,#29158,#29159,#29160,
#29161,#29162,#29163,#29164,#29165,#29166,#29167,#29168,#29169,#29170,#29171,
#29172,#29173,#29174,#29175,#29176,#29177,#29178,#29179,#29180,#29181,#29182,
#29183,#29184,#29185,#29186,#29187,#29188,#29189,#29190,#29191,#29192,#29193,
#29194,#29195,#29196,#29197,#29198,#29199,#29200,#29201,#29202,#29203,#29204,
#29205,#29206,#29207,#29208,#29209,#29210,#29211,#29212,#29213,#29214,#29215,
#29216,#29217,#29218,#29219,#29220,#29221,#29222,#29223,#29224,#29225),
 .UNSPECIFIED.,.F.,.F.,(4,2,2,2,2,2,2,2,2,2,2,2,2,2,2,2,2,2,2,2,2,2,2,2,
2,2,2,2,2,2,2,2,2,2,4),(-2.51322710726194,-2.50306881125958,-2.500318325518,
-2.49815032271898,-2.4959489582546,-2.49342563129446,-2.48918475967013,
-2.47519140971142,-2.41681275051123,-2.40166680893969,-2.3989300207045,
-2.39744323970873,-2.39618634741625,-2.39460061606263,-2.39148957656057,
-2.36733357237162,-2.32989726596998,-2.31379660224984,-2.30685603765565,
-2.30301464286754,-2.29965910347358,-2.29735087919383,-2.29505941343393,
-2.29230722082498,-2.28539985991157,-2.23532504570624,-2.21251159976598,
-2.20536789146102,-2.20054240368459,-2.1986744984044,-2.19737683100111,
-2.19618986191896,-2.19454439272652,-2.1903186976033,-2.18264003139251),
 .UNSPECIFIED.);
#456=B_SPLINE_CURVE_WITH_KNOTS('',3,(#29226,#29227,#29228,#29229,#29230,
#29231,#29232,#29233,#29234,#29235,#29236,#29237,#29238,#29239,#29240,#29241,
#29242,#29243,#29244,#29245,#29246,#29247,#29248,#29249,#29250,#29251,#29252,
#29253,#29254,#29255,#29256,#29257,#29258,#29259,#29260,#29261,#29262,#29263,
#29264,#29265,#29266,#29267,#29268,#29269,#29270,#29271,#29272,#29273,#29274,
#29275,#29276,#29277,#29278,#29279,#29280,#29281,#29282,#29283,#29284,#29285,
#29286,#29287,#29288,#29289,#29290,#29291,#29292,#29293,#29294,#29295,#29296,
#29297,#29298,#29299,#29300,#29301,#29302,#29303,#29304,#29305,#29306,#29307,
#29308,#29309,#29310,#29311,#29312,#29313,#29314,#29315,#29316,#29317,#29318,
#29319,#29320,#29321,#29322,#29323,#29324,#29325,#29326,#29327,#29328,#29329,
#29330,#29331,#29332,#29333,#29334,#29335,#29336,#29337,#29338,#29339,#29340,
#29341,#29342,#29343,#29344,#29345,#29346,#29347,#29348,#29349,#29350,#29351,
#29352,#29353,#29354,#29355,#29356,#29357,#29358,#29359,#29360,#29361,#29362,
#29363,#29364,#29365,#29366,#29367,#29368,#29369,#29370,#29371,#29372,#29373,
#29374,#29375,#29376,#29377,#29378,#29379,#29380,#29381,#29382,#29383,#29384,
#29385,#29386,#29387,#29388,#29389,#29390,#29391,#29392,#29393,#29394,#29395,
#29396,#29397,#29398,#29399,#29400,#29401,#29402,#29403,#29404,#29405,#29406,
#29407,#29408,#29409,#29410,#29411,#29412,#29413,#29414,#29415,#29416,#29417,
#29418,#29419,#29420,#29421,#29422,#29423,#29424,#29425,#29426,#29427,#29428,
#29429,#29430,#29431),.UNSPECIFIED.,.F.,.F.,(4,2,2,2,2,2,2,2,2,2,2,2,2,
2,2,2,2,2,2,2,2,2,2,2,2,2,2,2,2,2,2,2,2,2,2,2,2,2,2,2,2,2,2,2,2,2,2,2,2,
2,2,2,2,2,2,2,2,2,2,2,2,2,2,2,2,2,2,2,2,2,2,2,2,2,2,2,2,2,2,2,2,2,2,2,2,
2,2,2,2,2,2,2,2,2,2,2,2,2,2,2,2,2,4),(-1.58839498599662,-1.57389679594943,
-1.53012524666282,-1.51520503035608,-1.51247775967064,-1.51099264995324,
-1.50973506747913,-1.50814581829002,-1.50562556430176,-1.49206516637976,
-1.48508584688019,-1.43335240337203,-1.42318373105345,-1.41583489023955,
-1.41270008424995,-1.41040822700298,-1.40829630140824,-1.40542764008709,
-1.39827798178308,-1.35366871659575,-1.31743508525211,-1.3135487905047,
-1.31183575689162,-1.31056465268956,-1.30915580048413,-1.30677702832592,
-1.29849796658949,-1.25782231538263,-1.25419345451046,-1.22028973431126,
-1.21562517441884,-1.21272792532229,-1.21047206546839,-1.20797728645389,
-1.20386992457662,-1.18855331909787,-1.13738865577281,-1.11664590076547,
-1.11358558436978,-1.11201027469046,-1.11075341699938,-1.10925695855602,
-1.10647688108613,-1.0903574930049,-1.03553479667585,-1.01925934847971,
-1.01493416233628,-1.01236678209581,-1.01012261103052,-1.00734260511122,
-1.00189982430362,-0.964635404703312,-0.923660173673593,-0.915723316973921,
-0.913381301371229,-0.911980585637987,-0.910706838537789,-0.908976374686079,
-0.904991790424494,-0.88720698795585,-0.844130026595071,-0.820569568567948,
-0.816185610615111,-0.813373101539888,-0.811126170030985,-0.808580924010213,
-0.804244487974513,-0.786017809540127,-0.764732584541424,-0.723010575005474,
-0.715967458056545,-0.713728838222886,-0.712351086200415,-0.711068255573755,
-0.709282598561758,-0.704975328454701,-0.68423109950062,-0.624017932979638,
-0.617203246173567,-0.614465329367151,-0.612176940933543,-0.609815841503152,
-0.606324959288843,-0.596640907909793,-0.581981948412719,-0.551236680492311,
-0.520479501240534,-0.515690744058459,-0.513772684182183,-0.512594840768582,
-0.511287165012195,-0.5093706262964,-0.504221547627114,-0.474249737280712,
-0.424678480154916,-0.417717637722567,-0.414956446843606,-0.412662192114699,
-0.410308947906355,-0.406855666865491,-0.397442401063055,-0.3833359825281,
-0.331428972207689),.UNSPECIFIED.);
#457=B_SPLINE_CURVE_WITH_KNOTS('',3,(#29436,#29437,#29438,#29439,#29440,
#29441,#29442,#29443,#29444,#29445,#29446,#29447,#29448,#29449,#29450,#29451,
#29452,#29453,#29454,#29455,#29456,#29457,#29458,#29459,#29460,#29461,#29462,
#29463,#29464,#29465,#29466,#29467,#29468,#29469,#29470,#29471,#29472,#29473,
#29474,#29475,#29476,#29477,#29478,#29479,#29480,#29481,#29482,#29483,#29484,
#29485,#29486,#29487,#29488,#29489,#29490,#29491,#29492,#29493,#29494,#29495,
#29496,#29497,#29498,#29499,#29500,#29501,#29502,#29503,#29504,#29505,#29506,
#29507,#29508,#29509,#29510,#29511,#29512,#29513,#29514,#29515,#29516,#29517,
#29518,#29519,#29520,#29521,#29522,#29523,#29524,#29525,#29526,#29527,#29528,
#29529,#29530,#29531,#29532,#29533,#29534,#29535,#29536,#29537,#29538,#29539,
#29540,#29541,#29542,#29543,#29544,#29545,#29546,#29547,#29548,#29549,#29550,
#29551,#29552,#29553,#29554,#29555,#29556,#29557,#29558,#29559,#29560,#29561,
#29562,#29563,#29564,#29565,#29566,#29567,#29568,#29569,#29570,#29571,#29572,
#29573,#29574,#29575,#29576,#29577,#29578,#29579,#29580,#29581,#29582,#29583,
#29584,#29585,#29586,#29587,#29588,#29589,#29590,#29591,#29592,#29593,#29594,
#29595,#29596,#29597,#29598,#29599,#29600,#29601,#29602,#29603,#29604,#29605,
#29606,#29607,#29608,#29609,#29610,#29611,#29612,#29613,#29614,#29615,#29616,
#29617,#29618,#29619,#29620,#29621,#29622,#29623,#29624,#29625,#29626,#29627,
#29628,#29629,#29630,#29631,#29632,#29633,#29634,#29635,#29636,#29637,#29638,
#29639,#29640,#29641,#29642,#29643,#29644,#29645,#29646,#29647,#29648,#29649,
#29650,#29651),.UNSPECIFIED.,.F.,.F.,(4,2,2,2,2,2,2,2,2,2,2,2,2,2,2,2,2,
2,2,2,2,2,2,2,2,2,2,2,2,2,2,2,2,2,2,2,2,2,2,2,2,2,2,2,2,2,2,2,2,2,2,2,2,
2,2,2,2,2,2,2,2,2,2,2,2,2,2,2,2,2,2,2,2,2,2,2,2,2,2,2,2,2,2,2,2,2,2,2,2,
2,2,2,2,2,2,2,2,2,2,2,2,2,2,2,2,2,2,4),(-2.18327158177654,-2.18237473463362,
-2.1798643145631,-2.17761231538485,-2.17474482746901,-2.1701782813769,-2.14119715670792,
-2.09884498927307,-2.08412528277437,-2.08140785580374,-2.07992502811304,
-2.07866750515955,-2.07707591611306,-2.07393831137517,-2.04707624538335,
-2.01093049290248,-1.99572431302921,-1.98905151351183,-1.9837710798474,
-1.9810245526589,-1.97899869223382,-1.97648204385171,-1.97227433396359,
-1.957673757243,-1.94954653254484,-1.89650001839176,-1.88842577944554,-1.88313696289202,
-1.88120032976807,-1.87988853525725,-1.87871423424549,-1.87681543313071,
-1.87214168097356,-1.83434134530135,-1.78938220949677,-1.78418661432689,
-1.78145753919213,-1.77921661409665,-1.77661040136295,-1.7721153282108,
-1.75357539473028,-1.70111512496838,-1.68520588740849,-1.68243472274365,
-1.68094022540139,-1.67968332464732,-1.67810580755332,-1.6750349335161,
-1.65394829732468,-1.60305970955705,-1.58787946106536,-1.58378424760483,
-1.58129220698214,-1.57903581742817,-1.57613367572018,-1.57145251493047,
-1.53446495148284,-1.49946601313129,-1.48553350804964,-1.48285462501969,
-1.48137997219493,-1.4801214786333,-1.47851851655293,-1.47595282504375,
-1.46149580455587,-1.45617430555503,-1.40387978146931,-1.388414579538,-1.38429462681168,
-1.38179719136077,-1.37954212907725,-1.37665035336343,-1.37200364225382,
-1.33262458000192,-1.2995395597515,-1.28598744316519,-1.28332849442826,
-1.28185818415954,-1.2805992736605,-1.27899046539558,-1.27640527788,-1.26154228164339,
-1.2576224943358,-1.2187346028497,-1.19060414772441,-1.18606172708297,-1.18320127153122,
-1.18094974656275,-1.17843461100669,-1.1742344872179,-1.15780836471621,
-1.0965292632248,-1.08627150875081,-1.08373530750034,-1.08227662295387,
-1.08102796737465,-1.07940830558278,-1.07602408042783,-1.04721034938435,
-0.996823319807449,-0.9879960720525,-0.984523368248433,-0.982401526806259,
-0.980116372271241,-0.977021824067564,-0.969908843914664,-0.960159636101433,
-0.92677959358465),.UNSPECIFIED.);
#458=B_SPLINE_CURVE_WITH_KNOTS('',3,(#29653,#29654,#29655,#29656,#29657,
#29658,#29659,#29660,#29661,#29662,#29663,#29664,#29665,#29666,#29667,#29668,
#29669,#29670,#29671,#29672,#29673,#29674,#29675,#29676,#29677,#29678,#29679,
#29680,#29681,#29682,#29683,#29684,#29685,#29686,#29687,#29688,#29689,#29690,
#29691,#29692,#29693,#29694,#29695,#29696,#29697,#29698,#29699,#29700,#29701,
#29702,#29703,#29704,#29705,#29706,#29707,#29708,#29709,#29710,#29711,#29712,
#29713,#29714,#29715,#29716,#29717,#29718,#29719,#29720),.UNSPECIFIED.,
 .F.,.F.,(4,2,2,2,2,2,2,2,2,2,2,2,2,2,2,2,2,2,2,2,2,2,2,2,2,2,2,2,2,2,2,
2,2,4),(-0.331428972207689,-0.329069592277333,-0.31754448082226,-0.314911286889619,
-0.313430515309816,-0.312172530874924,-0.310577569749016,-0.307318810788601,
-0.272108301779798,-0.225394121966846,-0.218355992557429,-0.215506219692164,
-0.213398962200356,-0.21114907560631,-0.208088514010398,-0.20466469999614,
-0.198783566725625,-0.160678346912252,-0.12099775587246,-0.116413804600362,
-0.114529870692238,-0.113241624547243,-0.111899440938968,-0.10982164988372,
-0.103461667375636,-0.0930722481795077,-0.0320180274467594,-0.0203029537165471,
-0.0164251417768983,-0.0139809767253367,-0.011820034564099,-0.00961711351532164,
-0.00560281701044909,-0.000589238754991204),.UNSPECIFIED.);
#459=B_SPLINE_CURVE_WITH_KNOTS('',3,(#29721,#29722,#29723,#29724,#29725,
#29726,#29727,#29728,#29729,#29730,#29731,#29732,#29733,#29734,#29735,#29736,
#29737,#29738,#29739,#29740,#29741,#29742,#29743,#29744,#29745,#29746,#29747,
#29748,#29749,#29750,#29751,#29752,#29753,#29754,#29755,#29756,#29757,#29758,
#29759,#29760,#29761,#29762,#29763,#29764,#29765,#29766,#29767,#29768,#29769,
#29770,#29771,#29772,#29773,#29774,#29775,#29776,#29777,#29778,#29779,#29780,
#29781,#29782,#29783,#29784,#29785,#29786,#29787,#29788,#29789,#29790,#29791,
#29792,#29793,#29794,#29795,#29796,#29797,#29798,#29799,#29800,#29801,#29802,
#29803,#29804,#29805,#29806,#29807,#29808,#29809,#29810,#29811,#29812,#29813,
#29814,#29815,#29816,#29817,#29818,#29819,#29820,#29821,#29822,#29823,#29824,
#29825,#29826,#29827,#29828,#29829,#29830,#29831,#29832,#29833,#29834,#29835,
#29836,#29837,#29838,#29839,#29840,#29841,#29842,#29843,#29844,#29845,#29846,
#29847,#29848,#29849,#29850,#29851,#29852,#29853,#29854,#29855,#29856,#29857,
#29858,#29859,#29860,#29861,#29862,#29863,#29864,#29865,#29866,#29867,#29868,
#29869,#29870,#29871,#29872,#29873,#29874,#29875,#29876,#29877,#29878,#29879,
#29880,#29881,#29882,#29883,#29884,#29885,#29886,#29887,#29888,#29889,#29890,
#29891,#29892,#29893,#29894,#29895,#29896,#29897,#29898,#29899,#29900,#29901,
#29902,#29903,#29904,#29905,#29906,#29907,#29908,#29909,#29910),
 .UNSPECIFIED.,.F.,.F.,(4,2,2,2,2,2,2,2,2,2,2,2,2,2,2,2,2,2,2,2,2,2,2,2,
2,2,2,2,2,2,2,2,2,2,2,2,2,2,2,2,2,2,2,2,2,2,2,2,2,2,2,2,2,2,2,2,2,2,2,2,
2,2,2,2,2,2,2,2,2,2,2,2,2,2,2,2,2,2,2,2,2,2,2,2,2,2,2,2,2,2,2,2,2,2,4),
(-2.51385800421912,-2.44636517931643,-2.431612280618,-2.42889332475062,
-2.42741020504889,-2.42615277103915,-2.42456175169058,-2.42142665686335,
-2.39504305790227,-2.34861391700199,-2.33910351988365,-2.33430548895331,
-2.33132315755465,-2.32857636760943,-2.32854220446278,-2.32850690336214,
-2.32847038404083,-2.32843255880197,-2.32839333146543,-2.32835259642427,
-2.32831023743384,-2.3282661261745,-2.32822012052279,-2.32817206277085,
-2.32812177731026,-2.32809325676061,-2.32805762578005,-2.32801285630427,
-2.32795619200621,-2.32788379186356,-2.32779013116768,-2.32559208321247,
-2.32272021037873,-2.3181389885118,-2.28886693672711,-2.24676880078385,
-2.23208397823921,-2.22936822641916,-2.22788578304132,-2.22662827238712,
-2.22503632728358,-2.22189693076285,-2.19439071927247,-2.15792878071183,
-2.14329755799621,-2.1368005931387,-2.13163115886668,-2.12890766716624,
-2.12666718396756,-2.12405678205579,-2.1195427478348,-2.10072813596257,
-2.09399861600692,-2.05216146011603,-2.03454642543843,-2.03058191621004,
-2.02885519540958,-2.0275822319552,-2.02635660388504,-2.02419252284182,
-2.01773514987145,-1.95224143081994,-1.94120671222611,-1.9333823437529,
-1.93016920728132,-1.92786370886945,-1.92576895023238,-1.92244140505524,
-1.91625461428461,-1.86576513105235,-1.83362518615939,-1.83050911421993,
-1.82894304034653,-1.82780852984964,-1.82635534807342,-1.8238416015201,
-1.81384137755083,-1.75232256766172,-1.73588031383969,-1.73167986356789,
-1.72916519412771,-1.72691450722465,-1.7240556984035,-1.71951703761676,
-1.69148772476889,-1.64825210442742,-1.63340831816123,-1.63068535834978,
-1.62920150167953,-1.627944318572,-1.62635473168511,-1.62383237486457,-1.61021973740491,
-1.60334132476312,-1.58784363167967),.UNSPECIFIED.);
#460=B_SPLINE_CURVE_WITH_KNOTS('',3,(#29916,#29917,#29918,#29919,#29920,
#29921,#29922,#29923,#29924,#29925,#29926,#29927,#29928,#29929,#29930,#29931,
#29932,#29933,#29934,#29935,#29936,#29937,#29938,#29939,#29940,#29941,#29942,
#29943,#29944,#29945,#29946,#29947,#29948,#29949,#29950,#29951,#29952,#29953,
#29954,#29955,#29956,#29957,#29958,#29959,#29960,#29961,#29962,#29963,#29964,
#29965,#29966,#29967,#29968,#29969,#29970,#29971,#29972,#29973,#29974,#29975,
#29976,#29977,#29978,#29979,#29980,#29981,#29982,#29983,#29984,#29985,#29986,
#29987,#29988,#29989,#29990,#29991,#29992,#29993,#29994,#29995,#29996,#29997,
#29998,#29999,#30000,#30001,#30002,#30003,#30004,#30005,#30006,#30007,#30008,
#30009,#30010,#30011,#30012,#30013,#30014,#30015,#30016,#30017,#30018,#30019,
#30020,#30021,#30022,#30023,#30024,#30025,#30026,#30027,#30028,#30029,#30030,
#30031,#30032,#30033,#30034,#30035,#30036,#30037,#30038,#30039,#30040,#30041,
#30042,#30043,#30044,#30045,#30046,#30047,#30048,#30049,#30050,#30051,#30052,
#30053,#30054,#30055,#30056,#30057,#30058,#30059,#30060,#30061,#30062,#30063,
#30064,#30065,#30066,#30067,#30068,#30069,#30070,#30071,#30072,#30073),
 .UNSPECIFIED.,.F.,.F.,(4,2,2,2,2,2,2,2,2,2,2,2,2,2,2,2,2,2,2,2,2,2,2,2,
2,2,2,2,2,2,2,2,2,2,2,2,2,2,2,2,2,2,2,2,2,2,2,2,2,2,2,2,2,2,2,2,2,2,2,2,
2,2,2,2,2,2,2,2,2,2,2,2,2,2,2,2,2,2,4),(-0.926655402496498,-0.923325713363623,
-0.875292521762498,-0.868346533299104,-0.865512679640234,-0.863409460980203,
-0.861110593662156,-0.857936137348705,-0.850350669588792,-0.839753052092,
-0.80865427827618,-0.771245861527511,-0.766547068349882,-0.764644066482668,
-0.763468989606336,-0.76215809480017,-0.760225876991041,-0.754968056358794,
-0.74695836949584,-0.694972907930171,-0.684978571269381,-0.670996910459284,
-0.666853556032092,-0.664350981166793,-0.662097059452066,-0.659214757552757,
-0.653256188746563,-0.612550460754442,-0.571486359006606,-0.56695796555454,
-0.565269281098544,-0.564070607723434,-0.562781806314694,-0.560962224650154,
-0.556446943285244,-0.533636464436129,-0.510487308828706,-0.473380312573813,
-0.468700165707988,-0.465798253733345,-0.463541815998277,-0.461049491659218,
-0.456953285347575,-0.441763515642257,-0.390850431239601,-0.36975580306435,
-0.366684518508422,-0.365106856799941,-0.363849876085606,-0.362355318467321,
-0.359584148064584,-0.343675898136389,-0.291197077674096,-0.272699618055052,
-0.268207304685064,-0.265601569733216,-0.263360387709269,-0.260630165087058,
-0.255429819582491,-0.248883755018148,-0.23409264982936,-0.182540404821751,
-0.169618780281208,-0.167133463660783,-0.165554781913349,-0.16429772163908,
-0.163102679175141,-0.160860067986025,-0.152482104862663,-0.13694380760027,
-0.115306868483614,-0.0741973780390122,-0.0695757179166427,-0.0666911871463561,
-0.0644366553561687,-0.0619345645218826,-0.0577947266259297,-0.0528738525793985,
-0.000589974190451465),.UNSPECIFIED.);
#461=B_SPLINE_CURVE_WITH_KNOTS('',3,(#30074,#30075,#30076,#30077,#30078,
#30079,#30080,#30081,#30082,#30083,#30084,#30085,#30086,#30087,#30088,#30089,
#30090,#30091,#30092,#30093,#30094,#30095,#30096,#30097,#30098,#30099,#30100,
#30101,#30102,#30103,#30104,#30105,#30106,#30107,#30108,#30109,#30110,#30111,
#30112,#30113,#30114,#30115,#30116,#30117,#30118,#30119,#30120,#30121,#30122,
#30123,#30124,#30125,#30126,#30127,#30128,#30129,#30130,#30131,#30132,#30133,
#30134,#30135,#30136,#30137,#30138,#30139,#30140,#30141,#30142,#30143,#30144,
#30145,#30146,#30147,#30148,#30149,#30150,#30151,#30152,#30153,#30154,#30155,
#30156,#30157,#30158,#30159,#30160,#30161,#30162,#30163,#30164,#30165,#30166,
#30167,#30168,#30169,#30170,#30171,#30172,#30173,#30174,#30175,#30176,#30177,
#30178,#30179,#30180,#30181,#30182,#30183,#30184,#30185,#30186,#30187),
 .UNSPECIFIED.,.F.,.F.,(4,2,2,2,2,2,2,2,2,2,2,2,2,2,2,2,2,2,2,2,2,2,2,2,
2,2,2,2,2,2,2,2,2,2,2,2,2,2,2,2,2,2,2,2,2,2,2,2,2,2,2,2,2,2,2,2,4),(-2.5136943146703,
-2.48380750396871,-2.48159185501007,-2.48012132498352,-2.47892808420488,
-2.47767089825701,-2.47608450433997,-2.47297130089924,-2.44869524354049,
-2.43335605149126,-2.39114991208164,-2.38382693609609,-2.38069679813858,
-2.37840599846826,-2.37629339513071,-2.37342127026519,-2.36624967973667,
-2.32226479000931,-2.28769438669882,-2.28397482608036,-2.28110157668122,
-2.27958653808802,-2.27958267230492,-2.27957879377167,-2.27957490225234,
-2.27957099774637,-2.27956708041037,-2.27956315007698,-2.27955920645746,
-2.27955524962164,-2.2795512794122,-2.27954729589535,-2.2795432988887,-2.27953928829381,
-2.27953526406274,-2.2795312261854,-2.27952717450785,-2.2795231090035,-2.27951902952133,
-2.27951493603563,-2.27951082802332,-2.2795067058843,-2.27950256948525,
-2.27949841863929,-2.27949425329322,-2.27949007323984,-2.27948587865382,
-2.27948160529282,-2.27947726300606,-2.27947285048055,-2.27821609677091,
-2.27663886446651,-2.27415779496651,-2.261334242407,-2.2027368319213,-2.18655457165281,
-2.18327158177654),.UNSPECIFIED.);
#462=B_SPLINE_CURVE_WITH_KNOTS('',3,(#30188,#30189,#30190,#30191,#30192,
#30193,#30194,#30195,#30196,#30197,#30198,#30199,#30200,#30201,#30202,#30203,
#30204,#30205,#30206,#30207,#30208,#30209,#30210,#30211,#30212,#30213,#30214,
#30215,#30216,#30217,#30218,#30219,#30220,#30221,#30222,#30223,#30224,#30225,
#30226,#30227,#30228,#30229,#30230,#30231,#30232,#30233,#30234,#30235,#30236,
#30237,#30238,#30239,#30240,#30241,#30242,#30243,#30244,#30245,#30246,#30247,
#30248,#30249,#30250,#30251,#30252,#30253,#30254,#30255,#30256,#30257,#30258,
#30259,#30260,#30261,#30262,#30263,#30264,#30265,#30266,#30267,#30268,#30269,
#30270,#30271,#30272,#30273,#30274,#30275,#30276,#30277,#30278,#30279,#30280,
#30281,#30282,#30283,#30284,#30285,#30286,#30287,#30288,#30289,#30290,#30291,
#30292,#30293,#30294,#30295,#30296,#30297,#30298,#30299,#30300,#30301,#30302,
#30303,#30304,#30305,#30306,#30307,#30308,#30309,#30310,#30311,#30312,#30313,
#30314,#30315,#30316,#30317,#30318,#30319,#30320,#30321,#30322,#30323,#30324,
#30325,#30326,#30327,#30328,#30329,#30330,#30331,#30332,#30333,#30334,#30335,
#30336,#30337,#30338,#30339,#30340,#30341,#30342,#30343,#30344,#30345,#30346,
#30347,#30348,#30349,#30350,#30351,#30352,#30353,#30354,#30355,#30356,#30357,
#30358,#30359,#30360,#30361,#30362,#30363,#30364,#30365,#30366,#30367,#30368,
#30369,#30370,#30371,#30372,#30373,#30374,#30375,#30376,#30377,#30378,#30379,
#30380,#30381,#30382,#30383,#30384,#30385,#30386,#30387,#30388,#30389,#30390,
#30391,#30392,#30393,#30394,#30395),.UNSPECIFIED.,.F.,.F.,(4,2,2,2,2,2,
2,2,2,2,2,2,2,2,2,2,2,2,2,2,2,2,2,2,2,2,2,2,2,2,2,2,2,2,2,2,2,2,2,2,2,2,
2,2,2,2,2,2,2,2,2,2,2,2,2,2,2,2,2,2,2,2,2,2,2,2,2,2,2,2,2,2,2,2,2,2,2,2,
2,2,2,2,2,2,2,2,2,2,2,2,2,2,2,2,2,2,2,2,2,2,2,2,2,4),(-1.58784363167967,
-1.55653980649131,-1.53682627591046,-1.53239112152884,-1.52982491184867,
-1.52758152976368,-1.52480219787095,-1.5205246686636,-1.4991362545965,-1.4495755190104,
-1.43395890214868,-1.43120089727338,-1.42970948290601,-1.42845279554363,
-1.4268725656368,-1.42378773388125,-1.40213419884548,-1.36619124270863,
-1.34057587306419,-1.33416475951176,-1.33119691501943,-1.32893222794554,
-1.32647324435256,-1.32252648248045,-1.31029044259186,-1.25706652143903,
-1.25621897288139,-1.2350281280096,-1.23195418944306,-1.2303761830444,-1.22911947666921,
-1.22762592046895,-1.22485840672266,-1.2090251233432,-1.15732730437855,
-1.13806118812672,-1.1335162372456,-1.13089886856031,-1.12868029723667,
-1.12597482324312,-1.12089126147169,-1.08347584283976,-1.04337702507936,
-1.03435336219944,-1.0318995445329,-1.03047424955446,-1.02920787039768,
-1.02752769853864,-1.02382166632852,-0.992139621717132,-0.942218023775984,
-0.935292937536694,-0.932537678671096,-0.930245188132086,-0.927890516315309,
-0.924429104431877,-0.914955356384526,-0.900725485187351,-0.84475086213516,
-0.834904872657207,-0.832404181503658,-0.830953864441757,-0.829818732357317,
-0.828248138572338,-0.825110504955073,-0.821021047967029,-0.77728167038638,
-0.739952702858024,-0.735273637980358,-0.73237221966898,-0.730116066076078,
-0.727623960439035,-0.723527910733295,-0.708336824255992,-0.657429690776177,
-0.636313026745115,-0.633241211270951,-0.631663541276157,-0.630406700922518,
-0.628912510370345,-0.626142571117113,-0.610258665634811,-0.558049427505137,
-0.539273879825064,-0.534762426406683,-0.532152499129624,-0.529911820416523,
-0.527187340481007,-0.52201373775495,-0.47680791018961,-0.439162346565744,
-0.434478173968208,-0.432577618931206,-0.431402995563107,-0.430091594735694,
-0.428156892725011,-0.422881651416646,-0.41483641160278,-0.362276266293727,
-0.354099082601777,-0.339103189566385,-0.334854231083463,-0.332328427301319,
-0.331109356375104),.UNSPECIFIED.);
#463=B_SPLINE_CURVE_WITH_KNOTS('',3,(#30400,#30401,#30402,#30403,#30404,
#30405,#30406,#30407,#30408,#30409,#30410,#30411,#30412,#30413,#30414,#30415,
#30416,#30417,#30418,#30419,#30420,#30421,#30422,#30423,#30424,#30425,#30426,
#30427,#30428,#30429,#30430,#30431,#30432,#30433,#30434,#30435,#30436,#30437,
#30438,#30439,#30440,#30441,#30442,#30443,#30444,#30445,#30446,#30447,#30448,
#30449,#30450,#30451,#30452,#30453,#30454,#30455,#30456,#30457,#30458,#30459,
#30460,#30461,#30462,#30463,#30464,#30465,#30466,#30467,#30468,#30469,#30470,
#30471,#30472,#30473,#30474,#30475,#30476,#30477,#30478,#30479,#30480,#30481,
#30482,#30483,#30484,#30485,#30486,#30487,#30488,#30489,#30490,#30491,#30492,
#30493,#30494,#30495,#30496,#30497,#30498,#30499,#30500,#30501,#30502,#30503,
#30504,#30505,#30506,#30507,#30508,#30509,#30510,#30511,#30512,#30513,#30514,
#30515,#30516,#30517,#30518,#30519,#30520,#30521,#30522,#30523,#30524,#30525,
#30526,#30527,#30528,#30529,#30530,#30531,#30532,#30533,#30534,#30535,#30536,
#30537,#30538,#30539,#30540,#30541,#30542,#30543,#30544,#30545,#30546,#30547,
#30548,#30549,#30550,#30551,#30552,#30553,#30554,#30555,#30556,#30557,#30558,
#30559,#30560,#30561,#30562,#30563,#30564,#30565,#30566,#30567,#30568,#30569,
#30570,#30571,#30572,#30573,#30574,#30575,#30576,#30577,#30578,#30579,#30580,
#30581,#30582,#30583,#30584,#30585,#30586,#30587,#30588,#30589,#30590,#30591,
#30592,#30593,#30594,#30595,#30596,#30597,#30598,#30599,#30600,#30601,#30602,
#30603,#30604,#30605,#30606,#30607,#30608,#30609,#30610,#30611,#30612,#30613,
#30614,#30615,#30616,#30617,#30618,#30619,#30620,#30621),.UNSPECIFIED.,
 .F.,.F.,(4,2,2,2,2,2,2,2,2,2,2,2,2,2,2,2,2,2,2,2,2,2,2,2,2,2,2,2,2,2,2,
2,2,2,2,2,2,2,2,2,2,2,2,2,2,2,2,2,2,2,2,2,2,2,2,2,2,2,2,2,2,2,2,2,2,2,2,
2,2,2,2,2,2,2,2,2,2,2,2,2,2,2,2,2,2,2,2,2,2,2,2,2,2,2,2,2,2,2,2,2,2,2,2,
2,2,2,2,2,2,2,4),(-2.18313823310106,-2.17650014074798,-2.16849956335008,
-2.16324663360991,-2.16131510569996,-2.16000435347047,-2.1588291534518,
-2.15692548973529,-2.15222274298792,-2.11487023056838,-2.08376576596208,
-2.0731669056622,-2.06558003609966,-2.06240529074588,-2.06010631427114,
-2.05800305845717,-2.05516924953659,-2.04822388216365,-2.00013839462087,
-1.96898236395335,-1.96374033751326,-1.96181030409453,-1.96049980788447,
-1.95932426178314,-1.957418964536,-1.9527068278182,-1.91570222526175,-1.87000896481567,
-1.86480345652993,-1.86207220397753,-1.85983102407378,-1.85722625106635,
-1.85273798025903,-1.83429862184862,-1.78172974525158,-1.76580949915184,
-1.76303771422548,-1.76154301824036,-1.7602860308786,-1.75870850659651,
-1.75563791355718,-1.73456528107433,-1.68369541475719,-1.66848094942072,
-1.66438252302699,-1.66188965770112,-1.65963325176594,-1.6567321110341,
-1.65205466644138,-1.61615542557009,-1.58024314816059,-1.56613753979821,
-1.5634497122733,-1.56197306179936,-1.56071466483217,-1.55911413597651,
-1.55655670877066,-1.54227070067467,-1.49018592542974,-1.46967833143249,
-1.46519267704807,-1.46261485308224,-1.46037166749937,-1.45760587903819,
-1.45337417161085,-1.43267580750312,-1.38240894350438,-1.37187447011469,
-1.36755647697839,-1.36428196163704,-1.36268385445326,-1.36142561557265,
-1.35994710565132,-1.35732397881196,-1.34593489590491,-1.29158172521746,
-1.27747394335548,-1.26805908156956,-1.26460544793684,-1.26225200778468,
-1.25995758854654,-1.25719621503331,-1.25023503729521,-1.22014279652187,
-1.18744383121592,-1.18147278862045,-1.16731804592522,-1.16476720102792,
-1.16316872289635,-1.16191055240079,-1.16043254288782,-1.15773815192072,
-1.14349749066547,-1.1230353616999,-1.07476600581412,-1.06783840326462,
-1.06500769531284,-1.06290523220257,-1.06060564806382,-1.05742736527376,
-1.04981897316048,-1.03917966466301,-1.00786834948704,-0.970762749794328,
-0.966051433093671,-0.964146324132916,-0.962970851662352,-0.961660393374075,
-0.959730346751497,-0.954487792326,-0.926655402496498),.UNSPECIFIED.);
#464=B_SPLINE_CURVE_WITH_KNOTS('',3,(#30623,#30624,#30625,#30626,#30627,
#30628,#30629,#30630,#30631,#30632,#30633,#30634,#30635,#30636,#30637,#30638,
#30639,#30640,#30641,#30642,#30643,#30644,#30645,#30646,#30647,#30648,#30649,
#30650,#30651,#30652,#30653,#30654,#30655,#30656,#30657,#30658,#30659,#30660,
#30661,#30662,#30663,#30664,#30665,#30666,#30667,#30668,#30669,#30670,#30671,
#30672,#30673,#30674,#30675,#30676,#30677,#30678,#30679,#30680,#30681,#30682,
#30683,#30684,#30685,#30686,#30687,#30688),.UNSPECIFIED.,.F.,.F.,(4,2,2,
2,2,2,2,2,2,2,2,2,2,2,2,2,2,2,2,2,2,2,2,2,2,2,2,2,2,2,2,2,4),(-0.331109356375104,
-0.330303897401218,-0.327570551246305,-0.322354305808374,-0.278470603079092,
-0.23948808912336,-0.23486645263933,-0.232976334313686,-0.231686962383251,
-0.230512412367563,-0.228725244679188,-0.224022011686405,-0.217062588272462,
-0.195224533200124,-0.14360464029413,-0.136858870570049,-0.133862335986385,
-0.131584959885326,-0.129159100344137,-0.125364891990015,-0.113222369558161,
-0.0848579885321056,-0.0607828913531212,-0.0560868797785358,-0.0521097054833987,
-0.037208406203165,-0.0346213853586508,-0.0330120986818491,-0.0317532478928443,
-0.0305638137843062,-0.0291095057448026,-0.026933433543985,-0.000589134625819604),
 .UNSPECIFIED.);
#465=B_SPLINE_CURVE_WITH_KNOTS('',3,(#30689,#30690,#30691,#30692,#30693,
#30694,#30695,#30696,#30697,#30698,#30699,#30700,#30701,#30702,#30703,#30704,
#30705,#30706,#30707,#30708,#30709,#30710,#30711,#30712,#30713,#30714,#30715,
#30716,#30717,#30718,#30719,#30720,#30721,#30722,#30723,#30724,#30725,#30726,
#30727,#30728,#30729,#30730,#30731,#30732,#30733,#30734,#30735,#30736,#30737,
#30738,#30739,#30740,#30741,#30742,#30743,#30744,#30745,#30746,#30747,#30748,
#30749,#30750,#30751,#30752,#30753,#30754,#30755,#30756,#30757,#30758,#30759,
#30760,#30761,#30762,#30763,#30764,#30765,#30766,#30767,#30768,#30769,#30770,
#30771,#30772,#30773,#30774,#30775,#30776,#30777,#30778,#30779,#30780,#30781,
#30782,#30783,#30784,#30785,#30786,#30787,#30788,#30789,#30790,#30791,#30792,
#30793,#30794,#30795,#30796,#30797,#30798,#30799,#30800,#30801,#30802,#30803,
#30804,#30805,#30806,#30807,#30808,#30809,#30810,#30811,#30812,#30813,#30814,
#30815,#30816,#30817,#30818,#30819,#30820,#30821,#30822,#30823,#30824,#30825,
#30826,#30827,#30828,#30829,#30830,#30831,#30832,#30833,#30834,#30835,#30836,
#30837,#30838,#30839,#30840,#30841,#30842),.UNSPECIFIED.,.F.,.F.,(4,2,2,
2,2,2,2,2,2,2,2,2,2,2,2,2,2,2,2,2,2,2,2,2,2,2,2,2,2,2,2,2,2,2,2,2,2,2,2,
2,2,2,2,2,2,2,2,2,2,2,2,2,2,2,2,2,2,2,2,2,2,2,2,2,2,2,2,2,2,2,2,2,2,2,2,
2,4),(-2.51375681360086,-2.45794213146706,-2.45071965764826,-2.44760757250335,
-2.44532072587026,-2.44320525687753,-2.44031919318414,-2.43305996673879,
-2.39470503687006,-2.37296163661332,-2.35801217863793,-2.34984917919882,
-2.34760362946983,-2.34641337301195,-2.34515585191424,-2.34355624402572,
-2.34099993793383,-2.32671139850862,-2.32106395787574,-2.27386825927659,
-2.25409208787252,-2.24965391941919,-2.24708754296824,-2.24484495058458,
-2.24206780788502,-2.23779593935463,-2.21649416166766,-2.16305184237234,
-2.15495619772662,-2.14965759124721,-2.14772017971664,-2.14640869992296,
-2.14523533076961,-2.14333926789419,-2.13867843596651,-2.10024950972278,
-2.05591925371147,-2.05072604681632,-2.04799832590834,-2.04597526168391,
-2.04344780178337,-2.03918762058278,-2.02404691056754,-2.01609730897087,
-1.96348548779911,-1.95543802649353,-1.95016278811696,-1.94822863453562,
-1.9469177773227,-1.94574376699351,-1.94384444309316,-1.939164485079,-1.90154490452413,
-1.856382454607,-1.85121484610332,-1.84849235200069,-1.84625270765591,-1.84364330378483,
-1.83913104721527,-1.82032471937217,-1.76814426432835,-1.75226448396576,
-1.74949550249777,-1.74800189206388,-1.74674557266302,-1.74516860558605,
-1.74209830147497,-1.72099784261568,-1.67013420248603,-1.65495626934021,
-1.65086249948869,-1.64837151860129,-1.64611621211735,-1.64321564406959,
-1.63853741526135,-1.60240793685852,-1.58789531626404),.UNSPECIFIED.);
#466=B_SPLINE_CURVE_WITH_KNOTS('',3,(#30848,#30849,#30850,#30851,#30852,
#30853,#30854,#30855,#30856,#30857,#30858,#30859,#30860,#30861,#30862,#30863,
#30864,#30865,#30866,#30867,#30868,#30869,#30870,#30871,#30872,#30873,#30874,
#30875,#30876,#30877,#30878,#30879,#30880,#30881,#30882,#30883,#30884,#30885,
#30886,#30887,#30888,#30889,#30890,#30891,#30892,#30893,#30894,#30895,#30896,
#30897,#30898,#30899,#30900,#30901,#30902,#30903,#30904,#30905,#30906,#30907,
#30908,#30909,#30910,#30911,#30912,#30913,#30914,#30915,#30916,#30917,#30918,
#30919,#30920,#30921,#30922,#30923,#30924,#30925,#30926,#30927,#30928,#30929,
#30930,#30931,#30932,#30933,#30934,#30935,#30936,#30937,#30938,#30939,#30940,
#30941,#30942,#30943,#30944,#30945,#30946,#30947,#30948,#30949,#30950,#30951,
#30952,#30953,#30954,#30955,#30956,#30957,#30958,#30959,#30960,#30961,#30962,
#30963,#30964,#30965,#30966,#30967,#30968,#30969,#30970,#30971,#30972,#30973,
#30974,#30975,#30976,#30977,#30978,#30979,#30980,#30981,#30982,#30983,#30984,
#30985,#30986,#30987,#30988,#30989,#30990,#30991,#30992,#30993,#30994,#30995,
#30996,#30997,#30998,#30999,#31000,#31001,#31002,#31003,#31004,#31005,#31006,
#31007),.UNSPECIFIED.,.F.,.F.,(4,2,2,2,2,2,2,2,2,2,2,2,2,2,2,2,2,2,2,2,
2,2,2,2,2,2,2,2,2,2,2,2,2,2,2,2,2,2,2,2,2,2,2,2,2,2,2,2,2,2,2,2,2,2,2,2,
2,2,2,2,2,2,2,2,2,2,2,2,2,2,2,2,2,2,2,2,2,2,2,4),(-0.926487082041935,-0.919519046294147,
-0.853132654091859,-0.850806128732264,-0.846777685742755,-0.845165205788428,
-0.843986415478232,-0.842679504961684,-0.840767190191302,-0.835647875483367,
-0.806046589922917,-0.756015259050599,-0.749101116906417,-0.746347187231973,
-0.744054631341706,-0.74169868715226,-0.738233142163533,-0.728733503487495,
-0.714451857078804,-0.685274123450052,-0.652362504504582,-0.647567338036432,
-0.64564813668675,-0.644470029801406,-0.643162466602563,-0.641246764996082,
-0.63610391052732,-0.606208788186661,-0.556561968077072,-0.550301752083055,
-0.546954121900428,-0.544855314483211,-0.542552296799797,-0.53935551746919,
-0.531635214359003,-0.520791476422158,-0.459490915981134,-0.449250893738567,
-0.446716110709871,-0.445257718833719,-0.444008966874389,-0.442388729902252,
-0.439001728829059,-0.410091087056446,-0.359401712627847,-0.350866874655805,
-0.347441217530255,-0.345328037532181,-0.343036517516631,-0.339905236346695,
-0.332578883096989,-0.322449737284953,-0.271172416483522,-0.262655587733686,
-0.249991584963173,-0.247518200743472,-0.245943073796501,-0.244686075622419,
-0.243189084274288,-0.240573585903472,-0.226724147250775,-0.189797330148935,
-0.154670677974332,-0.149998640334782,-0.147098871138603,-0.144842338239581,
-0.142348119410802,-0.139775265701751,-0.131246496577364,-0.106109691571056,
-0.0845309477201506,-0.0511203434290437,-0.0480282735500214,-0.0464460638951027,
-0.0451887123291273,-0.0436975490125595,-0.0421061898407145,-0.0395976931801813,
-0.0347318331322307,-0.000589557231629116),.UNSPECIFIED.);
#467=B_SPLINE_CURVE_WITH_KNOTS('',3,(#31008,#31009,#31010,#31011,#31012,
#31013,#31014,#31015,#31016,#31017,#31018,#31019,#31020,#31021,#31022,#31023,
#31024,#31025,#31026,#31027,#31028,#31029,#31030,#31031,#31032,#31033,#31034,
#31035,#31036,#31037,#31038,#31039,#31040,#31041,#31042,#31043,#31044,#31045,
#31046,#31047,#31048,#31049,#31050,#31051,#31052,#31053,#31054,#31055,#31056,
#31057,#31058,#31059,#31060,#31061),.UNSPECIFIED.,.F.,.F.,(4,2,2,2,2,2,
2,2,2,2,2,2,2,2,2,2,2,2,2,2,2,2,2,2,2,2,4),(-2.51392997756644,-2.47925034003837,
-2.46787561577195,-2.46443006814493,-2.46131418039933,-2.45902571130518,
-2.45690956220446,-2.45402383239197,-2.44677206785488,-2.40623254515391,
-2.37652497658567,-2.36409290225745,-2.36161581258405,-2.3601212717904,
-2.35886448832694,-2.35728731252615,-2.35421766679582,-2.33316258505554,
-2.28232116150033,-2.26711255886796,-2.2632077429606,-2.2606581810041,-2.25841224411778,
-2.25560730943267,-2.25124731827107,-2.22831283676925,-2.18313823310106),
 .UNSPECIFIED.);
#468=B_SPLINE_CURVE_WITH_KNOTS('',3,(#31062,#31063,#31064,#31065,#31066,
#31067,#31068,#31069,#31070,#31071,#31072,#31073,#31074,#31075,#31076,#31077,
#31078,#31079,#31080,#31081,#31082,#31083,#31084,#31085,#31086,#31087,#31088,
#31089,#31090,#31091,#31092,#31093,#31094,#31095,#31096,#31097,#31098,#31099,
#31100,#31101,#31102,#31103,#31104,#31105,#31106,#31107,#31108,#31109,#31110,
#31111,#31112,#31113,#31114,#31115,#31116,#31117,#31118,#31119,#31120,#31121,
#31122,#31123,#31124,#31125,#31126,#31127,#31128,#31129,#31130,#31131,#31132,
#31133,#31134,#31135,#31136,#31137,#31138,#31139,#31140,#31141,#31142,#31143,
#31144,#31145,#31146,#31147,#31148,#31149,#31150,#31151,#31152,#31153,#31154,
#31155,#31156,#31157,#31158,#31159,#31160,#31161,#31162,#31163,#31164,#31165,
#31166,#31167,#31168,#31169,#31170,#31171,#31172,#31173,#31174,#31175,#31176,
#31177,#31178,#31179,#31180,#31181,#31182,#31183,#31184,#31185,#31186,#31187,
#31188,#31189,#31190,#31191,#31192,#31193,#31194,#31195,#31196,#31197,#31198,
#31199,#31200,#31201,#31202,#31203,#31204,#31205,#31206,#31207,#31208,#31209,
#31210,#31211,#31212,#31213,#31214,#31215,#31216,#31217,#31218,#31219,#31220,
#31221,#31222,#31223,#31224,#31225,#31226,#31227,#31228,#31229,#31230,#31231,
#31232,#31233,#31234,#31235,#31236,#31237,#31238,#31239,#31240,#31241,#31242,
#31243,#31244,#31245,#31246,#31247,#31248,#31249,#31250,#31251,#31252,#31253,
#31254,#31255,#31256,#31257,#31258,#31259,#31260,#31261,#31262,#31263,#31264,
#31265,#31266,#31267,#31268,#31269,#31270,#31271,#31272,#31273,#31274,#31275,
#31276,#31277,#31278,#31279,#31280,#31281,#31282,#31283,#31284,#31285,#31286,
#31287,#31288,#31289),.UNSPECIFIED.,.F.,.F.,(4,2,2,2,2,2,2,2,2,2,2,2,2,
2,2,2,2,2,2,2,2,2,2,2,2,2,2,2,2,2,2,2,2,2,2,2,2,2,2,2,2,2,2,2,2,2,2,2,2,
2,2,2,2,2,2,2,2,2,2,2,2,2,2,2,2,2,2,2,2,2,2,2,2,2,2,2,2,2,2,2,2,2,2,2,2,
2,2,2,2,2,2,2,2,2,2,2,2,2,2,2,2,2,2,2,2,2,2,2,2,2,2,2,2,4),(-1.58789531626404,
-1.56632330799281,-1.55260822009488,-1.54994147171121,-1.5484698572259,
-1.54721170767095,-1.54560631769368,-1.54303130214716,-1.52836487517108,
-1.52461519682311,-1.5203290012024,-1.48046128243722,-1.46465960933695,
-1.45780804058913,-1.4524158361625,-1.44964691631573,-1.44740449457976,
-1.44483119678367,-1.44047708513609,-1.42375988623407,-1.419731981072,-1.36904200254157,
-1.35330846543775,-1.35054560027695,-1.34905323578783,-1.34779674539953,
-1.3462180236831,-1.34313981633201,-1.32173579179229,-1.28557433526854,
-1.25741014251873,-1.25304727454674,-1.25024182370792,-1.24799635770079,
-1.24544828740429,-1.24109590882473,-1.22262385693901,-1.17719385718619,
-1.17046508857678,-1.15414199680576,-1.15148964436731,-1.14986095769563,
-1.14860062026286,-1.14714480680467,-1.14455135921006,-1.13215052476846,
-1.10262864288724,-1.06189124980245,-1.05464303971722,-1.05175835511275,
-1.04964284529301,-1.04735495072256,-1.04423965684726,-1.0370016077036,
-1.02702903140207,-0.976068121315767,-0.954911323489691,-0.951838779759563,
-0.950261178635078,-0.949004629329425,-0.947511063962971,-0.94474301817856,
-0.928891577303083,-0.876993434721977,-0.857931354426813,-0.853400809660581,
-0.850786910127888,-0.848568451621496,-0.845859632614358,-0.840759179004347,
-0.802211488329657,-0.75959716218359,-0.758246928981988,-0.753248326244628,
-0.751295777078435,-0.750111692639656,-0.748811193966249,-0.746929145356903,
-0.742010928837825,-0.734685218248878,-0.710887218221637,-0.662321753614042,
-0.655418454892473,-0.652592377943891,-0.650491434511711,-0.648191638506678,
-0.645009619039459,-0.637375560064032,-0.626688763387258,-0.56806706677885,
-0.555215516452342,-0.552734240137113,-0.551157005829997,-0.549900336856127,
-0.548406142281509,-0.545635648562147,-0.529732423329915,-0.47730445538788,
-0.458750750228605,-0.454255168907759,-0.45164906871098,-0.44940849042876,
-0.446680157024712,-0.441486998095788,-0.396751603873804,-0.394935613176538,
-0.358755424237927,-0.354020532344979,-0.352111656716646,-0.350935627155792,
-0.349626272018241,-0.347700870858144,-0.342489365087485,-0.331435948914524),
 .UNSPECIFIED.);
#469=B_SPLINE_CURVE_WITH_KNOTS('',3,(#31294,#31295,#31296,#31297,#31298,
#31299,#31300,#31301,#31302,#31303,#31304,#31305,#31306,#31307,#31308,#31309,
#31310,#31311,#31312,#31313,#31314,#31315,#31316,#31317,#31318,#31319,#31320,
#31321,#31322,#31323,#31324,#31325,#31326,#31327,#31328,#31329,#31330,#31331,
#31332,#31333,#31334,#31335,#31336,#31337,#31338,#31339,#31340,#31341,#31342,
#31343,#31344,#31345,#31346,#31347,#31348,#31349,#31350,#31351,#31352,#31353,
#31354,#31355,#31356,#31357,#31358,#31359,#31360,#31361,#31362,#31363,#31364,
#31365,#31366,#31367,#31368,#31369,#31370,#31371,#31372,#31373,#31374,#31375,
#31376,#31377,#31378,#31379,#31380,#31381,#31382,#31383,#31384,#31385,#31386,
#31387,#31388,#31389,#31390,#31391,#31392,#31393,#31394,#31395,#31396,#31397,
#31398,#31399,#31400,#31401,#31402,#31403,#31404,#31405,#31406,#31407,#31408,
#31409,#31410,#31411,#31412,#31413,#31414,#31415,#31416,#31417,#31418,#31419,
#31420,#31421,#31422,#31423,#31424,#31425,#31426,#31427,#31428,#31429,#31430,
#31431,#31432,#31433,#31434,#31435,#31436,#31437,#31438,#31439,#31440,#31441,
#31442,#31443,#31444,#31445,#31446,#31447,#31448,#31449,#31450,#31451,#31452,
#31453,#31454,#31455,#31456,#31457,#31458,#31459,#31460,#31461,#31462,#31463,
#31464,#31465,#31466,#31467,#31468,#31469,#31470,#31471,#31472,#31473,#31474,
#31475,#31476,#31477,#31478,#31479,#31480,#31481,#31482,#31483,#31484,#31485,
#31486,#31487,#31488,#31489,#31490,#31491,#31492,#31493,#31494,#31495,#31496,
#31497,#31498,#31499,#31500,#31501,#31502,#31503,#31504,#31505,#31506,#31507,
#31508,#31509),.UNSPECIFIED.,.F.,.F.,(4,2,2,2,2,2,2,2,2,2,2,2,2,2,2,2,2,
2,2,2,2,2,2,2,2,2,2,2,2,2,2,2,2,2,2,2,2,2,2,2,2,2,2,2,2,2,2,2,2,2,2,2,2,
2,2,2,2,2,2,2,2,2,2,2,2,2,2,2,2,2,2,2,2,2,2,2,2,2,2,2,2,2,2,2,2,2,2,2,2,
2,2,2,2,2,2,2,2,2,2,2,2,2,2,2,2,2,2,4),(-2.18248318461725,-2.16336349765169,
-2.14775642214826,-2.14362542823053,-2.14112620280769,-2.13887266462903,
-2.13598720331341,-2.13135952756185,-2.09101285713337,-2.05871537336153,
-2.04532988201391,-2.04268065038738,-2.04121280606555,-2.03995418937083,
-2.03834340879016,-2.03575055044026,-2.02071709027729,-2.00365287757137,
-1.96641619692546,-1.9486888150696,-1.94438995119981,-1.94185372330336,
-1.9396067640389,-1.93678358100428,-1.93236219595033,-1.90777381868706,
-1.86134716771145,-1.84609173769782,-1.84334996726934,-1.84186210921606,
-1.84060528429423,-1.8390208785363,-1.83651548318221,-1.82321810605045,
-1.76511054911628,-1.74897914314285,-1.74480425872534,-1.74229536573777,
-1.74004382070738,-1.73717565454415,-1.73260549874066,-1.70345877118439,
-1.66127661793546,-1.64658360086218,-1.64386799739637,-1.64238580896394,
-1.64112861226076,-1.63953716091862,-1.636399004779,-1.60850569889185,-1.56832060422808,
-1.54990317304396,-1.54555492678409,-1.54300786036086,-1.54076241299782,
-1.53795583626916,-1.53358894387216,-1.51044337442874,-1.46264124661311,
-1.45229689633146,-1.44595822958394,-1.44388358670144,-1.44254247171398,
-1.4412544048148,-1.43936940494194,-1.43477616295435,-1.3953936444425,-1.36569265540894,
-1.35007293617909,-1.34594054339681,-1.34344082785594,-1.34118707567517,
-1.33830165647755,-1.33367469206995,-1.30235639717736,-1.25699012620154,
-1.24737099945124,-1.24489073699183,-1.24344531414065,-1.24230973545728,
-1.24073297319326,-1.23756375875274,-1.2334216389086,-1.22350116828241,
-1.18051471624533,-1.15227357639197,-1.1477288737738,-1.14486812041644,
-1.14261707205833,-1.1401032078919,-1.13590696259556,-1.11951961510119,
-1.05866957790602,-1.04802214982316,-1.04545456805297,-1.04398892211783,
-1.04272957398718,-1.04111446922409,-1.03775234990613,-1.00610343628861,
-0.955550692319651,-0.949374314961531,-0.946049295718204,-0.943954770855837,
-0.941648411420969,-0.938431986650012,-0.930589042675148,-0.926487082041935),
 .UNSPECIFIED.);
#470=B_SPLINE_CURVE_WITH_KNOTS('',3,(#31511,#31512,#31513,#31514,#31515,
#31516,#31517,#31518,#31519,#31520,#31521,#31522,#31523,#31524,#31525,#31526,
#31527,#31528,#31529,#31530,#31531,#31532,#31533,#31534,#31535,#31536,#31537,
#31538,#31539,#31540,#31541,#31542,#31543,#31544,#31545,#31546,#31547,#31548,
#31549,#31550,#31551,#31552,#31553,#31554,#31555,#31556,#31557,#31558,#31559,
#31560,#31561,#31562,#31563,#31564,#31565,#31566,#31567,#31568),
 .UNSPECIFIED.,.F.,.F.,(4,2,2,2,2,2,2,2,2,2,2,2,2,2,2,2,2,2,2,2,2,2,2,2,
2,2,2,2,4),(-0.331435948914524,-0.31172364526831,-0.263170569126268,-0.256269729644499,
-0.253443923322989,-0.25134291324687,-0.24904278206988,-0.245923315505089,
-0.23861127550794,-0.228414704350684,-0.176361379217015,-0.170372043346642,
-0.156223267255245,-0.153672912463893,-0.152074692451328,-0.150816698445778,
-0.149338891153073,-0.147766329218671,-0.141813366022237,-0.117459937775749,
-0.0948122256869664,-0.0607635253584692,-0.0560985289222733,-0.0532013378053364,
-0.0509457242613279,-0.0484514222973981,-0.0458781266326321,-0.0420670449395709,
-0.000589526463412705),.UNSPECIFIED.);
#471=B_SPLINE_CURVE_WITH_KNOTS('',3,(#31569,#31570,#31571,#31572,#31573,
#31574,#31575,#31576,#31577,#31578,#31579,#31580,#31581,#31582,#31583,#31584,
#31585,#31586,#31587,#31588,#31589,#31590,#31591,#31592,#31593,#31594,#31595,
#31596,#31597,#31598,#31599,#31600,#31601,#31602,#31603,#31604,#31605,#31606,
#31607,#31608,#31609,#31610,#31611,#31612,#31613,#31614,#31615,#31616,#31617,
#31618,#31619,#31620,#31621,#31622,#31623,#31624,#31625,#31626,#31627,#31628,
#31629,#31630,#31631,#31632,#31633,#31634,#31635,#31636,#31637,#31638,#31639,
#31640,#31641,#31642,#31643,#31644,#31645,#31646,#31647,#31648,#31649,#31650,
#31651,#31652,#31653,#31654,#31655,#31656,#31657,#31658,#31659,#31660,#31661,
#31662,#31663,#31664,#31665,#31666,#31667,#31668,#31669,#31670,#31671,#31672,
#31673,#31674,#31675,#31676,#31677,#31678,#31679,#31680,#31681,#31682,#31683,
#31684,#31685,#31686,#31687,#31688,#31689,#31690,#31691,#31692,#31693,#31694,
#31695,#31696,#31697,#31698,#31699,#31700,#31701,#31702,#31703,#31704,#31705,
#31706,#31707,#31708,#31709,#31710,#31711,#31712,#31713,#31714,#31715,#31716,
#31717,#31718,#31719,#31720,#31721,#31722),.UNSPECIFIED.,.F.,.F.,(4,2,2,
2,2,2,2,2,2,2,2,2,2,2,2,2,2,2,2,2,2,2,2,2,2,2,2,2,2,2,2,2,2,2,2,2,2,2,2,
2,2,2,2,2,2,2,2,2,2,2,2,2,2,2,2,2,2,2,2,2,2,2,2,2,2,2,2,2,2,2,2,2,2,2,2,
2,4),(-2.51402502574908,-2.47470167861683,-2.47062003550392,-2.46840356552127,
-2.46647396139582,-2.4651635116513,-2.46398783485779,-2.46208203007919,
-2.45736719978629,-2.42049621463849,-2.3890193225746,-2.37287541922573,
-2.36881096309099,-2.36626570081076,-2.36401867980291,-2.36120595955095,
-2.3568214433753,-2.33325996579091,-2.2888407998375,-2.27102594699721,-2.26798103580416,
-2.26639170069939,-2.26513400598461,-2.26364870331146,-2.26099585330683,
-2.24918990129547,-2.18952280113643,-2.17323531011668,-2.16904625267641,
-2.1665334770377,-2.16428137949127,-2.16141653246269,-2.15685976884375,
-2.12825919325423,-2.08552135832312,-2.07074349462449,-2.06802285906055,
-2.06653915626993,-2.06528142973848,-2.06369029740298,-2.06055574746516,
-2.03435014487387,-1.9882078129375,-1.97842959654965,-1.97129968270036,
-1.96820233117608,-1.96591683556777,-1.96379590253879,-1.96089194998257,
-1.95353338018007,-1.90152884560886,-1.87224016666654,-1.86884281858144,
-1.86722065633448,-1.86597182032097,-1.86451497458452,-1.86198660769655,
-1.85182126508958,-1.79045289250787,-1.77960610294204,-1.77188340450194,
-1.76868628535712,-1.76638325732925,-1.76428459859174,-1.76093757618218,
-1.75467941971044,-1.70494593862386,-1.67506476043248,-1.66992302203681,
-1.66800749053168,-1.66669997964575,-1.66552188110591,-1.6636026509022,
-1.6588072438466,-1.62596585191893,-1.59196095806438,-1.5879525852104),
 .UNSPECIFIED.);
#472=B_SPLINE_CURVE_WITH_KNOTS('',3,(#31728,#31729,#31730,#31731,#31732,
#31733,#31734,#31735,#31736,#31737,#31738,#31739,#31740,#31741,#31742,#31743,
#31744,#31745,#31746,#31747,#31748,#31749,#31750,#31751,#31752,#31753,#31754,
#31755,#31756,#31757,#31758,#31759,#31760,#31761,#31762,#31763,#31764,#31765,
#31766,#31767,#31768,#31769,#31770,#31771,#31772,#31773,#31774,#31775,#31776,
#31777,#31778,#31779,#31780,#31781,#31782,#31783,#31784,#31785,#31786,#31787,
#31788,#31789,#31790,#31791,#31792,#31793,#31794,#31795,#31796,#31797,#31798,
#31799,#31800,#31801,#31802,#31803,#31804,#31805,#31806,#31807,#31808,#31809,
#31810,#31811,#31812,#31813,#31814,#31815,#31816,#31817,#31818,#31819,#31820,
#31821,#31822,#31823,#31824,#31825,#31826,#31827,#31828,#31829,#31830,#31831,
#31832,#31833,#31834,#31835,#31836,#31837,#31838,#31839,#31840,#31841,#31842,
#31843,#31844,#31845,#31846,#31847,#31848,#31849,#31850,#31851,#31852,#31853,
#31854,#31855,#31856,#31857,#31858,#31859,#31860,#31861,#31862,#31863,#31864,
#31865,#31866,#31867,#31868,#31869,#31870,#31871,#31872,#31873,#31874,#31875,
#31876,#31877,#31878,#31879,#31880,#31881,#31882,#31883,#31884,#31885,#31886,
#31887,#31888,#31889,#31890,#31891,#31892,#31893,#31894,#31895,#31896,#31897,
#31898,#31899,#31900,#31901,#31902,#31903,#31904,#31905,#31906,#31907,#31908,
#31909,#31910,#31911,#31912,#31913,#31914,#31915,#31916,#31917,#31918,#31919,
#31920,#31921,#31922,#31923,#31924,#31925,#31926,#31927,#31928,#31929,#31930,
#31931,#31932,#31933),.UNSPECIFIED.,.F.,.F.,(4,2,2,2,2,2,2,2,2,2,2,2,2,
2,2,2,2,2,2,2,2,2,2,2,2,2,2,2,2,2,2,2,2,2,2,2,2,2,2,2,2,2,2,2,2,2,2,2,2,
2,2,2,2,2,2,2,2,2,2,2,2,2,2,2,2,2,2,2,2,2,2,2,2,2,2,2,2,2,2,2,2,2,2,2,2,
2,2,2,2,2,2,2,2,2,2,2,2,2,2,2,2,2,4),(-0.926835277835367,-0.925873954986695,
-0.924616719560883,-0.923122054168583,-0.920351198881222,-0.904459961791444,
-0.85218402580426,-0.833475406670089,-0.828967731157254,-0.826358178249558,
-0.824116738700649,-0.821389978043216,-0.816207851056626,-0.770588219191198,
-0.733406653481095,-0.728695513022017,-0.726790111156261,-0.725614346494368,
-0.724303452166689,-0.722372575413242,-0.717126617220737,-0.685931186638188,
-0.637914418002453,-0.630964077153999,-0.628128997746839,-0.626025068300671,
-0.623725618163677,-0.62055071342649,-0.612965900694323,-0.602370404817436,
-0.571289038902266,-0.533831200997893,-0.5291332070713,-0.527230013076427,
-0.52605466001535,-0.52474330552582,-0.522810143482474,-0.517548115017041,
-0.509530608633596,-0.457439357740223,-0.447738933322376,-0.433588926130673,
-0.429427092553468,-0.426919987581367,-0.424666203224915,-0.421789894136978,
-0.41586475120717,-0.379738571169095,-0.339499260650803,-0.330648600981391,
-0.328211072449628,-0.326788996218543,-0.325521122392203,-0.323833035129925,
-0.320086179787175,-0.290444882365525,-0.238142037225003,-0.231476457226726,
-0.228493681253355,-0.226218043360304,-0.226090576380072,-0.226019531974051,
-0.225975147795664,-0.225924403061927,-0.22587830618997,-0.225836428431162,
-0.225798378662318,-0.225763802883822,-0.225732380059235,-0.225703819142697,
-0.2256778562844,-0.225654252329823,-0.225632790482336,-0.225613274183203,
-0.225595525137274,-0.225569083041879,-0.225543190903403,-0.22551783493928,
-0.225493001826754,-0.225468678521816,-0.225444852352635,-0.222797620932892,
-0.2179184717921,-0.211809510273456,-0.198416180491977,-0.147913974553709,
-0.131910990608478,-0.129270577017266,-0.127644936627505,-0.126384195817458,
-0.124924731411772,-0.12231708124785,-0.109694986464427,-0.0577111029791184,
-0.0429217872131351,-0.0332814200974314,-0.029681477805666,-0.0275353780005982,
-0.0253744016189034,-0.0231701734708456,-0.0203093949989657,-0.0130520156989647,
-0.000589121680142322),.UNSPECIFIED.);
#473=B_SPLINE_CURVE_WITH_KNOTS('',3,(#31934,#31935,#31936,#31937,#31938,
#31939,#31940,#31941,#31942,#31943,#31944,#31945,#31946,#31947,#31948,#31949,
#31950,#31951,#31952,#31953,#31954,#31955,#31956,#31957,#31958,#31959,#31960,
#31961,#31962,#31963,#31964,#31965,#31966,#31967,#31968,#31969,#31970,#31971,
#31972,#31973,#31974,#31975,#31976,#31977,#31978,#31979,#31980,#31981,#31982,
#31983,#31984,#31985,#31986,#31987,#31988,#31989,#31990,#31991,#31992,#31993,
#31994,#31995,#31996,#31997,#31998,#31999,#32000,#32001,#32002,#32003,#32004,
#32005,#32006,#32007,#32008,#32009,#32010,#32011,#32012,#32013,#32014,#32015,
#32016,#32017),.UNSPECIFIED.,.F.,.F.,(4,2,2,2,2,2,2,2,2,2,2,2,2,2,2,2,2,
2,2,2,2,2,2,2,2,2,2,2,2,2,2,2,2,2,2,2,2,2,2,2,2,4),(-2.51280355570323,-2.45942325427332,
-2.44426263417454,-2.44152553787292,-2.44003884905819,-2.43878219077984,
-2.43719695276756,-2.43408746645967,-2.41001272855345,-2.37137025137207,
-2.35597755753649,-2.34924913535989,-2.34398785574709,-2.34125531572185,
-2.3412229317397,-2.34118921587799,-2.34115408029595,-2.34111742920532,
-2.3410791580746,-2.34103915256707,-2.34099728740793,-2.34095342507851,
-2.34090741430289,-2.34085908829961,-2.34080826280075,-2.34077591693697,
-2.34073458978196,-2.3406815253674,-2.33843678314745,-2.33563570741767,
-2.33128627055838,-2.30827056865735,-2.26033131742769,-2.24997680995143,
-2.24363387596532,-2.24155886128455,-2.24021776650185,-2.23892994151421,
-2.23704564013059,-2.23245581633457,-2.19302657914985,-2.18248318461725),
 .UNSPECIFIED.);
#474=B_SPLINE_CURVE_WITH_KNOTS('',3,(#32018,#32019,#32020,#32021,#32022,
#32023,#32024,#32025,#32026,#32027,#32028,#32029,#32030,#32031,#32032,#32033,
#32034,#32035,#32036,#32037,#32038,#32039,#32040,#32041,#32042,#32043,#32044,
#32045,#32046,#32047,#32048,#32049,#32050,#32051,#32052,#32053,#32054,#32055,
#32056,#32057,#32058,#32059,#32060,#32061,#32062,#32063,#32064,#32065,#32066,
#32067,#32068,#32069,#32070,#32071,#32072,#32073,#32074,#32075,#32076,#32077,
#32078,#32079,#32080,#32081,#32082,#32083,#32084,#32085,#32086,#32087,#32088,
#32089,#32090,#32091,#32092,#32093,#32094,#32095,#32096,#32097,#32098,#32099,
#32100,#32101,#32102,#32103,#32104,#32105,#32106,#32107,#32108,#32109,#32110,
#32111,#32112,#32113,#32114,#32115,#32116,#32117,#32118,#32119,#32120,#32121,
#32122,#32123,#32124,#32125,#32126,#32127,#32128,#32129,#32130,#32131,#32132,
#32133,#32134,#32135,#32136,#32137,#32138,#32139,#32140,#32141,#32142,#32143,
#32144,#32145,#32146,#32147,#32148,#32149,#32150,#32151,#32152,#32153,#32154,
#32155,#32156,#32157,#32158,#32159,#32160,#32161,#32162,#32163,#32164,#32165,
#32166,#32167,#32168,#32169,#32170,#32171,#32172,#32173,#32174,#32175,#32176,
#32177,#32178,#32179,#32180,#32181,#32182,#32183,#32184,#32185,#32186,#32187,
#32188,#32189,#32190,#32191,#32192,#32193,#32194,#32195,#32196,#32197,#32198,
#32199,#32200,#32201,#32202,#32203,#32204,#32205,#32206,#32207,#32208,#32209,
#32210,#32211,#32212,#32213,#32214,#32215,#32216,#32217,#32218,#32219,#32220,
#32221,#32222,#32223,#32224,#32225,#32226,#32227,#32228,#32229,#32230,#32231,
#32232,#32233,#32234,#32235,#32236,#32237,#32238,#32239),.UNSPECIFIED.,
 .F.,.F.,(4,2,2,2,2,2,2,2,2,2,2,2,2,2,2,2,2,2,2,2,2,2,2,2,2,2,2,2,2,2,2,
2,2,2,2,2,2,2,2,2,2,2,2,2,2,2,2,2,2,2,2,2,2,2,2,2,2,2,2,2,2,2,2,2,2,2,2,
2,2,2,2,2,2,2,2,2,2,2,2,2,2,2,2,2,2,2,2,2,2,2,2,2,2,2,2,2,2,2,2,2,2,2,2,
2,2,2,2,2,2,2,4),(-1.5879525852104,-1.57458975846264,-1.57031589714921,
-1.56778442442157,-1.56553552113557,-1.56270165497985,-1.55824738786618,
-1.53283690906585,-1.48713337491167,-1.47695949055901,-1.47069522210094,
-1.46862911772098,-1.4672894683517,-1.46599934335257,-1.46410597685683,
-1.45946567791737,-1.42081262487195,-1.3905755159231,-1.37478462430487,
-1.37063640389922,-1.36813248210081,-1.36587836901618,-1.36299724250785,
-1.35838683962124,-1.32784152922721,-1.32046832379782,-1.29791034683781,
-1.27511800236025,-1.27060440611576,-1.26878500556775,-1.26749616821184,
-1.26613064332966,-1.26394701480732,-1.25734176148359,-1.20613204574239,
-1.17688360054628,-1.17230876636834,-1.1694384613991,-1.16718575653382,
-1.16467611364536,-1.16050128245191,-1.14438835909185,-1.11308895462519,
-1.07593598975129,-1.07122413184009,-1.06931887704709,-1.06814334149643,
-1.06683285438391,-1.06490286406299,-1.0596611051626,-1.02851446561567,
-0.980429497837874,-0.973484364673308,-0.970650578686587,-0.968547315311905,
-0.966248311079458,-0.96307351276614,-0.955486563056699,-0.944886569682506,
-0.913780305458279,-0.876351126063622,-0.87165146342062,-0.869748261097883,
-0.868573111342117,-0.867262200115879,-0.865330097651549,-0.860073486389425,
-0.852066583450143,-0.800148059178257,-0.789871417493344,-0.776037280291282,
-0.771909406682415,-0.76941016981365,-0.767155410872964,-0.764266713540674,
-0.758275540828574,-0.71361597576308,-0.67677955776591,-0.672063761634389,
-0.670157855106759,-0.668982205056979,-0.667671868691615,-0.665742584942656,
-0.66050570585247,-0.629421761550526,-0.581258922383746,-0.574319923965814,
-0.571487204135684,-0.569384211666245,-0.567084995480548,-0.563908970881281,
-0.556314561231851,-0.545700973670453,-0.514525319663746,-0.477193503629126,
-0.47249153165773,-0.470587950222745,-0.469412736280955,-0.46810191850319,
-0.466170240828056,-0.460916546151231,-0.452915598598613,-0.401094191418584,
-0.378171405590259,-0.373813392885962,-0.371008939127249,-0.368762898642373,
-0.366212698859851,-0.361853005045509,-0.343290147407682,-0.331151912909351),
 .UNSPECIFIED.);
#475=B_SPLINE_CURVE_WITH_KNOTS('',3,(#32244,#32245,#32246,#32247,#32248,
#32249,#32250,#32251,#32252,#32253,#32254,#32255,#32256,#32257,#32258,#32259,
#32260,#32261,#32262,#32263,#32264,#32265,#32266,#32267,#32268,#32269,#32270,
#32271,#32272,#32273,#32274,#32275,#32276,#32277,#32278,#32279,#32280,#32281,
#32282,#32283,#32284,#32285,#32286,#32287,#32288,#32289,#32290,#32291,#32292,
#32293,#32294,#32295,#32296,#32297,#32298,#32299,#32300,#32301,#32302,#32303,
#32304,#32305,#32306,#32307,#32308,#32309,#32310,#32311,#32312,#32313,#32314,
#32315,#32316,#32317,#32318,#32319,#32320,#32321,#32322,#32323,#32324,#32325,
#32326,#32327,#32328,#32329,#32330,#32331,#32332,#32333,#32334,#32335,#32336,
#32337,#32338,#32339,#32340,#32341,#32342,#32343,#32344,#32345,#32346,#32347,
#32348,#32349,#32350,#32351,#32352,#32353,#32354,#32355,#32356,#32357,#32358,
#32359,#32360,#32361,#32362,#32363,#32364,#32365,#32366,#32367,#32368,#32369,
#32370,#32371,#32372,#32373,#32374,#32375,#32376,#32377,#32378,#32379,#32380,
#32381,#32382,#32383,#32384,#32385,#32386,#32387,#32388,#32389,#32390,#32391,
#32392,#32393,#32394,#32395,#32396,#32397,#32398,#32399,#32400,#32401,#32402,
#32403,#32404,#32405,#32406,#32407,#32408,#32409,#32410,#32411,#32412,#32413,
#32414,#32415,#32416,#32417,#32418,#32419,#32420,#32421,#32422,#32423,#32424,
#32425,#32426,#32427,#32428,#32429,#32430,#32431,#32432,#32433,#32434,#32435,
#32436,#32437,#32438,#32439,#32440,#32441,#32442,#32443,#32444,#32445,#32446,
#32447,#32448,#32449,#32450,#32451,#32452,#32453,#32454,#32455,#32456,#32457,
#32458,#32459,#32460,#32461),.UNSPECIFIED.,.F.,.F.,(4,2,2,2,2,2,2,2,2,2,
2,2,2,2,2,2,2,2,2,2,2,2,2,2,2,2,2,2,2,2,2,2,2,2,2,2,2,2,2,2,2,2,2,2,2,2,
2,2,2,2,2,2,2,2,2,2,2,2,2,2,2,2,2,2,2,2,2,2,2,2,2,2,2,2,2,2,2,2,2,2,2,2,
2,2,2,2,2,2,2,2,2,2,2,2,2,2,2,2,2,2,2,2,2,2,2,2,2,2,4),(-2.18338867985252,
-2.17304102988321,-2.14381756447417,-2.1271921983873,-2.12439157541843,
-2.12289076920439,-2.12163422263203,-2.12006425966396,-2.11702845541298,
-2.09720648249968,-2.0452628747484,-2.02984328028683,-2.0257272289343,-2.02323064208988,
-2.02097537416667,-2.01808198470289,-2.01342992921446,-1.97361130766299,
-1.9449569257605,-1.92769844533424,-1.92487370296174,-1.92336787825266,
-1.92211158462659,-1.9205475312516,-1.91811005656014,-1.90600388047791,
-1.85236702256448,-1.83831538914147,-1.82892820216747,-1.82547838001922,
-1.82312566603208,-1.82083051271919,-1.81806650850368,-1.81108909052652,
-1.76168820128402,-1.73157398844635,-1.72641370241309,-1.72449536261635,
-1.72318718926321,-1.72200949545005,-1.7200926604049,-1.71531175522481,
-1.68116104507842,-1.64814376354915,-1.63106079131407,-1.62680882216696,
-1.62428212525191,-1.62203237841302,-1.61919059209525,-1.61471032533007,
-1.58857937680316,-1.54357474743067,-1.52849283191948,-1.52575798827675,
-1.52427119393879,-1.52301364856646,-1.5214262796317,-1.51891239275892,
-1.50547285596822,-1.49829187463721,-1.47797313779314,-1.43317493124286,
-1.42799749527775,-1.42527192048741,-1.42303080119901,-1.42042087737265,
-1.41591070050339,-1.39716179654827,-1.34490038017141,-1.32900828147958,
-1.32623749695321,-1.32474293226893,-1.32348580182992,-1.32190778247953,
-1.31942492141555,-1.30654851665753,-1.30464536226076,-1.30116546215753,
-1.28765141072812,-1.25764727507516,-1.23319178199413,-1.22877343820248,
-1.22595018234654,-1.22370189341153,-1.22116281080147,-1.2168557943578,
-1.19904517832619,-1.1614926124188,-1.14636738239161,-1.1298255910023,-1.12716366101996,
-1.12553164279912,-1.1242703544355,-1.12281527533551,-1.12022747617846,
-1.10793741531231,-1.07891704772819,-1.03752382415657,-1.03028082601933,
-1.02739609263648,-1.02527979888145,-1.02299033730041,-1.01987161430627,
-1.01261958760833,-1.00262356482312,-0.951655457150748,-0.930525054975316,
-0.927452143251984,-0.926835277835367),.UNSPECIFIED.);
#476=B_SPLINE_CURVE_WITH_KNOTS('',3,(#32463,#32464,#32465,#32466,#32467,
#32468,#32469,#32470,#32471,#32472,#32473,#32474,#32475,#32476,#32477,#32478,
#32479,#32480,#32481,#32482,#32483,#32484,#32485,#32486,#32487,#32488,#32489,
#32490,#32491,#32492,#32493,#32494,#32495,#32496,#32497,#32498,#32499,#32500,
#32501,#32502,#32503,#32504,#32505,#32506,#32507,#32508,#32509,#32510,#32511,
#32512,#32513,#32514,#32515,#32516,#32517,#32518,#32519,#32520,#32521,#32522,
#32523,#32524,#32525,#32526,#32527,#32528,#32529,#32530,#32531,#32532,#32533,
#32534,#32535,#32536,#32537,#32538,#32539,#32540,#32541,#32542,#32543,#32544,
#32545,#32546,#32547,#32548),.UNSPECIFIED.,.F.,.F.,(4,2,2,2,2,2,2,2,2,2,
2,2,2,2,2,2,2,2,2,2,2,2,2,2,2,2,2,2,2,2,2,2,2,2,2,2,2,2,2,2,2,2,4),(-0.331151912909351,
-0.302471423886003,-0.275268135967566,-0.272128314356745,-0.270536129369491,
-0.269278417518081,-0.267795714444919,-0.265079445863502,-0.250389152885383,
-0.208251852747366,-0.179067406331704,-0.174477397694502,-0.171602589951601,
-0.169349459873731,-0.169264139805164,-0.169198402560599,-0.169147373229639,
-0.169107530917496,-0.169076282320816,-0.169025601796399,-0.16897739650466,
-0.168931486879703,-0.168887710062428,-0.168845918062359,-0.168805976109094,
-0.168767761222614,-0.168731161031078,-0.168696072668769,-0.168662401753735,
-0.168630061519431,-0.165890851613642,-0.160611945406604,-0.153849295199289,
-0.138345925343512,-0.0988768538035574,-0.0756831005859633,-0.072574003326672,
-0.0709883571160977,-0.0697310616221267,-0.0682432680326189,-0.0655032703358452,
-0.0503020257269651,-0.000590129853255855),.UNSPECIFIED.);
#477=B_SPLINE_CURVE_WITH_KNOTS('',3,(#32549,#32550,#32551,#32552,#32553,
#32554,#32555,#32556,#32557,#32558,#32559,#32560,#32561,#32562,#32563,#32564,
#32565,#32566,#32567,#32568,#32569,#32570,#32571,#32572,#32573,#32574,#32575,
#32576,#32577,#32578,#32579,#32580,#32581,#32582,#32583,#32584,#32585,#32586,
#32587,#32588,#32589,#32590,#32591,#32592,#32593,#32594,#32595,#32596,#32597,
#32598,#32599,#32600,#32601,#32602,#32603,#32604,#32605,#32606,#32607,#32608,
#32609,#32610,#32611,#32612,#32613,#32614,#32615,#32616,#32617,#32618,#32619,
#32620,#32621,#32622,#32623,#32624,#32625,#32626,#32627,#32628,#32629,#32630,
#32631,#32632,#32633,#32634,#32635,#32636,#32637,#32638,#32639,#32640,#32641,
#32642,#32643,#32644,#32645,#32646,#32647,#32648,#32649,#32650,#32651,#32652,
#32653,#32654,#32655,#32656,#32657,#32658,#32659,#32660,#32661,#32662,#32663,
#32664,#32665,#32666,#32667,#32668,#32669,#32670,#32671,#32672,#32673,#32674,
#32675,#32676,#32677,#32678,#32679,#32680,#32681,#32682,#32683,#32684,#32685,
#32686,#32687,#32688,#32689,#32690),.UNSPECIFIED.,.F.,.F.,(4,3,3,3,3,3,
3,3,3,3,3,3,3,3,3,3,3,3,3,3,3,3,3,3,3,3,3,3,3,3,3,3,3,3,3,3,3,3,3,3,3,3,
3,3,3,3,3,4),(147.65485471872,147.7596787603,147.864497286824,147.974284115959,
148.079269184167,148.184337191304,148.289587067188,148.303644603364,148.408603236093,
148.513404407742,148.618082360711,148.72269449813,148.82727638342,148.931863536024,
149.036561338889,149.141320371478,149.246261485861,149.301361766912,149.406320459688,
149.51112169103,149.615799702885,149.720411898661,149.824993841696,149.929581051351,
150.034278909835,150.139037997312,150.24397916487,150.299078930459,150.404037717633,
150.508839044419,150.613517152794,150.718129445701,150.822711486324,150.92729879388,
151.031996750053,151.136755935245,151.241697199507,151.296796094007,151.401755143354,
151.506556527578,151.611233913488,151.715845195958,151.820425938971,151.925011662141,
152.029704696172,152.134458843432,152.23938750251,152.284650028018),
 .UNSPECIFIED.);
#478=B_SPLINE_CURVE_WITH_KNOTS('',3,(#32696,#32697,#32698,#32699,#32700,
#32701,#32702,#32703,#32704,#32705,#32706,#32707,#32708,#32709,#32710,#32711,
#32712,#32713,#32714,#32715,#32716,#32717,#32718,#32719,#32720,#32721,#32722,
#32723,#32724,#32725,#32726,#32727,#32728,#32729,#32730,#32731,#32732,#32733,
#32734,#32735,#32736,#32737,#32738,#32739,#32740,#32741,#32742,#32743,#32744,
#32745,#32746,#32747,#32748,#32749,#32750,#32751,#32752,#32753,#32754,#32755,
#32756,#32757,#32758,#32759,#32760,#32761,#32762,#32763,#32764,#32765,#32766,
#32767,#32768,#32769,#32770,#32771,#32772,#32773,#32774,#32775,#32776,#32777,
#32778,#32779,#32780,#32781,#32782,#32783,#32784,#32785,#32786,#32787,#32788,
#32789,#32790,#32791,#32792,#32793,#32794,#32795,#32796,#32797,#32798,#32799,
#32800,#32801,#32802,#32803,#32804,#32805,#32806,#32807,#32808,#32809,#32810,
#32811,#32812,#32813,#32814,#32815,#32816,#32817,#32818,#32819,#32820,#32821,
#32822,#32823,#32824,#32825,#32826,#32827,#32828,#32829,#32830,#32831,#32832,
#32833,#32834,#32835,#32836,#32837),.UNSPECIFIED.,.F.,.F.,(4,3,3,3,3,3,
3,3,3,3,3,3,3,3,3,3,3,3,3,3,3,3,3,3,3,3,3,3,3,3,3,3,3,3,3,3,3,3,3,3,3,3,
3,3,3,3,3,4),(153.9380400259,153.974863605114,154.079804365441,154.184587631212,
154.289247714775,154.393842015211,154.498406122077,154.602975581005,154.707655938966,
154.812397641858,154.917321790079,154.972580768661,155.077561582248,155.182384840127,
155.28708463541,155.391718452278,155.496321823315,155.600930236945,155.705648817651,
155.810428384599,155.915389438099,155.970297932209,156.075278237136,156.180101410843,
156.284801742362,156.389436478036,156.49404114557,156.598651228907,156.703372026609,
156.808154124326,156.913118164361,156.968015095757,157.07284356268,157.177514242715,
157.282061843758,157.386543784192,157.490995815696,157.595453646235,157.700023809841,
157.804655964143,157.909472737595,157.965732259304,158.070872240667,158.175862782332,
158.280733003082,158.385531426381,158.490318442128,158.567664456021),
 .UNSPECIFIED.);
#479=B_SPLINE_CURVE_WITH_KNOTS('',3,(#32838,#32839,#32840,#32841,#32842,
#32843,#32844,#32845,#32846,#32847,#32848,#32849,#32850,#32851,#32852,#32853,
#32854,#32855,#32856,#32857,#32858,#32859,#32860,#32861,#32862,#32863,#32864,
#32865,#32866,#32867,#32868,#32869,#32870,#32871,#32872,#32873,#32874,#32875,
#32876,#32877,#32878,#32879,#32880,#32881,#32882,#32883,#32884,#32885,#32886,
#32887,#32888,#32889,#32890,#32891,#32892,#32893,#32894,#32895,#32896,#32897,
#32898,#32899,#32900,#32901,#32902,#32903,#32904,#32905,#32906,#32907,#32908,
#32909),.UNSPECIFIED.,.F.,.F.,(4,2,2,2,2,2,2,2,2,2,2,2,2,2,2,2,2,2,2,2,
2,2,2,2,2,2,2,2,2,2,2,2,2,2,2,4),(-2.5140779328986,-2.47849070595892,-2.44670937580689,
-2.42920952710399,-2.42492483703576,-2.42239027827562,-2.42014066872104,
-2.41730862047916,-2.41286246276546,-2.38769182458136,-2.34612449882485,
-2.33310382859779,-2.32811400782696,-2.32556025767983,-2.32395001442939,
-2.32246645753187,-2.32245942734251,-2.32245234484813,-2.32244520895705,
-2.32243801850278,-2.32243077248093,-2.32242346972502,-2.32241610902578,
-2.32240868916012,-2.32118643060593,-2.31961822636813,-2.31659184641,-2.29693492462091,
-2.24483702526331,-2.22939701795696,-2.2252787097483,-2.22278132735393,
-2.22052570599751,-2.21763236829677,-2.21298142448337,-2.18338867985252),
 .UNSPECIFIED.);
#480=B_SPLINE_CURVE_WITH_KNOTS('',3,(#32911,#32912,#32913,#32914,#32915,
#32916,#32917,#32918,#32919,#32920,#32921,#32922,#32923,#32924,#32925,#32926,
#32927,#32928,#32929,#32930,#32931,#32932,#32933,#32934,#32935,#32936,#32937,
#32938,#32939,#32940,#32941,#32942,#32943,#32944,#32945,#32946,#32947,#32948,
#32949,#32950,#32951,#32952,#32953,#32954,#32955,#32956,#32957,#32958,#32959,
#32960,#32961,#32962,#32963,#32964,#32965),.UNSPECIFIED.,.F.,.F.,(4,3,3,
3,3,3,3,3,3,3,3,3,3,3,3,3,3,3,4),(152.284650028018,152.294513257555,152.399472165554,
152.504273610123,152.608951831273,152.7135642338,152.818146380757,152.92273379122,
153.027431844461,153.132191123553,153.237132475827,153.292230421102,153.397521479036,
153.502654337752,153.611500759789,153.71641998599,153.821291112116,153.926162314978,
153.9380400259),.UNSPECIFIED.);
#481=B_SPLINE_CURVE_WITH_KNOTS('',3,(#32966,#32967,#32968,#32969,#32970,
#32971,#32972,#32973,#32974),.UNSPECIFIED.,.F.,.F.,(4,1,1,1,1,1,4),(153.938047498774,
154.28994758465,155.287664748197,156.285381911745,157.283099075293,158.28081623884,
158.568767222197),.UNSPECIFIED.);
#482=B_SPLINE_CURVE_WITH_KNOTS('',3,(#32978,#32979,#32980,#32981,#32982,
#32983),.UNSPECIFIED.,.F.,.F.,(4,1,1,4),(-4.09157007060747,-3.99086865419044,
-2.99315149064283,-2.06679288006903),.UNSPECIFIED.);
#483=B_SPLINE_CURVE_WITH_KNOTS('',3,(#32987,#32988,#32989,#32990,#32991),
 .UNSPECIFIED.,.F.,.F.,(4,1,4),(0.,0.997717163547601,1.11662023360664),
 .UNSPECIFIED.);
#484=B_SPLINE_CURVE_WITH_KNOTS('',3,(#32993,#32994,#32995,#32996,#32997,
#32998,#32999,#33000,#33001,#33002,#33003,#33004,#33005,#33006,#33007,#33008,
#33009,#33010,#33011,#33012,#33013,#33014,#33015,#33016,#33017,#33018,#33019,
#33020,#33021,#33022,#33023,#33024,#33025,#33026,#33027,#33028,#33029,#33030,
#33031,#33032,#33033,#33034,#33035,#33036,#33037,#33038,#33039,#33040,#33041,
#33042,#33043,#33044,#33045,#33046,#33047,#33048,#33049,#33050,#33051,#33052,
#33053,#33054,#33055,#33056,#33057,#33058,#33059,#33060,#33061,#33062,#33063,
#33064,#33065,#33066,#33067,#33068,#33069,#33070,#33071,#33072,#33073,#33074,
#33075,#33076,#33077,#33078,#33079,#33080,#33081,#33082,#33083,#33084,#33085,
#33086,#33087,#33088,#33089,#33090,#33091,#33092,#33093,#33094,#33095,#33096,
#33097,#33098,#33099,#33100,#33101,#33102,#33103,#33104,#33105,#33106,#33107,
#33108,#33109,#33110,#33111,#33112,#33113,#33114,#33115,#33116,#33117,#33118,
#33119,#33120,#33121,#33122,#33123,#33124,#33125,#33126,#33127,#33128,#33129,
#33130,#33131,#33132,#33133,#33134,#33135,#33136,#33137,#33138,#33139,#33140,
#33141,#33142,#33143,#33144,#33145,#33146,#33147,#33148,#33149,#33150,#33151,
#33152,#33153,#33154,#33155,#33156,#33157,#33158,#33159,#33160,#33161,#33162,
#33163,#33164,#33165,#33166,#33167,#33168,#33169,#33170,#33171,#33172,#33173,
#33174,#33175,#33176,#33177,#33178,#33179,#33180,#33181,#33182),
 .UNSPECIFIED.,.F.,.F.,(4,3,3,3,3,3,3,3,3,3,3,3,3,3,3,3,3,3,3,3,3,3,3,3,
3,3,3,3,3,3,3,3,3,3,3,3,3,3,3,3,3,3,3,3,3,3,3,3,3,3,3,3,3,3,3,3,3,3,3,3,
3,3,3,4),(1.11662023360664,1.21403017783247,1.31170569649031,1.40889083867501,
1.50602851129987,1.60315132101257,1.70122207253323,1.79846974995715,1.89695203852618,
1.99543432709521,2.09523986473024,2.19490213157771,2.29468330146085,2.39416483461276,
2.49361268276311,2.59305713236532,2.69308072193469,2.79266593261604,2.89290871162943,
2.99315149064282,3.09301416604425,3.19273726352095,3.29250368735464,3.39205463887835,
3.49157499828158,3.5910949646367,3.69103838702513,3.79070576812542,3.89078721115793,
3.99086865419044,4.09044699529707,4.18988074033137,4.2897188750072,4.38897039473104,
4.48818819271083,4.58740287522122,4.68769861085042,4.78705712910369,4.88782147342087,
4.98858581773805,5.08830325928589,5.18787780272281,5.28768095004317,5.38707637536471,
5.48643893157123,5.58579903228547,5.68592501953552,5.78542910701009,5.88586604414787,
5.98630298128566,6.08601752413451,6.18558951336581,6.28539334229924,6.38478707876317,
6.48414827749628,6.58350735551845,6.68363555284716,6.78313945746615,6.88357980114971,
6.98402014483327,7.09349031126651,7.2026554514492,7.31130400709731,7.39980554040953),
 .UNSPECIFIED.);
#485=B_SPLINE_CURVE_WITH_KNOTS('',3,(#33184,#33185,#33186,#33187,#33188,
#33189,#33190,#33191,#33192,#33193,#33194,#33195,#33196,#33197,#33198,#33199,
#33200,#33201,#33202,#33203,#33204,#33205,#33206,#33207,#33208,#33209,#33210,
#33211,#33212,#33213,#33214,#33215,#33216,#33217,#33218,#33219,#33220,#33221,
#33222,#33223,#33224,#33225,#33226,#33227,#33228,#33229,#33230,#33231,#33232,
#33233,#33234,#33235,#33236,#33237,#33238,#33239,#33240,#33241,#33242,#33243,
#33244,#33245,#33246,#33247,#33248,#33249,#33250,#33251,#33252,#33253,#33254,
#33255,#33256,#33257,#33258,#33259,#33260,#33261,#33262,#33263,#33264,#33265,
#33266,#33267,#33268,#33269,#33270,#33271,#33272,#33273,#33274,#33275,#33276,
#33277,#33278,#33279,#33280,#33281,#33282,#33283,#33284,#33285,#33286,#33287,
#33288,#33289,#33290,#33291,#33292,#33293,#33294,#33295,#33296,#33297,#33298,
#33299,#33300,#33301,#33302,#33303,#33304,#33305,#33306,#33307,#33308,#33309,
#33310,#33311,#33312,#33313,#33314,#33315,#33316,#33317,#33318,#33319,#33320,
#33321,#33322,#33323,#33324,#33325,#33326,#33327,#33328,#33329,#33330,#33331,
#33332,#33333,#33334,#33335,#33336,#33337,#33338,#33339,#33340,#33341,#33342,
#33343,#33344,#33345,#33346,#33347,#33348,#33349,#33350,#33351,#33352,#33353,
#33354,#33355,#33356,#33357,#33358,#33359,#33360,#33361,#33362,#33363,#33364,
#33365,#33366,#33367,#33368,#33369,#33370,#33371,#33372,#33373,#33374,#33375,
#33376),.UNSPECIFIED.,.F.,.F.,(4,3,3,3,3,3,3,3,3,3,3,3,3,3,3,3,3,3,3,3,
3,3,3,3,3,3,3,3,3,3,3,3,3,3,3,3,3,3,3,3,3,3,3,3,3,3,3,3,3,3,3,3,3,3,3,3,
3,3,3,3,3,3,3,3,4),(7.39980554078624,7.50091414539458,7.60207208886389,
7.70338883416616,7.80478910492028,7.90640042005354,7.98173730838088,8.08143708868561,
8.18099393916635,8.28080150576161,8.38017929631084,8.47952428002577,8.57886689516197,
8.6790137893536,8.7785007869756,8.87897762945204,8.97945447192849,9.0791522318597,
9.1787070823736,9.27851515151141,9.37789100753077,9.47723408588057,9.57657482757993,
9.67672402955397,9.77620925214669,9.87669044381139,9.9771716354761,10.0768652714557,
10.1764159173836,10.2762250275886,10.3755965132625,10.474935168476,10.5742714401109,
10.6744257798391,10.7739064621368,10.8743976305802,10.9748887990237,11.0745852497462,
11.1741387497813,11.2739471513801,11.3733215659471,11.4726631716966,11.5720024115391,
11.6721532992972,11.7716369630197,11.8721214627955,11.9726059625713,12.0723019306664,
12.1718549473224,12.2716634696719,12.371037402717,12.4703785287419,12.5697172913276,
12.6698687500254,12.7693519475211,12.86983753682,12.9703231261189,13.0692183781977,
13.1679810507849,13.2666427695192,13.3652350418257,13.463808588127,13.5623731344459,
13.6609891043227,13.6829908479658),.UNSPECIFIED.);
#486=B_SPLINE_CURVE_WITH_KNOTS('',3,(#33378,#33379,#33380,#33381,#33382,
#33383,#33384,#33385,#33386,#33387,#33388,#33389,#33390,#33391,#33392,#33393,
#33394,#33395,#33396,#33397,#33398,#33399,#33400,#33401,#33402,#33403,#33404,
#33405,#33406,#33407,#33408,#33409,#33410,#33411,#33412,#33413,#33414,#33415,
#33416,#33417,#33418,#33419,#33420,#33421,#33422,#33423,#33424,#33425,#33426,
#33427,#33428,#33429,#33430,#33431,#33432,#33433,#33434,#33435,#33436,#33437,
#33438,#33439,#33440,#33441,#33442,#33443,#33444,#33445,#33446,#33447,#33448,
#33449,#33450,#33451,#33452,#33453,#33454,#33455,#33456,#33457,#33458,#33459,
#33460,#33461,#33462,#33463,#33464,#33465,#33466,#33467,#33468,#33469,#33470,
#33471,#33472,#33473,#33474,#33475,#33476,#33477,#33478,#33479,#33480,#33481,
#33482,#33483,#33484,#33485,#33486,#33487,#33488,#33489,#33490,#33491,#33492,
#33493,#33494,#33495,#33496,#33497,#33498,#33499,#33500,#33501,#33502,#33503,
#33504,#33505,#33506,#33507,#33508,#33509,#33510,#33511,#33512,#33513,#33514,
#33515,#33516,#33517,#33518,#33519,#33520,#33521,#33522,#33523,#33524,#33525,
#33526,#33527,#33528,#33529,#33530,#33531,#33532,#33533,#33534,#33535,#33536,
#33537,#33538,#33539,#33540,#33541,#33542,#33543,#33544,#33545,#33546,#33547,
#33548,#33549,#33550,#33551,#33552,#33553,#33554,#33555,#33556,#33557,#33558,
#33559,#33560,#33561,#33562,#33563,#33564,#33565,#33566,#33567,#33568,#33569,
#33570),.UNSPECIFIED.,.F.,.F.,(4,3,3,3,3,3,3,3,3,3,3,3,3,3,3,3,3,3,3,3,
3,3,3,3,3,3,3,3,3,3,3,3,3,3,3,3,3,3,3,3,3,3,3,3,3,3,3,3,3,3,3,3,3,3,3,3,
3,3,3,3,3,3,3,3,4),(13.6829908482444,13.8045870330681,13.9281224185238,
13.9680402896666,14.0677361753039,14.1672891052979,14.2670976487875,14.3664714855134,
14.465812511784,14.5651511713017,14.6653027417798,14.7647858290595,14.8652716411369,
14.9657574532142,15.0654532473382,15.1650060852554,15.2648146516937,15.3641883956647,
15.4635293291348,15.5628678959341,15.663019576141,15.7625025718607,15.8629885943112,
15.9634746167618,16.0631703607544,16.1627231473695,16.262531726487,16.3619054166746,
16.4612462955444,16.5605848069985,16.6607365503262,16.7602194894246,16.860705634867,
16.9611917803094,17.0608875760243,17.1604404151583,17.2602489812456,17.3596227255052,
17.4589636589118,17.5583022252944,17.658453904935,17.7579368993666,17.8584229216118,
17.958908943857,18.0586047239988,18.1581575474241,18.2579661174216,18.35733984576,
18.4566807632012,18.556019313596,18.6561710120482,18.7556539906012,18.8561400490029,
18.9566261074046,19.0563218826592,19.1558747010642,19.2556832723002,19.3550569953302,
19.454397907366,19.5537364522654,19.6538881569371,19.7533711298283,19.8538572003902,
19.9543432709522,19.9661761551454),.UNSPECIFIED.);
#487=B_SPLINE_CURVE_WITH_KNOTS('',3,(#33572,#33573,#33574,#33575,#33576,
#33577,#33578,#33579,#33580,#33581,#33582,#33583,#33584,#33585,#33586,#33587,
#33588,#33589,#33590,#33591,#33592,#33593,#33594,#33595,#33596,#33597,#33598,
#33599,#33600,#33601,#33602,#33603,#33604,#33605,#33606,#33607,#33608,#33609,
#33610,#33611,#33612,#33613,#33614,#33615,#33616,#33617,#33618,#33619,#33620,
#33621,#33622,#33623,#33624,#33625,#33626,#33627,#33628,#33629,#33630,#33631,
#33632,#33633,#33634,#33635,#33636,#33637,#33638,#33639,#33640,#33641,#33642,
#33643,#33644,#33645,#33646,#33647,#33648,#33649,#33650,#33651,#33652,#33653,
#33654,#33655,#33656,#33657,#33658,#33659,#33660,#33661,#33662,#33663,#33664,
#33665,#33666,#33667,#33668,#33669,#33670,#33671,#33672,#33673,#33674,#33675,
#33676,#33677,#33678,#33679,#33680,#33681,#33682,#33683,#33684,#33685,#33686,
#33687,#33688,#33689,#33690,#33691,#33692,#33693,#33694,#33695,#33696,#33697,
#33698,#33699,#33700,#33701,#33702,#33703,#33704,#33705,#33706,#33707,#33708,
#33709,#33710,#33711,#33712,#33713,#33714,#33715,#33716,#33717,#33718,#33719,
#33720,#33721,#33722,#33723,#33724,#33725,#33726,#33727,#33728,#33729,#33730,
#33731,#33732,#33733,#33734,#33735,#33736,#33737,#33738,#33739,#33740,#33741,
#33742,#33743,#33744,#33745,#33746,#33747,#33748,#33749,#33750,#33751,#33752,
#33753,#33754,#33755,#33756,#33757,#33758,#33759,#33760,#33761),
 .UNSPECIFIED.,.F.,.F.,(4,3,3,3,3,3,3,3,3,3,3,3,3,3,3,3,3,3,3,3,3,3,3,3,
3,3,3,3,3,3,3,3,3,3,3,3,3,3,3,3,3,3,3,3,3,3,3,3,3,3,3,3,3,3,3,3,3,3,3,3,
3,3,3,4),(19.9661761554973,20.0656647147026,20.165010707087,20.2642422239616,
20.3634112611229,20.4625485789532,20.5616848984301,20.6609195515273,20.760201924141,
20.8596630799886,20.9520604344998,21.0517562140533,21.1513090368406,21.2511176069915,
21.3504913345749,21.4498322512187,21.5491708007745,21.6493225000927,21.7488054777122,
21.8492915378798,21.9497775980474,22.0494733772045,22.1490261995813,22.248834769833,
22.3482084969741,22.4475494131644,22.5468879622562,22.6470396620909,22.7465226392252,
22.8470087004101,22.947494761595,23.0471905416208,23.1467433648807,23.2465519349134,
23.3459256629671,23.445266580079,23.5446051301003,23.6447568288609,23.7442398069341,
23.8447258660384,23.9452119251426,24.0449077047904,24.1444605276681,24.2442690977958,
24.3436428254591,24.4429837421786,24.5423222918056,24.6424739910267,24.7419569687061,
24.8424430286982,24.9429290886902,25.0426248683205,25.1421776911792,25.2419862613116,
25.3413599889527,25.4407009056489,25.5400394552514,25.640191154498,25.7396741321502,
25.8401601921941,25.9406462522379,26.0607488610849,26.1793890881263,26.2493612672369),
 .UNSPECIFIED.);
#488=B_SPLINE_CURVE_WITH_KNOTS('',3,(#33763,#33764,#33765,#33766,#33767,
#33768,#33769,#33770,#33771,#33772),.UNSPECIFIED.,.F.,.F.,(4,1,1,1,1,1,
1,4),(26.249361462325,26.9383634157855,27.9360805793331,28.9337977428807,
29.9315149064283,30.9292320699759,31.9269492335235,32.5325467695046),
 .UNSPECIFIED.);
#489=B_SPLINE_CURVE_WITH_KNOTS('',3,(#33774,#33775,#33776,#33777,#33778,
#33779,#33780,#33781,#33782,#33783,#33784,#33785,#33786,#33787,#33788,#33789,
#33790,#33791,#33792,#33793,#33794,#33795,#33796,#33797,#33798,#33799,#33800,
#33801,#33802,#33803,#33804,#33805,#33806,#33807,#33808,#33809,#33810,#33811,
#33812,#33813,#33814,#33815,#33816,#33817,#33818,#33819,#33820,#33821,#33822,
#33823,#33824,#33825,#33826,#33827,#33828,#33829,#33830,#33831,#33832,#33833,
#33834,#33835,#33836,#33837,#33838,#33839,#33840,#33841,#33842,#33843,#33844,
#33845,#33846,#33847,#33848,#33849,#33850,#33851,#33852,#33853,#33854,#33855,
#33856,#33857,#33858,#33859,#33860,#33861,#33862,#33863,#33864,#33865,#33866,
#33867,#33868,#33869,#33870,#33871,#33872,#33873,#33874,#33875,#33876,#33877,
#33878,#33879,#33880,#33881,#33882,#33883,#33884,#33885,#33886,#33887,#33888,
#33889,#33890,#33891,#33892,#33893,#33894,#33895,#33896,#33897,#33898,#33899,
#33900,#33901,#33902,#33903,#33904,#33905,#33906,#33907,#33908,#33909,#33910,
#33911,#33912,#33913,#33914,#33915,#33916,#33917,#33918,#33919,#33920,#33921,
#33922,#33923,#33924,#33925,#33926,#33927,#33928,#33929,#33930,#33931,#33932,
#33933,#33934,#33935,#33936,#33937,#33938,#33939,#33940,#33941,#33942,#33943,
#33944,#33945,#33946,#33947,#33948,#33949,#33950,#33951,#33952,#33953,#33954,
#33955,#33956,#33957,#33958,#33959,#33960,#33961,#33962,#33963,#33964,#33965,
#33966),.UNSPECIFIED.,.F.,.F.,(4,3,3,3,3,3,3,3,3,3,3,3,3,3,3,3,3,3,3,3,
3,3,3,3,3,3,3,3,3,3,3,3,3,3,3,3,3,3,3,3,3,3,3,3,3,3,3,3,3,3,3,3,3,3,3,3,
3,3,3,3,3,3,3,3,4),(32.5325469962121,32.6429236413342,32.7537139011972,
32.8650586993773,32.9246663970711,33.0243621767635,33.1239149996856,33.2237235698022,
33.3230972975093,33.4224382142723,33.5217767639425,33.6219284631115,33.7214114408325,
33.8218975007256,33.9223835606187,34.0220793403112,34.1216321632334,34.22144073335,
34.3208144610572,34.4201553778202,34.5194939274904,34.6196456266594,34.7191286043804,
34.8196146642734,34.9201007241663,35.019796503859,35.1193493267814,35.2191578968979,
35.3185316246053,35.4178725413685,35.517211091039,35.6173627902077,35.716845767929,
35.8173318278214,35.9178178877139,36.0175136674065,36.1170664903288,36.2168750604454,
36.3162487881527,36.4155897049157,36.514928254586,36.6150799537549,36.714562931476,
36.8150489913688,36.9155350512616,37.0152308309542,37.1147836538765,37.2145922239931,
37.3139659517004,37.4133068684635,37.5126454181339,37.6127971173027,37.7122800950239,
37.8127661549165,37.9132522148092,38.0117371315798,38.1122364996896,38.2104651268854,
38.3086346576359,38.4067769601568,38.509015739232,38.6072534265365,38.7055475932706,
38.8039800274578,38.8157320764579),.UNSPECIFIED.);
#490=B_SPLINE_CURVE_WITH_KNOTS('',3,(#33968,#33969,#33970,#33971,#33972,
#33973,#33974,#33975,#33976,#33977,#33978,#33979,#33980,#33981,#33982,#33983,
#33984,#33985,#33986,#33987,#33988,#33989,#33990,#33991,#33992,#33993,#33994,
#33995,#33996,#33997,#33998,#33999,#34000,#34001,#34002,#34003,#34004,#34005,
#34006,#34007,#34008,#34009,#34010,#34011,#34012,#34013,#34014,#34015,#34016,
#34017,#34018,#34019,#34020,#34021,#34022,#34023,#34024,#34025,#34026,#34027,
#34028,#34029,#34030,#34031,#34032,#34033,#34034,#34035,#34036,#34037,#34038,
#34039,#34040,#34041,#34042,#34043,#34044,#34045,#34046,#34047,#34048,#34049,
#34050,#34051,#34052,#34053,#34054,#34055,#34056,#34057,#34058,#34059,#34060,
#34061,#34062,#34063,#34064,#34065,#34066,#34067,#34068,#34069,#34070,#34071,
#34072,#34073,#34074,#34075,#34076,#34077,#34078,#34079,#34080,#34081,#34082,
#34083,#34084,#34085,#34086,#34087,#34088,#34089,#34090,#34091,#34092,#34093,
#34094,#34095,#34096,#34097,#34098,#34099,#34100,#34101,#34102,#34103,#34104,
#34105,#34106,#34107,#34108,#34109,#34110,#34111,#34112,#34113,#34114,#34115,
#34116,#34117,#34118,#34119,#34120,#34121,#34122,#34123,#34124,#34125,#34126,
#34127,#34128,#34129,#34130,#34131,#34132,#34133,#34134,#34135,#34136,#34137,
#34138,#34139,#34140,#34141,#34142,#34143,#34144,#34145,#34146,#34147,#34148,
#34149,#34150,#34151,#34152,#34153,#34154,#34155,#34156,#34157),
 .UNSPECIFIED.,.F.,.F.,(4,3,3,3,3,3,3,3,3,3,3,3,3,3,3,3,3,3,3,3,3,3,3,3,
3,3,3,3,3,3,3,3,3,3,3,3,3,3,3,3,3,3,3,3,3,3,3,3,3,3,3,3,3,3,3,3,3,3,3,3,
3,3,3,4),(38.8157320766842,38.9109693783568,39.0106651580491,39.1102179809711,
39.2100265510878,39.3094002787948,39.4087411955576,39.5080797452276,39.6082314443968,
39.7077144221177,39.808200482011,39.9086865419044,40.0083823215971,40.1079351445195,
40.2077437146361,40.3071174423435,40.4064583591067,40.5057969087771,40.6059486079458,
40.7054315856671,40.8059176455595,40.906403705452,41.0060994851446,41.1056523080669,
41.2054608781835,41.3048346058908,41.4041755226539,41.5035140723242,41.6036657714931,
41.7031487492143,41.8036348091069,41.9041208689996,42.0038166486922,42.1033694716144,
42.203178041731,42.3025517694383,42.4018926862013,42.5012312358716,42.6013829350405,
42.7008659127616,42.8013519726544,42.9018380325472,43.0015338122398,43.1010866351621,
43.2008952052787,43.300268932986,43.3996098497491,43.4989483994195,43.5991000985883,
43.6985830763095,43.7990691362021,43.8995551960948,43.9992509757874,44.0988037987097,
44.1986123688262,44.2979860965335,44.3973270132966,44.4966655629669,44.5968172621358,
44.6963002398569,44.7967862997496,44.8972723596424,45.0393109849315,45.0989173838638),
 .UNSPECIFIED.);
#491=B_SPLINE_CURVE_WITH_KNOTS('',3,(#34159,#34160,#34161,#34162,#34163,
#34164,#34165,#34166,#34167,#34168),.UNSPECIFIED.,.F.,.F.,(4,1,1,1,1,1,
1,4),(45.0989204148471,45.89498952319,46.8927066867377,47.8904238502853,
48.8881410138329,49.8858581773805,50.8835753409281,51.3821026672746),
 .UNSPECIFIED.);
#492=B_SPLINE_CURVE_WITH_KNOTS('',3,(#34170,#34171,#34172,#34173,#34174,
#34175,#34176,#34177,#34178,#34179,#34180,#34181,#34182,#34183,#34184,#34185,
#34186,#34187,#34188,#34189,#34190,#34191,#34192,#34193,#34194,#34195,#34196,
#34197,#34198,#34199,#34200,#34201,#34202,#34203,#34204,#34205,#34206,#34207,
#34208,#34209,#34210,#34211,#34212,#34213,#34214,#34215,#34216,#34217,#34218,
#34219,#34220,#34221,#34222,#34223,#34224,#34225,#34226,#34227,#34228,#34229,
#34230,#34231,#34232,#34233,#34234,#34235,#34236,#34237,#34238,#34239,#34240,
#34241,#34242,#34243,#34244,#34245,#34246,#34247,#34248,#34249,#34250,#34251,
#34252,#34253,#34254,#34255,#34256,#34257,#34258,#34259,#34260,#34261,#34262,
#34263,#34264,#34265,#34266,#34267,#34268,#34269,#34270,#34271,#34272,#34273,
#34274,#34275,#34276,#34277,#34278,#34279,#34280,#34281,#34282,#34283,#34284,
#34285,#34286,#34287,#34288,#34289,#34290,#34291,#34292,#34293,#34294,#34295,
#34296,#34297,#34298,#34299,#34300,#34301,#34302,#34303,#34304,#34305,#34306,
#34307,#34308,#34309,#34310,#34311,#34312,#34313,#34314,#34315,#34316,#34317,
#34318,#34319,#34320,#34321,#34322,#34323,#34324,#34325,#34326,#34327,#34328,
#34329,#34330,#34331,#34332,#34333,#34334,#34335,#34336,#34337,#34338,#34339,
#34340,#34341,#34342,#34343,#34344,#34345,#34346,#34347,#34348,#34349,#34350,
#34351,#34352,#34353,#34354,#34355,#34356,#34357,#34358,#34359),
 .UNSPECIFIED.,.F.,.F.,(4,3,3,3,3,3,3,3,3,3,3,3,3,3,3,3,3,3,3,3,3,3,3,3,
3,3,3,3,3,3,3,3,3,3,3,3,3,3,3,3,3,3,3,3,3,3,3,3,3,3,3,3,3,3,3,3,3,3,3,3,
3,3,3,4),(51.3821026910434,51.4861327815925,51.5904454853881,51.6949031312876,
51.7996461633303,51.8812925044757,51.9809882841683,52.0805411070906,52.1803496772072,
52.2797234049145,52.3790643216776,52.4784028713478,52.5785545705166,52.6780375482378,
52.7785236081306,52.8790096680233,52.9787054477158,53.0782582706381,53.1780668407547,
53.2774405684621,53.3767814852251,53.4761200348954,53.5762717340643,53.6757547117854,
53.7762407716782,53.8767268315709,53.9764226112636,54.075975434186,54.1757840043025,
54.2751577320098,54.3744986487728,54.4738371984431,54.573988897612,54.6734718753331,
54.7739579352258,54.8744439951185,54.9741397748111,55.0736925977335,55.1735011678501,
55.2728748955575,55.3722158123206,55.4715543619908,55.5717060611596,55.6711890388808,
55.7716750987734,55.8721611586661,55.9718569383586,56.0714097612811,56.1712183313977,
56.270592059105,56.369932975868,56.4692715255384,56.5694232247072,56.6689062024283,
56.7693922623211,56.8698783222138,56.9693045316758,57.067409750273,57.1654215585788,
57.2633721047655,57.3638510780515,57.4618119537227,57.5635499758161,57.6652879979096),
 .UNSPECIFIED.);
#493=B_SPLINE_CURVE_WITH_KNOTS('',3,(#34361,#34362,#34363,#34364,#34365,
#34366,#34367,#34368,#34369,#34370,#34371,#34372,#34373,#34374,#34375,#34376,
#34377,#34378,#34379,#34380,#34381,#34382,#34383,#34384,#34385,#34386,#34387,
#34388,#34389,#34390,#34391,#34392,#34393,#34394,#34395,#34396,#34397,#34398,
#34399,#34400,#34401,#34402,#34403,#34404,#34405,#34406,#34407,#34408,#34409,
#34410,#34411,#34412,#34413,#34414,#34415,#34416,#34417,#34418,#34419,#34420,
#34421,#34422,#34423,#34424,#34425,#34426,#34427,#34428,#34429,#34430,#34431,
#34432,#34433,#34434,#34435,#34436,#34437,#34438,#34439,#34440,#34441,#34442,
#34443,#34444,#34445,#34446,#34447,#34448,#34449,#34450,#34451,#34452,#34453,
#34454,#34455,#34456,#34457,#34458,#34459,#34460,#34461,#34462,#34463,#34464,
#34465,#34466,#34467,#34468,#34469,#34470,#34471,#34472,#34473,#34474,#34475,
#34476,#34477,#34478,#34479,#34480,#34481,#34482,#34483,#34484,#34485,#34486,
#34487,#34488,#34489,#34490,#34491,#34492,#34493,#34494,#34495,#34496,#34497,
#34498,#34499,#34500,#34501,#34502,#34503,#34504,#34505,#34506,#34507,#34508,
#34509,#34510,#34511,#34512,#34513,#34514,#34515,#34516,#34517,#34518,#34519,
#34520,#34521,#34522,#34523,#34524,#34525,#34526,#34527,#34528,#34529,#34530,
#34531,#34532,#34533,#34534,#34535,#34536,#34537,#34538,#34539,#34540,#34541,
#34542,#34543,#34544,#34545,#34546,#34547,#34548,#34549,#34550),
 .UNSPECIFIED.,.F.,.F.,(4,3,3,3,3,3,3,3,3,3,3,3,3,3,3,3,3,3,3,3,3,3,3,3,
3,3,3,3,3,3,3,3,3,3,3,3,3,3,3,3,3,3,3,3,3,3,3,3,3,3,3,3,3,3,3,3,3,3,3,3,
3,3,3,4),(57.665287998223,57.8070952114157,57.8675954857614,57.967291265454,
58.0668440883763,58.1666526584929,58.2660263862001,58.3653673029632,58.4647058526337,
58.5648575518025,58.6643405295236,58.7648265894163,58.865312649309,58.9650084290015,
59.0645612519237,59.1643698220403,59.2637435497476,59.3630844665106,59.4624230161809,
59.5625747153498,59.6620576930709,59.7625437529638,59.8630298128566,59.9627255925492,
60.0622784154715,60.162086985588,60.2614607132954,60.3608016300585,60.4601401797288,
60.5602918788976,60.6597748566188,60.7602609165115,60.8607469764042,60.9604427560968,
61.0599955790191,61.1598041491357,61.259177876843,61.3585187936061,61.4578573432764,
61.5580090424452,61.6574920201664,61.7579780800591,61.8584641399518,61.9581599196445,
62.0577127425668,62.1575213126834,62.2568950403907,62.3562359571538,62.4555745068242,
62.555726205993,62.6552091837141,62.7556952436068,62.8561813034994,62.955877083192,
63.0554299061143,63.1552384762309,63.2546122039382,63.3539531207012,63.4532916703714,
63.5534433695403,63.6529263472615,63.7534124071542,63.853898467047,63.9484733054025),
 .UNSPECIFIED.);
#494=B_SPLINE_CURVE_WITH_KNOTS('',3,(#34552,#34553,#34554,#34555,#34556,
#34557,#34558,#34559,#34560,#34561,#34562,#34563,#34564,#34565,#34566,#34567,
#34568,#34569,#34570,#34571,#34572,#34573,#34574,#34575,#34576,#34577,#34578,
#34579,#34580,#34581,#34582,#34583,#34584,#34585,#34586,#34587,#34588,#34589,
#34590,#34591,#34592,#34593,#34594,#34595,#34596,#34597,#34598,#34599,#34600,
#34601,#34602,#34603,#34604,#34605,#34606,#34607,#34608,#34609,#34610,#34611,
#34612,#34613,#34614,#34615,#34616,#34617,#34618,#34619,#34620,#34621,#34622,
#34623,#34624,#34625,#34626,#34627,#34628,#34629,#34630,#34631,#34632,#34633,
#34634,#34635,#34636,#34637,#34638,#34639,#34640,#34641,#34642,#34643,#34644,
#34645,#34646,#34647,#34648,#34649,#34650,#34651,#34652,#34653,#34654,#34655,
#34656,#34657,#34658,#34659,#34660,#34661,#34662,#34663,#34664,#34665,#34666,
#34667,#34668,#34669,#34670,#34671,#34672,#34673,#34674,#34675,#34676,#34677,
#34678,#34679,#34680,#34681,#34682,#34683,#34684,#34685,#34686,#34687,#34688,
#34689,#34690,#34691,#34692,#34693,#34694,#34695,#34696,#34697,#34698,#34699,
#34700,#34701,#34702,#34703,#34704,#34705,#34706,#34707,#34708,#34709,#34710,
#34711,#34712,#34713,#34714,#34715,#34716,#34717,#34718,#34719,#34720,#34721,
#34722,#34723,#34724,#34725,#34726,#34727,#34728,#34729,#34730,#34731,#34732,
#34733,#34734,#34735,#34736,#34737,#34738,#34739,#34740,#34741,#34742,#34743,
#34744),.UNSPECIFIED.,.F.,.F.,(4,3,3,3,3,3,3,3,3,3,3,3,3,3,3,3,3,3,3,3,
3,3,3,3,3,3,3,3,3,3,3,3,3,3,3,3,3,3,3,3,3,3,3,3,3,3,3,3,3,3,3,3,3,3,3,3,
3,3,3,3,3,3,3,3,4),(63.9484733056258,64.0469101210583,64.1474983097503,
64.2457098131483,64.3438737786661,64.4420220526341,64.5444204471243,64.6426930224998,
64.7410320253817,64.8395232369876,64.8516156305946,64.9513114102871,65.0508642332093,
65.1506728033259,65.2500465310332,65.3493874477962,65.4487259974665,65.5488776966354,
65.6483606743565,65.7488467342494,65.8493327941422,65.9490285738348,66.0485813967571,
66.1483899668737,66.247763694581,66.347104611344,66.4464431610144,66.5465948601833,
66.6460778379043,66.746563897797,66.8470499576898,66.9467457373824,67.0462985603045,
67.1461071304212,67.2454808581284,67.3448217748916,67.4441603245621,67.5443120237309,
67.6437950014522,67.7442810613448,67.8447671212375,67.9444629009302,68.0440157238524,
68.143824293969,68.2431980216763,68.3425389384395,68.4418774881096,68.5420291872785,
68.6415121649996,68.7419982248924,68.8424842847851,68.9421800644777,69.0417328874002,
69.1415414575167,69.240915185224,69.3402561019872,69.4395946516573,69.5397463508262,
69.6392293285473,69.73971538844,69.8402014483327,69.9515510975534,70.062533144783,
70.1728865793843,70.2316583852461),.UNSPECIFIED.);
#495=B_SPLINE_CURVE_WITH_KNOTS('',3,(#34746,#34747,#34748,#34749,#34750,
#34751,#34752,#34753,#34754,#34755),.UNSPECIFIED.,.F.,.F.,(4,1,1,1,1,1,
1,4),(70.2316586125821,70.8379186118803,71.8356357754279,72.8333529389755,
73.8310701025231,74.8287872660707,75.8265044296183,76.5148439197617),
 .UNSPECIFIED.);
#496=B_SPLINE_CURVE_WITH_KNOTS('',3,(#34757,#34758,#34759,#34760,#34761,
#34762,#34763,#34764,#34765,#34766,#34767,#34768,#34769,#34770,#34771,#34772,
#34773,#34774,#34775,#34776,#34777,#34778,#34779,#34780,#34781,#34782,#34783,
#34784,#34785,#34786,#34787,#34788,#34789,#34790,#34791,#34792,#34793,#34794,
#34795,#34796,#34797,#34798,#34799,#34800,#34801,#34802,#34803,#34804,#34805,
#34806,#34807,#34808,#34809,#34810,#34811,#34812,#34813,#34814,#34815,#34816,
#34817,#34818,#34819,#34820,#34821,#34822,#34823,#34824,#34825,#34826,#34827,
#34828,#34829,#34830,#34831,#34832,#34833,#34834,#34835,#34836,#34837,#34838,
#34839,#34840,#34841,#34842,#34843,#34844,#34845,#34846,#34847,#34848,#34849,
#34850,#34851,#34852,#34853,#34854,#34855,#34856,#34857,#34858,#34859,#34860,
#34861,#34862,#34863,#34864,#34865,#34866,#34867,#34868,#34869,#34870,#34871,
#34872,#34873,#34874,#34875,#34876,#34877,#34878,#34879,#34880,#34881,#34882,
#34883,#34884,#34885,#34886,#34887,#34888,#34889,#34890,#34891,#34892,#34893,
#34894,#34895,#34896,#34897,#34898,#34899,#34900,#34901,#34902,#34903,#34904,
#34905,#34906,#34907,#34908,#34909,#34910,#34911,#34912,#34913,#34914,#34915,
#34916,#34917,#34918,#34919,#34920,#34921,#34922,#34923,#34924,#34925,#34926,
#34927,#34928,#34929,#34930,#34931,#34932,#34933,#34934,#34935,#34936,#34937,
#34938,#34939,#34940,#34941,#34942,#34943,#34944,#34945,#34946),
 .UNSPECIFIED.,.F.,.F.,(4,3,3,3,3,3,3,3,3,3,3,3,3,3,3,3,3,3,3,3,3,3,3,3,
3,3,3,3,3,3,3,3,3,3,3,3,3,3,3,3,3,3,3,3,3,3,3,3,3,3,3,3,3,3,3,3,3,3,3,3,
3,3,3,4),(76.5148441159767,76.6331916616517,76.7530359215634,76.824221593166,
76.9239173728584,77.0234701957806,77.1232787658972,77.2226524936043,77.3219934103671,
77.4213319600372,77.5214836592063,77.6209666369272,77.7214526968204,77.8219387567136,
77.9216345364062,78.0211873593286,78.1209959294452,78.2203696571526,78.3197105739157,
78.4190491235861,78.5192008227549,78.6186838004761,78.7191698603686,78.8196559202612,
78.9193516999539,79.0189045228762,79.1187130929927,79.2180868207001,79.3174277374632,
79.4167662871335,79.5169179863023,79.6164009640235,79.7168870239162,79.8173730838088,
79.9170688635014,80.0166216864236,80.1164302565402,80.2158039842475,80.3151449010106,
80.4144834506808,80.5146351498497,80.6141181275708,80.7146041874636,80.8150902473564,
80.914786027049,81.0143388499712,81.1141474200878,81.2135211477951,81.3128620645582,
81.4122006142286,81.5123523133974,81.6118352911185,81.7123213510113,81.812807410904,
81.9122859939485,82.0116217850278,82.1108427790342,82.2100011139379,82.3091275647997,
82.4082528670978,82.5074761530274,82.6067470602028,82.7061961999099,82.7980292265394),
 .UNSPECIFIED.);
#497=B_SPLINE_CURVE_WITH_KNOTS('',3,(#34948,#34949,#34950,#34951,#34952,
#34953,#34954,#34955,#34956,#34957,#34958,#34959,#34960,#34961,#34962,#34963,
#34964,#34965,#34966,#34967,#34968,#34969,#34970,#34971,#34972,#34973,#34974,
#34975,#34976,#34977,#34978,#34979,#34980,#34981,#34982,#34983,#34984,#34985,
#34986,#34987,#34988,#34989,#34990,#34991,#34992,#34993,#34994,#34995,#34996,
#34997,#34998,#34999,#35000,#35001,#35002,#35003,#35004,#35005,#35006,#35007,
#35008,#35009,#35010,#35011,#35012,#35013,#35014,#35015,#35016,#35017,#35018,
#35019,#35020,#35021,#35022,#35023,#35024,#35025,#35026,#35027,#35028,#35029,
#35030,#35031,#35032,#35033,#35034,#35035,#35036,#35037,#35038,#35039,#35040,
#35041,#35042,#35043,#35044,#35045,#35046,#35047,#35048,#35049,#35050,#35051,
#35052,#35053,#35054,#35055,#35056,#35057,#35058,#35059,#35060,#35061,#35062,
#35063,#35064,#35065,#35066,#35067,#35068,#35069,#35070,#35071,#35072,#35073,
#35074,#35075,#35076,#35077,#35078,#35079,#35080,#35081,#35082,#35083,#35084,
#35085,#35086,#35087,#35088,#35089,#35090,#35091,#35092,#35093,#35094,#35095,
#35096,#35097,#35098,#35099,#35100,#35101,#35102,#35103,#35104,#35105,#35106,
#35107,#35108,#35109,#35110,#35111,#35112,#35113,#35114,#35115,#35116,#35117,
#35118,#35119,#35120,#35121,#35122,#35123,#35124,#35125,#35126,#35127,#35128,
#35129,#35130,#35131,#35132,#35133,#35134,#35135,#35136,#35137,#35138,#35139,
#35140),.UNSPECIFIED.,.F.,.F.,(4,3,3,3,3,3,3,3,3,3,3,3,3,3,3,3,3,3,3,3,
3,3,3,3,3,3,3,3,3,3,3,3,3,3,3,3,3,3,3,3,3,3,3,3,3,3,3,3,3,3,3,3,3,3,3,3,
3,3,3,3,3,3,3,3,4),(82.7980292269413,82.8105245744516,82.9102203541442,
83.0097731770666,83.1095817471832,83.2089554748905,83.3082963916536,83.407634941324,
83.5077866404928,83.6072696182139,83.7077556781066,83.8082417379992,83.9079375176917,
84.007490340614,84.1072989107306,84.2066726384379,84.3060135552009,84.4053521048711,
84.50550380404,84.6049867817612,84.705472841654,84.8059589015468,84.9056546812395,
85.0052075041618,85.1050160742784,85.2043898019857,85.3037307187489,85.4030692684192,
85.5032209675881,85.6027039453093,85.7031900052019,85.8036760650945,85.9033718447871,
86.0029246677094,86.102733237826,86.2021069655333,86.3014478822963,86.4007864319666,
86.5009381311355,86.6004211088566,86.7009071687494,86.8013932286421,86.9010890083347,
87.000641831257,87.1004504013736,87.1998241290809,87.299165045844,87.3985035955144,
87.4986552946832,87.5981382724043,87.698624332297,87.7991103921897,87.8988061718823,
87.9983589948046,88.0981675649212,88.1975412926285,88.2968822093916,88.3962207590619,
88.4963724582308,88.5958554359519,88.6963414958446,88.7968275557373,88.9205993160034,
89.0424478486719,89.0812145338453),.UNSPECIFIED.);
#498=B_SPLINE_CURVE_WITH_KNOTS('',3,(#35142,#35143,#35144,#35145,#35146,
#35147,#35148,#35149,#35150,#35151,#35152,#35153,#35154,#35155,#35156,#35157,
#35158,#35159,#35160,#35161,#35162,#35163,#35164,#35165,#35166,#35167,#35168,
#35169,#35170,#35171,#35172,#35173,#35174,#35175,#35176,#35177,#35178,#35179,
#35180,#35181,#35182,#35183,#35184,#35185,#35186,#35187,#35188,#35189,#35190,
#35191,#35192,#35193,#35194,#35195,#35196,#35197,#35198,#35199,#35200,#35201,
#35202,#35203,#35204,#35205,#35206,#35207,#35208,#35209,#35210,#35211,#35212,
#35213,#35214,#35215,#35216,#35217,#35218,#35219,#35220,#35221,#35222,#35223,
#35224,#35225,#35226,#35227,#35228,#35229,#35230,#35231,#35232,#35233,#35234,
#35235,#35236,#35237,#35238,#35239,#35240,#35241,#35242,#35243,#35244,#35245,
#35246,#35247,#35248,#35249,#35250,#35251,#35252,#35253,#35254,#35255,#35256,
#35257,#35258,#35259,#35260,#35261,#35262,#35263,#35264,#35265,#35266,#35267,
#35268,#35269,#35270,#35271,#35272,#35273,#35274,#35275,#35276,#35277,#35278,
#35279,#35280,#35281,#35282,#35283,#35284,#35285,#35286,#35287,#35288,#35289,
#35290,#35291,#35292,#35293,#35294,#35295,#35296,#35297,#35298,#35299,#35300,
#35301,#35302,#35303,#35304,#35305,#35306,#35307,#35308,#35309,#35310,#35311,
#35312,#35313,#35314,#35315,#35316,#35317,#35318,#35319,#35320,#35321,#35322,
#35323,#35324,#35325,#35326,#35327,#35328,#35329,#35330,#35331,#35332,#35333,
#35334),.UNSPECIFIED.,.F.,.F.,(4,3,3,3,3,3,3,3,3,3,3,3,3,3,3,3,3,3,3,3,
3,3,3,3,3,3,3,3,3,3,3,3,3,3,3,3,3,3,3,3,3,3,3,3,3,3,3,3,3,3,3,3,3,3,3,3,
3,3,3,3,3,3,3,3,4),(89.0812145341209,89.1798277015848,89.2783970373168,
89.3769539358606,89.4755297704361,89.5742162318756,89.6729694918042,89.7718816291792,
89.7945447192849,89.8942404989775,89.9937933218998,90.0936018920164,90.1929756197236,
90.2923165364868,90.3916550861572,90.491806785326,90.5912897630471,90.6917758229398,
90.7922618828325,90.8919576625251,90.9915104854473,91.0913190555639,91.1906927832712,
91.2900337000343,91.3893722497046,91.4895239488735,91.5890069265947,91.6894929864874,
91.7899790463801,91.8896748260726,91.9892276489952,92.0890362191118,92.1884099468192,
92.2877508635822,92.3870894132525,92.4872411124213,92.5867240901425,92.6872101500351,
92.7876962099277,92.8873919896202,92.9869448125427,93.0867533826593,93.1861271103666,
93.2854680271297,93.3848065767998,93.4849582759687,93.5844412536898,93.6849273135825,
93.7854133734753,93.8851091531678,93.9846619760905,94.0844705462071,94.1838442739143,
94.2831851906773,94.3825237403476,94.4826754395165,94.5821584172377,94.6826444771303,
94.7831305370229,94.8847948887262,94.9862963274486,95.0876311352717,95.1888678692207,
95.2900278217262,95.3643998413005),.UNSPECIFIED.);
#499=B_SPLINE_CURVE_WITH_KNOTS('',3,(#35336,#35337,#35338,#35339,#35340,
#35341,#35342,#35343,#35344,#35345,#35346,#35347,#35348,#35349,#35350,#35351,
#35352,#35353,#35354,#35355,#35356,#35357,#35358,#35359,#35360,#35361,#35362,
#35363,#35364,#35365,#35366,#35367,#35368,#35369,#35370,#35371,#35372,#35373,
#35374,#35375,#35376,#35377,#35378,#35379,#35380,#35381,#35382,#35383,#35384,
#35385,#35386,#35387,#35388,#35389,#35390,#35391,#35392,#35393,#35394,#35395,
#35396,#35397,#35398,#35399,#35400,#35401,#35402,#35403,#35404,#35405,#35406,
#35407,#35408,#35409,#35410,#35411,#35412,#35413,#35414,#35415,#35416,#35417,
#35418,#35419,#35420,#35421,#35422,#35423,#35424,#35425,#35426,#35427,#35428,
#35429,#35430,#35431,#35432,#35433,#35434,#35435,#35436,#35437,#35438,#35439,
#35440,#35441,#35442,#35443,#35444,#35445,#35446,#35447,#35448,#35449,#35450,
#35451,#35452,#35453,#35454,#35455,#35456,#35457,#35458,#35459,#35460,#35461,
#35462,#35463,#35464,#35465,#35466,#35467,#35468,#35469,#35470,#35471,#35472,
#35473,#35474,#35475,#35476,#35477,#35478,#35479,#35480,#35481,#35482,#35483,
#35484,#35485,#35486,#35487,#35488,#35489,#35490,#35491,#35492,#35493,#35494,
#35495,#35496,#35497,#35498,#35499,#35500,#35501,#35502,#35503,#35504,#35505,
#35506,#35507,#35508,#35509,#35510,#35511,#35512,#35513,#35514,#35515,#35516,
#35517,#35518,#35519,#35520,#35521,#35522,#35523,#35524,#35525),
 .UNSPECIFIED.,.F.,.F.,(4,3,3,3,3,3,3,3,3,3,3,3,3,3,3,3,3,3,3,3,3,3,3,3,
3,3,3,3,3,3,3,3,3,3,3,3,3,3,3,3,3,3,3,3,3,3,3,3,3,3,3,3,3,3,3,3,3,3,3,3,
3,3,3,4),(95.3643998416745,95.4730572664134,95.5820351393695,95.6915015544521,
95.7808477005705,95.880543480263,95.9800963031853,96.0799048733019,96.1792786010091,
96.2786195177721,96.3779580674424,96.4781097666113,96.5775927443324,96.6780788042252,
96.7785648641181,96.8782606438108,96.9778134667331,97.0776220368497,97.1769957645571,
97.2763366813202,97.3756752309906,97.4758269301594,97.5753099078806,97.6757959677732,
97.7762820276658,97.8759778073584,97.9755306302807,98.0753392003973,98.1747129281046,
98.2740538448677,98.373392394538,98.4735440937068,98.573027071428,98.6735131313206,
98.7739991912133,98.8736949709058,98.9732477938281,99.0730563639447,99.1724300916519,
99.2717710084149,99.3711095580852,99.4712612572542,99.5707442349753,99.6712302948681,
99.771716354761,99.8714121344538,99.9709649573763,100.070773527493,100.1701472552,
100.269488171964,100.368826721634,100.468978420803,100.568461398524,100.668947458417,
100.769433518309,100.867766132118,100.965935563168,101.064013280475,101.162031368816,
101.260021836025,101.358073520992,101.456152065062,101.554380441358,101.64758514848),
 .UNSPECIFIED.);
#500=B_SPLINE_CURVE_WITH_KNOTS('',3,(#35527,#35528,#35529,#35530,#35531,
#35532,#35533,#35534,#35535,#35536,#35537),.UNSPECIFIED.,.F.,.F.,(4,1,1,
1,1,1,1,1,4),(101.64758514848,101.767150681856,102.764867845404,103.762585008951,
104.760302172499,105.758019336047,106.755736499594,107.753453663142,107.93077045566),
 .UNSPECIFIED.);
#501=B_SPLINE_CURVE_WITH_KNOTS('',3,(#35539,#35540,#35541,#35542,#35543,
#35544,#35545,#35546,#35547,#35548,#35549,#35550,#35551,#35552,#35553,#35554,
#35555,#35556,#35557,#35558,#35559,#35560,#35561,#35562,#35563,#35564,#35565,
#35566,#35567,#35568,#35569,#35570,#35571,#35572,#35573,#35574,#35575,#35576,
#35577,#35578,#35579,#35580,#35581,#35582,#35583,#35584,#35585,#35586,#35587,
#35588,#35589,#35590,#35591,#35592,#35593,#35594,#35595,#35596,#35597,#35598,
#35599,#35600,#35601,#35602,#35603,#35604,#35605,#35606,#35607,#35608,#35609,
#35610,#35611,#35612,#35613,#35614,#35615,#35616,#35617,#35618,#35619,#35620,
#35621,#35622,#35623,#35624,#35625,#35626,#35627,#35628,#35629,#35630,#35631,
#35632,#35633,#35634,#35635,#35636,#35637,#35638,#35639,#35640,#35641,#35642,
#35643,#35644,#35645,#35646,#35647,#35648,#35649,#35650,#35651,#35652,#35653,
#35654,#35655,#35656,#35657,#35658,#35659,#35660,#35661,#35662,#35663,#35664,
#35665,#35666,#35667,#35668,#35669,#35670,#35671,#35672,#35673,#35674,#35675,
#35676,#35677,#35678,#35679,#35680,#35681,#35682,#35683,#35684,#35685,#35686,
#35687,#35688,#35689,#35690,#35691,#35692,#35693,#35694,#35695,#35696,#35697,
#35698,#35699,#35700,#35701,#35702,#35703,#35704,#35705,#35706,#35707,#35708,
#35709,#35710,#35711,#35712,#35713,#35714,#35715,#35716,#35717,#35718,#35719,
#35720,#35721,#35722,#35723,#35724,#35725,#35726,#35727,#35728,#35729,#35730,
#35731),.UNSPECIFIED.,.F.,.F.,(4,3,3,3,3,3,3,3,3,3,3,3,3,3,3,3,3,3,3,3,
3,3,3,3,3,3,3,3,3,3,3,3,3,3,3,3,3,3,3,3,3,3,3,3,3,3,3,3,3,3,3,3,3,3,3,3,
3,3,3,3,3,3,3,3,4),(107.93077045566,108.033320502039,108.131274959939,108.229174356975,
108.327050797025,108.424936350185,108.522922660142,108.620968324305,108.719170328587,
108.751170826689,108.850866606382,108.950419429304,109.050227999421,109.149601727128,
109.248942643891,109.348281193561,109.44843289273,109.547915870452,109.648401930344,
109.748887990237,109.84858376993,109.948136592852,110.047945162969,110.147318890677,
110.24665980744,110.34599835711,110.446150056279,110.545633034001,110.646119093893,
110.746605153785,110.846300933477,110.945853756399,111.045662326516,111.145036054223,
111.244376970986,111.343715520656,111.443867219825,111.543350197546,111.643836257439,
111.744322317332,111.844018097025,111.943570919947,112.043379490064,112.142753217771,
112.242094134534,112.341432684205,112.441584383373,112.541067361094,112.641553420987,
112.74203948088,112.841735260573,112.941288083496,113.041096653612,113.14047038132,
113.239811298083,113.339149847754,113.439301546922,113.538784524644,113.639270584536,
113.739756644428,113.845800654927,113.951510358964,114.057014148429,114.162240196533,
114.213955762579),.UNSPECIFIED.);
#502=B_SPLINE_CURVE_WITH_KNOTS('',3,(#35733,#35734,#35735,#35736,#35737,
#35738,#35739,#35740,#35741,#35742,#35743,#35744,#35745,#35746,#35747,#35748,
#35749,#35750,#35751,#35752,#35753,#35754,#35755,#35756,#35757,#35758,#35759,
#35760,#35761,#35762,#35763,#35764,#35765,#35766,#35767,#35768,#35769,#35770,
#35771,#35772,#35773,#35774,#35775,#35776,#35777,#35778,#35779,#35780,#35781,
#35782,#35783,#35784,#35785,#35786,#35787,#35788,#35789,#35790,#35791,#35792,
#35793,#35794,#35795,#35796,#35797,#35798,#35799,#35800,#35801,#35802,#35803,
#35804,#35805,#35806,#35807,#35808,#35809,#35810,#35811,#35812,#35813,#35814,
#35815,#35816,#35817,#35818,#35819,#35820,#35821,#35822,#35823,#35824,#35825,
#35826,#35827,#35828,#35829,#35830,#35831,#35832,#35833,#35834,#35835,#35836,
#35837,#35838,#35839,#35840,#35841,#35842,#35843,#35844,#35845,#35846,#35847,
#35848,#35849,#35850,#35851,#35852,#35853,#35854,#35855,#35856,#35857,#35858,
#35859,#35860,#35861,#35862,#35863,#35864,#35865,#35866,#35867,#35868,#35869,
#35870,#35871,#35872,#35873,#35874,#35875,#35876,#35877,#35878,#35879,#35880,
#35881,#35882,#35883,#35884,#35885,#35886,#35887,#35888,#35889,#35890,#35891,
#35892,#35893,#35894,#35895,#35896,#35897,#35898,#35899,#35900,#35901,#35902,
#35903,#35904,#35905,#35906,#35907,#35908,#35909,#35910,#35911,#35912,#35913,
#35914,#35915,#35916,#35917,#35918,#35919,#35920,#35921,#35922),
 .UNSPECIFIED.,.F.,.F.,(4,3,3,3,3,3,3,3,3,3,3,3,3,3,3,3,3,3,3,3,3,3,3,3,
3,3,3,3,3,3,3,3,3,3,3,3,3,3,3,3,3,3,3,3,3,3,3,3,3,3,3,3,3,3,3,3,3,3,3,3,
3,3,3,4),(114.213955762839,114.317000725158,114.422118995862,114.525515211232,
114.631494509603,114.737473807975,114.837169587668,114.93672241059,115.036530980707,
115.135904708414,115.235245625178,115.334584174848,115.434735874017,115.534218851738,
115.634704911631,115.735190971523,115.834886751215,115.934439574137,116.034248144254,
116.133621871961,116.232962788724,116.332301338394,116.432453037563,116.531936015284,
116.632422075177,116.73290813507,116.832603914763,116.932156737685,117.031965307801,
117.131339035509,117.230679952272,117.330018501942,117.430170201111,117.529653178832,
117.630139238725,117.730625298618,117.830321078311,117.929873901234,118.02968247135,
118.129056199058,118.228397115822,118.327735665493,118.427887364661,118.527370342383,
118.627856402274,118.728342462166,118.828038241858,118.92759106478,119.027399634897,
119.126773362604,119.226114279367,119.325452829037,119.425604528206,119.525087505926,
119.62557356582,119.726059625713,119.824409942825,119.922632846727,120.020760508367,
120.118824976187,120.216892947049,120.314957356844,120.413115312058,120.497141070019),
 .UNSPECIFIED.);
#503=B_SPLINE_CURVE_WITH_KNOTS('',3,(#35924,#35925,#35926,#35927,#35928,
#35929,#35930,#35931,#35932,#35933,#35934),.UNSPECIFIED.,.F.,.F.,(4,1,1,
1,1,1,1,1,4),(120.497141070019,120.723776789261,121.721493952808,122.719211116356,
123.716928279904,124.714645443451,125.712362606999,126.710079770546,126.780326377198),
 .UNSPECIFIED.);
#504=B_SPLINE_CURVE_WITH_KNOTS('',3,(#35936,#35937,#35938,#35939,#35940,
#35941,#35942,#35943,#35944,#35945,#35946,#35947,#35948,#35949,#35950,#35951,
#35952,#35953,#35954,#35955,#35956,#35957,#35958,#35959,#35960,#35961,#35962,
#35963,#35964,#35965,#35966,#35967,#35968,#35969,#35970,#35971,#35972,#35973,
#35974,#35975,#35976,#35977,#35978,#35979,#35980,#35981,#35982,#35983,#35984,
#35985,#35986,#35987,#35988,#35989,#35990,#35991,#35992,#35993,#35994,#35995,
#35996,#35997,#35998,#35999,#36000,#36001,#36002,#36003,#36004,#36005,#36006,
#36007,#36008,#36009,#36010,#36011,#36012,#36013,#36014,#36015,#36016,#36017,
#36018,#36019,#36020,#36021,#36022,#36023,#36024,#36025,#36026,#36027,#36028,
#36029,#36030,#36031,#36032,#36033,#36034,#36035,#36036,#36037,#36038,#36039,
#36040,#36041,#36042,#36043,#36044,#36045,#36046,#36047,#36048,#36049,#36050,
#36051,#36052,#36053,#36054,#36055,#36056,#36057,#36058,#36059,#36060,#36061,
#36062,#36063,#36064,#36065,#36066,#36067,#36068,#36069,#36070,#36071,#36072,
#36073,#36074,#36075,#36076,#36077,#36078,#36079,#36080,#36081,#36082,#36083,
#36084,#36085,#36086,#36087,#36088,#36089,#36090,#36091,#36092,#36093,#36094,
#36095,#36096,#36097,#36098,#36099,#36100,#36101,#36102,#36103,#36104,#36105,
#36106,#36107,#36108,#36109,#36110,#36111,#36112,#36113,#36114,#36115,#36116,
#36117,#36118,#36119,#36120,#36121,#36122,#36123,#36124,#36125,#36126,#36127,
#36128),.UNSPECIFIED.,.F.,.F.,(4,3,3,3,3,3,3,3,3,3,3,3,3,3,3,3,3,3,3,3,
3,3,3,3,3,3,3,3,3,3,3,3,3,3,3,3,3,3,3,3,3,3,3,3,3,3,3,3,3,3,3,3,3,3,3,3,
3,3,3,3,3,3,3,3,4),(126.780326377198,126.879001192006,126.982600659767,
127.08103492238,127.179417182261,127.277779082583,127.376152236855,127.474629094606,
127.57316636921,127.671863081557,127.707796934094,127.807492713718,127.907045536571,
128.006854106705,128.106227834345,128.20556875104,128.304907300644,128.405058999893,
128.50454197755,128.605028037596,128.705514097642,128.805209877294,128.904762700175,
129.004571270302,129.103944997966,129.203285914686,129.302624464312,129.402776163531,
129.502259141207,129.602745201198,129.703231261189,129.802927041231,129.902479864504,
130.002288434533,130.101662162591,130.201003079704,130.300341629723,130.400493328476,
130.499976306539,130.600462365638,130.700948424737,130.800644203842,130.900197026178,
131.000005596442,131.09937932357,131.198720239757,131.298058788856,131.398210488714,
131.497693465881,131.598179527083,131.698665588285,131.798361367887,131.897914190712,
131.997722760852,132.097096488448,132.196437405094,132.295775954643,132.39592765394,
132.495410631529,132.595896691681,132.696382751832,132.809856982766,132.922875421434,
133.035120909341,133.063511684147),.UNSPECIFIED.);
#505=B_SPLINE_CURVE_WITH_KNOTS('',3,(#36130,#36131,#36132,#36133,#36134,
#36135,#36136,#36137,#36138,#36139,#36140,#36141,#36142,#36143,#36144,#36145,
#36146,#36147,#36148,#36149,#36150,#36151,#36152,#36153,#36154,#36155,#36156,
#36157,#36158,#36159,#36160,#36161,#36162,#36163,#36164,#36165,#36166,#36167,
#36168,#36169,#36170,#36171,#36172,#36173,#36174,#36175,#36176,#36177,#36178,
#36179,#36180,#36181,#36182,#36183,#36184,#36185,#36186,#36187,#36188,#36189,
#36190,#36191,#36192,#36193,#36194,#36195,#36196,#36197,#36198,#36199,#36200,
#36201,#36202,#36203,#36204,#36205,#36206,#36207,#36208,#36209,#36210,#36211,
#36212,#36213,#36214,#36215,#36216,#36217,#36218,#36219,#36220,#36221,#36222,
#36223,#36224,#36225,#36226,#36227,#36228,#36229,#36230,#36231,#36232,#36233,
#36234,#36235,#36236,#36237,#36238,#36239,#36240,#36241,#36242,#36243,#36244,
#36245,#36246,#36247,#36248,#36249,#36250,#36251,#36252,#36253,#36254,#36255,
#36256,#36257,#36258,#36259,#36260,#36261,#36262,#36263,#36264,#36265,#36266,
#36267,#36268,#36269,#36270,#36271,#36272,#36273,#36274,#36275,#36276,#36277,
#36278,#36279,#36280,#36281,#36282,#36283,#36284,#36285,#36286,#36287,#36288,
#36289,#36290,#36291,#36292,#36293,#36294,#36295,#36296,#36297,#36298,#36299,
#36300,#36301,#36302,#36303,#36304,#36305,#36306,#36307,#36308,#36309,#36310,
#36311,#36312,#36313,#36314,#36315,#36316,#36317,#36318,#36319,#36320,#36321,
#36322),.UNSPECIFIED.,.F.,.F.,(4,3,3,3,3,3,3,3,3,3,3,3,3,3,3,3,3,3,3,3,
3,3,3,3,3,3,3,3,3,3,3,3,3,3,3,3,3,3,3,3,3,3,3,3,3,3,3,3,3,3,3,3,3,3,3,3,
3,3,3,3,3,3,3,3,4),(133.063511684378,133.163441927701,133.263379444908,
133.363353474979,133.463460668199,133.563646061882,133.664007338062,133.69409991538,
133.793795690245,133.893348508343,133.993157079666,134.092530802596,134.191871714609,
134.291210259562,134.391361964404,134.490844937539,134.591331008233,134.691817078927,
134.791512859528,134.891065683314,134.990874253209,135.090247981665,135.189588899133,
135.288927449464,135.389079147717,135.488562125982,135.589048184229,135.689534242475,
135.789230038708,135.888782878248,135.98859144422,136.087965188613,136.18730612205,
136.28664468836,136.386796367776,136.486279361883,136.586765383953,136.687251406023,
136.786947147162,136.886499931537,136.986308511291,137.085682200745,137.185023079448,
137.284361591303,137.38451333587,137.483996276754,137.584482423162,137.68496856957,
137.784664367767,137.884217208881,137.98402577441,138.083399519428,138.182740453135,
138.282079019362,138.382230697801,138.481713690971,138.582199712044,138.682685733118,
138.782337641651,138.881849707232,138.981252599569,139.080581051976,139.179864432588,
139.279162144185,139.346696991558),.UNSPECIFIED.);
#506=B_SPLINE_CURVE_WITH_KNOTS('',3,(#36324,#36325,#36326,#36327,#36328,
#36329,#36330,#36331,#36332,#36333),.UNSPECIFIED.,.F.,.F.,(4,1,1,1,1,1,
1,4),(139.346704108471,139.680402896665,140.678120060213,141.675837223761,
142.673554387308,143.671271550856,144.668988714403,145.629877388167),
 .UNSPECIFIED.);
#507=B_SPLINE_CURVE_WITH_KNOTS('',3,(#36335,#36336,#36337,#36338,#36339,
#36340,#36341,#36342,#36343,#36344,#36345,#36346,#36347,#36348,#36349,#36350,
#36351,#36352,#36353,#36354,#36355,#36356,#36357,#36358,#36359,#36360,#36361,
#36362,#36363,#36364,#36365,#36366,#36367,#36368,#36369,#36370,#36371,#36372,
#36373,#36374,#36375,#36376,#36377,#36378,#36379,#36380,#36381,#36382,#36383,
#36384,#36385,#36386,#36387,#36388,#36389,#36390,#36391,#36392,#36393,#36394,
#36395,#36396,#36397,#36398,#36399,#36400,#36401,#36402,#36403,#36404,#36405,
#36406,#36407,#36408,#36409,#36410,#36411,#36412,#36413,#36414,#36415,#36416,
#36417,#36418,#36419,#36420,#36421,#36422,#36423,#36424,#36425,#36426,#36427,
#36428,#36429,#36430,#36431,#36432,#36433,#36434,#36435,#36436,#36437,#36438,
#36439,#36440,#36441,#36442,#36443,#36444,#36445,#36446,#36447,#36448,#36449,
#36450,#36451,#36452,#36453,#36454,#36455,#36456,#36457,#36458,#36459,#36460,
#36461,#36462,#36463,#36464,#36465,#36466,#36467,#36468,#36469,#36470,#36471,
#36472,#36473,#36474,#36475,#36476,#36477,#36478,#36479,#36480,#36481,#36482,
#36483,#36484,#36485,#36486,#36487,#36488,#36489,#36490,#36491,#36492,#36493,
#36494,#36495,#36496,#36497,#36498,#36499,#36500,#36501,#36502,#36503,#36504,
#36505,#36506,#36507,#36508,#36509,#36510,#36511,#36512,#36513,#36514,#36515,
#36516,#36517,#36518),.UNSPECIFIED.,.F.,.F.,(4,3,3,3,3,3,3,3,3,3,3,3,3,
3,3,3,3,3,3,3,3,3,3,3,3,3,3,3,3,3,3,3,3,3,3,3,3,3,3,3,3,3,3,3,3,3,3,3,3,
3,3,3,3,3,3,3,3,3,3,3,3,4),(145.629882298737,145.666705877951,145.766384642873,
145.865920420162,145.965733247829,146.065089978344,146.164413953413,146.263735639361,
146.363907489895,146.463373965384,146.563898503442,146.664423041499,146.76413985131,
146.863713619766,146.963516942926,147.062911262015,147.162272592399,147.261631351433,
147.361758564836,147.461261049816,147.561700627431,147.662140205046,147.761856531703,
147.86143020012,147.961233596179,148.060628734971,148.159991226439,148.259351484042,
148.35947795518,148.458982740841,148.559420054718,148.659857368594,148.759429470789,
148.85885831745,148.958697844287,149.057947757569,149.157165188389,149.256380742093,
149.356679189605,149.45604160929,149.556808070715,149.657574532141,149.757455188729,
149.857192392999,149.956954805835,150.056510368982,150.156031757094,150.255549171896,
150.355484802844,150.455140905904,150.555216300796,150.655291695689,150.754023326402,
150.857477251065,150.955955233998,151.054376281426,151.152772005683,151.251173984121,
151.349671802857,151.44822569065,151.546931739433,151.581654723703),
 .UNSPECIFIED.);
#508=B_SPLINE_CURVE_WITH_KNOTS('',3,(#36522,#36523,#36524,#36525,#36526,
#36527,#36528,#36529,#36530),.UNSPECIFIED.,.F.,.F.,(4,1,1,1,1,1,4),(-153.648443186332,
-152.650726022784,-151.653008859237,-150.655291695689,-149.657574532141,
-148.659857368594,-148.604832135738),.UNSPECIFIED.);
#509=B_SPLINE_CURVE_WITH_KNOTS('',3,(#36532,#36533,#36534,#36535,#36536,
#36537,#36538,#36539,#36540,#36541,#36542,#36543,#36544,#36545,#36546,#36547,
#36548,#36549,#36550,#36551,#36552,#36553,#36554,#36555,#36556,#36557,#36558,
#36559,#36560,#36561,#36562,#36563,#36564,#36565,#36566,#36567,#36568,#36569,
#36570,#36571,#36572,#36573,#36574,#36575,#36576,#36577,#36578,#36579,#36580,
#36581,#36582,#36583,#36584,#36585,#36586,#36587,#36588,#36589,#36590,#36591,
#36592,#36593,#36594,#36595,#36596,#36597,#36598,#36599,#36600,#36601,#36602,
#36603,#36604,#36605,#36606,#36607,#36608,#36609,#36610,#36611,#36612,#36613,
#36614,#36615,#36616,#36617,#36618,#36619,#36620,#36621,#36622,#36623,#36624,
#36625,#36626,#36627,#36628,#36629,#36630,#36631,#36632,#36633,#36634,#36635,
#36636,#36637,#36638,#36639,#36640,#36641,#36642,#36643,#36644,#36645,#36646,
#36647,#36648,#36649,#36650,#36651,#36652,#36653,#36654,#36655,#36656,#36657,
#36658,#36659,#36660,#36661,#36662,#36663,#36664,#36665,#36666,#36667,#36668,
#36669,#36670,#36671,#36672,#36673,#36674,#36675,#36676,#36677,#36678,#36679,
#36680,#36681,#36682,#36683,#36684,#36685,#36686,#36687,#36688,#36689,#36690,
#36691,#36692,#36693,#36694,#36695,#36696,#36697,#36698,#36699,#36700,#36701,
#36702,#36703,#36704,#36705,#36706,#36707,#36708,#36709,#36710,#36711,#36712,
#36713,#36714,#36715,#36716,#36717,#36718,#36719,#36720,#36721),
 .UNSPECIFIED.,.F.,.F.,(4,3,3,3,3,3,3,3,3,3,3,3,3,3,3,3,3,3,3,3,3,3,3,3,
3,3,3,3,3,3,3,3,3,3,3,3,3,3,3,3,3,3,3,3,3,3,3,3,3,3,3,3,3,3,3,3,3,3,3,3,
3,3,3,4),(-148.604832135738,-148.505962784877,-148.407231123561,-148.30860605164,
-148.210037628834,-148.111494393919,-148.012944919945,-147.914294538918,
-147.815588589436,-147.716717637151,-147.662140205046,-147.562425664213,
-147.462853677051,-147.363049847607,-147.263656113331,-147.164294916824,
-147.064935841065,-146.964807641174,-146.865303738886,-146.764863390193,
-146.664423041499,-146.564743311022,-146.465206774951,-146.365394162826,
-146.266037180969,-146.166713145758,-146.067391590729,-145.967220162534,
-145.867754284884,-145.767230081417,-145.666705877951,-145.567006099255,
-145.467449250399,-145.3676416834,-145.268263894502,-145.168918912445,-145.069576298971,
-144.969429402829,-144.869942406862,-144.769465560633,-144.668988714403,
-144.569290954782,-144.469736104588,-144.369928035372,-144.270552179694,
-144.171209101692,-144.071868360348,-143.971719157975,-143.872233935751,
-143.771752743304,-143.671271550856,-143.57157791419,-143.472027267565,
-143.372218157532,-143.27284667114,-143.173508015202,-143.074171742837,
-142.974017403955,-142.874536720922,-142.774045554115,-142.673554387308,
-142.558582310432,-142.440114569609,-142.321646828785),.UNSPECIFIED.);
#510=B_SPLINE_CURVE_WITH_KNOTS('',3,(#36723,#36724,#36725,#36726,#36727,
#36728,#36729,#36730,#36731,#36732,#36733,#36734,#36735,#36736,#36737,#36738,
#36739,#36740,#36741,#36742,#36743,#36744,#36745,#36746,#36747,#36748,#36749,
#36750,#36751,#36752,#36753,#36754,#36755,#36756,#36757,#36758,#36759,#36760,
#36761,#36762,#36763,#36764,#36765,#36766,#36767,#36768,#36769,#36770,#36771,
#36772,#36773,#36774,#36775,#36776,#36777,#36778,#36779,#36780,#36781,#36782,
#36783,#36784,#36785,#36786,#36787,#36788,#36789,#36790,#36791,#36792,#36793,
#36794,#36795,#36796,#36797,#36798,#36799,#36800,#36801,#36802,#36803,#36804,
#36805,#36806,#36807,#36808,#36809,#36810,#36811,#36812,#36813,#36814,#36815,
#36816,#36817,#36818,#36819,#36820,#36821,#36822,#36823,#36824,#36825,#36826,
#36827,#36828,#36829,#36830,#36831,#36832,#36833,#36834,#36835,#36836,#36837,
#36838,#36839,#36840,#36841,#36842,#36843,#36844,#36845,#36846,#36847,#36848,
#36849,#36850,#36851,#36852,#36853,#36854,#36855,#36856,#36857,#36858,#36859,
#36860,#36861,#36862,#36863,#36864,#36865,#36866,#36867,#36868,#36869,#36870,
#36871,#36872,#36873,#36874,#36875,#36876,#36877,#36878,#36879,#36880,#36881,
#36882,#36883,#36884,#36885,#36886,#36887,#36888,#36889,#36890,#36891,#36892,
#36893,#36894,#36895,#36896,#36897,#36898,#36899,#36900,#36901,#36902,#36903,
#36904,#36905,#36906,#36907,#36908,#36909,#36910,#36911,#36912,#36913,#36914,
#36915),.UNSPECIFIED.,.F.,.F.,(4,3,3,3,3,3,3,3,3,3,3,3,3,3,3,3,3,3,3,3,
3,3,3,3,3,3,3,3,3,3,3,3,3,3,3,3,3,3,3,3,3,3,3,3,3,3,3,3,3,3,3,3,3,3,3,3,
3,3,3,3,3,3,3,3,4),(-142.321646828558,-142.222022503885,-142.122401901353,
-142.022755196475,-141.922984285233,-141.823143319578,-141.723124900889,
-141.675837223761,-141.576141255699,-141.476588239077,-141.376779716719,
-141.277405783711,-141.178064657725,-141.078725895178,-140.978574436437,
-140.879091238983,-140.778605649598,-140.678120060213,-140.578424560305,
-140.478872021712,-140.379063381081,-140.279689946681,-140.180349325956,
-140.081011074658,-139.98085903016,-139.881376353523,-139.780889625094,
-139.680402896665,-139.580707011083,-139.481154081145,-139.381345537641,
-139.281971700972,-139.182630674759,-139.083292015298,-138.983140444753,
-138.883657357531,-138.783171545324,-138.682685733118,-138.582989938995,
-138.483437101079,-138.383628534641,-138.284254790672,-138.184913857203,
-138.085575290406,-137.985423610197,-137.88594061448,-137.785454592025,
-137.68496856957,-137.58527282556,-137.485720038928,-137.385911459815,-137.286537769609,
-137.187196890722,-137.087858379249,-136.987706635943,-136.888223696826,
-136.787737551424,-136.687251406023,-136.587301790218,-136.48749505883,
-136.387800988718,-136.288189658078,-136.188626947872,-136.089062730842,
-136.038461521379),.UNSPECIFIED.);
#511=B_SPLINE_CURVE_WITH_KNOTS('',3,(#36917,#36918,#36919,#36920,#36921,
#36922,#36923,#36924,#36925,#36926,#36927,#36928,#36929,#36930,#36931,#36932,
#36933,#36934,#36935,#36936,#36937,#36938,#36939,#36940,#36941,#36942,#36943,
#36944,#36945,#36946,#36947,#36948,#36949,#36950,#36951,#36952,#36953,#36954,
#36955,#36956,#36957,#36958,#36959,#36960,#36961,#36962,#36963,#36964,#36965,
#36966,#36967,#36968,#36969,#36970,#36971,#36972,#36973,#36974,#36975,#36976,
#36977,#36978,#36979,#36980,#36981,#36982,#36983,#36984,#36985,#36986,#36987,
#36988,#36989,#36990,#36991,#36992,#36993,#36994,#36995,#36996,#36997,#36998,
#36999,#37000,#37001,#37002,#37003,#37004,#37005,#37006,#37007,#37008,#37009,
#37010,#37011,#37012,#37013,#37014,#37015,#37016,#37017,#37018,#37019,#37020,
#37021,#37022,#37023,#37024,#37025,#37026,#37027,#37028,#37029,#37030,#37031,
#37032,#37033,#37034,#37035,#37036,#37037,#37038,#37039,#37040,#37041,#37042,
#37043,#37044,#37045,#37046,#37047,#37048,#37049,#37050,#37051,#37052,#37053,
#37054,#37055,#37056,#37057,#37058,#37059,#37060,#37061,#37062,#37063,#37064,
#37065,#37066,#37067,#37068,#37069,#37070,#37071,#37072,#37073,#37074,#37075,
#37076,#37077,#37078,#37079,#37080,#37081,#37082,#37083,#37084,#37085,#37086,
#37087,#37088,#37089,#37090,#37091,#37092,#37093,#37094,#37095,#37096,#37097,
#37098,#37099,#37100,#37101,#37102,#37103,#37104,#37105,#37106),
 .UNSPECIFIED.,.F.,.F.,(4,3,3,3,3,3,3,3,3,3,3,3,3,3,3,3,3,3,3,3,3,3,3,3,
3,3,3,3,3,3,3,3,3,3,3,3,3,3,3,3,3,3,3,3,3,3,3,3,3,3,3,3,3,3,3,3,3,3,3,3,
3,3,3,4),(-136.038461521153,-135.924409265068,-135.806971753772,-135.689534242475,
-135.589838462332,-135.490285638907,-135.390477068909,-135.29110334057,
-135.191762423128,-135.092423872733,-134.992272174281,-134.892789195728,
-134.792303137327,-134.691817078927,-134.59212130367,-134.492568485263,
-134.392759914028,-134.293386190995,-134.194045278957,-134.094706734055,
-133.994555029386,-133.895072056493,-133.794585985936,-133.69409991538,
-133.594404133346,-133.494851308051,-133.395042738524,-133.29566900839,
-133.196328089184,-133.096989537059,-132.996837840753,-132.897354860572,
-132.796868806202,-132.696382751832,-132.596686972278,-132.497134149491,
-132.39732557934,-132.297951851756,-132.198610935112,-132.099272385557,
-131.999120686239,-131.899637708619,-131.799151648452,-131.698665588285,
-131.598969809128,-131.499416986751,-131.399608416499,-131.300234689358,
-131.200893773167,-131.101555224075,-131.001403524241,-130.901920547106,
-130.801434485922,-130.700948424737,-130.602038734921,-130.50327125118,
-130.404617056666,-130.30602371374,-130.207459776814,-130.108893838909,
-130.010232689273,-129.911519685389,-129.812645395257,-129.755276214539),
 .UNSPECIFIED.);
#512=B_SPLINE_CURVE_WITH_KNOTS('',3,(#37108,#37109,#37110,#37111,#37112,
#37113,#37114,#37115,#37116,#37117,#37118,#37119,#37120,#37121,#37122,#37123,
#37124,#37125,#37126,#37127,#37128,#37129,#37130,#37131,#37132,#37133,#37134,
#37135,#37136,#37137,#37138,#37139,#37140,#37141,#37142,#37143,#37144,#37145,
#37146,#37147,#37148,#37149,#37150,#37151,#37152,#37153,#37154,#37155,#37156,
#37157,#37158,#37159,#37160,#37161,#37162,#37163,#37164,#37165,#37166,#37167,
#37168,#37169,#37170,#37171,#37172,#37173,#37174,#37175,#37176,#37177,#37178,
#37179,#37180,#37181,#37182,#37183,#37184,#37185,#37186,#37187,#37188,#37189,
#37190,#37191,#37192,#37193,#37194,#37195,#37196,#37197,#37198,#37199,#37200,
#37201,#37202,#37203,#37204,#37205,#37206,#37207,#37208,#37209,#37210,#37211,
#37212,#37213,#37214,#37215,#37216,#37217,#37218,#37219,#37220,#37221,#37222,
#37223,#37224,#37225,#37226,#37227,#37228,#37229,#37230,#37231,#37232,#37233,
#37234,#37235,#37236,#37237,#37238,#37239,#37240,#37241,#37242,#37243,#37244,
#37245,#37246,#37247,#37248,#37249,#37250,#37251,#37252,#37253,#37254,#37255,
#37256,#37257,#37258,#37259,#37260,#37261,#37262,#37263,#37264,#37265,#37266,
#37267,#37268,#37269,#37270,#37271,#37272,#37273,#37274,#37275,#37276,#37277,
#37278,#37279,#37280,#37281,#37282,#37283,#37284,#37285,#37286,#37287,#37288,
#37289,#37290,#37291,#37292,#37293,#37294,#37295,#37296,#37297),
 .UNSPECIFIED.,.F.,.F.,(4,3,3,3,3,3,3,3,3,3,3,3,3,3,3,3,3,3,3,3,3,3,3,3,
3,3,3,3,3,3,3,3,3,3,3,3,3,3,3,3,3,3,3,3,3,3,3,3,3,3,3,3,3,3,3,3,3,3,3,3,
3,3,3,4),(-129.755276214199,-129.703231261189,-129.603535481542,-129.503982658665,
-129.404174088537,-129.304800360874,-129.205459444155,-129.106120894529,
-129.005969195307,-128.906486217628,-128.806000157635,-128.705514097642,
-128.605818318012,-128.506265495153,-128.406456925021,-128.307083197379,
-128.207742280683,-128.108403731081,-128.008252031834,-127.908769054182,
-127.808282994138,-127.707796934094,-127.608101154355,-127.508548331385,
-127.40873976128,-127.309366033524,-127.210025116712,-127.110686566993,
-127.010534867881,-126.911051890111,-126.810565830328,-126.710079770546,
-126.610383990863,-126.510831167951,-126.411022597832,-126.311648870134,
-126.212307953381,-126.11296940372,-126.01281770454,-125.913334726828,-125.812848666914,
-125.712362606999,-125.612666827313,-125.513114004398,-125.413305434279,
-125.313931706579,-125.214590789824,-125.115252240161,-125.015100540983,
-124.91561756327,-124.81513150336,-124.714645443451,-124.614949663752,-124.515396840823,
-124.415588270708,-124.316214542995,-124.216873626225,-124.117535076548,
-124.017383377387,-123.917900399659,-123.817414339782,-123.716928279904,
-123.586846403148,-123.472090978371),.UNSPECIFIED.);
#513=B_SPLINE_CURVE_WITH_KNOTS('',3,(#37299,#37300,#37301,#37302,#37303,
#37304,#37305,#37306,#37307,#37308),.UNSPECIFIED.,.F.,.F.,(4,1,1,1,1,1,
1,4),(-123.47209090702,-122.719211116356,-121.721493952808,-120.723776789261,
-119.726059625713,-118.728342462166,-117.730625298618,-117.18890559984),
 .UNSPECIFIED.);
#514=B_SPLINE_CURVE_WITH_KNOTS('',3,(#37310,#37311,#37312,#37313,#37314,
#37315,#37316,#37317,#37318,#37319,#37320,#37321,#37322,#37323,#37324,#37325,
#37326,#37327,#37328,#37329,#37330,#37331,#37332,#37333,#37334,#37335,#37336,
#37337,#37338,#37339,#37340,#37341,#37342,#37343,#37344,#37345,#37346,#37347,
#37348,#37349,#37350,#37351,#37352,#37353,#37354,#37355,#37356,#37357,#37358,
#37359,#37360,#37361,#37362,#37363,#37364,#37365,#37366,#37367,#37368,#37369,
#37370,#37371,#37372,#37373,#37374,#37375,#37376,#37377,#37378,#37379,#37380,
#37381,#37382,#37383,#37384,#37385,#37386,#37387,#37388,#37389,#37390,#37391,
#37392,#37393,#37394,#37395,#37396,#37397,#37398,#37399,#37400,#37401,#37402,
#37403,#37404,#37405,#37406,#37407,#37408,#37409,#37410,#37411,#37412,#37413,
#37414,#37415,#37416,#37417,#37418,#37419,#37420,#37421,#37422,#37423,#37424,
#37425,#37426,#37427,#37428,#37429,#37430,#37431,#37432,#37433,#37434,#37435,
#37436,#37437,#37438,#37439,#37440,#37441,#37442,#37443,#37444,#37445,#37446,
#37447,#37448,#37449,#37450,#37451,#37452,#37453,#37454,#37455,#37456,#37457,
#37458,#37459,#37460,#37461,#37462,#37463,#37464,#37465,#37466,#37467,#37468,
#37469,#37470,#37471,#37472,#37473,#37474,#37475,#37476,#37477,#37478,#37479,
#37480,#37481,#37482,#37483,#37484,#37485,#37486,#37487,#37488,#37489,#37490,
#37491,#37492,#37493,#37494,#37495,#37496,#37497,#37498,#37499,#37500,#37501,
#37502),.UNSPECIFIED.,.F.,.F.,(4,3,3,3,3,3,3,3,3,3,3,3,3,3,3,3,3,3,3,3,
3,3,3,3,3,3,3,3,3,3,3,3,3,3,3,3,3,3,3,3,3,3,3,3,3,3,3,3,3,3,3,3,3,3,3,3,
3,3,3,3,3,3,3,3,4),(-117.188905373774,-117.082806220657,-116.976309141457,
-116.869598521819,-116.76256993861,-116.73290813507,-116.633212355378,-116.533659532456,
-116.433850962339,-116.334477234632,-116.23513631787,-116.1357977682,-116.035646069031,
-115.93616309131,-115.835677031416,-115.735190971523,-115.63549519183,-115.535942368908,
-115.436133798791,-115.336760071084,-115.23741915432,-115.13808060465,-115.037928905481,
-114.93844592776,-114.837959867867,-114.737473807975,-114.637778028282,
-114.53822520536,-114.438416635244,-114.339042907536,-114.239701990773,
-114.140363441103,-114.040211741934,-113.940728764213,-113.840242704321,
-113.739756644428,-113.640060864735,-113.540508041813,-113.440699471697,
-113.341325743989,-113.241984827226,-113.142646277556,-113.042494578387,
-112.943011600666,-112.842525540773,-112.74203948088,-112.642343701187,
-112.542790878265,-112.442982308148,-112.343608580441,-112.244267663677,
-112.144929114007,-112.044777414838,-111.945294437117,-111.844808377224,
-111.744322317332,-111.646106275261,-111.548054692826,-111.45009534431,
-111.352196038359,-111.254324663627,-111.156401948211,-111.058451996033,
-110.960378173053,-110.905720293008),.UNSPECIFIED.);
#515=B_SPLINE_CURVE_WITH_KNOTS('',3,(#37504,#37505,#37506,#37507,#37508,
#37509,#37510,#37511,#37512,#37513,#37514,#37515,#37516,#37517,#37518,#37519,
#37520,#37521,#37522,#37523,#37524,#37525,#37526,#37527,#37528,#37529,#37530,
#37531,#37532,#37533,#37534,#37535,#37536,#37537,#37538,#37539,#37540,#37541,
#37542,#37543,#37544,#37545,#37546,#37547,#37548,#37549,#37550,#37551,#37552,
#37553,#37554,#37555,#37556,#37557,#37558,#37559,#37560,#37561,#37562,#37563,
#37564,#37565,#37566,#37567,#37568,#37569,#37570,#37571,#37572,#37573,#37574,
#37575,#37576,#37577,#37578,#37579,#37580,#37581,#37582,#37583,#37584,#37585,
#37586,#37587,#37588,#37589,#37590,#37591,#37592,#37593,#37594,#37595,#37596,
#37597,#37598,#37599,#37600,#37601,#37602,#37603,#37604,#37605,#37606,#37607,
#37608,#37609,#37610,#37611,#37612,#37613,#37614,#37615,#37616,#37617,#37618,
#37619,#37620,#37621,#37622,#37623,#37624,#37625,#37626,#37627,#37628,#37629,
#37630,#37631,#37632,#37633,#37634,#37635,#37636,#37637,#37638,#37639,#37640,
#37641,#37642,#37643,#37644,#37645,#37646,#37647,#37648,#37649,#37650,#37651,
#37652,#37653,#37654,#37655,#37656,#37657,#37658,#37659,#37660,#37661,#37662,
#37663,#37664,#37665,#37666,#37667,#37668,#37669,#37670,#37671,#37672,#37673,
#37674,#37675,#37676,#37677,#37678,#37679,#37680,#37681,#37682,#37683,#37684,
#37685,#37686,#37687,#37688,#37689,#37690),.UNSPECIFIED.,.F.,.F.,(4,3,3,
3,3,3,3,3,3,3,3,3,3,3,3,3,3,3,3,3,3,3,3,3,3,3,3,3,3,3,3,3,3,3,3,3,3,3,3,
3,3,3,3,3,3,3,3,3,3,3,3,3,3,3,3,3,3,3,3,3,3,3,4),(-110.90572029266,-110.746605153785,
-110.646909374091,-110.547356551166,-110.44754798105,-110.348174253341,
-110.248833336576,-110.149494786903,-110.049343087737,-109.949860110014,
-109.849374050125,-109.748887990237,-109.649192210544,-109.549639387622,
-109.449830817506,-109.350457089798,-109.251116173035,-109.151777623365,
-109.051625924196,-108.952142946475,-108.851656886582,-108.751170826689,
-108.651475046997,-108.551922224075,-108.452113653958,-108.352739926252,
-108.253399009489,-108.154060459819,-108.05390876065,-107.954425782929,
-107.853939723036,-107.753453663142,-107.653757883449,-107.554205060526,
-107.45439649041,-107.355022762702,-107.255681845939,-107.156343296268,
-107.0561915971,-106.956708619378,-106.856222559486,-106.755736499594,-106.656040719902,
-106.556487896979,-106.456679326863,-106.357305599156,-106.257964682393,
-106.158626132723,-106.058474433554,-105.958991455833,-105.85850539594,
-105.758019336047,-105.658323556354,-105.558770733432,-105.458962163316,
-105.359588435608,-105.260247518845,-105.160908969175,-105.060757270006,
-104.961274292285,-104.860788232392,-104.760302172499,-104.622534985481),
 .UNSPECIFIED.);
#516=B_SPLINE_CURVE_WITH_KNOTS('',3,(#37692,#37693,#37694,#37695,#37696,
#37697,#37698,#37699,#37700,#37701),.UNSPECIFIED.,.F.,.F.,(4,1,1,1,1,1,
1,4),(-104.622526910524,-103.762585008951,-102.764867845404,-101.767150681856,
-100.769433518309,-99.771716354761,-98.7739991912134,-98.3393545396807),
 .UNSPECIFIED.);
#517=B_SPLINE_CURVE_WITH_KNOTS('',3,(#37703,#37704,#37705,#37706,#37707,
#37708,#37709,#37710,#37711,#37712,#37713,#37714,#37715,#37716,#37717,#37718,
#37719,#37720,#37721,#37722,#37723,#37724,#37725,#37726,#37727,#37728,#37729,
#37730,#37731,#37732,#37733,#37734,#37735,#37736,#37737,#37738,#37739,#37740,
#37741,#37742,#37743,#37744,#37745,#37746,#37747,#37748,#37749,#37750,#37751,
#37752,#37753,#37754,#37755,#37756,#37757,#37758,#37759,#37760,#37761,#37762,
#37763,#37764,#37765,#37766,#37767,#37768,#37769,#37770,#37771,#37772,#37773,
#37774,#37775,#37776,#37777,#37778,#37779,#37780,#37781,#37782,#37783,#37784,
#37785,#37786,#37787,#37788,#37789,#37790,#37791,#37792,#37793,#37794,#37795,
#37796,#37797,#37798,#37799,#37800,#37801,#37802,#37803,#37804,#37805,#37806,
#37807,#37808,#37809,#37810,#37811,#37812,#37813,#37814,#37815,#37816,#37817,
#37818,#37819,#37820,#37821,#37822,#37823,#37824,#37825,#37826,#37827,#37828,
#37829,#37830,#37831,#37832,#37833,#37834,#37835,#37836,#37837,#37838,#37839,
#37840,#37841,#37842,#37843,#37844,#37845,#37846,#37847,#37848,#37849,#37850,
#37851,#37852,#37853,#37854,#37855,#37856,#37857,#37858,#37859,#37860,#37861,
#37862,#37863,#37864,#37865,#37866,#37867,#37868,#37869,#37870,#37871,#37872,
#37873,#37874,#37875,#37876,#37877,#37878,#37879,#37880,#37881,#37882,#37883,
#37884,#37885,#37886,#37887,#37888,#37889,#37890,#37891,#37892,#37893,#37894,
#37895),.UNSPECIFIED.,.F.,.F.,(4,3,3,3,3,3,3,3,3,3,3,3,3,3,3,3,3,3,3,3,
3,3,3,3,3,3,3,3,3,3,3,3,3,3,3,3,3,3,3,3,3,3,3,3,3,3,3,3,3,3,3,3,3,3,3,3,
3,3,3,3,3,3,3,3,4),(-98.3393496783013,-98.2376690492644,-98.1359188389092,
-98.0339904197929,-97.9319640594039,-97.8297250457828,-97.7762820276658,
-97.6765862479732,-97.5770334250509,-97.4772248549343,-97.377851127227,
-97.278510210464,-97.1791716607937,-97.0790199616248,-96.9795369839036,
-96.8790509240109,-96.7785648641182,-96.6788690844256,-96.5793162615036,
-96.4795076913869,-96.3801339636796,-96.2807930469166,-96.1814544972463,
-96.0813027980773,-95.9818198203562,-95.8813337604633,-95.7808477005705,
-95.6811519208779,-95.5815990979555,-95.4817905278389,-95.3824168001316,
-95.2830758833684,-95.1837373336981,-95.0835856345293,-94.9841026568082,
-94.8836165969155,-94.7831305370229,-94.6834347573304,-94.583881934408,
-94.4840733642914,-94.3846996365841,-94.2853587198211,-94.1860201701505,
-94.0858684709817,-93.9863854932605,-93.8858994333679,-93.7854133734753,
-93.6857175937827,-93.5861647708604,-93.4863562007438,-93.3869824730366,
-93.2876415562734,-93.1883030066032,-93.0881513074343,-92.9886683297131,
-92.8881822698204,-92.7876962099277,-92.6890183930632,-92.5904711330326,
-92.492022572886,-92.3936409753712,-92.2952704891613,-92.1969067553828,
-92.0984785297572,-92.0561643711217),.UNSPECIFIED.);
#518=B_SPLINE_CURVE_WITH_KNOTS('',3,(#37897,#37898,#37899,#37900,#37901,
#37902,#37903,#37904,#37905,#37906,#37907,#37908,#37909,#37910,#37911,#37912,
#37913,#37914,#37915,#37916,#37917,#37918,#37919,#37920,#37921,#37922,#37923,
#37924,#37925,#37926,#37927,#37928,#37929,#37930,#37931,#37932,#37933,#37934,
#37935,#37936,#37937,#37938,#37939,#37940,#37941,#37942,#37943,#37944,#37945,
#37946,#37947,#37948,#37949,#37950,#37951,#37952,#37953,#37954,#37955,#37956,
#37957,#37958,#37959,#37960,#37961,#37962,#37963,#37964,#37965,#37966,#37967,
#37968,#37969,#37970,#37971,#37972,#37973,#37974,#37975,#37976,#37977,#37978,
#37979,#37980,#37981,#37982,#37983,#37984,#37985,#37986,#37987,#37988,#37989,
#37990,#37991,#37992,#37993,#37994,#37995,#37996,#37997,#37998,#37999,#38000,
#38001,#38002,#38003,#38004,#38005,#38006,#38007,#38008,#38009,#38010,#38011,
#38012,#38013,#38014,#38015,#38016,#38017,#38018,#38019,#38020,#38021,#38022,
#38023,#38024,#38025,#38026,#38027,#38028,#38029,#38030,#38031,#38032,#38033,
#38034,#38035,#38036,#38037,#38038,#38039,#38040,#38041,#38042,#38043,#38044,
#38045,#38046,#38047,#38048,#38049,#38050,#38051,#38052,#38053,#38054,#38055,
#38056,#38057,#38058,#38059,#38060,#38061,#38062,#38063,#38064,#38065,#38066,
#38067,#38068,#38069,#38070,#38071,#38072,#38073,#38074,#38075,#38076,#38077,
#38078,#38079,#38080,#38081,#38082,#38083,#38084,#38085,#38086,#38087,#38088,
#38089),.UNSPECIFIED.,.F.,.F.,(4,3,3,3,3,3,3,3,3,3,3,3,3,3,3,3,3,3,3,3,
3,3,3,3,3,3,3,3,3,3,3,3,3,3,3,3,3,3,3,3,3,3,3,3,3,3,3,3,3,3,3,3,3,3,3,3,
3,3,3,3,3,3,3,3,4),(-92.0561643707478,-91.931627218391,-91.8046642324725,
-91.7899790463801,-91.6902832666874,-91.5907304437651,-91.4909218736485,
-91.3915481459411,-91.292207229178,-91.1928686795075,-91.0927169803387,
-90.9932340026175,-90.892747942725,-90.7922618828325,-90.6925661031399,
-90.5930132802175,-90.4932047101009,-90.3938309823936,-90.2944900656304,
-90.1951515159601,-90.0949998167913,-89.9955168390701,-89.8950307791775,
-89.7945447192849,-89.6948489395923,-89.5952961166701,-89.4954875465535,
-89.3961138188463,-89.2967729020832,-89.197434352413,-89.097282653244,-88.9977996755229,
-88.8973136156301,-88.7968275557373,-88.6971317760447,-88.5975789531223,
-88.4977703830058,-88.3983966552984,-88.2990557385353,-88.1997171888649,
-88.0995654896961,-88.000082511975,-87.8995964520823,-87.7991103921897,
-87.6994146124971,-87.5998617895749,-87.5000532194583,-87.400679491751,
-87.301338574988,-87.2020000253177,-87.1018483261488,-87.0023653484277,
-86.9018792885349,-86.8013932286421,-86.7016974489495,-86.6021446260272,
-86.5023360559106,-86.4029623282033,-86.3036214114402,-86.20428286177,-86.1041311626011,
-86.00464818488,-85.9041621249873,-85.8036760650945,-85.7729790639421),
 .UNSPECIFIED.);
#519=B_SPLINE_CURVE_WITH_KNOTS('',3,(#38091,#38092,#38093,#38094,#38095,
#38096,#38097,#38098,#38099,#38100,#38101,#38102,#38103,#38104,#38105,#38106,
#38107,#38108,#38109,#38110,#38111,#38112,#38113,#38114,#38115,#38116,#38117,
#38118,#38119,#38120,#38121,#38122,#38123,#38124,#38125,#38126,#38127,#38128,
#38129,#38130,#38131,#38132,#38133,#38134,#38135,#38136,#38137,#38138,#38139,
#38140,#38141,#38142,#38143,#38144,#38145,#38146,#38147,#38148,#38149,#38150,
#38151,#38152,#38153,#38154,#38155,#38156,#38157,#38158,#38159,#38160,#38161,
#38162,#38163,#38164,#38165,#38166,#38167,#38168,#38169,#38170,#38171,#38172,
#38173,#38174,#38175,#38176,#38177,#38178,#38179,#38180,#38181,#38182,#38183,
#38184,#38185,#38186,#38187,#38188,#38189,#38190,#38191,#38192,#38193,#38194,
#38195,#38196,#38197,#38198,#38199,#38200,#38201,#38202,#38203,#38204,#38205,
#38206,#38207,#38208,#38209,#38210,#38211,#38212,#38213,#38214,#38215,#38216,
#38217,#38218,#38219,#38220,#38221,#38222,#38223,#38224,#38225,#38226,#38227,
#38228,#38229,#38230,#38231,#38232,#38233,#38234,#38235,#38236,#38237,#38238,
#38239,#38240,#38241,#38242,#38243,#38244,#38245,#38246,#38247,#38248,#38249,
#38250,#38251,#38252,#38253,#38254,#38255,#38256,#38257,#38258,#38259,#38260,
#38261,#38262,#38263,#38264,#38265,#38266,#38267,#38268,#38269,#38270,#38271,
#38272,#38273,#38274,#38275,#38276,#38277,#38278,#38279,#38280),
 .UNSPECIFIED.,.F.,.F.,(4,3,3,3,3,3,3,3,3,3,3,3,3,3,3,3,3,3,3,3,3,3,3,3,
3,3,3,3,3,3,3,3,3,3,3,3,3,3,3,3,3,3,3,3,3,3,3,3,3,3,3,3,3,3,3,3,3,3,3,3,
3,3,3,4),(-85.7729790637246,-85.6737911039112,-85.5747441639126,-85.475808919837,
-85.3769340092717,-85.2780883091123,-85.1792407338146,-85.0802938326087,
-84.98129593964,-84.8821251945386,-84.8059589015468,-84.7062631218542,-84.6067102989321,
-84.5069017288155,-84.4075280011082,-84.3081870843452,-84.2088485346748,
-84.1086968355059,-84.0092138577848,-83.908727797892,-83.8082417379992,
-83.7085459583067,-83.6089931353844,-83.5091845652678,-83.4098108375605,
-83.3104699207974,-83.2111313711273,-83.1109796719583,-83.0114966942372,
-82.9110106343444,-82.8105245744516,-82.710828794759,-82.6112759718368,
-82.5114674017202,-82.4120936740129,-82.3127527572499,-82.2134142075797,
-82.1132625084108,-82.0137795306895,-81.9132934707968,-81.812807410904,
-81.7131116312114,-81.613558808289,-81.5137502381724,-81.4143765104651,
-81.3150355937019,-81.2156970440318,-81.1155453448629,-81.0160623671418,
-80.9155763072491,-80.8150902473564,-80.7153944676637,-80.6158416447413,
-80.5160330746247,-80.4166593469174,-80.3173184301543,-80.217979880484,
-80.1178281813152,-80.0183452035941,-79.9178591437014,-79.8173730838088,
-79.6996970766505,-79.5832300154978,-79.489793756973),.UNSPECIFIED.);
#520=B_SPLINE_CURVE_WITH_KNOTS('',3,(#38282,#38283,#38284,#38285,#38286,
#38287,#38288,#38289,#38290,#38291,#38292,#38293,#38294,#38295,#38296,#38297,
#38298,#38299,#38300,#38301,#38302,#38303,#38304,#38305,#38306,#38307,#38308,
#38309,#38310,#38311,#38312,#38313,#38314,#38315,#38316,#38317,#38318,#38319,
#38320,#38321,#38322,#38323,#38324,#38325,#38326,#38327,#38328,#38329,#38330,
#38331,#38332,#38333,#38334,#38335,#38336,#38337,#38338,#38339,#38340,#38341,
#38342,#38343,#38344,#38345,#38346,#38347,#38348,#38349,#38350,#38351,#38352,
#38353,#38354,#38355,#38356,#38357,#38358,#38359,#38360,#38361,#38362,#38363,
#38364,#38365,#38366,#38367,#38368,#38369,#38370,#38371,#38372,#38373,#38374,
#38375,#38376,#38377,#38378,#38379,#38380,#38381,#38382,#38383,#38384,#38385,
#38386,#38387,#38388,#38389,#38390,#38391,#38392,#38393,#38394,#38395,#38396,
#38397,#38398,#38399,#38400,#38401,#38402,#38403,#38404,#38405,#38406,#38407,
#38408,#38409,#38410,#38411,#38412,#38413,#38414,#38415,#38416,#38417,#38418,
#38419,#38420,#38421,#38422,#38423,#38424,#38425,#38426,#38427,#38428,#38429,
#38430,#38431,#38432,#38433,#38434,#38435,#38436,#38437,#38438,#38439,#38440,
#38441,#38442,#38443,#38444,#38445,#38446,#38447,#38448,#38449,#38450,#38451,
#38452,#38453,#38454,#38455,#38456,#38457,#38458,#38459,#38460,#38461,#38462,
#38463,#38464,#38465,#38466,#38467,#38468,#38469,#38470,#38471,#38472,#38473,
#38474),.UNSPECIFIED.,.F.,.F.,(4,3,3,3,3,3,3,3,3,3,3,3,3,3,3,3,3,3,3,3,
3,3,3,3,3,3,3,3,3,3,3,3,3,3,3,3,3,3,3,3,3,3,3,3,3,3,3,3,3,3,3,3,3,3,3,3,
3,3,3,3,3,3,3,3,4),(-79.4897937567625,-79.3905970449177,-79.2914199481721,
-79.192231915772,-79.0929327497898,-78.9935756638494,-78.8940377107173,
-78.8196559202612,-78.7199601405687,-78.6204073176465,-78.5205987475299,
-78.4212250198226,-78.3218841030596,-78.2225455533893,-78.1223938542204,
-78.0229108764993,-77.9224248166065,-77.8219387567136,-77.722242977021,
-77.6226901540989,-77.5228815839823,-77.423507856275,-77.3241669395119,
-77.2248283898415,-77.1246766906727,-77.0251937129515,-76.9247076530588,
-76.824221593166,-76.7245258134733,-76.6249729905509,-76.5251644204344,
-76.425790692727,-76.3264497759638,-76.2271112262934,-76.1269595271247,
-76.0274765494036,-75.926990489511,-75.8265044296184,-75.7268086499258,
-75.6272558270034,-75.5274472568868,-75.4280735291795,-75.3287326124164,
-75.2293940627459,-75.1292423635771,-75.0297593858559,-74.9292733259633,
-74.8287872660707,-74.7290914863781,-74.6295386634556,-74.5297300933391,
-74.4303563656318,-74.3310154488686,-74.2316768991982,-74.1315252000294,
-74.0320422223083,-73.9315561624157,-73.8310701025231,-73.7305796798271,
-73.6302379772179,-73.530015697372,-73.4298907195394,-73.3298214476302,
-73.229770789038,-73.206608449583),.UNSPECIFIED.);
#521=B_SPLINE_CURVE_WITH_KNOTS('',3,(#38476,#38477,#38478,#38479,#38480,
#38481,#38482,#38483,#38484,#38485,#38486,#38487,#38488,#38489,#38490,#38491,
#38492,#38493,#38494,#38495,#38496,#38497,#38498,#38499,#38500,#38501,#38502,
#38503,#38504,#38505,#38506,#38507,#38508,#38509,#38510,#38511,#38512,#38513,
#38514,#38515,#38516,#38517,#38518,#38519,#38520,#38521,#38522,#38523,#38524,
#38525,#38526,#38527,#38528,#38529,#38530,#38531,#38532,#38533,#38534,#38535,
#38536,#38537,#38538,#38539,#38540,#38541,#38542,#38543,#38544,#38545,#38546,
#38547,#38548,#38549,#38550,#38551,#38552,#38553,#38554,#38555,#38556,#38557,
#38558,#38559,#38560,#38561,#38562,#38563,#38564,#38565,#38566,#38567,#38568,
#38569,#38570,#38571,#38572,#38573,#38574,#38575,#38576,#38577,#38578,#38579,
#38580,#38581,#38582,#38583,#38584,#38585,#38586,#38587,#38588,#38589,#38590,
#38591,#38592,#38593,#38594,#38595,#38596,#38597,#38598,#38599,#38600,#38601,
#38602,#38603,#38604,#38605,#38606,#38607,#38608,#38609,#38610,#38611,#38612,
#38613,#38614,#38615,#38616,#38617,#38618,#38619,#38620,#38621,#38622,#38623,
#38624,#38625,#38626,#38627,#38628,#38629,#38630,#38631,#38632,#38633,#38634,
#38635,#38636,#38637,#38638,#38639,#38640,#38641,#38642,#38643,#38644,#38645,
#38646,#38647,#38648,#38649,#38650,#38651,#38652,#38653,#38654,#38655,#38656,
#38657,#38658,#38659,#38660,#38661,#38662,#38663,#38664,#38665,#38666,#38667,
#38668),.UNSPECIFIED.,.F.,.F.,(4,3,3,3,3,3,3,3,3,3,3,3,3,3,3,3,3,3,3,3,
3,3,3,3,3,3,3,3,3,3,3,3,3,3,3,3,3,3,3,3,3,3,3,3,3,3,3,3,3,3,3,3,3,3,3,3,
3,3,3,3,3,3,3,3,4),(-73.2066084493534,-73.0947351858594,-72.9823558650838,
-72.8693592293596,-72.8333529389755,-72.733657159283,-72.634104336361,-72.5342957662444,
-72.4349220385372,-72.3355811217742,-72.2362425721041,-72.136090872935,
-72.0366078952139,-71.9361218353209,-71.8356357754279,-71.7359399957353,
-71.6363871728129,-71.5365786026964,-71.437204874989,-71.3378639582259,
-71.2385254085555,-71.1383737093867,-71.0388907316655,-70.9384046717729,
-70.8379186118803,-70.7382228321877,-70.6386700092655,-70.5388614391489,
-70.4394877114416,-70.3401467946786,-70.2408082450082,-70.1406565458394,
-70.0411735681182,-69.9406875082255,-69.8402014483327,-69.7405056686401,
-69.6409528457178,-69.5411442756012,-69.4417705478939,-69.3424296311308,
-69.2430910814604,-69.1429393822916,-69.0434564045704,-68.9429703446778,
-68.8424842847851,-68.7427885050925,-68.6432356821703,-68.5434271120537,
-68.4440533843464,-68.3447124675833,-68.245373917913,-68.1452222187441,
-68.045739241023,-67.9452531811302,-67.8447671212375,-67.7461212768715,
-67.6432840100895,-67.5448962910023,-67.4465673157563,-67.3482653708917,
-67.2499587801198,-67.151559441021,-67.0531052122828,-66.9545027531578,
-66.923423142615),.UNSPECIFIED.);
#522=B_SPLINE_CURVE_WITH_KNOTS('',3,(#38670,#38671,#38672,#38673,#38674,
#38675,#38676,#38677,#38678,#38679,#38680,#38681,#38682,#38683,#38684,#38685,
#38686,#38687,#38688,#38689,#38690,#38691,#38692,#38693,#38694,#38695,#38696,
#38697,#38698,#38699,#38700,#38701,#38702,#38703,#38704,#38705,#38706,#38707,
#38708,#38709,#38710,#38711,#38712,#38713,#38714,#38715,#38716,#38717,#38718,
#38719,#38720,#38721,#38722,#38723,#38724,#38725,#38726,#38727,#38728,#38729,
#38730,#38731,#38732,#38733,#38734,#38735,#38736,#38737,#38738,#38739,#38740,
#38741,#38742,#38743,#38744,#38745,#38746,#38747,#38748,#38749,#38750,#38751,
#38752,#38753,#38754,#38755,#38756,#38757,#38758,#38759,#38760,#38761,#38762,
#38763,#38764,#38765,#38766,#38767,#38768,#38769,#38770,#38771,#38772,#38773,
#38774,#38775,#38776,#38777,#38778,#38779,#38780,#38781,#38782,#38783,#38784,
#38785,#38786,#38787,#38788,#38789,#38790,#38791,#38792,#38793,#38794,#38795,
#38796,#38797,#38798,#38799,#38800,#38801,#38802,#38803,#38804,#38805,#38806,
#38807,#38808,#38809,#38810,#38811,#38812,#38813,#38814,#38815,#38816,#38817,
#38818,#38819,#38820,#38821,#38822,#38823,#38824,#38825,#38826,#38827,#38828,
#38829,#38830,#38831,#38832,#38833,#38834,#38835,#38836,#38837,#38838,#38839,
#38840,#38841,#38842,#38843,#38844,#38845,#38846,#38847,#38848,#38849,#38850,
#38851,#38852,#38853,#38854,#38855,#38856,#38857,#38858,#38859),
 .UNSPECIFIED.,.F.,.F.,(4,3,3,3,3,3,3,3,3,3,3,3,3,3,3,3,3,3,3,3,3,3,3,3,
3,3,3,3,3,3,3,3,3,3,3,3,3,3,3,3,3,3,3,3,3,3,3,3,3,3,3,3,3,3,3,3,3,3,3,3,
3,3,3,4),(-66.9234231424034,-66.8470499576899,-66.7473541779973,-66.647801355075,
-66.5479927849585,-66.4486190572512,-66.3492781404881,-66.2499395908178,
-66.1497878916489,-66.0503049139278,-65.949818854035,-65.8493327941423,
-65.7496370144496,-65.6500841915273,-65.5502756214107,-65.4509018937034,
-65.3515609769403,-65.25222242727,-65.1520707281011,-65.0525877503799,-64.9521016904873,
-64.8516156305946,-64.751919850902,-64.6523670279797,-64.5525584578631,
-64.4531847301558,-64.3538438133927,-64.2545052637224,-64.1543535645535,
-64.0548705868324,-63.9543845269397,-63.853898467047,-63.7542026873544,
-63.6546498644322,-63.5548412943156,-63.4554675666083,-63.3561266498452,
-63.2567881001749,-63.156636401006,-63.0571534232849,-62.9566673633921,
-62.8561813034994,-62.7564855238068,-62.6569327008845,-62.5571241307679,
-62.4577504030606,-62.3584094862975,-62.2590709366272,-62.1589192374583,
-62.0594362597372,-61.9589501998445,-61.8584641399518,-61.7587683602592,
-61.6592155373369,-61.5594069672203,-61.4600332395129,-61.3606923227499,
-61.2613537730796,-61.1612020739108,-61.0617190961896,-60.9612330362969,
-60.8607469764042,-60.7246295825628,-60.6402378352238),.UNSPECIFIED.);
#523=B_SPLINE_CURVE_WITH_KNOTS('',3,(#38861,#38862,#38863,#38864,#38865,
#38866,#38867,#38868,#38869,#38870,#38871,#38872,#38873,#38874,#38875,#38876,
#38877,#38878,#38879,#38880,#38881,#38882,#38883,#38884,#38885,#38886,#38887,
#38888,#38889,#38890,#38891,#38892,#38893,#38894,#38895,#38896,#38897,#38898,
#38899,#38900,#38901,#38902,#38903,#38904,#38905,#38906,#38907,#38908,#38909,
#38910,#38911,#38912,#38913,#38914,#38915,#38916,#38917,#38918,#38919,#38920,
#38921,#38922,#38923,#38924,#38925,#38926,#38927,#38928,#38929,#38930,#38931,
#38932,#38933,#38934,#38935,#38936,#38937,#38938,#38939,#38940,#38941,#38942,
#38943,#38944,#38945,#38946,#38947,#38948,#38949,#38950,#38951,#38952,#38953,
#38954,#38955,#38956,#38957,#38958,#38959,#38960,#38961,#38962,#38963,#38964,
#38965,#38966,#38967,#38968,#38969,#38970,#38971,#38972,#38973,#38974,#38975,
#38976,#38977,#38978,#38979,#38980,#38981,#38982,#38983,#38984,#38985,#38986,
#38987,#38988,#38989,#38990,#38991,#38992,#38993,#38994,#38995,#38996,#38997,
#38998,#38999,#39000,#39001,#39002,#39003,#39004,#39005,#39006,#39007,#39008,
#39009,#39010,#39011,#39012,#39013,#39014,#39015,#39016,#39017,#39018,#39019,
#39020,#39021,#39022,#39023,#39024,#39025,#39026,#39027,#39028,#39029,#39030,
#39031,#39032,#39033,#39034,#39035,#39036,#39037,#39038,#39039,#39040,#39041,
#39042,#39043,#39044,#39045,#39046,#39047,#39048,#39049,#39050),
 .UNSPECIFIED.,.F.,.F.,(4,3,3,3,3,3,3,3,3,3,3,3,3,3,3,3,3,3,3,3,3,3,3,3,
3,3,3,3,3,3,3,3,3,3,3,3,3,3,3,3,3,3,3,3,3,3,3,3,3,3,3,3,3,3,3,3,3,3,3,3,
3,3,3,4),(-60.6402378349658,-60.5421067500117,-60.4440484045844,-60.3460307800577,
-60.2480219114026,-60.1499231427379,-60.0517813064526,-59.9534650966384,
-59.8630298128566,-59.763334033164,-59.6637812102418,-59.5639726401252,
-59.4645989124179,-59.3652579956548,-59.2659194459845,-59.1657677468156,
-59.0662847690945,-58.9657987092017,-58.865312649309,-58.7656168696164,
-58.6660640466941,-58.5662554765775,-58.4668817488702,-58.3675408321072,
-58.2682022824368,-58.1680505832679,-58.0685676055468,-57.9680815456541,
-57.8675954857614,-57.7678997060687,-57.6683468831465,-57.5685383130299,
-57.4691645853226,-57.3698236685596,-57.2704851188893,-57.1703334197204,
-57.0708504419992,-56.9703643821065,-56.8698783222138,-56.7701825425212,
-56.6706297195989,-56.5708211494823,-56.4714474217751,-56.3721065050121,
-56.2727679553418,-56.1726162561729,-56.0731332784519,-55.9726472185591,
-55.8721611586662,-55.7724653789736,-55.6729125560515,-55.5731039859349,
-55.4737302582276,-55.3743893414644,-55.2750507917943,-55.1748990926253,
-55.0754161149041,-54.9749300550113,-54.8744439951185,-54.7704583063323,
-54.6667439665697,-54.5631892926208,-54.4598284734441,-54.3570525280442),
 .UNSPECIFIED.);
#524=B_SPLINE_CURVE_WITH_KNOTS('',3,(#39052,#39053,#39054,#39055,#39056,
#39057,#39058,#39059,#39060,#39061,#39062,#39063,#39064,#39065,#39066,#39067,
#39068,#39069,#39070,#39071,#39072,#39073,#39074,#39075,#39076,#39077,#39078,
#39079,#39080,#39081,#39082,#39083,#39084,#39085,#39086,#39087,#39088,#39089,
#39090,#39091,#39092,#39093,#39094,#39095,#39096,#39097,#39098,#39099,#39100,
#39101,#39102,#39103,#39104,#39105,#39106,#39107,#39108,#39109,#39110,#39111,
#39112,#39113,#39114,#39115,#39116,#39117,#39118,#39119,#39120,#39121,#39122,
#39123,#39124,#39125,#39126,#39127,#39128,#39129,#39130,#39131,#39132,#39133,
#39134,#39135,#39136,#39137,#39138,#39139,#39140,#39141,#39142,#39143,#39144,
#39145,#39146,#39147,#39148,#39149,#39150,#39151,#39152,#39153,#39154,#39155,
#39156,#39157,#39158,#39159,#39160,#39161,#39162,#39163,#39164,#39165,#39166,
#39167,#39168,#39169,#39170,#39171,#39172,#39173,#39174,#39175,#39176,#39177,
#39178,#39179,#39180,#39181,#39182,#39183,#39184,#39185,#39186,#39187,#39188,
#39189,#39190,#39191,#39192,#39193,#39194,#39195,#39196,#39197,#39198,#39199,
#39200,#39201,#39202,#39203,#39204,#39205,#39206,#39207,#39208,#39209,#39210,
#39211,#39212,#39213,#39214,#39215,#39216,#39217,#39218,#39219,#39220,#39221,
#39222,#39223,#39224,#39225,#39226,#39227,#39228,#39229,#39230,#39231,#39232,
#39233,#39234,#39235,#39236,#39237,#39238,#39239,#39240,#39241,#39242,#39243,
#39244),.UNSPECIFIED.,.F.,.F.,(4,3,3,3,3,3,3,3,3,3,3,3,3,3,3,3,3,3,3,3,
3,3,3,3,3,3,3,3,3,3,3,3,3,3,3,3,3,3,3,3,3,3,3,3,3,3,3,3,3,3,3,3,3,3,3,3,
3,3,3,3,3,3,3,3,4),(-54.3570525276504,-54.2521726206048,-54.1469650788617,
-54.0415854281849,-53.9359076806462,-53.8767268315709,-53.7770310518783,
-53.6774782289559,-53.5776696588393,-53.4782959311319,-53.3789550143688,
-53.2796164646985,-53.1794647655297,-53.0799817878085,-52.9794957279159,
-52.8790096680233,-52.7793138883307,-52.6797610654085,-52.5799524952919,
-52.4805787675846,-52.3812378508216,-52.2818993011513,-52.1817476019824,
-52.0822646242613,-51.9817785643685,-51.8812925044757,-51.7815967247831,
-51.6820439018608,-51.5822353317442,-51.4828616040369,-51.3835206872739,
-51.2841821376035,-51.1840304384347,-51.0845474607135,-50.9840614008208,
-50.8835753409281,-50.7838795612355,-50.6843267383132,-50.5845181681966,
-50.4851444404893,-50.3858035237262,-50.2864649740559,-50.1863132748871,
-50.0868302971659,-49.9863442372732,-49.8858581773805,-49.7861623976879,
-49.6866095747656,-49.5868010046491,-49.4874272769417,-49.3880863601787,
-49.2887478105084,-49.1885961113395,-49.0891131336184,-48.9886270737257,
-48.8881410138329,-48.7863567897428,-48.6883018854676,-48.5903387778308,
-48.4924352823033,-48.3945592942371,-48.2966378664563,-48.1986884936107,
-48.1006313286397,-48.0738672211117),.UNSPECIFIED.);
#525=B_SPLINE_CURVE_WITH_KNOTS('',3,(#39246,#39247,#39248,#39249,#39250,
#39251,#39252,#39253,#39254,#39255,#39256,#39257,#39258,#39259,#39260,#39261,
#39262,#39263,#39264,#39265,#39266,#39267,#39268,#39269,#39270,#39271,#39272,
#39273,#39274,#39275,#39276,#39277,#39278,#39279,#39280,#39281,#39282,#39283,
#39284,#39285,#39286,#39287,#39288,#39289,#39290,#39291,#39292,#39293,#39294,
#39295,#39296,#39297,#39298,#39299,#39300,#39301,#39302,#39303,#39304,#39305,
#39306,#39307,#39308,#39309,#39310,#39311,#39312,#39313,#39314,#39315,#39316,
#39317,#39318,#39319,#39320,#39321,#39322,#39323,#39324,#39325,#39326,#39327,
#39328,#39329,#39330,#39331,#39332,#39333,#39334,#39335,#39336,#39337,#39338,
#39339,#39340,#39341,#39342,#39343,#39344,#39345,#39346,#39347,#39348,#39349,
#39350,#39351,#39352,#39353,#39354,#39355,#39356,#39357,#39358,#39359,#39360,
#39361,#39362,#39363,#39364,#39365,#39366,#39367,#39368,#39369,#39370,#39371,
#39372,#39373,#39374,#39375,#39376,#39377,#39378,#39379,#39380,#39381,#39382,
#39383,#39384,#39385,#39386,#39387,#39388,#39389,#39390,#39391,#39392,#39393,
#39394,#39395,#39396,#39397,#39398,#39399,#39400,#39401,#39402,#39403,#39404,
#39405,#39406,#39407,#39408,#39409,#39410,#39411,#39412,#39413,#39414,#39415,
#39416,#39417,#39418,#39419,#39420,#39421,#39422,#39423,#39424,#39425,#39426,
#39427,#39428,#39429,#39430,#39431,#39432,#39433,#39434,#39435),
 .UNSPECIFIED.,.F.,.F.,(4,3,3,3,3,3,3,3,3,3,3,3,3,3,3,3,3,3,3,3,3,3,3,3,
3,3,3,3,3,3,3,3,3,3,3,3,3,3,3,3,3,3,3,3,3,3,3,3,3,3,3,3,3,3,3,3,3,3,3,3,
3,3,3,4),(-48.0738672208646,-47.9246215794861,-47.8904238502853,-47.790728070593,
-47.6911752476712,-47.5913666775545,-47.4919929498476,-47.3926520330849,
-47.2933134834149,-47.1931617842456,-47.0936788065248,-46.9931927466313,
-46.8927066867377,-46.7930109070449,-46.6934580841225,-46.5936495140059,
-46.4942757862985,-46.3949348695353,-46.2955963198648,-46.1954446206961,
-46.0959616429748,-45.9954755830824,-45.89498952319,-45.7952937434974,-45.6957409205751,
-45.5959323504585,-45.4965586227512,-45.3972177059881,-45.2978791563177,
-45.1977274571489,-45.0982444794277,-44.9977584195351,-44.8972723596424,
-44.7975765799498,-44.6980237570276,-44.598215186911,-44.4988414592038,
-44.3995005424408,-44.3001619927705,-44.2000102936016,-44.1005273158805,
-44.0000412559877,-43.8995551960948,-43.7998594164022,-43.7003065934799,
-43.6004980233633,-43.501124295656,-43.4017833788929,-43.3024448292225,
-43.2022931300537,-43.1028101523325,-43.0023240924398,-42.9018380325472,
-42.8021422528546,-42.7025894299324,-42.6027808598158,-42.5034071321085,
-42.4040662153454,-42.304727665675,-42.2045759665062,-42.105092988785,-42.0046069288923,
-41.9041208689996,-41.790681913685),.UNSPECIFIED.);
#526=B_SPLINE_CURVE_WITH_KNOTS('',3,(#39437,#39438,#39439,#39440,#39441,
#39442,#39443,#39444,#39445,#39446,#39447,#39448,#39449,#39450,#39451,#39452,
#39453,#39454,#39455,#39456,#39457,#39458,#39459,#39460,#39461,#39462,#39463,
#39464,#39465,#39466,#39467,#39468,#39469,#39470,#39471,#39472,#39473,#39474,
#39475,#39476,#39477,#39478,#39479,#39480,#39481,#39482,#39483,#39484,#39485,
#39486,#39487,#39488,#39489,#39490,#39491,#39492,#39493,#39494,#39495,#39496,
#39497,#39498,#39499,#39500,#39501,#39502,#39503,#39504,#39505,#39506,#39507,
#39508,#39509,#39510,#39511,#39512,#39513,#39514,#39515,#39516,#39517,#39518,
#39519,#39520,#39521,#39522,#39523,#39524,#39525,#39526,#39527,#39528,#39529,
#39530,#39531,#39532,#39533,#39534,#39535,#39536,#39537,#39538,#39539,#39540,
#39541,#39542,#39543,#39544,#39545,#39546,#39547,#39548,#39549,#39550,#39551,
#39552,#39553,#39554,#39555,#39556,#39557,#39558,#39559,#39560,#39561,#39562,
#39563,#39564,#39565,#39566,#39567,#39568,#39569,#39570,#39571,#39572,#39573,
#39574,#39575,#39576,#39577,#39578,#39579,#39580,#39581,#39582,#39583,#39584,
#39585,#39586,#39587,#39588,#39589,#39590,#39591,#39592,#39593,#39594,#39595,
#39596,#39597,#39598,#39599,#39600,#39601,#39602,#39603,#39604,#39605,#39606,
#39607,#39608,#39609,#39610,#39611,#39612,#39613,#39614,#39615,#39616,#39617,
#39618,#39619,#39620,#39621,#39622,#39623,#39624,#39625,#39626),
 .UNSPECIFIED.,.F.,.F.,(4,3,3,3,3,3,3,3,3,3,3,3,3,3,3,3,3,3,3,3,3,3,3,3,
3,3,3,3,3,3,3,3,3,3,3,3,3,3,3,3,3,3,3,3,3,3,3,3,3,3,3,3,3,3,3,3,3,3,3,3,
3,3,3,4),(-41.790681913461,-41.692389330571,-41.5941411274311,-41.4960606609849,
-41.3980237415933,-41.299998413901,-41.2015997367888,-41.1034458577189,
-41.0049247815855,-40.906403705452,-40.8067079257594,-40.7071551028373,
-40.6073465327207,-40.5079728050133,-40.4086318882502,-40.3092933385798,
-40.209141639411,-40.1096586616898,-40.0091726017971,-39.9086865419044,
-39.8089907622117,-39.7094379392893,-39.6096293691727,-39.5102556414654,
-39.4109147247024,-39.3115761750321,-39.2114244758632,-39.1119414981421,
-39.0114554382495,-38.9109693783568,-38.8112735986641,-38.7117207757417,
-38.6119122056251,-38.5125384779178,-38.4131975611546,-38.3138590114842,
-38.2137073123155,-38.1142243345942,-38.0137382747017,-37.9132522148092,
-37.8135564351165,-37.714003612194,-37.6141950420775,-37.5148213143702,
-37.4154803976071,-37.3161418479371,-37.2159901487682,-37.116507171047,
-37.0160211111543,-36.9155350512616,-36.8158392715691,-36.716286448647,
-36.6164778785303,-36.5171041508231,-36.41776323406,-36.3184246843897,-36.2182729852208,
-36.1187900074996,-36.0183039476068,-35.917817887714,-35.8079248438542,
-35.6983489447371,-35.5893126975054,-35.5074966068976),.UNSPECIFIED.);
#527=B_SPLINE_CURVE_WITH_KNOTS('',3,(#39628,#39629,#39630,#39631,#39632,
#39633,#39634,#39635,#39636,#39637,#39638,#39639,#39640,#39641,#39642,#39643,
#39644,#39645,#39646,#39647,#39648,#39649,#39650,#39651,#39652,#39653,#39654,
#39655,#39656,#39657,#39658,#39659,#39660,#39661,#39662,#39663,#39664,#39665,
#39666,#39667,#39668,#39669,#39670,#39671,#39672,#39673,#39674,#39675,#39676,
#39677,#39678,#39679,#39680,#39681,#39682,#39683,#39684,#39685,#39686,#39687,
#39688,#39689,#39690,#39691,#39692,#39693,#39694,#39695,#39696,#39697,#39698,
#39699,#39700,#39701,#39702,#39703,#39704,#39705,#39706,#39707,#39708,#39709,
#39710,#39711,#39712,#39713,#39714,#39715,#39716,#39717,#39718,#39719,#39720,
#39721,#39722,#39723,#39724,#39725,#39726,#39727,#39728,#39729,#39730,#39731,
#39732,#39733,#39734,#39735,#39736,#39737,#39738,#39739,#39740,#39741,#39742,
#39743,#39744,#39745,#39746,#39747,#39748,#39749,#39750,#39751,#39752,#39753,
#39754,#39755,#39756,#39757,#39758,#39759,#39760,#39761,#39762,#39763,#39764,
#39765,#39766,#39767,#39768,#39769,#39770,#39771,#39772,#39773,#39774,#39775,
#39776,#39777,#39778,#39779,#39780,#39781,#39782,#39783,#39784,#39785,#39786,
#39787,#39788,#39789,#39790,#39791,#39792,#39793,#39794,#39795,#39796,#39797,
#39798,#39799,#39800,#39801,#39802,#39803,#39804,#39805,#39806,#39807,#39808,
#39809,#39810,#39811,#39812,#39813,#39814,#39815,#39816,#39817,#39818,#39819,
#39820),.UNSPECIFIED.,.F.,.F.,(4,3,3,3,3,3,3,3,3,3,3,3,3,3,3,3,3,3,3,3,
3,3,3,3,3,3,3,3,3,3,3,3,3,3,3,3,3,3,3,3,3,3,3,3,3,3,3,3,3,3,3,3,3,3,3,3,
3,3,3,3,3,3,3,3,4),(-35.5074966065054,-35.4065248779729,-35.305509076606,
-35.2043396116514,-35.1030905086744,-35.001630744129,-34.9201007241663,
-34.8204049444737,-34.7208521215515,-34.6210435514349,-34.5216698237276,
-34.4223289069646,-34.3229903572942,-34.2228386581253,-34.1233556804042,
-34.0228696205115,-33.9223835606187,-33.8226877809265,-33.7231349580045,
-33.6233263878879,-33.5239526601809,-33.4246117434182,-33.3252731937481,
-33.2251214945789,-33.1256385168581,-33.0251524569646,-32.9246663970711,
-32.8249706173775,-32.7254177944543,-32.625609224338,-32.5262354966298,
-32.4268945798657,-32.3275560301946,-32.2274043310268,-32.1279213533048,
-32.0274352934141,-31.9269492335235,-31.8272534538316,-31.7277006309103,
-31.6278920607935,-31.528518333087,-31.4291774163247,-31.3298388666551,
-31.2296871674853,-31.1302041897648,-31.0297181298704,-30.9292320699759,
-30.829536290285,-30.7299834673647,-30.6301748972477,-30.530801169542,-30.4314602527805,
-30.332121703112,-30.2319700039411,-30.1324870262215,-30.0320009663249,
-29.9315149064283,-29.8325486555065,-29.7337156387982,-29.6349843102171,
-29.5323160574943,-29.4336769479537,-29.3350464532442,-29.2363682515395,
-29.2243112993258),.UNSPECIFIED.);
#528=B_SPLINE_CURVE_WITH_KNOTS('',3,(#39822,#39823,#39824,#39825,#39826,
#39827,#39828,#39829,#39830,#39831,#39832,#39833,#39834,#39835,#39836,#39837,
#39838,#39839,#39840,#39841,#39842,#39843,#39844,#39845,#39846,#39847,#39848,
#39849,#39850,#39851,#39852,#39853,#39854,#39855,#39856,#39857,#39858,#39859,
#39860,#39861,#39862,#39863,#39864,#39865,#39866,#39867,#39868,#39869,#39870,
#39871,#39872,#39873,#39874,#39875,#39876,#39877,#39878,#39879,#39880,#39881,
#39882,#39883,#39884,#39885,#39886,#39887,#39888,#39889,#39890,#39891,#39892,
#39893,#39894,#39895,#39896,#39897,#39898,#39899,#39900,#39901,#39902,#39903,
#39904,#39905,#39906,#39907,#39908,#39909,#39910,#39911,#39912,#39913,#39914,
#39915,#39916,#39917,#39918,#39919,#39920,#39921,#39922,#39923,#39924,#39925,
#39926,#39927,#39928,#39929,#39930,#39931,#39932,#39933,#39934,#39935,#39936,
#39937,#39938,#39939,#39940,#39941,#39942,#39943,#39944,#39945,#39946,#39947,
#39948,#39949,#39950,#39951,#39952,#39953,#39954,#39955,#39956,#39957,#39958,
#39959,#39960,#39961,#39962,#39963,#39964,#39965,#39966,#39967,#39968,#39969,
#39970,#39971,#39972,#39973,#39974,#39975,#39976,#39977,#39978,#39979,#39980,
#39981,#39982,#39983,#39984,#39985,#39986,#39987,#39988,#39989,#39990,#39991,
#39992,#39993,#39994,#39995,#39996,#39997,#39998,#39999,#40000,#40001,#40002,
#40003,#40004,#40005,#40006,#40007,#40008,#40009,#40010,#40011,#40012,#40013,
#40014),.UNSPECIFIED.,.F.,.F.,(4,3,3,3,3,3,3,3,3,3,3,3,3,3,3,3,3,3,3,3,
3,3,3,3,3,3,3,3,3,3,3,3,3,3,3,3,3,3,3,3,3,3,3,3,3,3,3,3,3,3,3,3,3,3,3,3,
3,3,3,3,3,3,3,3,4),(-29.2243112990236,-29.103492898179,-28.9808497567486,
-28.9337977428807,-28.8341019631958,-28.7345491402811,-28.6347405701626,
-28.5353668424629,-28.4360259257073,-28.3366873760444,-28.2365356768666,
-28.1370526991525,-28.0365666392428,-27.9360805793331,-27.8363847996496,
-27.7368319767364,-27.6370234066176,-27.5376496789196,-27.438308762166,
-27.3389702125051,-27.2388185133252,-27.1393355356136,-27.0388494756995,
-26.9383634157855,-26.8386676360441,-26.7391148130729,-26.6393062429686,
-26.5399325152125,-26.4405915984007,-26.3412530486819,-26.2411013495709,
-26.1416183718023,-26.0411323120201,-25.9406462522379,-25.8409504726143,
-25.7413976497608,-25.641589079627,-25.5422153519875,-25.4428744352918,
-25.3435358856882,-25.2433841864387,-25.1439012087821,-25.0434151487361,
-24.9429290886902,-24.8432333090377,-24.7436804861565,-24.6438719160297,
-24.5444981883652,-24.4451572716455,-24.345818722019,-24.2456670227999,
-24.1461840451234,-24.045697985133,-23.9452119251426,-23.8455161451008,
-23.7459633218283,-23.6461547517991,-23.5467810237416,-23.447440106629,
-23.3481015566104,-23.2479498578566,-23.1484668797938,-23.0479808206944,
-22.947494761595,-22.9411259921462),.UNSPECIFIED.);
#529=B_SPLINE_CURVE_WITH_KNOTS('',3,(#40016,#40017,#40018,#40019,#40020,
#40021,#40022,#40023,#40024,#40025,#40026,#40027,#40028,#40029,#40030,#40031,
#40032,#40033,#40034,#40035,#40036,#40037,#40038,#40039,#40040,#40041,#40042,
#40043,#40044,#40045,#40046,#40047,#40048,#40049,#40050,#40051,#40052,#40053,
#40054,#40055,#40056,#40057,#40058,#40059,#40060,#40061,#40062,#40063,#40064,
#40065,#40066,#40067,#40068,#40069,#40070,#40071,#40072,#40073,#40074,#40075,
#40076,#40077,#40078,#40079,#40080,#40081,#40082,#40083,#40084,#40085,#40086,
#40087,#40088,#40089,#40090,#40091,#40092,#40093,#40094,#40095,#40096,#40097,
#40098,#40099,#40100,#40101,#40102,#40103,#40104,#40105,#40106,#40107,#40108,
#40109,#40110,#40111,#40112,#40113,#40114,#40115,#40116,#40117,#40118,#40119,
#40120,#40121,#40122,#40123,#40124,#40125,#40126,#40127,#40128,#40129,#40130,
#40131,#40132,#40133,#40134,#40135,#40136,#40137,#40138,#40139,#40140,#40141,
#40142,#40143,#40144,#40145,#40146,#40147,#40148,#40149,#40150,#40151,#40152,
#40153,#40154,#40155,#40156,#40157,#40158,#40159,#40160,#40161,#40162,#40163,
#40164,#40165,#40166,#40167,#40168,#40169,#40170,#40171,#40172,#40173,#40174,
#40175,#40176,#40177,#40178,#40179,#40180,#40181,#40182,#40183,#40184,#40185,
#40186,#40187,#40188,#40189,#40190,#40191,#40192,#40193,#40194,#40195,#40196,
#40197,#40198,#40199,#40200,#40201,#40202,#40203,#40204,#40205),
 .UNSPECIFIED.,.F.,.F.,(4,3,3,3,3,3,3,3,3,3,3,3,3,3,3,3,3,3,3,3,3,3,3,3,
3,3,3,3,3,3,3,3,3,3,3,3,3,3,3,3,3,3,3,3,3,3,3,3,3,3,3,3,3,3,3,3,3,3,3,3,
3,3,3,4),(-22.9411259917746,-22.8415435429852,-22.7421039011161,-22.6427792851694,
-22.5435176208825,-22.4442882702793,-22.3450606352053,-22.2457348632547,
-22.1463622498412,-22.0468091209728,-21.9497775980474,-21.850081818445,
-21.7505289956196,-21.6507204254796,-21.5513466978833,-21.4520057812365,
-21.3526672316874,-21.2525155323905,-21.1530325548013,-21.0525464946505,
-20.9520604344998,-20.8523646523694,-20.7528118270002,-20.6530032574942,
-20.5536295273353,-20.4542886081243,-20.3549500560131,-20.2547983597479,
-20.1553153796278,-20.05482932529,-19.9543432709522,-19.8546474960847,-19.7550946779828,
-19.6552861066605,-19.5559123837282,-19.4565714717126,-19.3572329267559,
-19.2570812219181,-19.1575982487803,-19.0571121780925,-18.9566261074046,
-18.8569303268034,-18.7573775030175,-18.6575689331224,-18.5581952046655,
-18.4588542871971,-18.3595157368665,-18.2593640386141,-18.1598810603482,
-18.0593950021026,-17.958908943857,-17.8592131476343,-17.759660308104,-17.6598517421297,
-17.560477997747,-17.4611370643201,-17.3617984980203,-17.2616468185926,
-17.1621638244946,-17.061677802402,-16.9611917803094,-16.8403231294146,
-16.7210048959573,-16.6579408702691),.UNSPECIFIED.);
#530=B_SPLINE_CURVE_WITH_KNOTS('',3,(#40207,#40208,#40209,#40210,#40211,
#40212,#40213,#40214,#40215,#40216),.UNSPECIFIED.,.F.,.F.,(4,1,1,1,1,1,
1,4),(-16.6579406849666,-15.9634746167618,-14.9657574532142,-13.9680402896665,
-12.9703231261189,-11.9726059625713,-10.9748887990237,-10.374755377787),
 .UNSPECIFIED.);
#531=B_SPLINE_CURVE_WITH_KNOTS('',3,(#40217,#40218,#40219,#40220,#40221,
#40222,#40223,#40224,#40225,#40226,#40227,#40228,#40229,#40230,#40231,#40232,
#40233,#40234,#40235,#40236,#40237,#40238,#40239,#40240,#40241,#40242,#40243,
#40244,#40245,#40246,#40247,#40248,#40249,#40250,#40251,#40252,#40253,#40254,
#40255,#40256,#40257,#40258,#40259,#40260,#40261,#40262,#40263,#40264,#40265,
#40266,#40267,#40268,#40269,#40270,#40271,#40272,#40273,#40274,#40275,#40276,
#40277,#40278,#40279,#40280,#40281,#40282,#40283,#40284,#40285,#40286,#40287,
#40288,#40289,#40290,#40291,#40292,#40293,#40294,#40295,#40296,#40297,#40298,
#40299,#40300,#40301,#40302,#40303,#40304,#40305,#40306,#40307,#40308,#40309,
#40310,#40311,#40312,#40313,#40314,#40315,#40316,#40317,#40318,#40319,#40320,
#40321,#40322,#40323,#40324,#40325,#40326,#40327,#40328,#40329,#40330,#40331,
#40332,#40333,#40334,#40335,#40336,#40337,#40338,#40339,#40340,#40341,#40342,
#40343,#40344,#40345,#40346,#40347,#40348,#40349,#40350,#40351,#40352,#40353,
#40354,#40355,#40356,#40357,#40358,#40359,#40360,#40361,#40362,#40363,#40364,
#40365,#40366,#40367,#40368,#40369,#40370,#40371,#40372,#40373,#40374,#40375,
#40376,#40377,#40378,#40379,#40380,#40381,#40382,#40383,#40384,#40385,#40386,
#40387,#40388,#40389,#40390,#40391,#40392,#40393,#40394,#40395,#40396,#40397,
#40398,#40399,#40400,#40401,#40402,#40403,#40404,#40405,#40406),
 .UNSPECIFIED.,.F.,.F.,(4,3,3,3,3,3,3,3,3,3,3,3,3,3,3,3,3,3,3,3,3,3,3,3,
3,3,3,3,3,3,3,3,3,3,3,3,3,3,3,3,3,3,3,3,3,3,3,3,3,3,3,3,3,3,3,3,3,3,3,3,
3,3,3,4),(-10.374755156708,-10.2647876514522,-10.1544297250587,-10.0435333536381,
-9.9771716354761,-9.8774735922054,-9.77791851937864,-9.67811051344737,-9.5787345848517,
-9.47939149034969,-9.38005078887961,-9.27990170964183,-9.18041666501551,
-9.079935568472,-8.97945447192849,-8.87975475068599,-8.78019794692404,-8.68039036710614,
-8.5810125929777,-8.48166761426253,-8.38232499271131,-8.2821780716287,-8.18269103968926,
-8.08221417403507,-7.98173730838088,-7.88205853932025,-7.78252275788716,
-7.68270993125542,-7.58335319660954,-7.48402921742459,-7.38470752738062,
-7.28453568174378,-7.18506920224763,-7.08454467354045,-6.98402014483327,
-6.88430333738403,-6.78472957127026,-6.68492624752219,-6.58553193070912,
-6.48617060257183,-6.38681184575184,-6.2866846296353,-6.18718214676953,
-6.08674256402759,-5.98630298128566,-5.88658666295721,-5.78701300292329,
-5.68720960477514,-5.58781447444025,-5.48845199143677,-5.38909174229588,
-5.28896526115642,-5.18946048386327,-5.08902315080066,-4.98858581773805,
-4.89025187082946,-4.79041664580171,-4.69233891542646,-4.59432039421673,
-4.49632908436476,-4.39513933092544,-4.29705324421013,-4.1943116574088,
-4.09157007060747),.UNSPECIFIED.);
#532=B_SPLINE_CURVE_WITH_KNOTS('',3,(#40409,#40410,#40411,#40412,#40413),
 .UNSPECIFIED.,.F.,.F.,(4,1,4),(158.568767222197,159.278533402388,160.221218674128),
 .UNSPECIFIED.);
#533=B_SPLINE_CURVE_WITH_KNOTS('',3,(#40415,#40416,#40417,#40418,#40419,
#40420,#40421,#40422,#40423,#40424,#40425,#40426,#40427,#40428,#40429,#40430,
#40431,#40432,#40433,#40434,#40435,#40436,#40437,#40438,#40439,#40440,#40441,
#40442,#40443,#40444,#40445,#40446,#40447,#40448,#40449,#40450,#40451,#40452,
#40453,#40454,#40455,#40456,#40457,#40458,#40459,#40460,#40461,#40462,#40463,
#40464,#40465,#40466,#40467,#40468,#40469,#40470,#40471,#40472,#40473,#40474,
#40475,#40476,#40477,#40478,#40479,#40480,#40481,#40482,#40483,#40484,#40485,
#40486,#40487,#40488,#40489,#40490,#40491,#40492,#40493,#40494,#40495,#40496,
#40497,#40498,#40499,#40500,#40501,#40502,#40503,#40504,#40505),
 .UNSPECIFIED.,.F.,.F.,(4,3,3,3,3,3,3,3,3,3,3,3,3,3,3,3,3,3,3,3,3,3,3,3,
3,3,3,3,3,3,4),(160.221225333079,160.276250565935,160.381079054541,160.485749756296,
160.590297379016,160.694779341089,160.799231394165,160.90368924618,161.008259430969,
161.112891606325,161.217708400402,161.273967729483,161.379121029899,161.484116312145,
161.588986618703,161.693789907966,161.798561461836,161.903336516804,162.008218273126,
162.113159280045,162.218277378404,162.271684893031,162.375628464312,162.479397941196,
162.583070245111,162.686682340639,162.790271110867,162.893943190511,162.997653572182,
163.101547205486,163.19821022681),.UNSPECIFIED.);
#534=B_SPLINE_CURVE_WITH_KNOTS('',3,(#40509,#40510,#40511,#40512,#40513,
#40514,#40515,#40516,#40517,#40518,#40519,#40520,#40521,#40522,#40523,#40524,
#40525,#40526,#40527,#40528,#40529,#40530,#40531,#40532,#40533,#40534,#40535,
#40536,#40537,#40538,#40539,#40540,#40541,#40542,#40543,#40544,#40545,#40546,
#40547,#40548,#40549,#40550,#40551,#40552,#40553,#40554,#40555,#40556,#40557,
#40558,#40559,#40560,#40561,#40562,#40563),.UNSPECIFIED.,.F.,.F.,(4,3,3,
3,3,3,3,3,3,3,3,3,3,3,3,3,3,3,4),(160.221225333079,160.323576356247,160.425868943639,
160.528141137588,160.6304309436,160.732846323553,160.835338090606,160.93801420435,
160.958883749947,161.066718047386,161.17795340565,161.285428499209,161.392801978492,
161.500102932275,161.607360355761,161.714633268257,161.821914162531,161.929269085492,
161.956600913495),.UNSPECIFIED.);
#535=B_SPLINE_CURVE_WITH_KNOTS('',3,(#40564,#40565,#40566,#40567,#40568,
#40569,#40570,#40571,#40572,#40573,#40574,#40575,#40576,#40577,#40578,#40579,
#40580,#40581,#40582,#40583,#40584,#40585,#40586,#40587,#40588,#40589,#40590,
#40591,#40592,#40593,#40594,#40595,#40596,#40597,#40598,#40599,#40600,#40601,
#40602,#40603,#40604,#40605,#40606,#40607,#40608,#40609,#40610,#40611,#40612),
 .UNSPECIFIED.,.F.,.F.,(4,3,3,3,3,3,3,3,3,3,3,3,3,3,3,3,4),(158.567664456021,
158.672535944769,158.777458396884,158.882566263536,158.963449422852,159.068511569472,
159.173418639729,159.278205451186,159.382928208473,159.487622287813,159.592323023176,
159.697135689129,159.8020104782,159.907067470358,159.961166586399,160.094360320626,
160.221225332746),.UNSPECIFIED.);
#536=B_SPLINE_CURVE_WITH_KNOTS('',3,(#40617,#40618,#40619,#40620,#40621,
#40622,#40623,#40624,#40625,#40626,#40627,#40628,#40629,#40630,#40631,#40632,
#40633,#40634,#40635,#40636,#40637,#40638,#40639,#40640,#40641,#40642,#40643,
#40644,#40645,#40646,#40647,#40648,#40649,#40650,#40651,#40652,#40653,#40654,
#40655,#40656,#40657,#40658,#40659,#40660,#40661,#40662,#40663,#40664,#40665,
#40666,#40667,#40668,#40669,#40670,#40671,#40672,#40673,#40674,#40675,#40676,
#40677,#40678,#40679,#40680,#40681,#40682,#40683,#40684,#40685,#40686,#40687,
#40688,#40689,#40690,#40691,#40692,#40693,#40694,#40695,#40696,#40697,#40698,
#40699,#40700,#40701,#40702,#40703,#40704),.UNSPECIFIED.,.F.,.F.,(4,3,3,
3,3,3,3,3,3,3,3,3,3,3,3,3,3,3,3,3,3,3,3,3,3,3,3,3,3,4),(-0.457078985060659,
-0.444385276561842,-0.418760344151197,-0.405811846153069,-0.39886744604032,
-0.394362276912132,-0.368978176374782,-0.349303253656113,-0.340015563076288,
-0.335861856280851,-0.331696484383836,-0.306965526627292,-0.282519434519426,
-0.258814906883348,-0.248499275797862,-0.244444801260351,-0.220954016702682,
-0.211584376181149,-0.187623099299552,-0.164170211887108,-0.158777333143535,
-0.135446414563357,-0.112194632335021,-0.0891371093918709,-0.0803323653505391,
-0.0766178985924528,-0.0541145820763493,-0.0322395508690489,-0.010671129319354,
0.),.UNSPECIFIED.);
#537=B_SPLINE_CURVE_WITH_KNOTS('',3,(#40705,#40706,#40707,#40708,#40709,
#40710,#40711,#40712,#40713,#40714,#40715,#40716,#40717,#40718,#40719,#40720,
#40721,#40722,#40723,#40724,#40725,#40726,#40727,#40728,#40729,#40730,#40731,
#40732,#40733,#40734,#40735,#40736,#40737,#40738,#40739,#40740,#40741,#40742,
#40743,#40744,#40745,#40746,#40747,#40748,#40749,#40750,#40751,#40752,#40753,
#40754,#40755,#40756,#40757,#40758,#40759,#40760,#40761,#40762,#40763,#40764,
#40765,#40766,#40767,#40768,#40769,#40770,#40771,#40772,#40773,#40774,#40775,
#40776,#40777,#40778,#40779,#40780,#40781,#40782,#40783,#40784,#40785,#40786,
#40787,#40788,#40789),.UNSPECIFIED.,.F.,.F.,(4,3,3,3,3,3,3,3,3,3,3,3,3,
3,3,3,3,3,3,3,3,3,3,3,3,3,3,3,4),(-0.463803050843693,-0.449398219400782,
-0.427690690340653,-0.415681595796131,-0.410727534513478,-0.405863614198107,
-0.383202928459213,-0.364728962044393,-0.357056800645003,-0.352630059545498,
-0.329188375163953,-0.305452986562277,-0.281845294580705,-0.274917746668043,
-0.270966521906024,-0.246538221694511,-0.235545177628289,-0.211713588834806,
-0.187882000041323,-0.183828909444003,-0.159579091238228,-0.134520943597755,
-0.109462795957281,-0.0941651274920544,-0.0900064894898221,-0.0642581539445237,
-0.0384830703539072,-0.01326410743577,0.),.UNSPECIFIED.);
#538=B_SPLINE_CURVE_WITH_KNOTS('',3,(#41419,#41420,#41421,#41422),
 .UNSPECIFIED.,.F.,.F.,(4,4),(-0.0473137948812196,0.),.UNSPECIFIED.);
#539=B_SPLINE_CURVE_WITH_KNOTS('',3,(#41424,#41425,#41426,#41427,#41428,
#41429,#41430,#41431,#41432,#41433,#41434,#41435,#41436,#41437,#41438,#41439,
#41440,#41441,#41442,#41443,#41444,#41445,#41446,#41447,#41448,#41449,#41450,
#41451,#41452,#41453,#41454,#41455,#41456,#41457,#41458,#41459,#41460,#41461,
#41462,#41463,#41464,#41465,#41466,#41467,#41468,#41469,#41470,#41471,#41472,
#41473,#41474,#41475,#41476,#41477,#41478,#41479,#41480,#41481,#41482,#41483,
#41484,#41485,#41486,#41487,#41488,#41489,#41490,#41491,#41492,#41493,#41494,
#41495,#41496,#41497,#41498,#41499,#41500,#41501,#41502,#41503,#41504,#41505,
#41506,#41507,#41508),.UNSPECIFIED.,.F.,.F.,(4,3,3,3,3,3,3,3,3,3,3,3,3,
3,3,3,3,3,3,3,3,3,3,3,3,3,3,3,4),(-0.463803050843679,-0.44939821940076,
-0.427589341418366,-0.415681597634893,-0.410727519266437,-0.405863611030377,
-0.38318378630743,-0.360186208150004,-0.357056795907073,-0.352630060245515,
-0.329269893234261,-0.305500004932649,-0.288041937515757,-0.274917747543885,
-0.270966522774074,-0.246538222518605,-0.23554517762827,-0.211959515268067,
-0.18788200185284,-0.183828910437428,-0.159579093158968,-0.134520946152716,
-0.109462799146463,-0.0941651345645707,-0.0900064900507649,-0.0642581550076631,
-0.0384830708873975,-0.0132641052952493,0.),.UNSPECIFIED.);
#540=B_SPLINE_CURVE_WITH_KNOTS('',3,(#41509,#41510,#41511,#41512),
 .UNSPECIFIED.,.F.,.F.,(4,4),(-0.0138026843193199,0.),.UNSPECIFIED.);
#541=B_SPLINE_CURVE_WITH_KNOTS('',3,(#41517,#41518,#41519,#41520,#41521,
#41522,#41523,#41524,#41525,#41526,#41527,#41528,#41529,#41530,#41531,#41532,
#41533,#41534,#41535,#41536,#41537,#41538,#41539,#41540,#41541,#41542,#41543,
#41544,#41545,#41546,#41547,#41548,#41549,#41550,#41551,#41552,#41553,#41554,
#41555,#41556,#41557,#41558,#41559,#41560,#41561,#41562,#41563,#41564,#41565,
#41566,#41567,#41568,#41569,#41570,#41571,#41572,#41573,#41574,#41575,#41576,
#41577,#41578,#41579,#41580,#41581,#41582,#41583,#41584,#41585,#41586,#41587,
#41588,#41589,#41590,#41591,#41592,#41593,#41594,#41595,#41596,#41597,#41598,
#41599,#41600,#41601,#41602,#41603,#41604),.UNSPECIFIED.,.F.,.F.,(4,3,3,
3,3,3,3,3,3,3,3,3,3,3,3,3,3,3,3,3,3,3,3,3,3,3,3,3,3,4),(-0.457078999239372,
-0.444385276561864,-0.418678196115324,-0.405811846078769,-0.398867444205902,
-0.394362273327402,-0.368978172738963,-0.349303250493666,-0.340015558281466,
-0.335861852484767,-0.331696483073541,-0.306947318623066,-0.2827283572022,
-0.259025657312411,-0.248499263812912,-0.244444801048436,-0.220954014795881,
-0.211584376181152,-0.18752381564345,-0.164170210903559,-0.158777333342259,
-0.135446414038975,-0.112194633282033,-0.0891371124572476,-0.0803323657407222,
-0.076617898847751,-0.0541145839112134,-0.0322395556953983,-0.0106711375989012,
0.),.UNSPECIFIED.);
#542=B_SPLINE_CURVE_WITH_KNOTS('',3,(#42234,#42235,#42236,#42237),
 .UNSPECIFIED.,.F.,.F.,(4,4),(-0.0475340594435537,0.),.UNSPECIFIED.);
#543=B_SPLINE_CURVE_WITH_KNOTS('',3,(#43212,#43213,#43214,#43215,#43216,
#43217,#43218,#43219,#43220,#43221,#43222,#43223,#43224,#43225,#43226,#43227,
#43228,#43229,#43230,#43231,#43232,#43233,#43234,#43235,#43236,#43237,#43238,
#43239,#43240,#43241,#43242,#43243,#43244,#43245,#43246,#43247,#43248,#43249,
#43250,#43251,#43252,#43253,#43254,#43255,#43256,#43257,#43258,#43259,#43260,
#43261,#43262,#43263,#43264,#43265,#43266,#43267,#43268,#43269,#43270,#43271,
#43272,#43273,#43274,#43275,#43276,#43277,#43278,#43279,#43280,#43281,#43282,
#43283,#43284,#43285,#43286,#43287,#43288,#43289,#43290,#43291,#43292,#43293,
#43294,#43295,#43296,#43297,#43298,#43299,#43300,#43301,#43302,#43303,#43304,
#43305,#43306,#43307,#43308,#43309,#43310,#43311,#43312,#43313,#43314,#43315,
#43316,#43317,#43318,#43319,#43320,#43321,#43322,#43323,#43324,#43325,#43326,
#43327,#43328,#43329,#43330,#43331,#43332,#43333,#43334,#43335,#43336,#43337,
#43338,#43339,#43340,#43341,#43342,#43343,#43344,#43345,#43346,#43347,#43348,
#43349,#43350,#43351,#43352,#43353,#43354,#43355,#43356,#43357,#43358,#43359,
#43360,#43361,#43362,#43363,#43364,#43365,#43366,#43367,#43368,#43369,#43370,
#43371,#43372,#43373,#43374,#43375,#43376,#43377,#43378,#43379,#43380,#43381,
#43382,#43383,#43384,#43385),.UNSPECIFIED.,.F.,.F.,(4,2,2,2,2,2,2,2,2,2,
2,2,2,2,2,2,2,2,2,2,2,2,2,2,2,2,2,2,2,2,2,2,2,2,2,2,2,2,2,2,2,2,2,2,2,2,
2,2,2,2,2,2,2,2,2,2,2,2,2,2,2,2,2,2,2,2,2,2,2,2,2,2,2,2,2,2,2,2,2,2,2,2,
2,2,2,2,4),(-1.02623154465591,-1.02612355094225,-1.0171949105878,-1.00173095718431,
-0.985469014925391,-0.982771946333453,-0.981106865955899,-0.979811649677182,
-0.978304805833221,-0.975593204166809,-0.962004888593598,-0.929009570235146,
-0.890102622931837,-0.885357205821845,-0.882392485048737,-0.88007255803002,
-0.87749442072948,-0.873218763358691,-0.856815386493199,-0.795998925748137,
-0.785774339547155,-0.783194740653446,-0.781700335240677,-0.780528775129861,
-0.778903222255259,-0.775642448166408,-0.771379179015789,-0.761149449011797,
-0.715168121526073,-0.690933730558083,-0.686443744461884,-0.683553504484392,
-0.681237215680206,-0.678604823233647,-0.674096245039031,-0.654637962169762,
-0.609759140741896,-0.587984786080504,-0.584837995230912,-0.583218043592144,
-0.581928744021515,-0.580398002638214,-0.577543750440399,-0.560583467376236,
-0.531668237094072,-0.491978203796283,-0.487259509009561,-0.48431303144165,
-0.482008603588994,-0.479449131679121,-0.475208298310883,-0.459005836096745,
-0.427573337459186,-0.416862164322599,-0.411468759639921,-0.388730249711721,
-0.385591832645818,-0.383978822110257,-0.382688106401478,-0.381143962853957,
-0.378268391996503,-0.361258822960958,-0.332370712217255,-0.292727546811052,
-0.287970926659497,-0.28499512806325,-0.282663948925388,-0.28007054667004,
-0.275762761562799,-0.259131125602471,-0.194877347651408,-0.187936721290845,
-0.185704718486579,-0.184300457443206,-0.182978277960871,-0.181156364600397,
-0.176843676191297,-0.156826183459693,-0.104384960191217,-0.0934748581158038,
-0.0896010514422441,-0.0873381573714681,-0.0849755616014679,-0.0818995433479831,
-0.0753249891341137,-0.0493613703757626,-0.00320473719929889),
 .UNSPECIFIED.);
#544=B_SPLINE_CURVE_WITH_KNOTS('',3,(#43388,#43389,#43390,#43391,#43392,
#43393,#43394,#43395,#43396,#43397,#43398,#43399,#43400,#43401,#43402,#43403,
#43404,#43405,#43406,#43407,#43408,#43409,#43410,#43411,#43412,#43413,#43414,
#43415,#43416,#43417,#43418,#43419,#43420,#43421,#43422,#43423,#43424,#43425,
#43426,#43427,#43428,#43429,#43430,#43431,#43432,#43433,#43434,#43435,#43436,
#43437,#43438,#43439,#43440,#43441,#43442,#43443,#43444,#43445,#43446,#43447,
#43448,#43449,#43450,#43451,#43452,#43453,#43454,#43455,#43456,#43457,#43458,
#43459,#43460,#43461,#43462,#43463,#43464,#43465,#43466,#43467,#43468,#43469,
#43470,#43471,#43472,#43473,#43474,#43475,#43476,#43477,#43478,#43479,#43480,
#43481,#43482,#43483,#43484,#43485,#43486,#43487,#43488,#43489,#43490,#43491,
#43492,#43493,#43494,#43495,#43496,#43497,#43498,#43499,#43500,#43501,#43502,
#43503,#43504,#43505),.UNSPECIFIED.,.F.,.F.,(4,3,3,3,3,3,3,3,3,3,3,3,3,
3,3,3,3,3,3,3,3,3,3,3,3,3,3,3,3,3,3,3,3,3,3,3,3,3,3,4),(11.6163931973415,
11.7237672656018,11.8347357199021,11.9420294578483,12.0493244336209,12.1566495119213,
12.264033585161,12.3715827272617,12.4792279734473,12.5870706422788,12.6115149000043,
12.7155317843677,12.8193765837255,12.9230806912589,13.0267085981463,13.1302971854635,
13.2338832777977,13.3375740056834,13.4413213587812,13.5452523118071,13.6066366026672,
13.7117447872625,13.8166959584208,13.9215236686367,14.0262853677174,14.1310163775997,
14.2357519758657,14.3405953724673,14.4454990552932,14.5505798283899,14.60175830533,
14.7069309232771,14.8119246326924,14.9168178106501,15.0216457587039,15.1264436979783,
15.2312999910099,15.3361865597888,15.4412122486148,15.503392487373),
 .UNSPECIFIED.);
#545=B_SPLINE_CURVE_WITH_KNOTS('',3,(#43510,#43511,#43512,#43513,#43514,
#43515,#43516,#43517,#43518,#43519,#43520,#43521,#43522,#43523,#43524,#43525,
#43526,#43527,#43528,#43529,#43530,#43531,#43532,#43533,#43534,#43535,#43536,
#43537,#43538,#43539,#43540,#43541,#43542,#43543,#43544,#43545,#43546,#43547,
#43548,#43549,#43550,#43551,#43552,#43553,#43554,#43555,#43556,#43557,#43558,
#43559,#43560,#43561,#43562,#43563,#43564,#43565,#43566,#43567,#43568,#43569,
#43570,#43571,#43572,#43573,#43574,#43575,#43576,#43577,#43578,#43579,#43580,
#43581,#43582,#43583,#43584,#43585,#43586,#43587,#43588,#43589,#43590,#43591,
#43592,#43593,#43594,#43595,#43596,#43597,#43598,#43599,#43600,#43601,#43602,
#43603,#43604,#43605,#43606,#43607,#43608,#43609,#43610,#43611,#43612,#43613,
#43614,#43615,#43616,#43617,#43618,#43619,#43620,#43621,#43622,#43623,#43624,
#43625,#43626,#43627,#43628,#43629,#43630,#43631,#43632,#43633,#43634,#43635,
#43636,#43637,#43638,#43639,#43640,#43641,#43642,#43643,#43644,#43645,#43646,
#43647,#43648,#43649,#43650,#43651,#43652,#43653,#43654,#43655,#43656,#43657,
#43658,#43659,#43660,#43661,#43662,#43663,#43664,#43665,#43666,#43667,#43668,
#43669,#43670,#43671,#43672,#43673,#43674,#43675,#43676,#43677,#43678,#43679,
#43680,#43681,#43682,#43683,#43684,#43685,#43686,#43687,#43688,#43689,#43690,
#43691,#43692,#43693,#43694,#43695,#43696,#43697,#43698,#43699,#43700,#43701,
#43702,#43703,#43704,#43705,#43706,#43707,#43708,#43709,#43710,#43711,#43712,
#43713,#43714,#43715,#43716,#43717,#43718,#43719,#43720,#43721,#43722,#43723,
#43724,#43725,#43726,#43727),.UNSPECIFIED.,.F.,.F.,(4,2,2,2,2,2,2,2,2,2,
2,2,2,2,2,2,2,2,2,2,2,2,2,2,2,2,2,2,2,2,2,2,2,2,2,2,2,2,2,2,2,2,2,2,2,2,
2,2,2,2,2,2,2,2,2,2,2,2,2,2,2,2,2,2,2,2,2,2,2,2,2,2,2,2,2,2,2,2,2,2,2,2,
2,2,2,2,2,2,2,2,2,2,2,2,2,2,2,2,2,2,2,2,2,2,2,2,2,2,4),(-2.28248600441818,
-2.2811956203742,-2.27687867721623,-2.27429210537512,-2.27220672013212,
-2.26937453435887,-2.26390906147731,-2.22240610456411,-2.1817125094513,
-2.17715654769303,-2.17543396354253,-2.17420503146357,-2.17287531524768,
-2.17098113067247,-2.16619035367949,-2.15916593209376,-2.13720086913996,
-2.08636498668884,-2.07952178065835,-2.07645687560523,-2.07411645664894,
-2.07161205809893,-2.06766952812952,-2.05478977904954,-2.03300524837185,
-2.00749534956624,-1.98067095547916,-1.97747634366124,-1.97584649129612,
-1.97455315241394,-1.97301858782097,-1.97017919487622,-1.9539413515156,
-1.89828031814689,-1.88325787526814,-1.87893503696039,-1.87634720382067,
-1.87426208439326,-1.87143195211724,-1.86597629628848,-1.82340189586034,
-1.78382863243893,-1.7792291896914,-1.77750098335071,-1.77627059073702,
-1.77494229662179,-1.77305485838914,-1.76830562448201,-1.74354356694527,
-1.70296881418663,-1.68482176820919,-1.6802749108557,-1.67761170307872,
-1.67530475013581,-1.67247298103653,-1.66700863526789,-1.62565360567816,
-1.58480006736649,-1.58025253527128,-1.57853116236556,-1.57730263481814,
-1.5759727918622,-1.57407758744025,-1.56927988593347,-1.56224194230279,
-1.54020668903168,-1.48947398675752,-1.48261819767435,-1.47955102359204,
-1.47721021482659,-1.47470670166459,-1.470768313846,-1.45792728125288,-1.43623945027337,
-1.41793753057054,-1.38622919963296,-1.38140332677764,-1.37944788184294,
-1.37823958839674,-1.37688861791258,-1.37488987940457,-1.36940037275679,
-1.36097330322796,-1.33073525762771,-1.29150189459091,-1.28418747392266,
-1.28124341165959,-1.27907187837465,-1.27671086179762,-1.27347240216341,
-1.26582988204842,-1.25520228059614,-1.2242321460654,-1.18720437551511,
-1.18246923433969,-1.18052893863192,-1.17920364751265,-1.1778234421524,
-1.17568254853977,-1.16908911148502,-1.15824282282221,-1.10372071610207,
-1.08761413813402,-1.08318926839738,-1.08058044249789,-1.07850064437566,
-1.0757066274937,-1.07041846733174,-1.02623154465591),.UNSPECIFIED.);
#546=B_SPLINE_CURVE_WITH_KNOTS('',3,(#43729,#43730,#43731,#43732,#43733,
#43734,#43735),.UNSPECIFIED.,.F.,.F.,(4,3,4),(15.503392487373,15.5968800079929,
15.707963267949),.UNSPECIFIED.);
#547=B_SPLINE_CURVE_WITH_KNOTS('',3,(#43736,#43737,#43738,#43739,#43740,
#43741,#43742,#43743,#43744,#43745,#43746,#43747,#43748,#43749,#43750,#43751,
#43752,#43753,#43754,#43755,#43756,#43757,#43758,#43759,#43760,#43761,#43762,
#43763,#43764,#43765,#43766,#43767,#43768,#43769,#43770,#43771,#43772,#43773,
#43774,#43775,#43776,#43777,#43778,#43779,#43780,#43781,#43782,#43783,#43784,
#43785,#43786,#43787,#43788,#43789,#43790,#43791,#43792,#43793,#43794,#43795,
#43796,#43797,#43798,#43799,#43800,#43801,#43802,#43803,#43804,#43805,#43806,
#43807,#43808,#43809,#43810,#43811,#43812,#43813,#43814,#43815,#43816,#43817,
#43818,#43819,#43820,#43821,#43822,#43823,#43824,#43825,#43826,#43827,#43828,
#43829,#43830,#43831,#43832,#43833,#43834,#43835,#43836,#43837,#43838,#43839,
#43840,#43841,#43842,#43843,#43844,#43845,#43846,#43847,#43848,#43849,#43850,
#43851,#43852,#43853,#43854,#43855,#43856,#43857,#43858,#43859,#43860,#43861,
#43862,#43863,#43864,#43865,#43866,#43867,#43868,#43869,#43870,#43871,#43872,
#43873,#43874,#43875,#43876,#43877,#43878,#43879,#43880,#43881,#43882,#43883,
#43884,#43885,#43886,#43887,#43888,#43889,#43890,#43891,#43892,#43893,#43894,
#43895,#43896,#43897,#43898,#43899,#43900,#43901,#43902,#43903,#43904,#43905,
#43906,#43907,#43908,#43909,#43910,#43911,#43912,#43913,#43914,#43915,#43916,
#43917,#43918,#43919,#43920,#43921,#43922,#43923,#43924,#43925,#43926,#43927,
#43928,#43929,#43930,#43931,#43932,#43933,#43934,#43935,#43936,#43937,#43938,
#43939,#43940,#43941,#43942,#43943,#43944,#43945,#43946,#43947,#43948,#43949),
 .UNSPECIFIED.,.F.,.F.,(4,2,2,2,2,2,2,2,2,2,2,2,2,2,2,2,2,2,2,2,2,2,2,2,
2,2,2,2,2,2,2,2,2,2,2,2,2,2,2,2,2,2,2,2,2,2,2,2,2,2,2,2,2,2,2,2,2,2,2,2,
2,2,2,2,2,2,2,2,2,2,2,2,2,2,2,2,2,2,2,2,2,2,2,2,2,2,2,2,2,2,2,2,2,2,2,2,
2,2,2,2,2,2,2,2,2,2,4),(-2.51348919495808,-2.45995851601186,-2.44925790244611,
-2.44158591510701,-2.43835650598829,-2.43601015635019,-2.4338578317885,
-2.43094871564621,-2.42376843780528,-2.37888300757562,-2.35263301679549,
-2.34484531596076,-2.34133001370335,-2.33859305270455,-2.33707981008272,
-2.33707269722718,-2.33706552307515,-2.33705828660438,-2.33577007911729,
-2.33415682383674,-2.33103861367995,-2.31009322063273,-2.27757904817603,
-2.25647341571697,-2.2438584508448,-2.23994050890193,-2.23743859686416,
-2.23509122518325,-2.2320036340304,-2.22505040650899,-2.17556520315596,
-2.15294426444102,-2.14579343223834,-2.14093587092273,-2.13902757770181,
-2.13769230437777,-2.13646400042466,-2.13474609670009,-2.13023488163978,
-2.08914229634523,-2.04807187876847,-2.04262861400778,-2.03980093767237,
-2.0377159797013,-2.0351262401371,-2.03079518447029,-2.01569288510483,-1.96004720133005,
-1.94913195234409,-1.94250852294172,-1.94036332624446,-1.93898170892837,
-1.93765828295266,-1.93572277165681,-1.93100843533646,-1.8937024317923,
-1.86296822323266,-1.85239159405453,-1.84477896167686,-1.84154836800767,
-1.83919138771524,-1.83702240249185,-1.83408005137926,-1.82676119050772,
-1.78762460911556,-1.7572348490669,-1.74878710216705,-1.7432898879598,-1.74129215945478,
-1.73994297505554,-1.73873568407142,-1.73678361862874,-1.73197564748851,
-1.69766276544465,-1.66518545527833,-1.65397499034014,-1.64601344078746,
-1.64272271925054,-1.64035279401862,-1.63819303988256,-1.63474720272636,
-1.6264172664817,-1.56276533470499,-1.54600974083554,-1.54314824158543,
-1.54160863683973,-1.540315373341,-1.53869096107488,-1.53552191650157,-1.51130281904821,
-1.47920823824311,-1.45300836406659,-1.44645045873991,-1.44340459316045,
-1.44107511265488,-1.4388518615698,-1.43506654701195,-1.42456374894158,
-1.36362634903188,-1.34701421169184,-1.34415923886547,-1.34262140174274,
-1.34132835458456,-1.33970275810793,-1.33652791435823,-1.31186486080438,
-1.29822679571031),.UNSPECIFIED.);
#548=B_SPLINE_CURVE_WITH_KNOTS('',3,(#43954,#43955,#43956,#43957,#43958,
#43959,#43960,#43961,#43962,#43963,#43964,#43965,#43966,#43967,#43968,#43969,
#43970,#43971,#43972,#43973,#43974,#43975,#43976,#43977,#43978,#43979,#43980,
#43981,#43982,#43983,#43984,#43985,#43986,#43987,#43988,#43989,#43990,#43991,
#43992,#43993,#43994,#43995,#43996,#43997,#43998,#43999,#44000,#44001,#44002,
#44003,#44004,#44005,#44006,#44007,#44008,#44009,#44010,#44011,#44012,#44013,
#44014,#44015,#44016,#44017,#44018,#44019,#44020,#44021,#44022,#44023,#44024,
#44025,#44026,#44027,#44028,#44029,#44030,#44031,#44032,#44033,#44034,#44035,
#44036,#44037,#44038,#44039,#44040,#44041,#44042,#44043,#44044,#44045,#44046,
#44047,#44048,#44049,#44050,#44051,#44052,#44053,#44054,#44055,#44056,#44057,
#44058,#44059,#44060,#44061,#44062,#44063,#44064,#44065,#44066,#44067,#44068,
#44069,#44070,#44071,#44072,#44073,#44074,#44075,#44076,#44077,#44078,#44079,
#44080,#44081,#44082,#44083,#44084,#44085,#44086,#44087,#44088,#44089,#44090,
#44091,#44092,#44093,#44094,#44095,#44096,#44097,#44098,#44099,#44100,#44101,
#44102,#44103,#44104,#44105,#44106,#44107,#44108,#44109,#44110,#44111,#44112,
#44113,#44114,#44115,#44116,#44117,#44118,#44119,#44120,#44121,#44122,#44123,
#44124,#44125,#44126,#44127,#44128,#44129,#44130,#44131,#44132,#44133,#44134,
#44135,#44136,#44137,#44138,#44139,#44140,#44141,#44142,#44143,#44144,#44145,
#44146,#44147,#44148,#44149,#44150,#44151,#44152,#44153,#44154,#44155,#44156,
#44157,#44158,#44159,#44160,#44161),.UNSPECIFIED.,.F.,.F.,(4,2,2,2,2,2,
2,2,2,2,2,2,2,2,2,2,2,2,2,2,2,2,2,2,2,2,2,2,2,2,2,2,2,2,2,2,2,2,2,2,2,2,
2,2,2,2,2,2,2,2,2,2,2,2,2,2,2,2,2,2,2,2,2,2,2,2,2,2,2,2,2,2,2,2,2,2,2,2,
2,2,2,2,2,2,2,2,2,2,2,2,2,2,2,2,2,2,2,2,2,2,2,2,2,4),(-3.53887107067202,
-3.50922941979923,-3.48733849991634,-3.47441513608124,-3.470467913123,-3.46796246119239,
-3.46562239711216,-3.46255988650963,-3.4557302926679,-3.40474048486825,
-3.38284495091239,-3.37583391707794,-3.37105038581197,-3.36915729607683,
-3.36782775521713,-3.3665985055681,-3.36487483895307,-3.36031064471525,
-3.31982533440377,-3.27816235897577,-3.27269644904552,-3.26986406919186,
-3.26755671103684,-3.26489313546167,-3.2603458836294,-3.24220191796138,
-3.20157591866347,-3.17681570460497,-3.17206648536367,-3.17017882791212,
-3.16885032819734,-3.16761981723845,-3.1658913646053,-3.16129051200363,
-3.12177121208322,-3.07920057734017,-3.07373035941,-3.0708971336758,-3.06881155608696,
-3.06622548522212,-3.0619111241625,-3.04697946666633,-2.99708607414523,
-2.98220671927603,-2.9767183889018,-2.97275102426313,-2.97099491119951,
-2.96968835147231,-2.96823377014834,-2.9657612443333,-2.95697562944232,
-2.89459661138065,-2.88367988327608,-2.87587851006771,-2.87261431699605,
-2.87024941465539,-2.86808457032404,-2.86516515011988,-2.85799153066069,
-2.81315219504935,-2.78712172843256,-2.77936190439719,-2.77419973397115,
-2.77224900268981,-2.77090836458305,-2.76969179651282,-2.76801607549204,
-2.76376836909518,-2.719655069334,-2.68136267313181,-2.67579019806618,-2.67293625034027,
-2.67064898845357,-2.66800983413166,-2.6635681375633,-2.64681610415624,
-2.59300891475173,-2.58220210556648,-2.57562530060871,-2.57348515905856,
-2.57210425470312,-2.57077848069766,-2.56883592423162,-2.56408679120747,
-2.52775288602899,-2.49631919577921,-2.48560181711695,-2.4779096554613,
-2.47466341619169,-2.47230152682221,-2.4701325213564,-2.46719697413253,
-2.45990329011298,-2.41824165612287,-2.38095092334477,-2.37622882016353,
-2.37429070004303,-2.37296574929545,-2.37158352194142,-2.36943753105829,
-2.36281254517813,-2.351896197006,-2.29615580431147,-2.28248600441818),
 .UNSPECIFIED.);
#549=B_SPLINE_CURVE_WITH_KNOTS('',3,(#44162,#44163,#44164,#44165,#44166,
#44167,#44168,#44169,#44170,#44171,#44172,#44173,#44174,#44175,#44176,#44177,
#44178,#44179,#44180,#44181,#44182,#44183,#44184,#44185,#44186,#44187,#44188,
#44189,#44190,#44191,#44192,#44193,#44194,#44195,#44196,#44197,#44198,#44199,
#44200,#44201,#44202,#44203,#44204,#44205,#44206,#44207,#44208,#44209,#44210,
#44211,#44212,#44213,#44214,#44215,#44216,#44217,#44218,#44219,#44220,#44221,
#44222,#44223,#44224,#44225,#44226,#44227,#44228,#44229,#44230,#44231,#44232,
#44233,#44234,#44235,#44236,#44237,#44238,#44239,#44240,#44241,#44242,#44243,
#44244,#44245,#44246,#44247,#44248,#44249,#44250,#44251,#44252,#44253,#44254,
#44255,#44256,#44257,#44258,#44259,#44260,#44261,#44262,#44263,#44264,#44265,
#44266,#44267,#44268,#44269,#44270,#44271,#44272,#44273,#44274,#44275,#44276,
#44277,#44278,#44279,#44280,#44281,#44282,#44283,#44284,#44285,#44286,#44287,
#44288,#44289,#44290,#44291,#44292,#44293,#44294,#44295,#44296,#44297,#44298,
#44299,#44300,#44301,#44302,#44303,#44304,#44305,#44306,#44307,#44308,#44309,
#44310,#44311,#44312,#44313,#44314,#44315,#44316,#44317,#44318,#44319,#44320,
#44321,#44322,#44323,#44324,#44325,#44326,#44327,#44328,#44329,#44330,#44331,
#44332,#44333,#44334,#44335,#44336,#44337,#44338,#44339,#44340,#44341,#44342,
#44343,#44344,#44345,#44346,#44347,#44348,#44349,#44350,#44351,#44352,#44353,
#44354,#44355,#44356,#44357,#44358,#44359,#44360,#44361,#44362,#44363,#44364,
#44365,#44366,#44367,#44368,#44369,#44370,#44371,#44372,#44373,#44374,#44375,
#44376,#44377,#44378,#44379,#44380,#44381),.UNSPECIFIED.,.F.,.F.,(4,2,2,
2,2,2,2,2,2,2,2,2,2,2,2,2,2,2,2,2,2,2,2,2,2,2,2,2,2,2,2,2,2,2,2,2,2,2,2,
2,2,2,2,2,2,2,2,2,2,2,2,2,2,2,2,2,2,2,2,2,2,2,2,2,2,2,2,2,2,2,2,2,2,2,2,
2,2,2,2,2,2,2,2,2,2,2,2,2,2,2,2,2,2,2,2,2,2,2,2,2,2,2,2,2,2,2,2,2,2,4),
(-1.29822679571031,-1.27895328969278,-1.25748672292451,-1.24864679765181,
-1.24511425309564,-1.24293884239871,-1.24058220098635,-1.23736524512498,
-1.22984615447287,-1.2194403163622,-1.16517567209637,-1.15788701334334,
-1.14761048742258,-1.14502837285733,-1.14353448051516,-1.1423664724244,
-1.14074924654084,-1.13751266436597,-1.13328644493537,-1.12317473779889,
-1.0786034610789,-1.05258498715359,-1.04802980704026,-1.04512275966436,
-1.04280920358247,-1.04019728265348,-1.03576682629165,-1.0173495029958,
-0.995874651050368,-0.95342497157346,-0.947648200200771,-0.94554254440962,
-0.944305538288356,-0.942981332078365,-0.941118073008606,-0.936522665539095,
-0.913386836116961,-0.888507509418362,-0.853989835326333,-0.849240647417688,
-0.846275000556268,-0.843955225127735,-0.841378163669728,-0.837106446233343,
-0.820747916845267,-0.760566052442591,-0.749677041194939,-0.747043947049844,
-0.74553806763779,-0.74425367182106,-0.742590563867531,-0.739123204089172,
-0.70954213204649,-0.657042481989379,-0.650393441978837,-0.64736294342257,
-0.645027347281515,-0.642507002341059,-0.638494072369844,-0.624950277399896,
-0.577450201276283,-0.551551734857781,-0.548362023650472,-0.546732844587719,
-0.545439098388867,-0.543902956566073,-0.541057689924605,-0.524698486331764,
-0.467528651101692,-0.45382606962641,-0.449641770181674,-0.447083822184037,
-0.444759448228052,-0.441757309449051,-0.435435615512219,-0.41104635857681,
-0.370013757478364,-0.36653701133575,-0.351960870592596,-0.349342541283221,
-0.347700151387892,-0.346405670633289,-0.344880089868795,-0.342083786621802,
-0.326831189945612,-0.280945091773491,-0.256309066476146,-0.251806534446449,
-0.248915399231092,-0.246603147222507,-0.243980528682811,-0.239708530630539,
-0.223567978482093,-0.191787527481715,-0.155877454641331,-0.151109484257704,
-0.149163463807437,-0.147836747515223,-0.146456246517117,-0.144319167732365,
-0.138696197858469,-0.11440300777536,-0.0894439206500073,-0.0577409661094255,
-0.0530218085822374,-0.0500650464892128,-0.0477461167947669,-0.0451637001010432,
-0.0424932371688889,-0.0416143629966081),.UNSPECIFIED.);
#550=B_SPLINE_CURVE_WITH_KNOTS('',3,(#44386,#44387,#44388,#44389,#44390,
#44391,#44392,#44393,#44394,#44395,#44396,#44397,#44398,#44399,#44400,#44401,
#44402,#44403,#44404,#44405,#44406,#44407,#44408,#44409,#44410,#44411,#44412,
#44413,#44414,#44415,#44416,#44417,#44418,#44419,#44420,#44421,#44422,#44423,
#44424,#44425,#44426,#44427,#44428,#44429,#44430,#44431,#44432,#44433,#44434,
#44435,#44436,#44437,#44438,#44439,#44440,#44441,#44442,#44443,#44444,#44445,
#44446,#44447,#44448,#44449,#44450,#44451,#44452,#44453,#44454,#44455,#44456,
#44457,#44458,#44459,#44460,#44461,#44462,#44463,#44464,#44465,#44466,#44467,
#44468,#44469,#44470,#44471,#44472,#44473,#44474,#44475,#44476,#44477,#44478,
#44479,#44480,#44481,#44482,#44483,#44484,#44485,#44486,#44487,#44488,#44489,
#44490,#44491,#44492,#44493,#44494,#44495,#44496,#44497,#44498,#44499,#44500,
#44501,#44502,#44503,#44504,#44505,#44506,#44507,#44508,#44509,#44510,#44511,
#44512,#44513,#44514,#44515,#44516,#44517,#44518,#44519,#44520,#44521,#44522,
#44523,#44524,#44525,#44526,#44527,#44528,#44529,#44530,#44531,#44532,#44533,
#44534,#44535,#44536,#44537,#44538,#44539,#44540,#44541,#44542,#44543,#44544,
#44545,#44546,#44547,#44548,#44549,#44550,#44551,#44552,#44553,#44554,#44555,
#44556,#44557,#44558,#44559,#44560,#44561,#44562,#44563,#44564,#44565,#44566,
#44567,#44568,#44569,#44570,#44571,#44572,#44573,#44574,#44575,#44576,#44577,
#44578,#44579,#44580,#44581,#44582,#44583,#44584,#44585,#44586,#44587,#44588,
#44589,#44590,#44591,#44592,#44593,#44594,#44595,#44596,#44597,#44598,#44599,
#44600,#44601,#44602,#44603,#44604,#44605,#44606,#44607,#44608,#44609,#44610,
#44611,#44612,#44613),.UNSPECIFIED.,.F.,.F.,(4,2,2,2,2,2,2,2,2,2,2,2,2,
2,2,2,2,2,2,2,2,2,2,2,2,2,2,2,2,2,2,2,2,2,2,2,2,2,2,2,2,2,2,2,2,2,2,2,2,
2,2,2,2,2,2,2,2,2,2,2,2,2,2,2,2,2,2,2,2,2,2,2,2,2,2,2,2,2,2,2,2,2,2,2,2,
2,2,2,2,2,2,2,2,2,2,2,2,2,2,2,2,2,2,2,2,2,2,2,2,2,2,2,2,4),(-4.79482997017295,
-4.77764623982758,-4.76922698254938,-4.76374262386725,-4.76174563263966,
-4.76039581283252,-4.7591881320624,-4.75723372644256,-4.75241090604438,
-4.72110610674379,-4.69427235077831,-4.67790801877642,-4.67084377371781,
-4.66534344969845,-4.66251519899233,-4.66029444284504,-4.65770135159296,
-4.65335261600249,-4.63807321811889,-4.59409640502174,-4.56937372866805,
-4.56462882140078,-4.56274222830511,-4.56141425632179,-4.56018405801937,
-4.5584558033292,-4.5538535997449,-4.51440833386472,-4.47142065959173,-4.46617668390806,
-4.46339089781846,-4.46131078331815,-4.45869309379428,-4.45423220543829,
-4.43786809123279,-4.38366584296189,-4.37283694175938,-4.36625098757193,
-4.36411006014671,-4.36272920012707,-4.36140395163977,-4.35946289693512,
-4.35472108591198,-4.318207846487,-4.28691406775286,-4.27622501850695,-4.26854888940172,
-4.26530580909572,-4.262944914523,-4.26077591839745,-4.25783900633327,-4.25056161927958,
-4.20863871521683,-4.19581447241706,-4.1714906864455,-4.16678286524389,
-4.16490205653054,-4.16357507980018,-4.16234333255227,-4.16060952994487,
-4.15596723145889,-4.11714354836527,-4.07376345262449,-4.06841021923842,
-4.06560155388367,-4.06351906919686,-4.06091752448886,-4.05653085092519,
-4.04084227114978,-3.98588408005581,-3.97501007467649,-3.9684043906448,
-3.96626096522958,-3.96487947694789,-3.9635544656636,-3.96161505461155,
-3.95688373404647,-3.9198347620443,-3.88892102005205,-3.87830615709546,
-3.87067079777651,-3.86743438585452,-3.86507451263597,-3.86290378945798,
-3.85996046878927,-3.8526461892945,-3.81327521715505,-3.78308608347465,
-3.77466625112952,-3.76918128045648,-3.76718391610852,-3.76583379955797,
-3.76462581931788,-3.76267086652365,-3.75784638340767,-3.72605209796989,
-3.69169657447381,-3.67417021710501,-3.66980669939626,-3.66721000705005,
-3.66489490984255,-3.66196566879379,-3.65733558871987,-3.6289447070153,
-3.57735130450709,-3.57280642681377,-3.56938034182256,-3.56772567830787,
-3.56643068883029,-3.56491515314762,-3.56223822761924,-3.55074954275652,
-3.5395432496804,-3.53887107067202),.UNSPECIFIED.);
#551=B_SPLINE_CURVE_WITH_KNOTS('',3,(#44615,#44616,#44617,#44618,#44619,
#44620),.UNSPECIFIED.,.F.,.F.,(4,2,4),(-0.0416143629966081,-0.0385168137734201,
-0.000582969486234699),.UNSPECIFIED.);
#552=B_SPLINE_CURVE_WITH_KNOTS('',3,(#44621,#44622,#44623,#44624,#44625,
#44626,#44627,#44628,#44629,#44630,#44631,#44632,#44633,#44634,#44635,#44636,
#44637,#44638,#44639,#44640,#44641,#44642,#44643,#44644,#44645,#44646,#44647,
#44648,#44649,#44650,#44651,#44652,#44653,#44654,#44655,#44656,#44657,#44658,
#44659,#44660,#44661,#44662,#44663,#44664,#44665,#44666,#44667,#44668,#44669,
#44670,#44671,#44672,#44673,#44674,#44675,#44676,#44677,#44678,#44679,#44680,
#44681,#44682,#44683,#44684,#44685,#44686,#44687,#44688,#44689,#44690,#44691,
#44692,#44693,#44694,#44695,#44696,#44697,#44698,#44699,#44700,#44701,#44702,
#44703,#44704,#44705,#44706,#44707,#44708,#44709,#44710,#44711,#44712,#44713,
#44714,#44715,#44716,#44717,#44718,#44719,#44720,#44721,#44722,#44723,#44724,
#44725,#44726,#44727,#44728,#44729,#44730,#44731,#44732,#44733,#44734,#44735,
#44736,#44737,#44738,#44739,#44740,#44741,#44742,#44743,#44744,#44745,#44746,
#44747,#44748,#44749,#44750,#44751,#44752,#44753,#44754,#44755,#44756,#44757,
#44758,#44759,#44760,#44761,#44762,#44763,#44764,#44765,#44766,#44767,#44768,
#44769,#44770,#44771,#44772,#44773,#44774,#44775,#44776,#44777,#44778,#44779,
#44780,#44781,#44782,#44783,#44784,#44785,#44786,#44787,#44788,#44789,#44790,
#44791,#44792,#44793,#44794,#44795,#44796,#44797,#44798,#44799,#44800,#44801),
 .UNSPECIFIED.,.F.,.F.,(4,3,3,3,3,3,3,3,3,3,3,3,3,3,3,3,3,3,3,3,3,3,3,3,
3,3,3,3,3,3,3,3,3,3,3,3,3,3,3,3,3,3,3,3,3,3,3,3,3,3,3,3,3,3,3,3,3,3,3,3,
4),(28.274333882559,28.4078755781023,28.5334621426098,28.6384554085175,
28.7432919913857,28.8480062043826,28.9526551590355,29.0572743614538,29.1618992742995,
29.2666344758122,29.3714312307972,29.4764081877237,29.5285838452726,29.6335770945177,
29.7384136605605,29.8431278565749,29.9477767941578,30.0523959794451,30.1570208751251,
30.2617560595375,30.3665527974347,30.4715297374735,30.5237055479355,30.6286987928139,
30.7335353543564,30.838249545694,30.9428984784934,31.0475176588977,31.1521425496021,
31.256877728932,31.3616744616784,31.4666513965143,31.5188272505983,31.6238205022426,
31.7286570706674,31.8333712690265,31.9380202089294,32.0426393965084,32.147264294448,
32.2519994810554,32.3567962211141,32.461773163239,32.5139489532611,32.6189422022832,
32.7237787680559,32.8284929637316,32.9331419009333,33.0377610857974,33.1423859810126,
33.2471211649,33.3519179022371,33.4568948416669,33.509070655924,33.6145354527492,
33.7193523119969,33.8240640404197,33.9287062339165,34.0347269330688,34.1393751681461,
34.2460820993359,34.3527890305257),.UNSPECIFIED.);
#553=B_SPLINE_CURVE_WITH_KNOTS('',3,(#44807,#44808,#44809,#44810,#44811,
#44812,#44813,#44814,#44815,#44816,#44817,#44818,#44819,#44820,#44821,#44822,
#44823,#44824,#44825,#44826,#44827,#44828,#44829,#44830,#44831,#44832,#44833,
#44834,#44835,#44836,#44837,#44838,#44839,#44840,#44841,#44842,#44843,#44844,
#44845,#44846,#44847,#44848,#44849,#44850,#44851,#44852,#44853,#44854,#44855,
#44856,#44857,#44858,#44859,#44860,#44861,#44862,#44863,#44864,#44865,#44866,
#44867,#44868,#44869,#44870,#44871,#44872,#44873,#44874,#44875,#44876,#44877,
#44878,#44879,#44880,#44881,#44882,#44883,#44884,#44885,#44886,#44887,#44888,
#44889,#44890,#44891,#44892,#44893,#44894,#44895,#44896,#44897,#44898,#44899,
#44900,#44901,#44902,#44903,#44904,#44905,#44906,#44907,#44908,#44909,#44910,
#44911,#44912,#44913,#44914,#44915,#44916,#44917,#44918,#44919,#44920,#44921,
#44922,#44923,#44924,#44925,#44926,#44927,#44928,#44929,#44930,#44931,#44932,
#44933,#44934,#44935,#44936,#44937,#44938,#44939,#44940,#44941,#44942,#44943,
#44944,#44945,#44946,#44947,#44948,#44949,#44950,#44951,#44952,#44953,#44954,
#44955,#44956,#44957,#44958,#44959,#44960,#44961,#44962,#44963,#44964,#44965,
#44966,#44967,#44968,#44969,#44970,#44971,#44972,#44973,#44974,#44975,#44976,
#44977,#44978,#44979,#44980,#44981,#44982,#44983,#44984,#44985,#44986,#44987,
#44988,#44989,#44990,#44991,#44992,#44993,#44994,#44995,#44996,#44997,#44998,
#44999,#45000,#45001,#45002,#45003,#45004,#45005,#45006,#45007,#45008,#45009,
#45010,#45011,#45012,#45013,#45014,#45015,#45016,#45017,#45018,#45019,#45020,
#45021,#45022,#45023,#45024,#45025,#45026,#45027,#45028,#45029,#45030,#45031,
#45032,#45033,#45034,#45035,#45036,#45037,#45038,#45039,#45040,#45041,#45042,
#45043,#45044,#45045,#45046,#45047,#45048,#45049,#45050,#45051,#45052,#45053,
#45054,#45055,#45056,#45057,#45058,#45059,#45060,#45061,#45062),
 .UNSPECIFIED.,.F.,.F.,(4,2,2,2,2,2,2,2,2,2,2,2,2,2,2,2,2,2,2,2,2,2,2,2,
2,2,2,2,2,2,2,2,2,2,2,2,2,2,2,2,2,2,2,2,2,2,2,2,2,2,2,2,2,2,2,2,2,2,2,2,
2,2,2,2,2,2,2,2,2,2,2,2,2,2,2,2,2,2,2,2,2,2,2,2,2,2,2,2,2,2,2,2,2,2,2,2,
2,2,2,2,2,2,2,2,2,2,2,2,2,2,2,2,2,2,2,2,2,2,2,2,2,2,2,2,2,2,2,4),(-1.21647185737743,
-1.21574655815076,-1.21140130549938,-1.19412114657841,-1.16062994279692,
-1.12762346677669,-1.12280095659216,-1.12084607037418,-1.11963790956277,
-1.11828737085617,-1.11628900652554,-1.11079885561553,-1.10236991516711,
-1.07212174717415,-1.0328502328975,-1.02553392661769,-1.02258987310533,
-1.02041863281981,-1.01805821985302,-1.01482112132328,-1.00718443816655,
-0.996566735416115,-0.965644232856276,-0.928543458792508,-0.923811121510414,
-0.92187123342243,-0.920545882514452,-0.919164018685551,-0.91701998760303,
-0.910412110785537,-0.8995355742952,-0.844509223842372,-0.828891860005707,
-0.824511168412601,-0.821910458068376,-0.819827131788921,-0.817015353896145,
-0.81164951182727,-0.767426867210257,-0.761872755202397,-0.747367535836241,
-0.739496965535903,-0.726512349777988,-0.723978604624732,-0.722362145974492,
-0.721069457705053,-0.719523812841109,-0.716632311116422,-0.699084973079515,
-0.670756543271938,-0.631506502268718,-0.626768082625019,-0.623805964803542,
-0.621486979092822,-0.618908767952702,-0.614630387967659,-0.598184357742755,
-0.536935064731781,-0.527071046981134,-0.524524638498465,-0.523038839300196,
-0.521869498478946,-0.520240452832437,-0.516945085351468,-0.512620914457062,
-0.502167929542529,-0.453496104684904,-0.433510236196657,-0.427593378772528,
-0.424669907447243,-0.422354800141479,-0.419753289145133,-0.415370062620266,
-0.397595933830812,-0.360476731321582,-0.345496125494898,-0.328842668633675,
-0.326127853350555,-0.324456598900775,-0.323159978644721,-0.321655589971298,
-0.318956768971214,-0.305610888592713,-0.273764237793886,-0.233455786535155,
-0.228729439617405,-0.225770751020104,-0.223451904777254,-0.223416428661751,
-0.223365488623818,-0.223318920660677,-0.22327634690799,-0.223237421829452,
-0.223201829683931,-0.223169282092572,-0.223139515701249,-0.223112290223071,
-0.223087386375076,-0.223064604014682,-0.223043760455055,-0.223024689007459,
-0.223007237569998,-0.222980072421483,-0.222953431311812,-0.222927301882303,
-0.222901672115073,-0.220168080228804,-0.215097309546578,-0.208729735302207,
-0.194653055997958,-0.135256349340276,-0.128422165925436,-0.126172185808727,
-0.124766764027862,-0.123440046395093,-0.121563596451935,-0.116887027265773,
-0.0929104680205791,-0.0540443370026769,-0.0386634350423491,-0.0307681848463778,
-0.0277285071760984,-0.0255325108033753,-0.0233171458246013,-0.0210389377766114,
-0.0180653078849011,-0.0113560425394448,-0.000720790627167),
 .UNSPECIFIED.);
#554=B_SPLINE_CURVE_WITH_KNOTS('',3,(#45063,#45064,#45065,#45066),
 .UNSPECIFIED.,.F.,.F.,(4,4),(-4.83557347754785,-4.79482997017295),
 .UNSPECIFIED.);
#555=B_SPLINE_CURVE_WITH_KNOTS('',3,(#45068,#45069,#45070,#45071,#45072,
#45073,#45074,#45075,#45076,#45077),.UNSPECIFIED.,.F.,.F.,(4,3,3,4),(34.3527890305257,
34.45776855454,34.5041923585868,34.5575191894877),.UNSPECIFIED.);
#556=B_SPLINE_CURVE_WITH_KNOTS('',3,(#45078,#45079,#45080,#45081,#45082,
#45083,#45084,#45085,#45086,#45087,#45088,#45089,#45090,#45091,#45092,#45093,
#45094,#45095,#45096,#45097,#45098,#45099,#45100,#45101,#45102,#45103,#45104,
#45105,#45106,#45107,#45108,#45109,#45110,#45111,#45112,#45113,#45114,#45115,
#45116,#45117,#45118,#45119,#45120,#45121,#45122,#45123,#45124,#45125,#45126,
#45127,#45128,#45129,#45130,#45131,#45132,#45133,#45134,#45135,#45136,#45137,
#45138,#45139,#45140,#45141,#45142,#45143,#45144,#45145,#45146,#45147,#45148,
#45149,#45150,#45151,#45152,#45153,#45154,#45155,#45156,#45157,#45158,#45159,
#45160,#45161,#45162,#45163,#45164,#45165,#45166,#45167,#45168,#45169,#45170,
#45171,#45172,#45173,#45174,#45175,#45176,#45177,#45178,#45179,#45180,#45181,
#45182,#45183,#45184,#45185,#45186,#45187,#45188,#45189,#45190,#45191,#45192,
#45193,#45194,#45195,#45196,#45197,#45198,#45199,#45200,#45201,#45202,#45203,
#45204,#45205,#45206,#45207,#45208,#45209,#45210,#45211,#45212,#45213,#45214,
#45215,#45216,#45217,#45218,#45219,#45220,#45221,#45222,#45223,#45224,#45225,
#45226,#45227,#45228,#45229,#45230,#45231,#45232,#45233,#45234,#45235,#45236,
#45237,#45238,#45239,#45240,#45241,#45242,#45243,#45244,#45245,#45246,#45247,
#45248,#45249,#45250,#45251,#45252,#45253,#45254,#45255,#45256,#45257,#45258,
#45259,#45260,#45261,#45262,#45263,#45264,#45265,#45266,#45267,#45268,#45269,
#45270,#45271,#45272,#45273,#45274,#45275,#45276,#45277,#45278,#45279,#45280,
#45281,#45282,#45283,#45284,#45285,#45286,#45287,#45288,#45289,#45290,#45291,
#45292,#45293,#45294,#45295,#45296,#45297,#45298,#45299,#45300,#45301,#45302,
#45303),.UNSPECIFIED.,.F.,.F.,(4,2,2,2,2,2,2,2,2,2,2,2,2,2,2,2,2,2,2,2,
2,2,2,2,2,2,2,2,2,2,2,2,2,2,2,2,2,2,2,2,2,2,2,2,2,2,2,2,2,2,2,2,2,2,2,2,
2,2,2,2,2,2,2,2,2,2,2,2,2,2,2,2,2,2,2,2,2,2,2,2,2,2,2,2,2,2,2,2,2,2,2,2,
2,2,2,2,2,2,2,2,2,2,2,2,2,2,2,2,2,2,2,2,4),(-2.51415926376174,-2.45595526132352,
-2.44112870201634,-2.43452733147181,-2.42926422031906,-2.42647356109047,
-2.42418954217027,-2.42149939363548,-2.41683691594838,-2.39707458547378,
-2.35094125696788,-2.33730636174485,-2.33212687745788,-2.32948552374808,
-2.32782396871898,-2.326294915424,-2.32628755800407,-2.32628014471568,-2.32627267422959,
-2.32626514551919,-2.32625755771562,-2.32624990970272,-2.32624220000473,
-2.32623442757019,-2.32622659123447,-2.32621868979411,-2.32496383987108,
-2.32334421218533,-2.32019835187765,-2.28767943860881,-2.26308488322178,
-2.23749095992347,-2.23101021476857,-2.22797818918882,-2.22565002438273,
-2.22310713799184,-2.21899074630113,-2.20589127340483,-2.14801148543067,
-2.13159679594088,-2.12874919284554,-2.12721258566695,-2.12591890451106,
-2.12429039737408,-2.12110376386547,-2.09598235628415,-2.05862531199044,
-2.04337535354933,-2.03335250231701,-2.02975417991429,-2.02732287246096,
-2.02496766086127,-2.02215054080926,-2.01513674188087,-1.9658654929862,
-1.95999471481222,-1.93541361300809,-1.9306801491706,-1.92879455543864,
-1.9274660726498,-1.92623442727144,-1.92450281351788,-1.91988148136306,
-1.88068929779506,-1.83778802082334,-1.83231421054579,-1.82947960385203,
-1.82717135622286,-1.82450778460227,-1.81996305645371,-1.80186986694142,
-1.76119638828816,-1.73639913349757,-1.73164560845845,-1.72975686854339,
-1.7284278215718,-1.72719697685618,-1.7254682890548,-1.72086863832788,-1.68127207798351,
-1.63862324798777,-1.63322505035667,-1.63040604947331,-1.62832139991219,
-1.62572423664867,-1.62136204267509,-1.60595289813047,-1.55651091477708,
-1.53664836875506,-1.53238776034315,-1.53057996895369,-1.52926513719045,
-1.52783349288848,-1.5254657537729,-1.51765735873293,-1.45415996457956,
-1.44318799478322,-1.43535578666817,-1.43208580874529,-1.42971924490477,
-1.42755461856165,-1.42463811815043,-1.41748492338795,-1.37215876014298,
-1.34645902812729,-1.33875441889072,-1.33361926215697,-1.33167212977002,
-1.33033187909921,-1.32911403718709,-1.32743443630268,-1.32316557584655,
-1.29810802178685),.UNSPECIFIED.);
#557=B_SPLINE_CURVE_WITH_KNOTS('',3,(#45308,#45309,#45310,#45311,#45312,
#45313,#45314,#45315,#45316,#45317,#45318,#45319,#45320,#45321,#45322,#45323,
#45324,#45325,#45326,#45327,#45328,#45329,#45330,#45331,#45332,#45333,#45334,
#45335,#45336,#45337,#45338,#45339,#45340,#45341,#45342,#45343,#45344,#45345,
#45346,#45347,#45348,#45349,#45350,#45351,#45352,#45353,#45354,#45355,#45356,
#45357,#45358,#45359,#45360,#45361,#45362,#45363,#45364,#45365,#45366,#45367,
#45368,#45369,#45370,#45371,#45372,#45373,#45374,#45375,#45376,#45377,#45378,
#45379,#45380,#45381,#45382,#45383,#45384,#45385,#45386,#45387,#45388,#45389,
#45390,#45391,#45392,#45393,#45394,#45395,#45396,#45397,#45398,#45399,#45400,
#45401,#45402,#45403,#45404,#45405,#45406,#45407,#45408,#45409,#45410,#45411,
#45412,#45413,#45414,#45415,#45416,#45417,#45418,#45419,#45420,#45421,#45422,
#45423,#45424,#45425,#45426,#45427,#45428,#45429,#45430,#45431,#45432,#45433,
#45434,#45435,#45436,#45437,#45438,#45439,#45440,#45441,#45442,#45443,#45444,
#45445,#45446,#45447,#45448,#45449,#45450,#45451,#45452,#45453,#45454,#45455,
#45456,#45457,#45458,#45459,#45460,#45461,#45462,#45463,#45464,#45465,#45466,
#45467,#45468,#45469,#45470,#45471,#45472,#45473,#45474,#45475,#45476,#45477,
#45478,#45479,#45480,#45481,#45482,#45483,#45484,#45485,#45486,#45487,#45488,
#45489,#45490,#45491,#45492,#45493,#45494,#45495,#45496,#45497,#45498,#45499,
#45500,#45501,#45502,#45503,#45504,#45505,#45506,#45507,#45508,#45509,#45510,
#45511,#45512,#45513,#45514,#45515,#45516,#45517,#45518,#45519),
 .UNSPECIFIED.,.F.,.F.,(4,2,2,2,2,2,2,2,2,2,2,2,2,2,2,2,2,2,2,2,2,2,2,2,
2,2,2,2,2,2,2,2,2,2,2,2,2,2,2,2,2,2,2,2,2,2,2,2,2,2,2,2,2,2,2,2,2,2,2,2,
2,2,2,2,2,2,2,2,2,2,2,2,2,2,2,2,2,2,2,2,2,2,2,2,2,2,2,2,2,2,2,2,2,2,2,2,
2,2,2,2,2,2,2,2,2,4),(-2.47295895309433,-2.44885936015139,-2.42419073849797,
-2.41783273887889,-2.41482448410038,-2.41250015570533,-2.40994705421754,
-2.40578159271537,-2.39223916332579,-2.33091091400115,-2.32240612463165,
-2.31688006810118,-2.31535570403553,-2.31412526478104,-2.31285727071393,
-2.31129528108774,-2.30833276977913,-2.29138578503038,-2.25408028794101,
-2.23337007549272,-2.22092288113042,-2.21702746204059,-2.21453321692116,
-2.21218836561025,-2.20909736242905,-2.20210785950399,-2.1526253717665,
-2.12977042082761,-2.12257655604796,-2.11769920213401,-2.11579142600398,
-2.11445905282926,-2.11323313253996,-2.11152211860302,-2.1070531863777,
-2.06511431395827,-2.02468895833362,-2.01927338729105,-2.0164512905228,
-2.01436682142138,-2.01177305459244,-2.00742417792338,-1.99215762227006,
-1.93671938522095,-1.92049283900378,-1.91765352130429,-1.91611884903683,
-1.91482528343907,-1.91319500426234,-1.9099992639834,-1.8818553179476,-1.86947680546592,
-1.8258164753382,-1.82031104387951,-1.81747029700834,-1.81516209315476,
-1.81250417492365,-1.80798271493916,-1.79014346356711,-1.74932881024771,
-1.72440976591321,-1.71964544664394,-1.71775522863683,-1.71642609751042,
-1.71519594002091,-1.71346925608493,-1.70888312775535,-1.66896429166959,
-1.62681496629872,-1.62131035018889,-1.61846980829889,-1.61616166478901,
-1.61350369818846,-1.60898186989493,-1.59113674761483,-1.54330699008263,
-1.52934334943206,-1.52408093000085,-1.52024034953513,-1.51850703450817,
-1.51720342664469,-1.51573663905622,-1.51320952468757,-1.50387412678734,
-1.44208537499504,-1.42559853136642,-1.42131675556956,-1.41873774531891,
-1.41641883129294,-1.41345789590429,-1.40872353746256,-1.36923943640455,
-1.34043543714986,-1.32350222914285,-1.32063419059999,-1.31909349594471,
-1.31780047657174,-1.3161779760227,-1.31301816763087,-1.28949542319404,
-1.25744063422231,-1.22824698623945,-1.22359274400703,-1.22065587844616,
-1.21833957189857,-1.21647185737743),.UNSPECIFIED.);
#558=B_SPLINE_CURVE_WITH_KNOTS('',3,(#45520,#45521,#45522,#45523,#45524,
#45525,#45526,#45527,#45528,#45529,#45530,#45531,#45532,#45533,#45534,#45535,
#45536,#45537,#45538,#45539,#45540,#45541,#45542,#45543,#45544,#45545,#45546,
#45547,#45548,#45549,#45550,#45551,#45552,#45553,#45554,#45555,#45556,#45557,
#45558,#45559,#45560,#45561,#45562,#45563,#45564,#45565,#45566,#45567,#45568,
#45569,#45570,#45571,#45572,#45573,#45574,#45575,#45576,#45577,#45578,#45579,
#45580,#45581,#45582,#45583,#45584,#45585,#45586,#45587,#45588,#45589,#45590,
#45591,#45592,#45593,#45594,#45595,#45596,#45597,#45598,#45599,#45600,#45601,
#45602,#45603,#45604,#45605,#45606,#45607,#45608,#45609,#45610,#45611,#45612,
#45613,#45614,#45615,#45616,#45617,#45618,#45619,#45620,#45621,#45622,#45623,
#45624,#45625,#45626,#45627,#45628,#45629,#45630,#45631,#45632,#45633,#45634,
#45635,#45636,#45637,#45638,#45639,#45640,#45641,#45642,#45643,#45644,#45645,
#45646,#45647,#45648,#45649,#45650,#45651,#45652,#45653,#45654,#45655,#45656,
#45657,#45658,#45659,#45660,#45661,#45662,#45663,#45664,#45665,#45666,#45667,
#45668,#45669,#45670,#45671,#45672,#45673,#45674,#45675,#45676,#45677,#45678,
#45679,#45680,#45681,#45682,#45683,#45684,#45685,#45686,#45687,#45688,#45689,
#45690,#45691,#45692,#45693,#45694,#45695,#45696,#45697,#45698,#45699,#45700,
#45701,#45702,#45703,#45704,#45705,#45706,#45707,#45708,#45709,#45710,#45711,
#45712,#45713,#45714,#45715,#45716,#45717,#45718,#45719,#45720,#45721,#45722,
#45723,#45724,#45725,#45726,#45727,#45728,#45729,#45730,#45731,#45732,#45733),
 .UNSPECIFIED.,.F.,.F.,(4,2,2,2,2,2,2,2,2,2,2,2,2,2,2,2,2,2,2,2,2,2,2,2,
2,2,2,2,2,2,2,2,2,2,2,2,2,2,2,2,2,2,2,2,2,2,2,2,2,2,2,2,2,2,2,2,2,2,2,2,
2,2,2,2,2,2,2,2,2,2,2,2,2,2,2,2,2,2,2,2,2,2,2,2,2,2,2,2,2,2,2,2,2,2,2,2,
2,2,2,2,2,2,2,2,2,2,4),(-1.29810802178685,-1.27921968545388,-1.25740555526706,
-1.23913038927513,-1.23457302838182,-1.23190672518364,-1.22959893476656,
-1.22676847374173,-1.2213140342513,-1.17962531716193,-1.13908164133103,
-1.13451676629869,-1.13279266191125,-1.13156307978308,-1.13023314682969,
-1.12833945162829,-1.12355409597805,-1.11654090740784,-1.09463840588977,
-1.0436781063232,-1.03684524936847,-1.03378163402275,-1.03144086216804,
-1.02893478620726,-1.02498686655944,-1.01206414164423,-0.990174758022966,
-0.960432153605713,-0.954391929902206,-0.937617396760882,-0.934897699586889,
-0.933224903647788,-0.931928030582676,-0.930424431422591,-0.92772965350664,
-0.914459243445751,-0.882965176492135,-0.845615597736493,-0.838306231331341,
-0.835368303227181,-0.833198359625308,-0.830836242992282,-0.827591150025706,
-0.819908708757381,-0.809208565701869,-0.777869762669467,-0.741335846481875,
-0.736590370490525,-0.734648110946369,-0.733322144659396,-0.731940632363951,
-0.729798874527761,-0.723211649543973,-0.712383419186299,-0.658201778397501,
-0.641810645576294,-0.637345838904488,-0.634726400837247,-0.632645200840464,
-0.629858340402704,-0.624613627725498,-0.581988792211057,-0.542068460938666,
-0.537480744494982,-0.53575373735109,-0.534523436709312,-0.533194238350855,
-0.531304075073505,-0.526540631472104,-0.501635579523521,-0.46088752252969,
-0.443006830540535,-0.438482072609989,-0.435823246267246,-0.433514881573657,
-0.430674738472802,-0.425173053104665,-0.382423295479736,-0.343084514515821,
-0.338470607530021,-0.336740056333561,-0.335508758284075,-0.334180185378971,
-0.332293707319613,-0.327554064687245,-0.302907111397752,-0.259189159116442,
-0.243603092652693,-0.239224539240506,-0.236623827500584,-0.234539791031282,
-0.231782183630919,-0.226613675264722,-0.220084264009965,-0.205490397402259,
-0.171518442852611,-0.141918102513248,-0.138721093394758,-0.137090410452765,
-0.135796653401168,-0.134261898089649,-0.131422819245342,-0.115206972302946,
-0.0787110639488752,-0.0628294140565956,-0.0449915074260607,-0.0415745928430485),
 .UNSPECIFIED.);
#559=B_SPLINE_CURVE_WITH_KNOTS('',3,(#45739,#45740,#45741,#45742,#45743,
#45744,#45745,#45746,#45747,#45748,#45749,#45750,#45751,#45752,#45753,#45754,
#45755,#45756,#45757,#45758,#45759,#45760,#45761,#45762,#45763,#45764,#45765,
#45766,#45767,#45768,#45769,#45770,#45771,#45772,#45773,#45774,#45775,#45776,
#45777,#45778,#45779,#45780,#45781,#45782,#45783,#45784,#45785,#45786,#45787,
#45788,#45789,#45790,#45791,#45792,#45793,#45794,#45795,#45796,#45797,#45798,
#45799,#45800,#45801,#45802,#45803,#45804,#45805,#45806,#45807,#45808,#45809,
#45810,#45811,#45812,#45813,#45814,#45815,#45816,#45817,#45818,#45819,#45820,
#45821,#45822,#45823,#45824,#45825,#45826,#45827,#45828,#45829,#45830,#45831,
#45832,#45833,#45834,#45835,#45836,#45837,#45838,#45839,#45840,#45841,#45842,
#45843,#45844,#45845,#45846,#45847,#45848,#45849,#45850,#45851,#45852,#45853,
#45854,#45855,#45856,#45857,#45858,#45859,#45860,#45861,#45862,#45863,#45864,
#45865,#45866,#45867,#45868,#45869,#45870,#45871,#45872,#45873,#45874,#45875,
#45876,#45877,#45878,#45879,#45880,#45881,#45882,#45883,#45884,#45885,#45886,
#45887,#45888,#45889,#45890,#45891,#45892,#45893,#45894,#45895,#45896,#45897,
#45898,#45899,#45900,#45901,#45902,#45903,#45904,#45905,#45906,#45907,#45908,
#45909,#45910,#45911,#45912,#45913,#45914,#45915,#45916,#45917,#45918,#45919,
#45920,#45921,#45922,#45923,#45924,#45925,#45926,#45927,#45928,#45929,#45930,
#45931,#45932,#45933,#45934,#45935,#45936,#45937,#45938,#45939,#45940,#45941,
#45942,#45943,#45944,#45945,#45946,#45947,#45948,#45949,#45950),
 .UNSPECIFIED.,.F.,.F.,(4,2,2,2,2,2,2,2,2,2,2,2,2,2,2,2,2,2,2,2,2,2,2,2,
2,2,2,2,2,2,2,2,2,2,2,2,2,2,2,2,2,2,2,2,2,2,2,2,2,2,2,2,2,2,2,2,2,2,2,2,
2,2,2,2,2,2,2,2,2,2,2,2,2,2,2,2,2,2,2,2,2,2,2,2,2,2,2,2,2,2,2,2,2,2,2,2,
2,2,2,2,2,2,2,2,2,4),(-1.21635119563388,-1.21207693671559,-1.19844759531399,
-1.19587794698547,-1.19425035099548,-1.19295682588383,-1.19141972505711,
-1.18856944154117,-1.17208333925388,-1.11309186406727,-1.10098107335217,
-1.09698257431772,-1.0944656612982,-1.09212938763119,-1.0890399361622,-1.08224769086417,
-1.05418399880212,-1.01644351206329,-0.999686296433748,-0.996967468468187,
-0.995295017567689,-0.993998289871211,-0.992494718966433,-0.989799651530586,
-0.976520655133499,-0.944984061690785,-0.907692231951055,-0.90038466347107,
-0.897447591220026,-0.895278003603272,-0.892916007321181,-0.889670593564283,
-0.881985074577244,-0.871279020686648,-0.839907549747837,-0.803427769017373,
-0.7986811834416,-0.796738853724702,-0.795412967688485,-0.794031665585379,
-0.791890453571497,-0.785306640849499,-0.774485835176934,-0.720415292109332,
-0.703926583731855,-0.699453709753687,-0.696832666042673,-0.694751896931358,
-0.691967797231712,-0.686735487484548,-0.64551684598223,-0.604077088579714,
-0.599565585103356,-0.597848675202553,-0.596621137953344,-0.595289942912662,
-0.593388713075026,-0.588553985358996,-0.581444358726452,-0.559036431683413,
-0.508893290218511,-0.502661604160232,-0.499274297743984,-0.49690976655445,
-0.494491691723901,-0.49095549117952,-0.481377810867618,-0.46703959914776,
-0.409751164883505,-0.40156629560217,-0.399156747565236,-0.397715926037381,
-0.396404654981518,-0.394618485250298,-0.390482406086816,-0.371756048263399,
-0.324110396351523,-0.306076910972717,-0.301537001155339,-0.298874719136166,
-0.296566659625016,-0.29373110166172,-0.288251708739175,-0.244198789376967,
-0.206226513255702,-0.201550418454958,-0.199651325819143,-0.198332751277305,
-0.19712369071345,-0.195239451184165,-0.190233719447223,-0.182788182716142,
-0.158564860469068,-0.111171174588618,-0.10399933478888,-0.101157208042907,
-0.0987957852667561,-0.0963731207737606,-0.0928157729289583,-0.0830895012703083,
-0.0684493069859314,-0.0395665089118686,-0.00519260416459741,-0.00195456514998335,
-0.000894772399990085,-0.000582812181395608),.UNSPECIFIED.);
#560=B_SPLINE_CURVE_WITH_KNOTS('',3,(#45951,#45952,#45953,#45954,#45955,
#45956,#45957,#45958,#45959,#45960,#45961,#45962,#45963,#45964,#45965,#45966),
 .UNSPECIFIED.,.F.,.F.,(4,2,2,2,2,2,2,4),(-2.51378930048981,-2.51347511735793,
-2.51242511769801,-2.51119511618193,-2.509198543763,-2.50386821565292,-2.49916942911693,
-2.47295895309433),.UNSPECIFIED.);
#561=B_SPLINE_CURVE_WITH_KNOTS('',3,(#45968,#45969,#45970,#45971,#45972,
#45973,#45974,#45975,#45976,#45977,#45978,#45979,#45980,#45981,#45982,#45983),
 .UNSPECIFIED.,.F.,.F.,(4,2,2,2,2,2,2,4),(-0.0415745928430485,-0.0404697249184593,
-0.0378114675414129,-0.0355028788490026,-0.033286401809328,-0.0305091547635283,
-0.0262748328075838,-0.000581010966936684),.UNSPECIFIED.);
#562=B_SPLINE_CURVE_WITH_KNOTS('',3,(#45984,#45985,#45986,#45987,#45988,
#45989,#45990,#45991,#45992,#45993,#45994,#45995,#45996,#45997,#45998,#45999,
#46000,#46001,#46002,#46003,#46004,#46005,#46006,#46007,#46008,#46009,#46010,
#46011,#46012,#46013,#46014,#46015,#46016,#46017,#46018,#46019,#46020,#46021,
#46022,#46023,#46024,#46025,#46026,#46027,#46028,#46029,#46030,#46031,#46032,
#46033,#46034,#46035,#46036,#46037,#46038,#46039,#46040,#46041,#46042,#46043,
#46044,#46045,#46046,#46047,#46048,#46049,#46050,#46051,#46052,#46053,#46054,
#46055,#46056,#46057,#46058,#46059,#46060,#46061,#46062,#46063,#46064,#46065,
#46066,#46067,#46068,#46069,#46070,#46071,#46072,#46073,#46074,#46075,#46076,
#46077,#46078,#46079,#46080,#46081,#46082,#46083,#46084,#46085,#46086,#46087,
#46088,#46089,#46090,#46091,#46092,#46093,#46094,#46095,#46096,#46097,#46098,
#46099,#46100,#46101,#46102,#46103,#46104,#46105,#46106,#46107,#46108,#46109,
#46110,#46111,#46112,#46113,#46114,#46115,#46116,#46117,#46118,#46119,#46120,
#46121,#46122,#46123,#46124,#46125,#46126,#46127,#46128,#46129,#46130,#46131,
#46132,#46133,#46134,#46135,#46136,#46137,#46138,#46139,#46140,#46141,#46142,
#46143,#46144,#46145,#46146,#46147,#46148,#46149,#46150,#46151,#46152,#46153,
#46154,#46155,#46156,#46157,#46158,#46159,#46160,#46161,#46162,#46163,#46164,
#46165,#46166,#46167,#46168,#46169,#46170,#46171,#46172,#46173,#46174,#46175,
#46176,#46177,#46178,#46179,#46180,#46181,#46182,#46183,#46184,#46185,#46186,
#46187),.UNSPECIFIED.,.F.,.F.,(4,2,2,2,2,2,2,2,2,2,2,2,2,2,2,2,2,2,2,2,
2,2,2,2,2,2,2,2,2,2,2,2,2,2,2,2,2,2,2,2,2,2,2,2,2,2,2,2,2,2,2,2,2,2,2,2,
2,2,2,2,2,2,2,2,2,2,2,2,2,2,2,2,2,2,2,2,2,2,2,2,2,2,2,2,2,2,2,2,2,2,2,2,
2,2,2,2,2,2,2,2,2,4),(-2.51486360124677,-2.48403448716676,-2.45940953353798,
-2.45467126794229,-2.45278458334456,-2.4514556130955,-2.45022374120684,
-2.4484921160338,-2.44387308597346,-2.40461054723988,-2.38051108660902,
-2.36710296080089,-2.35803643117646,-2.35469104542183,-2.35252903686565,
-2.35018327990953,-2.34709395636076,-2.3401208102182,-2.28982035667201,
-2.26751988023639,-2.26042907836603,-2.2556037056259,-2.25370326378715,
-2.25237165648517,-2.25114296638613,-2.24942341637417,-2.24489669596251,
-2.2036451249633,-2.16257882785529,-2.15714412037568,-2.15431696599936,
-2.15223078681754,-2.14963748721678,-2.14529560393497,-2.13011299363908,
-2.07453448222296,-2.05828890689929,-2.0554473756231,-2.05391162340847,
-2.05261721713411,-2.05098596671736,-2.04778858253313,-2.01879006596697,
-1.98665963626305,-1.97056016401614,-1.96357182846481,-1.95806431332904,
-1.95522196527578,-1.95291220141417,-1.95025219941751,-1.94572649715321,
-1.92785973427864,-1.88702599408337,-1.86209738422806,-1.85733049396155,
-1.85543908995706,-1.85410906846883,-1.85287804180157,-1.85115007668674,
-1.84656006016643,-1.80663506731546,-1.76432930337709,-1.75888592787529,
-1.75605678149165,-1.75374785620934,-1.75107777205386,-1.74650788670798,
-1.72808338397844,-1.68070786973389,-1.66684723767386,-1.66160951953553,
-1.65778232774098,-1.6560507619294,-1.65474664477987,-1.65327726100032,
-1.65074119392919,-1.64132371175794,-1.57957476062324,-1.56308307315322,
-1.55879889922861,-1.5562182430151,-1.55389772104179,-1.55093455602256,
-1.5461962745907,-1.50671247433801,-1.47794789754119,-1.46092342575762,
-1.45805028099995,-1.45650786442857,-1.45521400168965,-1.45359120108154,
-1.45043300679088,-1.42726983135739,-1.38359092894409,-1.36437053185251,
-1.35988241854872,-1.35725698896054,-1.35494388063394,-1.3520538140911,
-1.34755704445447,-1.32311316954842,-1.29859447736914),.UNSPECIFIED.);
#563=B_SPLINE_CURVE_WITH_KNOTS('',3,(#46192,#46193,#46194,#46195,#46196,
#46197,#46198,#46199,#46200,#46201,#46202,#46203,#46204,#46205,#46206,#46207,
#46208,#46209,#46210,#46211,#46212,#46213,#46214,#46215,#46216,#46217,#46218,
#46219,#46220,#46221,#46222,#46223,#46224,#46225,#46226,#46227,#46228,#46229,
#46230,#46231,#46232,#46233,#46234,#46235,#46236,#46237,#46238,#46239,#46240,
#46241,#46242,#46243,#46244,#46245,#46246,#46247,#46248,#46249,#46250,#46251,
#46252,#46253,#46254,#46255,#46256,#46257,#46258,#46259,#46260,#46261,#46262,
#46263,#46264,#46265,#46266,#46267,#46268,#46269,#46270,#46271,#46272,#46273,
#46274,#46275,#46276,#46277,#46278,#46279,#46280,#46281,#46282,#46283,#46284,
#46285,#46286,#46287,#46288,#46289,#46290,#46291,#46292,#46293,#46294,#46295,
#46296,#46297,#46298,#46299,#46300,#46301,#46302,#46303,#46304,#46305,#46306,
#46307,#46308,#46309,#46310,#46311,#46312,#46313,#46314,#46315,#46316,#46317,
#46318,#46319,#46320,#46321,#46322,#46323,#46324,#46325,#46326,#46327,#46328,
#46329,#46330,#46331,#46332,#46333,#46334,#46335,#46336,#46337,#46338,#46339,
#46340,#46341,#46342,#46343,#46344,#46345,#46346,#46347,#46348,#46349,#46350,
#46351,#46352,#46353,#46354,#46355,#46356,#46357,#46358,#46359,#46360,#46361,
#46362,#46363,#46364,#46365,#46366,#46367,#46368,#46369,#46370,#46371,#46372,
#46373,#46374,#46375,#46376,#46377,#46378,#46379,#46380,#46381,#46382,#46383,
#46384,#46385,#46386,#46387,#46388,#46389,#46390,#46391,#46392,#46393,#46394,
#46395,#46396,#46397,#46398,#46399,#46400,#46401),.UNSPECIFIED.,.F.,.F.,
(4,2,2,2,2,2,2,2,2,2,2,2,2,2,2,2,2,2,2,2,2,2,2,2,2,2,2,2,2,2,2,2,2,2,2,
2,2,2,2,2,2,2,2,2,2,2,2,2,2,2,2,2,2,2,2,2,2,2,2,2,2,2,2,2,2,2,2,2,2,2,2,
2,2,2,2,2,2,2,2,2,2,2,2,2,2,2,2,2,2,2,2,2,2,2,2,2,2,2,2,2,2,2,2,2,4),(-2.47309949534992,
-2.47127547339437,-2.45596006103672,-2.40491628643083,-2.39650863763585,
-2.39102905683977,-2.38903204129656,-2.387681681759,-2.38647312092219,-2.38451655599,
-2.37968473310878,-2.34873412281988,-2.32256922059027,-2.30553640783741,
-2.29827512753788,-2.29264198515644,-2.28979067358952,-2.28752610877192,
-2.28493184131325,-2.28058202631575,-2.26531082848368,-2.20986465472809,
-2.19363535655162,-2.19079553552778,-2.18926058893448,-2.18796679075073,
-2.18633621672529,-2.18313989340236,-2.15500002971538,-2.14261097198826,
-2.09858912234754,-2.09329500086617,-2.09049757612045,-2.08841510342249,
-2.08580273203755,-2.0813713009813,-2.06523230300893,-2.01636580159925,
-1.99675119591292,-1.99251736917353,-1.99071416212996,-1.98940007293583,
-1.98796647751316,-1.98558996315499,-1.97770421885991,-1.91429458288821,
-1.9033265672142,-1.89549651655011,-1.89222689205334,-1.88986038948655,
-1.88769568549551,-1.88477887864323,-1.87762391498049,-1.83233270826694,
-1.79710198034846,-1.79323600267408,-1.7914979399305,-1.79019359028901,
-1.78872909218208,-1.78621279111138,-1.77699129438329,-1.71507102457687,
-1.69857269557366,-1.69428966290926,-1.69171020055042,-1.68939107364854,
-1.68643013346672,-1.68169630883242,-1.64216279367231,-1.61325631853494,
-1.59645466063384,-1.59359163290892,-1.59205190488581,-1.59075867741116,
-1.58913462970404,-1.58596806924658,-1.56197965001694,-1.52371842417782,
-1.50831703627055,-1.50153991034737,-1.49616569710578,-1.49335192528585,
-1.49126810996243,-1.48866807496836,-1.48429162041681,-1.46872416729493,
-1.41360197174489,-1.3973997909313,-1.39456123801109,-1.39302661330261,
-1.39173286921736,-1.39010208809483,-1.38690454782772,-1.35708558526728,
-1.31884710612772,-1.30080077525413,-1.29639700584974,-1.29379077646065,
-1.29147608003524,-1.28855932084928,-1.28397261106968,-1.25702096238711,
-1.2318851758174,-1.21887035561419,-1.21635119563388),.UNSPECIFIED.);
#564=B_SPLINE_CURVE_WITH_KNOTS('',3,(#46402,#46403,#46404,#46405,#46406,
#46407,#46408,#46409,#46410,#46411,#46412,#46413,#46414,#46415,#46416,#46417,
#46418,#46419,#46420,#46421,#46422,#46423,#46424,#46425,#46426,#46427,#46428,
#46429,#46430,#46431,#46432,#46433,#46434,#46435,#46436,#46437,#46438,#46439,
#46440,#46441,#46442,#46443,#46444,#46445,#46446,#46447,#46448,#46449,#46450,
#46451,#46452,#46453,#46454,#46455,#46456,#46457,#46458,#46459,#46460,#46461,
#46462,#46463,#46464,#46465,#46466,#46467,#46468,#46469,#46470,#46471,#46472,
#46473,#46474,#46475,#46476,#46477,#46478,#46479,#46480,#46481,#46482,#46483,
#46484,#46485,#46486,#46487,#46488,#46489,#46490,#46491,#46492,#46493,#46494,
#46495,#46496,#46497,#46498,#46499,#46500,#46501,#46502,#46503,#46504,#46505,
#46506,#46507,#46508,#46509,#46510,#46511,#46512,#46513,#46514,#46515,#46516,
#46517,#46518,#46519,#46520,#46521,#46522,#46523,#46524,#46525,#46526,#46527,
#46528,#46529,#46530,#46531,#46532,#46533,#46534,#46535,#46536,#46537,#46538,
#46539,#46540,#46541,#46542,#46543,#46544,#46545,#46546,#46547,#46548,#46549,
#46550,#46551,#46552,#46553,#46554,#46555,#46556,#46557,#46558,#46559,#46560,
#46561,#46562,#46563,#46564,#46565,#46566,#46567,#46568,#46569,#46570,#46571,
#46572,#46573,#46574,#46575,#46576,#46577,#46578,#46579,#46580,#46581,#46582,
#46583,#46584,#46585,#46586,#46587,#46588,#46589,#46590,#46591,#46592,#46593,
#46594,#46595,#46596,#46597,#46598,#46599,#46600,#46601,#46602,#46603,#46604,
#46605,#46606,#46607,#46608,#46609,#46610,#46611,#46612,#46613,#46614,#46615,
#46616,#46617,#46618,#46619,#46620,#46621,#46622,#46623,#46624,#46625,#46626,
#46627,#46628,#46629,#46630,#46631),.UNSPECIFIED.,.F.,.F.,(4,2,2,2,2,2,
2,2,2,2,2,2,2,2,2,2,2,2,2,2,2,2,2,2,2,2,2,2,2,2,2,2,2,2,2,2,2,2,2,2,2,2,
2,2,2,2,2,2,2,2,2,2,2,2,2,2,2,2,2,2,2,2,2,2,2,2,2,2,2,2,2,2,2,2,2,2,2,2,
2,2,2,2,2,2,2,2,2,2,2,2,2,2,2,2,2,2,2,2,2,2,2,2,2,2,2,2,2,2,2,2,2,2,2,2,
4),(-1.29859447736914,-1.28129283734518,-1.26820788588034,-1.2631684333074,
-1.25945426865517,-1.25774374785694,-1.25644235569197,-1.25496132484305,
-1.25237185122733,-1.24082785893824,-1.21516384004797,-1.16979233478358,
-1.162639221935,-1.15972194754688,-1.15755644932196,-1.15518864174769,-1.15191642406315,
-1.1440763531082,-1.13309031562372,-1.06942196452236,-1.06170599567376,
-1.0593480342408,-1.05791807363478,-1.05660155986945,-1.05478690255315,
-1.05048942982765,-1.03029546681689,-0.978697638071059,-0.965382691780355,
-0.961240019357399,-0.958690243456607,-0.95636193703801,-0.953338548582027,
-0.946910346128419,-0.921731856699086,-0.888847539858425,-0.864065687375207,
-0.860886464234897,-0.859259032453427,-0.857964765139316,-0.856425750023858,
-0.853569203110952,-0.836963675480725,-0.776223441941107,-0.765537558119888,
-0.761724595605466,-0.759494709965725,-0.757165137336825,-0.754130468325904,
-0.747640946311518,-0.721989899614708,-0.68730331149973,-0.681821045869953,
-0.677837000456514,-0.664290686584514,-0.661724609722285,-0.660097688471191,
-0.658803613579935,-0.657264574536392,-0.654407318071632,-0.637777125920965,
-0.576594586152884,-0.566277214713519,-0.562516695795688,-0.5602971750145,
-0.557963746862912,-0.554899642784734,-0.548250413348906,-0.52134826547736,
-0.490388923078804,-0.465763674943844,-0.462587198713617,-0.460960615809743,
-0.459666727180571,-0.458127811600798,-0.455270526206553,-0.438632178116423,
-0.377279559925415,-0.3671078915294,-0.36336875654538,-0.361153567188859,
-0.358818646675264,-0.355742441571501,-0.349026011748525,-0.321584123080141,
-0.295621854099429,-0.266687527647133,-0.263490946993484,-0.261860210784585,
-0.260566267907173,-0.259031122765637,-0.256190880536305,-0.239955303435136,
-0.184399156138189,-0.169244673385418,-0.16490679653023,-0.162314912300009,
-0.160229323722529,-0.160187496920376,-0.160147215561924,-0.160108385173283,
-0.160070918697468,-0.157225475235737,-0.15169789706795,-0.144559425541735,
-0.127947301775496,-0.106655130377444,-0.0699756605761903,-0.0652331800173265,
-0.0632912907347226,-0.0619652915547201,-0.0605834626182379,-0.0584407227816428,
-0.051846602696853,-0.0412924016477382),.UNSPECIFIED.);
#565=B_SPLINE_CURVE_WITH_KNOTS('',3,(#46637,#46638,#46639,#46640,#46641,
#46642,#46643,#46644,#46645,#46646,#46647,#46648,#46649,#46650,#46651,#46652,
#46653,#46654,#46655,#46656,#46657,#46658,#46659,#46660,#46661,#46662,#46663,
#46664,#46665,#46666,#46667,#46668,#46669,#46670,#46671,#46672,#46673,#46674,
#46675,#46676,#46677,#46678,#46679,#46680,#46681,#46682,#46683,#46684,#46685,
#46686,#46687,#46688,#46689,#46690,#46691,#46692,#46693,#46694,#46695,#46696,
#46697,#46698,#46699,#46700,#46701,#46702,#46703,#46704,#46705,#46706,#46707,
#46708,#46709,#46710,#46711,#46712,#46713,#46714,#46715,#46716,#46717,#46718,
#46719,#46720,#46721,#46722,#46723,#46724,#46725,#46726,#46727,#46728,#46729,
#46730,#46731,#46732,#46733,#46734,#46735,#46736,#46737,#46738,#46739,#46740,
#46741,#46742,#46743,#46744,#46745,#46746,#46747,#46748,#46749,#46750,#46751,
#46752,#46753,#46754,#46755,#46756,#46757,#46758,#46759,#46760,#46761,#46762,
#46763,#46764,#46765,#46766,#46767,#46768,#46769,#46770,#46771,#46772,#46773,
#46774,#46775,#46776,#46777,#46778,#46779,#46780,#46781,#46782,#46783,#46784,
#46785,#46786,#46787,#46788,#46789,#46790,#46791,#46792,#46793,#46794,#46795,
#46796,#46797,#46798,#46799,#46800,#46801,#46802,#46803,#46804,#46805,#46806,
#46807,#46808,#46809,#46810,#46811,#46812,#46813,#46814,#46815,#46816,#46817,
#46818,#46819,#46820,#46821,#46822,#46823,#46824,#46825,#46826,#46827,#46828,
#46829,#46830,#46831,#46832,#46833,#46834,#46835,#46836,#46837,#46838,#46839,
#46840,#46841,#46842,#46843,#46844,#46845,#46846,#46847,#46848,#46849,#46850),
 .UNSPECIFIED.,.F.,.F.,(4,2,2,2,2,2,2,2,2,2,2,2,2,2,2,2,2,2,2,2,2,2,2,2,
2,2,2,2,2,2,2,2,2,2,2,2,2,2,2,2,2,2,2,2,2,2,2,2,2,2,2,2,2,2,2,2,2,2,2,2,
2,2,2,2,2,2,2,2,2,2,2,2,2,2,2,2,2,2,2,2,2,2,2,2,2,2,2,2,2,2,2,2,2,2,2,2,
2,2,2,2,2,2,2,2,2,2,4),(-1.21647209020946,-1.20589754521165,-1.17728609578228,
-1.17264689952674,-1.1697137667687,-1.16739678821615,-1.16479923697488,
-1.16043729128841,-1.14296139717832,-1.10880317286871,-1.09664657958352,
-1.09359574351831,-1.08782688556157,-1.07362109533104,-1.07102075317838,
-1.06938357257115,-1.06808910253175,-1.06655872237724,-1.06374126600813,
-1.04803646139591,-0.998223915396606,-0.977575769909869,-0.972853143571639,
-0.970148711929969,-0.967864416501892,-0.965087923199884,-0.959895474988632,
-0.921988001161925,-0.881110384082842,-0.873542277167189,-0.871202010586539,
-0.869776299564524,-0.868458714016256,-0.866635502902323,-0.862285213711711,
-0.841584302635778,-0.781913120280027,-0.774961987239186,-0.771876960211157,
-0.769532311194114,-0.767034120193988,-0.763123862939929,-0.750552668497476,
-0.729540240789816,-0.692915539454742,-0.689092808822501,-0.675376451790558,
-0.672801756170647,-0.671172440856944,-0.669878557342289,-0.668342221213909,
-0.665496475777756,-0.649130957240392,-0.591892213373294,-0.578244083325774,
-0.574065535528693,-0.571508697372987,-0.569183762550786,-0.566178680668933,
-0.559842405967283,-0.53534628654806,-0.493815537298598,-0.489903610915842,
-0.476285836237096,-0.473716544678314,-0.472088936057674,-0.47079523786801,
-0.469257738613073,-0.466406210156904,-0.449897471486241,-0.390592061796495,
-0.378739380276266,-0.374772798373961,-0.372262637225479,-0.369923422814105,
-0.366816339259474,-0.359928228156171,-0.331080622654647,-0.296216517854237,
-0.292222645233031,-0.277342208287288,-0.274709165460133,-0.273062352041594,
-0.271767585211212,-0.270245401868124,-0.267464838261181,-0.252545203241682,
-0.209212567071252,-0.181880435471606,-0.177266988788374,-0.174342167002432,
-0.172026731425725,-0.169527458724321,-0.165387238678503,-0.160407971473687,
-0.150490071467178,-0.122941966355962,-0.0808072168409335,-0.076350980466186,
-0.074641486042469,-0.0734157974432842,-0.0720826928009046,-0.0701722454890665,
-0.0652792612178099,-0.0580560680089516,-0.0350476812884346,-0.000583285542807006),
 .UNSPECIFIED.);
#566=B_SPLINE_CURVE_WITH_KNOTS('',3,(#46851,#46852,#46853,#46854,#46855,
#46856,#46857,#46858,#46859,#46860,#46861,#46862,#46863,#46864,#46865,#46866,
#46867,#46868),.UNSPECIFIED.,.F.,.F.,(4,2,2,2,2,2,2,2,4),(-2.51402391418862,
-2.50161511808339,-2.49426729550675,-2.49130566087207,-2.48903181552238,
-2.48681378261952,-2.48461343489582,-2.48094913905227,-2.47309949534992),
 .UNSPECIFIED.);
#567=B_SPLINE_CURVE_WITH_KNOTS('',3,(#46870,#46871,#46872,#46873),
 .UNSPECIFIED.,.F.,.F.,(4,4),(-0.0412924016477382,-0.00058319047411503),
 .UNSPECIFIED.);
#568=B_SPLINE_CURVE_WITH_KNOTS('',3,(#46874,#46875,#46876,#46877,#46878,
#46879,#46880,#46881,#46882,#46883,#46884,#46885,#46886,#46887,#46888,#46889,
#46890,#46891,#46892,#46893,#46894,#46895,#46896,#46897,#46898,#46899,#46900,
#46901,#46902,#46903,#46904,#46905,#46906,#46907,#46908,#46909,#46910,#46911,
#46912,#46913,#46914,#46915,#46916,#46917,#46918,#46919,#46920,#46921,#46922,
#46923,#46924,#46925,#46926,#46927,#46928,#46929,#46930,#46931,#46932,#46933,
#46934,#46935,#46936,#46937,#46938,#46939,#46940,#46941,#46942,#46943,#46944,
#46945,#46946,#46947,#46948,#46949,#46950,#46951,#46952,#46953,#46954,#46955,
#46956,#46957,#46958,#46959,#46960,#46961,#46962,#46963,#46964,#46965,#46966,
#46967,#46968,#46969,#46970,#46971,#46972,#46973,#46974,#46975,#46976,#46977,
#46978,#46979,#46980,#46981,#46982,#46983,#46984,#46985,#46986,#46987,#46988,
#46989,#46990,#46991,#46992,#46993,#46994,#46995,#46996,#46997,#46998,#46999,
#47000,#47001,#47002,#47003,#47004,#47005,#47006,#47007,#47008,#47009,#47010,
#47011,#47012,#47013,#47014,#47015,#47016,#47017,#47018,#47019,#47020,#47021,
#47022,#47023,#47024,#47025,#47026,#47027,#47028,#47029,#47030,#47031,#47032,
#47033,#47034,#47035,#47036,#47037,#47038,#47039,#47040,#47041,#47042,#47043,
#47044,#47045,#47046,#47047,#47048,#47049,#47050,#47051,#47052,#47053,#47054,
#47055,#47056,#47057,#47058,#47059,#47060,#47061,#47062,#47063,#47064,#47065,
#47066,#47067,#47068,#47069,#47070,#47071,#47072,#47073,#47074,#47075,#47076,
#47077,#47078,#47079,#47080,#47081,#47082,#47083,#47084,#47085,#47086,#47087,
#47088,#47089,#47090,#47091,#47092,#47093,#47094,#47095,#47096,#47097,#47098,
#47099,#47100,#47101,#47102,#47103,#47104,#47105,#47106,#47107,#47108,#47109,
#47110,#47111,#47112,#47113),.UNSPECIFIED.,.F.,.F.,(4,2,2,2,2,2,2,2,2,2,
2,2,2,2,2,2,2,2,2,2,2,2,2,2,2,2,2,2,2,2,2,2,2,2,2,2,2,2,2,2,2,2,2,2,2,2,
2,2,2,2,2,2,2,2,2,2,2,2,2,2,2,2,2,2,2,2,2,2,2,2,2,2,2,2,2,2,2,2,2,2,2,2,
2,2,2,2,2,2,2,2,2,2,2,2,2,2,2,2,2,2,2,2,2,2,2,2,2,2,2,2,2,2,2,2,2,2,2,2,
2,4),(-2.51466580210535,-2.48688043602376,-2.48277505446942,-2.48005091685726,
-2.47784835815228,-2.47556362045631,-2.47286451274943,-2.46816601787414,
-2.44788520736209,-2.43123540376619,-2.39822109209008,-2.38199005697294,
-2.37914957060266,-2.3776142267035,-2.37632007114578,-2.37468901830606,
-2.37149167276508,-2.34203292298677,-2.30698665792291,-2.29296590346264,
-2.28661466642606,-2.28156095138116,-2.27882637395884,-2.27880121072071,
-2.27877556151567,-2.27874941389501,-2.27872275507702,-2.27869557186183,
-2.27867790142337,-2.27865859030209,-2.27863748217226,-2.27861440508373,
-2.27858916990709,-2.27856156847561,-2.27853137153467,-2.27849832659295,
-2.2784621552807,-2.27842255072964,-2.27837917458935,-2.27833165364839,
-2.2782795759228,-2.2782362568903,-2.27816849121875,-2.27806256515577,-2.27572531069299,
-2.2726878408054,-2.26600358860942,-2.21372177780222,-2.18363399095287,
-2.18034140120792,-2.1787124315905,-2.17754261698338,-2.17605547546703,
-2.17350518619371,-2.1636065206156,-2.10238719054798,-2.08593977255182,
-2.08165972058762,-2.07908023978216,-2.07675994361423,-2.07379591987535,
-2.06905393715311,-2.02967739097466,-2.00112346715458,-1.98382227877162,
-1.98093875177067,-1.97939428168329,-1.97810076280821,-1.97648099236103,
-1.97333620040045,-1.95168560699098,-1.89917127732409,-1.88620410615282,
-1.88225086801538,-1.87974324891727,-1.87740230765782,-1.87434030136554,
-1.86751886251849,-1.81639903645351,-1.78569005745561,-1.78219212378759,
-1.78052287570537,-1.77923766987557,-1.7777354265077,-1.77511904348417,
-1.76444159799782,-1.70405503714433,-1.68767854334814,-1.68340466630013,
-1.68082672169296,-1.67850641648367,-1.67554045928842,-1.67079147746974,
-1.6366133362829,-1.59931894013552,-1.58532429091377,-1.58258963623933,
-1.58107717856096,-1.57978108284506,-1.57812019096764,-1.57544095440127,
-1.5596530589867,-1.52414295979256,-1.49330714115335,-1.48618344248167,
-1.48303394117644,-1.48068764341093,-1.47819318793872,-1.47430020272724,
-1.46302056253795,-1.41965460667862,-1.38992742748971,-1.38474642238979,
-1.38279217985026,-1.38145025889512,-1.38023340354888,-1.37855843139856,
-1.37431868058543,-1.33008093193916,-1.29825834795597),.UNSPECIFIED.);
#569=B_SPLINE_CURVE_WITH_KNOTS('',3,(#47118,#47119,#47120,#47121,#47122,
#47123,#47124,#47125,#47126,#47127,#47128,#47129,#47130,#47131,#47132,#47133,
#47134,#47135,#47136,#47137,#47138,#47139,#47140,#47141,#47142,#47143,#47144,
#47145,#47146,#47147,#47148,#47149,#47150,#47151,#47152,#47153,#47154,#47155,
#47156,#47157,#47158,#47159,#47160,#47161,#47162,#47163,#47164,#47165,#47166,
#47167,#47168,#47169,#47170,#47171,#47172,#47173,#47174,#47175,#47176,#47177,
#47178,#47179,#47180,#47181,#47182,#47183,#47184,#47185,#47186,#47187,#47188,
#47189,#47190,#47191,#47192,#47193,#47194,#47195,#47196,#47197,#47198,#47199,
#47200,#47201,#47202,#47203,#47204,#47205,#47206,#47207,#47208,#47209,#47210,
#47211,#47212,#47213,#47214,#47215,#47216,#47217,#47218,#47219,#47220,#47221,
#47222,#47223,#47224,#47225,#47226,#47227,#47228,#47229,#47230,#47231,#47232,
#47233,#47234,#47235,#47236,#47237,#47238,#47239,#47240,#47241,#47242,#47243,
#47244,#47245,#47246,#47247,#47248,#47249,#47250,#47251,#47252,#47253,#47254,
#47255,#47256,#47257,#47258,#47259,#47260,#47261,#47262,#47263,#47264,#47265,
#47266,#47267,#47268,#47269,#47270,#47271,#47272,#47273,#47274,#47275,#47276,
#47277,#47278,#47279,#47280,#47281,#47282,#47283,#47284,#47285,#47286,#47287,
#47288,#47289,#47290,#47291,#47292,#47293,#47294,#47295,#47296,#47297,#47298,
#47299,#47300,#47301,#47302,#47303,#47304,#47305,#47306,#47307,#47308,#47309,
#47310,#47311,#47312,#47313,#47314,#47315,#47316,#47317,#47318,#47319,#47320,
#47321,#47322,#47323,#47324,#47325,#47326,#47327,#47328,#47329,#47330,#47331,
#47332,#47333,#47334,#47335,#47336,#47337,#47338,#47339,#47340,#47341),
 .UNSPECIFIED.,.F.,.F.,(4,2,2,2,2,2,2,2,2,2,2,2,2,2,2,2,2,2,2,2,2,2,2,2,
2,2,2,2,2,2,2,2,2,2,2,2,2,2,2,2,2,2,2,2,2,2,2,2,2,2,2,2,2,2,2,2,2,2,2,2,
2,2,2,2,2,2,2,2,2,2,2,2,2,2,2,2,2,2,2,2,2,2,2,2,2,2,2,2,2,2,2,2,2,2,2,2,
2,2,2,2,2,2,2,2,2,2,2,2,2,2,2,4),(-2.4734065574123,-2.47297094298435,-2.46819529786363,
-2.46570077595541,-2.46356993923343,-2.46219069903809,-2.46086279749131,
-2.45891133447964,-2.45411149328566,-2.41957982033227,-2.39731631674372,
-2.37192125438772,-2.36680120692414,-2.36450853056401,-2.36216850816659,
-2.35965931269944,-2.35569815671919,-2.34389108645553,-2.30261089368116,
-2.27161104047677,-2.2663939033618,-2.26439611016055,-2.26304535843778,
-2.26183654803884,-2.2598797668444,-2.2550483480496,-2.2224529611183,-2.1886717061223,
-2.17720764647332,-2.16910831427439,-2.16579433853441,-2.16341932628676,
-2.16126284188574,-2.15783926750935,-2.15147425401397,-2.10279534521424,
-2.07054523797849,-2.06670121460668,-2.06496693257838,-2.06366284590181,
-2.062195794547,-2.05966883269793,-2.05034059131633,-1.98852054316546,-1.97202744021389,
-1.96774419256317,-1.96516432295667,-1.96284465350098,-1.95988277733525,
-1.95514696292316,-1.91564611785823,-1.88704685311041,-1.86991096625504,
-1.86703424787001,-1.86549140296358,-1.86419805741198,-1.86257700882889,
-1.86002925029812,-1.84679845275327,-1.83938011510562,-1.82656853589027,
-1.80145622565971,-1.77658074803303,-1.77019356539879,-1.76717876093513,
-1.76485248085871,-1.76230034545287,-1.75814350271749,-1.74469187152918,
-1.68719789561958,-1.6708084491133,-1.6679614382322,-1.66642475992443,-1.66513078620306,
-1.66350161623062,-1.66031282125465,-1.63454604213219,-1.60799301556141,
-1.58618626350811,-1.57329380082639,-1.56934835693358,-1.56684230940579,
-1.56450048853119,-1.56143394646554,-1.55458797190715,-1.50367731083793,
-1.48170022316211,-1.47467177393256,-1.46987857180819,-1.46798328022903,
-1.46665274259573,-1.46542301038193,-1.4636992611816,-1.45913961508351,
-1.41890134726393,-1.41680857109891,-1.37718360549119,-1.37156448972294,
-1.3686998114636,-1.3663889940198,-1.36374653607847,-1.35929561310345,-1.3423972858068,
-1.29381662297137,-1.27470587676728,-1.27052657001854,-1.2687324676093,
-1.26741955150624,-1.26616162001951,-1.26395179797613,-1.25742858636991,
-1.21647209020946),.UNSPECIFIED.);
#570=B_SPLINE_CURVE_WITH_KNOTS('',3,(#47342,#47343,#47344,#47345,#47346,
#47347,#47348,#47349,#47350,#47351,#47352,#47353,#47354,#47355,#47356,#47357,
#47358,#47359,#47360,#47361,#47362,#47363,#47364,#47365,#47366,#47367,#47368,
#47369,#47370,#47371,#47372,#47373,#47374,#47375,#47376,#47377,#47378,#47379,
#47380,#47381,#47382,#47383,#47384,#47385,#47386,#47387,#47388,#47389,#47390,
#47391,#47392,#47393,#47394,#47395,#47396,#47397,#47398,#47399,#47400,#47401,
#47402,#47403,#47404,#47405,#47406,#47407,#47408,#47409,#47410,#47411,#47412,
#47413,#47414,#47415,#47416,#47417,#47418,#47419,#47420,#47421,#47422,#47423,
#47424,#47425,#47426,#47427,#47428,#47429,#47430,#47431,#47432,#47433,#47434,
#47435,#47436,#47437,#47438,#47439,#47440,#47441,#47442,#47443,#47444,#47445,
#47446,#47447,#47448,#47449,#47450,#47451,#47452,#47453,#47454,#47455,#47456,
#47457,#47458,#47459,#47460,#47461,#47462,#47463,#47464,#47465,#47466,#47467,
#47468,#47469,#47470,#47471,#47472,#47473,#47474,#47475,#47476,#47477,#47478,
#47479,#47480,#47481,#47482,#47483,#47484,#47485,#47486,#47487,#47488,#47489,
#47490,#47491,#47492,#47493,#47494,#47495,#47496,#47497,#47498,#47499,#47500,
#47501,#47502,#47503,#47504,#47505,#47506,#47507,#47508,#47509,#47510,#47511,
#47512,#47513,#47514,#47515,#47516,#47517,#47518,#47519,#47520,#47521,#47522,
#47523,#47524,#47525,#47526,#47527,#47528,#47529,#47530,#47531,#47532,#47533,
#47534,#47535,#47536,#47537,#47538,#47539,#47540,#47541,#47542,#47543,#47544,
#47545,#47546,#47547,#47548,#47549,#47550,#47551,#47552,#47553,#47554,#47555,
#47556,#47557,#47558,#47559,#47560,#47561,#47562,#47563,#47564,#47565,#47566,
#47567,#47568,#47569,#47570,#47571,#47572,#47573,#47574,#47575,#47576,#47577,
#47578,#47579),.UNSPECIFIED.,.F.,.F.,(4,2,2,2,2,2,2,2,2,2,2,2,2,2,2,2,2,
2,2,2,2,2,2,2,2,2,2,2,2,2,2,2,2,2,2,2,2,2,2,2,2,2,2,2,2,2,2,2,2,2,2,2,2,
2,2,2,2,2,2,2,2,2,2,2,2,2,2,2,2,2,2,2,2,2,2,2,2,2,2,2,2,2,2,2,2,2,2,2,2,
2,2,2,2,2,2,2,2,2,2,2,2,2,2,2,2,2,2,2,2,2,2,2,2,2,2,2,2,2,4),(-1.29825834795597,
-1.29123229092342,-1.28602653061877,-1.28324731967477,-1.28116624603691,
-1.27853959641259,-1.27404412637148,-1.25730238843777,-1.22458933826295,
-1.19048854204325,-1.18567886039837,-1.18372563591847,-1.18251742264463,
-1.18116576825898,-1.17916390624951,-1.17365253509172,-1.16518073419774,
-1.1046732911913,-1.09040568752403,-1.08615969824611,-1.08358801057558,
-1.08126657320199,-1.0782897747918,-1.07210141763832,-1.04869905839798,
-1.02244590874265,-0.991437463326771,-0.986604499062264,-0.98464753312995,
-0.98343874508643,-0.982088148423329,-0.980090820162957,-0.974610538158568,
-0.966202942906196,-0.936106345915818,-0.896617770542071,-0.889303357891865,
-0.886359127148623,-0.884187423377715,-0.881826185490253,-0.878587373419486,
-0.870943890916088,-0.860314813266051,-0.829341363081878,-0.792290315776044,
-0.787553784610154,-0.785612862203943,-0.784287032959841,-0.782904896261069,
-0.780760835209874,-0.774155979058116,-0.763287687444722,-0.708443228461425,
-0.692639211776866,-0.68823984302026,-0.685634550525839,-0.683551169459506,
-0.680744019251714,-0.675402913302647,-0.632480468576317,-0.593034951823787,
-0.588426491595111,-0.586696601157218,-0.585465433331811,-0.584136622106021,
-0.582249183658804,-0.577503904549001,-0.552798002155749,-0.512281684402921,
-0.493995753103682,-0.489437230267483,-0.486770463735911,-0.484462403020355,
-0.481631776240677,-0.476177541548953,-0.469272896926145,-0.453448973639084,
-0.416407945837161,-0.391843153536159,-0.388662103396604,-0.387034752223112,
-0.385741088598687,-0.384203429399182,-0.381351076316759,-0.364821427219705,
-0.305192063682197,-0.293613971076619,-0.289682514395162,-0.287180055190972,
-0.284837889688967,-0.281711620366249,-0.274716410776126,-0.244971085234562,
-0.213389191432959,-0.192666474932515,-0.189556669796834,-0.187944726748438,
-0.18669092098631,-0.186683178564903,-0.186675500392306,-0.186667885331728,
-0.186660332243027,-0.186652840091513,-0.186645407650691,-0.186638033859088,
-0.186630717608753,-0.185102328142878,-0.183441804139831,-0.180803067062052,
-0.175631169124425,-0.162027308915024,-0.11606608232098,-0.0961395206307786,
-0.0914679593369492,-0.088775632090244,-0.0864915565936915,-0.0837030370058112,
-0.0784507275611289,-0.041493788302871),.UNSPECIFIED.);
#571=B_SPLINE_CURVE_WITH_KNOTS('',3,(#47585,#47586,#47587,#47588,#47589,
#47590,#47591,#47592,#47593,#47594,#47595,#47596,#47597,#47598,#47599,#47600,
#47601,#47602,#47603,#47604,#47605,#47606,#47607,#47608,#47609,#47610,#47611,
#47612,#47613,#47614,#47615,#47616,#47617,#47618,#47619,#47620,#47621,#47622,
#47623,#47624,#47625,#47626,#47627,#47628,#47629,#47630,#47631,#47632,#47633,
#47634,#47635,#47636,#47637,#47638,#47639,#47640,#47641,#47642,#47643,#47644,
#47645,#47646,#47647,#47648,#47649,#47650,#47651,#47652,#47653,#47654,#47655,
#47656,#47657,#47658,#47659,#47660,#47661,#47662,#47663,#47664,#47665,#47666,
#47667,#47668,#47669,#47670,#47671,#47672,#47673,#47674,#47675,#47676,#47677,
#47678,#47679,#47680,#47681,#47682,#47683,#47684,#47685,#47686,#47687,#47688,
#47689,#47690,#47691,#47692,#47693,#47694,#47695,#47696,#47697,#47698,#47699,
#47700,#47701,#47702,#47703,#47704,#47705,#47706,#47707,#47708,#47709,#47710,
#47711,#47712,#47713,#47714,#47715,#47716,#47717,#47718,#47719,#47720,#47721,
#47722,#47723,#47724,#47725,#47726,#47727,#47728,#47729,#47730,#47731,#47732,
#47733,#47734,#47735,#47736,#47737,#47738,#47739,#47740,#47741,#47742,#47743,
#47744,#47745,#47746,#47747,#47748,#47749,#47750,#47751,#47752,#47753,#47754,
#47755,#47756,#47757,#47758,#47759,#47760,#47761,#47762,#47763,#47764,#47765,
#47766,#47767,#47768),.UNSPECIFIED.,.F.,.F.,(4,3,3,3,3,3,3,3,3,3,3,3,3,
3,3,3,3,3,3,3,3,3,3,3,3,3,3,3,3,3,3,3,3,3,3,3,3,3,3,3,3,3,3,3,3,3,3,3,3,
3,3,3,3,3,3,3,3,3,3,3,3,4),(72.2566310325653,72.3602553809559,72.4638199284958,
72.5673616020167,72.6732883015743,72.7769587590038,72.8840135796256,72.9910684002473,
73.0960616494774,73.200898215455,73.3056124113295,73.4102613487264,73.5148805337815,
73.6195054291833,73.7242406132493,73.8290373507608,73.9340142903564,73.9861901029102,
74.0911833521404,74.1960199181177,74.3007341139922,74.4053830513891,74.5100022364442,
74.6146271318463,74.7193623159124,74.8241590534239,74.9291359930195,74.981311805573,
75.0863050548031,75.1911416207804,75.2958558166549,75.4005047540517,75.5051239391068,
75.6097488345088,75.7144840185748,75.8192807560863,75.9242576956819,75.9764335082359,
76.0814267574661,76.1862633234431,76.2909775193177,76.3956264567146,76.5002456417698,
76.6048705371713,76.7096057212374,76.8144024587489,76.9193793983445,76.9715552108987,
77.0765484601287,77.1813850261059,77.2860992219805,77.3907481593772,77.4953673444324,
77.5999922398345,77.7047274239005,77.8095241614122,77.9145011010078,77.9666769135615,
78.0739238974765,78.1810066065371,78.2879201148065,78.336051653945),
 .UNSPECIFIED.);
#572=B_SPLINE_CURVE_WITH_KNOTS('',3,(#47769,#47770,#47771,#47772),
 .UNSPECIFIED.,.F.,.F.,(4,4),(-2.51409019964695,-2.4734065574123),
 .UNSPECIFIED.);
#573=B_SPLINE_CURVE_WITH_KNOTS('',3,(#47774,#47775,#47776,#47777,#47778,
#47779),.UNSPECIFIED.,.F.,.F.,(4,2,4),(-0.041493788302871,-0.0346416690046193,
-0.000583262449505623),.UNSPECIFIED.);
#574=B_SPLINE_CURVE_WITH_KNOTS('',3,(#47780,#47781,#47782,#47783,#47784,
#47785,#47786,#47787,#47788,#47789,#47790,#47791,#47792,#47793,#47794,#47795,
#47796,#47797,#47798,#47799,#47800,#47801,#47802,#47803,#47804,#47805,#47806,
#47807,#47808,#47809,#47810,#47811,#47812,#47813,#47814,#47815,#47816,#47817,
#47818,#47819,#47820,#47821,#47822,#47823,#47824,#47825,#47826,#47827,#47828,
#47829,#47830,#47831,#47832,#47833,#47834,#47835,#47836,#47837,#47838,#47839,
#47840,#47841,#47842,#47843,#47844,#47845,#47846,#47847,#47848,#47849,#47850,
#47851,#47852,#47853,#47854,#47855,#47856,#47857,#47858,#47859,#47860,#47861,
#47862,#47863,#47864,#47865,#47866,#47867,#47868,#47869,#47870,#47871,#47872,
#47873,#47874,#47875,#47876,#47877,#47878,#47879,#47880,#47881,#47882,#47883,
#47884,#47885,#47886,#47887,#47888,#47889,#47890,#47891,#47892,#47893,#47894,
#47895,#47896,#47897,#47898,#47899,#47900,#47901,#47902,#47903,#47904,#47905,
#47906,#47907,#47908,#47909,#47910,#47911,#47912,#47913,#47914,#47915,#47916,
#47917,#47918,#47919,#47920,#47921,#47922,#47923,#47924,#47925,#47926,#47927,
#47928,#47929,#47930,#47931,#47932,#47933,#47934,#47935,#47936,#47937,#47938,
#47939,#47940,#47941,#47942,#47943,#47944,#47945,#47946,#47947,#47948,#47949,
#47950,#47951,#47952,#47953,#47954,#47955,#47956,#47957,#47958,#47959,#47960,
#47961,#47962,#47963,#47964,#47965,#47966,#47967,#47968,#47969,#47970,#47971,
#47972,#47973,#47974,#47975,#47976,#47977,#47978,#47979,#47980,#47981,#47982,
#47983,#47984,#47985,#47986,#47987,#47988,#47989,#47990,#47991,#47992,#47993,
#47994,#47995,#47996,#47997,#47998,#47999,#48000,#48001,#48002,#48003),
 .UNSPECIFIED.,.F.,.F.,(4,2,2,2,2,2,2,2,2,2,2,2,2,2,2,2,2,2,2,2,2,2,2,2,
2,2,2,2,2,2,2,2,2,2,2,2,2,2,2,2,2,2,2,2,2,2,2,2,2,2,2,2,2,2,2,2,2,2,2,2,
2,2,2,2,2,2,2,2,2,2,2,2,2,2,2,2,2,2,2,2,2,2,2,2,2,2,2,2,2,2,2,2,2,2,2,2,
2,2,2,2,2,2,2,2,2,2,2,2,2,2,2,4),(-2.51380311614403,-2.5057188902465,-2.50390337305145,
-2.50257646804571,-2.50135832362811,-2.50014405372957,-2.49847678018933,
-2.49513428537836,-2.48528681981277,-2.44176071704383,-2.41372553721965,
-2.40693781727606,-2.4038499815795,-2.40151474568926,-2.39930555125731,
-2.39559180528697,-2.38558201918726,-2.32022389081281,-2.31145165745222,
-2.30762322644957,-2.30548677708257,-2.30362737465592,-2.30231906796012,
-2.30109681102103,-2.2993992272215,-2.29502015054223,-2.25255271667082,
-2.2122212141153,-2.20699962375403,-2.20421810288363,-2.20213792126715,
-2.19951586008346,-2.19503687021547,-2.17846988738744,-2.12446576606885,
-2.10836160348672,-2.10552785894564,-2.10399453337647,-2.1027011064052,
-2.10106973833147,-2.09786813605386,-2.06988250608802,-2.03673414804337,
-2.02068900706426,-2.01371865924593,-2.00822332833925,-2.00538488588434,
-2.00307712132473,-2.00041811730562,-1.99589094348477,-1.9779692450429,
-1.93720972933782,-1.91233601420066,-1.90757622789669,-1.90568688219965,
-1.90435804943943,-1.90312791592093,-1.90140092337691,-1.89681126371826,
-1.85701485778536,-1.81449304220479,-1.80915018370927,-1.80634320712155,
-1.80426040555171,-1.80165643180366,-1.79726072499105,-1.78148587064127,
-1.72660185231637,-1.71573004400992,-1.70912479807251,-1.70698105967961,
-1.70559925545828,-1.70427384355068,-1.70233369566118,-1.69759982566183,
-1.66056625049074,-1.62962657454605,-1.61900536744556,-1.61136602308453,
-1.60812841143886,-1.60576784127861,-1.60359660075783,-1.60065276770379,
-1.59333819324359,-1.5538687041214,-1.52373991786759,-1.51532798084632,
-1.50984642709876,-1.50784921361958,-1.50649887481976,-1.50529044989673,
-1.50333432227674,-1.49850466511426,-1.46609143223948,-1.43219103696873,
-1.42070617305763,-1.41259625959539,-1.40928120813914,-1.40690654525286,
-1.4047511351797,-1.4013308910304,-1.39497634440314,-1.34617882612164,-1.3228721828953,
-1.31559392671055,-1.31067345759629,-1.30875891696104,-1.30742515108399,
-1.30620059109701,-1.30449499662752,-1.3000647200745,-1.29834900329513),
 .UNSPECIFIED.);
#575=B_SPLINE_CURVE_WITH_KNOTS('',3,(#48009,#48010,#48011,#48012,#48013,
#48014,#48015,#48016,#48017,#48018,#48019,#48020,#48021,#48022,#48023,#48024,
#48025,#48026,#48027,#48028,#48029,#48030,#48031,#48032,#48033,#48034,#48035,
#48036,#48037,#48038,#48039,#48040,#48041,#48042,#48043,#48044,#48045,#48046,
#48047,#48048,#48049,#48050,#48051,#48052,#48053,#48054,#48055,#48056,#48057,
#48058,#48059,#48060,#48061,#48062,#48063,#48064,#48065,#48066,#48067,#48068,
#48069,#48070,#48071,#48072,#48073,#48074,#48075,#48076,#48077,#48078,#48079,
#48080,#48081,#48082,#48083,#48084,#48085,#48086,#48087,#48088,#48089,#48090,
#48091,#48092,#48093,#48094,#48095,#48096,#48097,#48098,#48099,#48100,#48101,
#48102,#48103,#48104,#48105,#48106,#48107,#48108,#48109,#48110,#48111,#48112,
#48113,#48114,#48115,#48116,#48117,#48118,#48119,#48120,#48121,#48122,#48123,
#48124,#48125,#48126,#48127,#48128,#48129,#48130,#48131,#48132,#48133,#48134,
#48135,#48136,#48137,#48138,#48139,#48140,#48141,#48142,#48143,#48144,#48145,
#48146,#48147,#48148,#48149,#48150,#48151,#48152,#48153,#48154,#48155,#48156,
#48157,#48158,#48159,#48160,#48161,#48162,#48163,#48164,#48165,#48166,#48167,
#48168,#48169,#48170,#48171,#48172,#48173,#48174,#48175,#48176,#48177,#48178,
#48179,#48180,#48181,#48182,#48183,#48184,#48185,#48186,#48187,#48188,#48189,
#48190,#48191,#48192,#48193,#48194,#48195,#48196,#48197,#48198,#48199,#48200,
#48201,#48202,#48203,#48204,#48205,#48206,#48207,#48208,#48209,#48210,#48211,
#48212,#48213,#48214,#48215,#48216,#48217,#48218,#48219,#48220,#48221,#48222,
#48223,#48224,#48225,#48226,#48227,#48228,#48229,#48230,#48231,#48232,#48233,
#48234,#48235,#48236,#48237,#48238,#48239,#48240,#48241,#48242,#48243,#48244,
#48245,#48246),.UNSPECIFIED.,.F.,.F.,(4,2,2,2,2,2,2,2,2,2,2,2,2,2,2,2,2,
2,2,2,2,2,2,2,2,2,2,2,2,2,2,2,2,2,2,2,2,2,2,2,2,2,2,2,2,2,2,2,2,2,2,2,2,
2,2,2,2,2,2,2,2,2,2,2,2,2,2,2,2,2,2,2,2,2,2,2,2,2,2,2,2,2,2,2,2,2,2,2,2,
2,2,2,2,2,2,2,2,2,2,2,2,2,2,2,2,2,2,2,2,2,2,2,2,2,2,2,2,2,4),(-1.21658137004514,
-1.1891249839804,-1.1843917540007,-1.18143090687014,-1.17911169725611,-1.17653198226384,
-1.17224815723712,-1.15574253158255,-1.09376935906015,-1.08456372110044,
-1.08204876568971,-1.08058446891245,-1.07927988123128,-1.07754095822139,
-1.07367086323986,-1.06835697899584,-1.0541898966876,-1.00572967857163,
-0.988715278580078,-0.984255077292539,-0.981610878746839,-0.979300866989459,
-0.976440201664556,-0.970838824113962,-0.931739979786828,-0.888544954491291,
-0.884191888413404,-0.882497926606543,-0.881276221370208,-0.879939249599092,
-0.878009546020247,-0.872991747009221,-0.865522653847871,-0.841170505219558,
-0.793952846619021,-0.786766266065938,-0.783921548247851,-0.781559209727695,
-0.77913686767823,-0.775582341858262,-0.765878726818815,-0.751285666006921,
-0.721090668731977,-0.690178943060794,-0.685342668611477,-0.683385110578194,
-0.682176185169055,-0.680825658063772,-0.678828821404486,-0.673352317519568,
-0.66495265862472,-0.634910248621997,-0.59535003929974,-0.588036431321171,
-0.585092277732971,-0.582920543405897,-0.580559187884376,-0.577320061322963,
-0.569675110979303,-0.559043485783338,-0.52805790291404,-0.491021286121869,
-0.486284099893265,-0.484343028524726,-0.483017137351736,-0.481634975426314,
-0.479490943649205,-0.472886718508895,-0.462020032633777,-0.407207753238175,
-0.391371892227016,-0.386969374816044,-0.384363333825422,-0.382279973594379,
-0.379473655660843,-0.374136846508977,-0.330609740525097,-0.291816863380292,
-0.287164954229007,-0.285429083749242,-0.28419628866504,-0.282868640438062,
-0.280987634957947,-0.276283151283912,-0.252013880783432,-0.222217868926318,
-0.193681998635353,-0.189039120965494,-0.186105130120254,-0.183845936529115,
-0.183750679937684,-0.183675581972278,-0.183615743063987,-0.183567664959165,
-0.183528781625933,-0.183497169253304,-0.183444700826453,-0.183394391883649,
-0.183346079567604,-0.183299616694927,-0.183254869807652,-0.183211717708318,
-0.183170049975852,-0.183129765793954,-0.183090772939764,-0.183052986826154,
-0.180212188641947,-0.177123262222999,-0.172136563485539,-0.162198427827386,
-0.115791646890992,-0.090547535821272,-0.0873640374779424,-0.0857360691090431,
-0.0844422519689053,-0.0829048087542316,-0.0800539024920105,-0.0635645684128408,
-0.000583171670547464),.UNSPECIFIED.);
#576=B_SPLINE_CURVE_WITH_KNOTS('',3,(#48247,#48248,#48249,#48250,#48251,
#48252,#48253),.UNSPECIFIED.,.F.,.F.,(4,3,4),(78.336051653945,78.4428050925864,
78.5398163397449),.UNSPECIFIED.);
#577=B_SPLINE_CURVE_WITH_KNOTS('',3,(#48254,#48255,#48256,#48257,#48258,
#48259,#48260,#48261,#48262,#48263,#48264,#48265,#48266,#48267,#48268,#48269,
#48270,#48271,#48272,#48273,#48274,#48275,#48276,#48277,#48278,#48279,#48280,
#48281,#48282,#48283,#48284,#48285,#48286,#48287,#48288,#48289,#48290,#48291,
#48292,#48293,#48294,#48295,#48296,#48297,#48298,#48299,#48300,#48301,#48302,
#48303,#48304,#48305,#48306,#48307,#48308,#48309,#48310,#48311,#48312,#48313,
#48314,#48315,#48316,#48317,#48318,#48319,#48320,#48321,#48322,#48323,#48324,
#48325,#48326,#48327,#48328,#48329,#48330,#48331,#48332,#48333,#48334,#48335,
#48336,#48337,#48338,#48339,#48340,#48341,#48342,#48343,#48344,#48345,#48346,
#48347,#48348,#48349,#48350,#48351,#48352,#48353,#48354,#48355,#48356,#48357,
#48358,#48359,#48360,#48361,#48362,#48363,#48364,#48365,#48366,#48367,#48368,
#48369,#48370,#48371,#48372,#48373,#48374,#48375,#48376,#48377,#48378,#48379,
#48380,#48381,#48382,#48383,#48384,#48385,#48386,#48387,#48388,#48389,#48390,
#48391,#48392,#48393,#48394,#48395,#48396,#48397,#48398,#48399,#48400,#48401,
#48402,#48403,#48404,#48405,#48406,#48407,#48408,#48409,#48410,#48411,#48412,
#48413,#48414,#48415,#48416,#48417,#48418,#48419,#48420,#48421,#48422,#48423,
#48424,#48425,#48426,#48427,#48428,#48429,#48430,#48431,#48432,#48433,#48434,
#48435,#48436,#48437,#48438,#48439,#48440,#48441,#48442,#48443,#48444,#48445,
#48446,#48447,#48448,#48449,#48450,#48451,#48452,#48453,#48454,#48455,#48456,
#48457,#48458,#48459,#48460,#48461,#48462,#48463,#48464,#48465,#48466,#48467),
 .UNSPECIFIED.,.F.,.F.,(4,2,2,2,2,2,2,2,2,2,2,2,2,2,2,2,2,2,2,2,2,2,2,2,
2,2,2,2,2,2,2,2,2,2,2,2,2,2,2,2,2,2,2,2,2,2,2,2,2,2,2,2,2,2,2,2,2,2,2,2,
2,2,2,2,2,2,2,2,2,2,2,2,2,2,2,2,2,2,2,2,2,2,2,2,2,2,2,2,2,2,2,2,2,2,2,2,
2,2,2,2,2,2,2,2,2,2,4),(-1.29834900329513,-1.25769021628927,-1.21735607324619,
-1.21263190090603,-1.20967386889312,-1.20735510138914,-1.20477406029058,
-1.20048375289467,-1.18389667504742,-1.12081858482312,-1.11261720688062,
-1.11020573147173,-1.10876440566488,-1.10745315500985,-1.10566768037584,
-1.1015361016775,-1.08285159066525,-1.03535184568982,-1.01714043042331,
-1.01258739326859,-1.00992196706622,-1.0078447531676,-1.00511361576107,
-1.00013392309523,-0.970900720720121,-0.935194953403005,-0.927291043545992,
-0.914321163787172,-0.911787692663085,-0.910171056051705,-0.908877980806288,
-0.90733158191397,-0.904437888767709,-0.886850461634557,-0.858538343808799,
-0.819287970420795,-0.814548009231563,-0.811584950934823,-0.809265243273779,
-0.806686244241806,-0.802406591509152,-0.78595612430463,-0.7246961065986,
-0.71482123216225,-0.712273339026079,-0.710786918663496,-0.709617240942895,
-0.70798792288454,-0.704692698584166,-0.700369134651098,-0.689919742061426,
-0.641322050429228,-0.632048711086285,-0.618247549860236,-0.614051893361414,
-0.611491123602568,-0.609166864531534,-0.606168650993029,-0.599869433120256,
-0.575652327407577,-0.535264902496132,-0.531253714115416,-0.516369866010922,
-0.513736250728469,-0.512089083090206,-0.510794040321335,-0.509271535630656,
-0.506490392836548,-0.49156785183812,-0.448228001386511,-0.42086121195442,
-0.416260735079831,-0.413339515701385,-0.411024012225265,-0.408419758047953,
-0.404026337512082,-0.386128308483794,-0.348514712031086,-0.3401378681956,
-0.335459963329045,-0.331895901021324,-0.317310579935759,-0.314691496716336,
-0.313048744779638,-0.311754048660356,-0.310228294326044,-0.307431898677704,
-0.292184788732463,-0.246355848138599,-0.221671323967535,-0.217152841288632,
-0.214256590269068,-0.21216828598887,-0.209677527262702,-0.20707537119769,
-0.203265316565563,-0.196486150564352,-0.181078706396089,-0.142737591051673,
-0.118770649616248,-0.115603323007869,-0.113978849986806,-0.112685266448303,
-0.111145086787342,-0.108281161234025,-0.0914698421241412,-0.0414797095138316),
 .UNSPECIFIED.);
#578=B_SPLINE_CURVE_WITH_KNOTS('',3,(#48472,#48473,#48474,#48475,#48476,
#48477,#48478,#48479,#48480,#48481,#48482,#48483,#48484,#48485,#48486,#48487,
#48488,#48489,#48490,#48491,#48492,#48493,#48494,#48495,#48496,#48497,#48498,
#48499,#48500,#48501,#48502,#48503,#48504,#48505,#48506,#48507,#48508,#48509,
#48510,#48511,#48512,#48513,#48514,#48515,#48516,#48517,#48518,#48519,#48520,
#48521,#48522,#48523,#48524,#48525,#48526,#48527,#48528,#48529,#48530,#48531,
#48532,#48533,#48534,#48535,#48536,#48537,#48538,#48539,#48540,#48541,#48542,
#48543,#48544,#48545,#48546,#48547,#48548,#48549,#48550,#48551,#48552,#48553,
#48554,#48555,#48556,#48557,#48558,#48559,#48560,#48561,#48562,#48563,#48564,
#48565,#48566,#48567,#48568,#48569,#48570,#48571,#48572,#48573,#48574,#48575,
#48576,#48577,#48578,#48579,#48580,#48581,#48582,#48583,#48584,#48585,#48586,
#48587,#48588,#48589,#48590,#48591,#48592,#48593,#48594,#48595,#48596,#48597,
#48598,#48599,#48600,#48601,#48602,#48603,#48604,#48605,#48606,#48607,#48608,
#48609,#48610,#48611,#48612,#48613,#48614,#48615,#48616,#48617,#48618,#48619,
#48620,#48621,#48622,#48623,#48624,#48625,#48626,#48627,#48628,#48629,#48630,
#48631,#48632,#48633,#48634,#48635,#48636,#48637,#48638,#48639,#48640,#48641,
#48642,#48643,#48644,#48645,#48646,#48647,#48648,#48649,#48650,#48651,#48652,
#48653,#48654,#48655,#48656,#48657,#48658,#48659,#48660,#48661,#48662,#48663,
#48664,#48665,#48666,#48667,#48668,#48669,#48670,#48671,#48672,#48673,#48674,
#48675,#48676,#48677,#48678,#48679,#48680,#48681,#48682,#48683),
 .UNSPECIFIED.,.F.,.F.,(4,2,2,2,2,2,2,2,2,2,2,2,2,2,2,2,2,2,2,2,2,2,2,2,
2,2,2,2,2,2,2,2,2,2,2,2,2,2,2,2,2,2,2,2,2,2,2,2,2,2,2,2,2,2,2,2,2,2,2,2,
2,2,2,2,2,2,2,2,2,2,2,2,2,2,2,2,2,2,2,2,2,2,2,2,2,2,2,2,2,2,2,2,2,2,2,2,
2,2,2,2,2,2,2,2,2,4),(-2.47330352940323,-2.47280614242241,-2.4711756610841,
-2.46797964661157,-2.43960318315561,-2.42172026383921,-2.40591459269085,
-2.38677460043587,-2.37943395651363,-2.37618822907268,-2.37382579792882,
-2.37165566101622,-2.36871761703384,-2.36140609639352,-2.32049284656353,
-2.29148639305627,-2.27915696341582,-2.27658115067425,-2.27532535894301,
-2.2741550328263,-2.27267372870349,-2.27014746237708,-2.26050939864939,
-2.19903388004811,-2.18256954668905,-2.17828905454494,-2.17571000992547,
-2.17339055189566,-2.17042821398372,-2.16569017671535,-2.126337966641,-2.09782835895185,
-2.08048501145368,-2.07760059542768,-2.07605623995757,-2.07476316327683,
-2.07314438168212,-2.07000276304802,-2.04844520065214,-1.99588895420398,
-1.98290086511098,-1.97894623463244,-1.9764388474031,-1.97409889657658,
-1.97103929983643,-1.96422796104393,-1.91305571414945,-1.88238468702453,
-1.87890681664904,-1.87724177884773,-1.87595733776832,-1.87445308451574,
-1.87182665421821,-1.8610179778599,-1.80653839398111,-1.78511786598161,
-1.78049289825892,-1.77783848381455,-1.77552993218143,-1.77268441683706,
-1.76833045158494,-1.74687689351158,-1.69787064445871,-1.68225286051899,
-1.67943989844966,-1.67791078637913,-1.67661667464073,-1.67497904740741,
-1.67237633995476,-1.65811016173779,-1.65252892927466,-1.6128500606956,
-1.58884361882339,-1.58257311247748,-1.57958078748119,-1.57725770531214,
-1.57469480614609,-1.57048780261165,-1.55657746088346,-1.50562015581286,
-1.49060640987102,-1.48508494857162,-1.48109885171595,-1.47933909390867,
-1.47803171681945,-1.47657829054539,-1.47411213578008,-1.46539313685228,
-1.40292039766669,-1.38637984987438,-1.38209329515882,-1.37951302275186,
-1.37719399952684,-1.3742343382562,-1.36950488169606,-1.32953036843299,
-1.29738107416082,-1.28397005257281,-1.28126745941335,-1.27976221539201,
-1.27846564292004,-1.27679548575481,-1.27408449122815,-1.25752712896311,
-1.22864179188508,-1.21658137004514),.UNSPECIFIED.);
#579=B_SPLINE_CURVE_WITH_KNOTS('',3,(#48685,#48686,#48687,#48688,#48689,
#48690,#48691,#48692,#48693,#48694,#48695,#48696,#48697,#48698,#48699,#48700,
#48701,#48702),.UNSPECIFIED.,.F.,.F.,(4,2,2,2,2,2,2,2,4),(-0.0414797095138316,
-0.0326304630026233,-0.0206541176175663,-0.0166774261868832,-0.0141649808844975,
-0.0119423353386409,-0.00967246363527554,-0.00562235294686388,-0.000582410650389689),
 .UNSPECIFIED.);
#580=B_SPLINE_CURVE_WITH_KNOTS('',3,(#48703,#48704,#48705,#48706,#48707,
#48708,#48709,#48710,#48711,#48712,#48713,#48714,#48715,#48716,#48717,#48718,
#48719,#48720,#48721,#48722,#48723,#48724,#48725,#48726,#48727,#48728,#48729,
#48730,#48731,#48732,#48733,#48734,#48735,#48736,#48737,#48738,#48739,#48740,
#48741,#48742,#48743,#48744,#48745,#48746,#48747,#48748,#48749,#48750,#48751,
#48752,#48753,#48754,#48755,#48756,#48757,#48758,#48759,#48760,#48761,#48762,
#48763,#48764,#48765,#48766,#48767,#48768,#48769,#48770,#48771,#48772,#48773,
#48774,#48775,#48776,#48777,#48778,#48779,#48780,#48781,#48782,#48783,#48784,
#48785,#48786,#48787,#48788,#48789,#48790,#48791,#48792,#48793,#48794,#48795,
#48796,#48797,#48798,#48799,#48800,#48801,#48802,#48803,#48804,#48805,#48806,
#48807,#48808,#48809,#48810,#48811,#48812,#48813,#48814,#48815,#48816,#48817,
#48818,#48819,#48820,#48821,#48822,#48823,#48824,#48825,#48826,#48827,#48828,
#48829,#48830,#48831,#48832,#48833,#48834,#48835,#48836,#48837,#48838,#48839,
#48840,#48841,#48842,#48843,#48844,#48845,#48846,#48847,#48848,#48849,#48850,
#48851,#48852,#48853,#48854,#48855,#48856,#48857,#48858,#48859,#48860,#48861,
#48862,#48863,#48864,#48865,#48866,#48867,#48868,#48869,#48870,#48871,#48872,
#48873,#48874,#48875,#48876,#48877,#48878,#48879,#48880,#48881,#48882,#48883,
#48884,#48885,#48886,#48887,#48888,#48889,#48890,#48891,#48892,#48893,#48894,
#48895,#48896,#48897,#48898,#48899,#48900,#48901,#48902,#48903,#48904,#48905,
#48906),.UNSPECIFIED.,.F.,.F.,(4,2,2,2,2,2,2,2,2,2,2,2,2,2,2,2,2,2,2,2,
2,2,2,2,2,2,2,2,2,2,2,2,2,2,2,2,2,2,2,2,2,2,2,2,2,2,2,2,2,2,2,2,2,2,2,2,
2,2,2,2,2,2,2,2,2,2,2,2,2,2,2,2,2,2,2,2,2,2,2,2,2,2,2,2,2,2,2,2,2,2,2,2,
2,2,2,2,2,2,2,2,2,4),(-2.51371035365293,-2.4579504817706,-2.43416740516342,
-2.43004801671431,-2.42826483372786,-2.42695409888032,-2.42569340243194,
-2.42346779248273,-2.41682035801184,-2.35198938452692,-2.34096226702292,
-2.33559623235447,-2.33235203769843,-2.32953209064636,-2.32727584407651,
-2.32477982545212,-2.32087622259088,-2.3095078309908,-2.24961716772916,
-2.23306859439498,-2.2302157801933,-2.22867820112247,-2.22738479512049,
-2.22575801653735,-2.22257881244245,-2.19266679039188,-2.16151537431149,
-2.14539267592957,-2.13839880197559,-2.13288853662587,-2.13004669736339,
-2.12773829558897,-2.12508091436886,-2.12056222319378,-2.10276249916337,
-2.06192160984306,-2.03698100262777,-2.03221454124705,-2.03032391678356,
-2.02899465054679,-2.0277644886657,-2.02603796230798,-2.02145355324458,
-1.98147467137878,-1.93910692738182,-1.93376530375697,-1.93095824545593,
-1.92865178809561,-1.92596695496633,-1.92132805618564,-1.90187319043129,
-1.85083571142052,-1.83500549762557,-1.83218303215559,-1.83065185447081,
-1.82935786235572,-1.82772276086709,-1.82512848123981,-1.81102895595153,
-1.80513103306592,-1.78987777237792,-1.76117246414887,-1.74649221279437,
-1.73674525407137,-1.7331849049545,-1.73076151742669,-1.72840040203304,
-1.72555985795933,-1.71839878120607,-1.67081827678341,-1.64668913940135,
-1.6392602371041,-1.63426322589407,-1.6323367728804,-1.63100052242948,-1.62977826650148,
-1.62774906672787,-1.62247715032362,-1.55594593902264,-1.54485413063994,
-1.53695669802163,-1.53367609684562,-1.53130770775992,-1.5291454278617,
-1.52623813228733,-1.51913780518289,-1.47286199762123,-1.43759508102176,
-1.43434305891225,-1.43272266618112,-1.43155422303622,-1.43006225098546,
-1.42748922832941,-1.41732204744941,-1.35642138730097,-1.34000533668762,
-1.33572919419386,-1.3331513145379,-1.33083197846093,-1.32786851809341,
-1.32312609003501,-1.29776408237656),.UNSPECIFIED.);
#581=B_SPLINE_CURVE_WITH_KNOTS('',3,(#48912,#48913,#48914,#48915,#48916,
#48917,#48918,#48919,#48920,#48921,#48922,#48923,#48924,#48925,#48926,#48927,
#48928,#48929,#48930,#48931,#48932,#48933,#48934,#48935,#48936,#48937,#48938,
#48939,#48940,#48941,#48942,#48943,#48944,#48945,#48946,#48947,#48948,#48949,
#48950,#48951,#48952,#48953,#48954,#48955,#48956,#48957,#48958,#48959,#48960,
#48961,#48962,#48963,#48964,#48965,#48966,#48967,#48968,#48969,#48970,#48971,
#48972,#48973,#48974,#48975,#48976,#48977,#48978,#48979,#48980,#48981,#48982,
#48983,#48984,#48985,#48986,#48987,#48988,#48989,#48990,#48991,#48992,#48993,
#48994,#48995,#48996,#48997,#48998,#48999,#49000,#49001,#49002,#49003,#49004,
#49005,#49006,#49007,#49008,#49009,#49010,#49011,#49012,#49013,#49014,#49015,
#49016,#49017,#49018,#49019,#49020,#49021,#49022,#49023,#49024,#49025,#49026,
#49027,#49028,#49029,#49030,#49031,#49032,#49033,#49034,#49035,#49036,#49037,
#49038,#49039,#49040,#49041,#49042,#49043,#49044,#49045,#49046,#49047,#49048,
#49049,#49050,#49051,#49052,#49053,#49054,#49055,#49056,#49057,#49058,#49059,
#49060,#49061,#49062,#49063,#49064,#49065,#49066,#49067,#49068,#49069,#49070,
#49071,#49072,#49073,#49074,#49075,#49076,#49077,#49078,#49079,#49080,#49081,
#49082,#49083,#49084,#49085,#49086,#49087,#49088,#49089,#49090,#49091,#49092,
#49093,#49094,#49095,#49096,#49097,#49098,#49099,#49100,#49101,#49102,#49103,
#49104,#49105,#49106,#49107,#49108,#49109,#49110,#49111,#49112,#49113),
 .UNSPECIFIED.,.F.,.F.,(4,2,2,2,2,2,2,2,2,2,2,2,2,2,2,2,2,2,2,2,2,2,2,2,
2,2,2,2,2,2,2,2,2,2,2,2,2,2,2,2,2,2,2,2,2,2,2,2,2,2,2,2,2,2,2,2,2,2,2,2,
2,2,2,2,2,2,2,2,2,2,2,2,2,2,2,2,2,2,2,2,2,2,2,2,2,2,2,2,2,2,2,2,2,2,2,2,
2,2,2,2,4),(-1.21683047486584,-1.20679256159222,-1.16543709119454,-1.15844305223591,
-1.15617277744239,-1.15476283884563,-1.15343845239932,-1.15157488200906,
-1.14697850405559,-1.12383611992667,-1.09895533047361,-1.06443264535201,
-1.05968271506895,-1.0567166080109,-1.05439647483337,-1.05181901809905,
-1.04754664991083,-1.03118564928897,-0.970992344237733,-0.960105421157891,
-0.957472203332062,-0.955966145548304,-0.954681525503829,-0.953018031781168,
-0.949549535957342,-0.919942748590857,-0.867462827865426,-0.860809245694334,
-0.857777619158547,-0.855441539367763,-0.85292105326658,-0.84890872049112,
-0.835375022146676,-0.787857423192222,-0.761950954079996,-0.758760696070722,
-0.757131243673212,-0.75583729204823,-0.754300923174751,-0.751455243089941,
-0.735093884907736,-0.677919693028221,-0.664211245605211,-0.660025908777287,
-0.65746749366856,-0.655142804267596,-0.652140412272213,-0.645818768518974,
-0.621433276428417,-0.580427602991764,-0.576908853820052,-0.562329284511881,
-0.559710511922897,-0.558067866435139,-0.556773194997694,-0.555247400364807,
-0.552450753535979,-0.537197571217976,-0.491318514544147,-0.466663890333215,
-0.462160077727896,-0.459268318599959,-0.456955695209536,-0.454332792450086,
-0.44985392187971,-0.430755985057016,-0.387693860348781,-0.363777477763212,
-0.360610822319399,-0.358986486659055,-0.357692902078161,-0.356152590255361,
-0.3532880729308,-0.336462345462607,-0.273037661111589,-0.264549335977496,
-0.26107690882888,-0.25891193296584,-0.256545443178191,-0.253276419378178,
-0.245714404202163,-0.235092338387338,-0.204152554346614,-0.177308349506666,
-0.164066311524436,-0.161518036181473,-0.159896923336077,-0.158603699368851,
-0.157061198063145,-0.154514459216343,-0.141476710761522,-0.110310002664115,
-0.0724072341375291,-0.0650899867698462,-0.0621454468154719,-0.0599738095846168,
-0.0576129282440144,-0.0543751205765847,-0.0507846473231634,-0.0394419541871347,
-0.000582966585860259),.UNSPECIFIED.);
#582=B_SPLINE_CURVE_WITH_KNOTS('',3,(#49114,#49115,#49116,#49117,#49118,
#49119,#49120,#49121,#49122,#49123,#49124,#49125),.UNSPECIFIED.,.F.,.F.,
(4,2,2,2,2,4),(-2.5139747976882,-2.47986063878101,-2.47727398228966,-2.47563484175021,
-2.47409990132521,-2.47330352940323),.UNSPECIFIED.);
#583=B_SPLINE_CURVE_WITH_KNOTS('',3,(#49126,#49127,#49128,#49129,#49130,
#49131,#49132,#49133,#49134,#49135,#49136,#49137,#49138,#49139,#49140,#49141,
#49142,#49143,#49144,#49145,#49146,#49147,#49148,#49149,#49150,#49151,#49152,
#49153,#49154,#49155,#49156,#49157,#49158,#49159,#49160,#49161,#49162,#49163,
#49164,#49165,#49166,#49167,#49168,#49169,#49170,#49171,#49172,#49173,#49174,
#49175,#49176,#49177,#49178,#49179,#49180,#49181,#49182,#49183,#49184,#49185,
#49186,#49187,#49188,#49189,#49190,#49191,#49192,#49193,#49194,#49195,#49196,
#49197,#49198,#49199,#49200,#49201,#49202,#49203,#49204,#49205,#49206,#49207,
#49208,#49209,#49210,#49211,#49212,#49213,#49214,#49215,#49216,#49217,#49218,
#49219,#49220,#49221,#49222,#49223,#49224,#49225,#49226,#49227,#49228,#49229,
#49230,#49231,#49232,#49233,#49234,#49235,#49236,#49237,#49238,#49239,#49240,
#49241,#49242,#49243,#49244,#49245,#49246,#49247,#49248,#49249,#49250,#49251,
#49252,#49253,#49254,#49255,#49256,#49257,#49258,#49259,#49260,#49261,#49262,
#49263,#49264,#49265,#49266,#49267,#49268,#49269,#49270,#49271,#49272,#49273,
#49274,#49275,#49276,#49277,#49278,#49279,#49280,#49281,#49282,#49283,#49284,
#49285,#49286,#49287,#49288,#49289,#49290,#49291,#49292,#49293,#49294,#49295,
#49296,#49297,#49298,#49299,#49300,#49301,#49302,#49303,#49304,#49305,#49306,
#49307,#49308,#49309,#49310,#49311,#49312,#49313,#49314,#49315,#49316,#49317,
#49318,#49319,#49320,#49321,#49322,#49323,#49324,#49325,#49326,#49327,#49328,
#49329,#49330,#49331,#49332,#49333,#49334,#49335,#49336,#49337,#49338,#49339,
#49340,#49341,#49342,#49343,#49344,#49345),.UNSPECIFIED.,.F.,.F.,(4,2,2,
2,2,2,2,2,2,2,2,2,2,2,2,2,2,2,2,2,2,2,2,2,2,2,2,2,2,2,2,2,2,2,2,2,2,2,2,
2,2,2,2,2,2,2,2,2,2,2,2,2,2,2,2,2,2,2,2,2,2,2,2,2,2,2,2,2,2,2,2,2,2,2,2,
2,2,2,2,2,2,2,2,2,2,2,2,2,2,2,2,2,2,2,2,2,2,2,2,2,2,2,2,2,2,2,2,2,2,4),
(-1.29776408237656,-1.28432009226333,-1.25680382844245,-1.2528784758829,
-1.23800659097861,-1.23537428957193,-1.23372784705557,-1.23243331005041,
-1.23091132484804,-1.22813094060947,-1.21320760685108,-1.1698366198042,
-1.14253210028953,-1.13793505328303,-1.13501546220267,-1.13270090182622,
-1.13009734162604,-1.12570420162332,-1.10779405108135,-1.07011660389385,
-1.06348480410166,-1.03951434998688,-1.03634797718423,-1.03472404202459,
-1.03343091275736,-1.03189130473323,-1.02902852341146,-1.01222648624909,
-0.983346385135795,-0.943834982664761,-0.93910228251295,-0.93614177289407,
-0.933822831428776,-0.931243418614563,-0.926960104619756,-0.9104565711911,
-0.848492997300875,-0.839286150291822,-0.836771264950108,-0.835307088991741,
-0.834002664845639,-0.832264035653893,-0.828394895937816,-0.823082526364711,
-0.808920694111929,-0.76047429163564,-0.743450207156665,-0.738989535784814,
-0.73634541689553,-0.734035695925081,-0.731175676896869,-0.725576499116564,
-0.68652992082639,-0.643280646736572,-0.638934287405839,-0.637241530728495,
-0.636020230429521,-0.634683168190679,-0.632752438849346,-0.627726975238482,
-0.620242377925727,-0.595801390165363,-0.548722755129127,-0.541621265703519,
-0.538742473485475,-0.536586957222302,-0.534211696795687,-0.530894923104883,
-0.522776324393855,-0.51127450535185,-0.477290137704637,-0.44492794974094,
-0.440100232826018,-0.438144219647476,-0.436935662348577,-0.435584973786195,
-0.43358689960873,-0.428100753148054,-0.419680792069218,-0.389499198547466,
-0.350124516892673,-0.342808609693789,-0.339864240633898,-0.337692598974088,
-0.33533158697108,-0.332093371917713,-0.324452658339215,-0.313828379069186,
-0.282877708697353,-0.245786866345511,-0.24106096326923,-0.239121886924017,
-0.237796481891147,-0.236413959221531,-0.234381199865635,-0.228326969423526,
-0.185284654858206,-0.17930286323177,-0.147675970453935,-0.1429582134248,
-0.140001846486526,-0.137682927946228,-0.13510021508179,-0.130803582133839,
-0.114308930124998,-0.0928284065903526,-0.0721380315305199,-0.0444747427209316,
-0.041277742169082,-0.0412313986595946),.UNSPECIFIED.);
#584=B_SPLINE_CURVE_WITH_KNOTS('',3,(#49350,#49351,#49352,#49353,#49354,
#49355,#49356,#49357,#49358,#49359,#49360,#49361,#49362,#49363,#49364,#49365,
#49366,#49367,#49368,#49369,#49370,#49371,#49372,#49373,#49374,#49375,#49376,
#49377,#49378,#49379,#49380,#49381,#49382,#49383,#49384,#49385,#49386,#49387,
#49388,#49389,#49390,#49391,#49392,#49393,#49394,#49395,#49396,#49397,#49398,
#49399,#49400,#49401,#49402,#49403,#49404,#49405,#49406,#49407,#49408,#49409,
#49410,#49411,#49412,#49413,#49414,#49415,#49416,#49417,#49418,#49419,#49420,
#49421,#49422,#49423,#49424,#49425,#49426,#49427,#49428,#49429,#49430,#49431,
#49432,#49433,#49434,#49435,#49436,#49437,#49438,#49439,#49440,#49441,#49442,
#49443,#49444,#49445,#49446,#49447,#49448,#49449,#49450,#49451,#49452,#49453,
#49454,#49455,#49456,#49457,#49458,#49459,#49460,#49461,#49462,#49463,#49464,
#49465,#49466,#49467,#49468,#49469,#49470,#49471,#49472,#49473,#49474,#49475,
#49476,#49477,#49478,#49479,#49480,#49481,#49482,#49483,#49484,#49485,#49486,
#49487,#49488,#49489,#49490,#49491,#49492,#49493,#49494,#49495,#49496,#49497,
#49498,#49499,#49500,#49501,#49502,#49503,#49504,#49505,#49506,#49507,#49508,
#49509,#49510,#49511,#49512,#49513,#49514,#49515,#49516,#49517,#49518,#49519,
#49520,#49521,#49522,#49523,#49524,#49525,#49526,#49527,#49528,#49529,#49530,
#49531,#49532,#49533,#49534,#49535,#49536,#49537,#49538,#49539,#49540,#49541,
#49542,#49543,#49544,#49545,#49546,#49547,#49548,#49549,#49550,#49551,#49552,
#49553,#49554,#49555,#49556,#49557,#49558,#49559,#49560,#49561,#49562,#49563,
#49564,#49565,#49566,#49567,#49568,#49569,#49570,#49571),.UNSPECIFIED.,
 .F.,.F.,(4,2,2,2,2,2,2,2,2,2,2,2,2,2,2,2,2,2,2,2,2,2,2,2,2,2,2,2,2,2,2,
2,2,2,2,2,2,2,2,2,2,2,2,2,2,2,2,2,2,2,2,2,2,2,2,2,2,2,2,2,2,2,2,2,2,2,2,
2,2,2,2,2,2,2,2,2,2,2,2,2,2,2,2,2,2,2,2,2,2,2,2,2,2,2,2,2,2,2,2,2,2,2,2,
2,2,2,2,2,2,2,4),(-2.47379053097235,-2.47277706034237,-2.45616941361428,
-2.45187626101787,-2.44929391236621,-2.44697422438702,-2.44401536844734,
-2.4392905461352,-2.4002035463753,-2.37895316559793,-2.36207130719172,-2.35611108284694,
-2.35194700764502,-2.35014091991578,-2.34881997424031,-2.34740211450615,
-2.34509699755382,-2.3378229275557,-2.28755552908443,-2.2681124474593,-2.26017314504604,
-2.25408168955763,-2.25112344436621,-2.24880395067457,-2.24622152430073,
-2.24192755427174,-2.22722079040336,-2.2202433820079,-2.21471035435831,
-2.17644297809176,-2.15703383368175,-2.15282214965174,-2.15102263979531,
-2.14970904056391,-2.14827362748805,-2.14588934700611,-2.13793590743231,
-2.07459555771243,-2.05799040386735,-2.05369808027617,-2.05111626267205,
-2.04879707225391,-2.04583887922292,-2.0411151726313,-2.00202601282964,
-1.96913687927961,-1.95556962679675,-1.9528580948639,-1.95135075592513,
-1.95005420588683,-1.94838644972539,-1.94568396764216,-1.92934438661946,
-1.9139883508809,-1.8891589058606,-1.86281369368209,-1.85623546600458,-1.85318489192438,
-1.85085378274345,-1.84863046111866,-1.84484870177201,-1.83437924532905,
-1.77954755202239,-1.75904552485829,-1.75471657034165,-1.75289705397616,
-1.75158018145489,-1.75015316904785,-1.74780669110749,-1.74018419259941,
-1.67646746340632,-1.66548488211813,-1.65764669069571,-1.65437552253935,
-1.65200856163981,-1.64984389111909,-1.64692781252371,-1.63977807666126,
-1.59436499454103,-1.56872167767359,-1.56102640836016,-1.5558957727273,
-1.55394919225547,-1.55260895397547,-1.55139083685934,-1.54971048141597,
-1.54543769895588,-1.5015197045881,-1.46303829476585,-1.45745757749046,
-1.45460117703445,-1.45229155263442,-1.44964444198346,-1.44517129780746,
-1.42796859692916,-1.37961831176807,-1.36063108595812,-1.35646600106596,
-1.35467466373518,-1.35336247171798,-1.35192371217131,-1.34952392215997,
-1.34142946178886,-1.28348471803442,-1.26228869855122,-1.25767659876421,
-1.25502481699826,-1.25271576582657,-1.24986605401527,-1.24431776853978,
-1.21683047486584),.UNSPECIFIED.);
#585=B_SPLINE_CURVE_WITH_KNOTS('',3,(#49573,#49574,#49575,#49576,#49577,
#49578,#49579,#49580,#49581,#49582,#49583,#49584,#49585,#49586),
 .UNSPECIFIED.,.F.,.F.,(4,2,2,2,2,2,4),(-0.0412313986595946,-0.0396470820645504,
-0.038353352883166,-0.036818642137068,-0.0351798751504305,-0.0325941196013304,
-0.000582505019790992),.UNSPECIFIED.);
#586=B_SPLINE_CURVE_WITH_KNOTS('',3,(#49587,#49588,#49589,#49590,#49591,
#49592,#49593,#49594,#49595,#49596,#49597,#49598,#49599,#49600,#49601,#49602,
#49603,#49604,#49605,#49606,#49607,#49608,#49609,#49610,#49611,#49612,#49613,
#49614,#49615,#49616,#49617,#49618,#49619,#49620,#49621,#49622,#49623,#49624,
#49625,#49626,#49627,#49628,#49629,#49630,#49631,#49632,#49633,#49634,#49635,
#49636,#49637,#49638,#49639,#49640,#49641,#49642,#49643,#49644,#49645,#49646,
#49647,#49648,#49649,#49650,#49651,#49652,#49653,#49654,#49655,#49656,#49657,
#49658,#49659,#49660,#49661,#49662,#49663,#49664,#49665,#49666,#49667,#49668,
#49669,#49670,#49671,#49672,#49673,#49674,#49675,#49676,#49677,#49678,#49679,
#49680,#49681,#49682,#49683,#49684,#49685,#49686,#49687,#49688,#49689,#49690,
#49691,#49692,#49693,#49694,#49695,#49696,#49697,#49698,#49699,#49700,#49701,
#49702,#49703,#49704,#49705,#49706,#49707,#49708,#49709,#49710,#49711,#49712,
#49713,#49714,#49715,#49716,#49717,#49718,#49719,#49720,#49721,#49722,#49723,
#49724,#49725,#49726,#49727,#49728,#49729,#49730,#49731,#49732,#49733,#49734,
#49735,#49736,#49737,#49738,#49739,#49740,#49741,#49742,#49743,#49744,#49745,
#49746,#49747,#49748,#49749,#49750,#49751,#49752,#49753,#49754,#49755,#49756,
#49757,#49758,#49759,#49760,#49761,#49762,#49763,#49764,#49765,#49766,#49767,
#49768,#49769,#49770,#49771,#49772,#49773,#49774,#49775,#49776,#49777,#49778,
#49779,#49780,#49781,#49782,#49783,#49784,#49785,#49786,#49787,#49788,#49789,
#49790,#49791,#49792,#49793,#49794),.UNSPECIFIED.,.F.,.F.,(4,2,2,2,2,2,
2,2,2,2,2,2,2,2,2,2,2,2,2,2,2,2,2,2,2,2,2,2,2,2,2,2,2,2,2,2,2,2,2,2,2,2,
2,2,2,2,2,2,2,2,2,2,2,2,2,2,2,2,2,2,2,2,2,2,2,2,2,2,2,2,2,2,2,2,2,2,2,2,
2,2,2,2,2,2,2,2,2,2,2,2,2,2,2,2,2,2,2,2,2,2,2,2,2,4),(-2.51364950707999,
-2.46516245737415,-2.46005517763998,-2.45576754002935,-2.45318755664763,
-2.45086938983275,-2.44791164329971,-2.44318691055976,-2.40403108147615,
-2.3817763523131,-2.36570047798798,-2.3570881685732,-2.35478757315713,-2.35355825771939,
-2.35226531411621,-2.35063936543889,-2.34746250935437,-2.32261004107419,
-2.28039792543269,-2.26151107224442,-2.25702874626616,-2.25440603863628,
-2.25209492729012,-2.24920682686437,-2.2447120938145,-2.22024105461167,
-2.17419215983501,-2.15892103831632,-2.15612462883171,-2.1545993970621,
-2.15330546089989,-2.15166408790375,-2.14904800061621,-2.13450001635116,
-2.13105269901126,-2.11744862642065,-2.08021139904624,-2.06241048495044,
-2.05802609220555,-2.05542474162584,-2.05311030301585,-2.05018838508111,
-2.04558273145918,-2.01799466936758,-1.97486230763878,-1.95997130895771,
-1.95719271316586,-1.95567125582441,-1.95437688474557,-1.95273030180939,
-1.95009713149807,-1.93532539569104,-1.93156099143708,-1.89096967889108,
-1.86670067938995,-1.86039573032512,-1.85739736873002,-1.85507410795253,
-1.85251555981715,-1.84832611334552,-1.83456904106027,-1.77745464575305,
-1.7610988176287,-1.75825422161019,-1.75671849278625,-1.75542510772869,
-1.7537964120863,-1.7506077621314,-1.72470375950036,-1.68334369378189,-1.66459879954058,
-1.66014551148911,-1.65752876310615,-1.65521619427778,-1.65231738443914,
-1.64778871577487,-1.62247466217351,-1.58530993182366,-1.56447655225384,
-1.56011372478146,-1.55828894767348,-1.55697160527419,-1.5555475979752,
-1.55321297052502,-1.54568659129769,-1.48188938944291,-1.4709066146748,
-1.46306907324937,-1.45979882400841,-1.45743275793673,-1.45526906370794,
-1.45235453859142,-1.44520981142519,-1.39977491042776,-1.37417104185583,
-1.36648389757969,-1.36135784304428,-1.35941243019359,-1.35807281538934,
-1.35685512431365,-1.35517517251909,-1.35090243194385,-1.30701829225585,
-1.298038620556),.UNSPECIFIED.);
#587=B_SPLINE_CURVE_WITH_KNOTS('',3,(#49800,#49801,#49802,#49803,#49804,
#49805,#49806,#49807,#49808,#49809,#49810,#49811,#49812,#49813,#49814,#49815,
#49816,#49817,#49818,#49819,#49820,#49821,#49822,#49823,#49824,#49825,#49826,
#49827,#49828,#49829,#49830,#49831,#49832,#49833,#49834,#49835,#49836,#49837,
#49838,#49839,#49840,#49841,#49842,#49843,#49844,#49845,#49846,#49847,#49848,
#49849,#49850,#49851,#49852,#49853,#49854,#49855,#49856,#49857,#49858,#49859,
#49860,#49861,#49862,#49863,#49864,#49865,#49866,#49867,#49868,#49869,#49870,
#49871,#49872,#49873,#49874,#49875,#49876,#49877,#49878,#49879,#49880,#49881,
#49882,#49883,#49884,#49885,#49886,#49887,#49888,#49889,#49890,#49891,#49892,
#49893,#49894,#49895,#49896,#49897,#49898,#49899,#49900,#49901,#49902,#49903,
#49904,#49905,#49906,#49907,#49908,#49909,#49910,#49911,#49912,#49913,#49914,
#49915,#49916,#49917,#49918,#49919,#49920,#49921,#49922,#49923,#49924,#49925,
#49926,#49927,#49928,#49929,#49930,#49931,#49932,#49933,#49934,#49935,#49936,
#49937,#49938,#49939,#49940,#49941,#49942,#49943,#49944,#49945,#49946,#49947,
#49948,#49949,#49950,#49951,#49952,#49953,#49954,#49955,#49956,#49957,#49958,
#49959,#49960,#49961,#49962,#49963,#49964,#49965,#49966,#49967,#49968,#49969,
#49970,#49971,#49972,#49973,#49974,#49975,#49976,#49977,#49978,#49979,#49980,
#49981,#49982,#49983,#49984,#49985,#49986,#49987,#49988,#49989,#49990,#49991,
#49992,#49993,#49994,#49995,#49996,#49997,#49998,#49999,#50000,#50001,#50002,
#50003,#50004,#50005,#50006,#50007,#50008,#50009,#50010,#50011,#50012,#50013,
#50014,#50015,#50016,#50017,#50018,#50019,#50020,#50021,#50022,#50023,#50024,
#50025,#50026,#50027,#50028,#50029,#50030,#50031,#50032,#50033,#50034,#50035,
#50036,#50037,#50038,#50039,#50040,#50041,#50042,#50043,#50044,#50045,#50046,
#50047,#50048,#50049,#50050,#50051,#50052,#50053,#50054,#50055,#50056,#50057,
#50058,#50059,#50060,#50061,#50062,#50063,#50064,#50065,#50066,#50067),
 .UNSPECIFIED.,.F.,.F.,(4,2,2,2,2,2,2,2,2,2,2,2,2,2,2,2,2,2,2,2,2,2,2,2,
2,2,2,2,2,2,2,2,2,2,2,2,2,2,2,2,2,2,2,2,2,2,2,2,2,2,2,2,2,2,2,2,2,2,2,2,
2,2,2,2,2,2,2,2,2,2,2,2,2,2,2,2,2,2,2,2,2,2,2,2,2,2,2,2,2,2,2,2,2,2,2,2,
2,2,2,2,2,2,2,2,2,2,2,2,2,2,2,2,2,2,2,2,2,2,2,2,2,2,2,2,2,2,2,2,2,2,2,2,
2,4),(-1.21618442679459,-1.20602901916137,-1.17728167417851,-1.13783240099854,
-1.13309869507937,-1.13013798205412,-1.12781914414893,-1.1252401172321,
-1.12095808040505,-1.10446782140823,-1.04266508258569,-1.03331449682863,
-1.03078585013742,-1.02931869540624,-1.02801511219157,-1.02628232619738,
-1.02244482358703,-1.01718836886191,-1.00324957104713,-0.955506687798199,
-0.937586429586425,-0.933058921434141,-0.930399566244293,-0.928091403480923,
-0.925252352269582,-0.919755475683438,-0.91278238757453,-0.896728103080514,
-0.863506038814794,-0.835538756173074,-0.83234234548286,-0.8307119055099,
-0.829418308326185,-0.827883703775578,-0.825044802242606,-0.808826962190664,
-0.753450396021484,-0.738150714936052,-0.733798986162438,-0.731204503752045,
-0.729120016153655,-0.726298614565452,-0.720886880598065,-0.714049446300602,
-0.698447023878693,-0.660039824643096,-0.636474652985608,-0.633313804152959,
-0.631691031287016,-0.63039793471395,-0.62885730689311,-0.625989828171946,
-0.609071221681158,-0.58027714965765,-0.540804177800965,-0.536070537089696,
-0.533109711905419,-0.530790691707117,-0.528211364776918,-0.523928601172082,
-0.507432541859197,-0.445568323423664,-0.436268722056494,-0.433744828592099,
-0.432278644704489,-0.430974683344121,-0.429239716823355,-0.425390775152348,
-0.395529266777317,-0.344092827437908,-0.337314901950657,-0.334261190319299,
-0.331922060740202,-0.329411963983509,-0.325445430559417,-0.312347012519461,
-0.264606013869831,-0.238419037081571,-0.235227146902527,-0.233597557176833,
-0.232303864908656,-0.232298630006489,-0.232293472873671,-0.23228839252191,
-0.232283387303515,-0.232278456074548,-0.232273597844024,-0.232268811324586,
-0.232264095336892,-0.23225944866851,-0.232254870064762,-0.232250358445751,
-0.232245912749121,-0.232241531906298,-0.232237214942207,-0.232232960853369,
-0.232228654517377,-0.232224361742382,-0.232220082421133,-0.232215816227752,
-0.232211563214092,-0.232207323363667,-0.232203096720666,-0.232198882956517,
-0.232194682048601,-0.232190494181375,-0.232186319252025,-0.232182156831804,
-0.232178007069417,-0.232173869813819,-0.23216974514067,-0.232165632685057,
-0.230598809036455,-0.227597573119974,-0.223698117333866,-0.185933129451229,
-0.146059040181378,-0.138739071096871,-0.135799644110363,-0.133629232272127,
-0.131267223567011,-0.128023401909181,-0.12034931857652,-0.0993266993999184,
-0.0816547681768319,-0.0627343545680858,-0.0393728063109915,-0.0362144430830506,
-0.0345920434080208,-0.0332987611035165,-0.0320681220626925,-0.0305437290303957,
-0.0282358676238496,-0.00058235440496028),.UNSPECIFIED.);
#588=B_SPLINE_CURVE_WITH_KNOTS('',3,(#50068,#50069,#50070,#50071),
 .UNSPECIFIED.,.F.,.F.,(4,4),(-2.51480909694823,-2.47379053097235),
 .UNSPECIFIED.);
#589=B_SPLINE_CURVE_WITH_KNOTS('',3,(#50072,#50073,#50074,#50075,#50076,
#50077,#50078,#50079,#50080,#50081,#50082,#50083,#50084,#50085,#50086,#50087,
#50088,#50089,#50090,#50091,#50092,#50093,#50094,#50095,#50096,#50097,#50098,
#50099,#50100,#50101,#50102,#50103,#50104,#50105,#50106,#50107,#50108,#50109,
#50110,#50111,#50112,#50113,#50114,#50115,#50116,#50117,#50118,#50119,#50120,
#50121,#50122,#50123,#50124,#50125,#50126,#50127,#50128,#50129,#50130,#50131,
#50132,#50133,#50134,#50135,#50136,#50137,#50138,#50139,#50140,#50141,#50142,
#50143,#50144,#50145,#50146,#50147,#50148,#50149,#50150,#50151,#50152,#50153,
#50154,#50155,#50156,#50157,#50158,#50159,#50160,#50161,#50162,#50163,#50164,
#50165,#50166,#50167,#50168,#50169,#50170,#50171,#50172,#50173,#50174,#50175,
#50176,#50177,#50178,#50179,#50180,#50181,#50182,#50183,#50184,#50185,#50186,
#50187,#50188,#50189,#50190,#50191,#50192,#50193,#50194,#50195,#50196,#50197,
#50198,#50199,#50200,#50201,#50202,#50203,#50204,#50205,#50206,#50207,#50208,
#50209,#50210,#50211,#50212,#50213,#50214,#50215,#50216,#50217,#50218,#50219,
#50220,#50221,#50222,#50223,#50224,#50225,#50226,#50227,#50228,#50229,#50230,
#50231,#50232,#50233,#50234,#50235,#50236,#50237,#50238,#50239,#50240,#50241,
#50242,#50243,#50244,#50245,#50246,#50247,#50248,#50249,#50250,#50251,#50252,
#50253,#50254,#50255,#50256,#50257,#50258,#50259,#50260,#50261,#50262,#50263,
#50264,#50265,#50266,#50267,#50268,#50269,#50270,#50271,#50272,#50273,#50274,
#50275,#50276,#50277,#50278,#50279,#50280,#50281,#50282,#50283,#50284,#50285,
#50286,#50287,#50288,#50289,#50290,#50291,#50292,#50293,#50294,#50295,#50296,
#50297),.UNSPECIFIED.,.F.,.F.,(4,2,2,2,2,2,2,2,2,2,2,2,2,2,2,2,2,2,2,2,
2,2,2,2,2,2,2,2,2,2,2,2,2,2,2,2,2,2,2,2,2,2,2,2,2,2,2,2,2,2,2,2,2,2,2,2,
2,2,2,2,2,2,2,2,2,2,2,2,2,2,2,2,2,2,2,2,2,2,2,2,2,2,2,2,2,2,2,2,2,2,2,2,
2,2,2,2,2,2,2,2,2,2,2,2,2,2,2,2,2,2,2,2,4),(-1.298038620556,-1.28518477492575,
-1.26659110951169,-1.26214889648848,-1.25953479674532,-1.25722221376322,
-1.25432025570229,-1.2485099737604,-1.24103059169013,-1.22323486762303,
-1.18182496135094,-1.17836580391313,-1.16422782172899,-1.16163208277177,
-1.15999681531125,-1.15870319260542,-1.15717303208584,-1.15435395906807,
-1.13858350023123,-1.08807524478368,-1.06815460073119,-1.06348447848502,
-1.06079298808077,-1.05850962691057,-1.05572198480439,-1.05047134461615,
-1.00668118447764,-1.00437172518463,-0.968198674133801,-0.963441883720382,
-0.961498094337659,-0.960172118688768,-0.958791618565002,-0.956653204195387,
-0.950090216242167,-0.939316412722717,-0.88598819475271,-0.868801014420672,
-0.864330576459267,-0.861684811153804,-0.859376203650546,-0.856520858579278,
-0.850941559411361,-0.812451150535233,-0.768542688842383,-0.764269501946701,
-0.762589470364484,-0.761371760340662,-0.760032159631958,-0.758086834263315,
-0.752961332050261,-0.745276149825901,-0.719682632012063,-0.674275634441559,
-0.667131684008038,-0.664217292874704,-0.66205362633767,-0.659687520292765,
-0.656417099670902,-0.648578626422449,-0.63759289911443,-0.573788637756297,
-0.566240713939279,-0.563903430862806,-0.562478766745775,-0.561161553900476,
-0.559338013177925,-0.554983019012877,-0.53422835773226,-0.509010619116768,
-0.472134220389905,-0.467372634548957,-0.464403311419755,-0.462083160494708,
-0.459508245663754,-0.455246081259015,-0.439001343358237,-0.407501199655168,
-0.371216127374185,-0.366452132230693,-0.364506867544745,-0.363180376456594,
-0.361799824160692,-0.359662169040866,-0.353108098743345,-0.342355806521128,
-0.289398155463731,-0.271840828526119,-0.267340865108757,-0.264687930608783,
-0.262379378787629,-0.259532212314096,-0.253995100933304,-0.246957478626795,
-0.23068548910416,-0.180067527739042,-0.168886447477057,-0.166232598349115,
-0.164722109847122,-0.163426175483797,-0.162162938960683,-0.159612812438825,
-0.146885778986395,-0.117779555395451,-0.0774601860868628,-0.0742590008540955,
-0.0694234780118543,-0.0664319935225179,-0.0641090963614894,-0.0615459281247616,
-0.0573373953712801,-0.0523476908568135,-0.0416325986123643),
 .UNSPECIFIED.);
#590=B_SPLINE_CURVE_WITH_KNOTS('',3,(#50302,#50303,#50304,#50305,#50306,
#50307,#50308,#50309,#50310,#50311,#50312,#50313,#50314,#50315,#50316,#50317,
#50318,#50319,#50320,#50321,#50322,#50323,#50324,#50325,#50326,#50327,#50328,
#50329,#50330,#50331,#50332,#50333,#50334,#50335,#50336,#50337,#50338,#50339,
#50340,#50341,#50342,#50343,#50344,#50345,#50346,#50347,#50348,#50349,#50350,
#50351,#50352,#50353,#50354,#50355,#50356,#50357,#50358,#50359,#50360,#50361,
#50362,#50363,#50364,#50365,#50366,#50367,#50368,#50369,#50370,#50371,#50372,
#50373,#50374,#50375,#50376,#50377,#50378,#50379,#50380,#50381,#50382,#50383,
#50384,#50385,#50386,#50387,#50388,#50389,#50390,#50391,#50392,#50393,#50394,
#50395,#50396,#50397,#50398,#50399,#50400,#50401,#50402,#50403,#50404,#50405,
#50406,#50407,#50408,#50409,#50410,#50411,#50412,#50413,#50414,#50415,#50416,
#50417,#50418,#50419,#50420,#50421,#50422,#50423,#50424,#50425,#50426,#50427,
#50428,#50429,#50430,#50431,#50432,#50433,#50434,#50435,#50436,#50437,#50438,
#50439,#50440,#50441,#50442,#50443,#50444,#50445,#50446,#50447,#50448,#50449,
#50450,#50451,#50452,#50453,#50454,#50455,#50456,#50457,#50458,#50459,#50460,
#50461,#50462,#50463,#50464,#50465,#50466,#50467,#50468,#50469,#50470,#50471,
#50472,#50473,#50474,#50475,#50476,#50477,#50478,#50479,#50480,#50481,#50482,
#50483,#50484,#50485,#50486,#50487,#50488,#50489,#50490,#50491,#50492,#50493,
#50494,#50495,#50496,#50497,#50498,#50499,#50500,#50501,#50502,#50503,#50504,
#50505,#50506,#50507,#50508,#50509,#50510,#50511,#50512,#50513,#50514,#50515,
#50516,#50517,#50518,#50519,#50520,#50521,#50522,#50523,#50524,#50525,#50526,
#50527,#50528,#50529,#50530,#50531,#50532,#50533),.UNSPECIFIED.,.F.,.F.,
(4,2,2,2,2,2,2,2,2,2,2,2,2,2,2,2,2,2,2,2,2,2,2,2,2,2,2,2,2,2,2,2,2,2,2,
2,2,2,2,2,2,2,2,2,2,2,2,2,2,2,2,2,2,2,2,2,2,2,2,2,2,2,2,2,2,2,2,2,2,2,2,
2,2,2,2,2,2,2,2,2,2,2,2,2,2,2,2,2,2,2,2,2,2,2,2,2,2,2,2,2,2,2,2,2,2,2,2,
2,2,2,2,2,2,2,2,4),(-2.47226785878759,-2.44315262999097,-2.4265493773509,
-2.42369517961594,-2.4221576717896,-2.42086481042697,-2.41923932921738,
-2.41606445023606,-2.39136211892146,-2.34495212060522,-2.32954671256529,
-2.32646922213363,-2.32372673233149,-2.32368173597199,-2.32363591157625,
-2.32358917750693,-2.32354144531909,-2.32349261869542,-2.32138662359374,
-2.31878608606322,-2.31458483610215,-2.29992789744491,-2.24972977461377,
-2.23484724352276,-2.22935852650405,-2.22539113236106,-2.22363522959312,
-2.22232891709944,-2.22087470883029,-2.21840303053684,-2.20962256755983,
-2.14725270028537,-2.13072560853464,-2.12644158137443,-2.12386266129053,
-2.12154474615733,-2.11858635123024,-2.11385861866163,-2.07437290301597,
-2.0455643345363,-2.0286571824889,-2.02579096297739,-2.02425098809859,-2.02295842092606,
-2.02133629634428,-2.01817666430633,-1.99459470257733,-1.95619068143742,
-1.94064592648934,-1.93382638990624,-1.92842599729637,-1.92560760865676,
-1.9235241398696,-1.92092938379755,-1.91657348357221,-1.9012135598243,-1.84589992968617,
-1.82968748645245,-1.8268494962571,-1.82531542242399,-1.82402229010215,
-1.82239246683785,-1.81919735475115,-1.78964838535882,-1.75122451981294,
-1.73313848852572,-1.72873323226305,-1.72612743795481,-1.72381393800529,
-1.72089977282247,-1.71631928020207,-1.68950850830298,-1.6456623496029,
-1.63067487493781,-1.62789183078225,-1.62636949052947,-1.62507531930725,
-1.62343020791712,-1.62080168706969,-1.60599736991801,-1.6016956259522,
-1.58936041687335,-1.5573174904848,-1.54240876289479,-1.53578261411349,
-1.53050406740892,-1.52771061083931,-1.52562929209383,-1.52301601410596,
-1.51857725781707,-1.50234770938831,-1.44796322564263,-1.43712141379915,
-1.43052934755061,-1.42838731951397,-1.42700597246057,-1.42568044721729,
-1.42373928147752,-1.41899866957122,-1.38237238157978,-1.35114408966658,
-1.33498087006502,-1.33072601837987,-1.32815295531946,-1.32583283076147,
-1.32286126356138,-1.31809138604049,-1.28162623786546,-1.25685729748551,
-1.23348909408972,-1.23033134675811,-1.22870931924426,-1.22741636345724,
-1.22587536583413,-1.2230057744408,-1.21618442679459),.UNSPECIFIED.);
#591=B_SPLINE_CURVE_WITH_KNOTS('',3,(#50535,#50536,#50537,#50538),
 .UNSPECIFIED.,.F.,.F.,(4,4),(-0.0416325986123643,-0.00058313060358834),
 .UNSPECIFIED.);
#592=B_SPLINE_CURVE_WITH_KNOTS('',3,(#50539,#50540,#50541,#50542,#50543,
#50544,#50545,#50546,#50547,#50548,#50549,#50550,#50551,#50552,#50553,#50554,
#50555,#50556,#50557,#50558,#50559,#50560,#50561,#50562,#50563,#50564,#50565,
#50566,#50567,#50568,#50569,#50570,#50571,#50572,#50573,#50574,#50575,#50576,
#50577,#50578,#50579,#50580,#50581,#50582,#50583,#50584,#50585,#50586,#50587,
#50588,#50589,#50590,#50591,#50592,#50593,#50594,#50595,#50596,#50597,#50598,
#50599,#50600,#50601,#50602,#50603,#50604,#50605,#50606,#50607,#50608,#50609,
#50610,#50611,#50612,#50613,#50614,#50615,#50616,#50617,#50618,#50619,#50620,
#50621,#50622,#50623,#50624,#50625,#50626,#50627,#50628,#50629,#50630,#50631,
#50632,#50633,#50634,#50635,#50636,#50637,#50638,#50639,#50640,#50641,#50642,
#50643,#50644,#50645,#50646,#50647,#50648,#50649,#50650,#50651,#50652,#50653,
#50654,#50655,#50656,#50657,#50658,#50659,#50660,#50661,#50662,#50663,#50664,
#50665,#50666,#50667,#50668,#50669,#50670,#50671,#50672,#50673,#50674,#50675,
#50676,#50677,#50678,#50679,#50680,#50681,#50682,#50683,#50684,#50685,#50686,
#50687,#50688,#50689,#50690,#50691,#50692,#50693,#50694,#50695,#50696,#50697,
#50698,#50699,#50700,#50701,#50702,#50703,#50704,#50705,#50706,#50707,#50708,
#50709,#50710,#50711,#50712,#50713,#50714,#50715,#50716,#50717,#50718,#50719,
#50720,#50721,#50722,#50723,#50724,#50725,#50726,#50727,#50728,#50729,#50730,
#50731,#50732,#50733,#50734,#50735,#50736,#50737,#50738,#50739,#50740,#50741,
#50742,#50743,#50744,#50745,#50746,#50747,#50748,#50749,#50750,#50751,#50752,
#50753,#50754,#50755,#50756,#50757,#50758,#50759,#50760,#50761,#50762,#50763,
#50764,#50765,#50766,#50767,#50768,#50769,#50770,#50771,#50772,#50773,#50774,
#50775,#50776,#50777,#50778,#50779,#50780,#50781,#50782,#50783,#50784,#50785,
#50786,#50787,#50788,#50789,#50790,#50791,#50792,#50793,#50794,#50795,#50796,
#50797,#50798,#50799,#50800),.UNSPECIFIED.,.F.,.F.,(4,2,2,2,2,2,2,2,2,2,
2,2,2,2,2,2,2,2,2,2,2,2,2,2,2,2,2,2,2,2,2,2,2,2,2,2,2,2,2,2,2,2,2,2,2,2,
2,2,2,2,2,2,2,2,2,2,2,2,2,2,2,2,2,2,2,2,2,2,2,2,2,2,2,2,2,2,2,2,2,2,2,2,
2,2,2,2,2,2,2,2,2,2,2,2,2,2,2,2,2,2,2,2,2,2,2,2,2,2,2,2,2,2,2,2,2,2,2,2,
2,2,2,2,2,2,2,2,2,2,2,2,4),(-2.51400264948435,-2.48421836071445,-2.48192163669727,
-2.48040181517654,-2.47917229137992,-2.47787865972753,-2.47625012840667,
-2.47306319379138,-2.44741318866998,-2.42529602530809,-2.40088110763266,
-2.38642684357947,-2.38230233158867,-2.37975744191638,-2.37742943659178,
-2.37445087829526,-2.36955085144401,-2.36646446508994,-2.32614418677038,
-2.28874616452835,-2.28486187851215,-2.28187238973397,-2.28030678901279,
-2.28030267401512,-2.2802985464738,-2.28029440633816,-2.28029025383883,
-2.28028608858994,-2.28028191080908,-2.28027771999208,-2.28027351615463,
-2.28026929938522,-2.28026506959409,-2.28026082671353,-2.28025657058589,
-2.28025230108468,-2.28024801814176,-2.28024372186064,-2.2802394120175,
-2.28023513939178,-2.28023080342924,-2.28022640299119,-2.28022193709567,
-2.2802174049142,-2.28021280536375,-2.28020813695118,-2.28020339868081,
-2.28019858944706,-2.28019370816035,-2.28018875346816,-2.2801837239967,
-2.27889021515564,-2.2772669983009,-2.27410549855148,-2.24256840317327,
-2.22909775646131,-2.19000465811213,-2.18440338265633,-2.18154262245319,
-2.17923245949173,-2.17658800594296,-2.17212717701184,-2.15510854333331,
-2.10627900681833,-2.09233449351235,-2.08707633689177,-2.08323790214284,
-2.08150466404738,-2.08020073617748,-2.07873317016305,-2.0762037903952,
-2.06684996307841,-2.00505911035982,-1.98856852355242,-1.98428554311218,
-1.98170576625952,-1.97938613691062,-1.97642425226807,-1.9716883033089,
-1.93219771653853,-1.90339715313762,-1.88644220837923,-1.88357263561294,
-1.88203132944743,-1.88073792230771,-1.87911509336461,-1.87595510449785,
-1.85285401555903,-1.82068547130729,-1.79355103555675,-1.78687294651153,
-1.78380395321282,-1.78147025418424,-1.77894362239403,-1.77490255597318,
-1.7624480762994,-1.70991782953796,-1.68961524574869,-1.68530747157291,
-1.68349158038617,-1.68217534868089,-1.68074693338009,-1.67839399384082,
-1.67071536034148,-1.61287886515058,-1.59112116830058,-1.58647611847225,
-1.58381703823214,-1.58150843128679,-1.57866796227263,-1.57433128493264,
-1.55313559585049,-1.50385364861007,-1.4933504819802,-1.48901191318128,
-1.48570798427628,-1.48407701440211,-1.48290724750031,-1.48142219231935,
-1.47887988230922,-1.46906552985234,-1.40777556394142,-1.39132554786916,
-1.38704608146942,-1.3844671771677,-1.38214754171373,-1.37918455818483,
-1.37444463789547,-1.33513412792569,-1.30671152878061,-1.2981223786512),
 .UNSPECIFIED.);
#593=B_SPLINE_CURVE_WITH_KNOTS('',3,(#50806,#50807,#50808,#50809,#50810,
#50811,#50812,#50813,#50814,#50815,#50816,#50817,#50818,#50819,#50820,#50821,
#50822,#50823,#50824,#50825,#50826,#50827,#50828,#50829,#50830,#50831,#50832,
#50833,#50834,#50835,#50836,#50837,#50838,#50839,#50840,#50841,#50842,#50843,
#50844,#50845,#50846,#50847,#50848,#50849,#50850,#50851,#50852,#50853,#50854,
#50855,#50856,#50857,#50858,#50859,#50860,#50861,#50862,#50863,#50864,#50865,
#50866,#50867,#50868,#50869,#50870,#50871,#50872,#50873,#50874,#50875,#50876,
#50877,#50878,#50879,#50880,#50881,#50882,#50883,#50884,#50885,#50886,#50887,
#50888,#50889,#50890,#50891,#50892,#50893,#50894,#50895,#50896,#50897,#50898,
#50899,#50900,#50901,#50902,#50903,#50904,#50905,#50906,#50907,#50908,#50909,
#50910,#50911,#50912,#50913,#50914,#50915,#50916,#50917,#50918,#50919,#50920,
#50921,#50922,#50923,#50924,#50925,#50926,#50927,#50928,#50929,#50930,#50931,
#50932,#50933,#50934,#50935,#50936,#50937,#50938,#50939,#50940,#50941,#50942,
#50943,#50944,#50945,#50946,#50947,#50948,#50949,#50950,#50951,#50952,#50953,
#50954,#50955,#50956,#50957,#50958,#50959,#50960,#50961,#50962,#50963,#50964,
#50965,#50966,#50967,#50968,#50969,#50970,#50971,#50972,#50973,#50974,#50975,
#50976,#50977,#50978,#50979,#50980,#50981,#50982,#50983,#50984,#50985,#50986,
#50987,#50988,#50989,#50990,#50991,#50992,#50993,#50994,#50995,#50996,#50997,
#50998,#50999,#51000,#51001,#51002,#51003,#51004,#51005,#51006,#51007,#51008,
#51009,#51010,#51011,#51012,#51013,#51014,#51015,#51016,#51017,#51018,#51019,
#51020,#51021,#51022,#51023,#51024,#51025),.UNSPECIFIED.,.F.,.F.,(4,2,2,
2,2,2,2,2,2,2,2,2,2,2,2,2,2,2,2,2,2,2,2,2,2,2,2,2,2,2,2,2,2,2,2,2,2,2,2,
2,2,2,2,2,2,2,2,2,2,2,2,2,2,2,2,2,2,2,2,2,2,2,2,2,2,2,2,2,2,2,2,2,2,2,2,
2,2,2,2,2,2,2,2,2,2,2,2,2,2,2,2,2,2,2,2,2,2,2,2,2,2,2,2,2,2,2,2,2,2,4),
(-1.21660469756962,-1.21560513177792,-1.20832163108235,-1.20538563640586,
-1.2032160417423,-1.20085326046503,-1.19760535281686,-1.18990717030479,
-1.17917873754424,-1.147696759036,-1.11135820733462,-1.10660537746665,-1.1046617879558,
-1.1033354744309,-1.10195415414047,-1.09981365600362,-1.0932378797993,-1.0824363957164,
-1.02870806498096,-1.01187539626733,-1.00737826174651,-1.00475158765139,
-1.00246182527359,-0.999587416253969,-0.993917377552048,-0.95259563762134,
-0.912034853681237,-0.907470599208752,-0.905746551472394,-0.904516967928173,
-0.903186986538914,-0.901293145058762,-0.896507014298174,-0.889492369840031,
-0.867582639851953,-0.816632155793302,-0.80979793441561,-0.806734035387213,
-0.804393177932454,-0.801887137747357,-0.797939543990976,-0.785020376258243,
-0.763140183789312,-0.733722921882351,-0.727883598997912,-0.724268933398251,
-0.710320822671981,-0.707734310524198,-0.706101580902123,-0.704807746316235,
-0.703274720763992,-0.700443584799953,-0.684411747932148,-0.631217593331959,
-0.61388102336528,-0.609397841651758,-0.606748631557248,-0.60443953544755,
-0.601586828982065,-0.596023203713855,-0.55804042668657,-0.515496433565771,
-0.509809636449915,-0.507718001094443,-0.50648372969871,-0.505157492075355,
-0.503283384681019,-0.498621099075318,-0.474793280554394,-0.453883256124921,
-0.416142165685547,-0.411406773649788,-0.408445143824071,-0.406125672957546,
-0.403546029663099,-0.399263175365165,-0.382772470098717,-0.32100364952033,
-0.31160406007368,-0.30907029991932,-0.307601774890138,-0.306298078656024,
-0.304566633046494,-0.30073794472848,-0.295497469601035,-0.281624077645052,
-0.234094897535137,-0.215890789942289,-0.211336251199948,-0.208670270878735,
-0.206407968288284,-0.203850973880011,-0.200965344285523,-0.196470140986856,
-0.170933518498077,-0.13529488257053,-0.113675948221446,-0.110532110167491,
-0.108912655120551,-0.107619292972448,-0.106074890376176,-0.103191184303473,
-0.0858759175043473,-0.0250529057732762,-0.0150319442351391,-0.0113202422794324,
-0.00911053038409564,-0.0068859470510532,-0.00461814312859361,-0.000582527892639659),
 .UNSPECIFIED.);
#594=B_SPLINE_CURVE_WITH_KNOTS('',3,(#51026,#51027,#51028,#51029,#51030,
#51031,#51032,#51033),.UNSPECIFIED.,.F.,.F.,(4,2,2,4),(-2.51302961979646,
-2.50312569535042,-2.47230189720855,-2.47226785878759),.UNSPECIFIED.);
#595=B_SPLINE_CURVE_WITH_KNOTS('',3,(#51034,#51035,#51036,#51037,#51038,
#51039,#51040,#51041,#51042,#51043,#51044,#51045,#51046,#51047,#51048,#51049,
#51050,#51051,#51052,#51053,#51054,#51055,#51056,#51057,#51058,#51059,#51060,
#51061,#51062,#51063,#51064,#51065,#51066,#51067,#51068,#51069,#51070,#51071,
#51072,#51073,#51074,#51075,#51076,#51077,#51078,#51079,#51080,#51081,#51082,
#51083,#51084,#51085,#51086,#51087,#51088,#51089,#51090,#51091,#51092,#51093,
#51094,#51095,#51096,#51097,#51098,#51099,#51100,#51101,#51102,#51103,#51104,
#51105,#51106,#51107,#51108,#51109,#51110,#51111,#51112,#51113,#51114,#51115,
#51116,#51117,#51118,#51119,#51120,#51121,#51122,#51123,#51124,#51125,#51126,
#51127,#51128,#51129,#51130,#51131,#51132,#51133,#51134,#51135,#51136,#51137,
#51138,#51139,#51140,#51141,#51142,#51143,#51144,#51145,#51146,#51147,#51148,
#51149,#51150,#51151,#51152,#51153,#51154,#51155,#51156,#51157,#51158,#51159,
#51160,#51161,#51162,#51163,#51164,#51165,#51166,#51167,#51168,#51169,#51170,
#51171,#51172,#51173,#51174,#51175,#51176,#51177,#51178,#51179,#51180,#51181,
#51182,#51183,#51184,#51185,#51186,#51187,#51188,#51189,#51190,#51191,#51192,
#51193,#51194,#51195,#51196,#51197,#51198,#51199,#51200,#51201,#51202,#51203,
#51204,#51205,#51206,#51207,#51208,#51209,#51210,#51211,#51212,#51213,#51214,
#51215,#51216,#51217,#51218,#51219,#51220,#51221,#51222,#51223,#51224,#51225,
#51226,#51227,#51228,#51229,#51230,#51231,#51232,#51233,#51234,#51235,#51236,
#51237,#51238,#51239,#51240,#51241,#51242,#51243,#51244,#51245,#51246,#51247,
#51248,#51249,#51250,#51251,#51252,#51253,#51254,#51255,#51256,#51257,#51258,
#51259,#51260,#51261,#51262,#51263,#51264,#51265,#51266,#51267,#51268,#51269,
#51270,#51271,#51272,#51273,#51274,#51275,#51276,#51277,#51278,#51279),
 .UNSPECIFIED.,.F.,.F.,(4,2,2,2,2,2,2,2,2,2,2,2,2,2,2,2,2,2,2,2,2,2,2,2,
2,2,2,2,2,2,2,2,2,2,2,2,2,2,2,2,2,2,2,2,2,2,2,2,2,2,2,2,2,2,2,2,2,2,2,2,
2,2,2,2,2,2,2,2,2,2,2,2,2,2,2,2,2,2,2,2,2,2,2,2,2,2,2,2,2,2,2,2,2,2,2,2,
2,2,2,2,2,2,2,2,2,2,2,2,2,2,2,2,2,2,2,2,2,2,2,2,2,2,4),(-1.2981223786512,
-1.2892459881527,-1.2863568195862,-1.28481140686892,-1.28351831515963,-1.28190060790969,
-1.27876421797423,-1.2574525993154,-1.20862501435937,-1.19257426809608,
-1.18815147564813,-1.185541125541,-1.18345857202648,-1.18065884250332,-1.17535303922238,
-1.13132657066651,-1.11873435243647,-1.09078747636709,-1.08759075686629,
-1.08596016618755,-1.08466645304877,-1.08313171527733,-1.08029257868359,
-1.06407373543308,-1.00869780993439,-0.993391491732283,-0.989038921728858,
-0.986444107872633,-0.98435944952,-0.981537942179059,-0.976126435237369,
-0.969289520945197,-0.95368945582181,-0.915268874499263,-0.891705299202744,
-0.888544219078316,-0.886921312012993,-0.885628100256878,-0.884087325497926,
-0.881219547656855,-0.864298360366526,-0.835502470743149,-0.796026287637618,
-0.791292213826143,-0.788331120784207,-0.786011892691552,-0.783432336506779,
-0.779149196934187,-0.762651752870428,-0.700783273382089,-0.691481607473425,
-0.688957369455633,-0.687491028149465,-0.68618695650777,-0.684451883529049,
-0.680602864638799,-0.651467332720191,-0.599132316921038,-0.592462231962627,
-0.589427857296861,-0.587091611470286,-0.584572872022557,-0.580567474829767,
-0.567097949324753,-0.519537403066136,-0.493609003853499,-0.490418963370928,
-0.488789688590706,-0.487495913237913,-0.485959795333883,-0.483114689260777,
-0.466759911375288,-0.409651956494921,-0.395893709953167,-0.391703266766024,
-0.389143953734435,-0.386819895074774,-0.38382035859433,-0.37751241408995,
-0.353226022170356,-0.312599495962939,-0.308832167592656,-0.2940459943494,
-0.291411380084304,-0.289764071049895,-0.288469238850304,-0.28694735713961,
-0.284168303378318,-0.269281203640925,-0.226186761564817,-0.198573150191097,
-0.193962823065936,-0.191038905908958,-0.188778399240402,-0.188684497229446,
-0.188608927082289,-0.188547336342364,-0.188496637954795,-0.188454572900009,
-0.188419445739269,-0.188389957202828,-0.188337538842759,-0.188286914050502,
-0.188237938368303,-0.188190481228795,-0.18814442419915,-0.188099659591416,
-0.188056089114478,-0.188013622782854,-0.187972178006164,-0.185170242457677,
-0.182083928901597,-0.177103198736196,-0.16718128626347,-0.120765531311188,
-0.0955142687044764,-0.0923311215095132,-0.0907033688591454,-0.0894097423535389,
-0.0878725484329314,-0.0850221642633632,-0.0685376748017855,-0.0413768992123694),
 .UNSPECIFIED.);
#596=B_SPLINE_CURVE_WITH_KNOTS('',3,(#51284,#51285,#51286,#51287,#51288,
#51289,#51290,#51291,#51292,#51293,#51294,#51295,#51296,#51297,#51298,#51299,
#51300,#51301,#51302,#51303,#51304,#51305,#51306,#51307,#51308,#51309,#51310,
#51311,#51312,#51313,#51314,#51315,#51316,#51317,#51318,#51319,#51320,#51321,
#51322,#51323,#51324,#51325,#51326,#51327,#51328,#51329,#51330,#51331,#51332,
#51333,#51334,#51335,#51336,#51337,#51338,#51339,#51340,#51341,#51342,#51343,
#51344,#51345,#51346,#51347,#51348,#51349,#51350,#51351,#51352,#51353,#51354,
#51355,#51356,#51357,#51358,#51359,#51360,#51361,#51362,#51363,#51364,#51365,
#51366,#51367,#51368,#51369,#51370,#51371,#51372,#51373,#51374,#51375,#51376,
#51377,#51378,#51379,#51380,#51381,#51382,#51383,#51384,#51385,#51386,#51387,
#51388,#51389,#51390,#51391,#51392,#51393,#51394,#51395,#51396,#51397,#51398,
#51399,#51400,#51401,#51402,#51403,#51404,#51405,#51406,#51407,#51408,#51409,
#51410,#51411,#51412,#51413,#51414,#51415,#51416,#51417,#51418,#51419,#51420,
#51421,#51422,#51423,#51424,#51425,#51426,#51427,#51428,#51429,#51430,#51431,
#51432,#51433,#51434,#51435,#51436,#51437,#51438,#51439,#51440,#51441,#51442,
#51443,#51444,#51445,#51446,#51447,#51448,#51449,#51450,#51451,#51452,#51453,
#51454,#51455,#51456,#51457,#51458,#51459,#51460,#51461,#51462,#51463,#51464,
#51465,#51466,#51467,#51468,#51469,#51470,#51471,#51472,#51473,#51474,#51475,
#51476,#51477,#51478,#51479,#51480,#51481,#51482,#51483,#51484,#51485,#51486,
#51487),.UNSPECIFIED.,.F.,.F.,(4,2,2,2,2,2,2,2,2,2,2,2,2,2,2,2,2,2,2,2,
2,2,2,2,2,2,2,2,2,2,2,2,2,2,2,2,2,2,2,2,2,2,2,2,2,2,2,2,2,2,2,2,2,2,2,2,
2,2,2,2,2,2,2,2,2,2,2,2,2,2,2,2,2,2,2,2,2,2,2,2,2,2,2,2,2,2,2,2,2,2,2,2,
2,2,2,2,2,2,2,2,2,4),(-2.47330243401613,-2.42245091809077,-2.40486508519416,
-2.40049612610248,-2.39789774407745,-2.39558210310781,-2.39265347595769,
-2.38802695167722,-2.35979244577488,-2.30812033644537,-2.30351601419034,
-2.30108490173506,-2.29902432207317,-2.29767158938404,-2.29634483716351,
-2.2943986594292,-2.28962973924138,-2.25379289806888,-2.22199101529607,
-2.2056553257859,-2.20138531570239,-2.19880849348897,-2.19648842755216,
-2.19352170992676,-2.18876934135159,-2.15384875722703,-2.12912419348526,
-2.1061643608833,-2.10158618358893,-2.09972563089072,-2.09840185315068,
-2.09699096812524,-2.09471618273464,-2.087685359805,-2.02912550058502,-2.0147172656301,
-2.00510401090219,-2.00156268898467,-1.99914346871885,-1.99677963687774,
-1.99392760018832,-1.98698233139921,-1.9379740026273,-1.90603539007453,
-1.90219087256393,-1.90045679003201,-1.89915303213149,-1.89768654845573,
-1.89516100085917,-1.88584271509496,-1.82403207922562,-1.80754299005997,
-1.80326089516825,-1.80068173939704,-1.79836272417135,-1.79540170044825,
-1.7906672836817,-1.75117477108976,-1.72235506387672,-1.70544042188533,
-1.70257301873896,-1.70103241645799,-1.69973932772334,-1.6981165549582,
-1.69495567882391,-1.67136645436436,-1.6329670902671,-1.61740218266273,
-1.61057570165538,-1.6051704929249,-1.60235042224918,-1.6002660540789,-1.59767062009864,
-1.59331464426795,-1.57796748675147,-1.52261106371159,-1.50639040547052,
-1.50355119815981,-1.50201648948937,-1.5007228358218,-1.49909237293609,
-1.49589605837859,-1.46861168488881,-1.43317733018402,-1.41809223435838,
-1.41141130619422,-1.4060977246328,-1.40329640277701,-1.40121371354766,
-1.39860456922296,-1.39418717582083,-1.37819303451522,-1.32352925888638,
-1.31266838404468,-1.30606740809001,-1.30392384900638,-1.30254185730772,
-1.30121600648613,-1.29927481619259,-1.29453640384491,-1.25762792083579,
-1.21660469756962),.UNSPECIFIED.);
#597=B_SPLINE_CURVE_WITH_KNOTS('',3,(#51489,#51490,#51491,#51492,#51493,
#51494),.UNSPECIFIED.,.F.,.F.,(4,2,4),(-0.0413768992123694,-0.0396266779595947,
-0.000583049282567826),.UNSPECIFIED.);
#598=B_SPLINE_CURVE_WITH_KNOTS('',3,(#51495,#51496,#51497,#51498,#51499,
#51500,#51501,#51502,#51503,#51504,#51505,#51506,#51507,#51508,#51509,#51510,
#51511,#51512,#51513,#51514,#51515,#51516,#51517,#51518,#51519,#51520,#51521,
#51522,#51523,#51524,#51525,#51526,#51527,#51528,#51529,#51530,#51531,#51532,
#51533,#51534,#51535,#51536,#51537,#51538,#51539,#51540,#51541,#51542,#51543,
#51544,#51545,#51546,#51547,#51548,#51549,#51550,#51551,#51552,#51553,#51554,
#51555,#51556,#51557,#51558,#51559,#51560,#51561,#51562,#51563,#51564,#51565,
#51566,#51567,#51568,#51569,#51570,#51571,#51572,#51573,#51574,#51575,#51576,
#51577,#51578,#51579,#51580,#51581,#51582,#51583,#51584,#51585,#51586,#51587,
#51588,#51589,#51590,#51591,#51592,#51593,#51594,#51595,#51596,#51597,#51598,
#51599,#51600,#51601,#51602,#51603,#51604,#51605,#51606,#51607,#51608,#51609,
#51610,#51611,#51612,#51613,#51614,#51615,#51616,#51617,#51618,#51619,#51620,
#51621,#51622,#51623,#51624,#51625,#51626,#51627,#51628,#51629,#51630,#51631,
#51632,#51633,#51634,#51635,#51636,#51637,#51638,#51639,#51640,#51641,#51642,
#51643,#51644,#51645,#51646,#51647,#51648,#51649,#51650,#51651,#51652,#51653,
#51654,#51655,#51656,#51657,#51658,#51659,#51660,#51661,#51662,#51663,#51664,
#51665,#51666,#51667,#51668,#51669,#51670,#51671,#51672,#51673,#51674,#51675,
#51676,#51677,#51678,#51679,#51680,#51681,#51682,#51683,#51684,#51685,#51686,
#51687,#51688,#51689,#51690,#51691,#51692,#51693,#51694,#51695,#51696,#51697,
#51698,#51699,#51700,#51701,#51702,#51703,#51704,#51705,#51706,#51707,#51708,
#51709,#51710,#51711,#51712),.UNSPECIFIED.,.F.,.F.,(4,2,2,2,2,2,2,2,2,2,
2,2,2,2,2,2,2,2,2,2,2,2,2,2,2,2,2,2,2,2,2,2,2,2,2,2,2,2,2,2,2,2,2,2,2,2,
2,2,2,2,2,2,2,2,2,2,2,2,2,2,2,2,2,2,2,2,2,2,2,2,2,2,2,2,2,2,2,2,2,2,2,2,
2,2,2,2,2,2,2,2,2,2,2,2,2,2,2,2,2,2,2,2,2,2,2,2,2,2,4),(-2.51327713688667,
-2.51013830636087,-2.50709747201508,-2.50484278771018,-2.50260877932776,
-2.50038437760381,-2.4965899563431,-2.48597608443706,-2.42540070554653,
-2.40862072766969,-2.40575971115735,-2.4042208962479,-2.402928336082,-2.40130500076025,
-2.39813946372172,-2.37411751586636,-2.33645917876175,-2.32073492763113,
-2.31386141821673,-2.31001529286203,-2.30739913737221,-2.30489807320466,
-2.30264335814387,-2.29968183354299,-2.29494350057941,-2.25551157182444,
-2.22729377002798,-2.20980399058925,-2.20691533209874,-2.20537062231407,
-2.20407837016926,-2.20246202895205,-2.19992771589964,-2.18692044017818,
-2.18500081396825,-2.18054274361608,-2.14353957294601,-2.11422385720625,
-2.10924421555971,-2.10651419163426,-2.10443830128812,-2.10177523738696,
-2.09722784245689,-2.07906677141334,-2.02674393302767,-2.01603252412601,
-2.00949767248197,-2.00736291749321,-2.00598339693557,-2.00465716641096,
-2.00271116465616,-1.99793973470904,-1.96229386775239,-1.91598641569552,
-1.91058744700268,-1.90776931635448,-1.90568583743934,-1.90309081052351,
-1.89873383491006,-1.88336259831357,-1.82805960200115,-1.81184777304384,
-1.80900976361067,-1.80747566618814,-1.80618250612422,-1.8045526380147,
-1.80135740896999,-1.7738513440458,-1.76684167449921,-1.7326897473506,-1.71522098034031,
-1.71086186562058,-1.70826614185077,-1.7059508796863,-1.70302003710355,
-1.69838465557649,-1.66981556500371,-1.61828518355143,-1.61162197191828,
-1.60947146357422,-1.60808829828351,-1.60676413741854,-1.60482975605356,
-1.60012961498056,-1.56251287398724,-1.51785616806351,-1.51257839467297,
-1.50978503745772,-1.50770366179424,-1.50509014099243,-1.50065055068393,
-1.48441328876514,-1.43003445574989,-1.41919269728428,-1.41260058492475,
-1.41045850217162,-1.40907710985822,-1.40775153269376,-1.40581027789016,
-1.40106938347263,-1.36444695536187,-1.33321373418801,-1.32253511182631,
-1.31486418271768,-1.31162137447143,-1.30925998138158,-1.30709004375631,
-1.3041511197482,-1.2979599651136),.UNSPECIFIED.);
#599=B_SPLINE_CURVE_WITH_KNOTS('',3,(#51718,#51719,#51720,#51721,#51722,
#51723,#51724,#51725,#51726,#51727,#51728,#51729,#51730,#51731,#51732,#51733,
#51734,#51735,#51736,#51737,#51738,#51739,#51740,#51741,#51742,#51743,#51744,
#51745,#51746,#51747,#51748,#51749,#51750,#51751,#51752,#51753,#51754,#51755,
#51756,#51757,#51758,#51759,#51760,#51761,#51762,#51763,#51764,#51765,#51766,
#51767,#51768,#51769,#51770,#51771,#51772,#51773,#51774,#51775,#51776,#51777,
#51778,#51779,#51780,#51781,#51782,#51783,#51784,#51785,#51786,#51787,#51788,
#51789,#51790,#51791,#51792,#51793,#51794,#51795,#51796,#51797,#51798,#51799,
#51800,#51801,#51802,#51803,#51804,#51805,#51806,#51807,#51808,#51809,#51810,
#51811,#51812,#51813,#51814,#51815,#51816,#51817,#51818,#51819,#51820,#51821,
#51822,#51823,#51824,#51825,#51826,#51827,#51828,#51829,#51830,#51831,#51832,
#51833,#51834,#51835,#51836,#51837,#51838,#51839,#51840,#51841,#51842,#51843,
#51844,#51845,#51846,#51847,#51848,#51849,#51850,#51851,#51852,#51853,#51854,
#51855,#51856,#51857,#51858,#51859,#51860,#51861,#51862,#51863,#51864,#51865,
#51866,#51867,#51868,#51869,#51870,#51871,#51872,#51873,#51874,#51875,#51876,
#51877,#51878,#51879,#51880,#51881,#51882,#51883,#51884,#51885,#51886,#51887,
#51888,#51889,#51890,#51891,#51892,#51893,#51894,#51895,#51896,#51897,#51898,
#51899,#51900,#51901,#51902,#51903,#51904,#51905,#51906,#51907,#51908,#51909,
#51910,#51911,#51912,#51913,#51914,#51915,#51916,#51917,#51918,#51919,#51920,
#51921),.UNSPECIFIED.,.F.,.F.,(4,2,2,2,2,2,2,2,2,2,2,2,2,2,2,2,2,2,2,2,
2,2,2,2,2,2,2,2,2,2,2,2,2,2,2,2,2,2,2,2,2,2,2,2,2,2,2,2,2,2,2,2,2,2,2,2,
2,2,2,2,2,2,2,2,2,2,2,2,2,2,2,2,2,2,2,2,2,2,2,2,2,2,2,2,2,2,2,2,2,2,2,2,
2,2,2,2,2,2,2,2,2,4),(-1.21650036072889,-1.20367186994537,-1.18282116663411,
-1.17970077907486,-1.17808664867918,-1.17679388214389,-1.17524582955073,
-1.17234360293463,-1.15451466079211,-1.12652620541326,-1.08722012356821,
-1.08248265487359,-1.0795206005624,-1.07720133689639,-1.07462247951083,
-1.0703422350816,-1.05387867748003,-0.99243291407614,-0.982742471554037,
-0.980211444729834,-0.978729065316574,-0.977558951089079,-0.97592432504103,
-0.972601684253843,-0.9682320273792,-0.957619681100799,-0.906781926283804,
-0.887158309976383,-0.882507253059537,-0.879819477496966,-0.877512917767558,
-0.874708755984211,-0.86938195344554,-0.862679662250612,-0.847523928323767,
-0.811106078629044,-0.784862251302172,-0.781669943467085,-0.780040265626657,
-0.778746569580856,-0.777211017242905,-0.774368191834507,-0.758063423902879,
-0.701603942797503,-0.687274339295151,-0.683022133879214,-0.680449360193734,
-0.678128657692247,-0.675155185270078,-0.668982492772153,-0.66090702588705,
-0.640955800900654,-0.613221779684546,-0.585848361861189,-0.582651647437803,
-0.581021134736983,-0.579727523258687,-0.578192952960173,-0.575354248457255,
-0.55914148528599,-0.503828590668287,-0.488469185439362,-0.484112206372492,
-0.481516555517238,-0.479432229843889,-0.476612490472009,-0.471208886787708,
-0.426874476351277,-0.389086557088364,-0.384388177306999,-0.382453870014954,
-0.381129550381289,-0.37974600356618,-0.377594538691698,-0.370925306233708,
-0.319405261909269,-0.290851926464014,-0.286216345164176,-0.283285068668805,
-0.280969286795655,-0.278372794614662,-0.274011947866813,-0.256530708865576,
-0.222340001321887,-0.190273831804208,-0.185441780683738,-0.183485268354989,
-0.182276786076821,-0.180953642407111,-0.179088867087865,-0.17689189933228,
-0.172907165168017,-0.163617848116005,-0.126922269847658,-0.0921073323921683,
-0.0873569083596852,-0.0843910316936627,-0.082071410488705,-0.0794948632014784,
-0.0752248005201745,-0.0588829643078642,-0.000583356136067976),
 .UNSPECIFIED.);
#600=B_SPLINE_CURVE_WITH_KNOTS('',3,(#51922,#51923,#51924,#51925,#51926,
#51927,#51928,#51929,#51930,#51931,#51932,#51933,#51934,#51935,#51936,#51937,
#51938,#51939,#51940,#51941,#51942,#51943),.UNSPECIFIED.,.F.,.F.,(4,2,2,
2,2,2,2,2,2,2,4),(-2.51402463792542,-2.50549522727735,-2.50071004123171,
-2.49896216044422,-2.49765999716403,-2.49642378936312,-2.49500799844318,
-2.49271099182215,-2.48550006123663,-2.47542634793241,-2.47330243401613),
 .UNSPECIFIED.);
#601=B_SPLINE_CURVE_WITH_KNOTS('',3,(#51944,#51945,#51946,#51947,#51948,
#51949,#51950,#51951,#51952,#51953,#51954,#51955,#51956,#51957,#51958,#51959,
#51960,#51961,#51962,#51963,#51964,#51965,#51966,#51967,#51968,#51969,#51970,
#51971,#51972,#51973,#51974,#51975,#51976,#51977,#51978,#51979,#51980,#51981,
#51982,#51983,#51984,#51985,#51986,#51987,#51988,#51989,#51990,#51991,#51992,
#51993,#51994,#51995,#51996,#51997,#51998,#51999,#52000,#52001,#52002,#52003,
#52004,#52005,#52006,#52007,#52008,#52009,#52010,#52011,#52012,#52013,#52014,
#52015,#52016,#52017,#52018,#52019,#52020,#52021,#52022,#52023,#52024,#52025,
#52026,#52027,#52028,#52029,#52030,#52031,#52032,#52033,#52034,#52035,#52036,
#52037,#52038,#52039,#52040,#52041,#52042,#52043,#52044,#52045,#52046,#52047,
#52048,#52049,#52050,#52051,#52052,#52053,#52054,#52055,#52056,#52057,#52058,
#52059,#52060,#52061,#52062,#52063,#52064,#52065,#52066,#52067,#52068,#52069,
#52070,#52071,#52072,#52073,#52074,#52075,#52076,#52077,#52078,#52079,#52080,
#52081,#52082,#52083,#52084,#52085,#52086,#52087,#52088,#52089,#52090,#52091,
#52092,#52093,#52094,#52095,#52096,#52097,#52098,#52099,#52100,#52101,#52102,
#52103,#52104,#52105,#52106,#52107,#52108,#52109,#52110,#52111,#52112,#52113,
#52114,#52115,#52116,#52117,#52118,#52119,#52120,#52121,#52122,#52123,#52124,
#52125,#52126,#52127,#52128,#52129,#52130,#52131,#52132,#52133,#52134,#52135,
#52136,#52137,#52138,#52139,#52140,#52141,#52142,#52143,#52144,#52145,#52146,
#52147,#52148,#52149,#52150,#52151,#52152,#52153,#52154,#52155,#52156,#52157),
 .UNSPECIFIED.,.F.,.F.,(4,2,2,2,2,2,2,2,2,2,2,2,2,2,2,2,2,2,2,2,2,2,2,2,
2,2,2,2,2,2,2,2,2,2,2,2,2,2,2,2,2,2,2,2,2,2,2,2,2,2,2,2,2,2,2,2,2,2,2,2,
2,2,2,2,2,2,2,2,2,2,2,2,2,2,2,2,2,2,2,2,2,2,2,2,2,2,2,2,2,2,2,2,2,2,2,2,
2,2,2,2,2,2,2,2,2,2,4),(-1.2979599651136,-1.29683172309349,-1.25693384069821,
-1.21777271999702,-1.21314919010135,-1.2114175514501,-1.21018610818971,
-1.20885807811842,-1.20697351826947,-1.20224462656028,-1.177707910862,-1.17094480686257,
-1.1227154856321,-1.11561286154691,-1.11278199147127,-1.11042371348871,
-1.10799791325747,-1.10442405447166,-1.09457601726633,-1.07968485494448,
-1.04817950923121,-1.03165926508212,-1.01618198226899,-1.01351288545697,
-1.01185539675462,-1.01056005896471,-1.00904627471541,-1.00630375452611,
-0.992140708472749,-0.956198918232946,-0.920941082911946,-0.91618815099358,
-0.913221600078467,-0.910902000352238,-0.90832604029203,-0.904058269750652,
-0.887742257023649,-0.85599919378957,-0.820052965067163,-0.815287322838515,
-0.813341917151239,-0.812015507705065,-0.810635215782818,-0.808498267819918,
-0.801948746498178,-0.79120639885158,-0.738391663700838,-0.720705173585745,
-0.716195765677733,-0.713540850855021,-0.711232766319075,-0.70838898213429,
-0.702867467485636,-0.659823902089313,-0.620866468667174,-0.616229215977293,
-0.614495756431457,-0.613263866081292,-0.611936295925047,-0.610053932615929,
-0.605338507600838,-0.580944205932299,-0.569982853823161,-0.526199998315964,
-0.518981285203984,-0.516053857762003,-0.513886780194649,-0.511523038667,
-0.508267051420153,-0.500517252130685,-0.489694002144564,-0.429173972315372,
-0.418618658252525,-0.416012841042599,-0.414513325419673,-0.41322821998872,
-0.411556214653473,-0.408042297653843,-0.376664048771488,-0.326446396702602,
-0.320220844124137,-0.316835043363872,-0.314470653002961,-0.312051961087735,
-0.308513451095731,-0.298920708482545,-0.284552365815458,-0.255289392249783,
-0.223082005537083,-0.218254892260719,-0.216299106064572,-0.215090683644324,
-0.213767393184338,-0.211838465352321,-0.209600408345692,-0.205508614267596,
-0.195858245778487,-0.175151099567017,-0.127853858338076,-0.120675676913724,
-0.117832690836522,-0.115471183934514,-0.113049075906374,-0.109493741974358,
-0.0997805979002047,-0.0851668180726992,-0.0414579409595978),
 .UNSPECIFIED.);
#602=B_SPLINE_CURVE_WITH_KNOTS('',3,(#52162,#52163,#52164,#52165,#52166,
#52167,#52168,#52169,#52170,#52171,#52172,#52173,#52174,#52175,#52176,#52177,
#52178,#52179,#52180,#52181,#52182,#52183,#52184,#52185,#52186,#52187,#52188,
#52189,#52190,#52191,#52192,#52193,#52194,#52195,#52196,#52197,#52198,#52199,
#52200,#52201,#52202,#52203,#52204,#52205,#52206,#52207,#52208,#52209,#52210,
#52211,#52212,#52213,#52214,#52215,#52216,#52217,#52218,#52219,#52220,#52221,
#52222,#52223,#52224,#52225,#52226,#52227,#52228,#52229,#52230,#52231,#52232,
#52233,#52234,#52235,#52236,#52237,#52238,#52239,#52240,#52241,#52242,#52243,
#52244,#52245,#52246,#52247,#52248,#52249,#52250,#52251,#52252,#52253,#52254,
#52255,#52256,#52257,#52258,#52259,#52260,#52261,#52262,#52263,#52264,#52265,
#52266,#52267,#52268,#52269,#52270,#52271,#52272,#52273,#52274,#52275,#52276,
#52277,#52278,#52279,#52280,#52281,#52282,#52283,#52284,#52285,#52286,#52287,
#52288,#52289,#52290,#52291,#52292,#52293,#52294,#52295,#52296,#52297,#52298,
#52299,#52300,#52301,#52302,#52303,#52304,#52305,#52306,#52307,#52308,#52309,
#52310,#52311,#52312,#52313,#52314,#52315,#52316,#52317,#52318,#52319,#52320,
#52321,#52322,#52323,#52324,#52325,#52326,#52327,#52328,#52329,#52330,#52331,
#52332,#52333,#52334,#52335,#52336,#52337,#52338,#52339,#52340,#52341,#52342,
#52343,#52344,#52345,#52346,#52347,#52348,#52349,#52350,#52351,#52352,#52353,
#52354,#52355,#52356,#52357,#52358,#52359,#52360,#52361,#52362,#52363,#52364,
#52365,#52366,#52367,#52368,#52369,#52370,#52371,#52372,#52373,#52374,#52375,
#52376,#52377),.UNSPECIFIED.,.F.,.F.,(4,2,2,2,2,2,2,2,2,2,2,2,2,2,2,2,2,
2,2,2,2,2,2,2,2,2,2,2,2,2,2,2,2,2,2,2,2,2,2,2,2,2,2,2,2,2,2,2,2,2,2,2,2,
2,2,2,2,2,2,2,2,2,2,2,2,2,2,2,2,2,2,2,2,2,2,2,2,2,2,2,2,2,2,2,2,2,2,2,2,
2,2,2,2,2,2,2,2,2,2,2,2,2,2,2,2,2,2,4),(-2.47274746625746,-2.471414553606,
-2.4691009156549,-2.46618274476928,-2.46158840004806,-2.43433135557283,
-2.41229008486747,-2.39217407961196,-2.37612000131115,-2.37327759320698,
-2.37174271505682,-2.37044985026478,-2.36882156090834,-2.36563297270697,
-2.33958927769404,-2.29182976432504,-2.28311859426973,-2.27661796832897,
-2.27359455315258,-2.27125990403053,-2.26874299723464,-2.26474075416736,
-2.2525895908786,-2.19365390955991,-2.17717296614671,-2.17432382067116,
-2.17278740135833,-2.17149448489933,-2.16986770744262,-2.16668670669114,
-2.14146194487422,-2.09509765707905,-2.08518190363019,-2.07793721140512,
-2.07476787307734,-2.07241965899032,-2.06993507353194,-2.06608200034155,
-2.05508728776842,-1.99476793322313,-1.97819590965774,-1.97534272824399,
-1.97380532529832,-1.9725122893131,-1.97088625647507,-1.96770932991216,
-1.93763787784834,-1.93316837088126,-1.89900600571225,-1.88153374191713,
-1.87717415023586,-1.87457820814676,-1.87226279214933,-1.8693318102059,
-1.86469631835272,-1.83613233668754,-1.7845960136792,-1.77792831817086,
-1.77577718045054,-1.77439381391977,-1.77306963358639,-1.77113548983019,
-1.76643725668463,-1.72861795153154,-1.68417771525276,-1.67888623353082,
-1.67608990196283,-1.67400811585188,-1.67139643961998,-1.66696578001415,
-1.65082510687123,-1.59633679487874,-1.58548801942921,-1.57889273009809,
-1.57675016942139,-1.57536860824337,-1.57404298812628,-1.57210185424649,
-1.56736217354812,-1.53064984976071,-1.49947755820319,-1.48881054279297,
-1.48114588825112,-1.47790399433372,-1.47554263746853,-1.47337229590405,
-1.47043215790565,-1.4631124173592,-1.42369519390846,-1.39351920021738,
-1.38510018450829,-1.37961519610419,-1.37761747722383,-1.3762670178633,
-1.37505865278752,-1.3731029323962,-1.36827583132125,-1.33550052528379,
-1.31531667455507,-1.2883766060435,-1.28172364296457,-1.27865966399012,
-1.27632708699658,-1.27379905200053,-1.26975002003021,-1.25722474018032,
-1.23573035801547,-1.21650036072889),.UNSPECIFIED.);
#603=B_SPLINE_CURVE_WITH_KNOTS('',3,(#52379,#52380,#52381,#52382,#52383,
#52384,#52385,#52386,#52387,#52388,#52389,#52390,#52391,#52392,#52393,#52394,
#52395,#52396,#52397,#52398,#52399,#52400),.UNSPECIFIED.,.F.,.F.,(4,2,2,
2,2,2,2,2,2,2,4),(-0.0414579409595978,-0.035082825383997,-0.0251484303517282,
-0.0195179196149325,-0.0174347627193792,-0.0162021523227704,-0.0149718856855802,
-0.0136622933178273,-0.011894101725279,-0.00763339607549248,-0.000737909110566063),
 .UNSPECIFIED.);
#604=B_SPLINE_CURVE_WITH_KNOTS('',3,(#52401,#52402,#52403,#52404,#52405,
#52406,#52407,#52408,#52409,#52410,#52411,#52412,#52413,#52414,#52415,#52416,
#52417,#52418,#52419,#52420,#52421,#52422,#52423,#52424,#52425,#52426,#52427,
#52428,#52429,#52430,#52431,#52432,#52433,#52434,#52435,#52436,#52437,#52438,
#52439,#52440,#52441,#52442,#52443,#52444,#52445,#52446,#52447,#52448,#52449,
#52450,#52451,#52452,#52453,#52454,#52455,#52456,#52457,#52458,#52459,#52460,
#52461,#52462,#52463,#52464,#52465,#52466,#52467,#52468,#52469,#52470,#52471,
#52472,#52473,#52474,#52475,#52476,#52477,#52478,#52479,#52480,#52481,#52482,
#52483,#52484,#52485,#52486,#52487,#52488,#52489,#52490,#52491,#52492,#52493,
#52494,#52495,#52496,#52497,#52498,#52499,#52500,#52501,#52502,#52503,#52504,
#52505,#52506,#52507,#52508,#52509,#52510,#52511,#52512,#52513,#52514,#52515,
#52516,#52517,#52518,#52519,#52520,#52521,#52522,#52523,#52524,#52525,#52526,
#52527,#52528,#52529,#52530,#52531,#52532,#52533,#52534,#52535,#52536,#52537,
#52538,#52539,#52540,#52541,#52542,#52543,#52544,#52545,#52546,#52547,#52548,
#52549,#52550,#52551,#52552,#52553,#52554,#52555,#52556,#52557,#52558,#52559,
#52560,#52561,#52562,#52563,#52564,#52565,#52566,#52567,#52568,#52569,#52570,
#52571,#52572,#52573,#52574,#52575,#52576,#52577,#52578,#52579,#52580,#52581,
#52582,#52583,#52584,#52585,#52586,#52587,#52588,#52589,#52590,#52591,#52592,
#52593,#52594,#52595,#52596,#52597,#52598,#52599,#52600,#52601,#52602,#52603,
#52604,#52605,#52606),.UNSPECIFIED.,.F.,.F.,(4,2,2,2,2,2,2,2,2,2,2,2,2,
2,2,2,2,2,2,2,2,2,2,2,2,2,2,2,2,2,2,2,2,2,2,2,2,2,2,2,2,2,2,2,2,2,2,2,2,
2,2,2,2,2,2,2,2,2,2,2,2,2,2,2,2,2,2,2,2,2,2,2,2,2,2,2,2,2,2,2,2,2,2,2,2,
2,2,2,2,2,2,2,2,2,2,2,2,2,2,2,2,2,4),(-4.94417392363714,-4.91309937476047,
-4.86968439704114,-4.86421139772586,-4.86137802808041,-4.85907119219392,
-4.85640970024793,-4.85186962012977,-4.83381261522179,-4.79315018454536,
-4.77433350418817,-4.76794881584999,-4.76488705623448,-4.76305437616443,
-4.76140466693561,-4.76014136217213,-4.7586591429474,-4.75612644877624,
-4.74640621522903,-4.68506455852927,-4.66861826655063,-4.66434111431908,
-4.66176384290726,-4.65944582765207,-4.65648512272851,-4.65174927183508,
-4.61252305738833,-4.58424604816674,-4.56661882160062,-4.56372513596879,
-4.56217940540007,-4.56088727226615,-4.55927230071572,-4.55614562071163,
-4.53444460522209,-4.50393169553112,-4.48204132577849,-4.46911966755911,
-4.46517352707056,-4.46266888840275,-4.46032967164745,-4.45726839648233,
-4.45044209682022,-4.39946217048655,-4.37757928544131,-4.3705716713677,
-4.36579031290003,-4.36389796509929,-4.3625689053494,-4.36134006837862,
-4.35961693724228,-4.35505381427277,-4.31459501537612,-4.2728386550215,
-4.26743289722181,-4.26461349687611,-4.26253001990676,-4.25993620408022,
-4.25558416503592,-4.24026614476112,-4.18491133340216,-4.1686961834239,
-4.16585819813638,-4.16432417700165,-4.16303111903489,-4.16140142748592,
-4.15820668555396,-4.13035592368184,-4.09706635616234,-4.08103120601792,
-4.07406433375861,-4.06857143507874,-4.06573388044859,-4.06342665600911,
-4.06076807240829,-4.05624112352644,-4.03831269015808,-3.99057379301517,
-3.97663377193337,-3.97137788468322,-3.96754129516396,-3.96580906450669,
-3.96450596841191,-3.96303942038778,-3.96051197589568,-3.95116727443693,
-3.88941325803181,-3.87293312617115,-3.86865290733104,-3.86607480205627,
-3.86375668091635,-3.86079672924062,-3.85606388556261,-3.81659782472707,
-3.78781351117836,-3.7708729000657,-3.7680053230561,-3.76646504626298,-3.76517247769287,
-3.76355066910472,-3.76039257516026,-3.73692200761545,-3.72889146245253),
 .UNSPECIFIED.);
#605=B_SPLINE_CURVE_WITH_KNOTS('',3,(#52612,#52613,#52614,#52615,#52616,
#52617,#52618,#52619,#52620,#52621,#52622,#52623,#52624,#52625,#52626,#52627,
#52628,#52629,#52630,#52631,#52632,#52633,#52634,#52635,#52636,#52637,#52638,
#52639,#52640,#52641,#52642,#52643,#52644,#52645,#52646,#52647,#52648,#52649,
#52650,#52651,#52652,#52653,#52654,#52655,#52656,#52657,#52658,#52659,#52660,
#52661,#52662,#52663,#52664,#52665,#52666,#52667,#52668,#52669,#52670,#52671,
#52672,#52673,#52674,#52675,#52676,#52677,#52678,#52679,#52680,#52681,#52682,
#52683,#52684,#52685,#52686,#52687,#52688,#52689,#52690,#52691,#52692,#52693,
#52694,#52695,#52696,#52697,#52698,#52699,#52700,#52701,#52702,#52703,#52704,
#52705,#52706,#52707,#52708,#52709,#52710,#52711,#52712,#52713,#52714,#52715,
#52716,#52717,#52718,#52719,#52720,#52721,#52722,#52723,#52724,#52725,#52726,
#52727,#52728,#52729,#52730,#52731,#52732,#52733,#52734,#52735,#52736,#52737,
#52738,#52739,#52740,#52741,#52742,#52743,#52744,#52745,#52746,#52747,#52748,
#52749,#52750,#52751,#52752,#52753,#52754,#52755,#52756,#52757,#52758,#52759,
#52760,#52761,#52762,#52763,#52764,#52765,#52766,#52767,#52768,#52769,#52770,
#52771,#52772,#52773,#52774,#52775,#52776,#52777,#52778,#52779,#52780,#52781,
#52782,#52783,#52784,#52785,#52786,#52787,#52788,#52789,#52790,#52791,#52792,
#52793,#52794,#52795,#52796,#52797,#52798,#52799,#52800,#52801,#52802,#52803,
#52804,#52805,#52806,#52807,#52808,#52809,#52810,#52811,#52812,#52813,#52814,
#52815,#52816,#52817,#52818,#52819,#52820,#52821,#52822,#52823),
 .UNSPECIFIED.,.F.,.F.,(4,2,2,2,2,2,2,2,2,2,2,2,2,2,2,2,2,2,2,2,2,2,2,2,
2,2,2,2,2,2,2,2,2,2,2,2,2,2,2,2,2,2,2,2,2,2,2,2,2,2,2,2,2,2,2,2,2,2,2,2,
2,2,2,2,2,2,2,2,2,2,2,2,2,2,2,2,2,2,2,2,2,2,2,2,2,2,2,2,2,2,2,2,2,2,2,2,
2,2,2,2,2,2,2,2,2,4),(-1.21629508419202,-1.19678839020098,-1.16104491785065,
-1.15628570130955,-1.15331657066828,-1.15099577848306,-1.14841933863923,
-1.14415274393049,-1.12786642522531,-1.09623267748193,-1.06010503978159,
-1.05534344462364,-1.05339816777709,-1.0520713401155,-1.05069017862987,
-1.04855099304072,-1.04198762072658,-1.03121523453434,-0.977972166463608,
-0.96066908255111,-0.956187881121162,-0.953538795504893,-0.951229165488729,
-0.948374972133484,-0.942805766748834,-0.904684326654697,-0.861756292261737,
-0.856453418023476,-0.854419258705664,-0.85319596308645,-0.851860389793916,
-0.849937951754468,-0.844968078723773,-0.837593936543774,-0.813768795062902,
-0.765769968466468,-0.758644059750312,-0.755808917826503,-0.75344900265554,
-0.751023487926242,-0.747453738513993,-0.73764084906406,-0.722823887910961,
-0.691827481436309,-0.674143142336256,-0.659114303260826,-0.656473920147491,
-0.654824785869057,-0.653529694837953,-0.652008874976559,-0.649235250193616,
-0.634465333703563,-0.592212401814593,-0.563669993955392,-0.559033585760423,
-0.556101591969151,-0.553785121086686,-0.551187727972645,-0.546825058547546,
-0.52933203433922,-0.495107882335919,-0.463078324795227,-0.458234173098523,
-0.456275288138125,-0.455066111876199,-0.45371586914444,-0.451720418063046,
-0.446253730874893,-0.437874421452672,-0.40796825578915,-0.368245711051937,
-0.360927040955379,-0.357982029059069,-0.355810079437357,-0.353448892914874,
-0.350210729175154,-0.342571513127716,-0.331950278381618,-0.301017417565392,
-0.263904490107245,-0.25917058714467,-0.257230063246971,-0.255904279963507,
-0.254521966778183,-0.252377242892097,-0.246048019081636,-0.235678356871826,
-0.188090172556569,-0.165225680098754,-0.160793078874204,-0.157923110737925,
-0.155612349271606,-0.153439380975918,-0.149679596395542,-0.137398977606132,
-0.11699930020956,-0.0983284252223009,-0.0772706239788904,-0.0620776668811129,
-0.0594294807345166,-0.0577780454785035,-0.0564828586952099,-0.054963922106604,
-0.0521987249030516,-0.0487365117228446,-0.00058344341590058),
 .UNSPECIFIED.);
#606=B_SPLINE_CURVE_WITH_KNOTS('',3,(#52824,#52825,#52826,#52827,#52828,
#52829,#52830,#52831,#52832,#52833),.UNSPECIFIED.,.F.,.F.,(4,2,2,2,4),(-2.51371913210301,
-2.47983225959379,-2.47613607850828,-2.4735811998181,-2.47274746625746),
 .UNSPECIFIED.);
#607=B_SPLINE_CURVE_WITH_KNOTS('',3,(#52834,#52835,#52836,#52837,#52838,
#52839,#52840,#52841,#52842,#52843,#52844,#52845,#52846,#52847,#52848,#52849,
#52850,#52851,#52852,#52853,#52854,#52855,#52856,#52857,#52858,#52859,#52860,
#52861,#52862,#52863,#52864,#52865,#52866,#52867,#52868,#52869,#52870,#52871,
#52872,#52873,#52874,#52875,#52876,#52877,#52878,#52879,#52880,#52881,#52882,
#52883,#52884,#52885,#52886,#52887,#52888,#52889,#52890,#52891,#52892,#52893,
#52894,#52895,#52896,#52897,#52898,#52899,#52900,#52901,#52902,#52903,#52904,
#52905,#52906,#52907,#52908,#52909,#52910,#52911,#52912,#52913,#52914,#52915,
#52916,#52917,#52918,#52919,#52920,#52921,#52922,#52923,#52924,#52925,#52926,
#52927,#52928,#52929,#52930,#52931,#52932,#52933,#52934,#52935,#52936,#52937,
#52938,#52939,#52940,#52941,#52942,#52943,#52944,#52945,#52946,#52947,#52948,
#52949,#52950,#52951,#52952,#52953,#52954,#52955,#52956,#52957,#52958,#52959,
#52960,#52961,#52962,#52963,#52964,#52965,#52966,#52967,#52968,#52969,#52970,
#52971,#52972,#52973,#52974,#52975,#52976,#52977,#52978,#52979,#52980,#52981,
#52982,#52983,#52984,#52985,#52986,#52987,#52988,#52989,#52990,#52991,#52992,
#52993,#52994,#52995,#52996,#52997,#52998,#52999,#53000,#53001,#53002,#53003,
#53004,#53005,#53006,#53007,#53008,#53009,#53010,#53011,#53012,#53013,#53014,
#53015,#53016,#53017,#53018,#53019,#53020,#53021,#53022,#53023,#53024,#53025,
#53026,#53027,#53028,#53029,#53030,#53031,#53032,#53033,#53034,#53035,#53036,
#53037,#53038,#53039,#53040,#53041,#53042,#53043,#53044,#53045,#53046,#53047,
#53048,#53049),.UNSPECIFIED.,.F.,.F.,(4,2,2,2,2,2,2,2,2,2,2,2,2,2,2,2,2,
2,2,2,2,2,2,2,2,2,2,2,2,2,2,2,2,2,2,2,2,2,2,2,2,2,2,2,2,2,2,2,2,2,2,2,2,
2,2,2,2,2,2,2,2,2,2,2,2,2,2,2,2,2,2,2,2,2,2,2,2,2,2,2,2,2,2,2,2,2,2,2,2,
2,2,2,2,2,2,2,2,2,2,2,2,2,2,2,2,2,2,4),(-3.72889146245253,-3.70814737956327,
-3.67850138071064,-3.6715193570599,-3.66839644412708,-3.66605578815816,
-3.66355399236289,-3.6596215820007,-3.648026213805,-3.59456838646231,-3.57418488333566,
-3.56986991519399,-3.56805350092186,-3.56673783224545,-3.56548844789078,
-3.56331816032759,-3.55707816967706,-3.51509719579875,-3.47674241207794,
-3.47154701262265,-3.46877116179606,-3.46648852465219,-3.46378738866586,
-3.45907390511088,-3.43852733930262,-3.38863019253642,-3.37808559430011,
-3.37373601979671,-3.37042592299356,-3.36879427702333,-3.36762499636274,
-3.36614188270185,-3.36360576439069,-3.35384974949012,-3.29253812922952,
-3.27609291442109,-3.27181551147186,-3.26923799499472,-3.26691969959496,
-3.26395855442644,-3.25922183203965,-3.21998596548248,-3.19219438895693,
-3.17411045379676,-3.17119990338276,-3.16965049307307,-3.16835837464804,
-3.16674728923823,-3.16423037400043,-3.15154337062974,-3.14325158106825,
-3.1288173075177,-3.09480300866722,-3.07737428864688,-3.07301858821809,
-3.07042380086867,-3.06810869042,-3.06517711349699,-3.0605387265637,-3.03185332947279,
-2.98974000692742,-2.97499389114168,-2.97222264186156,-2.97070291720249,
-2.96940861376678,-2.96776031224662,-2.96512097607141,-2.95008743550299,
-2.93245114892786,-2.90150021336824,-2.88669189827361,-2.88009682737053,
-2.87483807038743,-2.8720488845178,-2.86976565030023,-2.86707593473933,
-2.86241297354053,-2.84259391659081,-2.79195382484259,-2.7813557142552,
-2.77487012829037,-2.77274118511584,-2.77136280098706,-2.7700354057418,
-2.76808419274215,-2.76328250359025,-2.72885535548839,-2.69644499336853,
-2.68524758058578,-2.67729326456345,-2.67400386593341,-2.67163432594743,
-2.66947454417706,-2.66602785580541,-2.6595723626451,-2.6121355126774,-2.57810149475438,
-2.57474320419319,-2.57310186053851,-2.57180781952792,-2.57028230126718,
-2.56756159203472,-2.55545353712949,-2.51816897716757,-2.48693956435907,
-2.4785150864885,-2.47515044650355,-2.47285424115159),.UNSPECIFIED.);
#608=B_SPLINE_CURVE_WITH_KNOTS('',3,(#53054,#53055,#53056,#53057,#53058,
#53059,#53060,#53061,#53062,#53063,#53064,#53065,#53066,#53067,#53068,#53069,
#53070,#53071,#53072,#53073,#53074,#53075,#53076,#53077,#53078,#53079,#53080,
#53081,#53082,#53083,#53084,#53085,#53086,#53087,#53088,#53089,#53090,#53091,
#53092,#53093,#53094,#53095,#53096,#53097,#53098,#53099,#53100,#53101,#53102,
#53103,#53104,#53105,#53106,#53107,#53108,#53109,#53110,#53111,#53112,#53113,
#53114,#53115,#53116,#53117,#53118,#53119,#53120,#53121,#53122,#53123,#53124,
#53125,#53126,#53127,#53128,#53129,#53130,#53131,#53132,#53133,#53134,#53135,
#53136,#53137,#53138,#53139,#53140,#53141,#53142,#53143,#53144,#53145,#53146,
#53147,#53148,#53149,#53150,#53151,#53152,#53153,#53154,#53155,#53156,#53157,
#53158,#53159,#53160,#53161,#53162,#53163,#53164,#53165,#53166,#53167,#53168,
#53169,#53170,#53171,#53172,#53173,#53174,#53175,#53176,#53177,#53178,#53179,
#53180,#53181,#53182,#53183,#53184,#53185,#53186,#53187,#53188,#53189,#53190,
#53191,#53192,#53193,#53194,#53195,#53196,#53197,#53198,#53199,#53200,#53201,
#53202,#53203,#53204,#53205,#53206,#53207,#53208,#53209,#53210,#53211,#53212,
#53213,#53214,#53215,#53216,#53217,#53218,#53219,#53220,#53221,#53222,#53223,
#53224,#53225,#53226,#53227,#53228,#53229,#53230,#53231,#53232,#53233,#53234,
#53235,#53236,#53237,#53238,#53239,#53240,#53241,#53242,#53243,#53244,#53245,
#53246,#53247,#53248,#53249,#53250,#53251,#53252,#53253,#53254,#53255,#53256,
#53257,#53258,#53259,#53260,#53261,#53262,#53263,#53264,#53265,#53266,#53267,
#53268,#53269,#53270,#53271,#53272,#53273,#53274,#53275,#53276,#53277,#53278,
#53279,#53280,#53281,#53282,#53283,#53284,#53285,#53286,#53287,#53288,#53289,
#53290,#53291,#53292,#53293,#53294,#53295,#53296,#53297,#53298,#53299,#53300,
#53301,#53302,#53303,#53304,#53305),.UNSPECIFIED.,.F.,.F.,(4,2,2,2,2,2,
2,2,2,2,2,2,2,2,2,2,2,2,2,2,2,2,2,2,2,2,2,2,2,2,2,2,2,2,2,2,2,2,2,2,2,2,
2,2,2,2,2,2,2,2,2,2,2,2,2,2,2,2,2,2,2,2,2,2,2,2,2,2,2,2,2,2,2,2,2,2,2,2,
2,2,2,2,2,2,2,2,2,2,2,2,2,2,2,2,2,2,2,2,2,2,2,2,2,2,2,2,2,2,2,2,2,2,2,2,
2,2,2,2,2,2,2,2,2,2,2,4),(-2.47288460460841,-2.46217668520358,-2.45385741648579,
-2.44842797008862,-2.44644735082339,-2.44510673058267,-2.44389844342252,
-2.44194264161838,-2.43711557726936,-2.40584105658942,-2.37909361016463,
-2.36259189401898,-2.35548163686839,-2.34995499696683,-2.34711409768511,
-2.34707612557772,-2.34703676848092,-2.34699593631053,-2.34695353125495,
-2.34690944682533,-2.34686356696828,-2.34681576497736,-2.34676590221363,
-2.34671382678595,-2.34668493887874,-2.34664924377911,-2.34660498019936,
-2.34654984827375,-2.34648080002835,-2.34639372332381,-2.34407313383829,
-2.34113701045427,-2.33649584305399,-2.30851326433016,-2.25667588832234,
-2.25002761095081,-2.24787382212599,-2.24648639122181,-2.24515909700479,
-2.24321700903982,-2.23847996446942,-2.20156569123459,-2.17057301912225,
-2.15994183953601,-2.15229669829309,-2.14905718721466,-2.14669541064296,
-2.14452318098929,-2.14157818494998,-2.13426162132827,-2.09452750657146,
-2.06455304929185,-2.05616275930657,-2.05069146109291,-2.04869575205888,
-2.04734580481157,-2.0461379936048,-2.04418213507868,-2.03934922351807,
-2.00848058426198,-1.98246078709795,-1.95879954636734,-1.95257820089051,
-1.94959690266899,-1.94727697053376,-1.94471207503551,-1.94048923367701,
-1.92641218740427,-1.86960509081213,-1.8532692903952,-1.85042685223263,
-1.84889223881666,-1.84759901138635,-1.84596987209372,-1.84278053276337,
-1.81689711895634,-1.76942955283411,-1.75587601875855,-1.75186136709879,
-1.74934014183666,-1.74700385540109,-1.74397262251822,-1.73732256888089,
-1.68484089034511,-1.68174005283103,-1.65710191660181,-1.65236252691992,
-1.65047546692496,-1.64914630902854,-1.64791466889562,-1.6461833084425,
-1.64156475153857,-1.60233722297374,-1.55952867962303,-1.55402525946383,
-1.55118463893462,-1.54887608804044,-1.54621727100728,-1.54169307227898,
-1.52382460898796,-1.47113653147148,-1.46039630121876,-1.45384771448924,
-1.45171051214816,-1.45032992927386,-1.4490031886144,-1.44705716119622,
-1.44228925704491,-1.40640458344367,-1.37462873679908,-1.3638434844486,
-1.35611341149774,-1.35286025042937,-1.35049659613107,-1.34832823557855,
-1.34483722250932,-1.33623989256087,-1.28593147523885,-1.25709695277123,
-1.25365003001172,-1.25199090293672,-1.25069502957743,-1.24918144133462,
-1.2464416207899,-1.23234706953041,-1.21629508419202),.UNSPECIFIED.);
#609=B_SPLINE_CURVE_WITH_KNOTS('',3,(#53306,#53307,#53308,#53309,#53310,
#53311,#53312,#53313,#53314,#53315,#53316,#53317,#53318,#53319,#53320,#53321,
#53322,#53323,#53324,#53325,#53326,#53327,#53328,#53329,#53330,#53331,#53332,
#53333,#53334,#53335,#53336,#53337,#53338,#53339,#53340,#53341,#53342,#53343,
#53344,#53345,#53346,#53347,#53348,#53349,#53350,#53351,#53352,#53353,#53354,
#53355,#53356,#53357,#53358,#53359,#53360,#53361,#53362,#53363,#53364,#53365,
#53366,#53367,#53368,#53369,#53370,#53371,#53372,#53373,#53374,#53375,#53376,
#53377,#53378,#53379,#53380,#53381,#53382,#53383,#53384,#53385,#53386,#53387,
#53388,#53389,#53390,#53391,#53392,#53393,#53394,#53395,#53396,#53397,#53398,
#53399,#53400,#53401,#53402,#53403,#53404,#53405,#53406,#53407,#53408,#53409,
#53410,#53411,#53412,#53413,#53414,#53415,#53416,#53417,#53418,#53419,#53420,
#53421,#53422,#53423,#53424,#53425,#53426,#53427,#53428,#53429,#53430,#53431,
#53432,#53433,#53434,#53435,#53436,#53437,#53438,#53439,#53440,#53441,#53442,
#53443,#53444,#53445,#53446,#53447,#53448,#53449,#53450,#53451,#53452,#53453,
#53454,#53455,#53456,#53457,#53458,#53459,#53460,#53461,#53462,#53463,#53464,
#53465,#53466,#53467,#53468,#53469,#53470,#53471,#53472,#53473,#53474,#53475,
#53476,#53477,#53478,#53479,#53480,#53481,#53482,#53483,#53484,#53485,#53486,
#53487,#53488,#53489,#53490,#53491,#53492,#53493,#53494,#53495,#53496,#53497,
#53498,#53499,#53500,#53501,#53502,#53503,#53504,#53505,#53506,#53507,#53508,
#53509,#53510,#53511,#53512,#53513,#53514,#53515),.UNSPECIFIED.,.F.,.F.,
(4,2,2,2,2,2,2,2,2,2,2,2,2,2,2,2,2,2,2,2,2,2,2,2,2,2,2,2,2,2,2,2,2,2,2,
2,2,2,2,2,2,2,2,2,2,2,2,2,2,2,2,2,2,2,2,2,2,2,2,2,2,2,2,2,2,2,2,2,2,2,2,
2,2,2,2,2,2,2,2,2,2,2,2,2,2,2,2,2,2,2,2,2,2,2,2,2,2,2,2,2,2,2,2,2,4),(-2.47285424115159,
-2.47276667947185,-2.47033894217288,-2.46675482693037,-2.45683029588147,
-2.44178044602466,-2.40684632584979,-2.37898262027467,-2.37578675672441,
-2.37415662269162,-2.37286329111761,-2.37132903311689,-2.36849081884094,
-2.35227832689895,-2.29693818648215,-2.28161785796799,-2.27726499472531,
-2.27467061613181,-2.2725866502792,-2.26976653019207,-2.2643592274727,-2.25752846390797,
-2.24194665569387,-2.20350418876136,-2.17995793241073,-2.17679795186298,
-2.17517556984587,-2.17388275549834,-2.17234243148313,-2.1694754358018,
-2.15255718248808,-2.12377036895969,-2.08430526037572,-2.07957252906431,
-2.07661229050696,-2.07429374131368,-2.07171495030411,-2.06743310510509,
-2.05094095163634,-1.98909488659044,-1.97979259054865,-1.97726874465643,
-1.97580274176805,-1.9744989898905,-1.97276440617903,-1.96891683109184,
-1.94091340271781,-1.89126325847109,-1.88208288643013,-1.87849833832595,
-1.87631303482458,-1.87396273849936,-1.87078471944681,-1.86349400104512,
-1.85349661124895,-1.80717375464674,-1.78198557872692,-1.7788037541961,
-1.77717648193925,-1.77588320504334,-1.7743464246059,-1.77149650921252,
-1.75500620911808,-1.69592313324971,-1.68389686184406,-1.67990947750519,
-1.67739542005782,-1.67505895586755,-1.67196503480076,-1.66514559041506,
-1.63685336161741,-1.59902673518337,-1.58261252315578,-1.5799077788609,
-1.57823975519537,-1.57694370123558,-1.57543773093574,-1.57273073884975,
-1.5592303819701,-1.52665110341384,-1.48726192284892,-1.48252798105792,
-1.47956720277366,-1.47724836684289,-1.47466939688573,-1.47038758219181,
-1.45389970584968,-1.39211166860824,-1.3827544126248,-1.38022496419106,
-1.37875753431934,-1.37745344989107,-1.37571989915154,-1.37188101517732,
-1.36662266732064,-1.35267808394763,-1.30495527656979,-1.28706433057526,
-1.28253825140109,-1.27987872429951,-1.27756978354487,-1.27472896091304,
-1.26922600650835,-1.22641655877088,-1.21637204632693),.UNSPECIFIED.);
#610=B_SPLINE_CURVE_WITH_KNOTS('',3,(#53519,#53520,#53521,#53522,#53523,
#53524),.UNSPECIFIED.,.F.,.F.,(4,1,1,4),(-4.09157007060747,-3.98048681065136,
-2.98536510798852,-2.06680503374274),.UNSPECIFIED.);
#611=B_SPLINE_CURVE_WITH_KNOTS('',3,(#53528,#53529,#53530,#53531,#53532),
 .UNSPECIFIED.,.F.,.F.,(4,1,4),(0.,0.995121702662836,1.11662023360664),
 .UNSPECIFIED.);
#612=B_SPLINE_CURVE_WITH_KNOTS('',3,(#53534,#53535,#53536,#53537,#53538,
#53539,#53540,#53541,#53542,#53543,#53544,#53545,#53546,#53547,#53548,#53549,
#53550,#53551,#53552,#53553,#53554,#53555,#53556,#53557,#53558,#53559,#53560,
#53561,#53562,#53563,#53564,#53565,#53566,#53567,#53568,#53569,#53570,#53571,
#53572,#53573,#53574,#53575,#53576,#53577,#53578,#53579,#53580,#53581,#53582,
#53583,#53584,#53585,#53586,#53587,#53588,#53589,#53590,#53591,#53592,#53593,
#53594,#53595,#53596,#53597,#53598,#53599,#53600,#53601,#53602,#53603,#53604,
#53605,#53606,#53607,#53608,#53609,#53610,#53611,#53612,#53613,#53614,#53615,
#53616,#53617,#53618,#53619,#53620,#53621,#53622,#53623,#53624,#53625,#53626,
#53627,#53628,#53629,#53630,#53631,#53632,#53633,#53634,#53635,#53636,#53637,
#53638,#53639,#53640,#53641,#53642,#53643,#53644,#53645,#53646,#53647,#53648,
#53649,#53650,#53651,#53652,#53653,#53654,#53655,#53656,#53657,#53658,#53659,
#53660,#53661,#53662,#53663,#53664,#53665,#53666,#53667,#53668,#53669,#53670,
#53671,#53672,#53673,#53674,#53675,#53676,#53677,#53678,#53679,#53680,#53681,
#53682,#53683,#53684,#53685,#53686,#53687,#53688,#53689,#53690,#53691,#53692,
#53693,#53694,#53695,#53696,#53697,#53698,#53699,#53700,#53701,#53702,#53703,
#53704,#53705,#53706,#53707,#53708,#53709,#53710,#53711,#53712,#53713,#53714,
#53715,#53716,#53717,#53718,#53719,#53720,#53721,#53722,#53723),
 .UNSPECIFIED.,.F.,.F.,(4,3,3,3,3,3,3,3,3,3,3,3,3,3,3,3,3,3,3,3,3,3,3,3,
3,3,3,3,3,3,3,3,3,3,3,3,3,3,3,3,3,3,3,3,3,3,3,3,3,3,3,3,3,3,3,3,3,3,3,3,
3,3,3,4),(1.11662023360664,1.21406248760952,1.31136251306232,1.40858355403428,
1.50575826510081,1.60291922999088,1.70016613702826,1.79745265447162,1.8949147603219,
1.99024340532568,2.0900809264776,2.18977589743065,2.28935514905995,2.38887084056714,
2.4883532496785,2.58783261362238,2.68740727963367,2.78702701630181,2.88682420965512,
2.98536510798852,3.08525785857347,3.18501169700715,3.28465506891586,3.3842380426777,
3.48379080751166,3.58334351505092,3.68299577388001,3.78269553538725,3.88257601633546,
3.98048681065136,4.08009956575734,4.17956843680165,4.27907344636572,4.37836158923314,
4.47761636387469,4.57686832789242,4.67655337424787,4.77594858235294,4.87577854783357,
4.9756085133142,5.07535894551674,5.17496719232404,5.27446071472182,5.37389132531015,
5.47328942836856,5.57268538835164,5.67219659525799,5.77173596693952,5.87145546527129,
5.97073021597704,6.07047695669942,6.17008183754323,6.26957250648138,6.36900057641264,
6.46839645591088,6.56779051402169,6.66730586517624,6.76684415007728,6.86656306647563,
6.96585191863989,7.0743403241005,7.18223019824974,7.29101786936603,7.39980554048232),
 .UNSPECIFIED.);
#613=B_SPLINE_CURVE_WITH_KNOTS('',3,(#53725,#53726,#53727,#53728,#53729,
#53730,#53731,#53732,#53733,#53734,#53735,#53736,#53737,#53738,#53739,#53740,
#53741,#53742,#53743,#53744,#53745,#53746,#53747,#53748,#53749,#53750,#53751,
#53752,#53753,#53754,#53755,#53756,#53757,#53758,#53759,#53760,#53761,#53762,
#53763,#53764,#53765,#53766,#53767,#53768,#53769,#53770,#53771,#53772,#53773,
#53774,#53775,#53776,#53777,#53778,#53779,#53780,#53781,#53782,#53783,#53784,
#53785,#53786,#53787,#53788,#53789,#53790,#53791,#53792,#53793,#53794,#53795,
#53796,#53797,#53798,#53799,#53800,#53801,#53802,#53803,#53804,#53805,#53806,
#53807,#53808,#53809,#53810,#53811,#53812,#53813,#53814,#53815,#53816,#53817,
#53818,#53819,#53820,#53821,#53822,#53823,#53824,#53825,#53826,#53827,#53828,
#53829,#53830,#53831,#53832,#53833,#53834,#53835,#53836,#53837,#53838,#53839,
#53840,#53841,#53842,#53843,#53844,#53845,#53846,#53847,#53848,#53849,#53850,
#53851,#53852,#53853,#53854,#53855,#53856,#53857,#53858,#53859,#53860,#53861,
#53862,#53863,#53864,#53865,#53866,#53867,#53868,#53869,#53870,#53871,#53872,
#53873,#53874,#53875,#53876,#53877,#53878,#53879,#53880,#53881,#53882,#53883,
#53884,#53885,#53886,#53887,#53888,#53889,#53890,#53891,#53892,#53893,#53894,
#53895,#53896,#53897,#53898,#53899,#53900,#53901,#53902,#53903,#53904,#53905,
#53906,#53907,#53908,#53909,#53910,#53911,#53912,#53913,#53914,#53915,#53916,
#53917),.UNSPECIFIED.,.F.,.F.,(4,3,3,3,3,3,3,3,3,3,3,3,3,3,3,3,3,3,3,3,
3,3,3,3,3,3,3,3,3,3,3,3,3,3,3,3,3,3,3,3,3,3,3,3,3,3,3,3,3,3,3,3,3,3,3,3,
3,3,3,3,3,3,3,3,4),(7.39980554078624,7.50151138056856,7.60328677665983,
7.7052395287897,7.80729009445515,7.90955145809102,7.96097362130273,8.06070626983946,
8.16029669361446,8.25977242032754,8.35918526010481,8.45856564232094,8.5579439565598,
8.65748179841125,8.75700390142675,8.85670650664603,8.95609532396558,9.05582580586708,
9.15541407968061,9.25488944804909,9.3543001957416,9.4536785121954,9.55305479000452,
9.6525953491605,9.75211550952065,9.85181624478125,9.95121702662841,10.0509435670901,
10.1505278213335,10.2500041848282,10.3494107525505,10.4487848377975,10.548156838838,
10.6477023114513,10.7472181266395,10.8469145096764,10.9463387292913,11.0460680233656,
11.145655070275,11.2451307404849,11.3445401750104,11.4439171485967,11.5432920555783,
11.6428341496723,11.7423528843177,11.842052171866,11.9414604319541,12.0411892223499,
12.1407757642195,12.2402515605191,12.3396604905676,12.4390369610488,12.5384113670061,
12.6379540589088,12.7374723028274,12.8371711097881,12.936582134617,13.035137737167,
13.1335648679788,13.2318955025576,13.3301614969694,13.4284230365986,13.5266798090921,
13.6250124709493,13.6829908479658),.UNSPECIFIED.);
#614=B_SPLINE_CURVE_WITH_KNOTS('',3,(#53919,#53920,#53921,#53922,#53923,
#53924,#53925,#53926,#53927,#53928,#53929,#53930,#53931,#53932,#53933,#53934,
#53935,#53936,#53937,#53938,#53939,#53940,#53941,#53942,#53943,#53944,#53945,
#53946,#53947,#53948,#53949,#53950,#53951,#53952,#53953,#53954,#53955,#53956,
#53957,#53958,#53959,#53960,#53961,#53962,#53963,#53964,#53965,#53966,#53967,
#53968,#53969,#53970,#53971,#53972,#53973,#53974,#53975,#53976,#53977,#53978,
#53979,#53980,#53981,#53982,#53983,#53984,#53985,#53986,#53987,#53988,#53989,
#53990,#53991,#53992,#53993,#53994,#53995,#53996,#53997,#53998,#53999,#54000,
#54001,#54002,#54003,#54004,#54005,#54006,#54007,#54008,#54009,#54010,#54011,
#54012,#54013,#54014,#54015,#54016,#54017,#54018,#54019,#54020,#54021,#54022,
#54023,#54024,#54025,#54026,#54027,#54028,#54029,#54030,#54031,#54032,#54033,
#54034,#54035,#54036,#54037,#54038,#54039,#54040,#54041,#54042,#54043,#54044,
#54045,#54046,#54047,#54048,#54049,#54050,#54051,#54052,#54053,#54054,#54055,
#54056,#54057,#54058,#54059,#54060,#54061,#54062,#54063,#54064,#54065,#54066,
#54067,#54068,#54069,#54070,#54071,#54072,#54073,#54074,#54075,#54076,#54077,
#54078,#54079,#54080,#54081,#54082,#54083,#54084,#54085,#54086,#54087,#54088,
#54089,#54090,#54091,#54092,#54093,#54094,#54095,#54096,#54097,#54098,#54099,
#54100,#54101,#54102,#54103,#54104,#54105,#54106,#54107,#54108),
 .UNSPECIFIED.,.F.,.F.,(4,3,3,3,3,3,3,3,3,3,3,3,3,3,3,3,3,3,3,3,3,3,3,3,
3,3,3,3,3,3,3,3,3,3,3,3,3,3,3,3,3,3,3,3,3,3,3,3,3,3,3,3,3,3,3,3,3,3,3,3,
3,3,3,4),(13.6829908483353,13.8119049794007,13.9317038372798,14.031432564536,
14.1310190394365,14.2304948519997,14.3299037062129,14.4292800976703,14.5286544215113,
14.6281972011191,14.7277153561338,14.8274140707772,14.9268255399426,15.0265541732415,
15.1261405535332,15.2256163896673,15.3250251484058,15.4244014442795,15.5237756725604,
15.6233185650717,15.7228366255694,15.8225352470782,15.9219472426055,16.0216758307429,
16.1212621647812,16.2207380123421,16.320146722509,16.4195229690432,16.5188971472824,
16.6184400967789,16.717958106017,16.8176566759335,16.9170689452683,17.0167975829567,
17.1163839673222,17.2158598023983,17.3152685644057,17.4146448632355,17.5140190941541,
17.6135619825984,17.713080044921,17.8127786677469,17.9121906479311,18.011919269849,
18.111505638297,18.2109814773342,18.3103902231869,18.4097665058091,18.5091407204898,
18.6086836280159,18.7082016741926,18.8079002810564,18.907312350594,19.0070409683728,
19.1066273325613,19.2061031726482,19.3055119139792,19.4048881919906,19.5042624019773,
19.6038053147972,19.7033233561234,19.8030219580802,19.9024340532568,19.9661761551454),
 .UNSPECIFIED.);
#615=B_SPLINE_CURVE_WITH_KNOTS('',3,(#54110,#54111,#54112,#54113,#54114,
#54115,#54116,#54117,#54118,#54119,#54120,#54121,#54122,#54123,#54124,#54125,
#54126,#54127,#54128,#54129,#54130,#54131,#54132,#54133,#54134,#54135,#54136,
#54137,#54138,#54139,#54140,#54141,#54142,#54143,#54144,#54145,#54146,#54147,
#54148,#54149,#54150,#54151,#54152,#54153,#54154,#54155,#54156,#54157,#54158,
#54159,#54160,#54161,#54162,#54163,#54164,#54165,#54166,#54167,#54168,#54169,
#54170,#54171,#54172,#54173,#54174,#54175,#54176,#54177,#54178,#54179,#54180,
#54181,#54182,#54183,#54184,#54185,#54186,#54187,#54188,#54189,#54190,#54191,
#54192,#54193,#54194,#54195,#54196,#54197,#54198,#54199,#54200,#54201,#54202,
#54203,#54204,#54205,#54206,#54207,#54208,#54209,#54210,#54211,#54212,#54213,
#54214,#54215,#54216,#54217,#54218,#54219,#54220,#54221,#54222,#54223,#54224,
#54225,#54226,#54227,#54228,#54229,#54230,#54231,#54232,#54233,#54234,#54235,
#54236,#54237,#54238,#54239,#54240,#54241,#54242,#54243,#54244,#54245,#54246,
#54247,#54248,#54249,#54250,#54251,#54252,#54253,#54254,#54255,#54256,#54257,
#54258,#54259,#54260,#54261,#54262,#54263,#54264,#54265,#54266,#54267,#54268,
#54269,#54270,#54271,#54272,#54273,#54274,#54275,#54276,#54277,#54278,#54279,
#54280,#54281,#54282,#54283,#54284,#54285,#54286,#54287,#54288,#54289,#54290,
#54291,#54292,#54293,#54294,#54295,#54296,#54297,#54298,#54299,#54300,#54301,
#54302),.UNSPECIFIED.,.F.,.F.,(4,3,3,3,3,3,3,3,3,3,3,3,3,3,3,3,3,3,3,3,
3,3,3,3,3,3,3,3,3,3,3,3,3,3,3,3,3,3,3,3,3,3,3,3,3,3,3,3,3,3,3,3,3,3,3,3,
3,3,3,3,3,3,3,3,4),(19.9661761555181,20.0649597355301,20.1636079450829,
20.2621527857533,20.3606432135408,20.4591107687241,20.5575869594835,20.656164904063,
20.7548007419313,20.8535976761377,20.8975557559197,20.9972843776227,21.0968707458138,
21.1963465849099,21.2957553304038,21.3951316126294,21.4945058268761,21.5940487348027,
21.6935667804576,21.7932653867505,21.8926774585825,21.9924060799964,22.0919924478857,
22.1914682870557,22.29087703222,22.3902533141063,22.4896275280042,22.5891704363145,
22.6886884816009,22.7883870875165,22.8877991612453,22.9875277834658,23.0871141521756,
23.1865899911422,23.2859987371549,23.3853750198979,23.48474923466,23.5842921419721,
23.6838101881323,23.7835087949203,23.8829208639082,23.982649485756,24.0822358540888,
24.1817116931491,24.2811204387762,24.3804967211317,24.4798709355044,24.5794138432711,
24.6789318890418,24.7786304954433,24.878042566571,24.9777711884159,25.0773575567441,
25.1768333958053,25.2762421414259,25.3756184237736,25.4749926381377,25.5745355459117,
25.6740535916712,25.7737521980603,25.8731642692339,25.9856807881721,26.0977868859121,
26.2091942719789,26.2493614621018),.UNSPECIFIED.);
#616=B_SPLINE_CURVE_WITH_KNOTS('',3,(#54304,#54305,#54306,#54307,#54308,
#54309,#54310,#54311,#54312,#54313,#54314,#54315,#54316,#54317,#54318,#54319,
#54320,#54321,#54322,#54323,#54324,#54325,#54326,#54327,#54328,#54329,#54330,
#54331,#54332,#54333,#54334,#54335,#54336,#54337,#54338,#54339,#54340,#54341,
#54342,#54343,#54344,#54345,#54346,#54347,#54348,#54349,#54350,#54351,#54352,
#54353,#54354,#54355,#54356,#54357,#54358,#54359,#54360,#54361,#54362,#54363,
#54364,#54365,#54366,#54367,#54368,#54369,#54370,#54371,#54372,#54373,#54374,
#54375,#54376,#54377,#54378,#54379,#54380,#54381,#54382,#54383,#54384,#54385,
#54386,#54387,#54388,#54389,#54390,#54391,#54392,#54393,#54394,#54395,#54396,
#54397,#54398,#54399,#54400,#54401,#54402,#54403,#54404,#54405,#54406,#54407,
#54408,#54409,#54410,#54411,#54412,#54413,#54414,#54415,#54416,#54417,#54418,
#54419,#54420,#54421,#54422,#54423,#54424,#54425,#54426,#54427,#54428,#54429,
#54430,#54431,#54432,#54433,#54434,#54435,#54436,#54437,#54438,#54439,#54440,
#54441,#54442,#54443,#54444,#54445,#54446,#54447,#54448,#54449,#54450,#54451,
#54452,#54453,#54454,#54455,#54456,#54457,#54458,#54459,#54460,#54461,#54462,
#54463,#54464,#54465,#54466,#54467,#54468,#54469,#54470,#54471,#54472,#54473,
#54474,#54475,#54476,#54477,#54478,#54479,#54480,#54481,#54482,#54483,#54484,
#54485,#54486,#54487,#54488,#54489,#54490,#54491,#54492,#54493,#54494,#54495,
#54496),.UNSPECIFIED.,.F.,.F.,(4,3,3,3,3,3,3,3,3,3,3,3,3,3,3,3,3,3,3,3,
3,3,3,3,3,3,3,3,3,3,3,3,3,3,3,3,3,3,3,3,3,3,3,3,3,3,3,3,3,3,3,3,3,3,3,3,
3,3,3,3,3,3,3,3,4),(26.249361462325,26.3495432146859,26.4497399602872,26.5543764631896,
26.6547586687675,26.7552256738968,26.8558647706909,26.8682859718967,26.9680145937861,
27.0676009621604,27.1670768012103,27.2664855468789,27.3658618292753,27.4652360436889,
27.5647789514065,27.6642969972169,27.7639956036571,27.8634076745596,27.9631362964534,
28.0627226648318,28.1621985038807,28.2616072495533,28.3609835319537,28.4603577463712,
28.559900654084,28.659418699898,28.7591173063415,28.8585293772224,28.9582579991278,
29.0578443675181,29.157320206564,29.2567289522489,29.3561052346618,29.4554794490917,
29.5550223567901,29.6545404026167,29.754239009073,29.8536510798852,29.9533797017831,
30.0529660701657,30.1524419092135,30.2518506548906,30.3512269372956,30.4506011517176,
30.5501440594253,30.6496621052439,30.7493607116922,30.8487727825481,30.9485014044471,
31.048087772831,31.1475636118785,31.2469723575565,31.3463486399627,31.4457228543857,
31.545265762092,31.6447838079117,31.7444824143612,31.8438944852109,31.9431350382334,
32.0422407490315,32.1412428341483,32.2401841982582,32.3390858292702,32.4380241896836,
32.5325467695046),.UNSPECIFIED.);
#617=B_SPLINE_CURVE_WITH_KNOTS('',3,(#54498,#54499,#54500,#54501,#54502,
#54503,#54504,#54505,#54506,#54507,#54508,#54509,#54510,#54511,#54512,#54513,
#54514,#54515,#54516,#54517,#54518,#54519,#54520,#54521,#54522,#54523,#54524,
#54525,#54526,#54527,#54528,#54529,#54530,#54531,#54532,#54533,#54534,#54535,
#54536,#54537,#54538,#54539,#54540,#54541,#54542,#54543,#54544,#54545,#54546,
#54547,#54548,#54549,#54550,#54551,#54552,#54553,#54554,#54555,#54556,#54557,
#54558,#54559,#54560,#54561,#54562,#54563,#54564,#54565,#54566,#54567,#54568,
#54569,#54570,#54571,#54572,#54573,#54574,#54575,#54576,#54577,#54578,#54579,
#54580,#54581,#54582,#54583,#54584,#54585,#54586,#54587,#54588,#54589,#54590,
#54591,#54592,#54593,#54594,#54595,#54596,#54597,#54598,#54599,#54600,#54601,
#54602,#54603,#54604,#54605,#54606,#54607,#54608,#54609,#54610,#54611,#54612,
#54613,#54614,#54615,#54616,#54617,#54618,#54619,#54620,#54621,#54622,#54623,
#54624,#54625,#54626,#54627,#54628,#54629,#54630,#54631,#54632,#54633,#54634,
#54635,#54636,#54637,#54638,#54639,#54640,#54641,#54642,#54643,#54644,#54645,
#54646,#54647,#54648,#54649,#54650,#54651,#54652,#54653,#54654,#54655,#54656,
#54657,#54658,#54659,#54660,#54661,#54662,#54663,#54664,#54665,#54666,#54667,
#54668,#54669,#54670,#54671,#54672,#54673,#54674,#54675,#54676,#54677,#54678,
#54679,#54680,#54681,#54682,#54683,#54684,#54685,#54686,#54687,#54688,#54689,
#54690),.UNSPECIFIED.,.F.,.F.,(4,3,3,3,3,3,3,3,3,3,3,3,3,3,3,3,3,3,3,3,
3,3,3,3,3,3,3,3,3,3,3,3,3,3,3,3,3,3,3,3,3,3,3,3,3,3,3,3,3,3,3,3,3,3,3,3,
3,3,3,3,3,3,3,3,4),(32.5325467698621,32.6510766728329,32.7711063593354,
32.8390161878737,32.9387448097729,33.038331178157,33.1378070172045,33.237215762883,
33.3365920452893,33.4359662597127,33.5355091674187,33.6350272132388,33.7347258196885,
33.8341378905366,33.9338665124361,34.0334528808205,34.1329287198679,34.2323374655466,
34.3317137479533,34.4310879623771,34.5306308700827,34.6301489159031,34.7298475223531,
34.8292595931994,34.9289882150991,35.0285745834837,35.128050422531,35.2274591682099,
35.3268354506168,35.4262096650407,35.5257525727461,35.6252706185667,35.7249692250169,
35.8243812958623,35.9241099177618,36.0236962861461,36.1231721251935,36.2225808708722,
36.3219571532788,36.4213313677026,36.5208742754082,36.6203923212285,36.7200909276785,
36.8195029985251,36.9192316204247,37.0188179888092,37.1182938278566,37.2177025735354,
37.3170788559422,37.4164530703661,37.5159959780715,37.615514023892,37.7152126303422,
37.814624701188,37.9143533230875,38.013939691472,38.1134155305193,38.2128242761981,
38.3122005586049,38.4115747730288,38.5111176807343,38.6106357265547,38.7103343330047,
38.8097464038508,38.8157320766842),.UNSPECIFIED.);
#618=B_SPLINE_CURVE_WITH_KNOTS('',3,(#54692,#54693,#54694,#54695,#54696,
#54697,#54698,#54699,#54700,#54701,#54702,#54703,#54704,#54705,#54706,#54707,
#54708,#54709,#54710,#54711,#54712,#54713,#54714,#54715,#54716,#54717,#54718,
#54719,#54720,#54721,#54722,#54723,#54724,#54725,#54726,#54727,#54728,#54729,
#54730,#54731,#54732,#54733,#54734,#54735,#54736,#54737,#54738,#54739,#54740,
#54741,#54742,#54743,#54744,#54745,#54746,#54747,#54748,#54749,#54750,#54751,
#54752,#54753,#54754,#54755,#54756,#54757,#54758,#54759,#54760,#54761,#54762,
#54763,#54764,#54765,#54766,#54767,#54768,#54769,#54770,#54771,#54772,#54773,
#54774,#54775,#54776,#54777,#54778,#54779,#54780,#54781,#54782,#54783,#54784,
#54785,#54786,#54787,#54788,#54789,#54790,#54791,#54792,#54793,#54794,#54795,
#54796,#54797,#54798,#54799,#54800,#54801,#54802,#54803,#54804,#54805,#54806,
#54807,#54808,#54809,#54810,#54811,#54812,#54813,#54814,#54815,#54816,#54817,
#54818,#54819,#54820,#54821,#54822,#54823,#54824,#54825,#54826,#54827,#54828,
#54829,#54830,#54831,#54832,#54833,#54834,#54835,#54836,#54837,#54838,#54839,
#54840,#54841,#54842,#54843,#54844,#54845,#54846,#54847,#54848,#54849,#54850,
#54851,#54852,#54853,#54854,#54855,#54856,#54857,#54858,#54859,#54860,#54861,
#54862,#54863,#54864,#54865,#54866,#54867,#54868,#54869,#54870,#54871,#54872,
#54873,#54874,#54875,#54876,#54877,#54878,#54879,#54880,#54881),
 .UNSPECIFIED.,.F.,.F.,(4,3,3,3,3,3,3,3,3,3,3,3,3,3,3,3,3,3,3,3,3,3,3,3,
3,3,3,3,3,3,3,3,3,3,3,3,3,3,3,3,3,3,3,3,3,3,3,3,3,3,3,3,3,3,3,3,3,3,3,3,
3,3,3,4),(38.8157320770262,38.9153542708244,39.0148343426844,39.1142001341494,
39.2135034514798,39.3127748761239,39.4120449501345,39.5114128104276,39.610827763068,
39.7104214250461,39.8048681065136,39.9045967284132,40.0041830967977,40.103658935845,
40.2030676815239,40.3024439639307,40.4018181783547,40.5013610860602,40.6008791318807,
40.7005777383308,40.7999898091765,40.8997184310759,40.9993047994602,41.0987806385076,
41.1981893841863,41.2975656665931,41.396939881017,41.4964827887225,41.5960008345429,
41.6956994409929,41.7951115118393,41.8948401337389,41.9944265021234,42.0939023411707,
42.1933110868495,42.2926873692563,42.3920615836801,42.4916044913856,42.5911225372061,
42.6908211436562,42.7902332145022,42.8899618364017,42.9895482047862,43.0890240438336,
43.1884327895123,43.2878090719191,43.3871832863429,43.4867261940484,43.586244239869,
43.6859428463191,43.785354917165,43.8850835390646,43.9846699074492,44.0841457464966,
44.1835544921752,44.282930774582,44.3823049890059,44.4818478967114,44.5813659425318,
44.6810645489819,44.7804766198279,44.899085633739,45.0164064706586,45.0989173834712),
 .UNSPECIFIED.);
#619=B_SPLINE_CURVE_WITH_KNOTS('',3,(#54883,#54884,#54885,#54886,#54887,
#54888,#54889,#54890,#54891,#54892,#54893,#54894,#54895,#54896,#54897,#54898,
#54899,#54900,#54901,#54902,#54903,#54904,#54905,#54906,#54907,#54908,#54909,
#54910,#54911,#54912,#54913,#54914,#54915,#54916,#54917,#54918,#54919,#54920,
#54921,#54922,#54923,#54924,#54925,#54926,#54927,#54928,#54929,#54930,#54931,
#54932,#54933,#54934,#54935,#54936,#54937,#54938,#54939,#54940,#54941,#54942,
#54943,#54944,#54945,#54946,#54947,#54948,#54949,#54950,#54951,#54952,#54953,
#54954,#54955,#54956,#54957,#54958,#54959,#54960,#54961,#54962,#54963,#54964,
#54965,#54966,#54967,#54968,#54969,#54970,#54971,#54972,#54973,#54974,#54975,
#54976,#54977,#54978,#54979,#54980,#54981,#54982,#54983,#54984,#54985,#54986,
#54987,#54988,#54989,#54990,#54991,#54992,#54993,#54994,#54995,#54996,#54997,
#54998,#54999,#55000,#55001,#55002,#55003,#55004,#55005,#55006,#55007,#55008,
#55009,#55010,#55011,#55012,#55013,#55014,#55015,#55016,#55017,#55018,#55019,
#55020,#55021,#55022,#55023,#55024,#55025,#55026,#55027,#55028,#55029,#55030,
#55031,#55032,#55033,#55034,#55035,#55036,#55037,#55038,#55039,#55040,#55041,
#55042,#55043,#55044,#55045,#55046,#55047,#55048,#55049,#55050,#55051,#55052,
#55053,#55054,#55055,#55056,#55057,#55058,#55059,#55060,#55061,#55062,#55063,
#55064,#55065,#55066,#55067,#55068,#55069,#55070,#55071,#55072,#55073,#55074,
#55075),.UNSPECIFIED.,.F.,.F.,(4,3,3,3,3,3,3,3,3,3,3,3,3,3,3,3,3,3,3,3,
3,3,3,3,3,3,3,3,3,3,3,3,3,3,3,3,3,3,3,3,3,3,3,3,3,3,3,3,3,3,3,3,3,3,3,3,
3,3,3,3,3,3,3,3,4),(45.0989173838638,45.1980218083953,45.2971017503985,
45.3961879153463,45.4953804966537,45.5946271163157,45.6940543865298,45.7755983224907,
45.8753269443902,45.9749133127746,46.0743891518219,46.1737978975007,46.2731741799074,
46.3725483943313,46.4720913020368,46.5716093478572,46.6713079543073,46.7707200251535,
46.870448647053,46.9700350154376,47.0695108544849,47.1689196001637,47.2682958825704,
47.3676700969942,47.4672130046997,47.5667310505201,47.6664296569702,47.7658417278164,
47.865570349716,47.9651567181005,48.0646325571478,48.1640413028266,48.2634175852335,
48.3627917996575,48.4623347073629,48.5618527531833,48.6615513596333,48.7609634304792,
48.8606920523788,48.9602784207636,49.0597542598109,49.1591630054897,49.2585392878962,
49.35791350232,49.4574564100255,49.5569744558458,49.6566730622959,49.7560851331421,
49.8558137550418,49.955400123426,50.0548759624733,50.1542847081522,50.2536609905587,
50.3530352049826,50.4525781126882,50.5520961585087,50.6517947649588,50.7512068358049,
50.8515389897043,50.9517252562119,51.0517952162203,51.1517736522124,51.2516994680995,
51.3516134530358,51.3821026910434),.UNSPECIFIED.);
#620=B_SPLINE_CURVE_WITH_KNOTS('',3,(#55077,#55078,#55079,#55080,#55081,
#55082,#55083,#55084,#55085,#55086,#55087,#55088,#55089,#55090,#55091,#55092,
#55093,#55094,#55095,#55096,#55097,#55098,#55099,#55100,#55101,#55102,#55103,
#55104,#55105,#55106,#55107,#55108,#55109,#55110,#55111,#55112,#55113,#55114,
#55115,#55116,#55117,#55118,#55119,#55120,#55121,#55122,#55123,#55124,#55125,
#55126,#55127,#55128,#55129,#55130,#55131,#55132,#55133,#55134,#55135,#55136,
#55137,#55138,#55139,#55140,#55141,#55142,#55143,#55144,#55145,#55146,#55147,
#55148,#55149,#55150,#55151,#55152,#55153,#55154,#55155,#55156,#55157,#55158,
#55159,#55160,#55161,#55162,#55163,#55164,#55165,#55166,#55167,#55168,#55169,
#55170,#55171,#55172,#55173,#55174,#55175,#55176,#55177,#55178,#55179,#55180,
#55181,#55182,#55183,#55184,#55185,#55186,#55187,#55188,#55189,#55190,#55191,
#55192,#55193,#55194,#55195,#55196,#55197,#55198,#55199,#55200,#55201,#55202,
#55203,#55204,#55205,#55206,#55207,#55208,#55209,#55210,#55211,#55212,#55213,
#55214,#55215,#55216,#55217,#55218,#55219,#55220,#55221,#55222,#55223,#55224,
#55225,#55226,#55227,#55228,#55229,#55230,#55231,#55232,#55233,#55234,#55235,
#55236,#55237,#55238,#55239,#55240,#55241,#55242,#55243,#55244,#55245,#55246,
#55247,#55248,#55249,#55250,#55251,#55252,#55253,#55254,#55255,#55256,#55257,
#55258,#55259,#55260,#55261,#55262,#55263,#55264,#55265,#55266,#55267,#55268,
#55269),.UNSPECIFIED.,.F.,.F.,(4,3,3,3,3,3,3,3,3,3,3,3,3,3,3,3,3,3,3,3,
3,3,3,3,3,3,3,3,3,3,3,3,3,3,3,3,3,3,3,3,3,3,3,3,3,3,3,3,3,3,3,3,3,3,3,3,
3,3,3,3,3,3,3,3,4),(51.38210269127,51.494631253354,51.6077050198739,51.721416463853,
51.7463285384677,51.8460571603673,51.9456435287518,52.0451193677992,52.1445281134779,
52.2439043958847,52.3432786103086,52.4428215180141,52.5423395638346,52.6420381702847,
52.7414502411306,52.8411788630301,52.9407652314146,53.0402410704619,53.1396498161407,
53.2390260985474,53.3384003129713,53.4379432206768,53.5374612664973,53.6371598729474,
53.7365719437934,53.836300565693,53.9358869340774,54.0353627731248,54.1347715188035,
54.2341478012102,54.3335220156341,54.4330649233396,54.5325829691601,54.6322815756102,
54.7316936464563,54.8314222683558,54.9310086367403,55.0304844757877,55.1298932214664,
55.2292695038732,55.328643718297,55.4281866260025,55.527704671823,55.6274032782731,
55.7268153491191,55.8265439710186,55.9261303394031,56.0256061784504,56.1250149241292,
56.2243912065359,56.3237654209597,56.4233083286653,56.5228263744857,56.6225249809357,
56.7219370517819,56.8208847371964,56.9196908790247,57.0183844674433,57.1170176925836,
57.2156219572361,57.3142286261182,57.4129302438207,57.5116840268029,57.6105975209941,
57.6652879978908),.UNSPECIFIED.);
#621=B_SPLINE_CURVE_WITH_KNOTS('',3,(#55271,#55272,#55273,#55274,#55275,
#55276,#55277,#55278,#55279,#55280,#55281,#55282,#55283,#55284,#55285,#55286,
#55287,#55288,#55289,#55290,#55291,#55292,#55293,#55294,#55295,#55296,#55297,
#55298,#55299,#55300,#55301,#55302,#55303,#55304,#55305,#55306,#55307,#55308,
#55309,#55310,#55311,#55312,#55313,#55314,#55315,#55316,#55317,#55318,#55319,
#55320,#55321,#55322,#55323,#55324,#55325,#55326,#55327,#55328,#55329,#55330,
#55331,#55332,#55333,#55334,#55335,#55336,#55337,#55338,#55339,#55340,#55341,
#55342,#55343,#55344,#55345,#55346,#55347,#55348,#55349,#55350,#55351,#55352,
#55353,#55354,#55355,#55356,#55357,#55358,#55359,#55360,#55361,#55362,#55363,
#55364,#55365,#55366,#55367,#55368,#55369,#55370,#55371,#55372,#55373,#55374,
#55375,#55376,#55377,#55378,#55379,#55380,#55381,#55382,#55383,#55384,#55385,
#55386,#55387,#55388,#55389,#55390,#55391,#55392,#55393,#55394,#55395,#55396,
#55397,#55398,#55399,#55400,#55401,#55402,#55403,#55404,#55405,#55406,#55407,
#55408,#55409,#55410,#55411,#55412,#55413,#55414,#55415,#55416,#55417,#55418,
#55419,#55420,#55421,#55422,#55423,#55424,#55425,#55426,#55427,#55428,#55429,
#55430,#55431,#55432,#55433,#55434,#55435,#55436,#55437,#55438,#55439,#55440,
#55441,#55442,#55443,#55444,#55445,#55446,#55447,#55448,#55449,#55450,#55451,
#55452,#55453,#55454,#55455,#55456,#55457,#55458,#55459,#55460),
 .UNSPECIFIED.,.F.,.F.,(4,3,3,3,3,3,3,3,3,3,3,3,3,3,3,3,3,3,3,3,3,3,3,3,
3,3,3,3,3,3,3,3,3,3,3,3,3,3,3,3,3,3,3,3,3,3,3,3,3,3,3,3,3,3,3,3,3,3,3,3,
3,3,3,4),(57.665287998223,57.7170587544448,57.8167873763444,57.916373744729,
58.0158495837763,58.1152583294552,58.2146346118619,58.3140088262859,58.4135517339914,
58.5130697798119,58.612768386262,58.7121804571076,58.8119090790072,58.9114954473916,
59.0109712864389,59.1103800321177,59.2097563145245,59.3091305289483,59.4086734366539,
59.5081914824743,59.6078900889244,59.7073021597705,59.80703078167,59.9066171500545,
60.0060929891018,60.1055017347806,60.2048780171873,60.3042522316111,60.4037951393166,
60.503313185137,60.6030117915871,60.7024238624333,60.8021524843328,60.9017388527173,
61.0012146917646,61.1006234374434,61.1999997198501,61.2993739342739,61.3989168419794,
61.4984348877999,61.5981334942499,61.6975455650961,61.7972741869957,61.8968605553802,
61.9963363944276,62.0957451401064,62.1951214225132,62.2944956369371,62.3940385446426,
62.4935565904631,62.5932551969132,62.692667267759,62.7923958896585,62.8919822580429,
62.9914580970903,63.090866842769,63.1902431251756,63.2896173395995,63.389160247305,
63.4886782931254,63.5883768995755,63.6877889704218,63.8181311377544,63.9484733050871),
 .UNSPECIFIED.);
#622=B_SPLINE_CURVE_WITH_KNOTS('',3,(#55462,#55463,#55464,#55465,#55466,
#55467,#55468,#55469,#55470,#55471,#55472,#55473,#55474,#55475,#55476,#55477,
#55478,#55479,#55480,#55481,#55482,#55483,#55484,#55485,#55486,#55487,#55488,
#55489,#55490,#55491,#55492,#55493,#55494,#55495,#55496,#55497,#55498,#55499,
#55500,#55501,#55502,#55503,#55504,#55505,#55506,#55507,#55508,#55509,#55510,
#55511,#55512,#55513,#55514,#55515,#55516,#55517,#55518,#55519,#55520,#55521,
#55522,#55523,#55524,#55525,#55526,#55527,#55528,#55529,#55530,#55531,#55532,
#55533,#55534,#55535,#55536,#55537,#55538,#55539,#55540,#55541,#55542,#55543,
#55544,#55545,#55546,#55547,#55548,#55549,#55550,#55551,#55552,#55553,#55554,
#55555,#55556,#55557,#55558,#55559,#55560,#55561,#55562,#55563,#55564,#55565,
#55566,#55567,#55568,#55569,#55570,#55571,#55572,#55573,#55574,#55575,#55576,
#55577,#55578,#55579,#55580,#55581,#55582,#55583,#55584,#55585,#55586,#55587,
#55588,#55589,#55590,#55591,#55592,#55593,#55594,#55595,#55596,#55597,#55598,
#55599,#55600,#55601,#55602,#55603,#55604,#55605,#55606,#55607,#55608,#55609,
#55610,#55611,#55612,#55613,#55614,#55615,#55616,#55617,#55618,#55619,#55620,
#55621,#55622,#55623,#55624,#55625,#55626,#55627,#55628,#55629,#55630,#55631,
#55632,#55633,#55634,#55635,#55636,#55637,#55638,#55639,#55640,#55641,#55642,
#55643,#55644,#55645,#55646,#55647,#55648,#55649,#55650,#55651,#55652,#55653,
#55654),.UNSPECIFIED.,.F.,.F.,(4,3,3,3,3,3,3,3,3,3,3,3,3,3,3,3,3,3,3,3,
3,3,3,3,3,3,3,3,3,3,3,3,3,3,3,3,3,3,3,3,3,3,3,3,3,3,3,3,3,3,3,3,3,3,3,3,
3,3,3,3,3,3,3,3,4),(63.9484733054025,64.0469016666163,64.1452752386828,
64.2436256686098,64.3419845708388,64.440445668635,64.5389646754106,64.6376460323145,
64.6829106730847,64.7826392949843,64.8822256633687,64.9817015024161,65.0811102480948,
65.1804865305015,65.2798607449253,65.3794036526308,65.4789216984512,65.5786203049012,
65.6780323757475,65.777760997647,65.8773473660316,65.9768232050789,66.0762319507576,
66.1756082331642,66.274982447588,66.3745253552936,66.4740434011141,66.5737420075641,
66.6731540784104,66.77288270031,66.8724690686947,66.9719449077421,67.0713536534208,
67.1707299358277,67.2701041502517,67.3696470579571,67.4691651037777,67.5688637102279,
67.6682757810732,67.7680044029727,67.8675907713569,67.9670666104043,68.0664753560831,
68.1658516384898,68.2652258529134,68.3647687606191,68.4642868064395,68.5639854128896,
68.663397483736,68.7631261056355,68.8627124740203,68.9621883130676,69.0615970587463,
69.1609733411528,69.2603475555769,69.3598904632824,69.4594085091028,69.5591071155529,
69.6585191863989,69.760413026184,69.8621421786056,69.963700362568,70.0651579293423,
70.1665318849402,70.2316586125821),.UNSPECIFIED.);
#623=B_SPLINE_CURVE_WITH_KNOTS('',3,(#55656,#55657,#55658,#55659,#55660,
#55661,#55662,#55663,#55664,#55665,#55666,#55667,#55668,#55669,#55670,#55671,
#55672,#55673,#55674,#55675,#55676,#55677,#55678,#55679,#55680,#55681,#55682,
#55683,#55684,#55685,#55686,#55687,#55688,#55689,#55690,#55691,#55692,#55693,
#55694,#55695,#55696,#55697,#55698,#55699,#55700,#55701,#55702,#55703,#55704,
#55705,#55706,#55707,#55708,#55709,#55710,#55711,#55712,#55713,#55714,#55715,
#55716,#55717,#55718,#55719,#55720,#55721,#55722,#55723,#55724,#55725,#55726,
#55727,#55728,#55729,#55730,#55731,#55732,#55733,#55734,#55735,#55736,#55737,
#55738,#55739,#55740,#55741,#55742,#55743,#55744,#55745,#55746,#55747,#55748,
#55749,#55750,#55751,#55752,#55753,#55754,#55755,#55756,#55757,#55758,#55759,
#55760,#55761,#55762,#55763,#55764,#55765,#55766,#55767,#55768,#55769,#55770,
#55771,#55772,#55773,#55774,#55775,#55776,#55777,#55778,#55779,#55780,#55781,
#55782,#55783,#55784,#55785,#55786,#55787,#55788,#55789,#55790,#55791,#55792,
#55793,#55794,#55795,#55796,#55797,#55798,#55799,#55800,#55801,#55802,#55803,
#55804,#55805,#55806,#55807,#55808,#55809,#55810,#55811,#55812,#55813,#55814,
#55815,#55816,#55817,#55818,#55819,#55820,#55821,#55822,#55823,#55824,#55825,
#55826,#55827,#55828,#55829,#55830,#55831,#55832,#55833,#55834,#55835,#55836,
#55837,#55838,#55839,#55840,#55841,#55842,#55843,#55844,#55845),
 .UNSPECIFIED.,.F.,.F.,(4,3,3,3,3,3,3,3,3,3,3,3,3,3,3,3,3,3,3,3,3,3,3,3,
3,3,3,3,3,3,3,3,3,3,3,3,3,3,3,3,3,3,3,3,3,3,3,3,3,3,3,3,3,3,3,3,3,3,3,3,
3,3,3,4),(70.2316586129268,70.3398756418851,70.4483885887339,70.5573687920858,
70.6536408890617,70.7533695109613,70.8529558793459,70.9524317183932,71.051840464072,
71.1512167464788,71.2505909609028,71.3501338686082,71.4496519144287,71.5493505208788,
71.6487625917246,71.7484912136241,71.8480775820085,71.9475534210559,72.0469621667347,
72.1463384491414,72.2457126635652,72.3452555712707,72.4447736170912,72.5444722235412,
72.6438842943874,72.7436129162869,72.8431992846713,72.9426751237187,73.0420838693974,
73.1414601518041,73.2408343662279,73.3403772739335,73.4398953197539,73.5395939262039,
73.6390059970502,73.7387346189498,73.8383209873343,73.9377968263817,74.0372055720605,
74.1365818544673,74.2359560688912,74.3354989765967,74.4350170224171,74.5347156288673,
74.6341276997131,74.7338563216126,74.833442689997,74.9329185290444,75.0323272747231,
75.1317035571298,75.2310777715536,75.3306206792592,75.4301387250796,75.5298373315296,
75.6292494023759,75.7276742477903,75.8260704567589,75.9242418456712,76.0223541015018,
76.1204391481535,76.2190403409999,76.3172158795948,76.4160298995669,76.5148439195389),
 .UNSPECIFIED.);
#624=B_SPLINE_CURVE_WITH_KNOTS('',3,(#55847,#55848,#55849,#55850,#55851,
#55852,#55853,#55854,#55855,#55856,#55857,#55858,#55859,#55860,#55861,#55862,
#55863,#55864,#55865,#55866,#55867,#55868,#55869,#55870,#55871,#55872,#55873,
#55874,#55875,#55876,#55877,#55878,#55879,#55880,#55881,#55882,#55883,#55884,
#55885,#55886,#55887,#55888,#55889,#55890,#55891,#55892,#55893,#55894,#55895,
#55896,#55897,#55898,#55899,#55900,#55901,#55902,#55903,#55904,#55905,#55906,
#55907,#55908,#55909,#55910,#55911,#55912,#55913,#55914,#55915,#55916,#55917,
#55918,#55919,#55920,#55921,#55922,#55923,#55924,#55925,#55926,#55927,#55928,
#55929,#55930,#55931,#55932,#55933,#55934,#55935,#55936,#55937,#55938,#55939,
#55940,#55941,#55942,#55943,#55944,#55945,#55946,#55947,#55948,#55949,#55950,
#55951,#55952,#55953,#55954,#55955,#55956,#55957,#55958,#55959,#55960,#55961,
#55962,#55963,#55964,#55965,#55966,#55967,#55968,#55969,#55970,#55971,#55972,
#55973,#55974,#55975,#55976,#55977,#55978,#55979,#55980,#55981,#55982,#55983,
#55984,#55985,#55986,#55987,#55988,#55989,#55990,#55991,#55992,#55993,#55994,
#55995,#55996,#55997,#55998,#55999,#56000,#56001,#56002,#56003,#56004,#56005,
#56006,#56007,#56008,#56009,#56010,#56011,#56012,#56013,#56014,#56015,#56016,
#56017,#56018,#56019,#56020,#56021,#56022,#56023,#56024,#56025,#56026,#56027,
#56028,#56029,#56030,#56031,#56032,#56033,#56034,#56035,#56036),
 .UNSPECIFIED.,.F.,.F.,(4,3,3,3,3,3,3,3,3,3,3,3,3,3,3,3,3,3,3,3,3,3,3,3,
3,3,3,3,3,3,3,3,3,3,3,3,3,3,3,3,3,3,3,3,3,3,3,3,3,3,3,3,3,3,3,3,3,3,3,3,
3,3,3,4),(76.5148439197617,76.6243711050387,76.7240997269381,76.8236860953223,
76.9231619343697,77.0225706800483,77.1219469624549,77.2213211768786,77.3208640845843,
77.4203821304046,77.5200807368545,77.6194928077016,77.7192214296011,77.8188077979855,
77.9182836370329,78.0176923827116,78.1170686651182,78.216442879542,78.3159857872476,
78.415503833068,78.5152024395181,78.6146145103644,78.714343132264,78.8139295006486,
78.913405339696,79.0128140853748,79.1121903677816,79.2115645822056,79.311107489911,
79.4106255357315,79.5103241421817,79.6097362130273,79.7094648349268,79.8090512033113,
79.9085270423586,80.0079357880374,80.1073120704441,80.2066862848679,80.3062291925735,
80.4057472383939,80.5054458448439,80.6048579156901,80.7045865375896,80.8041729059741,
80.9036487450215,81.0030574907002,81.1024337731069,81.2018079875307,81.3013508952363,
81.4008689410567,81.5005675475068,81.599979618353,81.6997082402526,81.7992946086371,
81.8987704476845,81.9981791933633,82.0975554757701,82.1969296901939,82.2964725978994,
82.3959906437198,82.49568925017,82.5951013210158,82.7361481116942,82.7980292269413),
 .UNSPECIFIED.);
#625=B_SPLINE_CURVE_WITH_KNOTS('',3,(#56038,#56039,#56040,#56041,#56042,
#56043,#56044,#56045,#56046,#56047,#56048,#56049,#56050,#56051,#56052,#56053,
#56054,#56055,#56056,#56057,#56058,#56059,#56060,#56061,#56062,#56063,#56064,
#56065,#56066,#56067,#56068,#56069,#56070,#56071,#56072,#56073,#56074,#56075,
#56076,#56077,#56078,#56079,#56080,#56081,#56082,#56083,#56084,#56085,#56086,
#56087,#56088,#56089,#56090,#56091,#56092,#56093,#56094,#56095,#56096,#56097,
#56098,#56099,#56100,#56101,#56102,#56103,#56104,#56105,#56106,#56107,#56108,
#56109,#56110,#56111,#56112,#56113,#56114,#56115,#56116,#56117,#56118,#56119,
#56120,#56121,#56122,#56123,#56124,#56125,#56126,#56127,#56128,#56129,#56130,
#56131,#56132,#56133,#56134,#56135,#56136,#56137,#56138,#56139,#56140,#56141,
#56142,#56143,#56144,#56145,#56146,#56147,#56148,#56149,#56150,#56151,#56152,
#56153,#56154,#56155,#56156,#56157,#56158,#56159,#56160,#56161,#56162,#56163,
#56164,#56165,#56166,#56167,#56168,#56169,#56170,#56171,#56172,#56173,#56174,
#56175,#56176,#56177,#56178,#56179,#56180,#56181,#56182,#56183,#56184,#56185,
#56186,#56187,#56188,#56189,#56190,#56191,#56192,#56193,#56194,#56195,#56196,
#56197,#56198,#56199,#56200,#56201,#56202,#56203,#56204,#56205,#56206,#56207,
#56208,#56209,#56210,#56211,#56212,#56213,#56214,#56215,#56216,#56217,#56218,
#56219,#56220,#56221,#56222,#56223,#56224,#56225,#56226,#56227),
 .UNSPECIFIED.,.F.,.F.,(4,3,3,3,3,3,3,3,3,3,3,3,3,3,3,3,3,3,3,3,3,3,3,3,
3,3,3,3,3,3,3,3,3,3,3,3,3,3,3,3,3,3,3,3,3,3,3,3,3,3,3,3,3,3,3,3,3,3,3,3,
3,3,3,4),(82.7980292272367,82.8970534517919,82.9950894977502,83.0930789271652,
83.1910537466629,83.2908460659168,83.3889446960583,83.4895838598685,83.5902230236787,
83.6899516455782,83.7895380139627,83.88901385301,83.9884225986888,84.0877988810955,
84.1871730955195,84.286716003225,84.3862340490455,84.4859326554956,84.5853447263415,
84.6850733482411,84.7846597166256,84.8841355556729,84.9835443013518,85.0829205837586,
85.1822947981825,85.2818377058879,85.3813557517083,85.4810543581584,85.5804664290043,
85.6801950509038,85.7797814192885,85.8792572583358,85.9786660040146,86.0780422864214,
86.1774165008454,86.2769594085509,86.3764774543713,86.4761760608214,86.5755881316672,
86.6753167535667,86.7749031219511,86.8743789609985,86.9737877066772,87.0731639890841,
87.1725382035081,87.2720811112135,87.3715991570341,87.4712977634842,87.57070983433,
87.6704384562295,87.7700248246142,87.8695006636615,87.9689094093401,88.0682856917468,
88.1676599061707,88.2672028138763,88.3667208596967,88.4664194661467,88.5658315369929,
88.6698572087964,88.7736129224715,88.877209535948,88.9806129425655,89.0812145341209),
 .UNSPECIFIED.);
#626=B_SPLINE_CURVE_WITH_KNOTS('',3,(#56229,#56230,#56231,#56232,#56233,
#56234,#56235,#56236,#56237,#56238,#56239,#56240,#56241,#56242,#56243,#56244,
#56245,#56246,#56247,#56248,#56249,#56250,#56251,#56252,#56253,#56254,#56255,
#56256,#56257,#56258,#56259,#56260,#56261,#56262,#56263,#56264,#56265,#56266,
#56267,#56268,#56269,#56270,#56271,#56272,#56273,#56274,#56275,#56276,#56277,
#56278,#56279,#56280,#56281,#56282,#56283,#56284,#56285,#56286,#56287,#56288,
#56289,#56290,#56291,#56292,#56293,#56294,#56295,#56296,#56297,#56298,#56299,
#56300,#56301,#56302,#56303,#56304,#56305,#56306,#56307,#56308,#56309,#56310,
#56311,#56312,#56313,#56314,#56315,#56316,#56317,#56318,#56319,#56320,#56321,
#56322,#56323,#56324,#56325,#56326,#56327,#56328,#56329,#56330,#56331,#56332,
#56333,#56334,#56335,#56336,#56337,#56338,#56339,#56340,#56341,#56342,#56343,
#56344,#56345,#56346,#56347,#56348,#56349,#56350,#56351,#56352,#56353,#56354,
#56355,#56356,#56357,#56358,#56359,#56360,#56361,#56362,#56363,#56364,#56365,
#56366,#56367,#56368,#56369,#56370,#56371,#56372,#56373,#56374,#56375,#56376,
#56377,#56378,#56379,#56380,#56381,#56382,#56383,#56384,#56385,#56386,#56387,
#56388,#56389,#56390,#56391,#56392,#56393,#56394,#56395,#56396,#56397,#56398,
#56399,#56400,#56401,#56402,#56403,#56404,#56405,#56406,#56407,#56408,#56409,
#56410,#56411,#56412,#56413,#56414,#56415,#56416,#56417,#56418,#56419,#56420,
#56421),.UNSPECIFIED.,.F.,.F.,(4,3,3,3,3,3,3,3,3,3,3,3,3,3,3,3,3,3,3,3,
3,3,3,3,3,3,3,3,3,3,3,3,3,3,3,3,3,3,3,3,3,3,3,3,3,3,3,3,3,3,3,3,3,3,3,3,
3,3,3,3,3,3,3,3,4),(89.0812145344922,89.1860740166197,89.2912565031786,
89.3966087067022,89.5022553233101,89.5609532396557,89.6606818615553,89.7602682299397,
89.8597440689871,89.9591528146659,90.0585290970726,90.1579033114963,90.2574462192019,
90.3569642650223,90.4566628714724,90.5560749423185,90.655803564218,90.7553899326024,
90.8548657716498,90.9542745173286,91.0536507997353,91.1530250141591,91.2525679218647,
91.352085967685,91.4517845741351,91.5511966449814,91.6509252668809,91.7505116352654,
91.8499874743128,91.9493962199916,92.0487725023983,92.1481467168222,92.2476896245277,
92.3472076703481,92.4469062767982,92.5463183476442,92.6460469695437,92.7456333379281,
92.8451091769755,92.9445179226543,93.043894205061,93.1432684194848,93.2428113271904,
93.3423293730108,93.4420279794608,93.541440050307,93.6411686722065,93.7407550405911,
93.8402308796384,93.9396396253172,94.039015907724,94.1383901221479,94.2379330298534,
94.3374510756738,94.4371496821239,94.5365617529699,94.6348132263263,94.7329006641366,
94.8308961695538,94.9288319032292,95.0267399465123,95.1246969666554,95.2226815253506,
95.3207833079917,95.3643998409918),.UNSPECIFIED.);
#627=B_SPLINE_CURVE_WITH_KNOTS('',3,(#56423,#56424,#56425,#56426,#56427,
#56428,#56429,#56430,#56431,#56432,#56433,#56434,#56435,#56436,#56437,#56438,
#56439,#56440,#56441,#56442,#56443,#56444,#56445,#56446,#56447,#56448,#56449,
#56450,#56451,#56452,#56453,#56454,#56455,#56456,#56457,#56458,#56459,#56460,
#56461,#56462,#56463,#56464,#56465,#56466,#56467,#56468,#56469,#56470,#56471,
#56472,#56473,#56474,#56475,#56476,#56477,#56478,#56479,#56480,#56481,#56482,
#56483,#56484,#56485,#56486,#56487,#56488,#56489,#56490,#56491,#56492,#56493,
#56494,#56495,#56496,#56497,#56498,#56499,#56500,#56501,#56502,#56503,#56504,
#56505,#56506,#56507,#56508,#56509,#56510,#56511,#56512,#56513,#56514,#56515,
#56516,#56517,#56518,#56519,#56520,#56521,#56522,#56523,#56524,#56525,#56526,
#56527,#56528,#56529,#56530,#56531,#56532,#56533,#56534,#56535,#56536,#56537,
#56538,#56539,#56540,#56541,#56542,#56543,#56544,#56545,#56546,#56547,#56548,
#56549,#56550,#56551,#56552,#56553,#56554,#56555,#56556,#56557,#56558,#56559,
#56560,#56561,#56562,#56563,#56564,#56565,#56566,#56567,#56568,#56569,#56570,
#56571,#56572,#56573,#56574,#56575,#56576,#56577,#56578,#56579,#56580,#56581,
#56582,#56583,#56584,#56585,#56586,#56587,#56588,#56589,#56590,#56591,#56592,
#56593,#56594,#56595,#56596,#56597,#56598,#56599,#56600,#56601,#56602,#56603,
#56604,#56605,#56606,#56607,#56608,#56609,#56610,#56611,#56612),
 .UNSPECIFIED.,.F.,.F.,(4,3,3,3,3,3,3,3,3,3,3,3,3,3,3,3,3,3,3,3,3,3,3,3,
3,3,3,3,3,3,3,3,3,3,3,3,3,3,3,3,3,3,3,3,3,3,3,3,3,3,3,3,3,3,3,3,3,3,3,3,
3,3,3,4),(95.3643998413005,95.5209226988385,95.5316834556327,95.6314120775325,
95.730998445917,95.8304742849643,95.9298830306433,96.0292593130502,96.1286335274742,
96.2281764351796,96.3276944810002,96.4273930874506,96.5268051582956,96.626533780195,
96.7261201485794,96.8255959876268,96.9250047333054,97.024381015712,97.1237552301357,
97.2232981378414,97.3228161836617,97.4225147901116,97.5219268609584,97.6216554828579,
97.7212418512424,97.8207176902898,97.9201264359686,98.0195027183753,98.1188769327992,
98.2184198405047,98.3179378863252,98.4176364927753,98.5170485636213,98.6167771855208,
98.7163635539053,98.8158393929527,98.9152481386314,99.0146244210382,99.113998635462,
99.2135415431676,99.313059588988,99.4127581954381,99.5121702662841,99.6118988881836,
99.711485256568,99.8109610956154,99.9103698412941,100.009746123701,100.109120338125,
100.20866324583,100.308181291651,100.407879898101,100.507291968947,100.607020590847,
100.706606959231,100.806082798279,100.905491543958,101.004867826364,101.104242040788,
101.203784948494,101.303302994314,101.403001600765,101.50241367161,101.64758514848),
 .UNSPECIFIED.);
#628=B_SPLINE_CURVE_WITH_KNOTS('',3,(#56614,#56615,#56616,#56617,#56618,
#56619,#56620,#56621,#56622,#56623,#56624,#56625,#56626,#56627,#56628,#56629,
#56630,#56631,#56632,#56633,#56634,#56635,#56636,#56637,#56638,#56639,#56640,
#56641,#56642,#56643,#56644,#56645,#56646,#56647,#56648,#56649,#56650,#56651,
#56652,#56653,#56654,#56655,#56656,#56657,#56658,#56659,#56660,#56661,#56662,
#56663,#56664,#56665,#56666,#56667,#56668,#56669,#56670,#56671,#56672,#56673,
#56674,#56675,#56676,#56677,#56678,#56679,#56680,#56681,#56682,#56683,#56684,
#56685,#56686,#56687,#56688,#56689,#56690,#56691,#56692,#56693,#56694,#56695,
#56696,#56697,#56698,#56699,#56700,#56701,#56702,#56703,#56704,#56705,#56706,
#56707,#56708,#56709,#56710,#56711,#56712,#56713,#56714,#56715,#56716,#56717,
#56718,#56719,#56720,#56721,#56722,#56723,#56724,#56725,#56726,#56727,#56728,
#56729,#56730,#56731,#56732,#56733,#56734,#56735,#56736,#56737,#56738,#56739,
#56740,#56741,#56742,#56743,#56744,#56745,#56746,#56747,#56748,#56749,#56750,
#56751,#56752,#56753,#56754,#56755,#56756,#56757,#56758,#56759,#56760,#56761,
#56762,#56763,#56764,#56765,#56766,#56767,#56768,#56769,#56770,#56771,#56772,
#56773,#56774,#56775,#56776,#56777,#56778,#56779,#56780,#56781,#56782,#56783,
#56784,#56785,#56786,#56787,#56788,#56789,#56790,#56791,#56792,#56793,#56794,
#56795,#56796,#56797,#56798,#56799,#56800,#56801,#56802,#56803,#56804,#56805,
#56806),.UNSPECIFIED.,.F.,.F.,(4,3,3,3,3,3,3,3,3,3,3,3,3,3,3,3,3,3,3,3,
3,3,3,3,3,3,3,3,3,3,3,3,3,3,3,3,3,3,3,3,3,3,3,3,3,3,3,3,3,3,3,3,3,3,3,3,
3,3,3,3,3,3,3,3,4),(101.647585148862,101.745752943682,101.843798677613,
101.941778175553,102.039723508507,102.137666700871,102.235703069986,102.333788608231,
102.432039269302,102.497535374273,102.597263996172,102.696850364556,102.796326203604,
102.895734949282,102.995111231688,103.094485446112,103.194028353818,103.293546399638,
103.393245006088,103.492657076935,103.592385698834,103.691972067219,103.791447906266,
103.890856651945,103.990232934352,104.089607148775,104.189150056481,104.288668102301,
104.388366708751,104.487778779598,104.587507401498,104.687093769882,104.78656960893,
104.885978354609,104.985354637016,105.08472885144,105.184271759145,105.283789804966,
105.383488411416,105.482900482261,105.58262910416,105.682215472545,105.781691311592,
105.881100057271,105.980476339678,106.079850554102,106.179393461807,106.278911507628,
106.378610114078,106.478022184924,106.577750806823,106.677337175208,106.776813014255,
106.876221759934,106.975598042341,107.074972256764,107.17451516447,107.274033210291,
107.373731816741,107.473143887587,107.580031519542,107.686559866531,107.792861004934,
107.898852412545,107.930770455256),.UNSPECIFIED.);
#629=B_SPLINE_CURVE_WITH_KNOTS('',3,(#56808,#56809,#56810,#56811,#56812,
#56813,#56814,#56815,#56816,#56817,#56818,#56819,#56820,#56821,#56822,#56823,
#56824,#56825,#56826,#56827,#56828,#56829,#56830,#56831,#56832,#56833,#56834,
#56835,#56836,#56837,#56838,#56839,#56840,#56841,#56842,#56843,#56844,#56845,
#56846,#56847,#56848,#56849,#56850,#56851,#56852,#56853,#56854,#56855,#56856,
#56857,#56858,#56859,#56860,#56861,#56862,#56863,#56864,#56865,#56866,#56867,
#56868,#56869,#56870,#56871,#56872,#56873,#56874,#56875,#56876,#56877,#56878,
#56879,#56880,#56881,#56882,#56883,#56884,#56885,#56886,#56887,#56888,#56889,
#56890,#56891,#56892,#56893,#56894,#56895,#56896,#56897,#56898,#56899,#56900,
#56901,#56902,#56903,#56904,#56905,#56906,#56907,#56908,#56909,#56910,#56911,
#56912,#56913,#56914,#56915,#56916,#56917,#56918,#56919,#56920,#56921,#56922,
#56923,#56924,#56925,#56926,#56927,#56928,#56929,#56930,#56931,#56932,#56933,
#56934,#56935,#56936,#56937,#56938,#56939,#56940,#56941,#56942,#56943,#56944,
#56945,#56946,#56947,#56948,#56949,#56950,#56951,#56952,#56953,#56954,#56955,
#56956,#56957,#56958,#56959,#56960,#56961,#56962,#56963,#56964,#56965,#56966,
#56967,#56968,#56969,#56970,#56971,#56972,#56973,#56974,#56975,#56976,#56977,
#56978,#56979,#56980,#56981,#56982,#56983,#56984,#56985,#56986,#56987,#56988,
#56989,#56990,#56991,#56992,#56993,#56994,#56995,#56996,#56997,#56998,#56999,
#57000),.UNSPECIFIED.,.F.,.F.,(4,3,3,3,3,3,3,3,3,3,3,3,3,3,3,3,3,3,3,3,
3,3,3,3,3,3,3,3,3,3,3,3,3,3,3,3,3,3,3,3,3,3,3,3,3,3,3,3,3,3,3,3,3,3,3,3,
3,3,3,3,3,3,3,3,4),(107.93077045566,108.033274088848,108.135876649722,108.238684310835,
108.341609860134,108.444749596055,108.46826559025,108.56799421215,108.667580580534,
108.767056419582,108.866465165261,108.965841447667,109.065215662091,109.164758569797,
109.264276615617,109.363975222067,109.463387292913,109.563115914812,109.662702283196,
109.762178122244,109.861586867922,109.960963150329,110.060337364752,110.159880272458,
110.259398318278,110.359096924728,110.458508995575,110.558237617474,110.657823985859,
110.757299824906,110.856708570585,110.956084852992,111.055459067415,111.155001975121,
111.254520020941,111.354218627391,111.453630698238,111.553359320138,111.652945688522,
111.75242152757,111.851830273249,111.951206555656,112.05058077008,112.150123677785,
112.249641723605,112.349340330056,112.448752400901,112.5484810228,112.648067391185,
112.747543230233,112.846951975911,112.946328258318,113.045702472742,113.145245380447,
113.244763426268,113.344462032718,113.443874103564,113.542257329618,113.640513780549,
113.738675593745,113.836774785775,113.934878007869,114.032978129635,114.131171661169,
114.213955762534),.UNSPECIFIED.);
#630=B_SPLINE_CURVE_WITH_KNOTS('',3,(#57002,#57003,#57004,#57005,#57006,
#57007,#57008,#57009,#57010,#57011,#57012,#57013,#57014,#57015,#57016,#57017,
#57018,#57019,#57020,#57021,#57022,#57023,#57024,#57025,#57026,#57027,#57028,
#57029,#57030,#57031,#57032,#57033,#57034,#57035,#57036,#57037,#57038,#57039,
#57040,#57041,#57042,#57043,#57044,#57045,#57046,#57047,#57048,#57049,#57050,
#57051,#57052,#57053,#57054,#57055,#57056,#57057,#57058,#57059,#57060,#57061,
#57062,#57063,#57064,#57065,#57066,#57067,#57068,#57069,#57070,#57071,#57072,
#57073,#57074,#57075,#57076,#57077,#57078,#57079,#57080,#57081,#57082,#57083,
#57084,#57085,#57086,#57087,#57088,#57089,#57090,#57091,#57092,#57093,#57094,
#57095,#57096,#57097,#57098,#57099,#57100,#57101,#57102,#57103,#57104,#57105,
#57106,#57107,#57108,#57109,#57110,#57111,#57112,#57113,#57114,#57115,#57116,
#57117,#57118,#57119,#57120,#57121,#57122,#57123,#57124,#57125,#57126,#57127,
#57128,#57129,#57130,#57131,#57132,#57133,#57134,#57135,#57136,#57137,#57138,
#57139,#57140,#57141,#57142,#57143,#57144,#57145,#57146,#57147,#57148,#57149,
#57150,#57151,#57152,#57153,#57154,#57155,#57156,#57157,#57158,#57159,#57160,
#57161,#57162,#57163,#57164,#57165,#57166,#57167,#57168,#57169,#57170,#57171,
#57172,#57173,#57174,#57175,#57176,#57177,#57178,#57179,#57180,#57181,#57182,
#57183,#57184,#57185,#57186,#57187,#57188,#57189,#57190,#57191),
 .UNSPECIFIED.,.F.,.F.,(4,3,3,3,3,3,3,3,3,3,3,3,3,3,3,3,3,3,3,3,3,3,3,3,
3,3,3,3,3,3,3,3,3,3,3,3,3,3,3,3,3,3,3,3,3,3,3,3,3,3,3,3,3,3,3,3,3,3,3,3,
3,3,3,4),(114.213955762839,114.348406921202,114.438995806227,114.538724428126,
114.63831079651,114.737786635558,114.837195381236,114.936571663642,115.035945878065,
115.135488785772,115.235006831591,115.334705438041,115.43411750889,115.533846130789,
115.633432499173,115.732908338221,115.832317083899,115.931693366306,116.031067580729,
116.130610488435,116.230128534255,116.329827140705,116.429239211552,116.528967833451,
116.628554201836,116.728030040883,116.827438786562,116.926815068968,117.026189283392,
117.125732191097,117.225250236918,117.324948843368,117.424360914215,117.524089536115,
117.623675904501,117.723151743548,117.822560489228,117.921936771635,118.02131098606,
118.120853893765,118.220371939586,118.320070546037,118.419482616878,118.519211238777,
118.618797607161,118.718273446208,118.817682191886,118.917058474292,119.016432688716,
119.115975596422,119.215493642242,119.315192248691,119.414604319541,119.514332941439,
119.613919309822,119.713395148869,119.812803894546,119.912180176951,120.011554391374,
120.111097299081,120.2106153449,120.310313951348,120.409726022204,120.497141070019),
 .UNSPECIFIED.);
#631=B_SPLINE_CURVE_WITH_KNOTS('',3,(#57193,#57194,#57195,#57196,#57197,
#57198,#57199,#57200,#57201,#57202,#57203,#57204,#57205,#57206,#57207,#57208,
#57209,#57210,#57211,#57212,#57213,#57214,#57215,#57216,#57217,#57218,#57219,
#57220,#57221,#57222,#57223,#57224,#57225,#57226,#57227,#57228,#57229,#57230,
#57231,#57232,#57233,#57234,#57235,#57236,#57237,#57238,#57239,#57240,#57241,
#57242,#57243,#57244,#57245,#57246,#57247,#57248,#57249,#57250,#57251,#57252,
#57253,#57254,#57255,#57256,#57257,#57258,#57259,#57260,#57261,#57262,#57263,
#57264,#57265,#57266,#57267,#57268,#57269,#57270,#57271,#57272,#57273,#57274,
#57275,#57276,#57277,#57278,#57279,#57280,#57281,#57282,#57283,#57284,#57285,
#57286,#57287,#57288,#57289,#57290,#57291,#57292,#57293,#57294,#57295,#57296,
#57297,#57298,#57299,#57300,#57301,#57302,#57303,#57304,#57305,#57306,#57307,
#57308,#57309,#57310,#57311,#57312,#57313,#57314,#57315,#57316,#57317,#57318,
#57319,#57320,#57321,#57322,#57323,#57324,#57325,#57326,#57327,#57328,#57329,
#57330,#57331,#57332,#57333,#57334,#57335,#57336,#57337,#57338,#57339,#57340,
#57341,#57342,#57343,#57344,#57345,#57346,#57347,#57348,#57349,#57350,#57351,
#57352,#57353,#57354,#57355,#57356,#57357,#57358,#57359,#57360,#57361,#57362,
#57363,#57364,#57365,#57366,#57367,#57368,#57369,#57370,#57371,#57372,#57373,
#57374,#57375,#57376,#57377,#57378,#57379,#57380,#57381,#57382,#57383,#57384,
#57385),.UNSPECIFIED.,.F.,.F.,(4,3,3,3,3,3,3,3,3,3,3,3,3,3,3,3,3,3,3,3,
3,3,3,3,3,3,3,3,3,3,3,3,3,3,3,3,3,3,3,3,3,3,3,3,3,3,3,3,3,3,3,3,3,3,3,3,
3,3,3,3,3,3,3,3,4),(120.497141070234,120.595677943242,120.696824165945,
120.795132645144,120.893392568864,120.991635696353,121.094938703481,121.193304234699,
121.291735213299,121.390318471888,121.404847724867,121.50457634676,121.604162715137,
121.703638554186,121.803047299858,121.902423582258,122.001797796676,122.101340704389,
122.200858750203,122.300557356647,122.399969427529,122.499698049419,122.599284417793,
122.698760256843,122.798169002511,122.897545284908,122.996919499321,123.096462407039,
123.195980452849,123.295679059289,123.395091130192,123.494819752138,123.594406120569,
123.693881959605,123.793290705331,123.892666987784,123.992041202254,124.091584109904,
124.19110215577,124.290800762264,124.390212832855,124.489941454693,124.589527823017,
124.689003662079,124.788412407698,124.887788690045,124.987162904411,125.086705812187,
125.186223857951,125.285922464346,125.385334535518,125.485063157369,125.584649525705,
125.684125364764,125.783534110393,125.882910392748,125.982284607121,126.081827514886,
126.181345560654,126.281044167052,126.380456238181,126.49102766556,126.601262124105,
126.710922081326,126.780326376994),.UNSPECIFIED.);
#632=B_SPLINE_CURVE_WITH_KNOTS('',3,(#57387,#57388,#57389,#57390,#57391,
#57392,#57393,#57394,#57395,#57396,#57397,#57398,#57399,#57400,#57401,#57402,
#57403,#57404,#57405,#57406,#57407,#57408,#57409,#57410,#57411,#57412,#57413,
#57414,#57415,#57416,#57417,#57418,#57419,#57420,#57421,#57422,#57423,#57424,
#57425,#57426,#57427,#57428,#57429,#57430,#57431,#57432,#57433,#57434,#57435,
#57436,#57437,#57438,#57439,#57440,#57441,#57442,#57443,#57444,#57445,#57446,
#57447,#57448,#57449,#57450,#57451,#57452,#57453,#57454,#57455,#57456,#57457,
#57458,#57459,#57460,#57461,#57462,#57463,#57464,#57465,#57466,#57467,#57468,
#57469,#57470,#57471,#57472,#57473,#57474,#57475,#57476,#57477,#57478,#57479,
#57480,#57481,#57482,#57483,#57484,#57485,#57486,#57487,#57488,#57489,#57490,
#57491,#57492,#57493,#57494,#57495,#57496,#57497,#57498,#57499,#57500,#57501,
#57502,#57503,#57504,#57505,#57506,#57507,#57508,#57509,#57510,#57511,#57512,
#57513,#57514,#57515,#57516,#57517,#57518,#57519,#57520,#57521,#57522,#57523,
#57524,#57525,#57526,#57527,#57528,#57529,#57530,#57531,#57532,#57533,#57534,
#57535,#57536,#57537,#57538,#57539,#57540,#57541,#57542,#57543,#57544,#57545,
#57546,#57547,#57548,#57549,#57550,#57551,#57552,#57553,#57554,#57555,#57556,
#57557,#57558,#57559,#57560,#57561,#57562,#57563,#57564,#57565,#57566,#57567,
#57568,#57569,#57570,#57571,#57572,#57573,#57574,#57575,#57576,#57577,#57578,
#57579),.UNSPECIFIED.,.F.,.F.,(4,3,3,3,3,3,3,3,3,3,3,3,3,3,3,3,3,3,3,3,
3,3,3,3,3,3,3,3,3,3,3,3,3,3,3,3,3,3,3,3,3,3,3,3,3,3,3,3,3,3,3,3,3,3,3,3,
3,3,3,3,3,3,3,3,4),(126.780326377198,126.881078545404,126.9818657866,127.082797177342,
127.183801456351,127.285014187782,127.375577940844,127.475306562208,127.574892930058,
127.674368769239,127.773777514391,127.873153796274,127.972528010178,128.07207091851,
128.171588963827,128.271287569787,128.370699643506,128.470428265251,128.570014633474,
128.669490472561,128.768899218066,128.868275500294,128.967649714534,129.067192622443,
129.166710668072,129.266409274327,129.365821346169,129.465549970453,129.565136341231,
129.664612179681,129.764020927755,129.863397212554,129.962771429362,130.062314334229,
130.161832382391,130.261530991139,130.360943048832,130.460671666238,130.560258030133,
130.659733870304,130.759142611539,130.858518889529,130.957893099569,131.057436012551,
131.156954054111,131.256652656409,131.356064751495,131.455793373826,131.555379742598,
131.654855581543,131.754264327501,131.853640610147,131.953014824768,132.052557732116,
132.152075778033,132.25177438452,132.351186454158,132.450099816114,132.548881393724,
132.647562789345,132.746175488395,132.844770428116,132.94335698319,133.041995581221,
133.063511684378),.UNSPECIFIED.);
#633=B_SPLINE_CURVE_WITH_KNOTS('',3,(#57581,#57582,#57583,#57584,#57585,
#57586,#57587,#57588,#57589,#57590,#57591),.UNSPECIFIED.,.F.,.F.,(4,1,1,
1,1,1,1,1,4),(133.063516053725,133.346308156821,134.341429859484,135.336551562146,
136.331673264809,137.326794967472,138.321916670135,139.317038372798,139.346696991558),
 .UNSPECIFIED.);
#634=B_SPLINE_CURVE_WITH_KNOTS('',3,(#57593,#57594,#57595,#57596,#57597,
#57598,#57599,#57600,#57601,#57602,#57603,#57604,#57605,#57606,#57607,#57608,
#57609,#57610,#57611,#57612,#57613,#57614,#57615,#57616,#57617,#57618,#57619,
#57620,#57621,#57622,#57623,#57624,#57625,#57626,#57627,#57628,#57629,#57630,
#57631,#57632,#57633,#57634,#57635,#57636,#57637,#57638,#57639,#57640,#57641,
#57642,#57643,#57644,#57645,#57646,#57647,#57648,#57649,#57650,#57651,#57652,
#57653,#57654,#57655,#57656,#57657,#57658,#57659,#57660,#57661,#57662,#57663,
#57664,#57665,#57666,#57667,#57668,#57669,#57670,#57671,#57672,#57673,#57674,
#57675,#57676,#57677,#57678,#57679,#57680,#57681,#57682,#57683,#57684,#57685,
#57686,#57687,#57688,#57689,#57690,#57691,#57692,#57693,#57694,#57695,#57696,
#57697,#57698,#57699,#57700,#57701,#57702,#57703,#57704,#57705,#57706,#57707,
#57708,#57709,#57710,#57711,#57712,#57713,#57714,#57715,#57716,#57717,#57718,
#57719,#57720,#57721,#57722,#57723,#57724,#57725,#57726,#57727,#57728,#57729,
#57730,#57731,#57732,#57733,#57734,#57735,#57736,#57737,#57738,#57739,#57740,
#57741,#57742,#57743,#57744,#57745,#57746,#57747,#57748,#57749,#57750,#57751,
#57752,#57753,#57754,#57755,#57756,#57757,#57758,#57759,#57760,#57761,#57762,
#57763,#57764,#57765,#57766,#57767,#57768,#57769,#57770,#57771,#57772,#57773,
#57774,#57775,#57776,#57777,#57778,#57779,#57780,#57781,#57782),
 .UNSPECIFIED.,.F.,.F.,(4,3,3,3,3,3,3,3,3,3,3,3,3,3,3,3,3,3,3,3,3,3,3,3,
3,3,3,3,3,3,3,3,3,3,3,3,3,3,3,3,3,3,3,3,3,3,3,3,3,3,3,3,3,3,3,3,3,3,3,3,
3,3,3,4),(139.346696991558,139.445932219988,139.545026998055,139.644010661625,
139.742934364386,139.841829171499,139.940726110939,140.03972202176,140.138769074976,
140.237987522751,140.312160075461,140.411890830886,140.511479319214,140.610954626578,
140.710365444305,140.809743776229,140.909120014983,141.008660455768,141.108180444377,
141.207880929671,141.307281778123,141.40701438211,141.506604770947,141.606080477375,
141.70549330576,141.804873685462,141.904252006059,142.00378987474,142.103312005716,
142.203014651642,142.302403480786,142.402115418057,142.501685072281,142.601165086177,
142.700557167953,142.799916842311,142.899274526842,142.998837190994,143.098339064789,
143.198021841211,143.297525183449,143.39727413812,143.496880755207,143.596372432096,
143.695801067961,143.795197072117,143.894590813936,143.99410483198,144.093641727075,
144.193358620266,144.292646886112,144.392396271959,144.492003698188,144.591496744217,
144.690927087346,144.790325131506,144.889721240998,144.989233077942,145.088773106491,
145.188493561045,145.287768588775,145.403528113215,145.518253671831,145.629882298513),
 .UNSPECIFIED.);
#635=B_SPLINE_CURVE_WITH_KNOTS('',3,(#57784,#57785,#57786,#57787,#57788,
#57789,#57790,#57791,#57792,#57793,#57794,#57795,#57796,#57797,#57798,#57799,
#57800,#57801,#57802,#57803,#57804,#57805,#57806,#57807,#57808,#57809,#57810,
#57811,#57812,#57813,#57814,#57815,#57816,#57817,#57818,#57819,#57820,#57821,
#57822,#57823,#57824,#57825,#57826,#57827,#57828,#57829,#57830,#57831,#57832,
#57833,#57834,#57835,#57836,#57837,#57838,#57839,#57840,#57841,#57842,#57843,
#57844,#57845,#57846,#57847,#57848,#57849,#57850,#57851,#57852,#57853,#57854,
#57855,#57856,#57857,#57858,#57859,#57860,#57861,#57862,#57863,#57864,#57865),
 .UNSPECIFIED.,.F.,.F.,(4,3,3,3,3,3,3,3,3,3,3,3,3,3,3,3,3,3,3,3,3,3,3,3,
3,3,3,4),(145.629882298737,145.729225833863,145.828559651808,145.927914037052,
146.027388172392,146.126928281348,146.226647384157,146.282890291438,146.382800769648,
146.482568504997,146.582219937219,146.681807426266,146.78136116726,146.880911314415,
146.98055545124,147.080244052822,147.180108308869,147.2780119941,147.376723895628,
147.479230747624,147.577691171678,147.676094980091,147.774473804444,147.872859241564,
147.971339333989,148.069875915663,148.168560926324,148.196778711597),
 .UNSPECIFIED.);
#636=B_SPLINE_CURVE_WITH_KNOTS('',3,(#57869,#57870,#57871,#57872,#57873),
 .UNSPECIFIED.,.F.,.F.,(4,1,4),(-150.263377102089,-149.268255399426,-148.604832135738),
 .UNSPECIFIED.);
#637=B_SPLINE_CURVE_WITH_KNOTS('',3,(#57875,#57876,#57877,#57878,#57879,
#57880,#57881,#57882,#57883,#57884,#57885,#57886,#57887,#57888,#57889,#57890,
#57891,#57892,#57893,#57894,#57895,#57896,#57897,#57898,#57899,#57900,#57901,
#57902,#57903,#57904,#57905,#57906,#57907,#57908,#57909,#57910,#57911,#57912,
#57913,#57914,#57915,#57916,#57917,#57918,#57919,#57920,#57921,#57922,#57923,
#57924,#57925,#57926,#57927,#57928,#57929,#57930,#57931,#57932,#57933,#57934,
#57935,#57936,#57937,#57938,#57939,#57940,#57941,#57942,#57943,#57944,#57945,
#57946,#57947,#57948,#57949,#57950,#57951,#57952,#57953,#57954,#57955,#57956,
#57957,#57958,#57959,#57960,#57961,#57962,#57963,#57964,#57965,#57966,#57967,
#57968,#57969,#57970,#57971,#57972,#57973,#57974,#57975,#57976,#57977,#57978,
#57979,#57980,#57981,#57982,#57983,#57984,#57985,#57986,#57987,#57988,#57989,
#57990,#57991,#57992,#57993,#57994,#57995,#57996,#57997,#57998,#57999,#58000,
#58001,#58002,#58003,#58004,#58005,#58006,#58007,#58008,#58009,#58010,#58011,
#58012,#58013,#58014,#58015,#58016,#58017,#58018,#58019,#58020,#58021,#58022,
#58023,#58024,#58025,#58026,#58027,#58028,#58029,#58030,#58031,#58032,#58033,
#58034,#58035,#58036,#58037,#58038,#58039,#58040,#58041,#58042,#58043,#58044,
#58045,#58046,#58047,#58048,#58049,#58050,#58051,#58052,#58053,#58054,#58055,
#58056,#58057,#58058,#58059,#58060,#58061,#58062,#58063,#58064),
 .UNSPECIFIED.,.F.,.F.,(4,3,3,3,3,3,3,3,3,3,3,3,3,3,3,3,3,3,3,3,3,3,3,3,
3,3,3,3,3,3,3,3,3,3,3,3,3,3,3,3,3,3,3,3,3,3,3,3,3,3,3,3,3,3,3,3,3,3,3,3,
3,3,3,4),(-148.604831860765,-148.489732428586,-148.373417351629,-148.273133696763,
-148.173295902649,-148.073600655269,-147.974021123327,-147.87450514929,
-147.775022455839,-147.675542806154,-147.575967854218,-147.476347831078,
-147.376550353737,-147.2780119941,-147.17811920322,-147.078365323309,-146.978721908316,
-146.879138890514,-146.779586080743,-146.680033327426,-146.580381021796,
-146.480681212858,-146.380800683946,-146.282890291438,-146.183277645322,
-146.083808884829,-145.984303847822,-145.885015818526,-145.785761158351,
-145.68650930955,-145.586824129357,-145.487429037174,-145.387598812974,
-145.287768588775,-145.188018109967,-145.088409816086,-144.98891624613,
-144.889485587712,-144.790087436618,-144.69069142846,-144.591180292873,
-144.491640873192,-144.391921327373,-144.292646886112,-144.192900134702,
-144.093295242875,-143.993804562555,-143.894376481006,-143.794980589667,
-143.69558651951,-143.596071185495,-143.496532888165,-143.396813959209,
-143.297525183449,-143.198138538548,-143.098894126518,-142.999763678427,
-142.900695176485,-142.801657730765,-142.702620490327,-142.603485859914,
-142.504302501737,-142.404945286647,-142.321646828853),.UNSPECIFIED.);
#638=B_SPLINE_CURVE_WITH_KNOTS('',3,(#58066,#58067,#58068,#58069,#58070,
#58071,#58072,#58073,#58074,#58075,#58076,#58077,#58078,#58079,#58080,#58081,
#58082,#58083,#58084,#58085,#58086,#58087,#58088,#58089,#58090,#58091,#58092,
#58093,#58094,#58095,#58096,#58097,#58098,#58099,#58100,#58101,#58102,#58103,
#58104,#58105,#58106,#58107,#58108,#58109,#58110,#58111,#58112,#58113,#58114,
#58115,#58116,#58117,#58118,#58119,#58120,#58121,#58122,#58123,#58124,#58125,
#58126,#58127,#58128,#58129,#58130,#58131,#58132,#58133,#58134,#58135,#58136,
#58137,#58138,#58139,#58140,#58141,#58142,#58143,#58144,#58145,#58146,#58147,
#58148,#58149,#58150,#58151,#58152,#58153,#58154,#58155,#58156,#58157,#58158,
#58159,#58160,#58161,#58162,#58163,#58164,#58165,#58166,#58167,#58168,#58169,
#58170,#58171,#58172,#58173,#58174,#58175,#58176,#58177,#58178,#58179,#58180,
#58181,#58182,#58183,#58184,#58185,#58186,#58187,#58188,#58189,#58190,#58191,
#58192,#58193,#58194,#58195,#58196,#58197,#58198,#58199,#58200,#58201,#58202,
#58203,#58204,#58205,#58206,#58207,#58208,#58209,#58210,#58211,#58212,#58213,
#58214,#58215,#58216,#58217,#58218,#58219,#58220,#58221,#58222,#58223,#58224,
#58225,#58226,#58227,#58228,#58229,#58230,#58231,#58232,#58233,#58234,#58235,
#58236,#58237,#58238,#58239,#58240,#58241,#58242,#58243,#58244,#58245,#58246,
#58247,#58248,#58249,#58250,#58251,#58252,#58253,#58254,#58255,#58256,#58257,
#58258),.UNSPECIFIED.,.F.,.F.,(4,3,3,3,3,3,3,3,3,3,3,3,3,3,3,3,3,3,3,3,
3,3,3,3,3,3,3,3,3,3,3,3,3,3,3,3,3,3,3,3,3,3,3,3,3,3,3,3,3,3,3,3,3,3,3,3,
3,3,3,3,3,3,3,3,4),(-142.321646828558,-142.302403480786,-142.202670823123,
-142.103080390128,-142.003604654099,-141.904191804951,-141.804811413322,
-141.705433089642,-141.605895261762,-141.506373149337,-141.406670534806,
-141.307281778123,-141.207551294656,-141.107963019226,-141.008487651255,
-140.909076901832,-140.809698583607,-140.710322303991,-140.610781746858,
-140.511261584617,-140.411560847445,-140.312160075461,-140.212433538771,
-140.112849288359,-140.013372923913,-139.913966360139,-139.814592278875,
-139.715220281847,-139.615674804585,-139.516158993442,-139.416462614439,
-139.317038372798,-139.217309077004,-139.117722028356,-139.018246358578,
-138.918836922281,-138.819459946916,-138.720085038149,-138.620542946145,
-138.521024209718,-138.421324920405,-138.321916670135,-138.222187879593,
-138.12260133757,-138.023125541308,-137.923716611089,-137.824340140432,
-137.724965734292,-137.625423042587,-137.525904798474,-137.426205991313,
-137.326794967472,-137.227066614779,-137.127480520035,-137.028004613132,
-136.928596149847,-136.829220152506,-136.729846225434,-136.630302985278,
-136.53078522949,-136.4310869124,-136.331673264809,-136.209562139173,-136.089134680719,
-136.03846168399),.UNSPECIFIED.);
#639=B_SPLINE_CURVE_WITH_KNOTS('',3,(#58260,#58261,#58262,#58263,#58264,
#58265,#58266,#58267,#58268,#58269),.UNSPECIFIED.,.F.,.F.,(4,1,1,1,1,1,
1,4),(-136.038461521379,-135.336551562146,-134.341429859484,-133.346308156821,
-132.351186454158,-131.356064751495,-130.360943048832,-129.755276214199),
 .UNSPECIFIED.);
#640=B_SPLINE_CURVE_WITH_KNOTS('',3,(#58271,#58272,#58273,#58274,#58275,
#58276,#58277,#58278,#58279,#58280),.UNSPECIFIED.,.F.,.F.,(4,1,1,1,1,1,
1,4),(-129.755276214199,-129.365821346169,-128.370699643506,-127.375577940844,
-126.380456238181,-125.385334535518,-124.390212832855,-123.47209090702),
 .UNSPECIFIED.);
#641=B_SPLINE_CURVE_WITH_KNOTS('',3,(#58282,#58283,#58284,#58285,#58286,
#58287,#58288,#58289,#58290,#58291,#58292),.UNSPECIFIED.,.F.,.F.,(4,1,1,
1,1,1,1,1,4),(-123.47209090702,-123.395091130192,-122.399969427529,-121.404847724867,
-120.409726022204,-119.414604319541,-118.419482616878,-117.424360914215,
-117.18890559984),.UNSPECIFIED.);
#642=B_SPLINE_CURVE_WITH_KNOTS('',3,(#58294,#58295,#58296,#58297,#58298,
#58299,#58300,#58301,#58302,#58303),.UNSPECIFIED.,.F.,.F.,(4,1,1,1,1,1,
1,4),(-117.18890559984,-116.429239211552,-115.43411750889,-114.438995806227,
-113.443874103564,-112.448752400901,-111.453630698238,-110.905720292661),
 .UNSPECIFIED.);
#643=B_SPLINE_CURVE_WITH_KNOTS('',3,(#58305,#58306,#58307,#58308,#58309,
#58310,#58311,#58312,#58313,#58314),.UNSPECIFIED.,.F.,.F.,(4,1,1,1,1,1,
1,4),(-110.905720292661,-110.458508995575,-109.463387292913,-108.46826559025,
-107.473143887587,-106.478022184924,-105.482900482261,-104.622534985481),
 .UNSPECIFIED.);
#644=B_SPLINE_CURVE_WITH_KNOTS('',3,(#58316,#58317,#58318,#58319,#58320,
#58321,#58322,#58323,#58324,#58325,#58326),.UNSPECIFIED.,.F.,.F.,(4,1,1,
1,1,1,1,1,4),(-104.622534985481,-104.487778779598,-103.492657076935,-102.497535374273,
-101.50241367161,-100.507291968947,-99.5121702662841,-98.5170485636213,
-98.3393496783013),.UNSPECIFIED.);
#645=B_SPLINE_CURVE_WITH_KNOTS('',3,(#58328,#58329,#58330,#58331,#58332,
#58333,#58334,#58335,#58336,#58337,#58338,#58339,#58340,#58341,#58342,#58343,
#58344,#58345,#58346,#58347,#58348,#58349,#58350,#58351,#58352,#58353,#58354,
#58355,#58356,#58357,#58358,#58359,#58360,#58361,#58362,#58363,#58364,#58365,
#58366,#58367,#58368,#58369,#58370,#58371,#58372,#58373,#58374,#58375,#58376,
#58377,#58378,#58379,#58380,#58381,#58382,#58383,#58384,#58385,#58386,#58387,
#58388,#58389,#58390,#58391,#58392,#58393,#58394,#58395,#58396,#58397,#58398,
#58399,#58400,#58401,#58402,#58403,#58404,#58405,#58406,#58407,#58408,#58409,
#58410,#58411,#58412,#58413,#58414,#58415,#58416,#58417,#58418,#58419,#58420,
#58421,#58422,#58423,#58424,#58425,#58426,#58427,#58428,#58429,#58430,#58431,
#58432,#58433,#58434,#58435,#58436,#58437,#58438,#58439,#58440,#58441,#58442,
#58443,#58444,#58445,#58446,#58447,#58448,#58449,#58450,#58451,#58452,#58453,
#58454,#58455,#58456,#58457,#58458,#58459,#58460,#58461,#58462,#58463,#58464,
#58465,#58466,#58467,#58468,#58469,#58470,#58471,#58472,#58473,#58474,#58475,
#58476,#58477,#58478,#58479,#58480,#58481,#58482,#58483,#58484,#58485,#58486,
#58487,#58488,#58489,#58490,#58491,#58492,#58493,#58494,#58495,#58496,#58497,
#58498,#58499,#58500,#58501,#58502,#58503,#58504,#58505,#58506,#58507,#58508,
#58509,#58510,#58511,#58512,#58513,#58514,#58515,#58516,#58517,#58518,#58519,
#58520),.UNSPECIFIED.,.F.,.F.,(4,3,3,3,3,3,3,3,3,3,3,3,3,3,3,3,3,3,3,3,
3,3,3,3,3,3,3,3,3,3,3,3,3,3,3,3,3,3,3,3,3,3,3,3,3,3,3,3,3,3,3,3,3,3,3,3,
3,3,3,3,3,3,3,3,4),(-98.3393496783013,-98.2371718261334,-98.1391759064278,
-98.0412345205147,-97.9433155993773,-97.8453871071087,-97.7473580989926,
-97.649269359905,-97.5510258427676,-97.5219268609584,-97.4221982390589,
-97.3226118706745,-97.2231360316271,-97.1237272859484,-97.0243510035417,
-96.9249767891178,-96.8254338814122,-96.7259158355919,-96.6262172291419,
-96.5268051582956,-96.4270765363961,-96.3274901680115,-96.2280143289642,
-96.1286055832853,-96.0292293008786,-95.9298550864547,-95.8303121787492,
-95.7307941329288,-95.6310955264786,-95.5316834556327,-95.4319548337332,
-95.3323684653489,-95.2328926263015,-95.1334838806227,-95.034107598216,
-94.934733383792,-94.8351904760865,-94.735672430266,-94.6359738238159,-94.5365617529699,
-94.4368331310704,-94.3372467626859,-94.2377709236385,-94.1383621779598,
-94.0389858955531,-93.939611681129,-93.8400687734235,-93.7405507276031,
-93.640852121153,-93.541440050307,-93.4417114284074,-93.342125060023,-93.2426492209756,
-93.1432404752967,-93.04386419289,-92.9444899784661,-92.8449470707606,-92.7454290249403,
-92.6457304184902,-92.5463183476442,-92.4411448192608,-92.3362751483011,
-92.2315886854005,-92.1271417501303,-92.0561643714314),.UNSPECIFIED.);
#646=B_SPLINE_CURVE_WITH_KNOTS('',3,(#58522,#58523,#58524,#58525,#58526,
#58527,#58528,#58529,#58530,#58531,#58532,#58533,#58534,#58535,#58536,#58537,
#58538,#58539,#58540,#58541,#58542,#58543,#58544,#58545,#58546,#58547,#58548,
#58549,#58550,#58551,#58552,#58553,#58554,#58555,#58556,#58557,#58558,#58559,
#58560,#58561,#58562,#58563,#58564,#58565,#58566,#58567,#58568,#58569,#58570,
#58571,#58572,#58573,#58574,#58575,#58576,#58577,#58578,#58579,#58580,#58581,
#58582,#58583,#58584,#58585,#58586,#58587,#58588,#58589,#58590,#58591,#58592,
#58593,#58594,#58595,#58596,#58597,#58598,#58599,#58600,#58601,#58602,#58603,
#58604,#58605,#58606,#58607,#58608,#58609,#58610,#58611,#58612,#58613,#58614,
#58615,#58616,#58617,#58618,#58619,#58620,#58621,#58622,#58623,#58624,#58625,
#58626,#58627,#58628,#58629,#58630,#58631,#58632,#58633,#58634,#58635,#58636,
#58637,#58638,#58639,#58640,#58641,#58642,#58643,#58644,#58645,#58646,#58647,
#58648,#58649,#58650,#58651,#58652,#58653,#58654,#58655,#58656,#58657,#58658,
#58659,#58660,#58661,#58662,#58663,#58664,#58665,#58666,#58667,#58668,#58669,
#58670,#58671,#58672,#58673,#58674,#58675,#58676,#58677,#58678,#58679,#58680,
#58681,#58682,#58683,#58684,#58685,#58686,#58687,#58688,#58689,#58690,#58691,
#58692,#58693,#58694,#58695,#58696,#58697,#58698,#58699,#58700,#58701,#58702,
#58703,#58704,#58705,#58706,#58707,#58708,#58709,#58710,#58711,#58712,#58713,
#58714),.UNSPECIFIED.,.F.,.F.,(4,3,3,3,3,3,3,3,3,3,3,3,3,3,3,3,3,3,3,3,
3,3,3,3,3,3,3,3,3,3,3,3,3,3,3,3,3,3,3,3,3,3,3,3,3,3,3,3,3,3,3,3,3,3,3,3,
3,3,3,3,3,3,3,3,4),(-92.0561643711217,-91.9524176251218,-91.8484056440974,
-91.7442589618222,-91.6398339023725,-91.5511966449814,-91.4514680230817,
-91.3518816546971,-91.2524058156498,-91.1529970699709,-91.0536207875641,
-90.9542465731401,-90.8547036654347,-90.7551856196142,-90.655487013164,
-90.5560749423185,-90.4563463204189,-90.3567599520346,-90.2572841129873,
-90.1578753673086,-90.0584990849019,-89.9591248704779,-89.8595819627723,
-89.7600639169519,-89.6603653105018,-89.5609532396557,-89.4612246177562,
-89.3616382493717,-89.2621624103243,-89.1627536646456,-89.0633773822388,
-88.9640031678151,-88.8644602601095,-88.7649422142889,-88.6652436078388,
-88.5658315369928,-88.4661029150933,-88.3665165467089,-88.2670407076616,
-88.1676319619828,-88.0682556795761,-87.9688814651524,-87.8693385574468,
-87.7698205116263,-87.6701219051763,-87.57070983433,-87.4709812124306,-87.3713948440464,
-87.271919004999,-87.1725102593205,-87.073133976914,-86.9737597624899,-86.8742168547842,
-86.7746988089636,-86.6750002025136,-86.5755881316672,-86.4752619982512,
-86.3771456961652,-86.2791215528277,-86.181157433619,-86.079112841299,-85.9811338363746,
-85.8831260217789,-85.7850175359975,-85.7729790643388),.UNSPECIFIED.);
#647=B_SPLINE_CURVE_WITH_KNOTS('',3,(#58716,#58717,#58718,#58719,#58720,
#58721,#58722,#58723,#58724,#58725,#58726,#58727,#58728,#58729,#58730,#58731,
#58732,#58733,#58734,#58735,#58736,#58737,#58738,#58739,#58740,#58741,#58742,
#58743,#58744,#58745,#58746,#58747,#58748,#58749,#58750,#58751,#58752,#58753,
#58754,#58755,#58756,#58757,#58758,#58759,#58760,#58761,#58762,#58763,#58764,
#58765,#58766,#58767,#58768,#58769,#58770,#58771,#58772,#58773,#58774,#58775,
#58776,#58777,#58778,#58779,#58780,#58781,#58782,#58783,#58784,#58785,#58786,
#58787,#58788,#58789,#58790,#58791,#58792,#58793,#58794,#58795,#58796,#58797,
#58798,#58799,#58800,#58801,#58802,#58803,#58804,#58805,#58806,#58807,#58808,
#58809,#58810,#58811,#58812,#58813,#58814,#58815,#58816,#58817,#58818,#58819,
#58820,#58821,#58822,#58823,#58824,#58825,#58826,#58827,#58828,#58829,#58830,
#58831,#58832,#58833,#58834,#58835,#58836,#58837,#58838,#58839,#58840,#58841,
#58842,#58843,#58844,#58845,#58846,#58847,#58848,#58849,#58850,#58851,#58852,
#58853,#58854,#58855,#58856,#58857,#58858,#58859,#58860,#58861,#58862,#58863,
#58864,#58865,#58866,#58867,#58868,#58869,#58870,#58871,#58872,#58873,#58874,
#58875,#58876,#58877,#58878,#58879,#58880,#58881,#58882,#58883,#58884,#58885,
#58886,#58887,#58888,#58889,#58890,#58891,#58892,#58893,#58894,#58895,#58896,
#58897,#58898,#58899,#58900,#58901,#58902,#58903,#58904,#58905),
 .UNSPECIFIED.,.F.,.F.,(4,3,3,3,3,3,3,3,3,3,3,3,3,3,3,3,3,3,3,3,3,3,3,3,
3,3,3,3,3,3,3,3,3,3,3,3,3,3,3,3,3,3,3,3,3,3,3,3,3,3,3,3,3,3,3,3,3,3,3,3,
3,3,3,4),(-85.7729790639421,-85.628162953706,-85.5804664290043,-85.4807378071048,
-85.3811514387203,-85.281675599673,-85.1822668539941,-85.0828905715872,
-84.9835163571633,-84.8839734494578,-84.7844554036373,-84.6847567971871,
-84.5853447263415,-84.485616104442,-84.3860297360576,-84.2865538970102,
-84.1871451513315,-84.0877688689248,-83.9883946545009,-83.8888517467954,
-83.789333700975,-83.6896350945249,-83.5902230236786,-83.4904944017791,
-83.3909080333946,-83.2914321943472,-83.1920234486684,-83.0926471662617,
-82.9932729518379,-82.8937300441323,-82.7942119983119,-82.6945133918618,
-82.5951013210158,-82.4953726991163,-82.3957863307319,-82.2963104916845,
-82.1969017460058,-82.0975254635991,-81.9981512491754,-81.8986083414698,
-81.7990902956494,-81.6993916891993,-81.599979618353,-81.5002509964534,
-81.4006646280689,-81.3011887890216,-81.2017800433427,-81.102403760936,
-81.003029546512,-80.9034866388065,-80.8039685929861,-80.7042699865359,
-80.6048579156901,-80.5051292937906,-80.4055429254061,-80.3060670863588,
-80.20665834068,-80.1072820582732,-80.0079078438493,-79.9083649361438,-79.8088468903234,
-79.7091482838733,-79.6097362130273,-79.4897937567626),.UNSPECIFIED.);
#648=B_SPLINE_CURVE_WITH_KNOTS('',3,(#58907,#58908,#58909,#58910,#58911,
#58912,#58913,#58914,#58915,#58916,#58917,#58918,#58919,#58920,#58921,#58922,
#58923,#58924,#58925,#58926,#58927,#58928,#58929,#58930,#58931,#58932,#58933,
#58934,#58935,#58936,#58937,#58938,#58939,#58940,#58941,#58942,#58943,#58944,
#58945,#58946,#58947,#58948,#58949,#58950,#58951,#58952,#58953,#58954,#58955,
#58956,#58957,#58958,#58959,#58960,#58961,#58962,#58963,#58964,#58965,#58966,
#58967,#58968,#58969,#58970,#58971,#58972,#58973,#58974,#58975,#58976,#58977,
#58978,#58979,#58980,#58981,#58982,#58983,#58984,#58985,#58986,#58987,#58988,
#58989,#58990,#58991,#58992,#58993,#58994,#58995,#58996,#58997,#58998,#58999,
#59000,#59001,#59002,#59003,#59004,#59005,#59006,#59007,#59008,#59009,#59010,
#59011,#59012,#59013,#59014,#59015,#59016,#59017,#59018,#59019,#59020,#59021,
#59022,#59023,#59024,#59025,#59026,#59027,#59028,#59029,#59030,#59031,#59032,
#59033,#59034,#59035,#59036,#59037,#59038,#59039,#59040,#59041,#59042,#59043,
#59044,#59045,#59046,#59047,#59048,#59049,#59050,#59051,#59052,#59053,#59054,
#59055,#59056,#59057,#59058,#59059,#59060,#59061,#59062,#59063,#59064,#59065,
#59066,#59067,#59068,#59069,#59070,#59071,#59072,#59073,#59074,#59075,#59076,
#59077,#59078,#59079,#59080,#59081,#59082,#59083,#59084,#59085,#59086,#59087,
#59088,#59089,#59090,#59091,#59092,#59093,#59094,#59095,#59096),
 .UNSPECIFIED.,.F.,.F.,(4,3,3,3,3,3,3,3,3,3,3,3,3,3,3,3,3,3,3,3,3,3,3,3,
3,3,3,3,3,3,3,3,3,3,3,3,3,3,3,3,3,3,3,3,3,3,3,3,3,3,3,3,3,3,3,3,3,3,3,3,
3,3,3,4),(-79.4897937565462,-79.3915052515549,-79.2933497704462,-79.1952676454984,
-79.0972268719541,-78.9991954992728,-78.9010754287433,-78.8029128620371,
-78.7045773066325,-78.6146145103644,-78.5148858884649,-78.4152995200804,
-78.3158236810331,-78.2164149353542,-78.1170386529475,-78.0176644385236,
-77.9181215308181,-77.8186034849976,-77.7189048785475,-77.6194928077016,
-77.5197641858021,-77.4201778174178,-77.3207019783704,-77.2212932326916,
-77.121916950285,-77.0225427358611,-76.9229998281555,-76.8234817823351,
-76.723783175885,-76.6243711050388,-76.5246424831393,-76.4250561147545,
-76.3255802757072,-76.2261715300284,-76.1267952476215,-76.0274210331978,
-75.9278781254923,-75.8283600796719,-75.7286614732218,-75.6292494023759,
-75.5295207804764,-75.4299344120921,-75.3304585730447,-75.231049827366,
-75.1316735449592,-75.0322993305357,-74.93275642283,-74.8332383770095,-74.7335397705595,
-74.6341276997131,-74.5343990778136,-74.4348127094288,-74.3353368703815,
-74.2359281247027,-74.1365518422962,-74.0371776278724,-73.9376347201669,
-73.8381166743464,-73.7384180678963,-73.6390059970502,-73.530724223929,
-73.4227099506246,-73.3146592002585,-73.2066084498924),.UNSPECIFIED.);
#649=B_SPLINE_CURVE_WITH_KNOTS('',3,(#59098,#59099,#59100,#59101,#59102,
#59103,#59104,#59105,#59106,#59107,#59108,#59109,#59110,#59111,#59112,#59113,
#59114,#59115,#59116,#59117,#59118,#59119,#59120,#59121,#59122,#59123,#59124,
#59125,#59126,#59127,#59128,#59129,#59130,#59131,#59132,#59133,#59134,#59135,
#59136,#59137,#59138,#59139,#59140,#59141,#59142,#59143,#59144,#59145,#59146,
#59147,#59148,#59149,#59150,#59151,#59152,#59153,#59154,#59155,#59156,#59157,
#59158,#59159,#59160,#59161,#59162,#59163,#59164,#59165,#59166,#59167,#59168,
#59169,#59170,#59171,#59172,#59173,#59174,#59175,#59176,#59177,#59178,#59179,
#59180,#59181,#59182,#59183,#59184,#59185,#59186,#59187,#59188,#59189,#59190,
#59191,#59192,#59193,#59194,#59195,#59196,#59197,#59198,#59199,#59200,#59201,
#59202,#59203,#59204,#59205,#59206,#59207,#59208,#59209,#59210,#59211,#59212,
#59213,#59214,#59215,#59216,#59217,#59218,#59219,#59220,#59221,#59222,#59223,
#59224,#59225,#59226,#59227,#59228,#59229,#59230,#59231,#59232,#59233,#59234,
#59235,#59236,#59237,#59238,#59239,#59240,#59241,#59242,#59243,#59244,#59245,
#59246,#59247,#59248,#59249,#59250,#59251,#59252,#59253,#59254,#59255,#59256,
#59257,#59258,#59259,#59260,#59261,#59262,#59263,#59264,#59265,#59266,#59267,
#59268,#59269,#59270,#59271,#59272,#59273,#59274,#59275,#59276,#59277,#59278,
#59279,#59280,#59281,#59282,#59283,#59284,#59285,#59286,#59287,#59288,#59289,
#59290),.UNSPECIFIED.,.F.,.F.,(4,3,3,3,3,3,3,3,3,3,3,3,3,3,3,3,3,3,3,3,
3,3,3,3,3,3,3,3,3,3,3,3,3,3,3,3,3,3,3,3,3,3,3,3,3,3,3,3,3,3,3,3,3,3,3,3,
3,3,3,3,3,3,3,3,4),(-73.2066084495829,-73.1049365946532,-73.0031968130311,
-72.9012812821807,-72.7992691365912,-72.6970464527663,-72.6438842943874,
-72.5441556724878,-72.4445693041034,-72.345093465056,-72.2456847193772,
-72.1463084369706,-72.0469342225469,-71.9473913148413,-71.8478732690209,
-71.7481746625708,-71.6487625917245,-71.5490339698249,-71.4494476014406,
-71.3499717623932,-71.2505630167144,-71.1511867343078,-71.051812519884,
-70.9522696121784,-70.852751566358,-70.753052959908,-70.6536408890617,-70.5539122671622,
-70.4543258987778,-70.3548500597304,-70.2554413140517,-70.1560650316449,
-70.056690817221,-69.9571479095155,-69.8576298636952,-69.7579312572451,
-69.6585191863989,-69.5587905644993,-69.4592041961149,-69.3597283570676,
-69.2603196113887,-69.1609433289821,-69.0615691145583,-68.9620262068527,
-68.8625081610323,-68.7628095545821,-68.663397483736,-68.5636688618365,
-68.4640824934516,-68.3646066544043,-68.2651979087256,-68.1658216263188,
-68.0664474118948,-67.9669045041894,-67.8673864583689,-67.7676878519188,
-67.6682757810732,-67.5697064345155,-67.4712656835002,-67.3729215659591,
-67.2746422391412,-67.1763679415933,-67.0780985404751,-66.9797543738717,
-66.9234231424034),.UNSPECIFIED.);
#650=B_SPLINE_CURVE_WITH_KNOTS('',3,(#59292,#59293,#59294,#59295,#59296,
#59297,#59298,#59299,#59300,#59301,#59302,#59303,#59304,#59305,#59306,#59307,
#59308,#59309,#59310,#59311,#59312,#59313,#59314,#59315,#59316,#59317,#59318,
#59319,#59320,#59321,#59322,#59323,#59324,#59325,#59326,#59327,#59328,#59329,
#59330,#59331,#59332,#59333,#59334,#59335,#59336,#59337,#59338,#59339,#59340,
#59341,#59342,#59343,#59344,#59345,#59346,#59347,#59348,#59349,#59350,#59351,
#59352,#59353,#59354,#59355,#59356,#59357,#59358,#59359,#59360,#59361,#59362,
#59363,#59364,#59365,#59366,#59367,#59368,#59369,#59370,#59371,#59372,#59373,
#59374,#59375,#59376,#59377,#59378,#59379,#59380,#59381,#59382,#59383,#59384,
#59385,#59386,#59387,#59388,#59389,#59390,#59391,#59392,#59393,#59394,#59395,
#59396,#59397,#59398,#59399,#59400,#59401,#59402,#59403,#59404,#59405,#59406,
#59407,#59408,#59409,#59410,#59411,#59412,#59413,#59414,#59415,#59416,#59417,
#59418,#59419,#59420,#59421,#59422,#59423,#59424,#59425,#59426,#59427,#59428,
#59429,#59430,#59431,#59432,#59433,#59434,#59435,#59436,#59437,#59438,#59439,
#59440,#59441,#59442,#59443,#59444,#59445,#59446,#59447,#59448,#59449,#59450,
#59451,#59452,#59453,#59454,#59455,#59456,#59457,#59458,#59459,#59460,#59461,
#59462,#59463,#59464,#59465,#59466,#59467,#59468,#59469,#59470,#59471,#59472,
#59473,#59474,#59475,#59476,#59477,#59478,#59479,#59480,#59481),
 .UNSPECIFIED.,.F.,.F.,(4,3,3,3,3,3,3,3,3,3,3,3,3,3,3,3,3,3,3,3,3,3,3,3,
3,3,3,3,3,3,3,3,3,3,3,3,3,3,3,3,3,3,3,3,3,3,3,3,3,3,3,3,3,3,3,3,3,3,3,3,
3,3,3,4),(-66.923423141999,-66.7948298962433,-66.6731540784103,-66.5734254565109,
-66.4738390881268,-66.3743632490794,-66.2749545034008,-66.1755782209942,
-66.0762040065706,-65.9766610988649,-65.8771430530446,-65.7774444465947,
-65.6780323757475,-65.5783037538479,-65.4787173854634,-65.3792415464161,
-65.2798328007373,-65.1804565183305,-65.0810823039066,-64.9815393962011,
-64.8820213503807,-64.7823227439305,-64.6829106730847,-64.5831820511851,
-64.4835956828006,-64.3841198437533,-64.2847110980744,-64.1853348156677,
-64.0859606012438,-63.9864176935383,-63.8868996477178,-63.7872010412677,
-63.6877889704218,-63.5880603485223,-63.4884739801379,-63.3889981410905,
-63.2895893954118,-63.1902131130051,-63.0908388985813,-62.9912959908757,
-62.8917779450553,-62.7920793386053,-62.692667267759,-62.5929386458595,
-62.493352277475,-62.3938764384277,-62.2944676927489,-62.1950914103422,
-62.0957171959183,-61.9961742882127,-61.8966562423923,-61.7969576359422,
-61.6975455650961,-61.5978169431966,-61.4982305748122,-61.3987547357648,
-61.299345990086,-61.1999697076793,-61.1005954932555,-61.0010525855499,
-60.9015345397295,-60.8018359332794,-60.7024238624333,-60.6402378352238),
 .UNSPECIFIED.);
#651=B_SPLINE_CURVE_WITH_KNOTS('',3,(#59483,#59484,#59485,#59486,#59487,
#59488,#59489,#59490,#59491,#59492,#59493,#59494,#59495,#59496,#59497,#59498,
#59499,#59500,#59501,#59502,#59503,#59504,#59505,#59506,#59507,#59508,#59509,
#59510,#59511,#59512,#59513,#59514,#59515,#59516,#59517,#59518,#59519,#59520,
#59521,#59522,#59523,#59524,#59525,#59526,#59527,#59528,#59529,#59530,#59531,
#59532,#59533,#59534,#59535,#59536,#59537,#59538,#59539,#59540,#59541,#59542,
#59543,#59544,#59545,#59546,#59547,#59548,#59549,#59550,#59551,#59552,#59553,
#59554,#59555,#59556,#59557,#59558,#59559,#59560,#59561,#59562,#59563,#59564,
#59565,#59566,#59567,#59568,#59569,#59570,#59571,#59572,#59573,#59574,#59575,
#59576,#59577,#59578,#59579,#59580,#59581,#59582,#59583,#59584,#59585,#59586,
#59587,#59588,#59589,#59590,#59591,#59592,#59593,#59594,#59595,#59596,#59597,
#59598,#59599,#59600,#59601,#59602,#59603,#59604,#59605,#59606,#59607,#59608,
#59609,#59610,#59611,#59612,#59613,#59614,#59615,#59616,#59617,#59618,#59619,
#59620,#59621,#59622,#59623,#59624,#59625,#59626,#59627,#59628,#59629,#59630,
#59631,#59632,#59633,#59634,#59635,#59636,#59637,#59638,#59639,#59640,#59641,
#59642,#59643,#59644,#59645,#59646,#59647,#59648,#59649,#59650,#59651,#59652,
#59653,#59654,#59655,#59656,#59657,#59658,#59659,#59660,#59661,#59662,#59663,
#59664,#59665,#59666,#59667,#59668,#59669,#59670,#59671,#59672,#59673,#59674,
#59675),.UNSPECIFIED.,.F.,.F.,(4,3,3,3,3,3,3,3,3,3,3,3,3,3,3,3,3,3,3,3,
3,3,3,3,3,3,3,3,3,3,3,3,3,3,3,3,3,3,3,3,3,3,3,3,3,3,3,3,3,3,3,3,3,3,3,3,
3,3,3,3,3,3,3,3,4),(-60.6402378348566,-60.5414360827456,-60.442769991876,
-60.3442076929065,-60.2457001038484,-60.1472157017466,-60.0487229960321,
-59.9501286902306,-59.8514768227107,-59.7526634030564,-59.7073021597704,
-59.6075735378709,-59.5079871694863,-59.408511330439,-59.3091025847602,
-59.2097263023535,-59.1103520879298,-59.0108091802242,-58.9112911344038,
-58.8115925279537,-58.7121804571076,-58.6124518352081,-58.5128654668237,
-58.4133896277763,-58.3139808820975,-58.2146045996908,-58.1152303852671,
-58.0156874775615,-57.9161694317411,-57.8164708252911,-57.7170587544448,
-57.6173301325453,-57.517743764161,-57.4182679251136,-57.3188591794348,
-57.219482897028,-57.1201086826042,-57.0205657748986,-56.9210477290781,
-56.821349122628,-56.7219370517819,-56.6222084298823,-56.5226220614979,
-56.4231462224505,-56.3237374767719,-56.2243611943652,-56.1249869799411,
-56.0254440722356,-55.9259260264153,-55.8262274199651,-55.7268153491191,
-55.6270867272197,-55.5275003588357,-55.4280245197883,-55.3286157741095,
-55.2292394917031,-55.1298652772792,-55.0303223695735,-54.9308043237532,
-54.8311057173032,-54.7316936464563,-54.6190397884431,-54.5068020959542,
-54.3952724464623,-54.357052528268),.UNSPECIFIED.);
#652=B_SPLINE_CURVE_WITH_KNOTS('',3,(#59677,#59678,#59679,#59680,#59681,
#59682,#59683,#59684,#59685,#59686,#59687,#59688,#59689,#59690,#59691,#59692,
#59693,#59694,#59695,#59696,#59697,#59698,#59699,#59700,#59701,#59702,#59703,
#59704,#59705,#59706,#59707,#59708,#59709,#59710,#59711,#59712,#59713,#59714,
#59715,#59716,#59717,#59718,#59719,#59720,#59721,#59722,#59723,#59724,#59725,
#59726,#59727,#59728,#59729,#59730,#59731,#59732,#59733,#59734,#59735,#59736,
#59737,#59738,#59739,#59740,#59741,#59742,#59743,#59744,#59745,#59746,#59747,
#59748,#59749,#59750,#59751,#59752,#59753,#59754,#59755,#59756,#59757,#59758,
#59759,#59760,#59761,#59762,#59763,#59764,#59765,#59766,#59767,#59768,#59769,
#59770,#59771,#59772,#59773,#59774,#59775,#59776,#59777,#59778,#59779,#59780,
#59781,#59782,#59783,#59784,#59785,#59786,#59787,#59788,#59789,#59790,#59791,
#59792,#59793,#59794,#59795,#59796,#59797,#59798,#59799,#59800,#59801,#59802,
#59803,#59804,#59805,#59806,#59807,#59808,#59809,#59810,#59811,#59812,#59813,
#59814,#59815,#59816,#59817,#59818,#59819,#59820,#59821,#59822,#59823,#59824,
#59825,#59826,#59827,#59828,#59829,#59830,#59831,#59832,#59833,#59834,#59835,
#59836,#59837,#59838,#59839,#59840,#59841,#59842,#59843,#59844,#59845,#59846,
#59847,#59848,#59849,#59850,#59851,#59852,#59853,#59854,#59855,#59856,#59857,
#59858,#59859,#59860,#59861,#59862,#59863,#59864,#59865,#59866,#59867,#59868,
#59869),.UNSPECIFIED.,.F.,.F.,(4,3,3,3,3,3,3,3,3,3,3,3,3,3,3,3,3,3,3,3,
3,3,3,3,3,3,3,3,3,3,3,3,3,3,3,3,3,3,3,3,3,3,3,3,3,3,3,3,3,3,3,3,3,3,3,3,
3,3,3,3,3,3,3,3,4),(-54.3570525280442,-54.2569055163465,-54.1567447379845,
-54.0517015394367,-53.951357160527,-53.8509287440537,-53.7503282601737,
-53.7365719437934,-53.6368433218939,-53.5372569535095,-53.4377811144622,
-53.3383723687834,-53.2389960863768,-53.1396218719531,-53.0400789642475,
-52.9405609184271,-52.8408623119771,-52.7414502411306,-52.641721619231,
-52.5421352508463,-52.442659411799,-52.3432506661202,-52.2438743837134,
-52.1445001692895,-52.0449572615841,-51.9454392157635,-51.8457406093134,
-51.7463285384677,-51.6465999165682,-51.5470135481838,-51.4475377091365,
-51.3481289634577,-51.2487526810511,-51.1493784666272,-51.0498355589216,
-50.9503175131012,-50.8506189066511,-50.7512068358049,-50.6514782139054,
-50.5518918455211,-50.4524160064737,-50.353007260795,-50.2536309783884,
-50.1542567639646,-50.054713856259,-49.9551958104385,-49.8554972039884,
-49.7560851331421,-49.6563565112426,-49.556770142858,-49.4572943038106,
-49.3578855581318,-49.258509275725,-49.1591350613011,-49.0595921535956,
-48.960074107775,-48.8603755013249,-48.7609634304792,-48.6616990220686,
-48.5625696821931,-48.4635442241765,-48.3645802249587,-48.2656562064993,
-48.1666968095702,-48.0738672208646),.UNSPECIFIED.);
#653=B_SPLINE_CURVE_WITH_KNOTS('',3,(#59871,#59872,#59873,#59874,#59875,
#59876,#59877,#59878,#59879,#59880,#59881,#59882,#59883,#59884,#59885,#59886,
#59887,#59888,#59889,#59890,#59891,#59892,#59893,#59894,#59895,#59896,#59897,
#59898,#59899,#59900,#59901,#59902,#59903,#59904,#59905,#59906,#59907,#59908,
#59909,#59910,#59911,#59912,#59913,#59914,#59915,#59916,#59917,#59918,#59919,
#59920,#59921,#59922,#59923,#59924,#59925,#59926,#59927,#59928,#59929,#59930,
#59931,#59932,#59933,#59934,#59935,#59936,#59937,#59938,#59939,#59940,#59941,
#59942,#59943,#59944,#59945,#59946,#59947,#59948,#59949,#59950,#59951,#59952,
#59953,#59954,#59955,#59956,#59957,#59958,#59959,#59960,#59961,#59962,#59963,
#59964,#59965,#59966,#59967,#59968,#59969,#59970,#59971,#59972,#59973,#59974,
#59975,#59976,#59977,#59978,#59979,#59980,#59981,#59982,#59983,#59984,#59985,
#59986,#59987,#59988,#59989,#59990,#59991,#59992,#59993,#59994,#59995,#59996,
#59997,#59998,#59999,#60000,#60001,#60002,#60003,#60004,#60005,#60006,#60007,
#60008,#60009,#60010,#60011,#60012,#60013,#60014,#60015,#60016,#60017,#60018,
#60019,#60020,#60021,#60022,#60023,#60024,#60025,#60026,#60027,#60028,#60029,
#60030,#60031,#60032,#60033,#60034,#60035,#60036,#60037,#60038,#60039,#60040,
#60041,#60042,#60043,#60044,#60045,#60046,#60047,#60048,#60049,#60050,#60051,
#60052,#60053,#60054,#60055,#60056,#60057,#60058,#60059,#60060,#60061,#60062,
#60063),.UNSPECIFIED.,.F.,.F.,(4,3,3,3,3,3,3,3,3,3,3,3,3,3,3,3,3,3,3,3,
3,3,3,3,3,3,3,3,3,3,3,3,3,3,3,3,3,3,3,3,3,3,3,3,3,3,3,3,3,3,3,3,3,3,3,3,
3,3,3,3,3,3,3,3,4),(-48.073867220502,-47.9555291228368,-47.8357144863554,
-47.7658417278164,-47.6661131059167,-47.5665267375321,-47.4670508984848,
-47.3676421528058,-47.268265870399,-47.1688916559749,-47.0693487482695,
-46.9698307024489,-46.8701320959987,-46.7707200251535,-46.670991403254,
-46.5714050348696,-46.4719291958222,-46.3725204501435,-46.2731441677368,
-46.173769953313,-46.0742270456074,-45.974708999787,-45.8750103933369,-45.7755983224907,
-45.6758697005912,-45.5762833322068,-45.4768074931594,-45.3773987474807,
-45.2780224650739,-45.1786482506501,-45.0791053429445,-44.9795872971241,
-44.8798886906741,-44.7804766198278,-44.6807479979282,-44.5811616295438,
-44.4816857904964,-44.3822770448176,-44.2829007624109,-44.1835265479871,
-44.0839836402816,-43.9844655944611,-43.884766988011,-43.785354917165,-43.6856262952655,
-43.586039926881,-43.4865640878337,-43.3871553421549,-43.2877790597482,
-43.1884048453244,-43.0888619376189,-42.9893438917984,-42.8896452853484,
-42.7902332145022,-42.6905045926026,-42.5909182242181,-42.4914423851708,
-42.392033639492,-42.2926573570853,-42.1932831426614,-42.0937402349559,
-41.9942221891355,-41.8945235826853,-41.7951115118393,-41.790681913685),
 .UNSPECIFIED.);
#654=B_SPLINE_CURVE_WITH_KNOTS('',3,(#60065,#60066,#60067,#60068,#60069,
#60070,#60071,#60072,#60073,#60074,#60075,#60076,#60077,#60078,#60079,#60080,
#60081,#60082,#60083,#60084,#60085,#60086,#60087,#60088,#60089,#60090,#60091,
#60092,#60093,#60094,#60095,#60096,#60097,#60098,#60099,#60100,#60101,#60102,
#60103,#60104,#60105,#60106,#60107,#60108,#60109,#60110,#60111,#60112,#60113,
#60114,#60115,#60116,#60117,#60118,#60119,#60120,#60121,#60122,#60123,#60124,
#60125,#60126,#60127,#60128,#60129,#60130,#60131,#60132,#60133,#60134,#60135,
#60136,#60137,#60138,#60139,#60140,#60141,#60142,#60143,#60144,#60145,#60146,
#60147,#60148,#60149,#60150,#60151,#60152,#60153,#60154,#60155,#60156,#60157,
#60158,#60159,#60160,#60161,#60162,#60163,#60164,#60165,#60166,#60167,#60168,
#60169,#60170,#60171,#60172,#60173,#60174,#60175,#60176,#60177,#60178,#60179,
#60180,#60181,#60182,#60183,#60184,#60185,#60186,#60187,#60188,#60189,#60190,
#60191,#60192,#60193,#60194,#60195,#60196,#60197,#60198,#60199,#60200,#60201,
#60202,#60203,#60204,#60205,#60206,#60207,#60208,#60209,#60210,#60211,#60212,
#60213,#60214,#60215,#60216,#60217,#60218,#60219,#60220,#60221,#60222,#60223,
#60224,#60225,#60226,#60227,#60228,#60229,#60230,#60231,#60232,#60233,#60234,
#60235,#60236,#60237,#60238,#60239,#60240,#60241,#60242,#60243,#60244,#60245,
#60246,#60247,#60248,#60249,#60250,#60251,#60252,#60253,#60254),
 .UNSPECIFIED.,.F.,.F.,(4,3,3,3,3,3,3,3,3,3,3,3,3,3,3,3,3,3,3,3,3,3,3,3,
3,3,3,3,3,3,3,3,3,3,3,3,3,3,3,3,3,3,3,3,3,3,3,3,3,3,3,3,3,3,3,3,3,3,3,3,
3,3,3,4),(-41.7906819134384,-41.6910324087699,-41.5915250724781,-41.4921321462826,
-41.3928018135445,-41.2935035298061,-41.1942067901162,-41.0948123126013,
-40.9953709872715,-40.8957504652476,-40.7999898091765,-40.700261187277,
-40.6006748188926,-40.5011989798453,-40.4017902341665,-40.3024139517598,
-40.203039737336,-40.1034968296304,-40.0039787838099,-39.9042801773598,
-39.8048681065136,-39.705139484614,-39.6055531162297,-39.5060772771823,
-39.4066685315035,-39.3072922490968,-39.2079180346731,-39.1083751269675,
-39.0088570811471,-38.909158474697,-38.8097464038508,-38.7100177819513,
-38.6104314135668,-38.5109555745195,-38.4115468288407,-38.3121705464341,
-38.2127963320103,-38.1132534243047,-38.0137353784843,-37.9140367720343,
-37.814624701188,-37.7148960792884,-37.615309710904,-37.5158338718566,-37.4164251261779,
-37.3170488437712,-37.2176746293474,-37.1181317216418,-37.0186136758213,
-36.9189150693711,-36.8195029985251,-36.7197743766256,-36.6201880082412,
-36.5207121691938,-36.421303423515,-36.3219271411085,-36.2225529266847,
-36.1230100189791,-36.0234919731587,-35.9237933667087,-35.8243812958623,
-35.7055742237464,-35.5880755367551,-35.5074966068939),.UNSPECIFIED.);
#655=B_SPLINE_CURVE_WITH_KNOTS('',3,(#60256,#60257,#60258,#60259,#60260,
#60261,#60262,#60263,#60264,#60265,#60266,#60267,#60268,#60269,#60270,#60271,
#60272,#60273,#60274,#60275,#60276,#60277,#60278,#60279,#60280,#60281,#60282,
#60283,#60284,#60285,#60286,#60287,#60288,#60289,#60290,#60291,#60292,#60293,
#60294,#60295,#60296,#60297,#60298,#60299,#60300,#60301,#60302,#60303,#60304,
#60305,#60306,#60307,#60308,#60309,#60310,#60311,#60312,#60313,#60314,#60315,
#60316,#60317,#60318,#60319,#60320,#60321,#60322,#60323,#60324,#60325,#60326,
#60327,#60328,#60329,#60330,#60331,#60332,#60333,#60334,#60335,#60336,#60337,
#60338,#60339,#60340,#60341,#60342,#60343,#60344,#60345,#60346,#60347,#60348,
#60349,#60350,#60351,#60352,#60353,#60354,#60355,#60356,#60357,#60358,#60359,
#60360,#60361,#60362,#60363,#60364,#60365,#60366,#60367,#60368,#60369,#60370,
#60371,#60372,#60373,#60374,#60375,#60376,#60377,#60378,#60379,#60380,#60381,
#60382,#60383,#60384,#60385,#60386,#60387,#60388,#60389,#60390,#60391,#60392,
#60393,#60394,#60395,#60396,#60397,#60398,#60399,#60400,#60401,#60402,#60403,
#60404,#60405,#60406,#60407,#60408,#60409,#60410,#60411,#60412,#60413,#60414,
#60415,#60416,#60417,#60418,#60419,#60420,#60421,#60422,#60423,#60424,#60425,
#60426,#60427,#60428,#60429,#60430,#60431,#60432,#60433,#60434,#60435,#60436,
#60437,#60438,#60439,#60440,#60441,#60442,#60443,#60444,#60445,#60446,#60447,
#60448),.UNSPECIFIED.,.F.,.F.,(4,3,3,3,3,3,3,3,3,3,3,3,3,3,3,3,3,3,3,3,
3,3,3,3,3,3,3,3,3,3,3,3,3,3,3,3,3,3,3,3,3,3,3,3,3,3,3,3,3,3,3,3,3,3,3,3,
3,3,3,3,3,3,3,3,4),(-35.5074966065054,-35.4084154446817,-35.3093596833664,
-35.2102985815147,-35.1111318234569,-35.0119117474664,-34.9125107445922,
-34.8292595931994,-34.7295309712999,-34.6299446029154,-34.530468763868,
-34.4310600181895,-34.3316837357827,-34.232309521359,-34.1327666136534,
-34.033248567833,-33.933549961383,-33.8341378905366,-33.7344092686374,-33.6348229002533,
-33.5353470612059,-33.4359383155274,-33.3365620331209,-33.2371878186972,
-33.1376449109914,-33.0381268651713,-32.9384282587215,-32.8390161878738,
-32.7392875659734,-32.6397011975882,-32.540225358541,-32.4408166128614,
-32.3414403304539,-32.2420661160294,-32.1425232083248,-32.0430051625036,
-31.9433065560527,-31.8438944852109,-31.744165863312,-31.6445794949281,
-31.5451036558806,-31.4456949102025,-31.3463186277965,-31.2469444133734,
-31.1474015056671,-31.0478834598473,-30.9481848533977,-30.8487727825481,
-30.7490441606503,-30.6494577922679,-30.54998195322,-30.4505732075431,-30.3511969251383,
-30.251822710716,-30.1522798030083,-30.0527617571894,-29.953063150741,-29.8536510798852,
-29.7532833659848,-29.6530619260124,-29.5529572423997,-29.4529450306602,
-29.3529859149049,-29.2530399000807,-29.2243112993258),.UNSPECIFIED.);
#656=B_SPLINE_CURVE_WITH_KNOTS('',3,(#60450,#60451,#60452,#60453,#60454,
#60455,#60456,#60457,#60458,#60459,#60460,#60461,#60462,#60463,#60464,#60465,
#60466,#60467,#60468,#60469,#60470,#60471,#60472,#60473,#60474,#60475,#60476,
#60477,#60478,#60479,#60480,#60481,#60482,#60483,#60484,#60485,#60486,#60487,
#60488,#60489,#60490,#60491,#60492,#60493,#60494,#60495,#60496,#60497,#60498,
#60499,#60500,#60501,#60502,#60503,#60504,#60505,#60506,#60507,#60508,#60509,
#60510,#60511,#60512,#60513,#60514,#60515,#60516,#60517,#60518,#60519,#60520,
#60521,#60522,#60523,#60524,#60525,#60526,#60527,#60528,#60529,#60530,#60531,
#60532,#60533,#60534,#60535,#60536,#60537,#60538,#60539,#60540,#60541,#60542,
#60543,#60544,#60545,#60546,#60547,#60548,#60549,#60550,#60551,#60552,#60553,
#60554,#60555,#60556,#60557,#60558,#60559,#60560,#60561,#60562,#60563,#60564,
#60565,#60566,#60567,#60568,#60569,#60570,#60571,#60572,#60573,#60574,#60575,
#60576,#60577,#60578,#60579,#60580,#60581,#60582,#60583,#60584,#60585,#60586,
#60587,#60588,#60589,#60590,#60591,#60592,#60593,#60594,#60595,#60596,#60597,
#60598,#60599,#60600,#60601,#60602,#60603,#60604,#60605,#60606,#60607,#60608,
#60609,#60610,#60611,#60612,#60613,#60614,#60615,#60616,#60617,#60618,#60619,
#60620,#60621,#60622,#60623,#60624,#60625,#60626,#60627,#60628,#60629,#60630,
#60631,#60632,#60633,#60634,#60635,#60636,#60637,#60638,#60639,#60640,#60641,
#60642),.UNSPECIFIED.,.F.,.F.,(4,3,3,3,3,3,3,3,3,3,3,3,3,3,3,3,3,3,3,3,
3,3,3,3,3,3,3,3,3,3,3,3,3,3,3,3,3,3,3,3,3,3,3,3,3,3,3,3,3,3,3,3,3,3,3,3,
3,3,3,3,3,3,3,3,4),(-29.2243112990994,-29.1119176126332,-28.9989879022127,
-28.8854264210957,-28.8585293772224,-28.7588007553295,-28.6592143869515,
-28.5597385479025,-28.4603298022301,-28.3609535198297,-28.2615793054121,
-28.1620363976989,-28.0625183518846,-27.9628197454403,-27.8634076745595,
-27.76367905267,-27.6640926842956,-27.5646168452457,-27.4652080995772,-27.3658318171809,
-27.2664576027674,-27.1669146950497,-27.0673966492396,-26.9676980427998,
-26.8682859718967,-26.7685573499505,-26.6689709815193,-26.5694951424836,
-26.4700863967582,-26.370710114305,-26.2713358998348,-26.1717929921846,
-26.0722749463188,-25.9725763398244,-25.8731642692339,-25.7734356473956,
-25.6738492790722,-25.5743734400096,-25.4749646943909,-25.3755884120438,
-25.2762141976789,-25.176671289902,-25.0771532441386,-24.9774546377439,
-24.878042566571,-24.77831394472,-24.6787275763848,-24.5792517373252,-24.4798429916974,
-24.3804667093421,-24.2810924949701,-24.1815495872046,-24.0820315414365,
-23.9823329350386,-23.8829208639082,-23.7839919713175,-23.6852046011585,
-23.5865297484849,-23.4879152047942,-23.3893295469522,-23.2907413898845,
-23.1920584636559,-23.0933232402924,-22.9944290368006,-22.9411259924852),
 .UNSPECIFIED.);
#657=B_SPLINE_CURVE_WITH_KNOTS('',3,(#60644,#60645,#60646,#60647,#60648,
#60649,#60650,#60651,#60652,#60653,#60654,#60655,#60656,#60657,#60658,#60659,
#60660,#60661,#60662,#60663,#60664,#60665,#60666,#60667,#60668,#60669,#60670,
#60671,#60672,#60673,#60674,#60675,#60676,#60677,#60678,#60679,#60680,#60681,
#60682,#60683,#60684,#60685,#60686,#60687,#60688,#60689,#60690,#60691,#60692,
#60693,#60694,#60695,#60696,#60697,#60698,#60699,#60700,#60701,#60702,#60703,
#60704,#60705,#60706,#60707,#60708,#60709,#60710,#60711,#60712,#60713,#60714,
#60715,#60716,#60717,#60718,#60719,#60720,#60721,#60722,#60723,#60724,#60725,
#60726,#60727,#60728,#60729,#60730,#60731,#60732,#60733,#60734,#60735,#60736,
#60737,#60738,#60739,#60740,#60741,#60742,#60743,#60744,#60745,#60746,#60747,
#60748,#60749,#60750,#60751,#60752,#60753,#60754,#60755,#60756,#60757,#60758,
#60759,#60760,#60761,#60762,#60763,#60764,#60765,#60766,#60767,#60768,#60769,
#60770,#60771,#60772,#60773,#60774,#60775,#60776,#60777,#60778,#60779,#60780,
#60781,#60782,#60783,#60784,#60785,#60786,#60787,#60788,#60789,#60790,#60791,
#60792,#60793,#60794,#60795,#60796,#60797,#60798,#60799,#60800,#60801,#60802,
#60803,#60804,#60805,#60806,#60807,#60808,#60809,#60810,#60811,#60812,#60813,
#60814,#60815,#60816,#60817,#60818,#60819,#60820,#60821,#60822,#60823,#60824,
#60825,#60826,#60827,#60828,#60829,#60830,#60831,#60832,#60833),
 .UNSPECIFIED.,.F.,.F.,(4,3,3,3,3,3,3,3,3,3,3,3,3,3,3,3,3,3,3,3,3,3,3,3,
3,3,3,3,3,3,3,3,3,3,3,3,3,3,3,3,3,3,3,3,3,3,3,3,3,3,3,3,3,3,3,3,3,3,3,3,
3,3,3,4),(-22.9411259921462,-22.8877991612453,-22.7880705398818,-22.6884841720323,
-22.589008332851,-22.4895995877004,-22.3902233058181,-22.2908490919144,
-22.1913061835814,-22.0917881382652,-21.9920895323057,-21.8926774585825,
-21.792948836839,-21.6933624686168,-21.5938866295297,-21.4944778840265,
-21.3951016018,-21.2957273875606,-21.1961844796504,-21.0966664340231,-20.9969678277697,
-20.8975557559197,-20.7978271316268,-20.6982407608406,-20.5987649223926,
-20.4993561743092,-20.3999798895022,-20.3006056726855,-20.2010627678284,
-20.1015447196579,-20.001846110902,-19.9024340532568,-19.8027054358651,
-19.7031190719831,-19.6036432318095,-19.5042344905878,-19.4048582126111,
-19.3054840025846,-19.2059410895869,-19.1064230480395,-19.0067244457544,
-18.907312350594,-18.8075837282666,-18.7079973594981,-18.6085215205522,
-18.5091127745974,-18.4097364919555,-18.3103622773375,-18.2108193699859,
-18.1113013240723,-18.0116027175897,-17.9121906479311,-17.8124620096355,
-17.7128756247817,-17.6133997898425,-17.5139910276388,-17.4146147287232,
-17.315240497829,-17.2156976096888,-17.1161795476597,-17.0164809252863,
-16.9170689452683,-16.7875048152669,-16.6579406852656),.UNSPECIFIED.);
#658=B_SPLINE_CURVE_WITH_KNOTS('',3,(#60835,#60836,#60837,#60838,#60839,
#60840,#60841,#60842,#60843,#60844,#60845,#60846,#60847,#60848,#60849,#60850,
#60851,#60852,#60853,#60854,#60855,#60856,#60857,#60858,#60859,#60860,#60861,
#60862,#60863,#60864,#60865,#60866,#60867,#60868,#60869,#60870,#60871,#60872,
#60873,#60874,#60875,#60876,#60877,#60878,#60879,#60880,#60881,#60882,#60883,
#60884,#60885,#60886,#60887,#60888,#60889,#60890,#60891,#60892,#60893,#60894,
#60895,#60896,#60897,#60898,#60899,#60900,#60901,#60902,#60903,#60904,#60905,
#60906,#60907,#60908,#60909,#60910,#60911,#60912,#60913,#60914,#60915,#60916,
#60917,#60918,#60919,#60920,#60921,#60922,#60923,#60924,#60925,#60926,#60927,
#60928,#60929,#60930,#60931,#60932,#60933,#60934,#60935,#60936,#60937,#60938,
#60939,#60940,#60941,#60942,#60943,#60944,#60945,#60946,#60947,#60948,#60949,
#60950,#60951,#60952,#60953,#60954,#60955,#60956,#60957,#60958,#60959,#60960,
#60961,#60962,#60963,#60964,#60965,#60966,#60967,#60968,#60969,#60970,#60971,
#60972,#60973,#60974,#60975,#60976,#60977,#60978,#60979,#60980,#60981,#60982,
#60983,#60984,#60985,#60986,#60987,#60988,#60989,#60990,#60991,#60992,#60993,
#60994,#60995,#60996,#60997,#60998,#60999,#61000,#61001,#61002,#61003,#61004,
#61005,#61006,#61007,#61008,#61009,#61010,#61011,#61012,#61013,#61014,#61015,
#61016,#61017,#61018,#61019,#61020,#61021,#61022,#61023,#61024,#61025,#61026,
#61027),.UNSPECIFIED.,.F.,.F.,(4,3,3,3,3,3,3,3,3,3,3,3,3,3,3,3,3,3,3,3,
3,3,3,3,3,3,3,3,3,3,3,3,3,3,3,3,3,3,3,3,3,3,3,3,3,3,3,3,3,3,3,3,3,3,3,3,
3,3,3,3,3,3,3,3,4),(-16.6579406849666,-16.5595254138767,-16.4611656545462,
-16.3628297431378,-16.2644860491586,-16.1660406753646,-16.0675379808886,
-15.9688725793384,-15.9219472426055,-15.8222186055224,-15.722632222262,
-15.6231563869721,-15.5237476272617,-15.4243713311703,-15.324997103425,
-15.2254542125544,-15.1259361544264,-15.0262375363684,-14.9268255399426,
-14.8270968098077,-14.7275103325797,-14.6280345206672,-14.528625665478,
-14.4292492735555,-14.3298749497611,-14.2303321716408,-14.1308140179199,
-14.0311153053082,-13.9317038372798,-13.8319755046024,-13.7323894255564,
-13.6329135141889,-13.5335050560296,-13.434129059821,-13.3347551298906,
-13.2352118810722,-13.1356941127167,-13.0359957773353,-12.9365821346169,
-12.8368533112414,-12.7372667434675,-12.6377909545283,-12.5383820159022,
-12.4390055433873,-12.3396311419351,-12.2400884644398,-12.1405702409433,
-12.0408714637876,-11.9414604319541,-11.8417311293534,-11.7421440753674,
-11.6426684071079,-11.5432589690684,-11.4438819933176,-11.3445070855228,
-11.2449649964649,-11.1454462643122,-11.0457469812194,-10.9463387292913,
-10.8443976736582,-10.7426219664132,-10.6410185584271,-10.5395165541003,
-10.4380999037676,-10.3747553777871),.UNSPECIFIED.);
#659=B_SPLINE_CURVE_WITH_KNOTS('',3,(#61028,#61029,#61030,#61031,#61032,
#61033,#61034,#61035,#61036,#61037,#61038,#61039,#61040,#61041,#61042,#61043,
#61044,#61045,#61046,#61047,#61048,#61049,#61050,#61051,#61052,#61053,#61054,
#61055,#61056,#61057,#61058,#61059,#61060,#61061,#61062,#61063,#61064,#61065,
#61066,#61067,#61068,#61069,#61070,#61071,#61072,#61073,#61074,#61075,#61076,
#61077,#61078,#61079,#61080,#61081,#61082,#61083,#61084,#61085,#61086,#61087,
#61088,#61089,#61090,#61091,#61092,#61093,#61094,#61095,#61096,#61097,#61098,
#61099,#61100,#61101,#61102,#61103,#61104,#61105,#61106,#61107,#61108,#61109,
#61110,#61111,#61112,#61113,#61114,#61115,#61116,#61117,#61118,#61119,#61120,
#61121,#61122,#61123,#61124,#61125,#61126,#61127,#61128,#61129,#61130,#61131,
#61132,#61133,#61134,#61135,#61136,#61137,#61138,#61139,#61140,#61141,#61142,
#61143,#61144,#61145,#61146,#61147,#61148,#61149,#61150,#61151,#61152,#61153,
#61154,#61155,#61156,#61157,#61158,#61159,#61160,#61161,#61162,#61163,#61164,
#61165,#61166,#61167,#61168,#61169,#61170,#61171,#61172,#61173,#61174,#61175,
#61176,#61177,#61178,#61179,#61180,#61181,#61182,#61183,#61184,#61185,#61186,
#61187,#61188,#61189,#61190,#61191,#61192,#61193,#61194,#61195,#61196,#61197,
#61198,#61199,#61200,#61201,#61202,#61203,#61204,#61205,#61206,#61207,#61208,
#61209,#61210,#61211,#61212,#61213,#61214,#61215,#61216,#61217),
 .UNSPECIFIED.,.F.,.F.,(4,3,3,3,3,3,3,3,3,3,3,3,3,3,3,3,3,3,3,3,3,3,3,3,
3,3,3,3,3,3,3,3,3,3,3,3,3,3,3,3,3,3,3,3,3,3,3,3,3,3,3,3,3,3,3,3,3,3,3,3,
3,3,3,4),(-10.374755377445,-10.2666403402494,-10.1582341426202,-10.0493640278324,
-9.95121702662841,-9.85148626928268,-9.75189777905866,-9.65242247217202,
-9.55301165262249,-9.45363331890765,-9.35425707839538,-9.25471663978792,
-9.15519664952035,-9.05549616263931,-8.95609532396556,-8.85636271069546,
-8.75677231251689,-8.65729659670131,-8.55788375890536,-8.4585033697821,
-8.35912503976698,-8.25958718515092,-8.16006504486301,-8.06036238976783,
-7.96097362130273,-7.86126170701285,-7.76169207580455,-7.66221205615897,
-7.56281999731274,-7.46346034580379,-7.36410268400977,-7.2645399926673,
-7.16503814110849,-7.06535538645003,-6.96585191863989,-6.86610295137288,
-6.76649632180622,-6.66700463266673,-6.56757598469549,-6.46817996859153,
-6.3687862149989,-6.26927221524343,-6.16973530891784,-6.0700184049135,-5.97073021597704,
-5.87098078279411,-5.7713733089186,-5.67188021499968,-5.57244982385309,
-5.47305173161607,-5.37365557405361,-5.27414380886876,-5.17460373277934,
-5.07488323140633,-4.9756085133142,-4.87730205406189,-4.77908555613009,
-4.68103283919324,-4.58303928543698,-4.48507287255004,-4.3866971720644,
-4.28863976403018,-4.19010491731883,-4.09157007060747),.UNSPECIFIED.);
#660=B_SPLINE_CURVE_WITH_KNOTS('',3,(#61220,#61221,#61222,#61223,#61224,
#61225,#61226,#61227,#61228,#61229,#61230,#61231,#61232,#61233,#61234,#61235,
#61236,#61237,#61238,#61239,#61240,#61241,#61242,#61243,#61244,#61245,#61246,
#61247,#61248,#61249,#61250,#61251,#61252,#61253,#61254,#61255,#61256,#61257,
#61258,#61259,#61260,#61261,#61262,#61263,#61264,#61265,#61266,#61267,#61268,
#61269,#61270,#61271,#61272,#61273,#61274,#61275,#61276,#61277,#61278,#61279,
#61280,#61281,#61282,#61283,#61284,#61285,#61286,#61287,#61288,#61289,#61290,
#61291,#61292,#61293,#61294,#61295,#61296,#61297,#61298,#61299,#61300,#61301,
#61302,#61303,#61304,#61305,#61306,#61307,#61308,#61309,#61310,#61311,#61312,
#61313,#61314,#61315,#61316,#61317,#61318,#61319,#61320,#61321,#61322,#61323,
#61324,#61325,#61326,#61327,#61328,#61329,#61330,#61331,#61332,#61333,#61334,
#61335,#61336,#61337,#61338,#61339,#61340,#61341,#61342,#61343,#61344,#61345,
#61346,#61347,#61348,#61349,#61350,#61351,#61352,#61353,#61354,#61355,#61356,
#61357,#61358,#61359,#61360,#61361,#61362,#61363,#61364,#61365,#61366,#61367,
#61368,#61369,#61370,#61371,#61372,#61373,#61374,#61375,#61376,#61377,#61378,
#61379,#61380,#61381,#61382,#61383,#61384,#61385,#61386,#61387,#61388,#61389,
#61390,#61391,#61392,#61393,#61394,#61395,#61396,#61397,#61398,#61399,#61400,
#61401,#61402,#61403,#61404,#61405,#61406,#61407,#61408,#61409,#61410,#61411,
#61412,#61413,#61414,#61415,#61416,#61417,#61418,#61419,#61420,#61421,#61422,
#61423,#61424,#61425,#61426,#61427),.UNSPECIFIED.,.F.,.F.,(4,2,2,2,2,2,
2,2,2,2,2,2,2,2,2,2,2,2,2,2,2,2,2,2,2,2,2,2,2,2,2,2,2,2,2,2,2,2,2,2,2,2,
2,2,2,2,2,2,2,2,2,2,2,2,2,2,2,2,2,2,2,2,2,2,2,2,2,2,2,2,2,2,2,2,2,2,2,2,
2,2,2,2,2,2,2,2,2,2,2,2,2,2,2,2,2,2,2,2,2,2,2,2,2,4),(-1.21637204632693,
-1.18714290050887,-1.18252519076056,-1.1807942159484,-1.17956280411588,
-1.17823552312567,-1.17635158849732,-1.17162079875575,-1.14705039224846,
-1.14077796097892,-1.09197684086135,-1.08562311062903,-1.08220436766822,
-1.08005044700325,-1.07767787536863,-1.07436663504098,-1.06627092900157,
-1.05480887089881,-1.02102482040869,-0.988400361083974,-0.983570737553261,
-0.981615366171339,-0.98040759960187,-0.979057449006166,-0.97706100749205,
-0.971584919014512,-0.963185823572804,-0.933150358345562,-0.893530921537853,
-0.886213997454938,-0.883268847552423,-0.881096495416968,-0.878734576904006,
-0.875494868267652,-0.867849289884309,-0.857216314838179,-0.826216218525186,
-0.789262848239083,-0.784525102245509,-0.782582789002447,-0.781255367233748,
-0.779867817589057,-0.77771389121137,-0.771065412169405,-0.719245851386342,
-0.691239192782983,-0.686615884965941,-0.683684931943939,-0.681364583094547,
-0.678757827789386,-0.674367145504357,-0.656577561987564,-0.619456587063486,
-0.604213643902452,-0.587749283738322,-0.585041466858672,-0.583372101564736,
-0.582078570779847,-0.580584735903522,-0.57790246127404,-0.564608816748289,
-0.532983242490501,-0.495442277149877,-0.488137580459467,-0.485206205622946,
-0.483047363281574,-0.480703500033383,-0.477494910782589,-0.469954775086192,
-0.459493944316976,-0.429284366138851,-0.39109259755817,-0.38642283744968,
-0.384498988020802,-0.383180349796379,-0.381794201598762,-0.379639079791357,
-0.372961981016016,-0.321531606930985,-0.292543961380232,-0.287876426142365,
-0.284927377224576,-0.28259902175302,-0.279989859276483,-0.27561079366892,
-0.258079541803134,-0.223670634633327,-0.192200716316426,-0.187380329325498,
-0.185443294449896,-0.184115233500877,-0.182741261833012,-0.180638789586354,
-0.174620664136115,-0.133055970605354,-0.127524992631861,-0.0961719537331771,
-0.0914419738928427,-0.0884601980251379,-0.0861092523711643,-0.0834777457465266,
-0.0790673926692267,-0.0614849840781803,-0.00328557036190819),
 .UNSPECIFIED.);
#661=B_SPLINE_CURVE_WITH_KNOTS('',3,(#61431,#61432,#61433,#61434,#61435,
#61436,#61437,#61438,#61439,#61440,#61441,#61442,#61443,#61444,#61445,#61446,
#61447,#61448,#61449,#61450,#61451,#61452,#61453,#61454,#61455,#61456,#61457,
#61458,#61459,#61460,#61461,#61462,#61463,#61464,#61465,#61466,#61467,#61468,
#61469,#61470,#61471,#61472,#61473,#61474,#61475,#61476,#61477,#61478,#61479,
#61480,#61481,#61482,#61483,#61484,#61485,#61486,#61487,#61488,#61489,#61490,
#61491,#61492,#61493,#61494,#61495,#61496,#61497,#61498,#61499,#61500,#61501,
#61502,#61503,#61504,#61505,#61506,#61507,#61508,#61509,#61510,#61511,#61512,
#61513,#61514,#61515,#61516,#61517,#61518,#61519,#61520,#61521,#61522,#61523,
#61524,#61525,#61526,#61527,#61528,#61529,#61530,#61531,#61532,#61533,#61534,
#61535,#61536,#61537,#61538,#61539,#61540,#61541,#61542,#61543,#61544,#61545,
#61546,#61547,#61548,#61549,#61550,#61551,#61552,#61553,#61554,#61555,#61556,
#61557,#61558,#61559,#61560,#61561,#61562,#61563,#61564,#61565,#61566,#61567,
#61568,#61569,#61570,#61571,#61572),.UNSPECIFIED.,.F.,.F.,(4,3,3,3,3,3,
3,3,3,3,3,3,3,3,3,3,3,3,3,3,3,3,3,3,3,3,3,3,3,3,3,3,3,3,3,3,3,3,3,3,3,3,
3,3,3,3,3,4),(153.9380400259,154.042627859806,154.147205809574,154.251809213478,
154.35654362196,154.461356730466,154.566354309905,154.5910480186,154.696232724251,
154.801260196385,154.906163563652,155.011000480753,155.115806173648,155.220615823419,
155.325531863438,155.430507489867,155.535658420593,155.586169721263,155.691265762231,
155.796207481203,155.901029752881,156.005788504605,156.11051905473,156.215256679851,
156.320105840498,156.425017425559,156.530109315656,156.581291423926,156.685242476528,
156.789036407253,156.892712029041,156.996325266124,157.099912973806,157.203511967393,
157.307236501764,157.411029514324,157.515024345921,157.576413126589,157.684260599358,
157.795169878095,157.902660840125,158.010050857761,158.117368959288,158.22464408008,
158.331934949153,158.439234198118,158.546606884271,158.571534829252),
 .UNSPECIFIED.);
#662=B_SPLINE_CURVE_WITH_KNOTS('',3,(#61573,#61574,#61575,#61576),
 .UNSPECIFIED.,.F.,.F.,(4,4),(-2.51360796055909,-2.47288460460841),
 .UNSPECIFIED.);
#663=B_SPLINE_CURVE_WITH_KNOTS('',3,(#61581,#61582,#61583,#61584,#61585,
#61586,#61587,#61588,#61589,#61590,#61591,#61592,#61593,#61594,#61595,#61596,
#61597,#61598,#61599,#61600,#61601,#61602,#61603,#61604,#61605,#61606,#61607,
#61608,#61609,#61610,#61611,#61612,#61613,#61614,#61615,#61616,#61617,#61618,
#61619,#61620,#61621,#61622,#61623,#61624,#61625,#61626,#61627,#61628,#61629,
#61630,#61631,#61632,#61633,#61634,#61635,#61636,#61637,#61638,#61639,#61640,
#61641,#61642,#61643,#61644,#61645,#61646,#61647,#61648,#61649,#61650,#61651,
#61652,#61653,#61654,#61655,#61656,#61657,#61658,#61659,#61660,#61661,#61662,
#61663,#61664,#61665,#61666,#61667,#61668),.UNSPECIFIED.,.F.,.F.,(4,3,3,
3,3,3,3,3,3,3,3,3,3,3,3,3,3,3,3,3,3,3,3,3,3,3,3,3,3,4),(-0.45720120831918,
-0.443119064139232,-0.417479433866563,-0.404574804592397,-0.39832007975076,
-0.393505561949894,-0.368121979410151,-0.348481872316771,-0.338772362600017,
-0.332900697228815,-0.308156868840611,-0.283671164875764,-0.259896194857207,
-0.251236675637993,-0.247397000158282,-0.24318973513902,-0.219712589842507,
-0.211005365479902,-0.186944794736734,-0.163659385060356,-0.158785883220003,
-0.135404476683544,-0.112094332640347,-0.089146627335351,-0.0803319464901571,
-0.0766177528090602,-0.0541139355306132,-0.0322370316722101,-0.0106664437314021,
0.),.UNSPECIFIED.);
#664=B_SPLINE_CURVE_WITH_KNOTS('',3,(#61670,#61671,#61672,#61673),
 .UNSPECIFIED.,.F.,.F.,(4,4),(0.,0.013548856899879),.UNSPECIFIED.);
#665=B_SPLINE_CURVE_WITH_KNOTS('',3,(#61674,#61675,#61676,#61677,#61678,
#61679,#61680,#61681,#61682,#61683,#61684,#61685,#61686,#61687,#61688,#61689,
#61690,#61691,#61692,#61693,#61694,#61695,#61696,#61697,#61698,#61699,#61700,
#61701,#61702,#61703,#61704,#61705,#61706,#61707,#61708,#61709,#61710,#61711,
#61712,#61713,#61714,#61715,#61716,#61717,#61718,#61719,#61720,#61721,#61722,
#61723,#61724,#61725,#61726,#61727,#61728,#61729,#61730,#61731,#61732,#61733,
#61734,#61735,#61736,#61737,#61738,#61739,#61740,#61741,#61742,#61743,#61744,
#61745,#61746,#61747,#61748,#61749,#61750,#61751,#61752,#61753,#61754,#61755,
#61756,#61757,#61758),.UNSPECIFIED.,.F.,.F.,(4,3,3,3,3,3,3,3,3,3,3,3,3,
3,3,3,3,3,3,3,3,3,3,3,3,3,3,3,4),(-0.463803050843757,-0.448342324914894,
-0.426613591771729,-0.414011063870098,-0.409959849332504,-0.387413304468716,
-0.368330462284901,-0.359247061418826,-0.354808316317046,-0.331546268178802,
-0.307399571530292,-0.283764191523977,-0.275707032179122,-0.27179436159638,
-0.267658923961038,-0.243231654365683,-0.23495948158476,-0.211119300050522,
-0.187279118516284,-0.181503918087659,-0.157189728431955,-0.132120535354269,
-0.107051342276583,-0.0964113535606421,-0.0910152568088142,-0.0653193769800867,
-0.0396389090410066,-0.0142617177111558,0.),.UNSPECIFIED.);
#666=B_SPLINE_CURVE_WITH_KNOTS('',3,(#62376,#62377,#62378,#62379),
 .UNSPECIFIED.,.F.,.F.,(4,4),(-0.0456416910700171,0.),.UNSPECIFIED.);
#667=B_SPLINE_CURVE_WITH_KNOTS('',3,(#62381,#62382,#62383,#62384,#62385,
#62386,#62387,#62388,#62389,#62390,#62391,#62392,#62393,#62394,#62395,#62396,
#62397,#62398,#62399,#62400,#62401,#62402,#62403,#62404,#62405,#62406,#62407,
#62408,#62409,#62410,#62411,#62412,#62413,#62414,#62415,#62416,#62417,#62418,
#62419,#62420,#62421,#62422,#62423,#62424,#62425,#62426,#62427,#62428,#62429,
#62430,#62431,#62432,#62433,#62434,#62435,#62436,#62437,#62438,#62439,#62440,
#62441,#62442,#62443,#62444,#62445,#62446,#62447,#62448,#62449,#62450,#62451,
#62452,#62453,#62454,#62455,#62456,#62457,#62458,#62459,#62460,#62461,#62462,
#62463,#62464,#62465),.UNSPECIFIED.,.F.,.F.,(4,3,3,3,3,3,3,3,3,3,3,3,3,
3,3,3,3,3,3,3,3,3,3,3,3,3,3,3,4),(-0.463803050843767,-0.448342324914899,
-0.426613580872991,-0.414011043992197,-0.409959831578531,-0.387383433778229,
-0.368330439754046,-0.359247027935732,-0.354808278989149,-0.331103908693188,
-0.307399538397226,-0.283764158765723,-0.275707013541777,-0.2717942090871,
-0.267658891500947,-0.243231622613926,-0.234959481584771,-0.211363092564089,
-0.187279108106858,-0.181503921086847,-0.157189726180108,-0.13212052996401,
-0.107051333747913,-0.0964113400410272,-0.0904420396421145,-0.0646992370938577,
-0.0389224220676543,-0.0136952256569932,0.),.UNSPECIFIED.);
#668=B_SPLINE_CURVE_WITH_KNOTS('',3,(#62466,#62467,#62468,#62469),
 .UNSPECIFIED.,.F.,.F.,(4,4),(-0.0133434464393684,0.),.UNSPECIFIED.);
#669=B_SPLINE_CURVE_WITH_KNOTS('',3,(#62475,#62476,#62477,#62478,#62479,
#62480,#62481,#62482,#62483,#62484,#62485,#62486,#62487,#62488,#62489,#62490,
#62491,#62492,#62493,#62494,#62495,#62496,#62497,#62498,#62499,#62500,#62501,
#62502,#62503,#62504,#62505,#62506,#62507,#62508,#62509,#62510,#62511,#62512,
#62513,#62514,#62515,#62516,#62517,#62518,#62519,#62520,#62521,#62522,#62523,
#62524,#62525,#62526,#62527,#62528,#62529,#62530,#62531,#62532,#62533,#62534,
#62535,#62536,#62537,#62538,#62539,#62540,#62541,#62542,#62543,#62544,#62545,
#62546,#62547,#62548,#62549,#62550,#62551,#62552,#62553,#62554,#62555,#62556,
#62557,#62558,#62559,#62560,#62561,#62562),.UNSPECIFIED.,.F.,.F.,(4,3,3,
3,3,3,3,3,3,3,3,3,3,3,3,3,3,3,3,3,3,3,3,3,3,3,3,3,3,4),(-0.457201133310259,
-0.443119064139323,-0.41747943419836,-0.404574804903458,-0.398320120175313,
-0.393505569481669,-0.368121987119509,-0.348481879064538,-0.338772374950317,
-0.332900696925308,-0.308144898687338,-0.283887995601292,-0.2601352143991,
-0.251236713711485,-0.247397146482524,-0.243189764173982,-0.219712628371478,
-0.211005365479924,-0.186944796986518,-0.163659390555148,-0.158785882880634,
-0.135457646099974,-0.112205379051171,-0.0891466107339279,-0.0803319444019404,
-0.0766177517214363,-0.0541139253004491,-0.0322370044393299,-0.0106663968464944,
0.),.UNSPECIFIED.);
#670=B_SPLINE_CURVE_WITH_KNOTS('',3,(#63179,#63180,#63181,#63182),
 .UNSPECIFIED.,.F.,.F.,(4,4),(0.,0.0463476257986535),.UNSPECIFIED.);
#671=B_SPLINE_CURVE_WITH_KNOTS('',3,(#63350,#63351,#63352,#63353,#63354,
#63355,#63356,#63357,#63358,#63359,#63360,#63361,#63362,#63363,#63364,#63365,
#63366,#63367,#63368,#63369,#63370,#63371,#63372,#63373,#63374),
 .UNSPECIFIED.,.F.,.F.,(4,3,3,3,3,3,3,3,4),(13.9129741038925,14.0298422231105,
14.1472086449743,14.2651865303752,14.2961463649296,14.4010958048174,14.5059075633181,
14.6105993304191,14.6462589634952),.UNSPECIFIED.);
#672=B_SPLINE_CURVE_WITH_KNOTS('',3,(#63381,#63382,#63383,#63384,#63385,
#63386,#63387,#63388,#63389,#63390,#63391,#63392,#63393,#63394,#63395,#63396,
#63397,#63398,#63399,#63400,#63401,#63402,#63403,#63404,#63405,#63406,#63407,
#63408,#63409,#63410,#63411,#63412,#63413,#63414,#63415,#63416,#63417,#63418,
#63419,#63420,#63421,#63422,#63423,#63424,#63425,#63426,#63427,#63428,#63429,
#63430,#63431,#63432,#63433,#63434,#63435,#63436,#63437,#63438,#63439,#63440,
#63441,#63442,#63443,#63444,#63445,#63446,#63447,#63448,#63449,#63450,#63451,
#63452,#63453,#63454,#63455,#63456,#63457,#63458,#63459,#63460,#63461,#63462,
#63463,#63464,#63465,#63466,#63467,#63468,#63469,#63470,#63471,#63472,#63473,
#63474,#63475,#63476,#63477,#63478,#63479,#63480,#63481,#63482,#63483,#63484,
#63485,#63486,#63487,#63488,#63489,#63490,#63491,#63492,#63493,#63494,#63495,
#63496,#63497,#63498,#63499,#63500,#63501,#63502,#63503,#63504,#63505,#63506,
#63507,#63508,#63509,#63510,#63511,#63512,#63513,#63514,#63515,#63516,#63517,
#63518,#63519,#63520,#63521,#63522,#63523,#63524,#63525,#63526,#63527,#63528,
#63529,#63530,#63531,#63532,#63533,#63534),.UNSPECIFIED.,.F.,.F.,(4,2,2,
2,2,2,2,2,2,2,2,2,2,2,2,2,2,2,2,2,2,2,2,2,2,2,2,2,2,2,2,2,2,2,2,2,2,2,2,
2,2,2,2,2,2,2,2,2,2,2,2,2,2,2,2,2,2,2,2,2,2,2,2,2,2,2,2,2,2,2,2,2,2,2,2,
2,4),(-1.0446377710325,-1.03704628547549,-1.02453798687789,-1.01826350873426,
-1.01311579032622,-1.00702642354696,-0.995514059235476,-0.947709045396338,
-0.924297219571578,-0.919031598784486,-0.915866996576101,-0.912809965069769,
-0.908054054162346,-0.891699751850171,-0.852656081935246,-0.829130405191056,
-0.821244412043737,-0.816410755754987,-0.811111499453583,-0.803612062402073,
-0.782533692655034,-0.740280145029678,-0.723993434321385,-0.719119568461197,
-0.716342647433995,-0.713289272412789,-0.7085506531744,-0.692395375008069,
-0.654501639755035,-0.630010212765114,-0.62192770041256,-0.617060352471566,
-0.611789833475927,-0.604456364364755,-0.584839090837727,-0.549030241691706,
-0.52524011923178,-0.519962058444279,-0.516794816200759,-0.513739824324369,
-0.508994048639859,-0.492759522267891,-0.454420062653126,-0.43036810420016,
-0.422327522010767,-0.417466968026783,-0.412189851513824,-0.404820702068184,
-0.384905693225781,-0.347924053046102,-0.325585258048999,-0.320361737346843,
-0.31720570133217,-0.314140036955392,-0.309346210298665,-0.292552484015978,
-0.250772176410963,-0.229940259445161,-0.222307154400807,-0.21703582312508,
-0.211597412191101,-0.203362709041216,-0.1729171418179,-0.129868756538097,
-0.122377385415259,-0.11876359840398,-0.115846445273959,-0.112030289000885,
-0.103382003877119,-0.0905344276180329,-0.0573118511217321,-0.0312820276758043,
-0.0232232548363728,-0.0183617743957572,-0.0134528122916168,-0.00737114375286148,
-0.000589622106167569),.UNSPECIFIED.);
#673=B_SPLINE_CURVE_WITH_KNOTS('',3,(#63535,#63536,#63537,#63538,#63539,
#63540,#63541,#63542,#63543,#63544,#63545,#63546,#63547,#63548,#63549,#63550,
#63551,#63552,#63553,#63554,#63555,#63556,#63557,#63558,#63559,#63560,#63561,
#63562,#63563,#63564,#63565,#63566,#63567,#63568),.UNSPECIFIED.,.F.,.F.,
(4,3,3,3,3,3,3,3,3,3,3,4),(14.6462589634952,14.7508721781997,14.855467446032,
14.96513670233,15.0698705259915,15.1746781067958,15.2796561729127,15.2941444712241,
15.4095566049133,15.5246246005466,15.6391291191132,15.7079632676283),
 .UNSPECIFIED.);
#674=B_SPLINE_CURVE_WITH_KNOTS('',3,(#63572,#63573,#63574,#63575,#63576,
#63577,#63578,#63579,#63580,#63581,#63582,#63583,#63584,#63585,#63586,#63587,
#63588,#63589,#63590),.UNSPECIFIED.,.F.,.F.,(4,3,3,3,3,3,4),(15.1670719793089,
15.2750540414898,15.3832863567034,15.4916502992802,15.6002974383707,15.6768147086152,
15.7079632679489),.UNSPECIFIED.);
#675=B_SPLINE_CURVE_WITH_KNOTS('',3,(#63591,#63592,#63593,#63594,#63595,
#63596,#63597,#63598,#63599,#63600,#63601,#63602,#63603,#63604,#63605,#63606,
#63607,#63608,#63609,#63610,#63611,#63612,#63613,#63614,#63615,#63616,#63617,
#63618,#63619,#63620,#63621,#63622,#63623,#63624,#63625,#63626,#63627,#63628,
#63629,#63630,#63631,#63632,#63633,#63634,#63635,#63636,#63637,#63638,#63639,
#63640,#63641,#63642,#63643,#63644,#63645,#63646,#63647,#63648,#63649,#63650,
#63651,#63652,#63653,#63654,#63655,#63656,#63657,#63658,#63659,#63660,#63661,
#63662,#63663,#63664,#63665,#63666,#63667,#63668,#63669,#63670,#63671,#63672,
#63673,#63674,#63675,#63676,#63677,#63678,#63679,#63680,#63681,#63682,#63683,
#63684,#63685,#63686,#63687,#63688,#63689,#63690,#63691,#63692,#63693,#63694,
#63695,#63696,#63697,#63698,#63699,#63700,#63701,#63702,#63703,#63704,#63705,
#63706,#63707,#63708,#63709,#63710,#63711,#63712,#63713,#63714,#63715,#63716,
#63717,#63718,#63719,#63720,#63721,#63722,#63723,#63724,#63725,#63726,#63727,
#63728,#63729,#63730,#63731,#63732,#63733,#63734,#63735,#63736,#63737,#63738,
#63739,#63740,#63741,#63742,#63743,#63744,#63745,#63746,#63747,#63748,#63749,
#63750),.UNSPECIFIED.,.F.,.F.,(4,3,3,3,3,3,3,3,3,3,3,3,3,3,3,3,3,3,3,3,
3,3,3,3,3,3,3,3,3,3,3,3,3,3,3,3,3,3,3,3,3,3,3,3,3,3,3,3,3,3,3,3,3,4),(15.707963615131,
15.8124359612945,15.9200972960002,16.0242894539373,16.1284191800931,16.2325227207383,
16.3366362816606,16.4408602520689,16.545151109284,16.6496110332327,16.67372663894,
16.778864213501,16.8838480912526,16.9887133793969,17.0935156239512,17.1982900935492,
17.3030720155298,17.4079663194199,17.5129232696531,17.6180617879989,17.6706385692647,
17.7755020962003,17.8802068555822,17.9847868884979,18.0893002417826,18.1937826259329,
18.2982697066287,18.4028670126019,18.5075253033295,18.6123657467834,18.6675504995894,
18.7725356497586,18.8773635727404,18.9820684493609,19.0867076174307,19.191316598296,
19.2959308694104,19.4006553962451,19.5054411151893,19.6104079542118,19.6644624299141,
19.7694496102747,19.8742799638677,19.9789878560323,20.0836304009549,20.1882431156951,
20.2928614737947,20.3975905989735,20.502381213929,20.6073533634062,20.6613743602388,
20.7663251271889,20.8711079876035,20.9295978420031),.UNSPECIFIED.);
#676=B_SPLINE_CURVE_WITH_KNOTS('',3,(#63755,#63756,#63757,#63758,#63759,
#63760,#63761,#63762,#63763,#63764,#63765,#63766,#63767,#63768,#63769,#63770,
#63771,#63772,#63773,#63774,#63775,#63776,#63777,#63778,#63779,#63780,#63781,
#63782,#63783,#63784,#63785,#63786,#63787,#63788,#63789,#63790,#63791,#63792,
#63793,#63794,#63795,#63796,#63797,#63798,#63799,#63800,#63801,#63802,#63803,
#63804,#63805,#63806,#63807,#63808,#63809,#63810,#63811,#63812,#63813,#63814,
#63815,#63816,#63817,#63818,#63819,#63820,#63821,#63822,#63823,#63824,#63825,
#63826,#63827,#63828,#63829,#63830,#63831,#63832,#63833,#63834,#63835,#63836,
#63837,#63838,#63839,#63840,#63841,#63842,#63843,#63844,#63845,#63846,#63847,
#63848,#63849,#63850,#63851,#63852,#63853,#63854,#63855,#63856,#63857,#63858,
#63859,#63860,#63861,#63862,#63863,#63864,#63865,#63866,#63867,#63868,#63869,
#63870,#63871,#63872,#63873,#63874,#63875,#63876,#63877,#63878,#63879,#63880,
#63881,#63882,#63883,#63884,#63885,#63886,#63887,#63888,#63889,#63890,#63891,
#63892,#63893,#63894,#63895,#63896,#63897,#63898,#63899,#63900,#63901,#63902,
#63903,#63904,#63905,#63906,#63907,#63908,#63909,#63910,#63911,#63912,#63913,
#63914,#63915,#63916,#63917,#63918,#63919,#63920,#63921,#63922,#63923,#63924,
#63925,#63926,#63927,#63928,#63929,#63930),.UNSPECIFIED.,.F.,.F.,(4,2,2,
2,2,2,2,2,2,2,2,2,2,2,2,2,2,2,2,2,2,2,2,2,2,2,2,2,2,2,2,2,2,2,2,2,2,2,2,
2,2,2,2,2,2,2,2,2,2,2,2,2,2,2,2,2,2,2,2,2,2,2,2,2,2,2,2,2,2,2,2,2,2,2,2,
2,2,2,2,2,2,2,2,2,2,2,2,4),(-2.30066243309921,-2.29788522881955,-2.25643606788514,
-2.23231053948734,-2.2208999266823,-2.21483093325617,-2.2096837319818,-2.20338903083366,
-2.1911777499165,-2.14674900739685,-2.12948058846704,-2.11893355258783,
-2.11482350548001,-2.11187930309346,-2.10846627257702,-2.10219057115667,
-2.05840092364154,-2.02704354652168,-2.01876903108936,-2.01332541725472,
-2.00806430074847,-2.00047374523046,-1.98008732774641,-1.93781701131553,
-1.92094886167156,-1.9161511089752,-1.91308629977568,-1.91032182121032,
-1.90551082146163,-1.88983129230726,-1.84703778000152,-1.82586403756312,
-1.81835655060216,-1.81305734963996,-1.80758063617246,-1.79913899177679,
-1.76618947679809,-1.74118219640683,-1.72806218298243,-1.71928796613996,
-1.71545022891314,-1.71281098800718,-1.70935143126447,-1.70285538312276,
-1.67234372184617,-1.64306687837895,-1.6253960075888,-1.6183105974177,-1.61308099916133,
-1.60746915538487,-1.59835665179582,-1.55151207626044,-1.53210810751307,
-1.52429543297063,-1.51827267123986,-1.51494888437975,-1.51197840780787,
-1.50768793912509,-1.49664900107833,-1.46185758009169,-1.43502522348022,
-1.42322728284542,-1.41708470102283,-1.41193914795842,-1.40572499446052,
-1.39392685137102,-1.34085313215482,-1.32269209529888,-1.31779470287415,
-1.31470895160789,-1.31196123715408,-1.30724255800787,-1.29262423663785,
-1.25720059021258,-1.22903918551409,-1.22079248669028,-1.21535379123917,
-1.21002615087739,-1.20236320850391,-1.17967750017288,-1.12660399328951,
-1.11976116430686,-1.11627154936574,-1.11336903268774,-1.10940250060461,
-1.09982841549617,-1.08492361178958,-1.0446377710325),.UNSPECIFIED.);
#677=B_SPLINE_CURVE_WITH_KNOTS('',3,(#63932,#63933,#63934,#63935,#63936,
#63937,#63938,#63939,#63940,#63941,#63942,#63943,#63944,#63945,#63946,#63947,
#63948,#63949,#63950,#63951,#63952,#63953,#63954,#63955,#63956,#63957,#63958,
#63959,#63960,#63961,#63962),.UNSPECIFIED.,.F.,.F.,(4,3,3,3,3,3,3,3,3,3,
4),(20.9295978420031,21.034232002129,21.1388202476623,21.2433981166042,
21.3480763020097,21.4528016813787,21.5577233438514,21.6582862905635,21.78148022773,
21.9034423117292,21.9911485747748),.UNSPECIFIED.);
#678=B_SPLINE_CURVE_WITH_KNOTS('',3,(#63963,#63964,#63965,#63966,#63967,
#63968,#63969,#63970,#63971,#63972,#63973,#63974,#63975,#63976,#63977,#63978,
#63979,#63980,#63981,#63982,#63983,#63984,#63985,#63986,#63987,#63988,#63989,
#63990,#63991,#63992,#63993,#63994,#63995,#63996,#63997,#63998,#63999,#64000,
#64001,#64002,#64003,#64004,#64005,#64006,#64007,#64008,#64009,#64010,#64011,
#64012,#64013,#64014,#64015,#64016,#64017,#64018,#64019,#64020,#64021,#64022,
#64023,#64024,#64025,#64026,#64027,#64028,#64029,#64030,#64031,#64032,#64033,
#64034,#64035,#64036,#64037,#64038,#64039,#64040,#64041,#64042,#64043,#64044,
#64045,#64046,#64047,#64048,#64049,#64050,#64051,#64052,#64053,#64054,#64055,
#64056,#64057,#64058,#64059,#64060,#64061,#64062,#64063,#64064,#64065,#64066,
#64067,#64068,#64069,#64070,#64071,#64072,#64073,#64074,#64075,#64076,#64077,
#64078,#64079,#64080,#64081,#64082,#64083,#64084,#64085,#64086,#64087,#64088,
#64089,#64090,#64091,#64092,#64093,#64094,#64095,#64096,#64097,#64098,#64099,
#64100,#64101,#64102,#64103,#64104,#64105,#64106,#64107,#64108,#64109,#64110,
#64111,#64112,#64113,#64114,#64115,#64116,#64117,#64118,#64119,#64120,#64121,
#64122),.UNSPECIFIED.,.F.,.F.,(4,3,3,3,3,3,3,3,3,3,3,3,3,3,3,3,3,3,3,3,
3,3,3,3,3,3,3,3,3,3,3,3,3,3,3,3,3,3,3,3,3,3,3,3,3,3,3,3,3,3,3,3,3,4),(21.9911485751285,
22.095688555741,22.2002115015264,22.3047528752943,22.4094187078935,22.5141572541211,
22.6190804417956,22.6551982208882,22.7601694088621,22.8649834202261,22.9696745313311,
23.0743000328446,23.178895467564,23.2834963345106,23.3882077672821,23.4929805493257,
23.5979348357769,23.652110151213,23.7570778826979,23.8618883670311,23.9665758637526,
24.07119769881,24.1757894205315,24.2803865334175,24.385094175395,24.4898631401608,
24.5948136085044,24.6490220815377,24.7539919562389,24.8588046152603,24.9634943225966,
25.0681183892545,25.1727123601686,25.2773117364654,25.3820216478902,25.4867928888835,
25.591745619818,25.6459340118624,25.7509035844413,25.8557159417997,25.9604053496877,
26.0650291184504,26.1696227934869,26.27422187639,26.3789315002551,26.4837024565829,
26.5886549104258,26.6428459421871,26.7478058378387,26.8526160751731,26.9573035322347,
27.0619198861955,27.1665152309994,27.2120038885876),.UNSPECIFIED.);
#679=B_SPLINE_CURVE_WITH_KNOTS('',3,(#64128,#64129,#64130,#64131,#64132,
#64133,#64134,#64135,#64136,#64137,#64138,#64139,#64140,#64141,#64142,#64143,
#64144,#64145,#64146,#64147,#64148,#64149,#64150,#64151,#64152,#64153,#64154,
#64155,#64156,#64157,#64158,#64159,#64160,#64161,#64162,#64163,#64164,#64165,
#64166,#64167,#64168,#64169,#64170,#64171,#64172,#64173,#64174,#64175,#64176,
#64177,#64178,#64179,#64180,#64181,#64182,#64183,#64184,#64185,#64186,#64187,
#64188,#64189,#64190,#64191,#64192,#64193,#64194,#64195,#64196,#64197,#64198,
#64199,#64200,#64201,#64202,#64203,#64204,#64205,#64206,#64207,#64208,#64209,
#64210,#64211,#64212,#64213,#64214,#64215,#64216,#64217,#64218,#64219,#64220,
#64221,#64222,#64223,#64224,#64225,#64226,#64227,#64228,#64229,#64230,#64231,
#64232,#64233,#64234,#64235,#64236,#64237,#64238,#64239,#64240,#64241,#64242,
#64243,#64244,#64245,#64246,#64247,#64248,#64249,#64250,#64251,#64252,#64253,
#64254,#64255,#64256,#64257,#64258,#64259,#64260,#64261,#64262,#64263,#64264,
#64265,#64266,#64267,#64268,#64269,#64270,#64271,#64272,#64273,#64274,#64275,
#64276,#64277),.UNSPECIFIED.,.F.,.F.,(4,2,2,2,2,2,2,2,2,2,2,2,2,2,2,2,2,
2,2,2,2,2,2,2,2,2,2,2,2,2,2,2,2,2,2,2,2,2,2,2,2,2,2,2,2,2,2,2,2,2,2,2,2,
2,2,2,2,2,2,2,2,2,2,2,2,2,2,2,2,2,2,2,2,2,4),(-1.04468099360072,-1.01104765937819,
-1.00259006590934,-0.998844695782572,-0.995927263237864,-0.992305941515772,
-0.984770855439749,-0.974190770338106,-0.93945390892808,-0.911450453338721,
-0.903209196561764,-0.897770996660255,-0.892441539842163,-0.884771868974065,
-0.862024972451955,-0.810653544258749,-0.802759641619213,-0.799072772206062,
-0.796157071199431,-0.792419795704733,-0.7842410563506,-0.772376769687433,
-0.725601577139473,-0.70921626587037,-0.702832726546107,-0.697570332309719,
-0.692123839503641,-0.683841845073756,-0.652396847880456,-0.608663129143375,
-0.602366640022362,-0.598948362984966,-0.596003839861844,-0.591899157199889,
-0.581396787356787,-0.564246511806176,-0.520279466813033,-0.507514018233735,
-0.50119249911148,-0.496042267583961,-0.489991354373152,-0.47868366709079,
-0.44606513301449,-0.408796987329865,-0.402672218356862,-0.399290648278145,
-0.396336704030203,-0.392162834245318,-0.381164623297261,-0.362728953495016,
-0.313880882899363,-0.305054156032541,-0.299498434706146,-0.294240415059706,
-0.286986493010293,-0.268029948942486,-0.23686567177798,-0.209984437607884,
-0.203406725766932,-0.199929049164845,-0.197023975569625,-0.193037389752502,
-0.183335860251194,-0.168135428320574,-0.118035880101882,-0.107293205825593,
-0.10129079736115,-0.0961377416106961,-0.0897563339973962,-0.0766534350300926,
-0.0584458753898189,-0.0189947357403753,-0.00703089266578593,-0.0029658203194969,
-0.000590074059522167),.UNSPECIFIED.);
#680=B_SPLINE_CURVE_WITH_KNOTS('',3,(#64278,#64279,#64280,#64281,#64282,
#64283,#64284,#64285,#64286,#64287,#64288,#64289,#64290,#64291,#64292,#64293,
#64294,#64295,#64296,#64297,#64298,#64299,#64300,#64301,#64302,#64303,#64304,
#64305,#64306,#64307,#64308,#64309,#64310,#64311,#64312,#64313,#64314,#64315,
#64316,#64317),.UNSPECIFIED.,.F.,.F.,(4,2,2,2,2,2,2,2,2,2,2,2,2,2,2,2,2,
2,2,4),(-2.51292837387859,-2.51207339490121,-2.51041537048523,-2.50716497787441,
-2.50064795951601,-2.47306775569422,-2.44611086368794,-2.42444613760261,
-2.41688673613022,-2.41157827670629,-2.40611503543932,-2.39774151650212,
-2.36543277615857,-2.33431995757322,-2.32425922993822,-2.31699541168418,
-2.31342538340691,-2.31050531308142,-2.30670119723779,-2.30066243309921),
 .UNSPECIFIED.);
#681=B_SPLINE_CURVE_WITH_KNOTS('',3,(#64319,#64320,#64321,#64322,#64323,
#64324,#64325,#64326,#64327,#64328,#64329,#64330,#64331,#64332,#64333,#64334,
#64335,#64336,#64337,#64338,#64339,#64340,#64341,#64342,#64343,#64344,#64345,
#64346,#64347,#64348,#64349),.UNSPECIFIED.,.F.,.F.,(4,3,3,3,3,3,3,3,3,3,
4),(27.2120038885876,27.3189423845687,27.4236756493622,27.531716760937,
27.6397578725118,27.7453039754745,27.8506893660091,27.9566004950839,28.0617646729778,
28.1680492776429,28.2743338823081),.UNSPECIFIED.);
#682=B_SPLINE_CURVE_WITH_KNOTS('',3,(#64350,#64351,#64352,#64353,#64354,
#64355,#64356,#64357,#64358,#64359,#64360,#64361,#64362,#64363,#64364,#64365,
#64366,#64367,#64368,#64369,#64370,#64371,#64372,#64373,#64374,#64375,#64376,
#64377,#64378,#64379,#64380,#64381,#64382,#64383,#64384,#64385,#64386,#64387,
#64388,#64389,#64390,#64391,#64392,#64393,#64394,#64395,#64396,#64397,#64398,
#64399,#64400,#64401,#64402,#64403,#64404,#64405,#64406,#64407,#64408,#64409,
#64410,#64411,#64412,#64413,#64414,#64415,#64416,#64417,#64418,#64419,#64420,
#64421,#64422,#64423,#64424,#64425,#64426,#64427,#64428,#64429,#64430,#64431,
#64432,#64433,#64434,#64435,#64436,#64437,#64438,#64439,#64440,#64441,#64442,
#64443,#64444,#64445,#64446,#64447,#64448,#64449,#64450,#64451,#64452,#64453,
#64454,#64455,#64456,#64457,#64458,#64459,#64460,#64461,#64462,#64463,#64464,
#64465,#64466,#64467,#64468,#64469,#64470,#64471,#64472,#64473,#64474,#64475,
#64476,#64477,#64478,#64479,#64480,#64481,#64482,#64483,#64484,#64485,#64486,
#64487,#64488,#64489,#64490,#64491,#64492,#64493,#64494,#64495,#64496,#64497,
#64498,#64499,#64500,#64501,#64502,#64503,#64504,#64505,#64506),
 .UNSPECIFIED.,.F.,.F.,(4,3,3,3,3,3,3,3,3,3,3,3,3,3,3,3,3,3,3,3,3,3,3,3,
3,3,3,3,3,3,3,3,3,3,3,3,3,3,3,3,3,3,3,3,3,3,3,3,3,3,3,3,4),(28.2743338826888,
28.393063815122,28.5148668089793,28.6366698028365,28.7416392245898,28.8464514270167,
28.9511406746331,29.0557642799049,29.1603577884756,29.2649567021791,29.3696661538382,
29.4744369359963,29.5793892144469,29.6335817331613,29.7385511178593,29.8433632823423,
29.9480524908816,30.0526760563962,30.157269524589,30.2618683973533,30.3665778074985,
30.4713485477548,30.576300784142,30.630493663486,30.735463082248,30.8402752813481,
30.9449645251542,31.0495881263179,31.1541816304881,31.2587805395041,31.3634899860693,
31.4682607628949,31.5732130356956,31.6274055938107,31.7323750033433,31.8371871931352,
31.9418764275626,32.0465000193095,32.1510935140392,32.2556924136055,32.3604018507724,
32.4651726182151,32.5701248817571,32.6243175241354,32.7331396495773,32.8379273036281,
32.9426112832086,33.0472272190469,33.1518106575128,33.2564415872036,33.3611016458819,
33.4658787719657,33.4948945276705),.UNSPECIFIED.);
#683=B_SPLINE_CURVE_WITH_KNOTS('',3,(#64511,#64512,#64513,#64514,#64515,
#64516,#64517,#64518,#64519,#64520,#64521,#64522,#64523,#64524,#64525,#64526,
#64527,#64528,#64529,#64530,#64531,#64532,#64533,#64534,#64535,#64536,#64537,
#64538,#64539,#64540,#64541,#64542,#64543,#64544,#64545,#64546,#64547,#64548,
#64549,#64550,#64551,#64552,#64553,#64554,#64555,#64556,#64557,#64558,#64559,
#64560,#64561,#64562,#64563,#64564,#64565,#64566,#64567,#64568,#64569,#64570,
#64571,#64572,#64573,#64574,#64575,#64576,#64577,#64578,#64579,#64580,#64581,
#64582,#64583,#64584,#64585,#64586,#64587,#64588,#64589,#64590,#64591,#64592,
#64593,#64594,#64595,#64596,#64597,#64598,#64599,#64600,#64601,#64602,#64603,
#64604,#64605,#64606,#64607,#64608,#64609,#64610,#64611,#64612,#64613,#64614,
#64615,#64616,#64617,#64618,#64619,#64620,#64621,#64622,#64623,#64624,#64625,
#64626,#64627,#64628,#64629,#64630,#64631,#64632,#64633,#64634,#64635,#64636,
#64637,#64638,#64639,#64640,#64641,#64642,#64643,#64644,#64645,#64646,#64647,
#64648,#64649,#64650,#64651,#64652,#64653,#64654,#64655,#64656,#64657,#64658,
#64659,#64660,#64661,#64662,#64663,#64664,#64665,#64666,#64667,#64668,#64669,
#64670,#64671,#64672,#64673,#64674,#64675,#64676,#64677,#64678,#64679,#64680,
#64681,#64682,#64683,#64684,#64685,#64686,#64687,#64688,#64689,#64690,#64691,
#64692,#64693,#64694),.UNSPECIFIED.,.F.,.F.,(4,2,2,2,2,2,2,2,2,2,2,2,2,
2,2,2,2,2,2,2,2,2,2,2,2,2,2,2,2,2,2,2,2,2,2,2,2,2,2,2,2,2,2,2,2,2,2,2,2,
2,2,2,2,2,2,2,2,2,2,2,2,2,2,2,2,2,2,2,2,2,2,2,2,2,2,2,2,2,2,2,2,2,2,2,2,
2,2,2,2,2,2,4),(-2.30097243779293,-2.2982084838794,-2.29300504324686,-2.28730979449961,
-2.27779243223803,-2.23415843665506,-2.2130607051309,-2.20111173902322,
-2.19681393836065,-2.19384168655644,-2.19051969267145,-2.18450840712387,
-2.14551557849706,-2.10912812809171,-2.10067675346836,-2.09519706092268,
-2.08995769220102,-2.08366932417971,-2.06809639130763,-2.02211379568242,
-2.00912478124756,-2.00041054278591,-1.99658197821773,-1.99394296835498,
-1.99047489512536,-1.98394164174273,-1.9547577148748,-1.91401137189074,
-1.90317422854472,-1.89721522334071,-1.8920594167371,-1.88562246224264,
-1.8752837851228,-1.82979048226433,-1.81225532303406,-1.80489873878645,
-1.7991426198995,-1.79587388537908,-1.79291383950871,-1.78851338212549,
-1.77668381127525,-1.72996997801461,-1.70811713864274,-1.70053667164389,
-1.69522322247081,-1.68976305041935,-1.68141098379689,-1.64964070539387,
-1.61804960790433,-1.60791446342331,-1.60061096034024,-1.59703276096784,
-1.59411237100711,-1.59031581792478,-1.58155057719378,-1.53105887451293,
-1.5086776456401,-1.50104413206353,-1.49572127426977,-1.49027447815404,
-1.48198946467,-1.45280783481229,-1.41905664344557,-1.40369961322583,-1.39903251076247,
-1.39599345727858,-1.39280425651451,-1.38742299446439,-1.35781108261893,
-1.33324570910505,-1.3094676278794,-1.30170238600797,-1.29635536778667,
-1.29093883690591,-1.2828084729324,-1.25686005880491,-1.2339390603578,-1.20775013905048,
-1.20121672331594,-1.1977486848403,-1.19510971856197,-1.19128134342975,
-1.18256770076127,-1.16958109227768,-1.1239096827404,-1.10814925981019,
-1.10183267326071,-1.09658668681467,-1.09111748830219,-1.08271879721678,
-1.0482833648939,-1.04468099360072),.UNSPECIFIED.);
#684=B_SPLINE_CURVE_WITH_KNOTS('',3,(#64696,#64697,#64698,#64699,#64700,
#64701,#64702,#64703,#64704,#64705,#64706,#64707,#64708,#64709,#64710,#64711,
#64712,#64713,#64714,#64715,#64716,#64717,#64718,#64719,#64720,#64721,#64722,
#64723,#64724,#64725,#64726,#64727,#64728,#64729),.UNSPECIFIED.,.F.,.F.,
(4,3,3,3,3,3,3,3,3,3,3,4),(33.4948945276705,33.5998629780936,33.6212294544601,
33.7252663286542,33.8292979362022,33.9330581898076,34.0367561563849,34.140428630564,
34.2447012701825,34.3484924305647,34.4530058098014,34.5575191890381),
 .UNSPECIFIED.);
#685=B_SPLINE_CURVE_WITH_KNOTS('',3,(#64730,#64731,#64732,#64733,#64734,
#64735,#64736,#64737,#64738,#64739,#64740,#64741,#64742,#64743,#64744,#64745,
#64746,#64747,#64748,#64749,#64750,#64751,#64752,#64753,#64754,#64755,#64756,
#64757,#64758,#64759,#64760,#64761,#64762,#64763,#64764,#64765,#64766,#64767,
#64768,#64769,#64770,#64771,#64772,#64773,#64774,#64775,#64776,#64777,#64778,
#64779,#64780,#64781,#64782,#64783,#64784,#64785,#64786,#64787,#64788,#64789,
#64790,#64791,#64792,#64793,#64794,#64795,#64796,#64797,#64798,#64799,#64800,
#64801,#64802,#64803,#64804,#64805,#64806,#64807,#64808,#64809,#64810,#64811,
#64812,#64813,#64814,#64815,#64816,#64817,#64818,#64819,#64820,#64821,#64822,
#64823,#64824,#64825,#64826,#64827,#64828,#64829,#64830,#64831,#64832,#64833,
#64834,#64835,#64836,#64837,#64838,#64839,#64840,#64841,#64842,#64843,#64844,
#64845,#64846,#64847,#64848,#64849,#64850,#64851,#64852,#64853,#64854,#64855,
#64856,#64857,#64858,#64859,#64860,#64861,#64862,#64863,#64864,#64865,#64866,
#64867,#64868,#64869,#64870,#64871,#64872,#64873,#64874,#64875,#64876,#64877,
#64878,#64879,#64880,#64881,#64882,#64883,#64884,#64885,#64886,#64887,#64888,
#64889),.UNSPECIFIED.,.F.,.F.,(4,3,3,3,3,3,3,3,3,3,3,3,3,3,3,3,3,3,3,3,
3,3,3,3,3,3,3,3,3,3,3,3,3,3,3,3,3,3,3,3,3,3,3,3,3,3,3,3,3,3,3,3,3,4),(34.5575191894877,
34.6181413847848,34.72311079363,34.827922982696,34.9326122163436,35.0372358072776,
35.1418293011626,35.2464281998535,35.3511376361042,35.455908402606,35.5608606651787,
35.6150533151095,35.7200227236772,35.8248349124561,35.9295241458039,36.0341477364304,
36.1387412300007,36.24334012837,36.348049564291,36.4528203304579,36.5577725926912,
36.6119652454343,36.7169346544955,36.8217468437767,36.9264360776374,37.0310596687832,
37.1356531628781,37.2402520617767,37.3449614982305,37.449732264933,37.5546845277004,
37.608877175759,37.7138465846223,37.8186587737031,37.923348007361,38.0279715983023,
38.1325650921917,38.2371639908839,38.3418734271315,38.4466441936275,38.5515964561904,
38.6057891060837,38.7107585149317,38.8155707039964,38.9202599376368,39.02488352856,
39.1294770224305,39.2340759211033,39.3387853573303,39.4435561238053,39.5485083863464,
39.6027010364084,39.7076463034716,39.7791674689231),.UNSPECIFIED.);
#686=B_SPLINE_CURVE_WITH_KNOTS('',3,(#64895,#64896,#64897,#64898,#64899,
#64900,#64901,#64902,#64903,#64904,#64905,#64906,#64907,#64908,#64909,#64910,
#64911,#64912,#64913,#64914,#64915,#64916,#64917,#64918,#64919,#64920,#64921,
#64922,#64923,#64924,#64925,#64926,#64927,#64928,#64929,#64930,#64931,#64932,
#64933,#64934,#64935,#64936,#64937,#64938,#64939,#64940,#64941,#64942,#64943,
#64944,#64945,#64946,#64947,#64948,#64949,#64950,#64951,#64952,#64953,#64954,
#64955,#64956,#64957,#64958,#64959,#64960,#64961,#64962,#64963,#64964,#64965,
#64966,#64967,#64968,#64969,#64970,#64971,#64972,#64973,#64974,#64975,#64976,
#64977,#64978,#64979,#64980,#64981,#64982,#64983,#64984,#64985,#64986,#64987,
#64988,#64989,#64990,#64991,#64992,#64993,#64994,#64995,#64996,#64997,#64998,
#64999,#65000,#65001,#65002,#65003,#65004,#65005,#65006,#65007,#65008,#65009,
#65010,#65011,#65012,#65013,#65014,#65015,#65016,#65017,#65018,#65019,#65020,
#65021,#65022,#65023,#65024,#65025,#65026,#65027,#65028,#65029,#65030,#65031,
#65032,#65033,#65034,#65035,#65036,#65037,#65038),.UNSPECIFIED.,.F.,.F.,
(4,2,2,2,2,2,2,2,2,2,2,2,2,2,2,2,2,2,2,2,2,2,2,2,2,2,2,2,2,2,2,2,2,2,2,
2,2,2,2,2,2,2,2,2,2,2,2,2,2,2,2,2,2,2,2,2,2,2,2,2,2,2,2,2,2,2,2,2,2,2,2,
4),(-1.04476846723434,-1.02150271642865,-0.993063596993994,-0.9848039823034,
-0.979361582460874,-0.974033880152568,-0.966377200851466,-0.943772961992289,
-0.891483739472781,-0.884065891184975,-0.880465730964441,-0.877838866748591,
-0.87417164007109,-0.866388869442685,-0.855323679434048,-0.81669691676623,
-0.792924783185538,-0.784912136459898,-0.780056032336269,-0.77477431143751,
-0.767380752688617,-0.74726056802717,-0.709443651852004,-0.688096131336691,
-0.682917801108451,-0.679771349497663,-0.676698724781373,-0.671868768312631,
-0.6546184284537,-0.609649494447812,-0.591710754974352,-0.584406602933355,
-0.579139901386112,-0.573599585461145,-0.564851327222888,-0.528191572993887,
-0.490202957917336,-0.484144738453861,-0.480777245596411,-0.477818717440396,
-0.473615249035975,-0.462400607146182,-0.443384626730551,-0.395741783538845,
-0.386736941969618,-0.381144615420016,-0.375902277009579,-0.368750647334978,
-0.350603538309684,-0.319889862238882,-0.29143265093126,-0.284883531329093,
-0.281411520310055,-0.278772118211559,-0.274946507765831,-0.266254046123699,
-0.253314688736057,-0.20447525895154,-0.190468441596388,-0.183931492795003,
-0.178766680145095,-0.172873901467681,-0.162378502244032,-0.149027636898252,
-0.113059629756549,-0.0894576005504252,-0.0841843905074643,-0.0810176435442888,
-0.0779609679626385,-0.0732090866244718,-0.0569110159709185,-0.000590502373149791),
 .UNSPECIFIED.);
#687=B_SPLINE_CURVE_WITH_KNOTS('',3,(#65039,#65040,#65041,#65042,#65043,
#65044,#65045,#65046,#65047,#65048,#65049,#65050,#65051,#65052,#65053,#65054,
#65055,#65056,#65057,#65058,#65059,#65060,#65061,#65062,#65063,#65064,#65065,
#65066,#65067,#65068,#65069,#65070,#65071,#65072,#65073,#65074),
 .UNSPECIFIED.,.F.,.F.,(4,2,2,2,2,2,2,2,2,2,2,2,2,2,2,2,2,4),(-2.51338918611576,
-2.50374169630268,-2.49849421365228,-2.49362789901024,-2.48821474142374,
-2.48010299922175,-2.4532375491099,-2.42943506410213,-2.41123848858435,
-2.40033164905448,-2.39617065406752,-2.39321895615316,-2.3898316686122,
-2.38367881354038,-2.34682571576652,-2.32138694147655,-2.30510115965513,
-2.30097243779293),.UNSPECIFIED.);
#688=B_SPLINE_CURVE_WITH_KNOTS('',3,(#65076,#65077,#65078,#65079,#65080,
#65081,#65082,#65083,#65084,#65085,#65086,#65087,#65088,#65089,#65090,#65091,
#65092,#65093,#65094,#65095,#65096,#65097,#65098,#65099,#65100,#65101,#65102,
#65103,#65104,#65105,#65106),.UNSPECIFIED.,.F.,.F.,(4,3,3,3,3,3,3,3,3,3,
4),(39.7791674689231,39.8838850420608,39.9885256523606,40.0931248670507,
40.1977181979906,40.302414823731,40.4071626394716,40.5121024033064,40.5996129667331,
40.7373242033647,40.840704496397),.UNSPECIFIED.);
#689=B_SPLINE_CURVE_WITH_KNOTS('',3,(#65107,#65108,#65109,#65110,#65111,
#65112,#65113,#65114,#65115,#65116,#65117,#65118,#65119,#65120,#65121,#65122,
#65123,#65124,#65125,#65126,#65127,#65128,#65129,#65130,#65131,#65132,#65133,
#65134,#65135,#65136,#65137,#65138,#65139,#65140,#65141,#65142,#65143,#65144,
#65145,#65146,#65147,#65148,#65149,#65150,#65151,#65152,#65153,#65154,#65155,
#65156,#65157,#65158,#65159,#65160,#65161,#65162,#65163,#65164,#65165,#65166,
#65167,#65168,#65169,#65170,#65171,#65172,#65173,#65174,#65175,#65176,#65177,
#65178,#65179,#65180,#65181,#65182,#65183,#65184,#65185,#65186,#65187,#65188,
#65189,#65190,#65191,#65192,#65193,#65194,#65195,#65196,#65197,#65198,#65199,
#65200,#65201,#65202,#65203,#65204,#65205,#65206,#65207,#65208,#65209,#65210,
#65211,#65212,#65213,#65214,#65215,#65216,#65217,#65218,#65219,#65220,#65221,
#65222,#65223,#65224,#65225,#65226,#65227,#65228,#65229,#65230,#65231,#65232,
#65233,#65234,#65235,#65236,#65237,#65238,#65239,#65240,#65241,#65242,#65243,
#65244,#65245,#65246,#65247,#65248,#65249,#65250,#65251,#65252,#65253,#65254,
#65255,#65256,#65257,#65258,#65259,#65260,#65261,#65262,#65263,#65264,#65265,
#65266),.UNSPECIFIED.,.F.,.F.,(4,3,3,3,3,3,3,3,3,3,3,3,3,3,3,3,3,3,3,3,
3,3,3,3,3,3,3,3,3,3,3,3,3,3,3,3,3,3,3,3,3,3,3,3,3,3,3,3,3,3,3,3,3,4),(40.8407044966673,
40.9441437431212,41.047512994444,41.1508494291342,41.2541901753259,41.3576376869291,
41.4611485795811,41.5648311556846,41.5965248970578,41.7014943059365,41.8063064950327,
41.9109957287052,42.0156193196609,42.1202128135644,42.2248117122705,42.3295211485312,
42.4342919150401,42.5392441776152,42.5934368273825,42.6984062362677,42.8032184253704,
42.9079076590497,43.0125312500122,43.1171247439226,43.2217236426356,43.3264330789034,
43.4312038454195,43.5361561080017,43.5903487577073,43.6953181665887,43.8001303556876,
43.9048195893631,44.0094431803219,44.1140366742284,44.2186355729377,44.3233450092016,
44.4281157757136,44.533068038292,44.587260688032,44.6922300969138,44.7970422860127,
44.9017315196885,45.0063551106475,45.1109486045542,45.2155475032635,45.3202569395277,
45.42502770604,45.5299799686185,45.5841726183567,45.6891449771111,45.7939377108536,
45.8986263171477,46.0032482378794,46.0618376755064),.UNSPECIFIED.);
#690=B_SPLINE_CURVE_WITH_KNOTS('',3,(#65271,#65272,#65273,#65274,#65275,
#65276,#65277,#65278,#65279,#65280,#65281,#65282,#65283,#65284,#65285,#65286,
#65287,#65288,#65289,#65290,#65291,#65292,#65293,#65294,#65295,#65296,#65297,
#65298,#65299,#65300,#65301,#65302,#65303,#65304,#65305,#65306,#65307,#65308,
#65309,#65310,#65311,#65312,#65313,#65314,#65315,#65316,#65317,#65318,#65319,
#65320,#65321,#65322,#65323,#65324,#65325,#65326,#65327,#65328,#65329,#65330,
#65331,#65332,#65333,#65334,#65335,#65336,#65337,#65338,#65339,#65340,#65341,
#65342,#65343,#65344,#65345,#65346,#65347,#65348,#65349,#65350,#65351,#65352,
#65353,#65354,#65355,#65356,#65357,#65358,#65359,#65360,#65361,#65362,#65363,
#65364,#65365,#65366,#65367,#65368,#65369,#65370,#65371,#65372,#65373,#65374,
#65375,#65376,#65377,#65378,#65379,#65380,#65381,#65382,#65383,#65384,#65385,
#65386,#65387,#65388,#65389,#65390,#65391,#65392,#65393,#65394,#65395,#65396,
#65397,#65398,#65399,#65400,#65401,#65402,#65403,#65404,#65405,#65406,#65407,
#65408,#65409,#65410,#65411,#65412,#65413,#65414,#65415,#65416,#65417,#65418,
#65419,#65420,#65421,#65422,#65423,#65424,#65425,#65426,#65427,#65428,#65429,
#65430,#65431,#65432,#65433,#65434,#65435,#65436,#65437,#65438,#65439,#65440,
#65441,#65442,#65443,#65444,#65445,#65446,#65447,#65448,#65449,#65450,#65451,
#65452,#65453,#65454,#65455,#65456),.UNSPECIFIED.,.F.,.F.,(4,2,2,2,2,2,
2,2,2,2,2,2,2,2,2,2,2,2,2,2,2,2,2,2,2,2,2,2,2,2,2,2,2,2,2,2,2,2,2,2,2,2,
2,2,2,2,2,2,2,2,2,2,2,2,2,2,2,2,2,2,2,2,2,2,2,2,2,2,2,2,2,2,2,2,2,2,2,2,
2,2,2,2,2,2,2,2,2,2,2,2,2,2,4),(-2.30113049940868,-2.28395381723509,-2.27911355838418,
-2.27603930605954,-2.27289638060789,-2.26773249000325,-2.24671083359363,
-2.2086681222753,-2.18849926182321,-2.18110148672241,-2.17581991522202,
-2.17096603147906,-2.1629621128058,-2.13926611906222,-2.10054004779543,
-2.08423661461128,-2.07948482672064,-2.07642868911724,-2.07326293545978,
-2.06799225334365,-2.04441878173181,-1.99678704114304,-1.98529692454357,
-1.97921165659174,-1.97406354131609,-1.96778377988643,-1.95565527366273,
-1.91111370951703,-1.8938152493437,-1.88651880103419,-1.88079828986366,
-1.87753702425491,-1.87457354895486,-1.87015331940432,-1.85817511097887,
-1.82023363482106,-1.7910995737876,-1.78293960399924,-1.77751703402638,
-1.77223656446641,-1.76454562955879,-1.74334660796559,-1.70193614317224,
-1.68519457119303,-1.68040592973586,-1.6773422315343,-1.67457474782005,
-1.66975126908576,-1.65393982598308,-1.6112507192405,-1.59694130129796,
-1.58589834152536,-1.57989889439336,-1.57474596152609,-1.56836159141225,
-1.5582134364766,-1.50409687259827,-1.48583626369625,-1.48093060229145,
-1.4778424833586,-1.47509499078711,-1.47038083740912,-1.45582222708359,
-1.41192539191239,-1.39054217469516,-1.38301005123856,-1.37770475488341,
-1.3722312870301,-1.36381435924006,-1.33104009368651,-1.30617461108288,
-1.28646924331948,-1.2814668610639,-1.27835831635992,-1.2756256927715,-1.27099414663884,
-1.25725796700291,-1.22946477710496,-1.19576505927446,-1.1858831548253,
-1.18011368861761,-1.17492832734078,-1.16818419154964,-1.15288892991927,
-1.12989900952296,-1.09268773216276,-1.08419612089343,-1.08044466870857,
-1.07752652961233,-1.07390948022743,-1.06639935953652,-1.05586837319828,
-1.04476846723434),.UNSPECIFIED.);
#691=B_SPLINE_CURVE_WITH_KNOTS('',3,(#65458,#65459,#65460,#65461,#65462,
#65463,#65464,#65465,#65466,#65467,#65468,#65469,#65470,#65471,#65472,#65473,
#65474,#65475,#65476,#65477,#65478,#65479,#65480,#65481,#65482,#65483,#65484,
#65485,#65486,#65487,#65488),.UNSPECIFIED.,.F.,.F.,(4,3,3,3,3,3,3,3,3,3,
4),(46.0618376755064,46.1664298233713,46.271122390217,46.3758622586625,
46.4807982822054,46.5810845486814,46.6894780055152,46.7980809550981,46.9060565052648,
47.0149731545559,47.1238898038469),.UNSPECIFIED.);
#692=B_SPLINE_CURVE_WITH_KNOTS('',3,(#65489,#65490,#65491,#65492,#65493,
#65494,#65495,#65496,#65497,#65498,#65499,#65500,#65501,#65502,#65503,#65504,
#65505,#65506,#65507,#65508,#65509,#65510,#65511,#65512,#65513,#65514,#65515,
#65516,#65517,#65518,#65519,#65520,#65521,#65522,#65523,#65524,#65525,#65526,
#65527,#65528,#65529,#65530,#65531,#65532,#65533,#65534,#65535,#65536,#65537,
#65538,#65539,#65540,#65541,#65542,#65543,#65544,#65545,#65546,#65547,#65548,
#65549,#65550,#65551,#65552,#65553,#65554,#65555,#65556,#65557,#65558,#65559,
#65560,#65561,#65562,#65563,#65564,#65565,#65566,#65567,#65568,#65569,#65570,
#65571,#65572,#65573,#65574,#65575,#65576,#65577,#65578,#65579,#65580,#65581,
#65582,#65583,#65584,#65585,#65586,#65587,#65588,#65589,#65590,#65591,#65592,
#65593,#65594,#65595,#65596,#65597,#65598,#65599,#65600,#65601,#65602,#65603,
#65604,#65605,#65606,#65607,#65608,#65609,#65610,#65611,#65612,#65613,#65614,
#65615,#65616,#65617,#65618,#65619,#65620,#65621,#65622,#65623,#65624,#65625,
#65626,#65627,#65628,#65629,#65630,#65631,#65632,#65633,#65634,#65635,#65636,
#65637,#65638,#65639,#65640,#65641,#65642,#65643,#65644,#65645),
 .UNSPECIFIED.,.F.,.F.,(4,3,3,3,3,3,3,3,3,3,3,3,3,3,3,3,3,3,3,3,3,3,3,3,
3,3,3,3,3,3,3,3,3,3,3,3,3,3,3,3,3,3,3,3,3,3,3,3,3,3,3,3,4),(47.1238898042239,
47.2374164729195,47.3496420152373,47.4638192471217,47.5779964790061,47.6829658878876,
47.7877780769866,47.892467310662,47.9970909016209,48.1016843955274,48.2062832942367,
48.3109927305006,48.4157634970128,48.5207157595911,48.5749084093308,48.6798778182161,
48.7846900073189,48.8893792409982,48.9940028319608,49.0985963258712,49.2031952245843,
49.307904660852,49.4126754273679,49.51762768995,49.5718203396556,49.6767897485338,
49.7816019376294,49.8862911713016,49.9909147622572,50.0955082561606,50.2001071548667,
50.3048165911275,50.4095873576367,50.5145396202122,50.5687322699803,50.6737016788587,
50.7785138679544,50.8832031016266,50.9878266925821,51.0924201864853,51.1970190851913,
51.3017285214518,51.4064992879606,51.5114515505356,51.565644200305,51.6705832688796,
51.7753788717255,51.8800667792415,51.9846826335699,52.0892910010002,52.1938944136682,
52.2985747220174,52.3443673060611),.UNSPECIFIED.);
#693=B_SPLINE_CURVE_WITH_KNOTS('',3,(#65651,#65652,#65653,#65654,#65655,
#65656,#65657,#65658,#65659,#65660,#65661,#65662,#65663,#65664,#65665,#65666,
#65667,#65668,#65669,#65670,#65671,#65672,#65673,#65674,#65675,#65676,#65677,
#65678,#65679,#65680,#65681,#65682,#65683,#65684,#65685,#65686,#65687,#65688,
#65689,#65690,#65691,#65692,#65693,#65694,#65695,#65696,#65697,#65698,#65699,
#65700,#65701,#65702,#65703,#65704,#65705,#65706,#65707,#65708,#65709,#65710,
#65711,#65712,#65713,#65714,#65715,#65716,#65717,#65718,#65719,#65720,#65721,
#65722,#65723,#65724,#65725,#65726,#65727,#65728,#65729,#65730,#65731,#65732,
#65733,#65734,#65735,#65736,#65737,#65738,#65739,#65740,#65741,#65742,#65743,
#65744,#65745,#65746,#65747,#65748,#65749,#65750,#65751,#65752,#65753,#65754,
#65755,#65756,#65757,#65758,#65759,#65760,#65761,#65762,#65763,#65764,#65765,
#65766,#65767,#65768,#65769,#65770,#65771,#65772,#65773,#65774,#65775,#65776,
#65777,#65778,#65779,#65780,#65781,#65782,#65783,#65784,#65785,#65786,#65787,
#65788,#65789,#65790,#65791,#65792,#65793,#65794),.UNSPECIFIED.,.F.,.F.,
(4,2,2,2,2,2,2,2,2,2,2,2,2,2,2,2,2,2,2,2,2,2,2,2,2,2,2,2,2,2,2,2,2,2,2,
2,2,2,2,2,2,2,2,2,2,2,2,2,2,2,2,2,2,2,2,2,2,2,2,2,2,2,2,2,2,2,2,2,2,2,2,
4),(-1.04482798327345,-1.02521833172388,-0.972180197582751,-0.965310558681968,
-0.961815585981181,-0.95888580450642,-0.954908288972375,-0.945263772950211,
-0.930195614352971,-0.881098952879368,-0.870649047669339,-0.864181391520398,
-0.859023390789067,-0.853086348885525,-0.842361467695468,-0.828610786541678,
-0.790077000739879,-0.769620230500438,-0.764473565531389,-0.761334424353777,
-0.758257176819843,-0.75340224557667,-0.735817049268247,-0.688159890084346,
-0.672536397229376,-0.666240524652165,-0.660999363773463,-0.655522434708416,
-0.647085146240408,-0.611324400778314,-0.571460025601973,-0.565545794593591,
-0.56224392869706,-0.559263787029176,-0.554918443228039,-0.542583711759657,
-0.520325070808974,-0.478735874455346,-0.469032393960745,-0.463299284038973,
-0.458105845371439,-0.451291995923939,-0.43553902465202,-0.411442925616207,
-0.37200027436343,-0.366036174258641,-0.362723813758482,-0.359747569530664,
-0.355426507404534,-0.343291625879637,-0.321642007855759,-0.279020831328019,
-0.269404440677783,-0.263688778688569,-0.258490431235189,-0.251639667775339,
-0.235641944367935,-0.210937684362213,-0.172617574548671,-0.166622620027214,
-0.163269206157951,-0.160307077011138,-0.156076533213682,-0.144653888413341,
-0.125063991707449,-0.0786009326914746,-0.0694345400979581,-0.0638100911305126,
-0.0585820598898234,-0.0515195694092542,-0.043618414635837,-0.000590369335222942),
 .UNSPECIFIED.);
#694=B_SPLINE_CURVE_WITH_KNOTS('',3,(#65795,#65796,#65797,#65798,#65799,
#65800,#65801,#65802,#65803,#65804,#65805,#65806,#65807,#65808,#65809,#65810,
#65811,#65812,#65813,#65814,#65815,#65816,#65817,#65818,#65819,#65820,#65821,
#65822,#65823,#65824,#65825,#65826,#65827,#65828),.UNSPECIFIED.,.F.,.F.,
(4,2,2,2,2,2,2,2,2,2,2,2,2,2,2,2,4),(-2.51332854493083,-2.49186136662236,
-2.48284036378097,-2.47938770146182,-2.47614354600064,-2.47317215091288,
-2.46870608813633,-2.45637253479781,-2.41883687215827,-2.38979523543442,
-2.38161877317748,-2.37619320573188,-2.37091564981039,-2.36446931199275,
-2.34736277757965,-2.3013428215622,-2.30113049940868),.UNSPECIFIED.);
#695=B_SPLINE_CURVE_WITH_KNOTS('',3,(#65830,#65831,#65832,#65833,#65834,
#65835,#65836,#65837,#65838,#65839,#65840,#65841,#65842,#65843,#65844,#65845,
#65846,#65847,#65848,#65849,#65850,#65851,#65852,#65853,#65854,#65855,#65856,
#65857,#65858,#65859,#65860,#65861,#65862,#65863),.UNSPECIFIED.,.F.,.F.,
(4,3,3,3,3,3,3,3,3,3,3,4),(52.3443673060611,52.4534617183454,52.5625561306297,
52.6681209740064,52.7713623382937,52.8745054159359,52.9775877365012,53.0849595217868,
53.1880825012362,53.2912471673855,53.3945404609816,53.4070748776434),
 .UNSPECIFIED.);
#696=B_SPLINE_CURVE_WITH_KNOTS('',3,(#65864,#65865,#65866,#65867,#65868,
#65869,#65870,#65871,#65872,#65873),.UNSPECIFIED.,.F.,.F.,(4,1,1,1,1,1,
1,4),(53.4070751110264,53.5594680609544,54.5563799912791,55.5532919216039,
56.5502038519286,57.5471157822533,58.544027712578,58.6286430004606),
 .UNSPECIFIED.);
#697=B_SPLINE_CURVE_WITH_KNOTS('',3,(#65878,#65879,#65880,#65881,#65882,
#65883,#65884,#65885,#65886,#65887,#65888,#65889,#65890,#65891,#65892,#65893,
#65894,#65895,#65896,#65897,#65898,#65899,#65900,#65901,#65902,#65903,#65904,
#65905,#65906,#65907,#65908,#65909,#65910,#65911,#65912,#65913,#65914,#65915,
#65916,#65917,#65918,#65919,#65920,#65921,#65922,#65923,#65924,#65925,#65926,
#65927,#65928,#65929,#65930,#65931,#65932,#65933,#65934,#65935,#65936,#65937,
#65938,#65939,#65940,#65941,#65942,#65943,#65944,#65945,#65946,#65947,#65948,
#65949,#65950,#65951,#65952,#65953,#65954,#65955,#65956,#65957,#65958,#65959,
#65960,#65961,#65962,#65963,#65964,#65965,#65966,#65967,#65968,#65969,#65970,
#65971,#65972,#65973,#65974,#65975,#65976,#65977,#65978,#65979,#65980,#65981,
#65982,#65983,#65984,#65985,#65986,#65987,#65988,#65989,#65990,#65991,#65992,
#65993,#65994,#65995,#65996,#65997,#65998,#65999,#66000,#66001,#66002,#66003,
#66004,#66005,#66006,#66007,#66008,#66009,#66010,#66011,#66012,#66013,#66014,
#66015,#66016,#66017,#66018,#66019,#66020,#66021,#66022,#66023,#66024,#66025,
#66026,#66027,#66028,#66029,#66030,#66031,#66032,#66033,#66034,#66035,#66036,
#66037,#66038,#66039,#66040,#66041,#66042,#66043,#66044,#66045,#66046,#66047,
#66048,#66049,#66050,#66051,#66052,#66053,#66054,#66055,#66056,#66057,#66058,
#66059),.UNSPECIFIED.,.F.,.F.,(4,2,2,2,2,2,2,2,2,2,2,2,2,2,2,2,2,2,2,2,
2,2,2,2,2,2,2,2,2,2,2,2,2,2,2,2,2,2,2,2,2,2,2,2,2,2,2,2,2,2,2,2,2,2,2,2,
2,2,2,2,2,2,2,2,2,2,2,2,2,2,2,2,2,2,2,2,2,2,2,2,2,2,2,2,2,2,2,2,2,2,4),
(-2.30097507222157,-2.27184260697766,-2.26353996377759,-2.25809013588611,
-2.2528318611597,-2.24526132613213,-2.22511425467268,-2.18257822685029,
-2.16566793006745,-2.16086610611524,-2.15780008841559,-2.15464789182317,
-2.14944008827473,-2.127423792708,-2.09021166272833,-2.07024305908673,-2.0628685872235,
-2.05759110831319,-2.05273250288001,-2.04470069123103,-2.02073113458886,
-1.98229094023209,-1.9660377449484,-1.96129036166191,-1.95823515794079,
-1.9550683911771,-1.94979242052714,-1.92604329157949,-1.87857148150213,
-1.86710176762947,-1.86102065245453,-1.85587275367377,-1.84958915186538,
-1.83743951672762,-1.79292580938812,-1.77563464218439,-1.76507784620772,
-1.76096587045619,-1.7580209229682,-1.75460780473943,-1.74833367026587,
-1.7045180944078,-1.67316440965434,-1.66488865883195,-1.65944402534755,
-1.65418177731784,-1.64658933155429,-1.62619496017701,-1.58391902721668,
-1.56704778682396,-1.56224907817011,-1.5591836468353,-1.55603076680117,
-1.55081921957841,-1.52871536501292,-1.49157867342593,-1.47162925161676,
-1.46425738350926,-1.45898066026376,-1.45412200898185,-1.4460883830396,
-1.42128749281607,-1.38354035577394,-1.36740976601795,-1.36267325431155,
-1.35962043815872,-1.3564510544332,-1.35116225492438,-1.32694060534567,
-1.27933038786535,-1.26824465790243,-1.26223760085562,-1.25708619762342,
-1.25071408304169,-1.23765845465763,-1.21954412639077,-1.1972605483073,
-1.17128232626678,-1.16476013991665,-1.1612946917616,-1.15865569085706,
-1.15482462981984,-1.14609326872036,-1.13306797073562,-1.10275539929081,
-1.07457865085267,-1.06633096509937,-1.06089186133063,-1.05556399848102,
-1.04790104846741,-1.04482798327345),.UNSPECIFIED.);
#698=B_SPLINE_CURVE_WITH_KNOTS('',3,(#66061,#66062,#66063,#66064,#66065),
 .UNSPECIFIED.,.F.,.F.,(4,1,4),(58.6286430004606,59.5409396429027,59.690260418206),
 .UNSPECIFIED.);
#699=B_SPLINE_CURVE_WITH_KNOTS('',3,(#66066,#66067,#66068,#66069,#66070,
#66071,#66072,#66073,#66074,#66075,#66076,#66077,#66078,#66079,#66080,#66081,
#66082,#66083,#66084,#66085,#66086,#66087,#66088,#66089,#66090,#66091,#66092,
#66093,#66094,#66095,#66096,#66097,#66098,#66099,#66100,#66101,#66102,#66103,
#66104,#66105,#66106,#66107,#66108,#66109,#66110,#66111,#66112,#66113,#66114,
#66115,#66116,#66117,#66118,#66119,#66120,#66121,#66122,#66123,#66124,#66125,
#66126,#66127,#66128,#66129,#66130,#66131,#66132,#66133,#66134,#66135,#66136,
#66137,#66138,#66139,#66140,#66141,#66142,#66143,#66144,#66145,#66146,#66147,
#66148,#66149,#66150,#66151,#66152,#66153,#66154,#66155,#66156,#66157,#66158,
#66159,#66160,#66161,#66162,#66163,#66164,#66165,#66166,#66167,#66168,#66169,
#66170,#66171,#66172,#66173,#66174,#66175,#66176,#66177,#66178,#66179,#66180,
#66181,#66182,#66183,#66184,#66185,#66186,#66187,#66188,#66189,#66190,#66191,
#66192,#66193,#66194,#66195,#66196,#66197,#66198,#66199,#66200,#66201,#66202,
#66203,#66204,#66205,#66206,#66207,#66208,#66209,#66210,#66211,#66212,#66213,
#66214,#66215,#66216,#66217,#66218,#66219,#66220,#66221,#66222,#66223,#66224,
#66225),.UNSPECIFIED.,.F.,.F.,(4,3,3,3,3,3,3,3,3,3,3,3,3,3,3,3,3,3,3,3,
3,3,3,3,3,3,3,3,3,3,3,3,3,3,3,3,3,3,3,3,3,3,3,3,3,3,3,3,3,3,3,3,3,4),(59.6902606576805,
59.7962095221238,59.8993829629699,60.0024877467406,60.1055613221456,60.213633884916,
60.316822665245,60.4200786763603,60.5234998464774,60.5378515732274,60.6428209922896,
60.747633191622,60.8523224355587,60.9569460367901,61.0615395409651,61.166138449923,
61.2708478963356,61.3756186729547,61.4805709454672,61.5347635035521,61.6397328863229,
61.7445450493154,61.8492342570163,61.9538578220964,62.0584512902582,62.1630501633944,
62.2677595745191,62.3725303161014,62.4774825543385,62.5316754338769,62.6366448586233,
62.7414570633651,62.8461463122836,62.9507699182301,63.0553634268489,63.1599623399743,
63.2646717901123,63.3694425702111,63.4743948457886,63.5285873642016,63.6335568439146,
63.7383691043125,63.8430584096273,63.9476820723948,64.0522756381703,64.1568746087001,
64.2615841162163,64.3663549537629,64.4713072862801,64.5254992945263,64.6304386418885,
64.7352407025703,64.8399279937932,64.9116585324962),.UNSPECIFIED.);
#700=B_SPLINE_CURVE_WITH_KNOTS('',3,(#66231,#66232,#66233,#66234,#66235,
#66236,#66237,#66238,#66239,#66240,#66241,#66242,#66243,#66244,#66245,#66246,
#66247,#66248,#66249,#66250,#66251,#66252,#66253,#66254,#66255,#66256,#66257,
#66258,#66259,#66260,#66261,#66262,#66263,#66264,#66265,#66266,#66267,#66268,
#66269,#66270,#66271,#66272,#66273,#66274,#66275,#66276,#66277,#66278,#66279,
#66280,#66281,#66282,#66283,#66284,#66285,#66286,#66287,#66288,#66289,#66290,
#66291,#66292,#66293,#66294,#66295,#66296,#66297,#66298,#66299,#66300,#66301,
#66302,#66303,#66304,#66305,#66306,#66307,#66308,#66309,#66310,#66311,#66312,
#66313,#66314,#66315,#66316,#66317,#66318,#66319,#66320,#66321,#66322,#66323,
#66324,#66325,#66326,#66327,#66328,#66329,#66330,#66331,#66332,#66333,#66334,
#66335,#66336,#66337,#66338,#66339,#66340,#66341,#66342,#66343,#66344,#66345,
#66346,#66347,#66348,#66349,#66350,#66351,#66352,#66353,#66354,#66355,#66356,
#66357,#66358,#66359,#66360,#66361,#66362,#66363,#66364,#66365,#66366,#66367,
#66368,#66369,#66370,#66371,#66372,#66373,#66374,#66375,#66376,#66377,#66378,
#66379,#66380,#66381,#66382,#66383,#66384,#66385,#66386),.UNSPECIFIED.,
 .F.,.F.,(4,2,2,2,2,2,2,2,2,2,2,2,2,2,2,2,2,2,2,2,2,2,2,2,2,2,2,2,2,2,2,
2,2,2,2,2,2,2,2,2,2,2,2,2,2,2,2,2,2,2,2,2,2,2,2,2,2,2,2,2,2,2,2,2,2,2,2,
2,2,2,2,2,2,2,2,2,2,4),(-1.0443153183833,-1.04241560857417,-1.0394548464591,
-1.03573799890252,-1.02575940998438,-0.985758233817047,-0.961530523588478,
-0.95044472515653,-0.944458888694553,-0.939338584144273,-0.933023557475811,
-0.920170517525391,-0.902449044652388,-0.879473401761167,-0.85317485771094,
-0.846642782846574,-0.843188930944256,-0.840558470026248,-0.836748755654842,
-0.828146795396558,-0.815399212184051,-0.784406536744733,-0.756372102721844,
-0.74811987714739,-0.742673020800209,-0.737333483659212,-0.729645160127398,
-0.706758666737787,-0.681449487439988,-0.651722825886203,-0.64633127489472,
-0.643134028096896,-0.640089234738094,-0.635407192783891,-0.619916882197167,
-0.585517378644701,-0.557162184660311,-0.548905638304376,-0.543462612770092,
-0.538132194462761,-0.530467720558331,-0.50780144694809,-0.455014727323234,
-0.447940332893434,-0.44440530065395,-0.441481491866233,-0.437563651611919,
-0.428293602569473,-0.414082015187736,-0.378681545778949,-0.356479105908006,
-0.348711529911623,-0.343900157725863,-0.338585881880242,-0.330987466576925,
-0.308939408673464,-0.260987826958697,-0.250204724788896,-0.245955618970417,
-0.242991898655694,-0.239648765074693,-0.233537456253398,-0.225573648682296,
-0.205527386453999,-0.159895301639851,-0.150640824855572,-0.144997536919566,
-0.139774523257218,-0.132753490577631,-0.115716129881903,-0.0881644406393426,
-0.0548872374637813,-0.0484954929886149,-0.0450561579917568,-0.0421151848914067,
-0.0380438672445768,-0.0333678775887178,-0.000612794912691296),
 .UNSPECIFIED.);
#701=B_SPLINE_CURVE_WITH_KNOTS('',3,(#66387,#66388,#66389,#66390,#66391,
#66392,#66393,#66394,#66395,#66396,#66397,#66398,#66399,#66400,#66401,#66402,
#66403,#66404,#66405,#66406,#66407,#66408,#66409,#66410,#66411,#66412,#66413,
#66414,#66415,#66416,#66417,#66418),.UNSPECIFIED.,.F.,.F.,(4,2,2,2,2,2,
2,2,2,2,2,2,2,2,2,4),(-2.5135235169571,-2.48279461776556,-2.47022321311333,
-2.46246766610601,-2.45712250133492,-2.4517039407824,-2.44356287286976,
-2.41745455136848,-2.37196574750479,-2.3630699199823,-2.35921139583419,
-2.35656923776549,-2.35312238275445,-2.34668904599171,-2.30378846763817,
-2.30097507222157),.UNSPECIFIED.);
#702=B_SPLINE_CURVE_WITH_KNOTS('',3,(#66420,#66421,#66422,#66423,#66424,
#66425,#66426,#66427,#66428,#66429,#66430,#66431,#66432,#66433,#66434,#66435,
#66436,#66437,#66438,#66439,#66440,#66441,#66442,#66443,#66444,#66445,#66446,
#66447,#66448,#66449,#66450),.UNSPECIFIED.,.F.,.F.,(4,3,3,3,3,3,3,3,3,3,
4),(64.9116585324962,65.0162574550017,65.1208506087689,65.2255471356105,
65.3302949562089,65.4352346208628,65.522411224851,65.6352598287414,65.7478409063075,
65.8606433156557,65.973445725004),.UNSPECIFIED.);
#703=B_SPLINE_CURVE_WITH_KNOTS('',3,(#66451,#66452,#66453,#66454,#66455,
#66456,#66457,#66458,#66459,#66460,#66461,#66462,#66463,#66464,#66465,#66466,
#66467,#66468,#66469,#66470,#66471,#66472,#66473,#66474,#66475,#66476,#66477,
#66478,#66479,#66480,#66481,#66482,#66483,#66484,#66485,#66486,#66487,#66488,
#66489,#66490,#66491,#66492,#66493,#66494,#66495,#66496,#66497,#66498,#66499,
#66500,#66501,#66502,#66503,#66504,#66505,#66506,#66507,#66508,#66509,#66510,
#66511,#66512,#66513,#66514,#66515,#66516,#66517,#66518,#66519,#66520,#66521,
#66522,#66523,#66524,#66525,#66526,#66527,#66528,#66529,#66530,#66531,#66532,
#66533,#66534,#66535,#66536,#66537,#66538,#66539,#66540,#66541,#66542,#66543,
#66544,#66545,#66546,#66547,#66548,#66549,#66550,#66551,#66552,#66553,#66554,
#66555,#66556,#66557,#66558,#66559,#66560,#66561,#66562,#66563,#66564,#66565,
#66566,#66567,#66568,#66569,#66570,#66571,#66572,#66573,#66574,#66575,#66576,
#66577,#66578,#66579,#66580,#66581,#66582,#66583,#66584,#66585,#66586,#66587,
#66588,#66589,#66590,#66591,#66592,#66593,#66594,#66595,#66596,#66597,#66598,
#66599,#66600,#66601,#66602,#66603,#66604,#66605,#66606,#66607),
 .UNSPECIFIED.,.F.,.F.,(4,3,3,3,3,3,3,3,3,3,3,3,3,3,3,3,3,3,3,3,3,3,3,3,
3,3,3,3,3,3,3,3,3,3,3,3,3,3,3,3,3,3,3,3,3,3,3,3,3,3,3,3,4),(65.9734457253856,
66.081074447525,66.1906366244377,66.2985803622296,66.4089517587027,66.5193231551757,
66.6242930301999,66.7291056894711,66.8337953969479,66.9384194636786,67.0430134345979,
67.1476128108322,67.2523227220928,67.3570939628641,67.4620466934886,67.5162350855004,
67.6212027061388,67.7260131047489,67.8307005532449,67.9353223633164,68.0399140832534,
68.1445112175424,68.2492189158513,68.3539879568804,68.4589385316235,68.5131470158251,
68.6181184444408,68.7229326419031,68.8276238577,68.9322494134512,69.0368448520375,
69.1414456725101,69.2461569829797,69.3509295994489,69.4558836549037,69.5100589461499,
69.6150311701829,69.7198462083276,69.824538326873,69.9291648231743,70.03376123836,
70.1383630697676,70.24307543558,70.3478491341531,70.4528043012553,70.5069708764746,
70.6119036442383,70.7166902153778,70.8213663945815,70.9259799468757,71.0305556766275,
71.1351654797296,71.1940098997199),.UNSPECIFIED.);
#704=B_SPLINE_CURVE_WITH_KNOTS('',3,(#66614,#66615,#66616,#66617,#66618,
#66619,#66620,#66621,#66622,#66623,#66624,#66625,#66626,#66627,#66628,#66629,
#66630,#66631,#66632,#66633,#66634,#66635,#66636,#66637,#66638,#66639,#66640,
#66641),.UNSPECIFIED.,.F.,.F.,(4,2,2,2,2,2,2,2,2,2,2,2,2,4),(-1.11563238755794,
-1.07955432989617,-1.03866429355625,-0.965353884613767,-0.876709828383185,
-0.787134953185386,-0.711240432632776,-0.638657623954711,-0.583650144269578,
-0.53111472373597,-0.476882015471721,-0.423633401831507,-0.331772706465313,
-0.269307451570121),.UNSPECIFIED.);
#705=B_SPLINE_CURVE_WITH_KNOTS('',3,(#66644,#66645,#66646,#66647,#66648,
#66649,#66650,#66651,#66652,#66653),.UNSPECIFIED.,.F.,.F.,(4,2,2,2,4),(-0.269307451570121,
-0.238086410933035,-0.158868946271387,-0.0862199057315852,0.),
 .UNSPECIFIED.);
#706=B_SPLINE_CURVE_WITH_KNOTS('',3,(#66657,#66658,#66659,#66660,#66661,
#66662,#66663,#66664,#66665,#66666,#66667,#66668,#66669,#66670),
 .UNSPECIFIED.,.F.,.F.,(4,2,2,2,2,2,4),(-0.384491130116531,-0.271273669787035,
-0.181083343007982,-0.137241346038334,-0.067686198175976,-0.0316925286601113,
0.),.UNSPECIFIED.);
#707=B_SPLINE_CURVE_WITH_KNOTS('',3,(#66674,#66675,#66676,#66677,#66678,
#66679),.UNSPECIFIED.,.F.,.F.,(4,1,1,4),(-4.09157007060746,-4.06042151127377,
-3.06350958094905,-2.06659765062435),.UNSPECIFIED.);
#708=B_SPLINE_CURVE_WITH_KNOTS('',3,(#66681,#66682,#66683,#66684,#66685),
 .UNSPECIFIED.,.F.,.F.,(4,1,4),(0.,0.997998106294493,1.11662023360662),
 .UNSPECIFIED.);
#709=B_SPLINE_CURVE_WITH_KNOTS('',3,(#66687,#66688,#66689,#66690,#66691,
#66692,#66693,#66694,#66695,#66696,#66697,#66698,#66699,#66700,#66701,#66702,
#66703,#66704,#66705,#66706,#66707,#66708,#66709,#66710,#66711,#66712,#66713,
#66714,#66715,#66716,#66717,#66718,#66719,#66720,#66721,#66722,#66723,#66724,
#66725,#66726,#66727,#66728,#66729,#66730,#66731,#66732,#66733,#66734,#66735,
#66736,#66737,#66738,#66739,#66740,#66741,#66742,#66743,#66744,#66745,#66746,
#66747,#66748,#66749,#66750,#66751,#66752,#66753,#66754,#66755,#66756,#66757,
#66758,#66759,#66760,#66761,#66762,#66763,#66764,#66765,#66766,#66767,#66768,
#66769,#66770,#66771,#66772,#66773,#66774,#66775,#66776,#66777,#66778,#66779,
#66780,#66781,#66782,#66783,#66784,#66785,#66786,#66787,#66788,#66789,#66790,
#66791,#66792,#66793,#66794,#66795,#66796,#66797,#66798,#66799,#66800,#66801,
#66802,#66803,#66804,#66805,#66806,#66807,#66808,#66809,#66810,#66811,#66812,
#66813,#66814,#66815,#66816,#66817,#66818,#66819,#66820,#66821,#66822,#66823,
#66824,#66825,#66826,#66827,#66828,#66829,#66830,#66831,#66832,#66833,#66834,
#66835,#66836,#66837,#66838,#66839,#66840,#66841,#66842,#66843,#66844,#66845,
#66846,#66847,#66848,#66849,#66850,#66851,#66852,#66853,#66854,#66855,#66856,
#66857,#66858,#66859,#66860,#66861,#66862,#66863,#66864,#66865,#66866,#66867,
#66868,#66869,#66870,#66871,#66872,#66873,#66874,#66875,#66876),
 .UNSPECIFIED.,.F.,.F.,(4,3,3,3,3,3,3,3,3,3,3,3,3,3,3,3,3,3,3,3,3,3,3,3,
3,3,3,3,3,3,3,3,3,3,3,3,3,3,3,3,3,3,3,3,3,3,3,3,3,3,3,3,3,3,3,3,3,3,3,3,
3,3,3,4),(1.11662023360662,1.21411903985626,1.31185368644785,1.4091285442428,
1.50635618882577,1.60356917797076,1.70167593662532,1.79901395118647,1.89750508188772,
1.99599621258898,2.09575595181835,2.19537177172638,2.29519959012101,2.39463345345404,
2.49403329621222,2.59342947268088,2.69357068423153,2.7931075696835,2.89355094428349,
2.99399431888347,3.09384741984894,3.19356069033868,3.29336465719359,3.39290523805578,
3.49241505814163,3.59192433049513,3.69194135416584,3.79159787439762,3.89179514978779,
3.99199242517796,4.09158324220157,4.19102961866606,4.29089973276686,4.39016417384572,
4.48939498922613,4.58862276885971,4.6889647095129,4.78833649761076,4.8891635145416,
4.98999053147245,5.08969774466914,5.18926191652918,5.2891027566839,5.38848753760586,
5.48783938456321,5.58718872579993,5.68738870379168,5.7868821230465,5.88743538040672,
5.98798863776694,6.08769799308571,6.18726467488049,6.2871049335281,6.38649310806084,
6.48584867520973,6.58520205952138,6.68539823065639,6.78489645125149,6.88544159765645,
6.98598674406142,7.09561182117547,7.20492700212712,7.31371639735308,7.39980554040546),
 .UNSPECIFIED.);
#710=B_SPLINE_CURVE_WITH_KNOTS('',3,(#66878,#66879,#66880,#66881,#66882,
#66883,#66884,#66885,#66886,#66887,#66888,#66889,#66890,#66891,#66892,#66893,
#66894,#66895,#66896,#66897,#66898,#66899,#66900,#66901,#66902,#66903,#66904,
#66905,#66906,#66907,#66908,#66909,#66910,#66911,#66912,#66913,#66914,#66915,
#66916,#66917,#66918,#66919,#66920,#66921,#66922,#66923,#66924,#66925,#66926,
#66927,#66928,#66929,#66930,#66931,#66932,#66933,#66934,#66935,#66936,#66937,
#66938,#66939,#66940,#66941,#66942,#66943,#66944,#66945,#66946,#66947,#66948,
#66949,#66950,#66951,#66952,#66953,#66954,#66955,#66956,#66957,#66958,#66959,
#66960,#66961,#66962,#66963,#66964,#66965,#66966,#66967,#66968,#66969,#66970,
#66971,#66972,#66973,#66974,#66975,#66976,#66977,#66978,#66979,#66980,#66981,
#66982,#66983,#66984,#66985,#66986,#66987,#66988,#66989,#66990,#66991,#66992,
#66993,#66994,#66995,#66996,#66997,#66998,#66999,#67000,#67001,#67002,#67003,
#67004,#67005,#67006,#67007,#67008,#67009,#67010,#67011,#67012,#67013,#67014,
#67015,#67016,#67017,#67018,#67019,#67020,#67021,#67022,#67023,#67024,#67025,
#67026,#67027,#67028,#67029,#67030,#67031,#67032,#67033,#67034,#67035,#67036,
#67037,#67038,#67039,#67040,#67041,#67042,#67043,#67044,#67045,#67046,#67047,
#67048,#67049,#67050,#67051,#67052,#67053,#67054,#67055,#67056,#67057,#67058,
#67059,#67060,#67061,#67062,#67063,#67064,#67065,#67066,#67067,#67068,#67069,
#67070),.UNSPECIFIED.,.F.,.F.,(4,3,3,3,3,3,3,3,3,3,3,3,3,3,3,3,3,3,3,3,
3,3,3,3,3,3,3,3,3,3,3,3,3,3,3,3,3,3,3,3,3,3,3,3,3,3,3,3,3,3,3,3,3,3,3,3,
3,3,3,3,3,3,3,3,4),(7.39980554078621,7.50085641996669,7.60195463078282,
7.70320978748876,7.80454701233738,7.90609535985808,7.98398485035592,8.08367982463198,
8.1832317804571,8.28307567748127,8.38244839256476,8.48178825804934,8.5811257191651,
8.68134002853643,8.78082194156904,8.88140244910973,8.98198295665041,9.08167691055587,
9.18122787135141,9.2810720203006,9.38044381022138,9.47978277908141,9.57911937347872,
9.67933479584527,9.77881592522409,9.87939849408449,9.9799810629449,10.0796716629935,
10.1792192051011,10.2790642006184,10.3784324389066,10.477767813924,10.5771007770452,
10.6773203750937,10.776797817893,10.8773884935662,10.9779791692394,11.0776718340994,
11.1772214697375,11.2770659454621,11.3764363317309,11.4757738704398,11.5751090100447,
11.675326076417,11.7748057049477,11.8753914902408,11.9759772755339,12.0756696578348,
12.1752190114948,12.2750635577865,12.3744336656699,12.4737709279859,12.5731057935813,
12.6733231906431,12.7728025538994,12.8733889678639,12.9739753818284,13.0729162403087,
13.1717239927683,13.2704302143224,13.3735703727333,13.4721850961793,13.5707915293105,
13.6694467689652,13.6829908479658),.UNSPECIFIED.);
#711=B_SPLINE_CURVE_WITH_KNOTS('',3,(#67072,#67073,#67074,#67075,#67076,
#67077,#67078,#67079,#67080,#67081,#67082,#67083,#67084,#67085,#67086,#67087,
#67088,#67089,#67090,#67091,#67092,#67093,#67094,#67095,#67096,#67097,#67098,
#67099,#67100,#67101,#67102,#67103,#67104,#67105,#67106,#67107,#67108,#67109,
#67110,#67111,#67112,#67113,#67114,#67115,#67116,#67117,#67118,#67119,#67120,
#67121,#67122,#67123,#67124,#67125,#67126,#67127,#67128,#67129,#67130,#67131,
#67132,#67133,#67134,#67135,#67136,#67137,#67138,#67139,#67140,#67141,#67142,
#67143,#67144,#67145,#67146,#67147,#67148,#67149,#67150,#67151,#67152,#67153,
#67154,#67155,#67156,#67157,#67158,#67159,#67160,#67161,#67162,#67163,#67164,
#67165,#67166,#67167,#67168,#67169,#67170,#67171,#67172,#67173,#67174,#67175,
#67176,#67177,#67178,#67179,#67180,#67181,#67182,#67183,#67184,#67185,#67186,
#67187,#67188,#67189,#67190,#67191,#67192,#67193,#67194,#67195,#67196,#67197,
#67198,#67199,#67200,#67201,#67202,#67203,#67204,#67205,#67206,#67207,#67208,
#67209,#67210,#67211,#67212,#67213,#67214,#67215,#67216,#67217,#67218,#67219,
#67220,#67221,#67222,#67223,#67224,#67225,#67226,#67227,#67228,#67229,#67230,
#67231,#67232,#67233,#67234,#67235,#67236,#67237,#67238,#67239,#67240,#67241,
#67242,#67243,#67244,#67245,#67246,#67247,#67248,#67249,#67250,#67251,#67252,
#67253,#67254,#67255,#67256,#67257,#67258,#67259,#67260,#67261,#67262,#67263,
#67264),.UNSPECIFIED.,.F.,.F.,(4,3,3,3,3,3,3,3,3,3,3,3,3,3,3,3,3,3,3,3,
3,3,3,3,3,3,3,3,3,3,3,3,3,3,3,3,3,3,3,3,3,3,3,3,3,3,3,3,3,3,3,3,3,3,3,3,
3,3,3,3,3,3,3,3,4),(13.6829908482554,13.8040460294717,13.9269629425475,
13.9719734881229,14.0716657749935,14.1712150296549,14.2710596002502,14.3704296011319,
14.4697667536623,14.5691015068274,14.6693190287249,14.7687982741564,14.8693849342869,
14.9699715944174,15.0696638277482,15.1692130286241,15.2690576126351,15.3684275595413,
15.4677646581471,15.5670993575134,15.667316943313,15.7667961358123,15.867382918262,
15.9679697007118,16.0676618972506,16.1672110605043,16.267055653817,16.3664255613515,
16.4657626200133,16.565097278916,16.6653149109386,16.7647940621039,16.8653809345551,
16.9659678070063,17.0656600367114,17.1652092336409,17.2650538185984,17.3644237608008,
17.4637608544271,17.5630955485436,17.6633131397329,17.762792326367,17.8633791198339,
17.9639659133008,18.0636581342268,18.1632073223082,18.2630519094691,18.362421842722,
18.4617589273806,18.5610936125237,18.6613112142916,18.7607903920308,18.861377205813,
18.9619640195953,19.0616562370282,19.1612054215272,19.2610500095725,19.3604199390515,
19.4597570198723,19.5590917011189,19.6593093073117,19.7587884810486,19.8593753034692,
19.9599621258898,19.9661761551454),.UNSPECIFIED.);
#712=B_SPLINE_CURVE_WITH_KNOTS('',3,(#67266,#67267,#67268,#67269,#67270,
#67271,#67272,#67273,#67274,#67275,#67276,#67277,#67278,#67279,#67280,#67281,
#67282,#67283,#67284,#67285,#67286,#67287,#67288,#67289,#67290,#67291,#67292,
#67293,#67294,#67295,#67296,#67297,#67298,#67299,#67300,#67301,#67302,#67303,
#67304,#67305,#67306,#67307,#67308,#67309,#67310,#67311,#67312,#67313,#67314,
#67315,#67316,#67317,#67318,#67319,#67320,#67321,#67322,#67323,#67324,#67325,
#67326,#67327,#67328,#67329,#67330,#67331,#67332,#67333,#67334,#67335,#67336,
#67337,#67338,#67339,#67340,#67341,#67342,#67343,#67344,#67345,#67346,#67347,
#67348,#67349,#67350,#67351,#67352,#67353,#67354,#67355,#67356,#67357,#67358,
#67359,#67360,#67361,#67362,#67363,#67364,#67365,#67366,#67367,#67368,#67369,
#67370,#67371,#67372,#67373,#67374,#67375,#67376,#67377,#67378,#67379,#67380,
#67381,#67382,#67383,#67384,#67385,#67386,#67387,#67388,#67389,#67390,#67391,
#67392,#67393,#67394,#67395,#67396,#67397,#67398,#67399,#67400,#67401,#67402,
#67403,#67404,#67405,#67406,#67407,#67408,#67409,#67410,#67411,#67412,#67413,
#67414,#67415,#67416,#67417,#67418,#67419,#67420,#67421,#67422,#67423,#67424,
#67425,#67426,#67427,#67428,#67429,#67430,#67431,#67432,#67433,#67434,#67435,
#67436,#67437,#67438,#67439,#67440,#67441,#67442,#67443,#67444,#67445,#67446,
#67447,#67448,#67449,#67450,#67451,#67452,#67453,#67454,#67455),
 .UNSPECIFIED.,.F.,.F.,(4,3,3,3,3,3,3,3,3,3,3,3,3,3,3,3,3,3,3,3,3,3,3,3,
3,3,3,3,3,3,3,3,3,3,3,3,3,3,3,3,3,3,3,3,3,3,3,3,3,3,3,3,3,3,3,3,3,3,3,3,
3,3,3,4),(19.9661761555104,20.0657577276433,20.1651964120122,20.2645199722879,
20.3637805135757,20.4630086753788,20.5622350573188,20.6615596078517,20.7609309415982,
20.860483049496,20.9579602321843,21.0576524523546,21.1572016396432,21.2570462269977,
21.3564161593729,21.4557532431238,21.5550879273303,21.6553055301174,21.7547847068578,
21.8553715226683,21.9559583384788,22.0556505583573,22.1551997453451,22.2550443327736,
22.3544142648279,22.4537513482509,22.5530860321232,22.6533036352857,22.7527828116792,
22.8533696282262,22.9539564447733,23.0536486651395,23.1531978526233,23.2530424399289,
23.3524123724952,23.4517494564354,23.551084140829,23.6513017433887,23.750780920309,
23.8513677356884,23.9519545510678,24.051646771243,24.1511959585335,24.2510405458871,
24.3504104782565,24.4497475619987,24.5490822461939,24.649299848986,24.7487790257078,
24.849365841535,24.9499526573622,25.0496448775194,25.1491940647909,25.2490386521491,
25.3484085844979,25.4477456682185,25.547080352391,25.6472979552074,25.7467771319055,
25.8473639477811,25.9479507636567,26.0691100425263,26.1886825764541,26.2493614619858),
 .UNSPECIFIED.);
#713=B_SPLINE_CURVE_WITH_KNOTS('',3,(#67457,#67458,#67459,#67460,#67461,
#67462,#67463,#67464,#67465,#67466,#67467,#67468,#67469,#67470,#67471,#67472,
#67473,#67474,#67475,#67476,#67477,#67478,#67479,#67480,#67481,#67482,#67483,
#67484,#67485,#67486,#67487,#67488,#67489,#67490,#67491,#67492,#67493,#67494,
#67495,#67496,#67497,#67498,#67499,#67500,#67501,#67502,#67503,#67504,#67505,
#67506,#67507,#67508,#67509,#67510,#67511,#67512,#67513,#67514,#67515,#67516,
#67517,#67518,#67519,#67520,#67521,#67522,#67523,#67524,#67525,#67526,#67527,
#67528,#67529,#67530,#67531,#67532,#67533,#67534,#67535,#67536,#67537,#67538,
#67539,#67540,#67541,#67542,#67543,#67544,#67545,#67546,#67547,#67548,#67549,
#67550,#67551,#67552,#67553,#67554,#67555,#67556,#67557,#67558,#67559,#67560,
#67561,#67562,#67563,#67564,#67565,#67566,#67567,#67568,#67569,#67570,#67571,
#67572,#67573,#67574,#67575,#67576,#67577,#67578,#67579,#67580,#67581,#67582,
#67583,#67584,#67585,#67586,#67587,#67588,#67589,#67590,#67591,#67592,#67593,
#67594,#67595,#67596,#67597,#67598,#67599,#67600,#67601,#67602,#67603,#67604,
#67605,#67606,#67607,#67608,#67609,#67610,#67611,#67612,#67613,#67614,#67615,
#67616,#67617,#67618,#67619,#67620,#67621,#67622,#67623,#67624,#67625,#67626,
#67627,#67628,#67629,#67630,#67631,#67632,#67633,#67634,#67635,#67636,#67637,
#67638,#67639,#67640,#67641,#67642,#67643,#67644,#67645,#67646),
 .UNSPECIFIED.,.F.,.F.,(4,3,3,3,3,3,3,3,3,3,3,3,3,3,3,3,3,3,3,3,3,3,3,3,
3,3,3,3,3,3,3,3,3,3,3,3,3,3,3,3,3,3,3,3,3,3,3,3,3,3,3,3,3,3,3,3,3,3,3,3,
3,3,3,4),(26.249361462325,26.3481734936058,26.4469506347904,26.5457240082695,
26.6457802236899,26.7446986980816,26.8453237840164,26.9459488699512,27.0456410901392,
27.1451902774423,27.2450348647927,27.3444047971741,27.4437418809282,27.5430765651348,
27.6432941679125,27.7427733446451,27.8433601604454,27.9439469762457,28.0436391964338,
28.1431883837368,28.2430329710872,28.3424029034685,28.4417399872223,28.5410746714285,
28.6412922742064,28.7407714509386,28.8413582667394,28.9419450825402,29.0416373027347,
29.1411864900443,29.2410310773931,29.3404010097813,29.439738093542,29.5390727777552,
29.6392903805251,29.7387695572644,29.8393563730496,29.9399431888347,30.0396354090257,
30.139184596332,30.2390291836816,30.3383991160662,30.4377361998233,30.5370708840328,
30.6372884868069,30.7367676635423,30.8373544793357,30.9379412951292,31.0376335153205,
31.1371827026271,31.2370272899766,31.3363972223614,31.4357343061186,31.5350689903286,
31.6352865931024,31.7347657698382,31.8353525856309,31.9359394014237,32.0371556997279,
32.138214632322,32.2391188409517,32.3399315096669,32.4406844014574,32.5325467695046),
 .UNSPECIFIED.);
#714=B_SPLINE_CURVE_WITH_KNOTS('',3,(#67648,#67649,#67650,#67651,#67652,
#67653,#67654,#67655,#67656,#67657,#67658,#67659,#67660,#67661,#67662,#67663,
#67664,#67665,#67666,#67667,#67668,#67669,#67670,#67671,#67672,#67673,#67674,
#67675,#67676,#67677,#67678,#67679,#67680,#67681,#67682,#67683,#67684,#67685,
#67686,#67687,#67688,#67689,#67690,#67691,#67692,#67693,#67694,#67695,#67696,
#67697,#67698,#67699,#67700,#67701,#67702,#67703,#67704,#67705,#67706,#67707,
#67708,#67709,#67710,#67711,#67712,#67713,#67714,#67715,#67716,#67717,#67718,
#67719,#67720,#67721,#67722,#67723,#67724,#67725,#67726,#67727,#67728,#67729,
#67730,#67731,#67732,#67733,#67734,#67735,#67736,#67737,#67738,#67739,#67740,
#67741,#67742,#67743,#67744,#67745,#67746,#67747,#67748,#67749,#67750,#67751,
#67752,#67753,#67754,#67755,#67756,#67757,#67758,#67759,#67760,#67761,#67762,
#67763,#67764,#67765,#67766,#67767,#67768,#67769,#67770,#67771,#67772,#67773,
#67774,#67775,#67776,#67777,#67778,#67779,#67780,#67781,#67782,#67783,#67784,
#67785,#67786,#67787,#67788,#67789,#67790,#67791,#67792,#67793,#67794,#67795,
#67796,#67797,#67798,#67799,#67800,#67801,#67802,#67803,#67804,#67805,#67806,
#67807,#67808,#67809,#67810,#67811,#67812,#67813,#67814,#67815,#67816,#67817,
#67818,#67819,#67820,#67821,#67822,#67823,#67824,#67825,#67826,#67827,#67828,
#67829,#67830,#67831,#67832,#67833,#67834,#67835,#67836,#67837),
 .UNSPECIFIED.,.F.,.F.,(4,3,3,3,3,3,3,3,3,3,3,3,3,3,3,3,3,3,3,3,3,3,3,3,
3,3,3,3,3,3,3,3,3,3,3,3,3,3,3,3,3,3,3,3,3,3,3,3,3,3,3,3,3,3,3,3,3,3,3,3,
3,3,3,4),(32.5325467697112,32.642251979765,32.7523332142757,32.8629430985259,
32.9339375077182,33.0336297279098,33.1331789152162,33.2330235025658,33.3323934349508,
33.4317305187085,33.5310652029185,33.6312828056921,33.7307619824281,33.8313487982204,
33.9319356140127,34.0316278342047,34.1311770215117,34.2310216088611,34.3303915412466,
34.4297286250046,34.529063309215,34.629280911988,34.7287600887245,34.8293469045158,
34.9299337203071,35.0296259404984,35.1291751278049,35.2290197151545,35.3283896475393,
35.4277267312967,35.5270614155066,35.6272790182804,35.7267581950163,35.827345010809,
35.9279318266017,36.0276240467927,36.1271732340988,36.2270178214484,36.3263877538329,
36.42572483759,36.5250595217995,36.6252771245737,36.7247563013092,36.8253431171027,
36.9259299328961,37.0256221530908,37.1251713404006,37.2250159277493,37.3243858601375,
37.4237229438982,37.5230576281115,37.6232752308812,37.7227544076204,37.8233412234055,
37.9239280391906,38.0223327314332,38.1215076495607,38.2196568051179,38.3177465254137,
38.4158087531075,38.5157895839441,38.6139437328095,38.7148379046316,38.8157320764536),
 .UNSPECIFIED.);
#715=B_SPLINE_CURVE_WITH_KNOTS('',3,(#67839,#67840,#67841,#67842,#67843,
#67844,#67845,#67846,#67847,#67848,#67849,#67850,#67851,#67852,#67853,#67854,
#67855,#67856,#67857,#67858,#67859,#67860,#67861,#67862,#67863,#67864,#67865,
#67866,#67867,#67868,#67869,#67870,#67871,#67872,#67873,#67874,#67875,#67876,
#67877,#67878,#67879,#67880,#67881,#67882,#67883,#67884,#67885,#67886,#67887,
#67888,#67889,#67890,#67891,#67892,#67893,#67894,#67895,#67896,#67897,#67898,
#67899,#67900,#67901,#67902,#67903,#67904,#67905,#67906,#67907,#67908,#67909,
#67910,#67911,#67912,#67913,#67914,#67915,#67916,#67917,#67918,#67919,#67920,
#67921,#67922,#67923,#67924,#67925,#67926,#67927,#67928,#67929,#67930,#67931,
#67932,#67933,#67934,#67935,#67936,#67937,#67938,#67939,#67940,#67941,#67942,
#67943,#67944,#67945,#67946,#67947,#67948,#67949,#67950,#67951,#67952,#67953,
#67954,#67955,#67956,#67957,#67958,#67959,#67960,#67961,#67962,#67963,#67964,
#67965,#67966,#67967,#67968,#67969,#67970,#67971,#67972,#67973,#67974,#67975,
#67976,#67977,#67978,#67979,#67980,#67981,#67982,#67983,#67984,#67985,#67986,
#67987,#67988,#67989,#67990,#67991,#67992,#67993,#67994,#67995,#67996,#67997,
#67998,#67999,#68000,#68001,#68002,#68003,#68004,#68005,#68006,#68007,#68008,
#68009,#68010,#68011,#68012,#68013,#68014,#68015,#68016,#68017,#68018,#68019,
#68020,#68021,#68022,#68023,#68024,#68025,#68026,#68027,#68028),
 .UNSPECIFIED.,.F.,.F.,(4,3,3,3,3,3,3,3,3,3,3,3,3,3,3,3,3,3,3,3,3,3,3,3,
3,3,3,3,3,3,3,3,3,3,3,3,3,3,3,3,3,3,3,3,3,3,3,3,3,3,3,3,3,3,3,3,3,3,3,3,
3,3,3,4),(38.8157320766842,38.9219261454851,39.0216183656735,39.121167552977,
39.2210121403273,39.320382072709,39.4197191564632,39.5190538406699,39.6192714434473,
39.71875062018,39.8193374359798,39.9199242517796,40.0196164719951,40.1191656593257,
40.2190102466693,40.3183801790783,40.4177172628598,40.5170519470937,40.6172695498388,
40.7167487265982,40.8173355423361,40.9179223580741,41.0176145782277,41.1171637654965,
41.2170083528555,41.3163782852032,41.4157153689238,41.5150500530972,41.615267655915,
41.7147468326156,41.8153336484921,41.9159204643686,42.0156126845468,42.1151618718396,
42.2150064591925,42.3143763915628,42.4137134753053,42.5130481594999,42.6132657622907,
42.7127449390108,42.8133317548369,42.9139185706631,43.0136107910374,43.1131599785273,
43.2130045658311,43.3123744983996,43.4117115823403,43.5110462667328,43.611263869289,
43.7107430462041,43.8113298615808,43.9119166769576,44.0116088968064,44.1111580837707,
44.2110026712059,44.3103726032525,44.4097096866739,44.5090443705503,44.6092619737258,
44.7087411501379,44.809327966695,44.9099147832521,45.0568405353361,45.0989173838637),
 .UNSPECIFIED.);
#716=B_SPLINE_CURVE_WITH_KNOTS('',3,(#68030,#68031,#68032,#68033,#68034,
#68035,#68036,#68037,#68038,#68039,#68040,#68041,#68042,#68043,#68044,#68045,
#68046,#68047,#68048,#68049,#68050,#68051,#68052,#68053,#68054,#68055,#68056,
#68057,#68058,#68059,#68060,#68061,#68062,#68063,#68064,#68065,#68066,#68067,
#68068,#68069,#68070,#68071,#68072,#68073,#68074,#68075,#68076,#68077,#68078,
#68079,#68080,#68081,#68082,#68083,#68084,#68085,#68086,#68087,#68088,#68089,
#68090,#68091,#68092,#68093,#68094,#68095,#68096,#68097,#68098,#68099,#68100,
#68101,#68102,#68103,#68104,#68105,#68106,#68107,#68108,#68109,#68110,#68111,
#68112,#68113,#68114,#68115,#68116,#68117,#68118,#68119,#68120,#68121,#68122,
#68123,#68124,#68125,#68126,#68127,#68128,#68129,#68130,#68131,#68132,#68133,
#68134,#68135,#68136,#68137,#68138,#68139,#68140,#68141,#68142,#68143,#68144,
#68145,#68146,#68147,#68148,#68149,#68150,#68151,#68152,#68153,#68154,#68155,
#68156,#68157,#68158,#68159,#68160,#68161,#68162,#68163,#68164,#68165,#68166,
#68167,#68168,#68169,#68170,#68171,#68172,#68173,#68174,#68175,#68176,#68177,
#68178,#68179,#68180,#68181,#68182,#68183,#68184,#68185,#68186,#68187,#68188,
#68189,#68190,#68191,#68192,#68193,#68194,#68195,#68196,#68197,#68198,#68199,
#68200,#68201,#68202,#68203,#68204,#68205,#68206,#68207,#68208,#68209,#68210,
#68211,#68212,#68213,#68214,#68215,#68216,#68217,#68218,#68219,#68220,#68221,
#68222),.UNSPECIFIED.,.F.,.F.,(4,3,3,3,3,3,3,3,3,3,3,3,3,3,3,3,3,3,3,3,
3,3,3,3,3,3,3,3,3,3,3,3,3,3,3,3,3,3,3,3,3,3,3,3,3,3,3,3,3,3,3,3,3,3,3,3,
3,3,3,3,3,3,3,3,4),(45.0989173840905,45.2000418222725,45.2980012309023,
45.3959090948093,45.4937975009913,45.5916985068107,45.6897025308092,45.7877690184893,
45.885989317891,45.9079128895465,46.0076051110968,46.1071542997675,46.2069988867767,
46.3063688205293,46.4057059056527,46.5050405912249,46.6052581923789,46.7047373704543,
46.8053241831477,46.905910995841,47.0056032130355,47.1051523973474,47.2049969854459,
47.3043669148636,47.4037039956706,47.5030386769507,47.6032562832469,47.702735457133,
47.8033222796342,47.9039091021355,48.0036013233754,48.1031505117032,48.202995098794,
48.3023650321276,48.4017021168047,48.5010368019041,48.6012544035356,48.7007335810783,
48.8013203947542,48.90190720843,49.0015994384125,49.1011486355596,49.2009932204552,
49.3003631627289,49.3997002563714,49.4990349504489,49.5992525415178,49.6987317279782,
49.7993185213514,49.8999053147245,49.9995975093961,50.0991466711844,50.1989912649137,
50.298361171968,50.397698230521,50.4970328896857,50.597250522519,50.6967296748532,
50.7973165479361,50.897903421019,51.0034366957994,51.1086517278921,51.2136734259997,
51.3184380308843,51.3821026907301),.UNSPECIFIED.);
#717=B_SPLINE_CURVE_WITH_KNOTS('',3,(#68224,#68225,#68226,#68227,#68228,
#68229,#68230,#68231,#68232,#68233,#68234,#68235,#68236,#68237,#68238,#68239,
#68240,#68241,#68242,#68243,#68244,#68245,#68246,#68247,#68248,#68249,#68250,
#68251,#68252,#68253,#68254,#68255,#68256,#68257,#68258,#68259,#68260,#68261,
#68262,#68263,#68264,#68265,#68266,#68267,#68268,#68269,#68270,#68271,#68272,
#68273,#68274,#68275,#68276,#68277,#68278,#68279,#68280,#68281,#68282,#68283,
#68284,#68285,#68286,#68287,#68288,#68289,#68290,#68291,#68292,#68293,#68294,
#68295,#68296,#68297,#68298,#68299,#68300,#68301,#68302,#68303,#68304,#68305,
#68306,#68307,#68308,#68309,#68310,#68311,#68312,#68313,#68314,#68315,#68316,
#68317,#68318,#68319,#68320,#68321,#68322,#68323,#68324,#68325,#68326,#68327,
#68328,#68329,#68330,#68331,#68332,#68333,#68334,#68335,#68336,#68337,#68338,
#68339,#68340,#68341,#68342,#68343,#68344,#68345,#68346,#68347,#68348,#68349,
#68350,#68351,#68352,#68353,#68354,#68355,#68356,#68357,#68358,#68359,#68360,
#68361,#68362,#68363,#68364,#68365,#68366,#68367,#68368,#68369,#68370,#68371,
#68372,#68373,#68374,#68375,#68376,#68377,#68378,#68379,#68380,#68381,#68382,
#68383,#68384,#68385,#68386,#68387,#68388,#68389,#68390,#68391,#68392,#68393,
#68394,#68395,#68396,#68397,#68398,#68399,#68400,#68401,#68402,#68403,#68404,
#68405,#68406,#68407,#68408,#68409,#68410,#68411,#68412,#68413),
 .UNSPECIFIED.,.F.,.F.,(4,3,3,3,3,3,3,3,3,3,3,3,3,3,3,3,3,3,3,3,3,3,3,3,
3,3,3,3,3,3,3,3,3,3,3,3,3,3,3,3,3,3,3,3,3,3,3,3,3,3,3,3,3,3,3,3,3,3,3,3,
3,3,3,4),(51.3821026910433,51.4855307958723,51.5892117397779,51.6930192770188,
51.797104292293,51.8959015273135,51.9955938152988,52.095143070835,52.1949876411816,
52.2943576423501,52.3936947949456,52.4930295479546,52.593247069368,52.692726314102,
52.793312973855,52.893899633608,52.9935916415485,53.093140616474,53.1929852569026,
53.2923549781269,53.3916918516459,53.491026326818,53.5912441800891,53.6907231528435,
53.791310446373,53.8918977399025,53.9915901487866,54.0911395233135,54.1909840636739,
54.2903541783941,54.3896914422614,54.4890263041265,54.5892436896441,54.6887230362615,
54.7893094412292,54.8898958461969,54.9895885107553,55.0891381461562,55.1889826219481,
55.2883530081394,55.3876905468306,55.4870256864775,55.587242752981,55.6867223817006,
55.787308167096,55.8878939524914,55.9875844461522,56.0871319047493,56.1869769240039,
56.28634513493,56.3856805037378,56.4850134817863,56.5852331260362,56.6847106354235,
56.7853013471047,56.8858920587859,56.9841948130386,57.0823705698818,57.1804515428413,
57.2784698224436,57.3764943428403,57.4745156851681,57.5726368200333,57.6652879979023),
 .UNSPECIFIED.);
#718=B_SPLINE_CURVE_WITH_KNOTS('',3,(#68415,#68416,#68417,#68418,#68419,
#68420,#68421,#68422,#68423,#68424,#68425,#68426,#68427,#68428,#68429,#68430,
#68431,#68432,#68433,#68434,#68435,#68436,#68437,#68438,#68439,#68440,#68441,
#68442,#68443,#68444,#68445,#68446,#68447,#68448,#68449,#68450,#68451,#68452,
#68453,#68454,#68455,#68456,#68457,#68458,#68459,#68460,#68461,#68462,#68463,
#68464,#68465,#68466,#68467,#68468,#68469,#68470,#68471,#68472,#68473,#68474,
#68475,#68476,#68477,#68478,#68479,#68480,#68481,#68482,#68483,#68484,#68485,
#68486,#68487,#68488,#68489,#68490,#68491,#68492,#68493,#68494,#68495,#68496,
#68497,#68498,#68499,#68500,#68501,#68502,#68503,#68504,#68505,#68506,#68507,
#68508,#68509,#68510,#68511,#68512,#68513,#68514,#68515,#68516,#68517,#68518,
#68519,#68520,#68521,#68522,#68523,#68524,#68525,#68526,#68527,#68528,#68529,
#68530,#68531,#68532,#68533,#68534,#68535,#68536,#68537,#68538,#68539,#68540,
#68541,#68542,#68543,#68544,#68545,#68546,#68547,#68548,#68549,#68550,#68551,
#68552,#68553,#68554,#68555,#68556,#68557,#68558,#68559,#68560,#68561,#68562,
#68563,#68564,#68565,#68566,#68567,#68568,#68569,#68570,#68571,#68572,#68573,
#68574,#68575,#68576,#68577,#68578,#68579,#68580,#68581,#68582,#68583,#68584,
#68585,#68586,#68587,#68588,#68589,#68590,#68591,#68592,#68593,#68594,#68595,
#68596,#68597,#68598,#68599,#68600,#68601,#68602,#68603,#68604),
 .UNSPECIFIED.,.F.,.F.,(4,3,3,3,3,3,3,3,3,3,3,3,3,3,3,3,3,3,3,3,3,3,3,3,
3,3,3,3,3,3,3,3,3,3,3,3,3,3,3,3,3,3,3,3,3,3,3,3,3,3,3,3,3,3,3,3,3,3,3,3,
3,3,3,4),(57.6652879982229,57.8019872101644,57.8838901650804,57.9835850616989,
58.0831369565666,58.1829808709176,58.2823535660295,58.3816934269835,58.4810308989979,
58.5812452420922,58.6807272037328,58.7813077375538,58.8818882713749,58.9815667546959,
59.0811021788842,59.1809502037324,59.2803064091976,59.3796298098178,59.478950872875,
59.5791847490736,59.6786505945985,59.779268486134,59.8798863776694,59.9795977204589,
60.0791659622596,60.1790057774726,60.2783944630306,60.3777501459646,60.4771032511164,
60.5772985593283,60.6767955357196,60.7773400098417,60.8778844839639,60.9775904742664,
61.0771536862424,61.1769947992444,61.276379265716,61.3757310414051,61.4750805543747,
61.5752810633456,61.6747752481323,61.7753289191953,61.8758825902584,61.9754681206924,
62.0749103463045,62.1747816400855,62.2740447196494,62.3732752234771,62.4725037407329,
62.5728479796879,62.6722230732196,62.7730518848863,62.8738806965529,62.9737506217514,
63.0734770927308,63.1732773064954,63.2728222045018,63.372332990656,63.471839880485,
63.5718496110756,63.6714955828981,63.7716871928727,63.8718788028474,63.9484733054025),
 .UNSPECIFIED.);
#719=B_SPLINE_CURVE_WITH_KNOTS('',3,(#68606,#68607,#68608,#68609,#68610,
#68611,#68612,#68613,#68614,#68615,#68616,#68617,#68618,#68619,#68620,#68621,
#68622,#68623,#68624,#68625,#68626,#68627,#68628,#68629,#68630,#68631,#68632,
#68633),.UNSPECIFIED.,.F.,.F.,(4,3,3,3,3,3,3,3,3,4),(63.9484733057947,64.045833445615,
64.1430501669001,64.240187491038,64.3372781596142,64.4343548402426,64.5315110163484,
64.6287070047887,64.7260617590684,64.7992696555444),.UNSPECIFIED.);
#720=B_SPLINE_CURVE_WITH_KNOTS('',3,(#68639,#68640,#68641,#68642,#68643,
#68644,#68645,#68646,#68647,#68648),.UNSPECIFIED.,.F.,.F.,(4,1,1,1,1,1,
1,4),(-66.8658731217308,-65.8689611914061,-64.8720492610814,-63.8751373307567,
-62.878225400432,-61.8813134701072,-60.8844015397825,-60.6402388355142),
 .UNSPECIFIED.);
#721=B_SPLINE_CURVE_WITH_KNOTS('',3,(#68650,#68651,#68652,#68653,#68654,
#68655,#68656,#68657,#68658,#68659,#68660,#68661,#68662,#68663,#68664,#68665,
#68666,#68667,#68668,#68669,#68670,#68671,#68672,#68673,#68674,#68675,#68676,
#68677,#68678,#68679,#68680,#68681,#68682,#68683,#68684,#68685,#68686,#68687,
#68688,#68689,#68690,#68691,#68692,#68693,#68694,#68695,#68696,#68697,#68698,
#68699,#68700,#68701,#68702,#68703,#68704,#68705,#68706,#68707,#68708,#68709,
#68710,#68711,#68712,#68713,#68714,#68715,#68716,#68717,#68718,#68719,#68720,
#68721,#68722,#68723,#68724,#68725,#68726,#68727,#68728,#68729,#68730,#68731,
#68732,#68733,#68734,#68735,#68736,#68737,#68738,#68739,#68740,#68741,#68742,
#68743,#68744,#68745,#68746,#68747,#68748,#68749,#68750,#68751,#68752,#68753,
#68754,#68755,#68756,#68757,#68758,#68759,#68760,#68761,#68762,#68763,#68764,
#68765,#68766,#68767,#68768,#68769,#68770,#68771,#68772,#68773,#68774,#68775,
#68776,#68777,#68778,#68779,#68780,#68781,#68782,#68783,#68784,#68785,#68786,
#68787,#68788,#68789,#68790,#68791,#68792,#68793,#68794,#68795,#68796,#68797,
#68798,#68799,#68800,#68801,#68802,#68803,#68804,#68805,#68806,#68807,#68808,
#68809,#68810,#68811,#68812,#68813,#68814,#68815,#68816,#68817,#68818,#68819,
#68820,#68821,#68822,#68823,#68824,#68825,#68826,#68827,#68828,#68829,#68830,
#68831,#68832,#68833,#68834,#68835,#68836,#68837,#68838,#68839,#68840,#68841,
#68842),.UNSPECIFIED.,.F.,.F.,(4,3,3,3,3,3,3,3,3,3,3,3,3,3,3,3,3,3,3,3,
3,3,3,3,3,3,3,3,3,3,3,3,3,3,3,3,3,3,3,3,3,3,3,3,3,3,3,3,3,3,3,3,3,3,3,3,
3,3,3,3,3,3,3,3,4),(-60.6402378352238,-60.541941212625,-60.4437069664625,
-60.3455032818595,-60.2472983849303,-60.1489962635298,-60.0506424675455,
-59.9521211484188,-59.8874896094578,-59.7877964476612,-59.688246214181,
-59.5885376473,-59.4891664171286,-59.389827997839,-59.290491942401,-59.190513376584,
-59.0910331601191,-58.9908054196261,-58.8905776791331,-58.7908689547546,
-58.6913029540899,-58.5915983034297,-58.492210925325,-58.3928562507879,
-58.2935038548443,-58.1935443283353,-58.0940477288565,-57.9938567388324,
-57.8936657488084,-57.7939580819579,-57.6943931146846,-57.5946882026595,
-57.4953017907731,-57.3959480548088,-57.2965965683636,-57.1966358808936,
-57.0971401095801,-56.9969469640319,-56.8967538184837,-56.797049434805,
-56.6974878144905,-56.5977820736991,-56.4983991394847,-56.3990489227396,
-56.2997009923592,-56.1997362163091,-56.1002440555365,-56.0000429718477,
-55.899841888159,-55.8001354687304,-55.7005717841839,-55.6008665558901,
-55.5014815034612,-55.4021291529011,-55.3027790759983,-55.2028167964573,
-55.1033224798672,-55.0031262188507,-54.9029299578342,-54.8000855684324,
-54.6974202396436,-54.5949536053784,-54.4926049980164,-54.3903737338144,
-54.3570525280442),.UNSPECIFIED.);
#722=B_SPLINE_CURVE_WITH_KNOTS('',3,(#68844,#68845,#68846,#68847,#68848,
#68849,#68850,#68851,#68852,#68853,#68854,#68855,#68856,#68857,#68858,#68859,
#68860,#68861,#68862,#68863,#68864,#68865,#68866,#68867,#68868,#68869,#68870,
#68871,#68872,#68873,#68874,#68875,#68876,#68877,#68878,#68879,#68880,#68881,
#68882,#68883,#68884,#68885,#68886,#68887,#68888,#68889,#68890,#68891,#68892,
#68893,#68894,#68895,#68896,#68897,#68898,#68899,#68900,#68901,#68902,#68903,
#68904,#68905,#68906,#68907,#68908,#68909,#68910,#68911,#68912,#68913,#68914,
#68915,#68916,#68917,#68918,#68919,#68920,#68921,#68922,#68923,#68924,#68925,
#68926,#68927,#68928,#68929,#68930,#68931,#68932,#68933,#68934,#68935,#68936,
#68937,#68938,#68939,#68940,#68941,#68942,#68943,#68944,#68945,#68946,#68947,
#68948,#68949,#68950,#68951,#68952,#68953,#68954,#68955,#68956,#68957,#68958,
#68959,#68960,#68961,#68962,#68963,#68964,#68965,#68966,#68967,#68968,#68969,
#68970,#68971,#68972,#68973,#68974,#68975,#68976,#68977,#68978,#68979,#68980,
#68981,#68982,#68983,#68984,#68985,#68986,#68987,#68988,#68989,#68990,#68991,
#68992,#68993,#68994,#68995,#68996,#68997,#68998,#68999,#69000,#69001,#69002,
#69003,#69004,#69005,#69006,#69007,#69008,#69009,#69010,#69011,#69012,#69013,
#69014,#69015,#69016,#69017,#69018,#69019,#69020,#69021,#69022,#69023,#69024,
#69025,#69026,#69027,#69028,#69029,#69030,#69031,#69032,#69033,#69034,#69035,
#69036),.UNSPECIFIED.,.F.,.F.,(4,3,3,3,3,3,3,3,3,3,3,3,3,3,3,3,3,3,3,3,
3,3,3,3,3,3,3,3,3,3,3,3,3,3,3,3,3,3,3,3,3,3,3,3,3,3,3,3,3,3,3,3,3,3,3,3,
3,3,3,3,3,3,3,3,4),(-54.3570525278076,-54.2507043889139,-54.1439444211688,
-54.0369627416244,-53.9296600714483,-53.9060180275095,-53.8063122441195,
-53.7067492024809,-53.6070438143189,-53.5076594166994,-53.4083077239587,
-53.3089583069853,-53.2089952545352,-53.1095015962846,-53.0093038467347,
-52.9091060971848,-52.8094000541278,-52.7098367489929,-52.6101314262263,
-52.5107467577453,-52.4113947919731,-52.3120451001678,-52.2120823668409,
-52.1125884321395,-52.0123912994998,-51.9121941668601,-51.8124881776674,
-51.7129249266653,-51.613219590399,-51.5138349762923,-51.4144830648616,
-51.3151334272894,-51.2151706296009,-51.1156767483046,-51.01547949242,-50.9152822365354,
-50.8155762825399,-50.7160130675383,-50.6163077223724,-50.5169231459594,
-50.4175712727776,-50.3182216739587,-50.2182588320217,-50.118764990327,
-50.0185676482688,-49.9183703062107,-49.8186643198593,-49.7191010720012,
-49.6193957349868,-49.5200111247426,-49.4206592174378,-49.3213095842503,
-49.2213467821592,-49.1218529058425,-49.0216556408642,-48.9214583758859,
-48.8232165413679,-48.7251385007468,-48.6271523335141,-48.529225872404,
-48.4313270291267,-48.333374301944,-48.2353942142858,-48.1372843483312,
-48.0738672212483),.UNSPECIFIED.);
#723=B_SPLINE_CURVE_WITH_KNOTS('',3,(#69038,#69039,#69040,#69041,#69042,
#69043,#69044,#69045,#69046,#69047,#69048,#69049,#69050,#69051,#69052,#69053,
#69054,#69055,#69056,#69057,#69058,#69059,#69060,#69061,#69062,#69063,#69064,
#69065,#69066,#69067,#69068,#69069,#69070,#69071,#69072,#69073,#69074,#69075,
#69076,#69077,#69078,#69079,#69080,#69081,#69082,#69083,#69084,#69085,#69086,
#69087,#69088,#69089,#69090,#69091,#69092,#69093,#69094,#69095,#69096,#69097,
#69098,#69099,#69100,#69101,#69102,#69103,#69104,#69105,#69106,#69107,#69108,
#69109,#69110,#69111,#69112,#69113,#69114,#69115,#69116,#69117,#69118,#69119,
#69120,#69121,#69122,#69123,#69124,#69125,#69126,#69127,#69128,#69129,#69130,
#69131,#69132,#69133,#69134,#69135,#69136,#69137,#69138,#69139,#69140,#69141,
#69142,#69143,#69144,#69145,#69146,#69147,#69148,#69149,#69150,#69151,#69152,
#69153,#69154,#69155,#69156,#69157,#69158,#69159,#69160,#69161,#69162,#69163,
#69164,#69165,#69166,#69167,#69168,#69169,#69170,#69171,#69172,#69173,#69174,
#69175,#69176,#69177,#69178,#69179,#69180,#69181,#69182,#69183,#69184,#69185,
#69186,#69187,#69188,#69189,#69190,#69191,#69192,#69193,#69194,#69195,#69196,
#69197,#69198,#69199,#69200,#69201,#69202,#69203,#69204,#69205,#69206,#69207,
#69208,#69209,#69210,#69211,#69212,#69213,#69214,#69215,#69216,#69217,#69218,
#69219,#69220,#69221,#69222,#69223,#69224),.UNSPECIFIED.,.F.,.F.,(4,3,3,
3,3,3,3,3,3,3,3,3,3,3,3,3,3,3,3,3,3,3,3,3,3,3,3,3,3,3,3,3,3,3,3,3,3,3,3,
3,3,3,3,3,3,3,3,3,3,3,3,3,3,3,3,3,3,3,3,3,3,3,4),(-48.0738672208646,-47.9245464455612,
-47.824840471252,-47.725277235593,-47.6255718955484,-47.5261872977941,-47.4268354030607,
-47.327485782509,-47.2275229656908,-47.128029102039,-47.0278318086377,-46.9276345152365,
-46.8279285369865,-46.7283652973229,-46.6286599582715,-46.5292753563869,
-46.4299234574851,-46.3305738327324,-46.2306110207772,-46.1311171528873,
-46.0309198688996,-45.9307225849118,-45.8310166079799,-45.7314533696477,
-45.6317480302652,-45.5323634297345,-45.433011532192,-45.3336619088021,
-45.2336990952484,-45.1342052287161,-45.0340079416516,-44.9338106545871,
-44.8341046779189,-44.734541439859,-44.6348361004094,-44.53545150017,-44.4360996029253,
-44.3367499798393,-44.2367871659451,-44.1372932997287,-44.0370960119956,
-43.9368987242624,-43.8371927471253,-43.7376295085886,-43.6379241692572,
-43.5385395685251,-43.4391876707829,-43.3398380471953,-43.2398752338809,
-43.1403813671576,-43.0401840805477,-42.9399867939377,-42.8402808169886,
-42.7407175786422,-42.6410122392635,-42.5416276387255,-42.4422757411784,
-42.3429261177866,-42.2429633042431,-42.1434694377156,-42.0432721506642,
-41.9430748636129,-41.790681913685),.UNSPECIFIED.);
#724=B_SPLINE_CURVE_WITH_KNOTS('',3,(#69226,#69227,#69228,#69229,#69230,
#69231,#69232,#69233,#69234,#69235,#69236,#69237,#69238,#69239,#69240,#69241,
#69242,#69243,#69244,#69245,#69246,#69247,#69248,#69249,#69250,#69251,#69252,
#69253,#69254,#69255,#69256,#69257,#69258,#69259,#69260,#69261,#69262,#69263,
#69264,#69265,#69266,#69267,#69268,#69269,#69270,#69271,#69272,#69273,#69274,
#69275,#69276,#69277,#69278,#69279,#69280,#69281,#69282,#69283,#69284,#69285,
#69286,#69287,#69288,#69289,#69290,#69291,#69292,#69293,#69294,#69295,#69296,
#69297,#69298,#69299,#69300,#69301,#69302,#69303,#69304,#69305,#69306,#69307,
#69308,#69309,#69310,#69311,#69312,#69313,#69314,#69315,#69316,#69317,#69318,
#69319,#69320,#69321,#69322,#69323,#69324,#69325,#69326,#69327,#69328,#69329,
#69330,#69331,#69332,#69333,#69334,#69335,#69336,#69337,#69338,#69339,#69340,
#69341,#69342,#69343,#69344,#69345,#69346,#69347,#69348,#69349,#69350,#69351,
#69352,#69353,#69354,#69355,#69356,#69357,#69358,#69359,#69360,#69361,#69362,
#69363,#69364,#69365,#69366,#69367,#69368,#69369,#69370,#69371,#69372,#69373,
#69374,#69375,#69376,#69377,#69378,#69379,#69380,#69381,#69382,#69383,#69384,
#69385,#69386,#69387,#69388,#69389,#69390,#69391,#69392,#69393,#69394,#69395,
#69396,#69397,#69398,#69399,#69400,#69401,#69402,#69403,#69404,#69405,#69406,
#69407,#69408,#69409,#69410,#69411,#69412,#69413,#69414,#69415,#69416,#69417,
#69418),.UNSPECIFIED.,.F.,.F.,(4,3,3,3,3,3,3,3,3,3,3,3,3,3,3,3,3,3,3,3,
3,3,3,3,3,3,3,3,3,3,3,3,3,3,3,3,3,3,3,3,3,3,3,3,3,3,3,3,3,3,3,3,3,3,3,3,
3,3,3,3,3,3,3,3,4),(-41.7906819133136,-41.6925640062099,-41.5945653582671,
-41.4966311262791,-41.3987292076811,-41.3008275445918,-41.2028311665152,
-41.104783880033,-41.0065724507144,-40.9461629332882,-40.8464569562993,
-40.7468937179126,-40.647188378544,-40.5478037779658,-40.4484518803784,
-40.3491022569467,-40.2491394434509,-40.149645576884,-40.0494482899238,
-39.9492510029635,-39.8495450260004,-39.7499817876397,-39.6502764482646,
-39.5508918477131,-39.4515399501526,-39.3521903267478,-39.2522275132206,
-39.1527336466808,-39.0525363596598,-38.9523390726388,-38.8526330956752,
-38.7530698573145,-38.6533645179394,-38.5539799173876,-38.4546280198271,
-38.355278396422,-38.255315582895,-38.1558217163552,-38.0556244293346,-37.9554271423141,
-37.8557211653444,-37.7561579269774,-37.6564525876039,-37.5570679870457,
-37.4577160894784,-37.3583664660668,-37.2584036525475,-37.158909786001,
-37.0587124989952,-36.9585152119894,-36.8588092350233,-36.75924599666,-36.6595406572856,
-36.5601560567309,-36.4608041591676,-36.3614545357598,-36.261491722236,
-36.1619978556932,-36.0618005686789,-35.9616032816647,-35.8544601488088,
-35.7476875248841,-35.6411508212861,-35.5349368592938,-35.5074966067279),
 .UNSPECIFIED.);
#725=B_SPLINE_CURVE_WITH_KNOTS('',3,(#69420,#69421,#69422,#69423,#69424,
#69425,#69426,#69427,#69428,#69429,#69430,#69431,#69432,#69433,#69434,#69435,
#69436,#69437,#69438,#69439,#69440,#69441,#69442,#69443,#69444,#69445,#69446,
#69447,#69448,#69449,#69450,#69451,#69452,#69453,#69454,#69455,#69456,#69457,
#69458,#69459,#69460,#69461,#69462,#69463,#69464,#69465,#69466,#69467,#69468,
#69469,#69470,#69471,#69472,#69473,#69474,#69475,#69476,#69477,#69478,#69479,
#69480,#69481,#69482,#69483,#69484,#69485,#69486,#69487,#69488,#69489,#69490,
#69491,#69492,#69493,#69494,#69495,#69496,#69497,#69498,#69499,#69500,#69501,
#69502,#69503,#69504,#69505,#69506,#69507,#69508,#69509,#69510,#69511,#69512,
#69513,#69514,#69515,#69516,#69517,#69518,#69519,#69520,#69521,#69522,#69523,
#69524,#69525,#69526,#69527,#69528,#69529,#69530,#69531,#69532,#69533,#69534,
#69535,#69536,#69537,#69538,#69539,#69540,#69541,#69542,#69543,#69544,#69545,
#69546,#69547,#69548,#69549,#69550,#69551,#69552,#69553,#69554,#69555,#69556,
#69557,#69558,#69559,#69560,#69561,#69562,#69563,#69564,#69565,#69566,#69567,
#69568,#69569,#69570,#69571,#69572,#69573,#69574,#69575,#69576,#69577,#69578,
#69579,#69580,#69581,#69582,#69583,#69584,#69585,#69586,#69587,#69588,#69589,
#69590,#69591,#69592,#69593,#69594,#69595,#69596,#69597,#69598,#69599,#69600,
#69601,#69602,#69603,#69604,#69605,#69606,#69607,#69608,#69609,#69610,#69611,
#69612),.UNSPECIFIED.,.F.,.F.,(4,3,3,3,3,3,3,3,3,3,3,3,3,3,3,3,3,3,3,3,
3,3,3,3,3,3,3,3,3,3,3,3,3,3,3,3,3,3,3,3,3,3,3,3,3,3,3,3,3,3,3,3,3,3,3,3,
3,3,3,3,3,3,3,3,4),(-35.5074966065053,-35.4051595705186,-35.3027289474575,
-35.2000975899008,-35.0973517910919,-34.9943911189887,-34.9646913513399,
-34.8649853743722,-34.7654221360073,-34.6657167966333,-34.5663321960772,
-34.4669802985123,-34.367630675103,-34.267667861581,-34.1681739950367,-34.067976708026,
-33.9677794210152,-33.8680734440487,-33.768510205685,-33.6688048663107,
-33.5694202657559,-33.4700683681921,-33.370718744784,-33.2707559312606,
-33.1712620647175,-33.071064777704,-32.9708674906905,-32.8711615137242,
-32.7715982753605,-32.6718929359862,-32.5725083354315,-32.4731564378678,
-32.37380681446,-32.2738440009364,-32.1743501343935,-32.0741528473796,-31.9739555603658,
-31.8742495833959,-31.7746863450287,-31.6749810056553,-31.5755964050969,
-31.4762445075297,-31.3768948841183,-31.276932070599,-31.1774382040526,
-31.0772409170468,-30.9770436300411,-30.877337653078,-30.7777744147177,
-30.6780690753425,-30.5786844747909,-30.4793325772303,-30.3799829538252,
-30.280020140298,-30.180526273758,-30.0803289867372,-29.9801316997164,-29.8816680285451,
-29.7833326010158,-29.6850933512488,-29.5869183344749,-29.4887449677475,
-29.3905760088001,-29.2923247508768,-29.2243112993258),.UNSPECIFIED.);
#726=B_SPLINE_CURVE_WITH_KNOTS('',3,(#69614,#69615,#69616,#69617,#69618,
#69619,#69620,#69621,#69622,#69623,#69624,#69625,#69626,#69627,#69628,#69629,
#69630,#69631,#69632,#69633,#69634,#69635,#69636,#69637,#69638,#69639,#69640,
#69641,#69642,#69643,#69644,#69645,#69646,#69647,#69648,#69649,#69650,#69651,
#69652,#69653,#69654,#69655,#69656,#69657,#69658,#69659,#69660,#69661,#69662,
#69663,#69664,#69665,#69666,#69667,#69668,#69669,#69670,#69671,#69672,#69673,
#69674,#69675,#69676,#69677,#69678,#69679,#69680,#69681,#69682,#69683,#69684,
#69685,#69686,#69687,#69688,#69689,#69690,#69691,#69692,#69693,#69694,#69695,
#69696,#69697,#69698,#69699,#69700,#69701,#69702,#69703,#69704,#69705,#69706,
#69707,#69708,#69709,#69710,#69711,#69712,#69713,#69714,#69715,#69716,#69717,
#69718,#69719,#69720,#69721,#69722,#69723,#69724,#69725,#69726,#69727,#69728,
#69729,#69730,#69731,#69732,#69733,#69734,#69735,#69736,#69737,#69738,#69739,
#69740,#69741,#69742,#69743,#69744,#69745,#69746,#69747,#69748,#69749,#69750,
#69751,#69752,#69753,#69754,#69755,#69756,#69757,#69758,#69759,#69760,#69761,
#69762,#69763,#69764,#69765,#69766,#69767,#69768,#69769,#69770,#69771,#69772,
#69773,#69774,#69775,#69776,#69777,#69778,#69779,#69780,#69781,#69782,#69783,
#69784,#69785,#69786,#69787,#69788,#69789,#69790,#69791,#69792,#69793,#69794,
#69795,#69796,#69797,#69798,#69799,#69800,#69801,#69802,#69803),
 .UNSPECIFIED.,.F.,.F.,(4,3,3,3,3,3,3,3,3,3,3,3,3,3,3,3,3,3,3,3,3,3,3,3,
3,3,3,3,3,3,3,3,3,3,3,3,3,3,3,3,3,3,3,3,3,3,3,3,3,3,3,3,3,3,3,3,3,3,3,3,
3,3,3,4),(-29.2243112990037,-29.0935052524198,-28.9832197693916,-28.8835137924016,
-28.7839505540141,-28.6842452146457,-28.5848606140673,-28.4855087164801,
-28.3861590930487,-28.2861962795532,-28.1867024129872,-28.086505126027,
-27.9863078390669,-27.8866018621359,-27.7870386238074,-27.6873332844243,
-27.5879486839043,-27.4885967863751,-27.3892471630013,-27.2892843494365,
-27.1897904829265,-27.0895931958344,-26.9893959087422,-26.8896899317904,
-26.7901266934417,-26.6904213540637,-26.5910367535249,-26.4916848559776,
-26.3923352325861,-26.292372419044,-26.192878552518,-26.0926812654677,-25.9924839784175,
-25.8927780012723,-25.7932147627291,-25.6935094233996,-25.5941248226654,
-25.4947729249228,-25.3954233013364,-25.2954604880255,-25.1959666213074,
-25.0957693347001,-24.9955720480928,-24.8958660714534,-24.796302833416,
-24.69659749396,-24.5972128937279,-24.4978609964848,-24.3985113733948,-24.2985485594881,
-24.1990546932537,-24.0988574055109,-23.9986601177681,-23.8989541408065,
-23.7993909024511,-23.6996855630751,-23.6003009625368,-23.5009490649927,
-23.4015994416071,-23.3016366280662,-23.2021427615525,-23.101945474498,
-23.0017481874434,-22.9411259921462),.UNSPECIFIED.);
#727=B_SPLINE_CURVE_WITH_KNOTS('',3,(#69805,#69806,#69807,#69808,#69809,
#69810,#69811,#69812,#69813,#69814,#69815,#69816,#69817,#69818,#69819,#69820,
#69821,#69822,#69823,#69824,#69825,#69826,#69827,#69828,#69829,#69830,#69831,
#69832,#69833,#69834,#69835,#69836,#69837,#69838,#69839,#69840,#69841,#69842,
#69843,#69844,#69845,#69846,#69847,#69848,#69849,#69850,#69851,#69852,#69853,
#69854,#69855,#69856,#69857,#69858,#69859,#69860,#69861,#69862,#69863,#69864,
#69865,#69866,#69867,#69868,#69869,#69870,#69871,#69872,#69873,#69874,#69875,
#69876,#69877,#69878,#69879,#69880,#69881,#69882,#69883,#69884,#69885,#69886,
#69887,#69888,#69889,#69890,#69891,#69892,#69893,#69894,#69895,#69896,#69897,
#69898,#69899,#69900,#69901,#69902,#69903,#69904,#69905,#69906,#69907,#69908,
#69909,#69910,#69911,#69912,#69913,#69914,#69915,#69916,#69917,#69918,#69919,
#69920,#69921,#69922,#69923,#69924,#69925,#69926,#69927,#69928,#69929,#69930,
#69931,#69932,#69933,#69934,#69935,#69936,#69937,#69938,#69939,#69940,#69941,
#69942,#69943,#69944,#69945,#69946,#69947,#69948,#69949,#69950,#69951,#69952,
#69953,#69954,#69955,#69956,#69957,#69958,#69959,#69960,#69961,#69962,#69963,
#69964,#69965,#69966,#69967,#69968,#69969,#69970,#69971,#69972,#69973,#69974,
#69975,#69976,#69977,#69978,#69979,#69980,#69981,#69982,#69983,#69984,#69985,
#69986,#69987,#69988,#69989,#69990,#69991,#69992,#69993,#69994,#69995,#69996,
#69997),.UNSPECIFIED.,.F.,.F.,(4,3,3,3,3,3,3,3,3,3,3,3,3,3,3,3,3,3,3,3,
3,3,3,3,3,3,3,3,3,3,3,3,3,3,3,3,3,3,3,3,3,3,3,3,3,3,3,3,3,3,3,3,3,3,3,3,
3,3,3,3,3,3,3,3,4),(-22.9411259917771,-22.8423298884581,-22.7436701923909,
-22.6451152123133,-22.5466155817799,-22.4481397693788,-22.3496562767237,
-22.2510711285813,-22.1524289845342,-22.0536236607553,-22.0048362571186,
-21.9051302830416,-21.8055670475646,-21.7058617074683,-21.6064771097735,
-21.5071252150533,-21.4077755944685,-21.3078127775499,-21.2083189137523,
-21.1081216202731,-21.0079243267939,-20.9082183489098,-20.8086551096547,
-20.7089497705065,-20.6095651691311,-20.5102132707748,-20.4108636466031,
-20.3109008340696,-20.2114069668409,-20.111209681655,-20.0110123964692,
-19.9113064098326,-19.8117431617508,-19.7120378248,-19.6126532144827,-19.5133013071616,
-19.4139516740144,-19.3139888720469,-19.2144949959087,-19.1142977310266,
-19.0141004661445,-18.9143945139796,-18.8148313004146,-18.7151259548402,
-18.6157413788972,-18.5163895058211,-18.4170399067437,-18.3170770640127,
-18.2175832211708,-18.1173858784953,-18.0171885358198,-17.917482543784,
-17.8179192905504,-17.7182139549185,-17.6188293400818,-17.5194774284872,
-17.420127791317,-17.3201649948615,-17.2206711153469,-17.120473860421,-17.0202766054951,
-16.9063917652444,-16.7929807702555,-16.6803704353785,-16.6579406851942),
 .UNSPECIFIED.);
#728=B_SPLINE_CURVE_WITH_KNOTS('',3,(#69999,#70000,#70001,#70002,#70003,
#70004,#70005,#70006,#70007,#70008,#70009,#70010,#70011,#70012,#70013,#70014,
#70015,#70016,#70017,#70018,#70019,#70020,#70021,#70022,#70023,#70024,#70025,
#70026,#70027,#70028,#70029,#70030,#70031,#70032,#70033,#70034,#70035,#70036,
#70037,#70038,#70039,#70040,#70041,#70042,#70043,#70044,#70045,#70046,#70047,
#70048,#70049,#70050,#70051,#70052,#70053,#70054,#70055,#70056,#70057,#70058,
#70059,#70060,#70061,#70062,#70063,#70064,#70065,#70066,#70067,#70068,#70069,
#70070,#70071,#70072,#70073,#70074,#70075,#70076,#70077,#70078,#70079,#70080,
#70081,#70082,#70083,#70084,#70085,#70086,#70087,#70088,#70089,#70090,#70091,
#70092,#70093,#70094,#70095,#70096,#70097,#70098,#70099,#70100,#70101,#70102,
#70103,#70104,#70105,#70106,#70107,#70108,#70109,#70110,#70111,#70112,#70113,
#70114,#70115,#70116,#70117,#70118,#70119,#70120,#70121,#70122,#70123,#70124,
#70125,#70126,#70127,#70128,#70129,#70130,#70131,#70132,#70133,#70134,#70135,
#70136,#70137,#70138,#70139,#70140,#70141,#70142,#70143,#70144,#70145,#70146,
#70147,#70148,#70149,#70150,#70151,#70152,#70153,#70154,#70155,#70156,#70157,
#70158,#70159,#70160,#70161,#70162,#70163,#70164,#70165,#70166,#70167,#70168,
#70169,#70170,#70171,#70172,#70173,#70174,#70175,#70176,#70177,#70178,#70179,
#70180,#70181,#70182,#70183,#70184,#70185,#70186,#70187,#70188,#70189,#70190,
#70191),.UNSPECIFIED.,.F.,.F.,(4,3,3,3,3,3,3,3,3,3,3,3,3,3,3,3,3,3,3,3,
3,3,3,3,3,3,3,3,3,3,3,3,3,3,3,3,3,3,3,3,3,3,3,3,3,3,3,3,3,3,3,3,3,3,3,3,
3,3,3,3,3,3,3,3,4),(-16.6579406849666,-16.5580934344199,-16.4582422444312,
-16.3583577075461,-16.258342944254,-16.1582524650089,-16.0579861672984,
-16.0233646751703,-15.923658905856,-15.8240958752626,-15.7243904839604,
-15.625006089955,-15.5256543980263,-15.4263049790649,-15.3263419205101,
-15.2268482534387,-15.1266504991422,-15.0264527448456,-14.9267465864787,
-14.8271831681702,-14.727477873964,-14.6280930982588,-14.5287410277233,
-14.4293912337434,-14.3294286289377,-14.2299345993823,-14.1297377069516,
-14.0295408145209,-13.9298343947855,-13.8302707099986,-13.7305654817733,
-13.6311804292655,-13.5318280786876,-13.4324780018285,-13.3325157224204,
-13.2330214060225,-13.1328251451094,-13.0326288841962,-12.9329246058058,
-12.833363068111,-12.7336573038311,-12.6342743966511,-12.5349241859803,
-12.4355762407301,-12.3356114190155,-12.2361191922637,-12.1359180730676,
-12.0357169538715,-11.9360090584454,-11.8364439118102,-11.7367390507773,
-11.6373525802036,-11.5379988310565,-11.4386473768989,-11.3386867885609,
-11.2391911604896,-11.1389980920182,-11.0388050235468,-10.9391546302479,
-10.8396437149114,-10.740241606817,-10.6409133704535,-10.5416298901773,
-10.4423315635812,-10.374755377787),.UNSPECIFIED.);
#729=B_SPLINE_CURVE_WITH_KNOTS('',3,(#70192,#70193,#70194,#70195,#70196,
#70197,#70198,#70199,#70200,#70201,#70202,#70203,#70204,#70205,#70206,#70207,
#70208,#70209,#70210,#70211,#70212,#70213,#70214,#70215,#70216,#70217,#70218,
#70219,#70220,#70221,#70222,#70223,#70224,#70225,#70226,#70227,#70228,#70229,
#70230,#70231,#70232,#70233,#70234,#70235,#70236,#70237,#70238,#70239,#70240,
#70241,#70242,#70243,#70244,#70245,#70246,#70247,#70248,#70249,#70250,#70251,
#70252,#70253,#70254,#70255,#70256,#70257,#70258,#70259,#70260,#70261,#70262,
#70263,#70264,#70265,#70266,#70267,#70268,#70269,#70270,#70271,#70272,#70273,
#70274,#70275,#70276,#70277,#70278,#70279,#70280,#70281,#70282,#70283,#70284,
#70285,#70286,#70287,#70288,#70289,#70290,#70291,#70292,#70293,#70294,#70295,
#70296,#70297,#70298,#70299,#70300,#70301,#70302,#70303,#70304,#70305,#70306,
#70307,#70308,#70309,#70310,#70311,#70312,#70313,#70314,#70315,#70316,#70317,
#70318,#70319,#70320,#70321,#70322,#70323,#70324,#70325,#70326,#70327,#70328,
#70329,#70330,#70331,#70332,#70333,#70334,#70335,#70336,#70337,#70338,#70339,
#70340,#70341,#70342,#70343,#70344,#70345,#70346,#70347,#70348,#70349,#70350,
#70351,#70352,#70353,#70354,#70355,#70356,#70357,#70358,#70359,#70360,#70361,
#70362,#70363,#70364,#70365,#70366,#70367,#70368,#70369,#70370,#70371,#70372,
#70373,#70374,#70375,#70376,#70377,#70378,#70379,#70380,#70381),
 .UNSPECIFIED.,.F.,.F.,(4,3,3,3,3,3,3,3,3,3,3,3,3,3,3,3,3,3,3,3,3,3,3,3,
3,3,3,3,3,3,3,3,3,3,3,3,3,3,3,3,3,3,3,3,3,3,3,3,3,3,3,3,3,3,3,3,3,3,3,3,
3,3,3,4),(-10.3747553775759,-10.2591101330065,-10.1422757994338,-10.0418930932221,
-9.94220069316546,-9.84265105744093,-9.74294232062298,-9.64357128606953,
-9.54423291077586,-9.44489674782431,-9.34491785159257,-9.24543715783758,
-9.14520916036746,-9.04498116289735,-8.9452563413951,-8.84567432613174,
-8.74597368943685,-8.64657061042831,-8.54720038699816,-8.44783261431723,
-8.34789176888108,-8.24838036694254,-8.14822479975759,-8.04806923257263,
-7.94834950285117,-7.84877225956233,-7.74907038989803,-7.64967128144482,
-7.55030472044975,-7.45094029914482,-7.35099454992059,-7.25148571213079,
-7.15132150718935,-7.05115730224791,-6.95155715616721,-6.85210001837247,
-6.75236818756631,-6.65308957648869,-6.55384339551515,-6.45459907611016,
-6.35451065006342,-6.25512001485721,-6.15468269339021,-6.0542453719232,
-5.95436295273983,-5.85462368971806,-5.75496240870311,-5.65540408598084,
-5.55587972319795,-5.45635912459957,-5.3566027038493,-5.25694323810271,
-5.15710663205714,-5.05733344159848,-4.95810738230795,-4.85902171181877,
-4.76004703457688,-4.66113224957557,-4.56224628842496,-4.46335811984981,
-4.36437074477041,-4.26533216177527,-4.16612178033553,-4.09157041827049),
 .UNSPECIFIED.);
#730=B_SPLINE_CURVE_WITH_KNOTS('',3,(#70384,#70385,#70386,#70387,#70388,
#70389,#70390,#70391,#70392,#70393,#70394,#70395,#70396,#70397,#70398,#70399,
#70400,#70401,#70402,#70403,#70404,#70405,#70406,#70407,#70408,#70409,#70410,
#70411,#70412,#70413,#70414,#70415,#70416,#70417),.UNSPECIFIED.,.F.,.F.,
(4,3,3,3,3,3,3,3,3,3,3,4),(71.1940098997199,71.2987359719931,71.4036584532844,
71.5038828067993,71.607596420869,71.7111684685388,71.8146363092789,71.9180371573734,
72.0214389095813,72.1248428520168,72.2283284120281,72.2566310325653),
 .UNSPECIFIED.);
#731=B_SPLINE_CURVE_WITH_KNOTS('',3,(#70419,#70420,#70421,#70422,#70423,
#70424,#70425,#70426,#70427,#70428,#70429,#70430,#70431,#70432,#70433,#70434,
#70435,#70436,#70437,#70438,#70439,#70440,#70441,#70442,#70443,#70444,#70445,
#70446,#70447,#70448,#70449,#70450,#70451,#70452,#70453,#70454,#70455,#70456,
#70457,#70458,#70459,#70460,#70461,#70462,#70463,#70464,#70465,#70466,#70467,
#70468,#70469,#70470,#70471,#70472,#70473,#70474,#70475,#70476,#70477,#70478,
#70479,#70480,#70481,#70482,#70483,#70484,#70485,#70486,#70487,#70488,#70489,
#70490,#70491,#70492,#70493,#70494,#70495,#70496,#70497,#70498,#70499,#70500,
#70501,#70502,#70503,#70504,#70505,#70506,#70507,#70508,#70509,#70510,#70511,
#70512,#70513,#70514,#70515,#70516,#70517,#70518,#70519,#70520,#70521,#70522,
#70523,#70524,#70525,#70526,#70527,#70528,#70529,#70530,#70531,#70532,#70533,
#70534,#70535,#70536,#70537,#70538,#70539,#70540,#70541,#70542),
 .UNSPECIFIED.,.F.,.F.,(4,3,3,3,3,3,3,3,3,3,3,3,3,3,3,3,3,3,3,3,3,3,3,3,
3,3,3,3,3,3,3,3,3,3,3,3,3,3,3,3,3,4),(72.2566310329874,72.3935845469085,
72.500794737124,72.6057786247621,72.7106055714104,72.8153098988276,72.9199487824371,
73.0245577431498,73.1291722582607,73.233897426931,73.3386840147705,73.4436520658765,
73.4977066674487,73.6025646586816,73.7072651358392,73.8118427580766,73.916354860038,
74.0208371502974,74.1253252938358,74.2299254067418,74.3345874987602,74.4394332502781,
74.4946185977734,74.5997737631742,74.7047712383462,74.8096441674778,74.9144503584131,
75.019225085812,75.1240035792051,75.2288889103067,75.3338337191025,75.4389553227352,
75.4915305280982,75.5954266638067,75.699148837704,75.8027739576774,75.9063390395231,
76.0098810172454,76.1135062214272,76.2171700260122,76.3210160814776,76.4156412590678),
 .UNSPECIFIED.);
#732=B_SPLINE_CURVE_WITH_KNOTS('',3,(#70545,#70546,#70547,#70548,#70549,
#70550,#70551,#70552,#70553,#70554,#70555,#70556,#70557,#70558,#70559,#70560,
#70561,#70562,#70563,#70564,#70565,#70566,#70567,#70568,#70569,#70570,#70571,
#70572,#70573,#70574,#70575,#70576,#70577,#70578,#70579,#70580,#70581,#70582,
#70583,#70584,#70585,#70586,#70587,#70588,#70589,#70590,#70591,#70592,#70593,
#70594,#70595,#70596,#70597,#70598,#70599,#70600,#70601,#70602,#70603,#70604,
#70605,#70606,#70607,#70608,#70609,#70610,#70611,#70612,#70613,#70614,#70615,
#70616,#70617,#70618,#70619,#70620,#70621,#70622,#70623,#70624,#70625,#70626,
#70627,#70628,#70629,#70630,#70631,#70632,#70633,#70634,#70635,#70636,#70637,
#70638,#70639,#70640,#70641,#70642,#70643,#70644,#70645,#70646,#70647,#70648,
#70649,#70650,#70651,#70652,#70653,#70654,#70655,#70656,#70657,#70658),
 .UNSPECIFIED.,.F.,.F.,(4,2,2,2,2,2,2,2,2,2,2,2,2,2,2,2,2,2,2,2,2,2,2,2,
2,2,2,2,2,2,2,2,2,2,2,2,2,2,2,2,2,2,2,2,2,2,2,2,2,2,2,2,2,2,2,2,4),(-1.83983945624295,
-1.83795397537346,-1.83573652513345,-1.82949843462936,-1.79178426308305,
-1.76296147372845,-1.75453667498902,-1.7486351304989,-1.74325086347128,
-1.73439828645192,-1.70725676385421,-1.66626641078697,-1.64910413130173,
-1.64422596375543,-1.64112570463183,-1.63844711672127,-1.63388566353806,
-1.61996621044673,-1.57569789052089,-1.55447720636594,-1.5471665286971,
-1.54207966082191,-1.53689493023208,-1.52907708541865,-1.50552707052677,
-1.46407541746046,-1.45269140278871,-1.444811032953,-1.44124797603105,-1.438683102287,
-1.43521655468152,-1.42867176437277,-1.4021719058181,-1.36984066765876,
-1.35111068785806,-1.343833908549,-1.33852386818394,-1.33287687770572,-1.32380860300783,
-1.27821947713036,-1.259205164698,-1.24799348242959,-1.2437417789513,-1.24073351187944,
-1.23729752844853,-1.23100354292647,-1.19611231183529,-1.16969535698436,
-1.15303889570976,-1.14607155381394,-1.14083464371401,-1.13512337698453,
-1.12562653131419,-1.0813412211916,-1.05133401436251,-1.04567072466869,
-1.0443153183833),.UNSPECIFIED.);
#733=B_SPLINE_CURVE_WITH_KNOTS('',3,(#70931,#70932,#70933,#70934,#70935,
#70936,#70937,#70938,#70939,#70940,#70941,#70942,#70943,#70944,#70945,#70946,
#70947,#70948,#70949,#70950,#70951,#70952,#70953,#70954,#70955,#70956,#70957,
#70958,#70959,#70960,#70961,#70962,#70963,#70964,#70965,#70966,#70967,#70968,
#70969,#70970,#70971,#70972,#70973,#70974,#70975,#70976,#70977,#70978,#70979,
#70980,#70981,#70982,#70983,#70984,#70985,#70986,#70987,#70988,#70989,#70990,
#70991,#70992,#70993,#70994,#70995,#70996,#70997,#70998,#70999,#71000,#71001,
#71002,#71003,#71004,#71005,#71006,#71007,#71008,#71009,#71010,#71011,#71012,
#71013,#71014,#71015),.UNSPECIFIED.,.F.,.F.,(4,3,3,3,3,3,3,3,3,3,3,3,3,
3,3,3,3,3,3,3,3,3,3,3,3,3,3,3,4),(-0.463803050843692,-0.449070703225483,
-0.42735479445911,-0.415189549046521,-0.410496202330004,-0.406058805975524,
-0.383404300327137,-0.364881814729665,-0.357461864595492,-0.352400732469066,
-0.329036435798896,-0.305267012368989,-0.287822011874325,-0.274662752749041,
-0.270903259004613,-0.246475346213267,-0.23536348442085,-0.211528359113113,
-0.187693233805376,-0.183684004614737,-0.159318899344364,-0.134503159343954,
-0.109395145221359,-0.0938232102629364,-0.0899531631052965,-0.0642046403497918,
-0.0384306169102492,-0.0132144355033025,0.),.UNSPECIFIED.);
#734=B_SPLINE_CURVE_WITH_KNOTS('',3,(#71020,#71021,#71022,#71023,#71024,
#71025,#71026,#71027,#71028,#71029,#71030,#71031,#71032,#71033,#71034,#71035,
#71036,#71037,#71038,#71039,#71040,#71041,#71042,#71043,#71044,#71045,#71046,
#71047,#71048,#71049,#71050,#71051,#71052,#71053,#71054,#71055,#71056,#71057,
#71058,#71059,#71060,#71061,#71062,#71063,#71064,#71065,#71066,#71067,#71068,
#71069,#71070,#71071,#71072,#71073,#71074,#71075,#71076,#71077,#71078,#71079,
#71080,#71081,#71082,#71083,#71084,#71085,#71086,#71087,#71088,#71089,#71090,
#71091,#71092,#71093,#71094,#71095,#71096,#71097,#71098,#71099,#71100,#71101,
#71102,#71103,#71104,#71105,#71106,#71107),.UNSPECIFIED.,.F.,.F.,(4,3,3,
3,3,3,3,3,3,3,3,3,3,3,3,3,3,3,3,3,3,3,3,3,3,3,3,3,3,4),(-0.45706977230884,
-0.444522365548672,-0.418899005513524,-0.405945758827233,-0.399313330176187,
-0.394631600643061,-0.369313518144253,-0.344021007921678,-0.340358828086956,
-0.336108374295373,-0.33175454364197,-0.307004890679168,-0.282783792225254,
-0.259078063661601,-0.248631875962901,-0.244428173588767,-0.220936136292426,
-0.211647058532859,-0.187586133721808,-0.164224619203416,-0.15876767775089,
-0.135435698638008,-0.112185513746461,-0.089130325712887,-0.0803330397173641,
-0.0766181939392614,-0.0541584315341221,-0.0320645162777776,-0.0106795002206658,
0.),.UNSPECIFIED.);
#735=B_SPLINE_CURVE_WITH_KNOTS('',3,(#71389,#71390,#71391,#71392),
 .UNSPECIFIED.,.F.,.F.,(4,4),(-0.0469525346883488,0.),.UNSPECIFIED.);
#736=B_SPLINE_CURVE_WITH_KNOTS('',3,(#71464,#71465,#71466,#71467,#71468,
#71469,#71470,#71471,#71472,#71473,#71474,#71475,#71476,#71477,#71478,#71479,
#71480,#71481,#71482,#71483,#71484,#71485,#71486,#71487,#71488,#71489,#71490,
#71491,#71492,#71493,#71494,#71495,#71496,#71497,#71498,#71499,#71500,#71501,
#71502,#71503,#71504,#71505,#71506,#71507,#71508,#71509,#71510,#71511,#71512,
#71513),.UNSPECIFIED.,.F.,.F.,(4,2,2,2,2,2,2,2,2,2,2,2,2,2,2,2,2,2,2,2,
2,2,2,2,4),(-0.122423255841805,-0.0999829706431865,-0.0946734372657195,
-0.0915496508705648,-0.0890650675485836,-0.0885992594482396,-0.0883573289906038,
-0.0882095118206766,-0.0881118884764039,-0.0880444119263917,-0.0877866006987234,
-0.087536118637217,-0.0872881890861582,-0.0870385562324885,-0.0823894050783034,
-0.0766946381380574,-0.0645769068426376,-0.0442003190552192,-0.0363184547158113,
-0.0337638212259385,-0.0322886353240006,-0.0306601413305012,-0.028154169115766,
-0.0251639879571378,-1.64669222008241E-5),.UNSPECIFIED.);
#737=B_SPLINE_CURVE_WITH_KNOTS('',3,(#71519,#71520,#71521,#71522,#71523,
#71524,#71525,#71526,#71527,#71528,#71529,#71530,#71531,#71532,#71533,#71534,
#71535,#71536,#71537,#71538,#71539,#71540,#71541,#71542,#71543,#71544,#71545,
#71546,#71547,#71548,#71549,#71550,#71551,#71552,#71553,#71554,#71555,#71556,
#71557,#71558,#71559,#71560,#71561,#71562,#71563,#71564,#71565,#71566,#71567,
#71568,#71569,#71570,#71571,#71572,#71573,#71574,#71575,#71576,#71577,#71578,
#71579,#71580,#71581,#71582,#71583,#71584,#71585,#71586,#71587,#71588,#71589,
#71590,#71591,#71592,#71593,#71594,#71595,#71596,#71597,#71598,#71599,#71600,
#71601,#71602,#71603,#71604,#71605,#71606,#71607,#71608,#71609,#71610,#71611,
#71612,#71613,#71614,#71615,#71616,#71617,#71618,#71619,#71620,#71621,#71622,
#71623,#71624,#71625,#71626,#71627,#71628,#71629,#71630,#71631,#71632,#71633,
#71634,#71635,#71636,#71637,#71638,#71639,#71640,#71641,#71642,#71643,#71644,
#71645,#71646,#71647,#71648,#71649,#71650,#71651,#71652,#71653,#71654,#71655,
#71656,#71657,#71658,#71659,#71660,#71661,#71662,#71663,#71664,#71665,#71666,
#71667,#71668,#71669,#71670,#71671,#71672,#71673,#71674,#71675,#71676,#71677,
#71678,#71679,#71680,#71681,#71682,#71683,#71684,#71685,#71686,#71687,#71688,
#71689,#71690,#71691,#71692,#71693,#71694,#71695,#71696,#71697,#71698,#71699,
#71700,#71701,#71702,#71703,#71704,#71705,#71706,#71707,#71708,#71709,#71710,
#71711,#71712),.UNSPECIFIED.,.F.,.F.,(4,2,2,2,2,2,2,2,2,2,2,2,2,2,2,2,2,
2,2,2,2,2,2,2,2,2,2,2,2,2,2,2,2,2,2,2,2,2,2,2,2,2,2,2,2,2,2,2,2,2,2,2,2,
2,2,2,2,2,2,2,2,2,2,2,2,2,2,2,2,2,2,2,2,2,2,2,2,2,2,2,2,2,2,2,2,2,2,2,2,
2,2,2,2,2,2,2,4),(-0.864476967535523,-0.863889634574054,-0.854675797726696,
-0.851995417487591,-0.850332462543021,-0.848693725647681,-0.846126694304765,
-0.837342669241336,-0.817949626733269,-0.799856452191916,-0.795213179187172,
-0.792256402525947,-0.78944606020123,-0.785566598692449,-0.775646096380797,
-0.759356663236241,-0.739509218581221,-0.73591332044633,-0.734035765386652,
-0.732479759907595,-0.730418678303376,-0.725701864215524,-0.718740184720392,
-0.689763722041757,-0.681111783649308,-0.677684159242237,-0.67486735084454,
-0.671971200872892,-0.667628387988473,-0.65335413729465,-0.639005936404083,
-0.621515501088468,-0.618529978947483,-0.616801368435175,-0.615206389194971,
-0.612861067751976,-0.606175308750074,-0.594406778078637,-0.567202520344681,
-0.561989034076196,-0.558914841376038,-0.556146221350687,-0.552552000476236,
-0.544551840079185,-0.532961386299957,-0.51022384185869,-0.503511592953835,
-0.50109781664782,-0.499506041170944,-0.497806124230549,-0.494954209620038,
-0.481789387126653,-0.45255284874405,-0.446110537707706,-0.442751740029425,
-0.440002483373519,-0.436769946478657,-0.430772981453676,-0.42304054345816,
-0.401718761825549,-0.38765749554838,-0.384728284700792,-0.383011709734159,
-0.38141001687277,-0.379029680187536,-0.372057204892285,-0.35944246953021,
-0.333798244484927,-0.328467102130281,-0.325339129525335,-0.322855780507222,
-0.319491609711317,-0.31280977049461,-0.295705363046698,-0.273692192348844,
-0.268952640071077,-0.266909685660323,-0.265352735250808,-0.263489349530779,
-0.259848259621297,-0.245637777556396,-0.218799199836102,-0.212365474480367,
-0.209009532762126,-0.206261938931301,-0.203030665317132,-0.197034248549036,
-0.189301661782186,-0.167974324458412,-0.153915929666823,-0.150987715178024,
-0.149271939936827,-0.147670744624839,-0.145291645111244,-0.138328368373508,
-0.125743539426254,-0.122423255841805),.UNSPECIFIED.);
#738=B_SPLINE_CURVE_WITH_KNOTS('',3,(#71716,#71717,#71718,#71719,#71720,
#71721,#71722,#71723,#71724,#71725,#71726,#71727,#71728,#71729,#71730,#71731),
 .UNSPECIFIED.,.F.,.F.,(4,3,3,3,3,4),(15.2092144196076,15.3360303631197,
15.4631229098697,15.5906899826816,15.6658502388533,15.707963267949),
 .UNSPECIFIED.);
#739=B_SPLINE_CURVE_WITH_KNOTS('',3,(#71732,#71733,#71734,#71735,#71736,
#71737,#71738,#71739,#71740,#71741,#71742,#71743,#71744,#71745,#71746,#71747,
#71748,#71749,#71750,#71751,#71752,#71753,#71754,#71755,#71756,#71757,#71758,
#71759,#71760,#71761,#71762,#71763,#71764,#71765,#71766,#71767,#71768,#71769,
#71770,#71771,#71772,#71773,#71774,#71775,#71776,#71777,#71778,#71779,#71780,
#71781,#71782,#71783,#71784,#71785,#71786,#71787,#71788,#71789,#71790,#71791,
#71792,#71793,#71794,#71795,#71796,#71797,#71798,#71799,#71800,#71801,#71802,
#71803,#71804,#71805,#71806,#71807,#71808,#71809,#71810,#71811,#71812,#71813,
#71814,#71815,#71816,#71817,#71818,#71819,#71820,#71821,#71822,#71823,#71824,
#71825,#71826,#71827,#71828,#71829,#71830,#71831,#71832,#71833,#71834,#71835,
#71836,#71837,#71838,#71839,#71840,#71841,#71842,#71843,#71844,#71845,#71846,
#71847,#71848,#71849,#71850,#71851,#71852,#71853,#71854,#71855,#71856,#71857,
#71858,#71859,#71860,#71861,#71862,#71863,#71864,#71865,#71866,#71867,#71868,
#71869,#71870,#71871,#71872,#71873,#71874,#71875,#71876,#71877,#71878,#71879,
#71880,#71881,#71882),.UNSPECIFIED.,.F.,.F.,(4,3,3,3,3,3,3,3,3,3,3,3,3,
3,3,3,3,3,3,3,3,3,3,3,3,3,3,3,3,3,3,3,3,3,3,3,3,3,3,3,3,3,3,3,3,3,3,3,3,
3,4),(15.7079642759245,15.8269893519292,15.9458440195906,16.0645825459371,
16.1832590062766,16.3020151623243,16.4208033607179,16.5398240072109,16.65421914787,
16.7777652614971,16.8976025282206,17.0173252415981,17.1369855788367,17.2566356083551,
17.376407960716,17.4962551100189,17.6163141716932,17.6425880568867,17.7661341705138,
17.8856871273224,18.0051210589497,18.124488751243,18.2438428753474,18.3633167375596,
18.4828635828783,18.6026226744951,18.6309569659034,18.7545030795305,18.8741702459772,
18.9937195103916,19.113203420604,19.2326744112691,19.3522652237597,19.4719291891606,
19.5918044907923,19.6193258749201,19.7428719885472,19.8625446199524,19.9820997791249,
20.1015900018609,20.2210677113655,20.3406657945147,20.4603373617903,20.5802206731859,
20.6076947839369,20.7275367997089,20.8471946066813,20.9667304809259,21.0861923026828,
21.2056842522114,21.2859961957582),.UNSPECIFIED.);
#740=B_SPLINE_CURVE_WITH_KNOTS('',3,(#71887,#71888,#71889,#71890,#71891,
#71892,#71893,#71894,#71895,#71896,#71897,#71898,#71899,#71900,#71901,#71902,
#71903,#71904,#71905,#71906,#71907,#71908,#71909,#71910,#71911,#71912,#71913,
#71914,#71915,#71916,#71917,#71918,#71919,#71920,#71921,#71922,#71923,#71924,
#71925,#71926,#71927,#71928,#71929,#71930,#71931,#71932,#71933,#71934,#71935,
#71936,#71937,#71938,#71939,#71940,#71941,#71942,#71943,#71944,#71945,#71946,
#71947,#71948,#71949,#71950,#71951,#71952,#71953,#71954,#71955,#71956,#71957,
#71958,#71959,#71960,#71961,#71962,#71963,#71964,#71965,#71966,#71967,#71968,
#71969,#71970,#71971,#71972,#71973,#71974,#71975,#71976,#71977,#71978,#71979,
#71980,#71981,#71982,#71983,#71984,#71985,#71986,#71987,#71988,#71989,#71990,
#71991,#71992,#71993,#71994,#71995,#71996,#71997,#71998,#71999,#72000,#72001,
#72002,#72003,#72004,#72005,#72006,#72007,#72008,#72009,#72010,#72011,#72012,
#72013,#72014,#72015,#72016,#72017,#72018,#72019,#72020,#72021,#72022,#72023,
#72024,#72025,#72026,#72027,#72028,#72029,#72030,#72031,#72032,#72033,#72034,
#72035,#72036,#72037,#72038,#72039,#72040,#72041,#72042,#72043,#72044,#72045,
#72046,#72047,#72048,#72049,#72050,#72051,#72052,#72053,#72054,#72055,#72056,
#72057,#72058,#72059,#72060,#72061,#72062,#72063,#72064,#72065,#72066,#72067,
#72068,#72069,#72070,#72071,#72072,#72073,#72074),.UNSPECIFIED.,.F.,.F.,
(4,2,2,2,2,2,2,2,2,2,2,2,2,2,2,2,2,2,2,2,2,2,2,2,2,2,2,2,2,2,2,2,2,2,2,
2,2,2,2,2,2,2,2,2,2,2,2,2,2,2,2,2,2,2,2,2,2,2,2,2,2,2,2,2,2,2,2,2,2,2,2,
2,2,2,2,2,2,2,2,2,2,2,2,2,2,2,2,2,2,2,2,2,2,4),(-1.60658442102956,-1.60224560786445,
-1.58703238171082,-1.5734536786702,-1.55779363519776,-1.55404776376174,
-1.55216286224401,-1.55060743210901,-1.54855577362445,-1.54389533409889,
-1.5370509807898,-1.50958833980546,-1.49965316887026,-1.49566917207978,
-1.49286872478607,-1.48994894568779,-1.48548876262572,-1.46964021552359,
-1.46491862458907,-1.44377072705897,-1.43814235132304,-1.43588239170092,
-1.43430177257987,-1.43253826107621,-1.42938893998371,-1.4115371691861,
-1.38556738688697,-1.38026768918793,-1.37714661872821,-1.37438643815279,
-1.37087330911222,-1.36335832702959,-1.35278004079731,-1.34822560070426,
-1.32739842198097,-1.32139715254891,-1.31907787404184,-1.3175030806732,
-1.31577003692568,-1.31276400765762,-1.29344874239736,-1.26892156514752,
-1.26349525637699,-1.26034708690077,-1.25761709893635,-1.25416009797896,
-1.24696597825883,-1.23702677495449,-1.22302998282919,-1.20717547508139,
-1.20341685256838,-1.20152961580493,-1.19998948005837,-1.19795050560538,
-1.19336344955988,-1.1674264216449,-1.15039868698494,-1.14578342053174,
-1.14283242100576,-1.14001913252266,-1.1361217811602,-1.12606630931722,
-1.10939123146061,-1.09016198578807,-1.08653429012839,-1.08465013995714,
-1.08309486788521,-1.08104281701865,-1.0763790917414,-1.06952757044592,
-1.04196987920764,-1.03211911150126,-1.0281480061105,-1.02535007697864,
-1.02242733268321,-1.0179511079645,-1.00185202779994,-0.996794935981721,
-0.9745544455494,-0.97005663100529,-0.968054434720027,-0.966500232781827,
-0.964603936085443,-0.960798565106953,-0.955619183957662,-0.94093791664804,
-0.918459327905157,-0.912954086788694,-0.909789115755706,-0.907034914308456,
-0.903589053834301,-0.896457126838998,-0.886639159095262,-0.864476967535523),
 .UNSPECIFIED.);
#741=B_SPLINE_CURVE_WITH_KNOTS('',3,(#72076,#72077,#72078,#72079,#72080,
#72081,#72082,#72083,#72084,#72085,#72086,#72087,#72088,#72089,#72090,#72091,
#72092,#72093,#72094),.UNSPECIFIED.,.F.,.F.,(4,3,3,3,3,3,4),(21.2859961957582,
21.4056047705331,21.525437818082,21.5960636929536,21.7289761291196,21.8610704963778,
21.9911485745023),.UNSPECIFIED.);
#742=B_SPLINE_CURVE_WITH_KNOTS('',3,(#72095,#72096,#72097,#72098,#72099,
#72100,#72101,#72102,#72103,#72104,#72105,#72106,#72107,#72108,#72109,#72110,
#72111,#72112,#72113,#72114,#72115,#72116,#72117,#72118,#72119,#72120,#72121,
#72122,#72123,#72124,#72125,#72126,#72127,#72128,#72129,#72130,#72131,#72132,
#72133,#72134,#72135,#72136,#72137,#72138,#72139,#72140,#72141,#72142,#72143,
#72144,#72145,#72146,#72147,#72148,#72149,#72150,#72151,#72152,#72153,#72154,
#72155,#72156,#72157,#72158,#72159,#72160,#72161,#72162,#72163,#72164,#72165,
#72166,#72167,#72168,#72169,#72170,#72171,#72172,#72173,#72174,#72175,#72176,
#72177,#72178,#72179,#72180,#72181,#72182,#72183,#72184,#72185,#72186,#72187,
#72188,#72189,#72190,#72191,#72192,#72193,#72194,#72195,#72196,#72197,#72198,
#72199,#72200,#72201,#72202,#72203,#72204,#72205,#72206,#72207,#72208,#72209,
#72210,#72211,#72212,#72213,#72214,#72215,#72216,#72217,#72218,#72219,#72220,
#72221,#72222,#72223,#72224,#72225,#72226,#72227,#72228,#72229,#72230,#72231,
#72232,#72233,#72234,#72235,#72236,#72237,#72238,#72239,#72240,#72241,#72242,
#72243,#72244,#72245,#72246,#72247,#72248),.UNSPECIFIED.,.F.,.F.,(4,3,3,
3,3,3,3,3,3,3,3,3,3,3,3,3,3,3,3,3,3,3,3,3,3,3,3,3,3,3,3,3,3,3,3,3,3,3,3,
3,3,3,3,3,3,3,3,3,3,3,3,4),(21.9911485751286,22.1121823813204,22.2333768389223,
22.3546485764804,22.4762007130821,22.5844326019703,22.7079787155974,22.8276354609262,
22.9471744316454,23.0666481973393,23.1861092145952,23.3056903830167,23.425344887959,
23.5452110906813,23.572801510987,23.6963476246141,23.816001439762,23.9355374275848,
24.055008163879,24.1744661113735,24.2940441733778,24.4136955472502,24.5335586139338,
24.5611704200037,24.6847165336308,24.8043720806431,24.9239098215702,25.0433823285495,
25.1628420606792,25.2824219145154,25.4020750862542,25.5219399418086,25.5495393290204,
25.6730854426475,25.7927407520977,25.9122782564462,26.0317505283277,26.1512100273392,
26.2707896527571,26.3904425986054,26.5103072341942,26.5379082380372,26.6614543516643,
26.7811093846743,26.9006466071252,27.0201185922384,27.1395778001901,27.2591571303837,
27.378809778265,27.4986741148352,27.5262771470539,27.5698739474015),
 .UNSPECIFIED.);
#743=B_SPLINE_CURVE_WITH_KNOTS('',3,(#72253,#72254,#72255,#72256,#72257,
#72258,#72259,#72260,#72261,#72262,#72263,#72264,#72265,#72266,#72267,#72268,
#72269,#72270,#72271,#72272,#72273,#72274,#72275,#72276,#72277,#72278,#72279,
#72280,#72281,#72282,#72283,#72284,#72285,#72286,#72287,#72288,#72289,#72290,
#72291,#72292,#72293,#72294,#72295,#72296,#72297,#72298,#72299,#72300,#72301,
#72302,#72303,#72304,#72305,#72306,#72307,#72308,#72309,#72310,#72311,#72312,
#72313,#72314,#72315,#72316,#72317,#72318,#72319,#72320,#72321,#72322,#72323,
#72324,#72325,#72326,#72327,#72328,#72329,#72330,#72331,#72332,#72333,#72334,
#72335,#72336,#72337,#72338,#72339,#72340,#72341,#72342,#72343,#72344,#72345,
#72346,#72347,#72348,#72349,#72350,#72351,#72352,#72353,#72354,#72355,#72356,
#72357,#72358,#72359,#72360,#72361,#72362,#72363,#72364,#72365,#72366,#72367,
#72368,#72369,#72370,#72371,#72372,#72373,#72374,#72375,#72376,#72377,#72378,
#72379,#72380,#72381,#72382,#72383,#72384,#72385,#72386,#72387,#72388,#72389,
#72390,#72391,#72392,#72393,#72394,#72395,#72396,#72397,#72398,#72399,#72400,
#72401,#72402,#72403,#72404,#72405,#72406,#72407,#72408,#72409,#72410,#72411,
#72412,#72413,#72414,#72415,#72416,#72417,#72418,#72419,#72420,#72421,#72422,
#72423,#72424,#72425,#72426,#72427,#72428,#72429,#72430,#72431,#72432,#72433,
#72434,#72435,#72436,#72437,#72438,#72439,#72440),.UNSPECIFIED.,.F.,.F.,
(4,2,2,2,2,2,2,2,2,2,2,2,2,2,2,2,2,2,2,2,2,2,2,2,2,2,2,2,2,2,2,2,2,2,2,
2,2,2,2,2,2,2,2,2,2,2,2,2,2,2,2,2,2,2,2,2,2,2,2,2,2,2,2,2,2,2,2,2,2,2,2,
2,2,2,2,2,2,2,2,2,2,2,2,2,2,2,2,2,2,2,2,2,2,4),(-2.34888331669559,-2.34746415791081,
-2.33323501160312,-2.31883357825542,-2.31447996064606,-2.31158122471084,
-2.30876529751478,-2.30534295492001,-2.29673264795989,-2.26767399338713,
-2.26070236836814,-2.25598079788759,-2.25391860690272,-2.25236218744963,
-2.25048461817488,-2.24689008239023,-2.22702347649825,-2.21075478489965,
-2.20084034995889,-2.19696105929532,-2.19415012164969,-2.19119206971483,
-2.18654543399744,-2.16838822503978,-2.14901876408084,-2.14023740420851,
-2.13766996337183,-2.13603081806866,-2.13436724699173,-2.13168561909365,
-2.12246215236684,-2.08921550586199,-2.08251215181169,-2.079143853725,-2.07665996373838,
-2.07353461166598,-2.0682163769144,-2.04238737122532,-2.02984770173124,
-2.02289939478388,-2.02052184400997,-2.0189206744297,-2.01720292774031,
-2.0142692296875,-2.00005059485172,-1.97886294912189,-1.96745217568005,
-1.96338785874221,-1.96054463947029,-1.95797827887605,-1.95452846178216,
-1.94568771125277,-1.91690388219679,-1.90995277786879,-1.9052410964534,
-1.9031806101222,-1.90162436717276,-1.89974565078447,-1.89603211724303,
-1.87774127830691,-1.86047504687243,-1.85021759831574,-1.84629323668752,
-1.84347475358181,-1.84053085849146,-1.83595321550095,-1.81985346040924,
-1.79870863276069,-1.78956971120447,-1.78697104487409,-1.78532531851077,
-1.78366900536073,-1.78102099926561,-1.77210934584716,-1.7390312587843,
-1.73197807340727,-1.72854589354364,-1.72579214161752,-1.72261617274575,
-1.71706132757492,-1.697428494358,-1.68064602341512,-1.67246658763078,-1.66995596791786,
-1.66832875544202,-1.66665124653546,-1.66390430137832,-1.65382627828294,
-1.62704668560031,-1.61648688426369,-1.61252441522423,-1.60969960464756,
-1.60676733176927,-1.60658442102956),.UNSPECIFIED.);
#744=B_SPLINE_CURVE_WITH_KNOTS('',3,(#72442,#72443,#72444,#72445,#72446,
#72447,#72448,#72449,#72450,#72451,#72452,#72453,#72454,#72455,#72456,#72457,
#72458,#72459,#72460),.UNSPECIFIED.,.F.,.F.,(4,3,3,3,3,3,4),(27.5698739474015,
27.6882231470401,27.806414976291,27.924540614238,28.0426184394307,28.1607993193961,
28.2743338823079),.UNSPECIFIED.);
#745=B_SPLINE_CURVE_WITH_KNOTS('',3,(#72461,#72462,#72463,#72464,#72465,
#72466,#72467,#72468,#72469,#72470,#72471,#72472,#72473,#72474,#72475,#72476,
#72477,#72478,#72479,#72480,#72481,#72482,#72483,#72484,#72485,#72486,#72487,
#72488,#72489,#72490,#72491,#72492,#72493,#72494,#72495,#72496,#72497,#72498,
#72499,#72500,#72501,#72502,#72503,#72504,#72505,#72506,#72507,#72508,#72509,
#72510,#72511,#72512,#72513,#72514,#72515,#72516,#72517,#72518,#72519,#72520,
#72521,#72522,#72523,#72524,#72525,#72526,#72527,#72528,#72529,#72530,#72531,
#72532,#72533,#72534,#72535,#72536,#72537,#72538,#72539,#72540,#72541,#72542,
#72543,#72544,#72545,#72546,#72547,#72548,#72549,#72550,#72551,#72552,#72553,
#72554,#72555,#72556,#72557,#72558,#72559,#72560,#72561,#72562,#72563,#72564,
#72565,#72566,#72567,#72568,#72569,#72570,#72571,#72572,#72573,#72574,#72575,
#72576,#72577,#72578,#72579,#72580,#72581,#72582,#72583,#72584,#72585,#72586,
#72587,#72588,#72589,#72590,#72591,#72592,#72593,#72594,#72595,#72596,#72597,
#72598,#72599,#72600,#72601,#72602,#72603,#72604,#72605,#72606,#72607,#72608,
#72609,#72610,#72611,#72612,#72613,#72614),.UNSPECIFIED.,.F.,.F.,(4,3,3,
3,3,3,3,3,3,3,3,3,3,3,3,3,3,3,3,3,3,3,3,3,3,3,3,3,3,3,3,3,3,3,3,3,3,3,3,
3,3,3,3,3,3,3,3,3,3,3,3,4),(28.2743338827468,28.4302483032949,28.5146460560706,
28.6381921696977,28.7578473617235,28.8773847457103,28.9968568945427,29.1163162680635,
29.2358957653182,29.3555485813052,29.4754130858408,29.5030149650873,29.6265610787144,
29.7462162465358,29.865753605776,29.985225729371,30.1046850772144,30.2242645483331,
30.3439173378884,30.4637818158228,30.491383874104,30.6149299877311,30.7345851783267,
30.8541225606624,30.9735947076261,31.0930540790636,31.2126335739322,31.3322863873531,
31.4521508890851,31.4797527831207,31.6032988967478,31.7229540808906,31.842491456729,
31.9619635971646,32.0814229620567,32.2010024504039,32.3206552573107,32.4405197526041,
32.4681216921375,32.5916678057646,32.7113229880375,32.830860361955,32.9503325004226,
33.0697918633034,33.1893713495904,33.3090241544062,33.4288886475844,33.4564906011542,
33.5763334259412,33.6960035678199,33.8155402609469,33.8531165668701),
 .UNSPECIFIED.);
#746=B_SPLINE_CURVE_WITH_KNOTS('',3,(#72619,#72620,#72621,#72622,#72623,
#72624,#72625,#72626,#72627,#72628,#72629,#72630,#72631,#72632,#72633,#72634,
#72635,#72636,#72637,#72638,#72639,#72640,#72641,#72642,#72643,#72644,#72645,
#72646,#72647,#72648,#72649,#72650,#72651,#72652,#72653,#72654,#72655,#72656,
#72657,#72658,#72659,#72660,#72661,#72662,#72663,#72664,#72665,#72666,#72667,
#72668,#72669,#72670,#72671,#72672,#72673,#72674,#72675,#72676,#72677,#72678,
#72679,#72680,#72681,#72682,#72683,#72684,#72685,#72686,#72687,#72688,#72689,
#72690,#72691,#72692,#72693,#72694,#72695,#72696,#72697,#72698,#72699,#72700,
#72701,#72702,#72703,#72704,#72705,#72706,#72707,#72708,#72709,#72710,#72711,
#72712,#72713,#72714,#72715,#72716,#72717,#72718,#72719,#72720,#72721,#72722,
#72723,#72724,#72725,#72726,#72727,#72728,#72729,#72730,#72731,#72732,#72733,
#72734,#72735,#72736,#72737,#72738,#72739,#72740,#72741,#72742,#72743,#72744,
#72745,#72746,#72747,#72748,#72749,#72750,#72751,#72752,#72753,#72754,#72755,
#72756,#72757,#72758,#72759,#72760,#72761,#72762,#72763,#72764,#72765,#72766,
#72767,#72768,#72769,#72770,#72771,#72772,#72773,#72774,#72775,#72776,#72777,
#72778,#72779,#72780,#72781,#72782,#72783,#72784,#72785,#72786,#72787,#72788,
#72789,#72790,#72791,#72792,#72793,#72794,#72795,#72796,#72797,#72798,#72799,
#72800,#72801,#72802,#72803,#72804,#72805,#72806,#72807,#72808,#72809,#72810,
#72811,#72812,#72813,#72814),.UNSPECIFIED.,.F.,.F.,(4,2,2,2,2,2,2,2,2,2,
2,2,2,2,2,2,2,2,2,2,2,2,2,2,2,2,2,2,2,2,2,2,2,2,2,2,2,2,2,2,2,2,2,2,2,2,
2,2,2,2,2,2,2,2,2,2,2,2,2,2,2,2,2,2,2,2,2,2,2,2,2,2,2,2,2,2,2,2,2,2,2,2,
2,2,2,2,2,2,2,2,2,2,2,2,2,2,2,4),(-3.09104302557684,-3.07869878069296,-3.07412504340968,
-3.07208831983924,-3.07068215664841,-3.06885526655861,-3.06549798479306,
-3.04262401148008,-3.0280981740137,-3.02175927212834,-3.01659361681389,
-3.01352909921991,-3.01075789248408,-3.00720469848718,-2.99922146495274,
-2.97399056061458,-2.96389059346649,-2.95971844085165,-2.95648392273833,
-2.95470259192764,-2.95312795377868,-2.95090658683942,-2.94555301107947,
-2.92419057452729,-2.91935931921853,-2.90876099397085,-2.90123549326599,
-2.89772054260378,-2.89496012383153,-2.89184003507607,-2.88654517357406,
-2.86050324433681,-2.84808737661496,-2.84118059236707,-2.83880815862638,
-2.83720807092551,-2.83548884548837,-2.83254766854845,-2.81797261796609,
-2.79706805317956,-2.78573137778136,-2.78167585709646,-2.77883448728534,
-2.77626699321988,-2.77281139923282,-2.7638986200414,-2.73519821507583,
-2.72825392149456,-2.72354566748474,-2.72148590315028,-2.71992987522484,
-2.71805101371321,-2.71433606945545,-2.69927560193353,-2.68636556568058,
-2.67531891311813,-2.66757506820202,-2.66402285119664,-2.66125840988038,
-2.65815994273199,-2.65283077653672,-2.62653116316866,-2.61425677167171,
-2.60739724243166,-2.60503033515024,-2.60343116695458,-2.60170978947573,
-2.59875900737969,-2.58304110008063,-2.56299801580036,-2.55189338449423,
-2.54786463471413,-2.54502794492976,-2.54211332216001,-2.537679496406,-2.52405674287668,
-2.50061017391584,-2.49106678474372,-2.48843487079744,-2.48678210911646,
-2.4853302148218,-2.48289901835696,-2.4760552473746,-2.45345968718261,-2.44189573564967,
-2.43390671610912,-2.4303137324783,-2.42754459258856,-2.42446832179646,
-2.41924754495441,-2.3920615076513,-2.38026370220506,-2.37356726627186,
-2.37122014142609,-2.36962452179197,-2.36789591906688,-2.36491160636841,
-2.34888331669559),.UNSPECIFIED.);
#747=B_SPLINE_CURVE_WITH_KNOTS('',3,(#72816,#72817,#72818,#72819,#72820,
#72821,#72822,#72823,#72824,#72825,#72826,#72827,#72828,#72829,#72830,#72831,
#72832,#72833,#72834),.UNSPECIFIED.,.F.,.F.,(4,3,3,3,3,3,4),(33.8531165668701,
33.9725797586397,34.0921356915886,34.2117312225598,34.3315652548219,34.4448595101709,
34.5575191894876),.UNSPECIFIED.);
#748=B_SPLINE_CURVE_WITH_KNOTS('',3,(#72835,#72836,#72837,#72838,#72839,
#72840,#72841,#72842,#72843,#72844,#72845,#72846,#72847,#72848,#72849,#72850,
#72851,#72852,#72853,#72854,#72855,#72856,#72857,#72858,#72859,#72860,#72861,
#72862,#72863,#72864,#72865,#72866,#72867,#72868,#72869,#72870,#72871,#72872,
#72873,#72874,#72875,#72876,#72877,#72878,#72879,#72880,#72881,#72882,#72883,
#72884,#72885,#72886,#72887,#72888,#72889,#72890,#72891,#72892,#72893,#72894,
#72895,#72896,#72897,#72898,#72899,#72900,#72901,#72902,#72903,#72904,#72905,
#72906,#72907,#72908,#72909,#72910,#72911,#72912,#72913,#72914,#72915,#72916,
#72917,#72918,#72919,#72920,#72921,#72922,#72923,#72924,#72925,#72926,#72927,
#72928,#72929,#72930,#72931,#72932,#72933,#72934,#72935,#72936,#72937,#72938,
#72939,#72940,#72941,#72942,#72943,#72944,#72945,#72946,#72947,#72948,#72949,
#72950,#72951,#72952,#72953,#72954,#72955,#72956,#72957,#72958,#72959,#72960,
#72961,#72962,#72963,#72964,#72965,#72966,#72967,#72968,#72969,#72970,#72971,
#72972,#72973,#72974,#72975,#72976,#72977,#72978,#72979,#72980,#72981,#72982,
#72983,#72984,#72985,#72986,#72987,#72988),.UNSPECIFIED.,.F.,.F.,(4,3,3,
3,3,3,3,3,3,3,3,3,3,3,3,3,3,3,3,3,3,3,3,3,3,3,3,3,3,3,3,3,3,3,3,3,3,3,3,
3,3,3,3,3,3,3,3,3,3,3,3,4),(34.55751919,34.675703821994,34.7937403930487,
34.9116842733924,35.0295906618769,35.1475953577675,35.265656218042,35.3839289477292,
35.4332284191876,35.5567745328147,35.6764297165833,35.7959670920215,35.9154392320316,
36.0348985964736,36.1544780843377,36.2741308907417,36.3939953855082,36.4215973282043,
36.5451434418314,36.6647986258637,36.7843360015699,36.9038081418515,37.0232675065683,
37.1428469947097,37.2624998013925,37.3823642964378,37.409966237221,37.5335123508481,
37.6531675347659,37.7727049103562,37.8921770505211,38.0116364151202,38.1312159031439,
38.2508687097089,38.3707332046372,38.3983351462378,38.5218812598649,38.6415364437821,
38.7610738193715,38.8805459595352,39.000005324133,39.1195848121547,39.2392376187173,
39.3591021136428,39.3867040552545,39.5065507243149,39.6262160664111,39.7457528850742,
39.8652414842152,39.9847042607615,40.1042406011651,40.1354661882622),
 .UNSPECIFIED.);
#749=B_SPLINE_CURVE_WITH_KNOTS('',3,(#72994,#72995,#72996,#72997,#72998,
#72999,#73000,#73001,#73002,#73003,#73004,#73005,#73006,#73007,#73008,#73009,
#73010,#73011,#73012,#73013,#73014,#73015,#73016,#73017,#73018,#73019,#73020,
#73021,#73022,#73023,#73024,#73025,#73026,#73027,#73028,#73029,#73030,#73031,
#73032,#73033,#73034,#73035,#73036,#73037,#73038,#73039,#73040,#73041,#73042,
#73043,#73044,#73045,#73046,#73047,#73048,#73049,#73050,#73051,#73052,#73053,
#73054,#73055,#73056,#73057,#73058,#73059,#73060,#73061,#73062,#73063,#73064,
#73065,#73066,#73067,#73068,#73069,#73070,#73071,#73072,#73073,#73074,#73075,
#73076,#73077,#73078,#73079,#73080,#73081,#73082,#73083,#73084,#73085,#73086,
#73087,#73088,#73089,#73090,#73091,#73092,#73093,#73094,#73095,#73096,#73097,
#73098,#73099,#73100,#73101,#73102,#73103,#73104,#73105,#73106,#73107,#73108,
#73109,#73110,#73111,#73112,#73113,#73114,#73115,#73116,#73117,#73118,#73119,
#73120,#73121,#73122,#73123,#73124,#73125,#73126,#73127,#73128,#73129,#73130,
#73131,#73132,#73133,#73134,#73135,#73136,#73137,#73138,#73139,#73140,#73141,
#73142,#73143,#73144,#73145,#73146,#73147,#73148,#73149,#73150,#73151,#73152,
#73153,#73154,#73155,#73156,#73157,#73158,#73159,#73160,#73161,#73162,#73163,
#73164,#73165,#73166,#73167,#73168,#73169,#73170,#73171),.UNSPECIFIED.,
 .F.,.F.,(4,2,2,2,2,2,2,2,2,2,2,2,2,2,2,2,2,2,2,2,2,2,2,2,2,2,2,2,2,2,2,
2,2,2,2,2,2,2,2,2,2,2,2,2,2,2,2,2,2,2,2,2,2,2,2,2,2,2,2,2,2,2,2,2,2,2,2,
2,2,2,2,2,2,2,2,2,2,2,2,2,2,2,2,2,2,2,2,2,4),(-0.659092247150748,-0.657847337165459,
-0.655117324673011,-0.65166110052353,-0.644471813353595,-0.63454222140134,
-0.62053307279676,-0.604672714135786,-0.600913572830821,-0.599026192226777,
-0.597486005894416,-0.595447050537588,-0.590860376322777,-0.564932054450223,
-0.547893993018436,-0.543278235310928,-0.540327061979064,-0.53751370605405,
-0.53361642252045,-0.523562176068924,-0.506891094712074,-0.48765388920764,
-0.484026385933713,-0.482142235428155,-0.480586905160501,-0.478534701890131,
-0.473870318637051,-0.467017533005013,-0.439446449898104,-0.429605580366987,
-0.425635873237102,-0.42283811613999,-0.419914856274393,-0.415436408075053,
-0.399304690616214,-0.394388719380452,-0.372340388808994,-0.368089572832143,
-0.365847938672911,-0.36427030973432,-0.362498727035257,-0.359310560306125,
-0.355217272983698,-0.345425935937014,-0.315799574579589,-0.310366274793167,
-0.307216738613679,-0.304487124135408,-0.301032662642798,-0.293852047114042,
-0.283938994344236,-0.269912783892604,-0.254045872222858,-0.250286522225629,
-0.248399219286063,-0.246859201201512,-0.244820604207227,-0.240235270568493,
-0.214324914418814,-0.197273095786802,-0.192657296110063,-0.189706319921042,
-0.186893308904515,-0.182996760882585,-0.172946090052386,-0.156284068821107,
-0.137037260742728,-0.133410648173939,-0.131526798691344,-0.129971617569289,
-0.127919481821253,-0.123254734520903,-0.116400908893694,-0.0888112863161954,
-0.0789893013279216,-0.0750226842041575,-0.0722256779482118,-0.0693019805793304,
-0.0648203378049058,-0.0486333330234812,-0.0374569332473158,-0.0208126834134555,
-0.0167378495564204,-0.0147905127745936,-0.0132386998545472,-0.0117300280505381,
-0.00975889164009274,-0.00612376957510279,-0.000334755479537651),
 .UNSPECIFIED.);
#750=B_SPLINE_CURVE_WITH_KNOTS('',3,(#73172,#73173,#73174,#73175,#73176,
#73177,#73178,#73179,#73180,#73181,#73182,#73183,#73184,#73185,#73186,#73187,
#73188,#73189),.UNSPECIFIED.,.F.,.F.,(4,2,2,2,2,2,2,2,4),(-3.17436405700199,
-3.14598172734965,-3.13597100235351,-3.1320797025494,-3.12926746014941,
-3.12631460486497,-3.1216901755824,-3.10439275289458,-3.09104302557684),
 .UNSPECIFIED.);
#751=B_SPLINE_CURVE_WITH_KNOTS('',3,(#73191,#73192,#73193,#73194,#73195,
#73196,#73197,#73198,#73199,#73200,#73201,#73202,#73203,#73204,#73205,#73206,
#73207,#73208,#73209),.UNSPECIFIED.,.F.,.F.,(4,3,3,3,3,3,4),(40.1354661882622,
40.2552991262847,40.3750729642712,40.5025546826919,40.6297310288095,40.756488685127,
40.8407044962357),.UNSPECIFIED.);
#752=B_SPLINE_CURVE_WITH_KNOTS('',3,(#73210,#73211,#73212,#73213,#73214,
#73215,#73216,#73217,#73218,#73219,#73220,#73221,#73222,#73223,#73224,#73225,
#73226,#73227,#73228,#73229,#73230,#73231,#73232,#73233,#73234,#73235,#73236,
#73237,#73238,#73239,#73240,#73241,#73242,#73243,#73244,#73245,#73246,#73247,
#73248,#73249,#73250,#73251,#73252,#73253,#73254,#73255,#73256,#73257,#73258,
#73259,#73260,#73261,#73262,#73263,#73264,#73265,#73266,#73267,#73268,#73269,
#73270,#73271,#73272,#73273,#73274,#73275,#73276,#73277,#73278,#73279,#73280,
#73281,#73282,#73283,#73284,#73285,#73286,#73287,#73288,#73289,#73290,#73291,
#73292,#73293,#73294,#73295,#73296,#73297,#73298,#73299,#73300,#73301,#73302,
#73303,#73304,#73305,#73306,#73307,#73308,#73309,#73310,#73311,#73312,#73313,
#73314,#73315,#73316,#73317,#73318,#73319,#73320,#73321,#73322,#73323,#73324,
#73325,#73326,#73327,#73328,#73329,#73330,#73331,#73332,#73333,#73334,#73335,
#73336,#73337,#73338,#73339,#73340,#73341,#73342,#73343,#73344,#73345,#73346,
#73347,#73348,#73349,#73350,#73351,#73352,#73353,#73354,#73355,#73356,#73357,
#73358,#73359,#73360,#73361,#73362,#73363),.UNSPECIFIED.,.F.,.F.,(4,3,3,
3,3,3,3,3,3,3,3,3,3,3,3,3,3,3,3,3,3,3,3,3,3,3,3,3,3,3,3,3,3,3,3,3,3,3,3,
3,3,3,3,3,3,3,3,3,3,3,3,4),(40.8407044966672,40.9643627484298,41.0883098175793,
41.2124204083489,41.3368376192527,41.3634418732879,41.486987986915,41.6066431708463,
41.7261805464501,41.8456526866283,41.965112051241,42.0846915392776,42.2043443458554,
42.3242088407961,42.3518107823046,42.4753568959317,42.5950120798656,42.714549455472,
42.8340215956529,42.9534809602682,43.0730604483076,43.1927132548881,43.3125777498315,
43.3401796913213,43.4637258049484,43.5833809888806,43.7029183644854,43.8223905046646,
43.9418498692783,44.0614293573159,44.1810821638947,44.3009466588365,44.3285486003381,
44.4520947139652,44.5717498978977,44.6912872735026,44.8107594136822,44.9302187782958,
45.0497982663337,45.1694510729129,45.289315567855,45.3169175093548,45.4404636229819,
45.5601188069146,45.6796561825198,45.7991283226996,45.9185876873136,46.0381671753518,
46.1578199819315,46.2776844768739,46.3052864183715,46.4196372410064),
 .UNSPECIFIED.);
#753=B_SPLINE_CURVE_WITH_KNOTS('',3,(#73368,#73369,#73370,#73371,#73372,
#73373,#73374,#73375,#73376,#73377,#73378,#73379,#73380,#73381,#73382,#73383,
#73384,#73385,#73386,#73387,#73388,#73389,#73390,#73391,#73392,#73393,#73394,
#73395,#73396,#73397,#73398,#73399,#73400,#73401,#73402,#73403,#73404,#73405,
#73406,#73407,#73408,#73409,#73410,#73411,#73412,#73413,#73414,#73415,#73416,
#73417,#73418,#73419,#73420,#73421,#73422,#73423,#73424,#73425,#73426,#73427,
#73428,#73429,#73430,#73431,#73432,#73433,#73434,#73435,#73436,#73437,#73438,
#73439,#73440,#73441,#73442,#73443,#73444,#73445,#73446,#73447,#73448,#73449,
#73450,#73451,#73452,#73453,#73454,#73455,#73456,#73457,#73458,#73459,#73460,
#73461,#73462,#73463,#73464,#73465,#73466,#73467,#73468,#73469,#73470,#73471,
#73472,#73473,#73474,#73475,#73476,#73477,#73478,#73479,#73480,#73481,#73482,
#73483,#73484,#73485,#73486,#73487,#73488,#73489,#73490,#73491,#73492,#73493,
#73494,#73495,#73496,#73497,#73498,#73499,#73500,#73501,#73502,#73503,#73504,
#73505,#73506,#73507,#73508,#73509,#73510,#73511,#73512,#73513,#73514,#73515,
#73516,#73517,#73518,#73519,#73520,#73521,#73522,#73523,#73524,#73525,#73526,
#73527,#73528,#73529,#73530,#73531,#73532,#73533,#73534,#73535,#73536,#73537,
#73538,#73539,#73540,#73541,#73542,#73543),.UNSPECIFIED.,.F.,.F.,(4,2,2,
2,2,2,2,2,2,2,2,2,2,2,2,2,2,2,2,2,2,2,2,2,2,2,2,2,2,2,2,2,2,2,2,2,2,2,2,
2,2,2,2,2,2,2,2,2,2,2,2,2,2,2,2,2,2,2,2,2,2,2,2,2,2,2,2,2,2,2,2,2,2,2,2,
2,2,2,2,2,2,2,2,2,2,2,2,4),(-1.40166030916385,-1.37074872889547,-1.3636355541024,
-1.36019165817904,-1.35746122843946,-1.35430060238847,-1.34882185197481,
-1.32518254109912,-1.31127029750981,-1.30388514246043,-1.30145681422145,
-1.29984551946185,-1.29835559220305,-1.2957228104434,-1.2869965045143,-1.25377252721205,
-1.24666060403705,-1.24321716387714,-1.2404870327011,-1.23732668258277,
-1.23184822887434,-1.20821893014021,-1.19430311750791,-1.18691721660821,
-1.18448897746441,-1.18287782180291,-1.1813880928463,-1.17875579423015,
-1.17003276639959,-1.13681063724061,-1.12969878395935,-1.12625558837016,
-1.12352573916631,-1.12036581318139,-1.11488834943471,-1.0912510841642,
-1.07734384068059,-1.06996087918445,-1.0675331380666,-1.06592220078658,
-1.06443257611345,-1.06180027575788,-1.05307489220482,-1.01985869540226,
-1.01274856860719,-1.00930591358912,-1.006576369543,-1.00341665982202,-0.997939213915288,
-0.974319198894698,-0.960403498097602,-0.953018306682525,-0.950590489948238,
-0.948979659799876,-0.947490271238418,-0.94485864915994,-0.936138811395806,
-0.902922817532087,-0.895812093640249,-0.892369563957432,-0.889640292474709,
-0.886481090461841,-0.881005025615726,-0.857366915098181,-0.843466620408091,
-0.836086444308368,-0.83365935594194,-0.832048788812946,-0.830559451536752,
-0.827927554475934,-0.819202186325314,-0.785994425378115,-0.778886361423134,
-0.775444539068679,-0.772690334038145,-0.769521822841325,-0.764001148159297,
-0.742256424281249,-0.721251916090213,-0.717734189210468,-0.715872944427697,
-0.714314887116222,-0.712230601003129,-0.707374781410603,-0.700120614599103,
-0.666425615302329,-0.660996237232752,-0.659092247150748),.UNSPECIFIED.);
#754=B_SPLINE_CURVE_WITH_KNOTS('',3,(#73545,#73546,#73547,#73548,#73549,
#73550,#73551,#73552,#73553,#73554,#73555,#73556,#73557,#73558,#73559,#73560,
#73561,#73562,#73563),.UNSPECIFIED.,.F.,.F.,(4,3,3,3,3,3,4),(46.4196372410064,
46.5375477121673,46.6553395633796,46.773127793545,46.8909019183037,47.0088381638724,
47.1238898031507),.UNSPECIFIED.);
#755=B_SPLINE_CURVE_WITH_KNOTS('',3,(#73564,#73565,#73566,#73567,#73568,
#73569,#73570,#73571,#73572,#73573,#73574,#73575,#73576,#73577,#73578,#73579,
#73580,#73581,#73582,#73583,#73584,#73585,#73586,#73587,#73588,#73589,#73590,
#73591,#73592,#73593,#73594,#73595,#73596,#73597,#73598,#73599,#73600,#73601,
#73602,#73603,#73604,#73605,#73606,#73607,#73608,#73609,#73610,#73611,#73612,
#73613,#73614,#73615,#73616,#73617,#73618,#73619,#73620,#73621,#73622,#73623,
#73624,#73625,#73626,#73627,#73628,#73629,#73630,#73631,#73632,#73633,#73634,
#73635,#73636,#73637,#73638,#73639,#73640,#73641,#73642,#73643,#73644,#73645,
#73646,#73647,#73648,#73649,#73650,#73651,#73652,#73653,#73654,#73655,#73656,
#73657,#73658,#73659,#73660,#73661,#73662,#73663,#73664,#73665,#73666,#73667,
#73668,#73669,#73670,#73671,#73672,#73673,#73674,#73675,#73676,#73677,#73678,
#73679,#73680,#73681,#73682,#73683,#73684,#73685,#73686,#73687,#73688,#73689,
#73690,#73691,#73692,#73693,#73694,#73695,#73696,#73697,#73698,#73699,#73700,
#73701,#73702,#73703,#73704,#73705,#73706,#73707,#73708,#73709,#73710,#73711,
#73712,#73713,#73714),.UNSPECIFIED.,.F.,.F.,(4,3,3,3,3,3,3,3,3,3,3,3,3,
3,3,3,3,3,3,3,3,3,3,3,3,3,3,3,3,3,3,3,3,3,3,3,3,3,3,3,3,3,3,3,3,3,3,3,3,
3,4),(47.1238898038469,47.2936553273882,47.4172014410153,47.5368566249479,
47.656394000553,47.7758661407327,47.8953255053465,48.0149049933845,48.1345577999637,
48.2544222949058,48.2820242364049,48.405570350032,48.5252255339646,48.6447629095697,
48.7642350497494,48.8836944143633,49.0032739024013,49.1229267089805,49.2427912039227,
49.2703931454216,49.3939392590487,49.5135944429813,49.6331318185864,49.752603958766,
49.8720633233799,49.991642811418,50.1112956179972,50.2311601129393,50.2587620544383,
50.3823081680654,50.501963351998,50.6215007276031,50.7409728677827,50.8604322323966,
50.9800117204346,51.0996645270139,51.219529021956,51.2471309634551,51.3706770770822,
51.4903322610148,51.6098696366199,51.7293417767995,51.8488011414135,51.9683806294515,
52.0880334360308,52.2078979309729,52.2354998724718,52.355333838859,52.4749962045213,
52.5945469089048,52.7024741778816),.UNSPECIFIED.);
#756=B_SPLINE_CURVE_WITH_KNOTS('',3,(#73720,#73721,#73722,#73723,#73724,
#73725,#73726,#73727,#73728,#73729,#73730,#73731,#73732,#73733,#73734,#73735,
#73736,#73737,#73738,#73739,#73740,#73741,#73742,#73743,#73744,#73745,#73746,
#73747,#73748,#73749,#73750,#73751,#73752,#73753,#73754,#73755,#73756,#73757,
#73758,#73759,#73760,#73761,#73762,#73763,#73764,#73765,#73766,#73767,#73768,
#73769,#73770,#73771,#73772,#73773,#73774,#73775,#73776,#73777,#73778,#73779,
#73780,#73781,#73782,#73783,#73784,#73785,#73786,#73787,#73788,#73789,#73790,
#73791,#73792,#73793,#73794,#73795,#73796,#73797,#73798,#73799,#73800,#73801,
#73802,#73803,#73804,#73805,#73806,#73807,#73808,#73809,#73810,#73811,#73812,
#73813,#73814,#73815,#73816,#73817,#73818,#73819,#73820,#73821,#73822,#73823,
#73824,#73825,#73826,#73827,#73828,#73829,#73830,#73831,#73832,#73833,#73834,
#73835,#73836,#73837,#73838,#73839,#73840,#73841,#73842,#73843,#73844,#73845,
#73846,#73847,#73848,#73849,#73850,#73851,#73852,#73853,#73854,#73855,#73856,
#73857,#73858,#73859,#73860,#73861,#73862,#73863,#73864,#73865,#73866,#73867,
#73868,#73869,#73870,#73871,#73872,#73873,#73874,#73875,#73876,#73877,#73878,
#73879,#73880,#73881),.UNSPECIFIED.,.F.,.F.,(4,2,2,2,2,2,2,2,2,2,2,2,2,
2,2,2,2,2,2,2,2,2,2,2,2,2,2,2,2,2,2,2,2,2,2,2,2,2,2,2,2,2,2,2,2,2,2,2,2,
2,2,2,2,2,2,2,2,2,2,2,2,2,2,2,2,2,2,2,2,2,2,2,2,2,2,2,2,2,2,2,4),(-0.658976676139878,
-0.647559402944162,-0.637927955387454,-0.635212731971702,-0.63354277089442,
-0.631911429201569,-0.629377370601124,-0.620942458873841,-0.603098942762448,
-0.583272956277358,-0.578527048138876,-0.575550129005866,-0.572751425594615,
-0.56893724197842,-0.559483638379049,-0.544457139694901,-0.52251619138621,
-0.519057656415479,-0.517209586673753,-0.515665535348846,-0.513574049582365,
-0.508669836456843,-0.50131056459068,-0.474302815240831,-0.464695293598529,
-0.460760082909462,-0.457969203304208,-0.455038070071776,-0.450516166955131,
-0.433647955426323,-0.412767864189028,-0.404113671448546,-0.401488938447733,
-0.400001601301243,-0.398391108095587,-0.395960827919078,-0.388542165799128,
-0.37450773680041,-0.351120645350932,-0.345640890748171,-0.342482130135672,
-0.339754700192193,-0.336316412085633,-0.329222161378755,-0.296045771902395,
-0.287279273822127,-0.284644595690969,-0.282991774699758,-0.281344520600445,
-0.278735867794029,-0.269464638098045,-0.247581486561486,-0.232322135022478,
-0.22779876784903,-0.22486702568353,-0.222043860556855,-0.218085625133857,
-0.207551564710205,-0.178245401026454,-0.170279900333843,-0.167718353155734,
-0.166242919825262,-0.164620654983839,-0.162132366470803,-0.15416915973964,
-0.138213785211149,-0.117498585330046,-0.111966962519322,-0.108796677554783,
-0.106043495548194,-0.102606319690159,-0.0955210762894671,-0.0623627300998356,
-0.0535584119753678,-0.0509200626184618,-0.0492662023159992,-0.0476192065506048,
-0.045012939858365,-0.0357753380878062,-0.0198319199248591,-0.000335325052894208),
 .UNSPECIFIED.);
#757=B_SPLINE_CURVE_WITH_KNOTS('',3,(#73882,#73883,#73884,#73885,#73886,
#73887,#73888,#73889,#73890,#73891,#73892,#73893,#73894,#73895,#73896,#73897,
#73898,#73899,#73900,#73901,#73902,#73903,#73904,#73905,#73906,#73907,#73908,
#73909,#73910,#73911,#73912,#73913),.UNSPECIFIED.,.F.,.F.,(4,2,2,2,2,2,
2,2,2,2,2,2,2,2,2,4),(-1.48497886615627,-1.4804211924715,-1.47768304987249,
-1.47504991531636,-1.47243836288595,-1.46807733810784,-1.45459659168007,
-1.44217058245323,-1.4282532491641,-1.42086621108752,-1.41843750201499,
-1.41682601157226,-1.41533595304441,-1.41270303395089,-1.40397746823474,
-1.40166030916385),.UNSPECIFIED.);
#758=B_SPLINE_CURVE_WITH_KNOTS('',3,(#73915,#73916,#73917,#73918,#73919,
#73920,#73921,#73922,#73923,#73924,#73925,#73926,#73927,#73928,#73929,#73930,
#73931,#73932,#73933),.UNSPECIFIED.,.F.,.F.,(4,3,3,3,3,3,4),(52.7024741778816,
52.8219322553359,52.9415057835748,53.0611466250366,53.1810035178623,53.2238687814885,
53.4070751110266),.UNSPECIFIED.);
#759=B_SPLINE_CURVE_WITH_KNOTS('',3,(#73934,#73935,#73936,#73937,#73938,
#73939,#73940,#73941,#73942),.UNSPECIFIED.,.F.,.F.,(4,1,1,1,1,1,4),(53.4070796080658,
54.2122376905052,55.2006065995219,56.1889755085386,57.1773444175554,58.1657133265721,
58.98478654205),.UNSPECIFIED.);
#760=B_SPLINE_CURVE_WITH_KNOTS('',3,(#73947,#73948,#73949,#73950,#73951,
#73952,#73953,#73954,#73955,#73956,#73957,#73958,#73959,#73960,#73961,#73962,
#73963,#73964,#73965,#73966,#73967,#73968,#73969,#73970,#73971,#73972,#73973,
#73974,#73975,#73976,#73977,#73978,#73979,#73980,#73981,#73982,#73983,#73984,
#73985,#73986,#73987,#73988,#73989,#73990,#73991,#73992,#73993,#73994,#73995,
#73996,#73997,#73998,#73999,#74000,#74001,#74002,#74003,#74004,#74005,#74006,
#74007,#74008,#74009,#74010,#74011,#74012,#74013,#74014,#74015,#74016,#74017,
#74018,#74019,#74020,#74021,#74022,#74023,#74024,#74025,#74026,#74027,#74028,
#74029,#74030,#74031,#74032,#74033,#74034,#74035,#74036,#74037,#74038,#74039,
#74040,#74041,#74042,#74043,#74044,#74045,#74046,#74047,#74048,#74049,#74050,
#74051,#74052,#74053,#74054,#74055,#74056,#74057,#74058,#74059,#74060,#74061,
#74062,#74063,#74064,#74065,#74066,#74067,#74068,#74069,#74070,#74071,#74072,
#74073,#74074,#74075,#74076,#74077,#74078,#74079,#74080,#74081,#74082,#74083,
#74084,#74085,#74086,#74087,#74088,#74089,#74090,#74091,#74092,#74093,#74094,
#74095,#74096,#74097,#74098,#74099,#74100,#74101,#74102,#74103,#74104,#74105,
#74106,#74107,#74108,#74109,#74110,#74111,#74112,#74113,#74114,#74115,#74116,
#74117,#74118,#74119,#74120,#74121,#74122,#74123,#74124,#74125,#74126,#74127,
#74128,#74129,#74130,#74131,#74132,#74133,#74134,#74135,#74136,#74137,#74138,
#74139,#74140,#74141,#74142,#74143,#74144,#74145,#74146,#74147,#74148,#74149,
#74150,#74151,#74152,#74153,#74154),.UNSPECIFIED.,.F.,.F.,(4,2,2,2,2,2,
2,2,2,2,2,2,2,2,2,2,2,2,2,2,2,2,2,2,2,2,2,2,2,2,2,2,2,2,2,2,2,2,2,2,2,2,
2,2,2,2,2,2,2,2,2,2,2,2,2,2,2,2,2,2,2,2,2,2,2,2,2,2,2,2,2,2,2,2,2,2,2,2,
2,2,2,2,2,2,2,2,2,2,2,2,2,2,2,2,2,2,2,2,2,2,2,2,2,4),(-1.40060990531413,
-1.40037382044156,-1.39599762339415,-1.39575014915383,-1.39549983618132,
-1.39524186425832,-1.39516781273781,-1.39505951916284,-1.39489267534928,
-1.39461066040855,-1.391847860589,-1.38875732348354,-1.38345759566904,-1.35708953943928,
-1.34486077766074,-1.33801921058626,-1.33565591630552,-1.33405850864429,
-1.33233826489298,-1.32938798604826,-1.31324310260407,-1.30028806780615,
-1.28363297625614,-1.27912507054162,-1.27619739954667,-1.27340585518658,
-1.26946293789873,-1.25979633343448,-1.23202932454018,-1.2251617019475,
-1.22049151812755,-1.21843925448782,-1.21688497266861,-1.21500340595402,
-1.21126965979811,-1.19577217506231,-1.18250816094592,-1.16673162330973,
-1.16227931564973,-1.15936273881688,-1.15656395137175,-1.15257987465595,
-1.14263109077572,-1.11617567805781,-1.108752560566,-1.10381934049315,-1.10172341948776,
-1.10016536994534,-1.0983146323749,-1.09484236522338,-1.07317886049711,
-1.05800997387861,-1.04850268178769,-1.04468155758812,-1.04188219612432,
-1.03890861504133,-1.03417698814248,-1.01441705704065,-0.996487009525404,
-0.988031896282643,-0.985496169880248,-0.983864709844933,-0.982399085711126,
-0.979887372692515,-0.972372504022307,-0.950459221245068,-0.939018778799972,
-0.931089847324866,-0.927508715300317,-0.924743000140185,-0.921664744636298,
-0.916425885117246,-0.885594270838664,-0.876285131506364,-0.872318696963878,
-0.869206742945008,-0.867451871419008,-0.865869548480569,-0.86395344603747,
-0.859248924877213,-0.834431670681573,-0.822515504419465,-0.814365700373937,
-0.810748355721052,-0.807978054468326,-0.804918124638505,-0.799769184076685,
-0.768524176491352,-0.759369992386026,-0.755444718228545,-0.752357352827093,
-0.750607575485915,-0.74902301711675,-0.747097527128348,-0.742222305069737,
-0.734736854557467,-0.706522372836859,-0.697969709706433,-0.694557648814438,
-0.69174568931771,-0.688846522420659,-0.684483322910936,-0.669936264616971,
-0.658976676139878),.UNSPECIFIED.);
#761=B_SPLINE_CURVE_WITH_KNOTS('',3,(#74156,#74157,#74158,#74159,#74160),
 .UNSPECIFIED.,.F.,.F.,(4,1,4),(58.98478654205,59.1540822355888,59.6902604182062),
 .UNSPECIFIED.);
#762=B_SPLINE_CURVE_WITH_KNOTS('',3,(#74161,#74162,#74163,#74164,#74165,
#74166,#74167,#74168,#74169,#74170,#74171,#74172,#74173,#74174,#74175,#74176,
#74177,#74178,#74179,#74180,#74181,#74182,#74183,#74184,#74185,#74186,#74187,
#74188,#74189,#74190,#74191,#74192,#74193,#74194,#74195,#74196,#74197,#74198,
#74199,#74200,#74201,#74202,#74203,#74204,#74205,#74206,#74207,#74208,#74209,
#74210,#74211,#74212,#74213,#74214,#74215,#74216,#74217,#74218,#74219,#74220,
#74221,#74222,#74223,#74224,#74225,#74226,#74227,#74228,#74229,#74230,#74231,
#74232,#74233,#74234,#74235,#74236,#74237,#74238,#74239,#74240,#74241,#74242,
#74243,#74244,#74245,#74246,#74247,#74248,#74249,#74250,#74251,#74252,#74253,
#74254,#74255,#74256,#74257,#74258,#74259,#74260,#74261,#74262,#74263,#74264,
#74265,#74266,#74267,#74268,#74269,#74270,#74271,#74272,#74273,#74274,#74275,
#74276,#74277,#74278,#74279,#74280,#74281,#74282,#74283,#74284,#74285,#74286,
#74287,#74288,#74289,#74290,#74291,#74292,#74293,#74294,#74295,#74296,#74297,
#74298,#74299,#74300,#74301,#74302,#74303,#74304,#74305,#74306,#74307,#74308,
#74309,#74310,#74311,#74312,#74313,#74314),.UNSPECIFIED.,.F.,.F.,(4,3,3,
3,3,3,3,3,3,3,3,3,3,3,3,3,3,3,3,3,3,3,3,3,3,3,3,3,3,3,3,3,3,3,3,3,3,3,3,
3,3,3,3,3,3,3,3,3,3,3,3,4),(59.6902604182062,59.8178925384765,59.9458188551941,
60.07422224745,60.1424511446055,60.2659972582326,60.3856524421651,60.5051898177701,
60.6246619579496,60.7441213225634,60.8637008106013,60.9833536171804,61.1032181121225,
61.1308200536222,61.2543661672493,61.3740213511815,61.4935587267862,61.6130308669655,
61.7324902315789,61.8520697196166,61.9717225261954,62.0915870211372,62.119188962639,
62.2427350762661,62.3623902602,62.4819276358065,62.6013997759875,62.7208591406027,
62.840438628642,62.9600914352225,63.0799559301659,63.1075578716557,63.2311039852828,
63.3507591692139,63.4702965448176,63.5897686849959,63.7092280496084,63.8288075376451,
63.948460344223,64.0683248391639,64.0959267806724,64.2194728942995,64.3391280782295,
64.458665453832,64.578137594009,64.6975969586204,64.8171764466558,64.9368292532324,
65.056693748172,65.0842956896891,65.2026640796911,65.2692561001133),
 .UNSPECIFIED.);
#763=B_SPLINE_CURVE_WITH_KNOTS('',3,(#74320,#74321,#74322,#74323,#74324,
#74325,#74326,#74327,#74328,#74329,#74330,#74331,#74332,#74333,#74334,#74335,
#74336,#74337,#74338,#74339,#74340,#74341,#74342,#74343,#74344,#74345,#74346,
#74347,#74348,#74349,#74350,#74351,#74352,#74353,#74354,#74355,#74356,#74357,
#74358,#74359,#74360,#74361,#74362,#74363,#74364,#74365,#74366,#74367,#74368,
#74369,#74370,#74371,#74372,#74373,#74374,#74375,#74376,#74377,#74378,#74379,
#74380,#74381,#74382,#74383,#74384,#74385,#74386,#74387,#74388,#74389,#74390,
#74391,#74392,#74393,#74394,#74395,#74396,#74397,#74398,#74399,#74400,#74401,
#74402,#74403,#74404,#74405,#74406,#74407,#74408,#74409,#74410,#74411,#74412,
#74413,#74414,#74415,#74416,#74417,#74418,#74419,#74420,#74421,#74422,#74423,
#74424,#74425,#74426,#74427,#74428,#74429,#74430,#74431,#74432,#74433,#74434,
#74435,#74436,#74437,#74438,#74439,#74440,#74441,#74442,#74443,#74444,#74445,
#74446,#74447,#74448,#74449,#74450,#74451,#74452,#74453,#74454,#74455,#74456,
#74457,#74458,#74459,#74460,#74461,#74462,#74463,#74464,#74465,#74466,#74467,
#74468,#74469,#74470,#74471,#74472,#74473,#74474,#74475,#74476,#74477,#74478,
#74479,#74480,#74481,#74482,#74483,#74484,#74485,#74486,#74487,#74488,#74489,
#74490,#74491,#74492,#74493),.UNSPECIFIED.,.F.,.F.,(4,2,2,2,2,2,2,2,2,2,
2,2,2,2,2,2,2,2,2,2,2,2,2,2,2,2,2,2,2,2,2,2,2,2,2,2,2,2,2,2,2,2,2,2,2,2,
2,2,2,2,2,2,2,2,2,2,2,2,2,2,2,2,2,2,2,2,2,2,2,2,2,2,2,2,2,2,2,2,2,2,2,2,
2,2,2,2,4),(-0.659264417620488,-0.658306668539297,-0.645960048448501,-0.61982461602658,
-0.614480758731446,-0.611379560346641,-0.608616074379269,-0.605069816617077,
-0.597359875485747,-0.586381773310217,-0.573396687769836,-0.558275719414295,
-0.55455810877067,-0.55267886559312,-0.551123078322035,-0.549064391818707,
-0.544361546636229,-0.537428919706541,-0.508841969400668,-0.499844679485265,
-0.496383326405695,-0.493814681747486,-0.490975095378717,-0.486928206583286,
-0.475665123989059,-0.455040104275854,-0.440080751097174,-0.437133901566631,
-0.435413564555328,-0.433814276145509,-0.43144568631414,-0.424569465088856,
-0.412244386001662,-0.386071865031164,-0.380732430853882,-0.377632204285496,
-0.374868647312202,-0.371320993230495,-0.363602330709988,-0.352605978667221,
-0.339642846793759,-0.324531966155127,-0.320814893554997,-0.318935793468338,
-0.317380048331269,-0.315321318398518,-0.310617973524586,-0.303684215060326,
-0.275080294815655,-0.26610001569161,-0.262640009980384,-0.260071734880583,
-0.25723194005492,-0.253183536014559,-0.24190660401442,-0.221228980428054,
-0.206339977461716,-0.203393986108559,-0.201673867861735,-0.200074544553195,
-0.197705563126124,-0.190825659362085,-0.178489353268304,-0.152338529549808,
-0.146996925142279,-0.143896317902965,-0.141132938135055,-0.137586231032848,
-0.129872763694196,-0.11888702869055,-0.105916195971956,-0.090796970585841,
-0.0870796324137364,-0.0852005170170505,-0.0836448293163537,-0.0815862667767107,
-0.0815454327891802,-0.0768592190584028,-0.0673422136539098,-0.0406636701991896,
-0.0322018785559816,-0.0288030993362951,-0.0259935531815042,-0.02308821969655,
-0.0201488702907366,-0.0159551229479655,-0.000334955112094566),
 .UNSPECIFIED.);
#764=B_SPLINE_CURVE_WITH_KNOTS('',3,(#74494,#74495,#74496,#74497,#74498,
#74499,#74500,#74501,#74502,#74503,#74504,#74505,#74506,#74507,#74508,#74509,
#74510,#74511,#74512,#74513,#74514,#74515),.UNSPECIFIED.,.F.,.F.,(4,2,2,
2,2,2,2,2,2,2,4),(-1.4836709134642,-1.45834033302783,-1.45524331960259,
-1.45267009041877,-1.451030912921,-1.44937115674332,-1.4467017984514,-1.43755481426339,
-1.41636892125086,-1.40565146373752,-1.40060990531413),.UNSPECIFIED.);
#765=B_SPLINE_CURVE_WITH_KNOTS('',3,(#74517,#74518,#74519,#74520,#74521,
#74522,#74523,#74524,#74525,#74526,#74527,#74528,#74529,#74530,#74531,#74532,
#74533,#74534,#74535),.UNSPECIFIED.,.F.,.F.,(4,3,3,3,3,3,4),(65.2692561001133,
65.3873720613773,65.5054033502643,65.6234822689178,65.7415755373178,65.8598751587599,
65.9734457248711),.UNSPECIFIED.);
#766=B_SPLINE_CURVE_WITH_KNOTS('',3,(#74536,#74537,#74538,#74539,#74540,
#74541,#74542,#74543,#74544,#74545,#74546,#74547,#74548,#74549,#74550,#74551,
#74552,#74553,#74554,#74555,#74556,#74557,#74558,#74559,#74560,#74561,#74562,
#74563,#74564,#74565,#74566,#74567,#74568,#74569,#74570,#74571,#74572,#74573,
#74574,#74575,#74576,#74577,#74578,#74579,#74580,#74581,#74582,#74583,#74584,
#74585,#74586,#74587,#74588,#74589,#74590,#74591,#74592,#74593,#74594,#74595,
#74596,#74597,#74598,#74599,#74600,#74601,#74602,#74603,#74604,#74605,#74606,
#74607,#74608,#74609,#74610,#74611,#74612,#74613,#74614,#74615,#74616,#74617,
#74618,#74619,#74620,#74621,#74622,#74623,#74624,#74625,#74626,#74627,#74628,
#74629,#74630,#74631,#74632,#74633,#74634,#74635,#74636,#74637,#74638,#74639,
#74640,#74641,#74642,#74643,#74644,#74645,#74646,#74647,#74648,#74649,#74650,
#74651,#74652,#74653,#74654,#74655,#74656,#74657,#74658,#74659,#74660,#74661,
#74662,#74663,#74664,#74665,#74666,#74667,#74668,#74669,#74670,#74671,#74672,
#74673,#74674,#74675,#74676,#74677,#74678,#74679,#74680,#74681,#74682,#74683,
#74684,#74685,#74686,#74687,#74688,#74689),.UNSPECIFIED.,.F.,.F.,(4,3,3,
3,3,3,3,3,3,3,3,3,3,3,3,3,3,3,3,3,3,3,3,3,3,3,3,3,3,3,3,3,3,3,3,3,3,3,3,
3,3,3,3,3,3,3,3,3,3,3,3,4),(65.9734457253855,66.0726645987058,66.1962107123329,
66.3158658962491,66.435403271838,66.5548754120015,66.6743347765995,66.793914264622,
66.913567071186,67.0334315661134,67.0610335077225,67.1845796213496,67.304234805268,
67.4237721808587,67.5432443210237,67.6627036856228,67.782283173646,67.9019359802104,
68.0218004751376,68.0494024167392,68.1729485303663,68.2926037144019,68.41214109011,
68.5316132303923,68.6510725951084,68.7706520832471,68.8903048899263,69.0101693849663,
69.037771325756,69.1613174393831,69.2809726231416,69.4005099985737,69.5199821385816,
69.6394415030256,69.7590209908976,69.8786737973129,69.9985382920956,70.0261402347727,
70.1496863483998,70.2693415322863,70.3888789078432,70.5083510479725,70.6278104125342,
70.7473899005178,70.8670427070412,70.9869072019259,71.0145091437894,71.1343809419583,
71.2540404936461,71.3735768465406,71.4930579961026,71.5518219705938),
 .UNSPECIFIED.);
#767=B_SPLINE_CURVE_WITH_KNOTS('',3,(#74694,#74695,#74696,#74697,#74698,
#74699,#74700,#74701,#74702,#74703,#74704,#74705,#74706,#74707,#74708,#74709,
#74710,#74711,#74712,#74713,#74714,#74715,#74716,#74717,#74718,#74719,#74720,
#74721,#74722,#74723,#74724,#74725,#74726,#74727,#74728,#74729,#74730,#74731,
#74732,#74733,#74734,#74735,#74736,#74737,#74738,#74739,#74740,#74741,#74742,
#74743,#74744,#74745,#74746,#74747,#74748,#74749,#74750,#74751,#74752,#74753,
#74754,#74755,#74756,#74757,#74758,#74759,#74760,#74761,#74762,#74763,#74764,
#74765,#74766,#74767,#74768,#74769,#74770,#74771,#74772,#74773,#74774,#74775,
#74776,#74777,#74778,#74779,#74780,#74781,#74782,#74783,#74784,#74785,#74786,
#74787,#74788,#74789,#74790,#74791,#74792,#74793,#74794,#74795,#74796,#74797,
#74798,#74799,#74800,#74801,#74802,#74803,#74804,#74805,#74806,#74807,#74808,
#74809,#74810,#74811,#74812,#74813,#74814,#74815,#74816,#74817,#74818,#74819,
#74820,#74821,#74822,#74823,#74824,#74825,#74826,#74827,#74828,#74829,#74830,
#74831,#74832,#74833,#74834,#74835,#74836,#74837,#74838,#74839,#74840,#74841,
#74842,#74843,#74844,#74845,#74846,#74847,#74848,#74849,#74850,#74851,#74852,
#74853,#74854,#74855,#74856,#74857,#74858,#74859,#74860,#74861,#74862,#74863,
#74864,#74865,#74866,#74867,#74868,#74869,#74870,#74871,#74872,#74873,#74874,
#74875,#74876,#74877,#74878,#74879,#74880,#74881,#74882,#74883,#74884,#74885,
#74886,#74887,#74888,#74889),.UNSPECIFIED.,.F.,.F.,(4,2,2,2,2,2,2,2,2,2,
2,2,2,2,2,2,2,2,2,2,2,2,2,2,2,2,2,2,2,2,2,2,2,2,2,2,2,2,2,2,2,2,2,2,2,2,
2,2,2,2,2,2,2,2,2,2,2,2,2,2,2,2,2,2,2,2,2,2,2,2,2,2,2,2,2,2,2,2,2,2,2,2,
2,2,2,2,2,2,2,2,2,2,2,2,2,2,2,4),(-1.40128003339357,-1.39210941171292,-1.38043630308909,
-1.3737845005758,-1.37144360238271,-1.3698496377744,-1.36811984913717,-1.36512794361135,
-1.34833028183322,-1.33498901578421,-1.3192905432365,-1.3148417287557,-1.31192476653075,
-1.30912369157327,-1.30575915304785,-1.29737868129969,-1.27271691874549,
-1.26276733121124,-1.25863363351139,-1.25542192331339,-1.25364553967208,
-1.25206973021645,-1.24983906667524,-1.24440631083524,-1.22311320238154,
-1.21831559728887,-1.20772254920655,-1.20020010179226,-1.19668610621486,
-1.19392624880157,-1.19080659628913,-1.18551198137943,-1.15948182869849,
-1.14706432456199,-1.14015752285836,-1.1377853930556,-1.13618559271827,
-1.13446677244753,-1.13152646805925,-1.11697017177115,-1.10481838502156,
-1.09222494207606,-1.08376967217366,-1.0801027578258,-1.07732493605402,
-1.07428656651196,-1.06924666999661,-1.04076802383121,-1.02445723200069,
-1.02150162161994,-1.01977943105424,-1.01819967404407,-1.01585169881057,
-1.00962322763275,-0.986409728095614,-0.96893295280559,-0.964376153966052,
-0.961437037890596,-0.958648733233082,-0.954734450646943,-0.945255570838767,
-0.917228341016276,-0.910336449632518,-0.90565353335338,-0.903598157775324,
-0.902042584926881,-0.900160763029455,-0.896544548772937,-0.877099456031107,
-0.860576107283148,-0.850573056878916,-0.846682562952161,-0.843870276742218,
-0.84091681986949,-0.83629026310259,-0.818931252705608,-0.802545998320124,
-0.794332166578819,-0.789040367208318,-0.786886950727362,-0.785321627262545,
-0.783504375718744,-0.780191744834745,-0.756790572935862,-0.742555974090395,
-0.733587423972396,-0.730128104464985,-0.727559876792625,-0.724719682142326,
-0.720669814902384,-0.70938173381975,-0.688663578273523,-0.673824868879985,
-0.670879315580966,-0.669159222157904,-0.667559725729801,-0.665190209532858,
-0.659264417620488),.UNSPECIFIED.);
#768=B_SPLINE_CURVE_WITH_KNOTS('',3,(#74891,#74892,#74893,#74894,#74895,
#74896,#74897,#74898,#74899,#74900,#74901,#74902,#74903,#74904,#74905,#74906,
#74907,#74908,#74909),.UNSPECIFIED.,.F.,.F.,(4,3,3,3,3,3,4),(71.5518219705938,
71.6713814952313,71.7909889789199,71.9108277902384,72.0028780528061,72.155509984639,
72.2566310318613),.UNSPECIFIED.);
#769=B_SPLINE_CURVE_WITH_KNOTS('',3,(#74910,#74911,#74912,#74913,#74914,
#74915,#74916,#74917,#74918,#74919,#74920,#74921,#74922,#74923,#74924,#74925,
#74926,#74927,#74928,#74929,#74930,#74931,#74932,#74933,#74934,#74935,#74936,
#74937,#74938,#74939,#74940,#74941,#74942,#74943,#74944,#74945,#74946,#74947,
#74948,#74949,#74950,#74951,#74952,#74953,#74954,#74955,#74956,#74957,#74958,
#74959,#74960,#74961,#74962,#74963,#74964,#74965,#74966,#74967,#74968,#74969,
#74970,#74971,#74972,#74973,#74974,#74975,#74976,#74977,#74978,#74979,#74980,
#74981,#74982,#74983,#74984,#74985,#74986,#74987,#74988,#74989,#74990,#74991,
#74992,#74993,#74994,#74995,#74996,#74997,#74998,#74999,#75000,#75001,#75002,
#75003,#75004,#75005,#75006,#75007,#75008,#75009,#75010,#75011,#75012,#75013,
#75014,#75015,#75016,#75017,#75018,#75019,#75020,#75021,#75022,#75023,#75024,
#75025,#75026,#75027,#75028,#75029,#75030,#75031,#75032,#75033,#75034,#75035,
#75036,#75037,#75038,#75039,#75040,#75041,#75042,#75043,#75044,#75045,#75046,
#75047,#75048,#75049,#75050,#75051,#75052,#75053,#75054,#75055,#75056,#75057,
#75058,#75059,#75060,#75061,#75062,#75063),.UNSPECIFIED.,.F.,.F.,(4,3,3,
3,3,3,3,3,3,3,3,3,3,3,3,3,3,3,3,3,3,3,3,3,3,3,3,3,3,3,3,3,3,3,3,3,3,3,3,
3,3,3,3,3,3,3,3,3,3,3,3,4),(72.2566310325651,72.3749180120349,72.4931281764082,
72.6113162646557,72.7296157230161,72.8479843387787,72.9665609847747,72.9912469618228,
73.1147930754499,73.2344482597025,73.3539856356069,73.4734577760647,73.5929171409353,
73.7124966291971,73.8321494359811,73.9520139310986,73.9796158708395,74.1031619844666,
74.2228171752065,74.342354557629,74.4618267046219,74.5812860760313,74.7008655707878,
74.8205183840471,74.9403828855481,74.9679847798563,75.0915308934834,75.2111860605028,
75.3307234192612,75.4501955426938,75.5696548906937,75.6892343624356,75.8088871528883,
75.9287516321069,75.956353688873,76.0798998025001,76.1995549957352,76.3190923804485,
76.4385645295258,76.5580239028104,76.6776033991253,76.7972562137593,76.9171207163584,
76.9447225978897,77.0645588437826,77.1842191415837,77.3037562699964,77.4232228139605,
77.542731903974,77.6622643053389,77.7819561071778,77.8347123306237),
 .UNSPECIFIED.);
#770=B_SPLINE_CURVE_WITH_KNOTS('',3,(#75069,#75070,#75071,#75072,#75073,
#75074,#75075,#75076,#75077,#75078,#75079,#75080,#75081,#75082,#75083,#75084,
#75085,#75086,#75087,#75088,#75089,#75090,#75091,#75092,#75093,#75094,#75095,
#75096,#75097,#75098,#75099,#75100,#75101,#75102,#75103,#75104,#75105,#75106,
#75107,#75108,#75109,#75110,#75111,#75112,#75113,#75114,#75115,#75116,#75117,
#75118,#75119,#75120,#75121,#75122,#75123,#75124,#75125,#75126,#75127,#75128,
#75129,#75130,#75131,#75132,#75133,#75134,#75135,#75136,#75137,#75138,#75139,
#75140,#75141,#75142,#75143,#75144,#75145,#75146,#75147,#75148,#75149,#75150,
#75151,#75152,#75153,#75154,#75155,#75156,#75157,#75158,#75159,#75160,#75161,
#75162,#75163,#75164,#75165,#75166,#75167,#75168,#75169,#75170,#75171,#75172,
#75173,#75174,#75175,#75176,#75177,#75178,#75179,#75180,#75181,#75182,#75183,
#75184,#75185,#75186,#75187,#75188,#75189,#75190,#75191,#75192,#75193,#75194,
#75195,#75196,#75197,#75198,#75199,#75200,#75201,#75202,#75203,#75204,#75205,
#75206,#75207,#75208,#75209,#75210,#75211,#75212,#75213,#75214,#75215,#75216,
#75217,#75218,#75219,#75220,#75221,#75222,#75223,#75224,#75225,#75226,#75227,
#75228,#75229,#75230,#75231,#75232,#75233,#75234,#75235,#75236,#75237,#75238,
#75239,#75240,#75241,#75242,#75243,#75244,#75245,#75246),.UNSPECIFIED.,
 .F.,.F.,(4,2,2,2,2,2,2,2,2,2,2,2,2,2,2,2,2,2,2,2,2,2,2,2,2,2,2,2,2,2,2,
2,2,2,2,2,2,2,2,2,2,2,2,2,2,2,2,2,2,2,2,2,2,2,2,2,2,2,2,2,2,2,2,2,2,2,2,
2,2,2,2,2,2,2,2,2,2,2,2,2,2,2,2,2,2,2,2,2,4),(-0.659170325149453,-0.655256623528942,
-0.649784001405313,-0.646666348339993,-0.643922255609298,-0.640448200383027,
-0.633100017464438,-0.607089608807798,-0.596760357812911,-0.592534883661284,
-0.589272090014849,-0.587491318556743,-0.585922400426226,-0.583724000050673,
-0.578132244094427,-0.569222056456834,-0.540136017048644,-0.533563692045375,
-0.530176200660663,-0.527421915066887,-0.524204202362348,-0.518296138243247,
-0.510718176186608,-0.490293883619145,-0.475179063581887,-0.472228741143748,
-0.47050513421987,-0.468903326492536,-0.466528517525274,-0.459610265416756,
-0.447162378644605,-0.421223496116864,-0.415921823155921,-0.412799589114962,
-0.410038315090225,-0.406523657458192,-0.399004654764951,-0.38842020640015,
-0.383825145689173,-0.362920836027997,-0.357002122308034,-0.354695199602874,
-0.35312256171966,-0.351385555207384,-0.348358433767659,-0.329206254415996,
-0.304537463323012,-0.299122392672783,-0.295977777984708,-0.293249228730659,
-0.289791957447864,-0.282589546689366,-0.27263314195551,-0.258650231520054,
-0.242797284850174,-0.239039239971014,-0.237152861500545,-0.235613207142084,
-0.233574952373678,-0.228992107513741,-0.203128551472326,-0.186026285584048,
-0.181408154134144,-0.178456270294801,-0.175642776124923,-0.171746134850384,
-0.161698126017314,-0.145042792044167,-0.12579786732056,-0.122171372228599,
-0.120287198930523,-0.118731668144502,-0.11667879106968,-0.112010428535118,
-0.105149324099089,-0.0774720162932436,-0.0677246689046249,-0.0637686764328149,
-0.0609733952386566,-0.0580465437958409,-0.0535497882993478,-0.0371255518100336,
-0.0190527454480019,-0.0129595916652631,-0.00654563670509995,-0.00421896730293171,
-0.00264042997467122,-0.00137147600074732,-0.000346630335231024),
 .UNSPECIFIED.);
#771=B_SPLINE_CURVE_WITH_KNOTS('',3,(#75247,#75248,#75249,#75250,#75251,
#75252,#75253,#75254,#75255,#75256,#75257,#75258,#75259,#75260,#75261,#75262,
#75263,#75264,#75265,#75266,#75267,#75268),.UNSPECIFIED.,.F.,.F.,(4,2,2,
2,2,2,2,2,2,2,4),(-1.48452167401131,-1.48321766816317,-1.48078181711199,
-1.45391592152954,-1.44220222492896,-1.43414473492672,-1.43054163756083,
-1.42777239058184,-1.42470374612459,-1.4195154426393,-1.40128003339357),
 .UNSPECIFIED.);
#772=B_SPLINE_CURVE_WITH_KNOTS('',3,(#75270,#75271,#75272,#75273,#75274,
#75275,#75276,#75277,#75278,#75279,#75280,#75281,#75282,#75283,#75284,#75285,
#75286,#75287,#75288),.UNSPECIFIED.,.F.,.F.,(4,3,3,3,3,3,4),(77.8347123306237,
77.9330915069064,78.0542613844013,78.1756501232371,78.2964289099056,78.4181226248252,
78.5398163397448),.UNSPECIFIED.);
#773=B_SPLINE_CURVE_WITH_KNOTS('',3,(#75289,#75290,#75291,#75292,#75293,
#75294,#75295,#75296,#75297,#75298,#75299,#75300,#75301,#75302,#75303,#75304,
#75305,#75306,#75307,#75308,#75309,#75310,#75311,#75312,#75313,#75314,#75315,
#75316,#75317,#75318,#75319,#75320,#75321,#75322,#75323,#75324,#75325,#75326,
#75327,#75328,#75329,#75330,#75331,#75332,#75333,#75334,#75335,#75336,#75337,
#75338,#75339,#75340,#75341,#75342,#75343,#75344,#75345,#75346,#75347,#75348,
#75349,#75350,#75351,#75352,#75353,#75354,#75355,#75356,#75357,#75358,#75359,
#75360,#75361,#75362,#75363,#75364,#75365,#75366,#75367,#75368,#75369,#75370,
#75371,#75372,#75373,#75374,#75375,#75376,#75377,#75378,#75379,#75380,#75381,
#75382,#75383,#75384,#75385,#75386,#75387,#75388,#75389,#75390,#75391,#75392,
#75393,#75394,#75395,#75396,#75397,#75398,#75399,#75400,#75401,#75402,#75403,
#75404,#75405,#75406,#75407,#75408,#75409,#75410,#75411,#75412,#75413,#75414,
#75415,#75416,#75417,#75418,#75419,#75420,#75421,#75422,#75423,#75424,#75425,
#75426,#75427,#75428,#75429,#75430,#75431,#75432,#75433,#75434,#75435,#75436,
#75437,#75438,#75439,#75440,#75441,#75442),.UNSPECIFIED.,.F.,.F.,(4,3,3,
3,3,3,3,3,3,3,3,3,3,3,3,3,3,3,3,3,3,3,3,3,3,3,3,3,3,3,3,3,3,3,3,3,3,3,3,
3,3,3,3,3,3,3,3,3,3,3,3,4),(78.5398163404196,78.6729079988692,78.8069522576926,
78.9214604159231,79.0450065295502,79.1646618515047,79.284199363364,79.4036716377764,
79.5231311343454,79.6427107500453,79.7623636819029,79.8822282974684,79.9098293249398,
80.0333754385669,80.1530309862348,80.2725687275557,80.3920412346678,80.5115009666695,
80.6310808199963,80.7507339910015,80.870598845506,80.8981982339565,81.0217443475836,
81.1413981074268,81.2609340620303,81.3804047871306,81.4998627454262,81.6194408504108,
81.7390922861601,81.8589554414028,81.8865671429733,82.0101132566004,82.1297701253563,
82.2493091702118,82.3687829608855,82.4882439540318,82.6078250265274,82.7274793933696,
82.8473453984445,82.87493605199,82.9984821656171,83.1181396337386,83.2376793157842,
83.3571537797169,83.4766154804869,83.5961973051156,83.7158524508728,83.8357192653888,
83.8633049610067,83.9826046296134,84.1017010849209,84.1188182559913),
 .UNSPECIFIED.);
#774=B_SPLINE_CURVE_WITH_KNOTS('',3,(#75446,#75447,#75448,#75449,#75450,
#75451,#75452),.UNSPECIFIED.,.F.,.F.,(4,2,1,4),(-4.09202352044837,-4.0499104913527,
-3.06154158233598,-2.07317267331961),.UNSPECIFIED.);
#775=B_SPLINE_CURVE_WITH_KNOTS('',3,(#75456,#75457,#75458,#75459,#75460),
 .UNSPECIFIED.,.F.,.F.,(4,1,4),(0.,0.989559462785669,1.12274180646041),
 .UNSPECIFIED.);
#776=B_SPLINE_CURVE_WITH_KNOTS('',3,(#75462,#75463,#75464,#75465,#75466,
#75467,#75468,#75469,#75470,#75471,#75472,#75473,#75474,#75475,#75476,#75477,
#75478,#75479,#75480,#75481,#75482,#75483,#75484,#75485,#75486,#75487,#75488,
#75489,#75490,#75491,#75492,#75493,#75494,#75495,#75496,#75497,#75498,#75499,
#75500,#75501,#75502,#75503,#75504,#75505,#75506,#75507,#75508,#75509,#75510,
#75511,#75512,#75513,#75514,#75515,#75516,#75517,#75518,#75519,#75520,#75521,
#75522,#75523,#75524,#75525,#75526,#75527,#75528,#75529,#75530,#75531,#75532,
#75533,#75534,#75535,#75536,#75537,#75538,#75539,#75540,#75541,#75542,#75543,
#75544,#75545,#75546,#75547,#75548,#75549,#75550,#75551,#75552,#75553,#75554,
#75555,#75556,#75557,#75558,#75559,#75560,#75561,#75562,#75563,#75564,#75565,
#75566,#75567,#75568,#75569,#75570,#75571,#75572,#75573,#75574,#75575,#75576,
#75577,#75578,#75579,#75580,#75581,#75582,#75583,#75584,#75585,#75586,#75587,
#75588,#75589,#75590,#75591,#75592,#75593,#75594,#75595,#75596,#75597,#75598,
#75599,#75600,#75601,#75602,#75603,#75604,#75605,#75606,#75607,#75608,#75609,
#75610,#75611,#75612,#75613,#75614,#75615,#75616,#75617,#75618,#75619,#75620,
#75621,#75622,#75623,#75624,#75625,#75626,#75627,#75628,#75629,#75630,#75631,
#75632,#75633),.UNSPECIFIED.,.F.,.F.,(4,3,3,3,3,3,3,3,3,3,3,3,3,3,3,3,3,
3,3,3,3,3,3,3,3,3,3,3,3,3,3,3,3,3,3,3,3,3,3,3,3,3,3,3,3,3,3,3,3,3,3,3,3,
3,3,3,3,4),(1.12274180646041,1.23382961778976,1.34478346838675,1.45565131443454,
1.56648094818943,1.67739799460759,1.78835809282476,1.89952234791358,1.97911892557135,
2.09267048898284,2.20601859343239,2.31925352705299,2.43241996957223,2.545562499232,
2.65880529165444,2.77209826670266,2.88559915987598,2.96867838835702,3.08237111938443,
3.19586878054423,3.30925828831477,3.42258402266246,3.53589026815068,3.64930230557827,
3.7627678535008,3.87644462139266,3.9582378511427,4.07166735977434,4.18489457552661,
4.29800943267414,4.41105683010432,4.5240815661709,4.63720945218514,4.75038895656566,
4.86378013355541,4.94779731392838,5.06133349396987,5.17466928122119,5.28789378838566,
5.40105171175323,5.51418764845825,5.62742688859855,5.74071800081016,5.85421981781746,
5.93735677671406,6.05089770957896,6.16423890038886,6.27746920605335,6.39063331211564,
6.50377580544888,6.61702213100323,6.73032063390784,6.84383025098836,6.92691623949973,
7.04689316765889,7.16661181918139,7.28626946610256,7.40592711302372),
 .UNSPECIFIED.);
#777=B_SPLINE_CURVE_WITH_KNOTS('',3,(#75635,#75636,#75637,#75638,#75639,
#75640,#75641,#75642,#75643,#75644,#75645,#75646,#75647,#75648,#75649,#75650,
#75651,#75652,#75653,#75654,#75655,#75656,#75657,#75658,#75659,#75660,#75661,
#75662,#75663,#75664,#75665,#75666,#75667,#75668,#75669,#75670,#75671,#75672,
#75673,#75674,#75675,#75676,#75677,#75678,#75679,#75680,#75681,#75682,#75683,
#75684,#75685,#75686,#75687,#75688,#75689,#75690,#75691,#75692,#75693,#75694,
#75695,#75696,#75697,#75698,#75699,#75700,#75701,#75702,#75703,#75704,#75705,
#75706,#75707,#75708,#75709,#75710,#75711,#75712,#75713,#75714,#75715,#75716,
#75717,#75718,#75719,#75720,#75721,#75722,#75723,#75724,#75725,#75726,#75727,
#75728,#75729,#75730,#75731,#75732,#75733,#75734,#75735,#75736,#75737,#75738,
#75739,#75740,#75741,#75742,#75743,#75744,#75745,#75746,#75747,#75748,#75749,
#75750,#75751,#75752,#75753,#75754,#75755,#75756,#75757,#75758,#75759,#75760,
#75761,#75762,#75763,#75764,#75765,#75766,#75767,#75768,#75769,#75770,#75771,
#75772,#75773,#75774,#75775,#75776,#75777,#75778,#75779,#75780,#75781,#75782,
#75783,#75784,#75785,#75786,#75787,#75788,#75789,#75790,#75791,#75792,#75793,
#75794,#75795,#75796,#75797,#75798,#75799,#75800,#75801,#75802,#75803,#75804,
#75805,#75806,#75807,#75808,#75809),.UNSPECIFIED.,.F.,.F.,(4,3,3,3,3,3,
3,3,3,3,3,3,3,3,3,3,3,3,3,3,3,3,3,3,3,3,3,3,3,3,3,3,3,3,3,3,3,3,3,3,3,3,
3,3,3,3,3,3,3,3,3,3,3,3,3,3,3,3,4),(7.40592711364008,7.52358787815993,7.64154429499719,
7.75966365595211,7.87808317498899,7.91647570228541,8.03000264719238,8.14332932527602,
8.25654480818245,8.36969380919324,8.4828209425382,8.59605163600875,8.70933433192551,
8.82282805122039,8.90603516507109,9.01956138335161,9.13288737703557,9.24610220203009,
9.35925057286215,9.47237710503925,9.5856072473793,9.69888941923431,9.81238266542286,
9.89559462785677,10.0091181085231,10.1224412796891,10.2356532323887,10.3487986865135,
10.4619222628744,10.5751494124928,10.6884285665954,10.8019187914085,10.8851540906425,
10.998679191203,11.1120040174162,11.2252176453697,11.3383647918229,11.4514900744797,
11.5647189382983,11.677999813562,11.7914917495915,11.8747135534281,11.9882384330826,
12.1015630395301,12.2147764485999,12.3279233774626,12.4410484442335,12.5542770965709,
12.6675577624936,12.7810494952956,12.8642730162138,12.9760889596331,13.087748618379,
13.1992993741481,13.3107884237349,13.4223163638858,13.5338668329265,13.6455583786727,
13.689112420188),.UNSPECIFIED.);
#778=B_SPLINE_CURVE_WITH_KNOTS('',3,(#75811,#75812,#75813,#75814,#75815,
#75816,#75817,#75818,#75819,#75820,#75821,#75822,#75823,#75824,#75825,#75826,
#75827,#75828,#75829,#75830,#75831,#75832,#75833,#75834,#75835,#75836,#75837,
#75838,#75839,#75840,#75841,#75842,#75843,#75844,#75845,#75846,#75847,#75848,
#75849,#75850,#75851,#75852,#75853,#75854,#75855,#75856,#75857,#75858,#75859,
#75860,#75861,#75862,#75863,#75864,#75865,#75866,#75867,#75868,#75869,#75870,
#75871,#75872,#75873,#75874,#75875,#75876,#75877,#75878,#75879,#75880,#75881,
#75882,#75883,#75884,#75885,#75886,#75887,#75888,#75889,#75890,#75891,#75892,
#75893,#75894,#75895,#75896,#75897,#75898,#75899,#75900,#75901,#75902,#75903,
#75904,#75905,#75906,#75907,#75908,#75909,#75910,#75911,#75912,#75913,#75914,
#75915,#75916,#75917,#75918,#75919,#75920,#75921,#75922,#75923,#75924,#75925,
#75926,#75927,#75928,#75929,#75930,#75931,#75932,#75933,#75934,#75935,#75936,
#75937,#75938,#75939,#75940,#75941,#75942,#75943,#75944,#75945,#75946,#75947,
#75948,#75949,#75950,#75951,#75952,#75953,#75954,#75955,#75956,#75957,#75958,
#75959,#75960,#75961,#75962,#75963,#75964,#75965,#75966,#75967,#75968,#75969,
#75970,#75971,#75972,#75973,#75974,#75975,#75976,#75977,#75978,#75979,#75980,
#75981,#75982),.UNSPECIFIED.,.F.,.F.,(4,3,3,3,3,3,3,3,3,3,3,3,3,3,3,3,3,
3,3,3,3,3,3,3,3,3,3,3,3,3,3,3,3,3,3,3,3,3,3,3,3,3,3,3,3,3,3,3,3,3,3,3,3,
3,3,3,3,4),(13.6891124208198,13.8538324789995,13.9673572877926,14.0806818189803,
14.1938951501528,14.3070419986254,14.4201669826556,14.5333955492639,14.6466761276639,
14.7601677710853,14.8433919417852,14.9569167108435,15.0702412020156,15.1834544930335,
15.2966013012875,15.4097262451101,15.5229547718542,15.636235310522,15.7497269149215,
15.8329514045708,15.946476150597,16.0598006178626,16.1730138844571,16.2861606678164,
16.3992855863179,16.5125140872826,16.6257945998772,16.7392861780446,16.8225108673565,
16.9360356348413,17.0493601240942,17.1625734129822,17.2757202188998,17.388845160183,
17.5020736840922,17.6153542197563,17.728845820912,17.8120703301422,17.9255950916193,
18.038919574788,18.1521328575499,18.2652796573108,18.3784045924182,18.4916331101721,
18.604913639683,18.7184052347656,18.8016297929279,18.9151545525914,19.0284790338638,
19.1416923146804,19.2548391124505,19.3679640455252,19.4811925611976,19.5944730885968,
19.7079646815442,19.7911892557135,19.9596425437774,19.972297727999),
 .UNSPECIFIED.);
#779=B_SPLINE_CURVE_WITH_KNOTS('',3,(#75984,#75985,#75986,#75987,#75988,
#75989,#75990,#75991,#75992,#75993,#75994,#75995,#75996,#75997,#75998,#75999,
#76000,#76001,#76002,#76003,#76004,#76005,#76006,#76007,#76008,#76009,#76010,
#76011,#76012,#76013,#76014,#76015,#76016,#76017,#76018,#76019,#76020,#76021,
#76022,#76023,#76024,#76025,#76026,#76027,#76028,#76029,#76030,#76031,#76032,
#76033,#76034,#76035,#76036,#76037,#76038,#76039,#76040,#76041,#76042,#76043,
#76044,#76045,#76046,#76047,#76048,#76049,#76050,#76051,#76052,#76053,#76054,
#76055,#76056,#76057,#76058,#76059,#76060,#76061,#76062,#76063,#76064,#76065,
#76066,#76067,#76068,#76069,#76070,#76071,#76072,#76073,#76074,#76075,#76076,
#76077,#76078,#76079,#76080,#76081,#76082,#76083,#76084,#76085,#76086,#76087,
#76088,#76089,#76090,#76091,#76092,#76093,#76094,#76095,#76096,#76097,#76098,
#76099,#76100,#76101,#76102,#76103,#76104,#76105,#76106,#76107,#76108,#76109,
#76110,#76111,#76112,#76113,#76114,#76115,#76116,#76117,#76118,#76119,#76120,
#76121,#76122,#76123,#76124,#76125,#76126,#76127,#76128,#76129,#76130,#76131,
#76132,#76133,#76134,#76135,#76136,#76137,#76138,#76139,#76140,#76141,#76142,
#76143,#76144,#76145,#76146,#76147,#76148,#76149,#76150,#76151,#76152,#76153,
#76154,#76155,#76156,#76157,#76158),.UNSPECIFIED.,.F.,.F.,(4,3,3,3,3,3,
3,3,3,3,3,3,3,3,3,3,3,3,3,3,3,3,3,3,3,3,3,3,3,3,3,3,3,3,3,3,3,3,3,3,3,3,
3,3,3,3,3,3,3,3,3,3,3,3,3,3,3,3,4),(19.972297728497,20.0839743113852,20.1955429489355,
20.3070508212707,20.4185450026315,20.5301439596349,20.6418068892393,20.753658132519,
20.7807487184992,20.8942734796944,21.0075979625469,21.1208112449716,21.2339580443754,
21.3470829791058,21.4603114964553,21.573592025546,21.6870836201873,21.7703081812849,
21.8838329423694,21.997157425104,22.1103707074066,22.2235175066839,22.3366424412841,
22.4498709584984,22.5631514874508,22.6766430819507,22.7598676440706,22.8733924054068,
22.9867168883998,23.0999301709649,23.2130769705083,23.3262019053778,23.4394304228638,
23.5527109520897,23.6662025468629,23.7494271068562,23.8629518680848,23.9762763509684,
24.0894896334229,24.2026364328546,24.3157613676117,24.4289898849852,24.5422704140983,
24.6557620087595,24.7389865696419,24.8525113308689,24.9658358137503,25.0790490962022,
25.1921958956312,25.3053208303848,25.4185493477547,25.5318298768639,25.6453214715208,
25.7285460324276,25.8462362390639,25.9636191281052,26.0808182478312,26.1978234044031,
26.2554830351787),.UNSPECIFIED.);
#780=B_SPLINE_CURVE_WITH_KNOTS('',3,(#76160,#76161,#76162,#76163,#76164,
#76165,#76166,#76167,#76168,#76169,#76170,#76171,#76172,#76173,#76174,#76175,
#76176,#76177,#76178,#76179,#76180,#76181,#76182,#76183,#76184,#76185,#76186,
#76187,#76188,#76189,#76190,#76191,#76192,#76193,#76194,#76195,#76196,#76197,
#76198,#76199,#76200,#76201,#76202,#76203,#76204,#76205,#76206,#76207,#76208,
#76209,#76210,#76211,#76212,#76213,#76214,#76215,#76216,#76217,#76218,#76219,
#76220,#76221,#76222,#76223,#76224,#76225,#76226,#76227,#76228,#76229,#76230,
#76231,#76232,#76233,#76234,#76235,#76236,#76237,#76238,#76239,#76240,#76241,
#76242,#76243,#76244,#76245,#76246,#76247,#76248,#76249,#76250,#76251,#76252,
#76253,#76254,#76255,#76256,#76257,#76258,#76259,#76260,#76261,#76262,#76263,
#76264,#76265,#76266,#76267,#76268,#76269,#76270,#76271,#76272,#76273,#76274,
#76275,#76276,#76277,#76278,#76279,#76280,#76281,#76282,#76283,#76284,#76285,
#76286,#76287,#76288,#76289,#76290,#76291,#76292,#76293,#76294,#76295,#76296,
#76297,#76298,#76299,#76300,#76301,#76302,#76303,#76304,#76305,#76306,#76307,
#76308,#76309,#76310,#76311,#76312,#76313,#76314,#76315,#76316,#76317,#76318,
#76319,#76320,#76321,#76322,#76323,#76324,#76325,#76326,#76327,#76328,#76329,
#76330,#76331),.UNSPECIFIED.,.F.,.F.,(4,3,3,3,3,3,3,3,3,3,3,3,3,3,3,3,3,
3,3,3,3,3,3,3,3,3,3,3,3,3,3,3,3,3,3,3,3,3,3,3,3,3,3,3,3,3,3,3,3,3,3,3,3,
3,3,3,3,4),(26.2554830357989,26.3757798650132,26.4963153854641,26.6172862332497,
26.7181054952133,26.8316302564529,26.9449547393473,27.0581680218127,27.1713148212552,
27.284439756023,27.3976682734069,27.5109488025305,27.6244403972019,27.707664957999,
27.8211897192396,27.934514202135,28.0477274846013,28.1608742840448,28.2739992188135,
28.3872277361983,28.5005082653227,28.6139998599949,28.6972244207846,28.8107491820277,
28.9240736649257,29.0372869473946,29.1504337468408,29.2635586816123,29.3767871989999,
29.4900677281271,29.603559322802,29.6867838835703,29.8003086448119,29.9136331277083,
30.0268464101756,30.1399932096202,30.25311814439,30.3663466617759,30.4796271909015,
30.5931187855748,30.676343346356,30.7898681075978,30.9031925904945,31.0164058729621,
31.1295526724069,31.2426776071769,31.3559061245631,31.4691866536889,31.5826782483624,
31.6659028091417,31.7778650422759,31.8896720534227,32.0013710373486,32.1130090117127,
32.2246998396253,32.3364127594324,32.4483027983562,32.5386683419253),
 .UNSPECIFIED.);
#781=B_SPLINE_CURVE_WITH_KNOTS('',3,(#76333,#76334,#76335,#76336,#76337,
#76338,#76339,#76340,#76341,#76342,#76343,#76344,#76345,#76346,#76347,#76348,
#76349,#76350,#76351,#76352,#76353,#76354,#76355,#76356,#76357,#76358,#76359,
#76360,#76361,#76362,#76363,#76364,#76365,#76366,#76367,#76368,#76369,#76370,
#76371,#76372,#76373,#76374,#76375,#76376,#76377,#76378,#76379,#76380,#76381,
#76382,#76383,#76384,#76385,#76386,#76387,#76388,#76389,#76390,#76391,#76392,
#76393,#76394,#76395,#76396,#76397,#76398,#76399,#76400,#76401,#76402,#76403,
#76404,#76405,#76406,#76407,#76408,#76409,#76410,#76411,#76412,#76413,#76414,
#76415,#76416,#76417,#76418,#76419,#76420,#76421,#76422,#76423,#76424,#76425,
#76426,#76427,#76428,#76429,#76430,#76431,#76432,#76433,#76434,#76435,#76436,
#76437,#76438,#76439,#76440,#76441,#76442,#76443,#76444,#76445,#76446,#76447,
#76448,#76449,#76450,#76451,#76452,#76453,#76454,#76455,#76456,#76457,#76458,
#76459,#76460,#76461,#76462,#76463,#76464,#76465,#76466,#76467,#76468,#76469,
#76470,#76471,#76472,#76473,#76474,#76475,#76476,#76477,#76478,#76479,#76480,
#76481,#76482,#76483,#76484,#76485,#76486,#76487,#76488,#76489,#76490,#76491,
#76492,#76493,#76494,#76495,#76496,#76497,#76498,#76499,#76500,#76501,#76502,
#76503,#76504),.UNSPECIFIED.,.F.,.F.,(4,3,3,3,3,3,3,3,3,3,3,3,3,3,3,3,3,
3,3,3,3,3,3,3,3,3,3,3,3,3,3,3,3,3,3,3,3,3,3,3,3,3,3,3,3,3,3,3,3,3,3,3,3,
3,3,3,3,4),(32.5386683423583,32.6554622719273,32.7689870331684,32.8823115160644,
32.9955247985313,33.1086715979755,33.2217965327449,33.3350250501304,33.4483055792554,
33.5617971739282,33.645021734713,33.758546495955,33.8718709788518,33.9850842613196,
34.0982310607647,34.211355995535,34.3245845129214,34.4378650420474,34.5513566367211,
34.6345811974987,34.7481059587407,34.8614304416375,34.9746437241053,35.0877905235503,
35.2009154583206,35.3141439757069,35.4274245048329,35.5409160995067,35.6241406602844,
35.7376654215263,35.850989904423,35.9642031868906,36.0773499863355,36.1904749211056,
36.3037034384918,36.4169839676176,36.5304755622912,36.6137001230701,36.727224884312,
36.8405493672087,36.9537626496764,37.0669094491213,37.1800343838914,37.2932629012777,
37.4065434304035,37.5200350250771,37.6032595858557,37.7167843470976,37.8301088299943,
37.943322112462,38.0564689119069,38.1695938466771,38.2828223640633,38.3961028931892,
38.5095944878629,38.5928190486414,38.7436256884796,38.821853649538),
 .UNSPECIFIED.);
#782=B_SPLINE_CURVE_WITH_KNOTS('',3,(#76506,#76507,#76508,#76509,#76510,
#76511,#76512,#76513,#76514,#76515,#76516,#76517,#76518,#76519,#76520,#76521,
#76522,#76523,#76524,#76525,#76526,#76527,#76528,#76529,#76530,#76531,#76532,
#76533,#76534,#76535,#76536,#76537,#76538,#76539,#76540,#76541,#76542,#76543,
#76544,#76545,#76546,#76547,#76548,#76549,#76550,#76551,#76552,#76553,#76554,
#76555,#76556,#76557,#76558,#76559,#76560,#76561,#76562,#76563,#76564,#76565,
#76566,#76567,#76568,#76569,#76570,#76571,#76572,#76573,#76574,#76575,#76576,
#76577,#76578,#76579,#76580,#76581,#76582,#76583,#76584,#76585,#76586,#76587,
#76588,#76589,#76590,#76591,#76592,#76593,#76594,#76595,#76596,#76597,#76598,
#76599,#76600,#76601,#76602,#76603,#76604,#76605,#76606,#76607,#76608,#76609,
#76610,#76611,#76612,#76613,#76614,#76615,#76616,#76617,#76618,#76619,#76620,
#76621,#76622,#76623,#76624,#76625,#76626,#76627,#76628,#76629,#76630,#76631,
#76632,#76633,#76634,#76635,#76636,#76637,#76638,#76639,#76640,#76641,#76642,
#76643,#76644,#76645,#76646,#76647,#76648,#76649,#76650,#76651,#76652,#76653,
#76654,#76655,#76656,#76657,#76658,#76659,#76660,#76661,#76662,#76663,#76664,
#76665,#76666,#76667,#76668,#76669,#76670,#76671,#76672,#76673,#76674,#76675,
#76676,#76677),.UNSPECIFIED.,.F.,.F.,(4,3,3,3,3,3,3,3,3,3,3,3,3,3,3,3,3,
3,3,3,3,3,3,3,3,3,3,3,3,3,3,3,3,3,3,3,3,3,3,3,3,3,3,3,3,3,3,3,3,3,3,3,3,
3,3,3,3,4),(38.8218536499613,38.933680849631,39.045423619069,39.1571288157185,
39.268922463434,39.3807581546526,39.4928019474818,39.5823785114271,39.695903272669,
39.8092277555658,39.9224410380335,40.0355878374784,40.1487127722487,40.2619412896349,
40.3752218187608,40.4887134134344,40.5719379742128,40.6854627354546,40.7987872183514,
40.912000500819,41.0251473002639,41.1382722350339,41.2515007524201,41.3647812815461,
41.4782728762197,41.5614974369984,41.6750221982403,41.7883466811369,41.9015599636045,
42.0147067630493,42.1278316978194,42.2410602152056,42.3543407443315,42.467832339005,
42.5510568997841,42.664581661026,42.7779061439229,42.8911194263906,43.0042662258358,
43.1173911606058,43.2306196779922,43.3439002071181,43.4573918017918,43.5406163625698,
43.6541411238117,43.7674656067085,43.8806788891762,43.993825688621,44.1069506233916,
44.2201791407778,44.3334596699036,44.4469512645772,44.5301758253555,44.6459654331288,
44.7615021168754,44.8768893229516,44.9921613263788,45.1050389567177),
 .UNSPECIFIED.);
#783=B_SPLINE_CURVE_WITH_KNOTS('',3,(#76679,#76680,#76681,#76682,#76683,
#76684,#76685,#76686,#76687,#76688,#76689,#76690,#76691,#76692,#76693,#76694,
#76695,#76696,#76697,#76698,#76699,#76700,#76701,#76702,#76703,#76704,#76705,
#76706,#76707,#76708,#76709,#76710,#76711,#76712,#76713,#76714,#76715,#76716,
#76717,#76718,#76719,#76720,#76721,#76722,#76723,#76724,#76725,#76726,#76727,
#76728,#76729,#76730,#76731,#76732,#76733,#76734,#76735,#76736,#76737,#76738,
#76739,#76740,#76741,#76742,#76743,#76744,#76745,#76746,#76747,#76748,#76749,
#76750,#76751,#76752,#76753,#76754,#76755,#76756,#76757,#76758,#76759,#76760,
#76761,#76762,#76763,#76764,#76765,#76766,#76767,#76768,#76769,#76770,#76771,
#76772,#76773,#76774,#76775,#76776,#76777,#76778,#76779,#76780,#76781,#76782,
#76783,#76784,#76785,#76786,#76787,#76788,#76789,#76790,#76791,#76792,#76793,
#76794,#76795,#76796,#76797,#76798,#76799,#76800,#76801,#76802,#76803,#76804,
#76805,#76806,#76807,#76808,#76809,#76810,#76811,#76812,#76813,#76814,#76815,
#76816,#76817,#76818,#76819,#76820,#76821,#76822,#76823,#76824,#76825,#76826,
#76827,#76828,#76829,#76830,#76831,#76832,#76833,#76834,#76835,#76836,#76837,
#76838,#76839,#76840,#76841,#76842,#76843,#76844,#76845,#76846,#76847,#76848,
#76849,#76850,#76851,#76852,#76853),.UNSPECIFIED.,.F.,.F.,(4,3,3,3,3,3,
3,3,3,3,3,3,3,3,3,3,3,3,3,3,3,3,3,3,3,3,3,3,3,3,3,3,3,3,3,3,3,3,3,3,3,3,
3,3,3,3,3,3,3,3,3,3,3,3,3,3,3,3,4),(45.1050389573923,45.2284792407024,45.3523119932056,
45.4766794256201,45.5197352881411,45.6332600493829,45.7465845322797,45.8597978147473,
45.9729446141923,46.0860695489624,46.1992980663486,46.3125785954745,46.4260701901482,
46.5092947509268,46.6228195121686,46.7361439950652,46.8493572775328,46.9625040769776,
47.0756290117477,47.1888575291339,47.3021380582597,47.4156296529332,47.4988542137125,
47.6123789749546,47.7257034578515,47.8389167403194,47.9520635397645,48.0651884745348,
48.1784169919213,48.2916975210474,48.4051891157212,48.4884136764982,48.60193843774,
48.7152629206367,48.8284762031042,48.9416230025491,49.0547479373191,49.1679764547053,
49.2812569838311,49.3947485785046,49.4779731392839,49.5914979005253,49.7048223834217,
49.8180356658889,49.9311824653334,50.0443074001032,50.157535917489,50.2708164466145,
50.3843080412877,50.4675326020695,50.5826190597494,50.6948414249508,50.8069563908371,
50.9190104334366,51.0363138909547,51.1484549007705,51.2606600856853,51.3730430728924,
51.3882242635088),.UNSPECIFIED.);
#784=B_SPLINE_CURVE_WITH_KNOTS('',3,(#76855,#76856,#76857,#76858,#76859,
#76860,#76861,#76862,#76863,#76864,#76865,#76866,#76867,#76868,#76869,#76870,
#76871,#76872,#76873,#76874,#76875,#76876,#76877,#76878,#76879,#76880,#76881,
#76882,#76883,#76884,#76885,#76886,#76887,#76888,#76889,#76890,#76891,#76892,
#76893,#76894,#76895,#76896,#76897,#76898,#76899,#76900,#76901,#76902,#76903,
#76904,#76905,#76906,#76907,#76908,#76909,#76910,#76911,#76912,#76913,#76914,
#76915,#76916,#76917,#76918,#76919,#76920,#76921,#76922,#76923,#76924,#76925,
#76926,#76927,#76928,#76929,#76930,#76931,#76932,#76933,#76934,#76935,#76936,
#76937,#76938,#76939,#76940,#76941,#76942,#76943,#76944,#76945,#76946,#76947,
#76948,#76949,#76950,#76951,#76952,#76953,#76954,#76955,#76956,#76957,#76958,
#76959,#76960,#76961,#76962,#76963,#76964,#76965,#76966,#76967,#76968,#76969,
#76970,#76971,#76972,#76973,#76974,#76975,#76976,#76977,#76978,#76979,#76980,
#76981,#76982,#76983,#76984,#76985,#76986,#76987,#76988,#76989,#76990,#76991,
#76992,#76993,#76994,#76995,#76996,#76997,#76998,#76999,#77000,#77001,#77002,
#77003,#77004,#77005,#77006,#77007,#77008,#77009,#77010,#77011,#77012,#77013,
#77014,#77015,#77016,#77017,#77018,#77019,#77020,#77021,#77022,#77023,#77024,
#77025,#77026),.UNSPECIFIED.,.F.,.F.,(4,3,3,3,3,3,3,3,3,3,3,3,3,3,3,3,3,
3,3,3,3,3,3,3,3,3,3,3,3,3,3,3,3,3,3,3,3,3,3,3,3,3,3,3,3,3,3,3,3,3,3,3,3,
3,3,3,3,4),(51.3882242638969,51.4570920648552,51.570616826096,51.6839413089917,
51.7971545914583,51.9103013909022,52.0234263256714,52.1366548430567,52.2499353721816,
52.3634269668544,52.4466515276409,52.5601762888804,52.6735007717747,52.7867140542399,
52.8998608536823,53.01298578845,53.1262143058338,53.2394948349572,53.3529864296283,
53.4362109904266,53.5497357516802,53.6630602345886,53.7762735170679,53.8894203165245,
54.0025452513062,54.1157737687038,54.229054297841,54.3425458925257,54.4257704532122,
54.5392952144374,54.6526196973177,54.7658329797689,54.8789797791976,54.9921047139516,
55.1053332313221,55.2186137604324,55.332105355091,55.4153299159979,55.5288546772276,
55.6421791601119,55.7553924425668,55.8685392419988,55.9816641767559,56.094892694129,
56.2081732232416,56.321664817902,56.4048893787836,56.5184141401249,56.6317386231211,
56.7449519056883,56.8580987052325,56.9712236401015,57.0844521575854,57.1977326868084,
57.3112242815769,57.3944488415693,57.5345561648524,57.6714095706393),
 .UNSPECIFIED.);
#785=B_SPLINE_CURVE_WITH_KNOTS('',3,(#77028,#77029,#77030,#77031,#77032,
#77033,#77034,#77035,#77036,#77037,#77038,#77039,#77040,#77041,#77042,#77043,
#77044,#77045,#77046,#77047,#77048,#77049,#77050,#77051,#77052,#77053,#77054,
#77055,#77056,#77057,#77058,#77059,#77060,#77061,#77062,#77063,#77064,#77065,
#77066,#77067,#77068,#77069,#77070,#77071,#77072,#77073,#77074,#77075,#77076,
#77077,#77078,#77079,#77080,#77081,#77082,#77083,#77084,#77085,#77086,#77087,
#77088,#77089,#77090,#77091,#77092,#77093,#77094,#77095,#77096,#77097,#77098,
#77099,#77100,#77101,#77102,#77103,#77104,#77105,#77106,#77107,#77108,#77109,
#77110,#77111,#77112,#77113,#77114,#77115,#77116,#77117,#77118,#77119,#77120,
#77121,#77122,#77123,#77124,#77125,#77126,#77127,#77128,#77129,#77130,#77131,
#77132,#77133,#77134,#77135,#77136,#77137,#77138,#77139,#77140,#77141,#77142,
#77143,#77144,#77145,#77146,#77147,#77148,#77149,#77150,#77151,#77152,#77153,
#77154,#77155,#77156,#77157,#77158,#77159,#77160,#77161,#77162,#77163,#77164,
#77165,#77166,#77167,#77168,#77169,#77170,#77171,#77172,#77173,#77174,#77175,
#77176,#77177,#77178,#77179,#77180,#77181,#77182,#77183,#77184,#77185,#77186,
#77187,#77188,#77189,#77190,#77191,#77192,#77193,#77194,#77195,#77196,#77197,
#77198,#77199,#77200,#77201,#77202),.UNSPECIFIED.,.F.,.F.,(4,3,3,3,3,3,
3,3,3,3,3,3,3,3,3,3,3,3,3,3,3,3,3,3,3,3,3,3,3,3,3,3,3,3,3,3,3,3,3,3,3,3,
3,3,3,3,3,3,3,3,3,3,3,3,3,3,3,3,4),(57.6714095710766,57.7836618564575,57.8958578534188,
58.0080436898146,58.1203406487452,58.2327029112056,58.3452626102307,58.3840083043549,
58.4975330655654,58.6108575484274,58.7240708308583,58.8372176302646,58.9503425649941,
59.0635710823374,59.1768516114188,59.2903432060463,59.3735677671406,59.4870925291998,
59.6004170129164,59.7136302962048,59.8267770964696,59.9399020320575,60.0531305502517,
60.1664110801815,60.2799026756419,60.3631272299263,60.4766519894433,60.589976470624,
60.7031897513823,60.8163365491278,60.9294614822111,61.0426899979435,61.1559705254315,
61.269462118513,61.352686692712,61.4662114543692,61.5795359376507,61.6927492204843,
61.8058960202756,61.9190209553724,62.0322494730526,62.1455300024545,62.2590215973724,
62.3422461554977,62.4557709232019,62.5690954125922,62.6823087015674,62.795455507522,
62.908580448792,63.0218089726113,63.1350895081424,63.2485811090971,63.3318056182834,
63.4461307719924,63.5602703458314,63.6742546758765,63.7881483652435,63.9020107023695,
63.9545948782563),.UNSPECIFIED.);
#786=B_SPLINE_CURVE_WITH_KNOTS('',3,(#77204,#77205,#77206,#77207,#77208,
#77209,#77210,#77211,#77212,#77213,#77214,#77215,#77216,#77217,#77218,#77219,
#77220,#77221,#77222,#77223,#77224,#77225,#77226,#77227,#77228,#77229,#77230,
#77231,#77232,#77233,#77234,#77235,#77236,#77237,#77238,#77239,#77240,#77241,
#77242,#77243,#77244,#77245,#77246,#77247,#77248,#77249,#77250,#77251,#77252,
#77253,#77254,#77255,#77256,#77257,#77258,#77259,#77260,#77261,#77262,#77263,
#77264,#77265,#77266,#77267,#77268,#77269,#77270,#77271,#77272,#77273,#77274,
#77275,#77276,#77277,#77278,#77279,#77280,#77281,#77282,#77283,#77284,#77285,
#77286,#77287,#77288,#77289,#77290,#77291,#77292,#77293,#77294,#77295,#77296,
#77297,#77298,#77299,#77300,#77301,#77302,#77303,#77304,#77305,#77306,#77307,
#77308,#77309,#77310,#77311,#77312,#77313,#77314,#77315,#77316,#77317,#77318,
#77319,#77320,#77321,#77322,#77323,#77324,#77325,#77326,#77327,#77328,#77329,
#77330,#77331,#77332,#77333,#77334,#77335,#77336,#77337,#77338,#77339,#77340,
#77341,#77342,#77343,#77344,#77345,#77346,#77347,#77348,#77349,#77350,#77351,
#77352,#77353,#77354,#77355,#77356,#77357,#77358,#77359,#77360,#77361,#77362,
#77363,#77364,#77365,#77366,#77367,#77368,#77369,#77370,#77371,#77372,#77373,
#77374,#77375),.UNSPECIFIED.,.F.,.F.,(4,3,3,3,3,3,3,3,3,3,3,3,3,3,3,3,3,
3,3,3,3,3,3,3,3,3,3,3,3,3,3,3,3,3,3,3,3,3,3,3,3,3,3,3,3,3,3,3,3,3,3,3,3,
3,3,3,3,4),(63.9545948786762,64.0820709043049,64.2105457420236,64.321365081069,
64.4348898520805,64.5482143444765,64.6614276362709,64.7745744448554,64.887699388563,
65.0009279145079,65.1142084519941,65.2277000546061,65.3109245438547,65.4244493536668,
65.5377738854928,65.6509872170703,65.7641340657149,65.8772590496844,65.9904876158749,
66.1037681936576,66.2172598361454,66.3004840066404,66.4140086154073,66.5273329461732,
66.6405460768399,66.753692725083,66.8668175095198,66.9800458790991,67.0933262616046,
67.2068177133869,67.2900434694261,67.4035683690671,67.5168929880384,67.6301064050546,
67.7432533372985,67.8563784028926,67.9696070470509,68.0828877008817,68.1963794153923,
68.2796029322117,68.3931280332697,68.5064528597947,68.6196664879459,68.7328136344833,
68.8459389171108,68.9591677807257,69.0724486556885,69.1859405912626,69.2691623949974,
69.3822861022301,69.4952102742419,69.6080242981855,69.7207735977211,69.8335034979201,
69.946337047213,70.0592261968963,70.1723185919593,70.2377801848146),
 .UNSPECIFIED.);
#787=B_SPLINE_CURVE_WITH_KNOTS('',3,(#77377,#77378,#77379,#77380,#77381,
#77382,#77383,#77384,#77385,#77386,#77387,#77388,#77389,#77390,#77391,#77392,
#77393,#77394,#77395,#77396,#77397,#77398,#77399,#77400,#77401,#77402,#77403,
#77404,#77405,#77406,#77407,#77408,#77409,#77410,#77411,#77412,#77413,#77414,
#77415,#77416,#77417,#77418,#77419,#77420,#77421,#77422,#77423,#77424,#77425,
#77426,#77427,#77428,#77429,#77430,#77431,#77432,#77433,#77434,#77435,#77436,
#77437,#77438,#77439,#77440,#77441,#77442,#77443,#77444,#77445,#77446,#77447,
#77448,#77449,#77450,#77451,#77452,#77453,#77454,#77455,#77456,#77457,#77458,
#77459,#77460,#77461,#77462,#77463,#77464,#77465,#77466,#77467,#77468,#77469,
#77470,#77471,#77472,#77473,#77474,#77475,#77476,#77477,#77478,#77479,#77480,
#77481,#77482,#77483,#77484,#77485,#77486,#77487,#77488,#77489,#77490,#77491,
#77492,#77493,#77494,#77495,#77496,#77497,#77498,#77499,#77500,#77501,#77502,
#77503,#77504,#77505,#77506,#77507,#77508,#77509,#77510,#77511,#77512,#77513,
#77514,#77515,#77516,#77517,#77518,#77519,#77520,#77521,#77522,#77523,#77524,
#77525,#77526,#77527,#77528,#77529,#77530,#77531,#77532,#77533,#77534,#77535,
#77536,#77537,#77538,#77539,#77540,#77541,#77542,#77543,#77544,#77545,#77546,
#77547,#77548,#77549,#77550,#77551),.UNSPECIFIED.,.F.,.F.,(4,3,3,3,3,3,
3,3,3,3,3,3,3,3,3,3,3,3,3,3,3,3,3,3,3,3,3,3,3,3,3,3,3,3,3,3,3,3,3,3,3,3,
3,3,3,3,3,3,3,3,3,3,3,3,3,3,3,3,4),(70.2377801854359,70.2587218577831,70.3722482718241,
70.4855743881732,70.5987892909973,70.7119376949459,70.8250642155941,70.93829427782,
71.0515763312372,71.1650693982657,71.2482813205688,71.361808193455,71.4751348264099,
71.5883502806829,71.7014992695103,71.8146264070972,71.9278571300423,72.0411398695331,
72.1546336547418,72.2378407833544,72.3513536455233,72.4646662250971,72.577867610997,
72.6910025419092,72.8041156574683,72.9173325254023,73.0306014822085,73.1440817724136,
73.2274002461401,73.340943030771,73.4542853818596,73.5675164236272,73.6806808427758,
73.7938232268161,73.9070687942867,74.0203661765388,74.1338740986414,74.2169597089258,
74.3304945869268,74.4438295583308,74.5570535478833,74.6702112510593,74.783347264545,
74.8965870376472,75.0098789377407,75.1233819464769,75.2065191717115,75.3199437476938,
75.4331678716963,75.5462807658169,75.6593273258388,75.7723523484109,75.8854822487551,
75.9986647322451,76.1120604195263,76.1960786344971,76.3301552019644,76.4628063366748,
76.5209654922348),.UNSPECIFIED.);
#788=B_SPLINE_CURVE_WITH_KNOTS('',3,(#77553,#77554,#77555,#77556,#77557,
#77558,#77559,#77560,#77561,#77562,#77563,#77564,#77565,#77566,#77567,#77568,
#77569,#77570,#77571,#77572,#77573,#77574,#77575,#77576,#77577,#77578,#77579,
#77580,#77581,#77582,#77583,#77584,#77585,#77586,#77587,#77588,#77589,#77590,
#77591,#77592,#77593,#77594,#77595),.UNSPECIFIED.,.F.,.F.,(4,3,3,3,3,3,
3,3,3,3,3,3,3,3,4),(76.5209654926156,76.6340655761394,76.7471410409961,
76.8603208092053,76.9735499264755,77.0869996187066,77.1856380972828,77.2977002565008,
77.4096095529624,77.52141302601,77.6331575453624,77.7451540359881,77.8569843073373,
77.9690639076012,78.0811435078651),.UNSPECIFIED.);
#789=B_SPLINE_CURVE_WITH_KNOTS('',3,(#77599,#77600,#77601,#77602,#77603,
#77604,#77605,#77606,#77607,#77608,#77609,#77610,#77611,#77612,#77613,#77614,
#77615,#77616,#77617),.UNSPECIFIED.,.F.,.F.,(4,3,3,3,3,3,4),(-80.1543164856399,
-80.0391241641348,-79.9240212140723,-79.8089315194197,-79.6938570316342,
-79.5786881247276,-79.4902472066036),.UNSPECIFIED.);
#790=B_SPLINE_CURVE_WITH_KNOTS('',3,(#77619,#77620,#77621,#77622,#77623,
#77624,#77625,#77626,#77627,#77628,#77629,#77630,#77631,#77632,#77633,#77634,
#77635,#77636,#77637,#77638,#77639,#77640,#77641,#77642,#77643,#77644,#77645,
#77646,#77647,#77648,#77649,#77650,#77651,#77652,#77653,#77654,#77655,#77656,
#77657,#77658,#77659,#77660,#77661,#77662,#77663,#77664,#77665,#77666,#77667,
#77668,#77669,#77670,#77671,#77672,#77673,#77674,#77675,#77676,#77677,#77678,
#77679,#77680,#77681,#77682,#77683,#77684,#77685,#77686,#77687,#77688,#77689,
#77690,#77691,#77692,#77693,#77694,#77695,#77696,#77697,#77698,#77699,#77700,
#77701,#77702,#77703,#77704,#77705,#77706,#77707,#77708,#77709,#77710,#77711,
#77712,#77713,#77714,#77715,#77716,#77717,#77718,#77719,#77720,#77721,#77722,
#77723,#77724,#77725,#77726,#77727,#77728,#77729,#77730,#77731,#77732,#77733,
#77734,#77735,#77736,#77737,#77738,#77739,#77740,#77741,#77742,#77743,#77744,
#77745,#77746,#77747,#77748,#77749,#77750,#77751,#77752,#77753,#77754,#77755,
#77756,#77757,#77758,#77759,#77760,#77761,#77762,#77763,#77764,#77765,#77766,
#77767,#77768,#77769,#77770,#77771,#77772,#77773,#77774,#77775,#77776,#77777,
#77778,#77779,#77780,#77781,#77782,#77783,#77784,#77785,#77786,#77787,#77788,
#77789,#77790,#77791,#77792,#77793),.UNSPECIFIED.,.F.,.F.,(4,3,3,3,3,3,
3,3,3,3,3,3,3,3,3,3,3,3,3,3,3,3,3,3,3,3,3,3,3,3,3,3,3,3,3,3,3,3,3,3,3,3,
3,3,3,3,3,3,3,3,3,3,3,3,3,3,3,3,4),(-79.4902472059884,-79.3517265673382,
-79.2109681612931,-79.1659475766232,-79.0532136190919,-78.9406994479234,
-78.8283078716632,-78.7159927295406,-78.6037079777077,-78.4913266274999,
-78.3788983233038,-78.2662576917523,-78.1775786676064,-78.0640108726353,
-77.9506460297327,-77.8373940448906,-77.7242102710254,-77.6110501621686,
-77.4977899323899,-77.3844793408537,-77.2709617991828,-77.1892097585897,
-77.0755011786657,-76.9619871711567,-76.8485810089956,-76.7352383459469,
-76.6219149308344,-76.5084858806415,-76.3950031491562,-76.281310178521,
-76.200840849573,-76.087393653663,-75.9741482172093,-75.8610148098562,-75.7479485673088,
-75.6349047254006,-75.521757871416,-75.408559211561,-75.2951498661576,-75.2124719405563,
-75.0989187057383,-74.985565332653,-74.872322911805,-74.7591467814323,-74.6459923785403,
-74.5327348079852,-74.4194251795107,-74.3059058225146,-74.2241030315395,
-74.1105453008867,-73.9971867919935,-73.8839388466325,-73.7707568133287,
-73.6575961388973,-73.5443317745932,-73.431015050961,-73.3174881929719,
-73.2357341225228,-73.2070618994239),.UNSPECIFIED.);
#791=B_SPLINE_CURVE_WITH_KNOTS('',3,(#77795,#77796,#77797,#77798,#77799,
#77800,#77801,#77802,#77803,#77804,#77805,#77806,#77807,#77808,#77809,#77810,
#77811,#77812,#77813,#77814,#77815,#77816,#77817,#77818,#77819,#77820,#77821,
#77822,#77823,#77824,#77825,#77826,#77827,#77828,#77829,#77830,#77831,#77832,
#77833,#77834,#77835,#77836,#77837,#77838,#77839,#77840,#77841,#77842,#77843,
#77844,#77845,#77846,#77847,#77848,#77849,#77850,#77851,#77852,#77853,#77854,
#77855,#77856,#77857,#77858,#77859,#77860,#77861,#77862,#77863,#77864,#77865,
#77866,#77867,#77868,#77869,#77870,#77871,#77872,#77873,#77874,#77875,#77876,
#77877,#77878,#77879,#77880,#77881,#77882,#77883,#77884,#77885,#77886,#77887,
#77888,#77889,#77890,#77891,#77892,#77893,#77894,#77895,#77896,#77897,#77898,
#77899,#77900,#77901,#77902,#77903,#77904,#77905,#77906,#77907,#77908,#77909,
#77910,#77911,#77912,#77913,#77914,#77915,#77916,#77917,#77918,#77919,#77920,
#77921,#77922,#77923,#77924,#77925,#77926,#77927,#77928,#77929,#77930,#77931,
#77932,#77933,#77934,#77935,#77936,#77937,#77938,#77939,#77940,#77941,#77942,
#77943,#77944,#77945,#77946,#77947,#77948,#77949,#77950,#77951,#77952,#77953,
#77954,#77955,#77956,#77957,#77958,#77959,#77960,#77961,#77962,#77963,#77964,
#77965,#77966),.UNSPECIFIED.,.F.,.F.,(4,3,3,3,3,3,3,3,3,3,3,3,3,3,3,3,3,
3,3,3,3,3,3,3,3,3,3,3,3,3,3,3,3,3,3,3,3,3,3,3,3,3,3,3,3,3,3,3,3,3,3,3,3,
3,3,3,3,4),(-73.2070618990321,-73.094069831628,-72.9812742087319,-72.8685866160268,
-72.7559614314162,-72.6433531292006,-72.5306393615614,-72.4178673681802,
-72.3048943277318,-72.2473652135061,-72.1338212398093,-72.0204770062008,
-71.9072436423942,-71.7940764694817,-71.680930907221,-71.5676819239201,
-71.4543807539108,-71.3408695399352,-71.2589963044894,-71.1454530983356,
-71.0321095918641,-70.9188769297667,-70.805710431801,-70.6925655163593,
-70.5793171308957,-70.4660165322699,-70.3525058392914,-70.2706273954727,
-70.1570868730669,-70.0437461340144,-69.9305162883949,-69.8173526506773,
-69.7042106340253,-69.5909651837839,-69.4776675450336,-69.3641598157257,
-69.282258486456,-69.1687163625939,-69.0553739871095,-68.9421424849538,
-68.8289771737097,-68.7158334696301,-68.6025863240228,-68.4892869829797,
-68.3757775610722,-68.2938895774393,-68.1803476792412,-68.0670055285297,
-67.9537742504107,-67.8406091620442,-67.7274656792597,-67.6142187506927,
-67.5009196246352,-67.3874104116913,-67.3055206684225,-67.178427761061,
-67.051152176854,-66.9238765926471),.UNSPECIFIED.);
#792=B_SPLINE_CURVE_WITH_KNOTS('',3,(#77968,#77969,#77970,#77971,#77972,
#77973,#77974,#77975,#77976,#77977,#77978,#77979,#77980,#77981,#77982,#77983,
#77984,#77985,#77986,#77987,#77988,#77989,#77990,#77991,#77992,#77993,#77994,
#77995,#77996,#77997,#77998,#77999,#78000,#78001,#78002,#78003,#78004,#78005,
#78006,#78007,#78008,#78009,#78010,#78011,#78012,#78013,#78014,#78015,#78016,
#78017,#78018,#78019,#78020,#78021,#78022,#78023,#78024,#78025,#78026,#78027,
#78028,#78029,#78030,#78031,#78032,#78033,#78034,#78035,#78036,#78037,#78038,
#78039,#78040,#78041,#78042,#78043,#78044,#78045,#78046,#78047,#78048,#78049,
#78050,#78051,#78052,#78053,#78054,#78055,#78056,#78057,#78058,#78059,#78060,
#78061,#78062,#78063,#78064,#78065,#78066,#78067,#78068,#78069,#78070,#78071,
#78072,#78073,#78074,#78075,#78076,#78077,#78078,#78079,#78080,#78081,#78082,
#78083,#78084,#78085,#78086,#78087,#78088,#78089,#78090,#78091,#78092,#78093,
#78094,#78095,#78096,#78097,#78098,#78099,#78100,#78101,#78102,#78103,#78104,
#78105,#78106,#78107,#78108,#78109,#78110,#78111,#78112,#78113,#78114,#78115,
#78116,#78117,#78118,#78119,#78120,#78121,#78122,#78123,#78124,#78125,#78126,
#78127,#78128,#78129,#78130,#78131,#78132,#78133,#78134,#78135,#78136,#78137,
#78138,#78139,#78140,#78141,#78142),.UNSPECIFIED.,.F.,.F.,(4,3,3,3,3,3,
3,3,3,3,3,3,3,3,3,3,3,3,3,3,3,3,3,3,3,3,3,3,3,3,3,3,3,3,3,3,3,3,3,3,3,3,
3,3,3,3,3,3,3,3,3,3,3,3,3,3,3,3,4),(-66.9238765922442,-66.8096120241358,
-66.6953173784797,-66.5808654330042,-66.4663215349714,-66.3515549173767,
-66.3171517594058,-66.2036099273518,-66.0902678470314,-65.9770366418524,
-65.8638716288386,-65.7507282236856,-65.6374813756652,-65.5241823318996,
-65.4106732030888,-65.3287828503891,-65.2152410584719,-65.1018990185986,
-64.9886678540232,-64.8755028816931,-64.7623595172278,-64.649112709571,
-64.5358137060477,-64.4223046167831,-64.3404139413724,-64.2268721714598,
-64.113530154438,-64.0002990132152,-63.8871340646948,-63.7739907244533,
-63.6607439414676,-63.5474449629013,-63.4339358987536,-63.3520450323557,
-63.2385032414485,-63.1251612029106,-63.0119300398699,-62.8987650692705,
-62.7856217067293,-62.6723749012822,-62.5590759001311,-62.4455668134755,
-62.363676123339,-62.2501343384519,-62.136792306014,-62.0235611491169,-61.9103961846934,
-61.7972528283492,-61.6840060290806,-61.570707034107,-61.457197953551,-61.3753072143223,
-61.2630150155433,-61.1508849762602,-61.0388702925052,-60.926894102488,
-60.8149424610336,-60.702909004196,-60.6406912850646),.UNSPECIFIED.);
#793=B_SPLINE_CURVE_WITH_KNOTS('',3,(#78144,#78145,#78146,#78147,#78148,
#78149,#78150,#78151,#78152,#78153,#78154,#78155,#78156,#78157,#78158,#78159,
#78160,#78161,#78162,#78163,#78164,#78165,#78166,#78167,#78168,#78169,#78170,
#78171,#78172,#78173,#78174,#78175,#78176,#78177,#78178,#78179,#78180,#78181,
#78182,#78183,#78184,#78185,#78186,#78187,#78188,#78189,#78190,#78191,#78192,
#78193,#78194,#78195,#78196,#78197,#78198,#78199,#78200,#78201,#78202,#78203,
#78204,#78205,#78206,#78207,#78208,#78209,#78210,#78211,#78212,#78213,#78214,
#78215,#78216,#78217,#78218,#78219,#78220,#78221,#78222,#78223,#78224,#78225,
#78226,#78227,#78228,#78229,#78230,#78231,#78232,#78233,#78234,#78235,#78236,
#78237,#78238,#78239,#78240,#78241,#78242,#78243,#78244,#78245,#78246,#78247,
#78248,#78249,#78250,#78251,#78252,#78253,#78254,#78255,#78256,#78257,#78258,
#78259,#78260,#78261,#78262,#78263,#78264,#78265,#78266,#78267,#78268,#78269,
#78270,#78271,#78272,#78273,#78274,#78275,#78276,#78277,#78278,#78279,#78280,
#78281,#78282,#78283,#78284,#78285,#78286,#78287,#78288,#78289,#78290,#78291,
#78292,#78293,#78294,#78295,#78296,#78297,#78298,#78299,#78300,#78301,#78302,
#78303,#78304,#78305,#78306,#78307,#78308,#78309,#78310,#78311,#78312,#78313,
#78314,#78315),.UNSPECIFIED.,.F.,.F.,(4,3,3,3,3,3,3,3,3,3,3,3,3,3,3,3,3,
3,3,3,3,3,3,3,3,3,3,3,3,3,3,3,3,3,3,3,3,3,3,3,3,3,3,3,3,3,3,3,3,3,3,3,3,
3,3,3,3,4),(-60.6406912846449,-60.4961271710891,-60.3869383053055,-60.2733965198114,
-60.160054486785,-60.0468233293113,-59.9336583643241,-59.8205150074302,
-59.7072682076384,-59.5939692121555,-59.4804601311195,-59.3985693962888,
-59.285027611619,-59.1716855794305,-59.0584544228024,-58.9452894586669,
-58.8321461026291,-58.7188993036937,-58.6056003090684,-58.4920912288815,
-58.4102004872721,-58.2966587026979,-58.1833166706118,-58.0700855140902,
-57.9569205500651,-57.8437771941414,-57.7305303953247,-57.6172314008211,
-57.5037223207591,-57.4218315782554,-57.308289793439,-57.194947761104,-57.0817166043295,
-56.968551640048,-56.855408283865,-56.7421614847864,-56.6288624900191,-56.5153534096935,
-56.4334626692387,-56.3199208845285,-56.2065788523017,-56.0933476956365,
-55.9801827314653,-55.8670393753932,-55.7537925764259,-55.6404935817701,
-55.5269845015553,-55.445093760222,-55.3315519755118,-55.2182099432853,
-55.1049787866209,-54.9918138224506,-54.8786704663798,-54.7654236674143,
-54.6521246727606,-54.5386155925483,-54.4567248512052,-54.3575059778849),
 .UNSPECIFIED.);
#794=B_SPLINE_CURVE_WITH_KNOTS('',3,(#78317,#78318,#78319,#78320,#78321,
#78322,#78323,#78324,#78325,#78326,#78327,#78328,#78329,#78330,#78331,#78332,
#78333,#78334,#78335,#78336,#78337,#78338,#78339,#78340,#78341,#78342,#78343,
#78344,#78345,#78346,#78347,#78348,#78349,#78350,#78351,#78352,#78353,#78354,
#78355,#78356,#78357,#78358,#78359,#78360,#78361,#78362,#78363,#78364,#78365,
#78366,#78367,#78368,#78369,#78370,#78371,#78372,#78373,#78374,#78375,#78376,
#78377,#78378,#78379,#78380,#78381,#78382,#78383,#78384,#78385,#78386,#78387,
#78388,#78389,#78390,#78391,#78392,#78393,#78394,#78395,#78396,#78397,#78398,
#78399,#78400,#78401,#78402,#78403,#78404,#78405,#78406,#78407,#78408,#78409,
#78410,#78411,#78412,#78413,#78414,#78415,#78416,#78417,#78418,#78419,#78420,
#78421,#78422,#78423,#78424,#78425,#78426,#78427,#78428,#78429,#78430,#78431,
#78432,#78433,#78434,#78435,#78436,#78437,#78438,#78439,#78440,#78441,#78442,
#78443,#78444,#78445,#78446,#78447,#78448,#78449,#78450,#78451,#78452,#78453,
#78454,#78455,#78456,#78457,#78458,#78459,#78460,#78461,#78462,#78463,#78464,
#78465,#78466,#78467,#78468,#78469,#78470,#78471,#78472,#78473,#78474,#78475,
#78476,#78477,#78478,#78479,#78480,#78481,#78482,#78483,#78484,#78485,#78486,
#78487,#78488),.UNSPECIFIED.,.F.,.F.,(4,3,3,3,3,3,3,3,3,3,3,3,3,3,3,3,3,
3,3,3,3,3,3,3,3,3,3,3,3,3,3,3,3,3,3,3,3,3,3,3,3,3,3,3,3,3,3,3,3,3,3,3,3,
3,3,3,3,4),(-54.3575059774559,-54.2454588905404,-54.133550138024,-54.021732773941,
-53.9099599987096,-53.7981045612228,-53.686213474605,-53.5741099150809,
-53.4683559421885,-53.3548141574668,-53.2414721252284,-53.1282409685518,
-53.0150760043692,-52.9019326482856,-52.7886858493072,-52.6753868546403,
-52.5618777744148,-52.4799870331718,-52.3664452484487,-52.2531032162091,
-52.1398720595313,-52.0267070953474,-51.9135637392627,-51.8003169402832,
-51.6870179456152,-51.5735088653886,-51.4916181241551,-51.3780763394296,
-51.2647343071875,-51.1515031505072,-51.0383381863207,-50.9251948302337,
-50.8119480312515,-50.6986490365809,-50.5851399563517,-50.5032492151384,
-50.3897074304145,-50.2763653981741,-50.1631342414952,-50.0499692773104,
-49.9368259212247,-49.8235791222442,-49.7102801275752,-49.5967710473476,
-49.5148803061217,-49.4013385213976,-49.2879964891568,-49.1747653324776,
-49.0616003682925,-48.9484570122066,-48.8352102132257,-48.7219112185563,
-48.6084021383284,-48.5265113971049,-48.4049309512446,-48.2836454588316,
-48.1627910448778,-48.0743206711006),.UNSPECIFIED.);
#795=B_SPLINE_CURVE_WITH_KNOTS('',3,(#78490,#78491,#78492,#78493,#78494,
#78495,#78496,#78497,#78498,#78499,#78500,#78501,#78502,#78503,#78504,#78505,
#78506,#78507,#78508,#78509,#78510,#78511,#78512,#78513,#78514,#78515,#78516,
#78517,#78518,#78519,#78520,#78521,#78522,#78523,#78524,#78525,#78526,#78527,
#78528,#78529,#78530,#78531,#78532,#78533,#78534,#78535,#78536,#78537,#78538,
#78539,#78540,#78541,#78542,#78543,#78544,#78545,#78546,#78547,#78548,#78549,
#78550,#78551,#78552,#78553,#78554,#78555,#78556,#78557,#78558,#78559,#78560,
#78561,#78562,#78563,#78564,#78565,#78566,#78567,#78568,#78569,#78570,#78571,
#78572,#78573,#78574,#78575,#78576,#78577,#78578,#78579,#78580,#78581,#78582,
#78583,#78584,#78585,#78586,#78587,#78588,#78589,#78590,#78591,#78592,#78593,
#78594,#78595,#78596,#78597,#78598,#78599,#78600,#78601,#78602,#78603,#78604,
#78605,#78606,#78607,#78608,#78609,#78610,#78611,#78612,#78613,#78614,#78615,
#78616,#78617,#78618,#78619,#78620,#78621,#78622,#78623,#78624,#78625,#78626,
#78627,#78628,#78629,#78630,#78631,#78632,#78633,#78634,#78635,#78636,#78637,
#78638,#78639,#78640,#78641,#78642,#78643,#78644,#78645,#78646,#78647,#78648,
#78649,#78650,#78651,#78652,#78653,#78654,#78655,#78656,#78657,#78658,#78659,
#78660,#78661,#78662,#78663,#78664),.UNSPECIFIED.,.F.,.F.,(4,3,3,3,3,3,
3,3,3,3,3,3,3,3,3,3,3,3,3,3,3,3,3,3,3,3,3,3,3,3,3,3,3,3,3,3,3,3,3,3,3,3,
3,3,3,3,3,3,3,3,3,3,3,3,3,3,3,3,4),(-48.0743206707057,-47.9577457517774,
-47.8409315728867,-47.7239904093878,-47.6067638311109,-47.5381424880882,
-47.424600703364,-47.3112586711233,-47.1980275144443,-47.0848625502592,
-46.9717191941734,-46.8584723951926,-46.7451734005234,-46.6316643202955,
-46.5497735790715,-46.4362317943472,-46.3228897621064,-46.2096586054272,
-46.096493641242,-45.9833502851561,-45.8701034861752,-45.7568044915059,
-45.6432954112779,-45.5614046700548,-45.4478628853305,-45.3345208530897,
-45.2212896964106,-45.1081247322255,-44.9949813761396,-44.8817345771588,
-44.7684355824895,-44.6549265022615,-44.5730357610381,-44.4594939763138,
-44.3461519440729,-44.2329207873937,-44.1197558232086,-44.0066124671228,
-43.8933656681419,-43.7800666734726,-43.6665575932446,-43.5846668520214,
-43.4711250672973,-43.3577830350565,-43.2445518783773,-43.1313869141921,
-43.0182435581061,-42.9049967591252,-42.7916977644559,-42.6781886842278,
-42.5962979430046,-42.4844449995889,-42.3727487802306,-42.2611619429958,
-42.1496373311032,-42.0380799748944,-41.9265002728943,-41.814793727549,
-41.791135364003),.UNSPECIFIED.);
#796=B_SPLINE_CURVE_WITH_KNOTS('',3,(#78666,#78667,#78668,#78669,#78670,
#78671,#78672,#78673,#78674,#78675,#78676,#78677,#78678,#78679,#78680,#78681,
#78682,#78683,#78684,#78685,#78686,#78687,#78688,#78689,#78690,#78691,#78692,
#78693,#78694,#78695,#78696,#78697,#78698,#78699,#78700,#78701,#78702,#78703,
#78704,#78705,#78706,#78707,#78708,#78709,#78710,#78711,#78712,#78713,#78714,
#78715,#78716,#78717,#78718,#78719,#78720,#78721,#78722,#78723,#78724,#78725,
#78726,#78727,#78728,#78729,#78730,#78731,#78732,#78733,#78734,#78735,#78736,
#78737,#78738,#78739,#78740,#78741,#78742,#78743,#78744,#78745,#78746,#78747,
#78748,#78749,#78750,#78751,#78752,#78753,#78754,#78755,#78756,#78757,#78758,
#78759,#78760,#78761,#78762,#78763,#78764,#78765,#78766,#78767,#78768,#78769,
#78770,#78771,#78772,#78773,#78774,#78775,#78776,#78777,#78778,#78779,#78780,
#78781,#78782,#78783,#78784,#78785,#78786,#78787,#78788,#78789,#78790,#78791,
#78792,#78793,#78794,#78795,#78796,#78797,#78798,#78799,#78800,#78801,#78802,
#78803,#78804,#78805,#78806,#78807,#78808,#78809,#78810,#78811,#78812,#78813,
#78814,#78815,#78816,#78817,#78818,#78819,#78820,#78821,#78822,#78823,#78824,
#78825,#78826,#78827,#78828,#78829,#78830,#78831,#78832,#78833,#78834,#78835,
#78836,#78837),.UNSPECIFIED.,.F.,.F.,(4,3,3,3,3,3,3,3,3,3,3,3,3,3,3,3,3,
3,3,3,3,3,3,3,3,3,3,3,3,3,3,3,3,3,3,3,3,3,3,3,3,3,3,3,3,3,3,3,3,3,3,3,3,
3,3,3,3,4),(-41.791135363526,-41.6240474718283,-41.6079290339879,-41.4943872492642,
-41.3810452170238,-41.267814060345,-41.1546490961603,-41.0415057400747,
-40.9282589410942,-40.8149599464254,-40.7014508661978,-40.6195601249712,
-40.506018340247,-40.3926763080061,-40.2794451513269,-40.1662801871417,
-40.0531368310557,-39.9398900320748,-39.8265910374055,-39.7130819571774,
-39.6311912159545,-39.5176494312303,-39.4043073989894,-39.2910762423102,
-39.177911278125,-39.064767922039,-38.951521123058,-38.8382221283887,-38.7247130481606,
-38.6428223069378,-38.5292805222136,-38.4159384899729,-38.3027073332938,
-38.1895423691087,-38.0763990130228,-37.963152214042,-37.8498532193727,
-37.7363441391448,-37.6544533979211,-37.5409116131968,-37.427569580956,
-37.3143384242768,-37.2011734600916,-37.0880301040056,-36.9747833050247,
-36.8614843103553,-36.7479752301273,-36.6660844889043,-36.55254270418,-36.4392006719391,
-36.3259695152599,-36.2128045510747,-36.0996611949886,-35.9864143960077,
-35.8731154013383,-35.7596063211103,-35.6777155798876,-35.5079500563463),
 .UNSPECIFIED.);
#797=B_SPLINE_CURVE_WITH_KNOTS('',3,(#78839,#78840,#78841,#78842,#78843,
#78844,#78845,#78846,#78847,#78848,#78849,#78850,#78851,#78852,#78853,#78854,
#78855,#78856,#78857,#78858,#78859,#78860,#78861,#78862,#78863,#78864,#78865,
#78866,#78867,#78868,#78869,#78870,#78871,#78872,#78873,#78874,#78875,#78876,
#78877,#78878,#78879,#78880,#78881,#78882,#78883,#78884,#78885,#78886,#78887,
#78888,#78889,#78890,#78891,#78892,#78893,#78894,#78895,#78896,#78897,#78898,
#78899,#78900,#78901,#78902,#78903,#78904,#78905,#78906,#78907,#78908,#78909,
#78910,#78911,#78912,#78913,#78914,#78915,#78916,#78917,#78918,#78919,#78920,
#78921,#78922,#78923,#78924,#78925,#78926,#78927,#78928,#78929,#78930,#78931,
#78932,#78933,#78934,#78935,#78936,#78937,#78938,#78939,#78940,#78941,#78942,
#78943,#78944,#78945,#78946,#78947,#78948,#78949,#78950,#78951,#78952,#78953,
#78954,#78955,#78956,#78957,#78958,#78959,#78960,#78961,#78962,#78963,#78964,
#78965,#78966,#78967,#78968,#78969,#78970,#78971,#78972,#78973,#78974,#78975,
#78976,#78977,#78978,#78979,#78980,#78981,#78982,#78983,#78984,#78985,#78986,
#78987,#78988,#78989,#78990,#78991,#78992,#78993,#78994,#78995,#78996,#78997,
#78998,#78999,#79000,#79001,#79002,#79003,#79004,#79005,#79006,#79007,#79008,
#79009,#79010,#79011,#79012,#79013),.UNSPECIFIED.,.F.,.F.,(4,3,3,3,3,3,
3,3,3,3,3,3,3,3,3,3,3,3,3,3,3,3,3,3,3,3,3,3,3,3,3,3,3,3,3,3,3,3,3,3,3,3,
3,3,3,3,3,3,3,3,3,3,3,3,3,3,3,3,4),(-35.5079500557628,-35.39624939281,-35.2846613019993,
-35.1731385997513,-35.0616342152309,-34.9500286488472,-34.8383632661675,
-34.7265074019316,-34.6893466708709,-34.5758048861466,-34.4624628539057,
-34.3492316972264,-34.2360667330411,-34.1229233769552,-34.0096765779742,
-33.8963775833048,-33.7828685030767,-33.7009777618542,-33.5874359771301,
-33.4740939448894,-33.3608627882104,-33.2476978240254,-33.1345544679397,
-33.0213076689589,-32.9080086742896,-32.7944995940618,-32.7126088528375,
-32.5990670681136,-32.4857250358731,-32.3724938791943,-32.2593289150094,
-32.1461855589239,-32.0329387599433,-31.9196397652743,-31.8061306850466,
-31.7242399438208,-31.6106981590953,-31.4973561268532,-31.3841249701728,
-31.2709600059863,-31.1578166498988,-31.0445698509166,-30.9312708562461,
-30.8177617760168,-30.735871034804,-30.6223292500811,-30.5089872178417,
-30.395756061164,-30.2825910969801,-30.1694477408954,-30.0562009419158,
-29.9429019472477,-29.8293928670209,-29.7475021257873,-29.6296432390198,
-29.5120953361175,-29.3947339709123,-29.2775721209935,-29.2247647491666),
 .UNSPECIFIED.);
#798=B_SPLINE_CURVE_WITH_KNOTS('',3,(#79015,#79016,#79017,#79018,#79019,
#79020,#79021,#79022,#79023,#79024,#79025,#79026,#79027,#79028,#79029,#79030,
#79031,#79032,#79033,#79034,#79035,#79036,#79037,#79038,#79039,#79040,#79041,
#79042,#79043,#79044,#79045,#79046,#79047,#79048,#79049,#79050,#79051,#79052,
#79053,#79054,#79055,#79056,#79057,#79058,#79059,#79060,#79061,#79062,#79063,
#79064,#79065,#79066,#79067,#79068,#79069,#79070,#79071,#79072,#79073,#79074,
#79075,#79076,#79077,#79078,#79079,#79080,#79081,#79082,#79083,#79084,#79085,
#79086,#79087,#79088,#79089,#79090,#79091,#79092,#79093,#79094,#79095,#79096,
#79097,#79098,#79099,#79100,#79101,#79102,#79103,#79104,#79105,#79106,#79107,
#79108,#79109,#79110,#79111,#79112,#79113,#79114,#79115,#79116,#79117,#79118,
#79119,#79120,#79121,#79122,#79123,#79124,#79125,#79126,#79127,#79128,#79129,
#79130,#79131,#79132,#79133,#79134,#79135,#79136,#79137,#79138,#79139,#79140,
#79141,#79142,#79143,#79144,#79145,#79146,#79147,#79148,#79149,#79150,#79151,
#79152,#79153,#79154,#79155,#79156,#79157,#79158,#79159,#79160,#79161,#79162,
#79163,#79164,#79165,#79166,#79167,#79168,#79169,#79170,#79171,#79172,#79173,
#79174,#79175,#79176,#79177,#79178,#79179,#79180,#79181,#79182,#79183,#79184,
#79185,#79186),.UNSPECIFIED.,.F.,.F.,(4,3,3,3,3,3,3,3,3,3,3,3,3,3,3,3,3,
3,3,3,3,3,3,3,3,3,3,3,3,3,3,3,3,3,3,3,3,3,3,3,3,3,3,3,3,3,3,3,3,3,3,3,3,
3,3,3,3,4),(-29.2247647486182,-29.1046697390539,-28.9843458860535,-28.8635945576143,
-28.7591332167706,-28.6455914320349,-28.5322493997827,-28.4190182430922,
-28.3058532788957,-28.1927099227984,-28.0794631238063,-27.966164129126,
-27.8526550488872,-27.7707643077539,-27.6572225230454,-27.5438804908201,
-27.4306493341564,-27.3174843699866,-27.2043410139158,-27.0910942149496,
-26.9777952202949,-26.8642861400811,-26.7823953987372,-26.6688536140261,
-26.5555115817988,-26.4422804251333,-26.329115460962,-26.21597210489,-26.1027253059232,
-25.989426311268,-25.8759172310541,-25.7940264897205,-25.6804847048989,
-25.5671426725605,-25.4539115157839,-25.3407465515014,-25.2276031953185,
-25.1143563962419,-25.0010574014776,-24.8875483211567,-24.8056575807037,
-24.6921157961455,-24.5787737640694,-24.4655426075542,-24.3523776435318,
-24.2392342876072,-24.1259874887841,-24.0126884942709,-23.8991794141944,
-23.817288671687,-23.7052818012017,-23.5934297836473,-23.4816854814853,
-23.3700019323537,-23.258264522408,-23.1465049263617,-23.0345659897191,
-22.9415794424194),.UNSPECIFIED.);
#799=B_SPLINE_CURVE_WITH_KNOTS('',3,(#79188,#79189,#79190,#79191,#79192,
#79193,#79194,#79195,#79196,#79197,#79198,#79199,#79200,#79201,#79202,#79203,
#79204,#79205,#79206,#79207,#79208,#79209,#79210,#79211,#79212,#79213,#79214,
#79215,#79216,#79217,#79218,#79219,#79220,#79221,#79222,#79223,#79224,#79225,
#79226,#79227,#79228,#79229,#79230,#79231,#79232,#79233,#79234,#79235,#79236,
#79237,#79238,#79239,#79240,#79241,#79242,#79243,#79244,#79245,#79246,#79247,
#79248,#79249,#79250,#79251,#79252,#79253,#79254,#79255,#79256,#79257,#79258,
#79259,#79260,#79261,#79262,#79263,#79264,#79265,#79266,#79267,#79268,#79269,
#79270,#79271,#79272,#79273,#79274,#79275,#79276,#79277,#79278,#79279,#79280,
#79281,#79282,#79283,#79284,#79285,#79286,#79287,#79288,#79289,#79290,#79291,
#79292,#79293,#79294,#79295,#79296,#79297,#79298,#79299,#79300,#79301,#79302,
#79303,#79304,#79305,#79306,#79307,#79308,#79309,#79310,#79311,#79312,#79313,
#79314,#79315,#79316,#79317,#79318,#79319,#79320,#79321,#79322,#79323,#79324,
#79325,#79326,#79327,#79328,#79329,#79330,#79331,#79332,#79333,#79334,#79335,
#79336,#79337,#79338,#79339,#79340,#79341,#79342,#79343,#79344,#79345,#79346,
#79347,#79348,#79349,#79350,#79351,#79352,#79353,#79354,#79355,#79356,#79357,
#79358,#79359),.UNSPECIFIED.,.F.,.F.,(4,3,3,3,3,3,3,3,3,3,3,3,3,3,3,3,3,
3,3,3,3,3,3,3,3,3,3,3,3,3,3,3,3,3,3,3,3,3,3,3,3,3,3,3,3,3,3,3,3,3,3,3,3,
3,3,3,3,4),(-22.941579441987,-22.8289197626703,-22.7153779771406,-22.6020359440922,
-22.4888047866046,-22.3756398216119,-22.2624964647207,-22.1492496649442,
-22.0359506694838,-21.9224415884814,-21.8405508536536,-21.7270090705954,
-21.6136670400118,-21.5004358849831,-21.3872709224387,-21.2741275679811,
-21.1608807705963,-21.0475817775076,-20.9340726988158,-20.8521819446369,
-20.7386401595786,-20.6252981270335,-20.5120669700684,-20.398902005616,
-20.2857586492819,-20.1725118500836,-20.0592128552139,-19.9457037748149,
-19.8638130356202,-19.7502712444879,-19.6369292058091,-19.523698042679,
-19.4105330720417,-19.2973897095143,-19.1841429041596,-19.0708439031449,
-18.9573348166956,-18.8754441266034,-18.7619023579417,-18.6485603417033,
-18.5353292009772,-18.4221642526673,-18.3090209123506,-18.1957741288513,
-18.0824751495262,-17.9689660842323,-17.8870752175867,-17.7735334237832,
-17.6601913827284,-17.5469602174043,-17.4337952447568,-17.3206518804049,
-17.2074050735226,-17.0941060711434,-16.9805969836074,-16.89870630857,-16.7510332120614,
-16.6583941353321),.UNSPECIFIED.);
#800=B_SPLINE_CURVE_WITH_KNOTS('',3,(#79361,#79362,#79363,#79364,#79365,
#79366,#79367,#79368,#79369,#79370,#79371,#79372,#79373,#79374,#79375,#79376,
#79377,#79378,#79379,#79380,#79381,#79382,#79383,#79384,#79385,#79386,#79387,
#79388,#79389,#79390,#79391,#79392,#79393,#79394,#79395,#79396,#79397,#79398,
#79399,#79400,#79401,#79402,#79403,#79404,#79405,#79406,#79407,#79408,#79409,
#79410,#79411,#79412,#79413,#79414,#79415,#79416,#79417,#79418,#79419,#79420,
#79421,#79422,#79423,#79424,#79425,#79426,#79427,#79428,#79429,#79430,#79431,
#79432,#79433,#79434,#79435,#79436,#79437,#79438,#79439,#79440,#79441,#79442,
#79443,#79444,#79445,#79446,#79447,#79448,#79449,#79450,#79451,#79452,#79453,
#79454,#79455,#79456,#79457,#79458,#79459,#79460,#79461,#79462,#79463,#79464,
#79465,#79466,#79467,#79468,#79469,#79470,#79471,#79472,#79473,#79474,#79475,
#79476,#79477,#79478,#79479,#79480,#79481,#79482,#79483,#79484,#79485,#79486,
#79487,#79488,#79489,#79490,#79491,#79492,#79493,#79494,#79495,#79496,#79497,
#79498,#79499,#79500,#79501,#79502,#79503,#79504,#79505,#79506,#79507,#79508,
#79509,#79510,#79511,#79512,#79513,#79514,#79515,#79516,#79517,#79518,#79519,
#79520,#79521,#79522,#79523,#79524,#79525,#79526,#79527,#79528,#79529,#79530,
#79531,#79532,#79533,#79534,#79535),.UNSPECIFIED.,.F.,.F.,(4,3,3,3,3,3,
3,3,3,3,3,3,3,3,3,3,3,3,3,3,3,3,3,3,3,3,3,3,3,3,3,3,3,3,3,3,3,3,3,3,3,3,
3,3,3,3,3,3,3,3,3,3,3,3,3,3,3,3,4),(-16.6583941348077,-16.5464691647472,
-16.4346221070533,-16.3228062630273,-16.2108970233939,-16.0989402980712,
-15.9867792411841,-15.9103373995533,-15.796795764382,-15.683453881344,-15.5702228735346,
-15.4570580576209,-15.3439148489425,-15.2306681948749,-15.1173693439421,
-15.0038604037858,-14.9219684905366,-14.8084265728354,-14.6950844099091,
-14.5818531240481,-14.4686880324003,-14.3555445507884,-14.2422976302287,
-14.1289985160019,-14.0154893209314,-13.9335995815199,-13.8200574566352,
-13.7067150805103,-13.5934835779487,-13.4803182665326,-13.3671745625144,
-13.2539274173268,-13.140628076904,-13.0271186559336,-12.9452306725032,
-12.831690236357,-12.7183495513293,-12.6051197399521,-12.4919561167483,
-12.3788140949112,-12.2655686092554,-12.1522709181811,-12.0387631098226,
-11.9568617634864,-11.8433183648221,-11.7299747377807,-11.6167419992646,
-11.5035754689113,-11.3904305650464,-11.277182258624,-11.163881776779,-11.0503712602273,
-10.9684928544697,-10.853324442696,-10.733795538929,-10.6190059812326,-10.5043180362164,
-10.3896917480248,-10.375208827628),.UNSPECIFIED.);
#801=B_SPLINE_CURVE_WITH_KNOTS('',3,(#79536,#79537,#79538,#79539,#79540,
#79541,#79542,#79543,#79544,#79545,#79546,#79547,#79548,#79549,#79550,#79551,
#79552,#79553,#79554,#79555,#79556,#79557,#79558,#79559,#79560,#79561,#79562,
#79563,#79564,#79565,#79566,#79567,#79568,#79569,#79570,#79571,#79572,#79573,
#79574,#79575,#79576,#79577,#79578,#79579,#79580,#79581,#79582,#79583,#79584,
#79585,#79586,#79587,#79588,#79589,#79590,#79591,#79592,#79593,#79594,#79595,
#79596,#79597,#79598,#79599,#79600,#79601,#79602,#79603,#79604,#79605,#79606,
#79607,#79608,#79609,#79610,#79611,#79612,#79613,#79614,#79615,#79616,#79617,
#79618,#79619,#79620,#79621,#79622,#79623,#79624,#79625,#79626,#79627,#79628,
#79629,#79630,#79631,#79632,#79633,#79634,#79635,#79636,#79637,#79638,#79639,
#79640,#79641,#79642,#79643,#79644,#79645,#79646,#79647,#79648,#79649,#79650,
#79651,#79652,#79653,#79654,#79655,#79656,#79657,#79658,#79659,#79660,#79661,
#79662,#79663,#79664,#79665,#79666,#79667,#79668,#79669,#79670,#79671,#79672,
#79673,#79674,#79675,#79676,#79677,#79678,#79679,#79680,#79681,#79682,#79683,
#79684,#79685,#79686,#79687,#79688,#79689,#79690,#79691,#79692,#79693,#79694,
#79695,#79696,#79697,#79698,#79699,#79700,#79701,#79702,#79703,#79704,#79705,
#79706,#79707,#79708,#79709,#79710),.UNSPECIFIED.,.F.,.F.,(4,3,3,3,3,3,
3,3,3,3,3,3,3,3,3,3,3,3,3,3,3,3,3,3,3,3,3,3,3,3,3,3,3,3,3,3,3,3,3,3,3,3,
3,3,3,3,3,3,3,3,3,3,3,3,3,3,3,3,4),(-10.3752088272474,-10.2502773954362,
-10.1248700505524,-9.99887819217141,-9.980123945453,-9.86659394391158,-9.75326369870371,
-9.64004432201014,-9.52689110957821,-9.41375945581954,-9.30052419031302,
-9.18723665200623,-9.07373876275237,-8.99175503643628,-8.87819547394066,
-8.76483581781232,-8.65158714539727,-8.53840480407569,-8.42524424003464,
-8.31198062809963,-8.19866501599926,-8.08513983703984,-8.00338612741957,
-7.88983416985714,-7.77648159669808,-7.66323968282041,-7.55006376726034,
-7.4369092874615,-7.32365119238403,-7.21034078897404,-7.09682026133563,
-7.01501721840285,-6.9015749348315,-6.78833257589082,-6.675201120441,-6.56213570727318,
-6.44909157391288,-6.33594270730992,-6.22274107269596,-6.10932722940379,
-6.02664830938613,-5.91292273846379,-5.79939809503559,-5.68598519987283,
-5.57263969617861,-5.45931732698102,-5.34589527909879,-5.23242288611039,
-5.11874551146585,-5.03827940036942,-4.91999754158034,-4.807427696645,-4.69496234793574,
-4.58255554919585,-4.47016144711192,-4.35766024245203,-4.24509639495919,
-4.13233837516928,-4.0920245300568),.UNSPECIFIED.);
#802=B_SPLINE_CURVE_WITH_KNOTS('',3,(#79713,#79714,#79715,#79716,#79717,
#79718,#79719,#79720,#79721,#79722,#79723,#79724,#79725,#79726,#79727,#79728,
#79729,#79730,#79731),.UNSPECIFIED.,.F.,.F.,(4,3,3,3,3,3,4),(84.1188182559913,
84.2377747874144,84.3566749310004,84.4756604736118,84.5946823768654,84.7139370724539,
84.8230016464385),.UNSPECIFIED.);
#803=B_SPLINE_CURVE_WITH_KNOTS('',3,(#79733,#79734,#79735,#79736,#79737,
#79738,#79739,#79740,#79741,#79742,#79743,#79744,#79745,#79746,#79747,#79748,
#79749,#79750,#79751,#79752,#79753,#79754,#79755,#79756,#79757,#79758,#79759,
#79760,#79761,#79762,#79763,#79764,#79765,#79766,#79767,#79768,#79769,#79770,
#79771,#79772,#79773,#79774,#79775,#79776,#79777,#79778,#79779,#79780,#79781,
#79782,#79783,#79784,#79785,#79786,#79787,#79788,#79789,#79790,#79791,#79792,
#79793,#79794,#79795,#79796,#79797,#79798,#79799,#79800,#79801,#79802,#79803,
#79804,#79805,#79806,#79807,#79808,#79809,#79810,#79811,#79812,#79813,#79814,
#79815,#79816,#79817,#79818,#79819,#79820,#79821,#79822,#79823,#79824,#79825,
#79826,#79827,#79828,#79829,#79830,#79831,#79832,#79833,#79834,#79835,#79836,
#79837,#79838,#79839,#79840,#79841,#79842,#79843,#79844,#79845,#79846,#79847,
#79848,#79849,#79850,#79851,#79852,#79853,#79854,#79855,#79856,#79857,#79858,
#79859,#79860,#79861,#79862,#79863,#79864,#79865,#79866,#79867,#79868),
 .UNSPECIFIED.,.F.,.F.,(4,3,3,3,3,3,3,3,3,3,3,3,3,3,3,3,3,3,3,3,3,3,3,3,
3,3,3,3,3,3,3,3,3,3,3,3,3,3,3,3,3,3,3,3,3,4),(84.8230016469245,84.8516738700234,
84.9752199836505,85.0948937895338,85.214449654091,85.333940114396,85.4534175942909,
85.5730147644292,85.6926850173288,85.8125664477791,85.8400427790401,85.9635888926672,
86.0832552402075,86.2028040127739,86.3222877573057,86.4417589080134,86.5613503570413,
86.6810152388168,86.8008918518797,86.8284116880568,86.9519578016839,87.0715076090144,
87.1909396478129,87.3103067004851,87.4296614364613,87.5491377425846,87.6686881070327,
87.7884522382243,87.8167805970736,87.9403267107007,88.0601748712716,88.1799041213034,
88.2995666497992,88.4192145310629,88.5389783935626,88.658813324919,88.7788549188096,
88.8051495060903,88.9234621670989,89.0416062513237,89.1596371181447,89.2776099218732,
89.3956552369875,89.5137386349911,89.6320206411716,89.6970539997882),
 .UNSPECIFIED.);
#804=B_SPLINE_CURVE_WITH_KNOTS('',3,(#79871,#79872,#79873,#79874,#79875,
#79876,#79877,#79878,#79879,#79880,#79881,#79882,#79883,#79884,#79885,#79886,
#79887,#79888,#79889,#79890,#79891,#79892,#79893,#79894,#79895,#79896,#79897,
#79898,#79899,#79900,#79901,#79902,#79903,#79904,#79905,#79906,#79907,#79908,
#79909,#79910,#79911,#79912,#79913,#79914,#79915,#79916,#79917,#79918,#79919,
#79920,#79921,#79922,#79923,#79924,#79925,#79926,#79927,#79928,#79929,#79930,
#79931,#79932,#79933,#79934,#79935,#79936,#79937,#79938,#79939,#79940,#79941,
#79942,#79943,#79944,#79945,#79946,#79947,#79948,#79949,#79950,#79951,#79952,
#79953,#79954,#79955,#79956,#79957,#79958,#79959,#79960,#79961,#79962,#79963,
#79964,#79965,#79966,#79967,#79968,#79969,#79970,#79971,#79972,#79973,#79974,
#79975,#79976,#79977,#79978,#79979,#79980,#79981,#79982,#79983,#79984,#79985,
#79986,#79987,#79988,#79989,#79990,#79991,#79992,#79993,#79994,#79995,#79996,
#79997,#79998,#79999,#80000),.UNSPECIFIED.,.F.,.F.,(4,2,2,2,2,2,2,2,2,2,
2,2,2,2,2,2,2,2,2,2,2,2,2,2,2,2,2,2,2,2,2,2,2,2,2,2,2,2,2,2,2,2,2,2,2,2,
2,2,2,2,2,2,2,2,2,2,2,2,2,2,2,2,2,2,4),(-1.17147551345429,-1.17041713686015,
-1.16918572837233,-1.16564844753094,-1.15001847616683,-1.13401607500194,
-1.12438570179208,-1.12034552846442,-1.11728048252947,-1.11390493508872,
-1.10821504990784,-1.07769516555731,-1.06001325769979,-1.05697285375094,
-1.05522549263754,-1.05366084578698,-1.05176762634352,-1.04708474465781,
-1.02547499614846,-1.02080515614898,-1.01014525025442,-1.00266167458256,
-0.999233957057352,-0.99657391708826,-0.993604704512768,-0.988546528493683,
-0.958921768333237,-0.947339080328778,-0.942844249513928,-0.939450345775342,
-0.937694002922724,-0.93615756660019,-0.934128090749497,-0.929626737542632,
-0.907385479409659,-0.890014022000379,-0.883313757805212,-0.879927605904625,
-0.877421985882495,-0.874256697322647,-0.868830559115028,-0.845641155737674,
-0.832099312629197,-0.824837146876158,-0.822399814519567,-0.820768075456655,
-0.819036637907101,-0.816078805539853,-0.80128721868014,-0.780639481455452,
-0.769373270357963,-0.765314122595176,-0.762461090514392,-0.759533291233767,
-0.755085518342012,-0.741459818616593,-0.71796640205416,-0.708404813167555,
-0.705765778738023,-0.704107888407975,-0.702660192915801,-0.700237000373645,
-0.693413487796553,-0.673264483182991,-0.659170325149453),.UNSPECIFIED.);
#805=B_SPLINE_CURVE_WITH_KNOTS('',3,(#80338,#80339,#80340,#80341,#80342,
#80343,#80344,#80345,#80346,#80347,#80348,#80349,#80350,#80351,#80352,#80353,
#80354,#80355,#80356,#80357,#80358,#80359,#80360,#80361,#80362,#80363,#80364,
#80365),.UNSPECIFIED.,.F.,.F.,(4,2,2,2,2,2,2,2,2,2,2,2,2,4),(-0.863984233696383,
-0.800933779317784,-0.743377583289618,-0.694285453635929,-0.646603013239699,
-0.594660249030955,-0.546279950529435,-0.49124254158724,-0.424015568120234,
-0.331555083406496,-0.269861277973257,-0.218601022857884,-0.163097142851994,
-0.161658288922872),.UNSPECIFIED.);
#806=B_SPLINE_CURVE_WITH_KNOTS('',3,(#80367,#80368,#80369,#80370,#80371,
#80372,#80373,#80374,#80375,#80376,#80377,#80378,#80379,#80380,#80381,#80382,
#80383,#80384,#80385,#80386,#80387,#80388,#80389,#80390,#80391,#80392,#80393,
#80394,#80395,#80396,#80397,#80398,#80399,#80400,#80401,#80402,#80403,#80404,
#80405,#80406,#80407,#80408,#80409,#80410,#80411,#80412,#80413,#80414,#80415,
#80416,#80417,#80418,#80419,#80420,#80421,#80422,#80423,#80424,#80425,#80426,
#80427,#80428,#80429,#80430,#80431,#80432,#80433,#80434,#80435,#80436,#80437,
#80438,#80439,#80440,#80441,#80442,#80443,#80444,#80445,#80446,#80447,#80448),
 .UNSPECIFIED.,.F.,.F.,(4,3,3,3,3,3,3,3,3,3,3,3,3,3,3,3,3,3,3,3,3,3,3,3,
3,3,3,4),(-0.272951148249661,-0.261636095840719,-0.24446844212677,-0.238751575154802,
-0.234137442773466,-0.216941407287095,-0.205360589642349,-0.200111031359439,
-0.196872097333499,-0.180187285724421,-0.163773299048735,-0.153903690818833,
-0.149145887979538,-0.14599519523252,-0.130113230624166,-0.124294866129125,
-0.108025584337116,-0.100828807434257,-0.0956114852142788,-0.0925945277179398,
-0.0768292134716253,-0.0611421123676899,-0.0532933939326321,-0.0475091511222262,
-0.0447106207682135,-0.0296049810521806,-0.0148024905260903,0.),
 .UNSPECIFIED.);
#807=B_SPLINE_CURVE_WITH_KNOTS('',3,(#80449,#80450,#80451,#80452),
 .UNSPECIFIED.,.F.,.F.,(4,4),(-0.0239932585534707,0.),.UNSPECIFIED.);
#808=B_SPLINE_CURVE_WITH_KNOTS('',3,(#80453,#80454,#80455,#80456,#80457,
#80458,#80459,#80460,#80461,#80462),.UNSPECIFIED.,.F.,.F.,(4,2,2,2,4),(-0.161658288922872,
-0.117667468158224,-0.0654756477726669,-0.0331448228557106,0.),
 .UNSPECIFIED.);
#809=B_SPLINE_CURVE_WITH_KNOTS('',3,(#80466,#80467,#80468,#80469,#80470,
#80471,#80472,#80473,#80474,#80475,#80476,#80477,#80478,#80479,#80480,#80481,
#80482,#80483,#80484,#80485,#80486,#80487,#80488,#80489,#80490,#80491,#80492,
#80493,#80494,#80495,#80496,#80497,#80498,#80499,#80500,#80501,#80502,#80503,
#80504,#80505,#80506,#80507,#80508,#80509,#80510,#80511,#80512,#80513,#80514,
#80515,#80516,#80517,#80518,#80519,#80520,#80521,#80522,#80523,#80524,#80525,
#80526,#80527,#80528,#80529,#80530,#80531,#80532,#80533,#80534,#80535,#80536,
#80537,#80538,#80539,#80540,#80541,#80542,#80543,#80544,#80545,#80546,#80547,
#80548,#80549,#80550),.UNSPECIFIED.,.F.,.F.,(4,3,3,3,3,3,3,3,3,3,3,3,3,
3,3,3,3,3,3,3,3,3,3,3,3,3,3,3,4),(-0.276631791712707,-0.2650733968956,-0.250399139533073,
-0.245003811270574,-0.241631211936854,-0.226360488171095,-0.215462829699367,
-0.211534219543691,-0.208388336956343,-0.192443228773931,-0.176580182967181,
-0.167229942324703,-0.162420312376621,-0.159532045368187,-0.143007019282824,
-0.139179220397272,-0.123204100204565,-0.115503843941779,-0.110594323382493,
-0.107673881166793,-0.0909437463342994,-0.0742136115018059,-0.0647340377437841,
-0.0583028985454159,-0.0537579646197444,-0.0363036304783943,-0.018705463131119,
-0.0011072957838437,0.),.UNSPECIFIED.);
#810=B_SPLINE_CURVE_WITH_KNOTS('',3,(#80880,#80881,#80882,#80883,#80884,
#80885,#80886,#80887,#80888,#80889,#80890,#80891,#80892,#80893),
 .UNSPECIFIED.,.F.,.F.,(4,2,2,2,2,2,4),(-0.204007502680633,-0.147316619177464,
-0.101895409296879,-0.0794299502568435,-0.0610500978728551,-0.0287479058543795,
0.),.UNSPECIFIED.);
#811=SHAPE_REPRESENTATION_RELATIONSHIP('SRR','None',#81130,#821);
#812=SHAPE_REPRESENTATION_RELATIONSHIP('SRR','None',#81131,#822);
#813=SHAPE_REPRESENTATION_RELATIONSHIP('SRR','None',#81132,#823);
#814=SHAPE_REPRESENTATION_RELATIONSHIP('SRR','None',#81133,#824);
#815=SHAPE_REPRESENTATION_RELATIONSHIP('SRR','None',#81134,#825);
#816=SHAPE_REPRESENTATION_RELATIONSHIP('SRR','None',#81135,#826);
#817=SHAPE_REPRESENTATION_RELATIONSHIP('SRR','None',#81136,#827);
#818=SHAPE_REPRESENTATION_RELATIONSHIP('SRR','None',#81137,#828);
#819=SHAPE_REPRESENTATION_RELATIONSHIP('SRR','None',#81138,#829);
#820=SHAPE_REPRESENTATION_RELATIONSHIP('SRR','None',#81139,#830);
#821=ADVANCED_BREP_SHAPE_REPRESENTATION('',(#841),#81030);
#822=ADVANCED_BREP_SHAPE_REPRESENTATION('',(#842),#81031);
#823=ADVANCED_BREP_SHAPE_REPRESENTATION('',(#843),#81032);
#824=ADVANCED_BREP_SHAPE_REPRESENTATION('',(#844),#81033);
#825=ADVANCED_BREP_SHAPE_REPRESENTATION('',(#845),#81034);
#826=ADVANCED_BREP_SHAPE_REPRESENTATION('',(#846),#81035);
#827=ADVANCED_BREP_SHAPE_REPRESENTATION('',(#847),#81036);
#828=ADVANCED_BREP_SHAPE_REPRESENTATION('',(#848),#81037);
#829=ADVANCED_BREP_SHAPE_REPRESENTATION('',(#849),#81038);
#830=ADVANCED_BREP_SHAPE_REPRESENTATION('',(#850),#81039);
#831=STYLED_ITEM('',(#81189),#841);
#832=STYLED_ITEM('',(#81190),#842);
#833=STYLED_ITEM('',(#81191),#843);
#834=STYLED_ITEM('',(#81192),#844);
#835=STYLED_ITEM('',(#81193),#845);
#836=STYLED_ITEM('',(#81194),#846);
#837=STYLED_ITEM('',(#81195),#847);
#838=STYLED_ITEM('',(#81196),#848);
#839=STYLED_ITEM('',(#81197),#849);
#840=STYLED_ITEM('',(#81198),#850);
#841=MANIFOLD_SOLID_BREP('Body1',#15084);
#842=MANIFOLD_SOLID_BREP('Body1',#15085);
#843=MANIFOLD_SOLID_BREP('Body1',#15086);
#844=MANIFOLD_SOLID_BREP('Body1',#15087);
#845=MANIFOLD_SOLID_BREP('Body1',#15088);
#846=MANIFOLD_SOLID_BREP('Body1',#15089);
#847=MANIFOLD_SOLID_BREP('Body1',#15090);
#848=MANIFOLD_SOLID_BREP('Body1',#15091);
#849=MANIFOLD_SOLID_BREP('Body1',#15092);
#850=MANIFOLD_SOLID_BREP('Body1',#15093);
#851=CYLINDRICAL_SURFACE('',#15214,2.74999999999999);
#852=CYLINDRICAL_SURFACE('',#15218,2.75);
#853=CYLINDRICAL_SURFACE('',#15222,2.75);
#854=CYLINDRICAL_SURFACE('',#15226,2.75);
#855=CYLINDRICAL_SURFACE('',#15235,2.74999999999999);
#856=CYLINDRICAL_SURFACE('',#15239,2.75);
#857=CYLINDRICAL_SURFACE('',#15243,2.75);
#858=CYLINDRICAL_SURFACE('',#15247,2.75);
#859=CYLINDRICAL_SURFACE('',#15260,3.05);
#860=CYLINDRICAL_SURFACE('',#15264,3.05);
#861=CYLINDRICAL_SURFACE('',#15268,3.05);
#862=CYLINDRICAL_SURFACE('',#15272,3.05);
#863=CYLINDRICAL_SURFACE('',#15276,3.05);
#864=CYLINDRICAL_SURFACE('',#15280,3.05);
#865=CYLINDRICAL_SURFACE('',#15284,3.05);
#866=CYLINDRICAL_SURFACE('',#15288,3.05);
#867=CYLINDRICAL_SURFACE('',#15336,2.55000000000001);
#868=CYLINDRICAL_SURFACE('',#15346,2.55000000000001);
#869=CYLINDRICAL_SURFACE('',#15356,2.55);
#870=CYLINDRICAL_SURFACE('',#15359,5.);
#871=CYLINDRICAL_SURFACE('',#15361,5.);
#872=CYLINDRICAL_SURFACE('',#15363,5.);
#873=CYLINDRICAL_SURFACE('',#15371,3.);
#874=CYLINDRICAL_SURFACE('',#15373,3.00000000000001);
#875=CYLINDRICAL_SURFACE('',#15375,3.00000000000001);
#876=CYLINDRICAL_SURFACE('',#15385,2.55000000000001);
#877=CYLINDRICAL_SURFACE('',#15395,2.55000000000001);
#878=CYLINDRICAL_SURFACE('',#15405,2.55);
#879=CYLINDRICAL_SURFACE('',#15408,5.);
#880=CYLINDRICAL_SURFACE('',#15410,5.);
#881=CYLINDRICAL_SURFACE('',#15412,5.);
#882=CYLINDRICAL_SURFACE('',#15420,3.);
#883=CYLINDRICAL_SURFACE('',#15422,3.00000000000001);
#884=CYLINDRICAL_SURFACE('',#15424,3.00000000000001);
#885=CYLINDRICAL_SURFACE('',#15433,2.05);
#886=CYLINDRICAL_SURFACE('',#15438,2.05);
#887=CYLINDRICAL_SURFACE('',#15443,2.05);
#888=CYLINDRICAL_SURFACE('',#15448,2.05);
#889=CYLINDRICAL_SURFACE('',#15462,2.05);
#890=CYLINDRICAL_SURFACE('',#15467,2.05);
#891=CYLINDRICAL_SURFACE('',#15472,2.05);
#892=CYLINDRICAL_SURFACE('',#15477,2.05);
#893=CYLINDRICAL_SURFACE('',#15501,3.05);
#894=CYLINDRICAL_SURFACE('',#15505,3.05);
#895=CYLINDRICAL_SURFACE('',#15509,3.05);
#896=CYLINDRICAL_SURFACE('',#15513,3.05);
#897=CYLINDRICAL_SURFACE('',#15517,3.05);
#898=CYLINDRICAL_SURFACE('',#15521,3.05);
#899=CYLINDRICAL_SURFACE('',#15531,5.50000000000001);
#900=CYLINDRICAL_SURFACE('',#15535,5.50000000000001);
#901=CYLINDRICAL_SURFACE('',#15539,5.5);
#902=CYLINDRICAL_SURFACE('',#15543,5.50000000000001);
#903=CYLINDRICAL_SURFACE('',#15547,5.5);
#904=CYLINDRICAL_SURFACE('',#15551,5.50000000000001);
#905=CYLINDRICAL_SURFACE('',#15555,5.50000000000001);
#906=CYLINDRICAL_SURFACE('',#15559,5.50000000000001);
#907=CYLINDRICAL_SURFACE('',#15577,3.50000000000001);
#908=CYLINDRICAL_SURFACE('',#15579,3.5);
#909=CYLINDRICAL_SURFACE('',#15581,3.5);
#910=CYLINDRICAL_SURFACE('',#15583,3.5);
#911=CYLINDRICAL_SURFACE('',#15585,3.5);
#912=CYLINDRICAL_SURFACE('',#15587,3.5);
#913=CYLINDRICAL_SURFACE('',#15589,3.5);
#914=CYLINDRICAL_SURFACE('',#15591,3.50000000000001);
#915=CYLINDRICAL_SURFACE('',#15619,1.55);
#916=CYLINDRICAL_SURFACE('',#15627,1.55);
#917=CYLINDRICAL_SURFACE('',#15637,2.55000000000001);
#918=CYLINDRICAL_SURFACE('',#15649,2.55000000000001);
#919=CYLINDRICAL_SURFACE('',#15661,2.55);
#920=CYLINDRICAL_SURFACE('',#15711,1.55);
#921=CYLINDRICAL_SURFACE('',#15720,1.55);
#922=CYLINDRICAL_SURFACE('',#15731,2.54999999999999);
#923=CYLINDRICAL_SURFACE('',#15743,2.55);
#924=CYLINDRICAL_SURFACE('',#15755,2.55000000000001);
#925=CYLINDRICAL_SURFACE('',#15767,2.55000000000001);
#926=CYLINDRICAL_SURFACE('',#15818,0.400000000000027);
#927=CYLINDRICAL_SURFACE('',#15822,0.399999999999956);
#928=CYLINDRICAL_SURFACE('',#15826,0.399999999999945);
#929=CYLINDRICAL_SURFACE('',#15830,0.400000000000027);
#930=CYLINDRICAL_SURFACE('',#15834,0.399999999999996);
#931=CYLINDRICAL_SURFACE('',#15838,0.4);
#932=CYLINDRICAL_SURFACE('',#15842,0.399999999999996);
#933=CYLINDRICAL_SURFACE('',#15846,0.399999999999996);
#934=CYLINDRICAL_SURFACE('',#15850,0.600000000000005);
#935=CYLINDRICAL_SURFACE('',#15854,0.600000000000005);
#936=CYLINDRICAL_SURFACE('',#15858,0.600000000000005);
#937=CYLINDRICAL_SURFACE('',#15862,0.600000000000005);
#938=CYLINDRICAL_SURFACE('',#15866,0.600000000000005);
#939=CYLINDRICAL_SURFACE('',#15870,0.600000000000005);
#940=CYLINDRICAL_SURFACE('',#15874,0.600000000000005);
#941=CYLINDRICAL_SURFACE('',#15878,0.600000000000005);
#942=CYLINDRICAL_SURFACE('',#15882,0.599999999999987);
#943=CYLINDRICAL_SURFACE('',#15886,0.599999999999987);
#944=CYLINDRICAL_SURFACE('',#15890,0.599999999999987);
#945=CYLINDRICAL_SURFACE('',#15894,0.599999999999987);
#946=CYLINDRICAL_SURFACE('',#15898,0.599999999999987);
#947=CYLINDRICAL_SURFACE('',#15902,0.599999999999987);
#948=CYLINDRICAL_SURFACE('',#15906,0.599999999999987);
#949=CYLINDRICAL_SURFACE('',#15910,0.599999999999987);
#950=CYLINDRICAL_SURFACE('',#15914,0.599999999999987);
#951=CYLINDRICAL_SURFACE('',#15918,0.599999999999987);
#952=CYLINDRICAL_SURFACE('',#15922,0.599999999999987);
#953=CYLINDRICAL_SURFACE('',#15926,0.599999999999987);
#954=CYLINDRICAL_SURFACE('',#15930,0.600000000000001);
#955=CYLINDRICAL_SURFACE('',#15934,0.600000000000005);
#956=CYLINDRICAL_SURFACE('',#15938,0.599999999999998);
#957=CYLINDRICAL_SURFACE('',#15942,0.600000000000005);
#958=CYLINDRICAL_SURFACE('',#15946,0.600000000000001);
#959=CYLINDRICAL_SURFACE('',#15950,0.600000000000005);
#960=CYLINDRICAL_SURFACE('',#15954,0.600000000000003);
#961=CYLINDRICAL_SURFACE('',#15958,0.600000000000005);
#962=CYLINDRICAL_SURFACE('',#15962,0.599999999999996);
#963=CYLINDRICAL_SURFACE('',#15966,0.600000000000005);
#964=CYLINDRICAL_SURFACE('',#15970,0.599999999999998);
#965=CYLINDRICAL_SURFACE('',#15974,0.600000000000005);
#966=CYLINDRICAL_SURFACE('',#15978,0.599999999999987);
#967=CYLINDRICAL_SURFACE('',#15982,0.599999999999987);
#968=CYLINDRICAL_SURFACE('',#15986,0.599999999999987);
#969=CYLINDRICAL_SURFACE('',#15990,0.599999999999987);
#970=CYLINDRICAL_SURFACE('',#15994,0.600000000000001);
#971=CYLINDRICAL_SURFACE('',#15998,0.600000000000005);
#972=CYLINDRICAL_SURFACE('',#16002,0.600000000000003);
#973=CYLINDRICAL_SURFACE('',#16006,0.600000000000005);
#974=CYLINDRICAL_SURFACE('',#16010,0.599999999999987);
#975=CYLINDRICAL_SURFACE('',#16014,0.600000000000005);
#976=CYLINDRICAL_SURFACE('',#16018,0.600000000000005);
#977=CYLINDRICAL_SURFACE('',#16022,0.599999999999987);
#978=CYLINDRICAL_SURFACE('',#16026,0.600000000000005);
#979=CYLINDRICAL_SURFACE('',#16030,0.600000000000005);
#980=CYLINDRICAL_SURFACE('',#16034,0.600000000000005);
#981=CYLINDRICAL_SURFACE('',#16038,0.600000000000005);
#982=CYLINDRICAL_SURFACE('',#16042,0.600000000000027);
#983=CYLINDRICAL_SURFACE('',#16046,0.600000000000023);
#984=CYLINDRICAL_SURFACE('',#16050,0.600000000000025);
#985=CYLINDRICAL_SURFACE('',#16054,0.600000000000023);
#986=CYLINDRICAL_SURFACE('',#16058,1.);
#987=CYLINDRICAL_SURFACE('',#16062,1.00000000000001);
#988=CYLINDRICAL_SURFACE('',#16066,1.00000000000001);
#989=CYLINDRICAL_SURFACE('',#16070,1.);
#990=CYLINDRICAL_SURFACE('',#16080,3.);
#991=CYLINDRICAL_SURFACE('',#16086,1.99475);
#992=CYLINDRICAL_SURFACE('',#16088,1.99475);
#993=CYLINDRICAL_SURFACE('',#16089,1.99475);
#994=CYLINDRICAL_SURFACE('',#16090,1.99475);
#995=CYLINDRICAL_SURFACE('',#16091,1.99475);
#996=CYLINDRICAL_SURFACE('',#16092,1.99475);
#997=CYLINDRICAL_SURFACE('',#16093,1.99475);
#998=CYLINDRICAL_SURFACE('',#16094,1.99475);
#999=CYLINDRICAL_SURFACE('',#16095,1.99475);
#1000=CYLINDRICAL_SURFACE('',#16096,1.99475);
#1001=CYLINDRICAL_SURFACE('',#16097,1.99475);
#1002=CYLINDRICAL_SURFACE('',#16098,1.99475);
#1003=CYLINDRICAL_SURFACE('',#16099,1.99475);
#1004=CYLINDRICAL_SURFACE('',#16100,1.99475);
#1005=CYLINDRICAL_SURFACE('',#16101,1.99475);
#1006=CYLINDRICAL_SURFACE('',#16102,1.99475);
#1007=CYLINDRICAL_SURFACE('',#16103,1.99475);
#1008=CYLINDRICAL_SURFACE('',#16104,1.99475);
#1009=CYLINDRICAL_SURFACE('',#16105,1.99475);
#1010=CYLINDRICAL_SURFACE('',#16106,1.99475);
#1011=CYLINDRICAL_SURFACE('',#16107,1.99475);
#1012=CYLINDRICAL_SURFACE('',#16108,1.99475);
#1013=CYLINDRICAL_SURFACE('',#16109,1.99475);
#1014=CYLINDRICAL_SURFACE('',#16110,1.99475);
#1015=CYLINDRICAL_SURFACE('',#16111,2.4505);
#1016=CYLINDRICAL_SURFACE('',#16114,1.99475);
#1017=CYLINDRICAL_SURFACE('',#16134,4.25);
#1018=CYLINDRICAL_SURFACE('',#16326,2.2594010767585);
#1019=CYLINDRICAL_SURFACE('',#16328,2.2594010767585);
#1020=CYLINDRICAL_SURFACE('',#16330,2.2594010767585);
#1021=CYLINDRICAL_SURFACE('',#16332,2.2594010767585);
#1022=CYLINDRICAL_SURFACE('',#16334,2.2594010767585);
#1023=CYLINDRICAL_SURFACE('',#16336,2.2594010767585);
#1024=CYLINDRICAL_SURFACE('',#16364,1.99475);
#1025=CYLINDRICAL_SURFACE('',#16366,1.99475);
#1026=CYLINDRICAL_SURFACE('',#16367,1.99475);
#1027=CYLINDRICAL_SURFACE('',#16368,1.99475);
#1028=CYLINDRICAL_SURFACE('',#16369,1.99475);
#1029=CYLINDRICAL_SURFACE('',#16370,1.99475);
#1030=CYLINDRICAL_SURFACE('',#16371,1.99475);
#1031=CYLINDRICAL_SURFACE('',#16372,1.99475);
#1032=CYLINDRICAL_SURFACE('',#16373,1.99475);
#1033=CYLINDRICAL_SURFACE('',#16374,1.99475);
#1034=CYLINDRICAL_SURFACE('',#16375,1.99475);
#1035=CYLINDRICAL_SURFACE('',#16376,1.99475);
#1036=CYLINDRICAL_SURFACE('',#16377,1.99475);
#1037=CYLINDRICAL_SURFACE('',#16378,1.99475);
#1038=CYLINDRICAL_SURFACE('',#16379,1.99475);
#1039=CYLINDRICAL_SURFACE('',#16380,1.99475);
#1040=CYLINDRICAL_SURFACE('',#16381,1.99475);
#1041=CYLINDRICAL_SURFACE('',#16382,1.99475);
#1042=CYLINDRICAL_SURFACE('',#16383,1.99475);
#1043=CYLINDRICAL_SURFACE('',#16384,1.99475);
#1044=CYLINDRICAL_SURFACE('',#16385,1.99475);
#1045=CYLINDRICAL_SURFACE('',#16386,1.99475);
#1046=CYLINDRICAL_SURFACE('',#16387,1.99475);
#1047=CYLINDRICAL_SURFACE('',#16388,2.4505);
#1048=CYLINDRICAL_SURFACE('',#16391,1.99475);
#1049=CYLINDRICAL_SURFACE('',#16407,1.39337567297407);
#1050=CYLINDRICAL_SURFACE('',#16409,1.39337567297407);
#1051=CYLINDRICAL_SURFACE('',#16411,1.39337567297407);
#1052=CYLINDRICAL_SURFACE('',#16413,1.39337567297407);
#1053=CYLINDRICAL_SURFACE('',#16415,1.39337567297407);
#1054=CYLINDRICAL_SURFACE('',#16417,1.39337567297407);
#1055=CYLINDRICAL_SURFACE('',#16451,1.99475);
#1056=CYLINDRICAL_SURFACE('',#16453,1.99475);
#1057=CYLINDRICAL_SURFACE('',#16455,1.99475);
#1058=CYLINDRICAL_SURFACE('',#16456,1.99475);
#1059=CYLINDRICAL_SURFACE('',#16457,1.99475);
#1060=CYLINDRICAL_SURFACE('',#16458,1.99475);
#1061=CYLINDRICAL_SURFACE('',#16459,1.99475);
#1062=CYLINDRICAL_SURFACE('',#16460,1.99475);
#1063=CYLINDRICAL_SURFACE('',#16461,1.99475);
#1064=CYLINDRICAL_SURFACE('',#16462,1.99475);
#1065=CYLINDRICAL_SURFACE('',#16468,2.4505);
#1066=CYLINDRICAL_SURFACE('',#16471,1.99475);
#1067=CYLINDRICAL_SURFACE('',#16508,4.75);
#1068=CYLINDRICAL_SURFACE('',#16513,1.17775);
#1069=CYLINDRICAL_SURFACE('',#16515,1.17775);
#1070=CYLINDRICAL_SURFACE('',#16517,1.17775);
#1071=CYLINDRICAL_SURFACE('',#16518,1.17775);
#1072=CYLINDRICAL_SURFACE('',#16519,1.17775);
#1073=CYLINDRICAL_SURFACE('',#16520,1.17775);
#1074=CYLINDRICAL_SURFACE('',#16521,1.17775);
#1075=CYLINDRICAL_SURFACE('',#16522,1.17775);
#1076=CYLINDRICAL_SURFACE('',#16523,1.17775);
#1077=CYLINDRICAL_SURFACE('',#16524,1.17775);
#1078=CYLINDRICAL_SURFACE('',#16525,1.17775);
#1079=CYLINDRICAL_SURFACE('',#16526,1.17775);
#1080=CYLINDRICAL_SURFACE('',#16527,1.4635);
#1081=CYLINDRICAL_SURFACE('',#16530,1.17775);
#1082=CYLINDRICAL_SURFACE('',#16546,2.75);
#1083=FACE_BOUND('',#2351,.T.);
#1084=FACE_BOUND('',#2352,.T.);
#1085=FACE_BOUND('',#2353,.T.);
#1086=FACE_BOUND('',#2354,.T.);
#1087=FACE_BOUND('',#2364,.T.);
#1088=FACE_BOUND('',#2365,.T.);
#1089=FACE_BOUND('',#2366,.T.);
#1090=FACE_BOUND('',#2367,.T.);
#1091=FACE_BOUND('',#2377,.T.);
#1092=FACE_BOUND('',#2378,.T.);
#1093=FACE_BOUND('',#2379,.T.);
#1094=FACE_BOUND('',#2380,.T.);
#1095=FACE_BOUND('',#2381,.T.);
#1096=FACE_BOUND('',#2382,.T.);
#1097=FACE_BOUND('',#2383,.T.);
#1098=FACE_BOUND('',#2384,.T.);
#1099=FACE_BOUND('',#2427,.T.);
#1100=FACE_BOUND('',#2428,.T.);
#1101=FACE_BOUND('',#2429,.T.);
#1102=FACE_BOUND('',#2430,.T.);
#1103=FACE_BOUND('',#2439,.T.);
#1104=FACE_BOUND('',#2440,.T.);
#1105=FACE_BOUND('',#2441,.T.);
#1106=FACE_BOUND('',#2442,.T.);
#1107=FACE_BOUND('',#2455,.T.);
#1108=FACE_BOUND('',#2456,.T.);
#1109=FACE_BOUND('',#2457,.T.);
#1110=FACE_BOUND('',#2462,.T.);
#1111=FACE_BOUND('',#2464,.T.);
#1112=FACE_BOUND('',#2466,.T.);
#1113=FACE_BOUND('',#2480,.T.);
#1114=FACE_BOUND('',#2481,.T.);
#1115=FACE_BOUND('',#2482,.T.);
#1116=FACE_BOUND('',#2487,.T.);
#1117=FACE_BOUND('',#2489,.T.);
#1118=FACE_BOUND('',#2491,.T.);
#1119=FACE_BOUND('',#2497,.T.);
#1120=FACE_BOUND('',#2498,.T.);
#1121=FACE_BOUND('',#2499,.T.);
#1122=FACE_BOUND('',#2500,.T.);
#1123=FACE_BOUND('',#2514,.T.);
#1124=FACE_BOUND('',#2515,.T.);
#1125=FACE_BOUND('',#2516,.T.);
#1126=FACE_BOUND('',#2517,.T.);
#1127=FACE_BOUND('',#2531,.T.);
#1128=FACE_BOUND('',#2532,.T.);
#1129=FACE_BOUND('',#2533,.T.);
#1130=FACE_BOUND('',#2534,.T.);
#1131=FACE_BOUND('',#2535,.T.);
#1132=FACE_BOUND('',#2536,.T.);
#1133=FACE_BOUND('',#2537,.T.);
#1134=FACE_BOUND('',#2538,.T.);
#1135=FACE_BOUND('',#2539,.T.);
#1136=FACE_BOUND('',#2540,.T.);
#1137=FACE_BOUND('',#2541,.T.);
#1138=FACE_BOUND('',#2542,.T.);
#1139=FACE_BOUND('',#2543,.T.);
#1140=FACE_BOUND('',#2544,.T.);
#1141=FACE_BOUND('',#2579,.T.);
#1142=FACE_BOUND('',#2581,.T.);
#1143=FACE_BOUND('',#2583,.T.);
#1144=FACE_BOUND('',#2585,.T.);
#1145=FACE_BOUND('',#2587,.T.);
#1146=FACE_BOUND('',#2589,.T.);
#1147=FACE_BOUND('',#2591,.T.);
#1148=FACE_BOUND('',#2593,.T.);
#1149=FACE_BOUND('',#2613,.T.);
#1150=FACE_BOUND('',#2614,.T.);
#1151=FACE_BOUND('',#2615,.T.);
#1152=FACE_BOUND('',#2616,.T.);
#1153=FACE_BOUND('',#2619,.T.);
#1154=FACE_BOUND('',#2620,.T.);
#1155=FACE_BOUND('',#2621,.T.);
#1156=FACE_BOUND('',#2622,.T.);
#1157=FACE_BOUND('',#2623,.T.);
#1158=FACE_BOUND('',#2624,.T.);
#1159=FACE_BOUND('',#2627,.T.);
#1160=FACE_BOUND('',#2628,.T.);
#1161=FACE_BOUND('',#2629,.T.);
#1162=FACE_BOUND('',#2630,.T.);
#1163=FACE_BOUND('',#2632,.T.);
#1164=FACE_BOUND('',#2633,.T.);
#1165=FACE_BOUND('',#2634,.T.);
#1166=FACE_BOUND('',#2635,.T.);
#1167=FACE_BOUND('',#2636,.T.);
#1168=FACE_BOUND('',#2637,.T.);
#1169=FACE_BOUND('',#2653,.T.);
#1170=FACE_BOUND('',#2654,.T.);
#1171=FACE_BOUND('',#2655,.T.);
#1172=FACE_BOUND('',#2705,.T.);
#1173=FACE_BOUND('',#2706,.T.);
#1174=FACE_BOUND('',#2707,.T.);
#1175=FACE_BOUND('',#2708,.T.);
#1176=FACE_BOUND('',#2884,.T.);
#1177=FACE_BOUND('',#2885,.T.);
#1178=FACE_BOUND('',#2886,.T.);
#1179=FACE_BOUND('',#2887,.T.);
#1180=FACE_BOUND('',#2888,.T.);
#1181=FACE_BOUND('',#2889,.T.);
#1182=FACE_BOUND('',#2890,.T.);
#1183=FACE_BOUND('',#2891,.T.);
#1184=FACE_BOUND('',#2892,.T.);
#1185=FACE_BOUND('',#2893,.T.);
#1186=FACE_BOUND('',#2894,.T.);
#1187=FACE_BOUND('',#2895,.T.);
#1188=FACE_BOUND('',#2896,.T.);
#1189=FACE_BOUND('',#2897,.T.);
#1190=FACE_BOUND('',#2898,.T.);
#1191=FACE_BOUND('',#2900,.T.);
#1192=FACE_BOUND('',#2901,.T.);
#1193=FACE_BOUND('',#2902,.T.);
#1194=FACE_BOUND('',#2903,.T.);
#1195=FACE_BOUND('',#2904,.T.);
#1196=FACE_BOUND('',#2905,.T.);
#1197=FACE_BOUND('',#2906,.T.);
#1198=FACE_BOUND('',#2907,.T.);
#1199=FACE_BOUND('',#2908,.T.);
#1200=FACE_BOUND('',#2909,.T.);
#1201=FACE_BOUND('',#2910,.T.);
#1202=FACE_BOUND('',#2911,.T.);
#1203=FACE_BOUND('',#2912,.T.);
#1204=FACE_BOUND('',#2913,.T.);
#1205=FACE_BOUND('',#2914,.T.);
#1206=FACE_BOUND('',#2952,.T.);
#1207=FACE_BOUND('',#3067,.T.);
#1208=FACE_BOUND('',#3150,.T.);
#1209=FACE_BOUND('',#3174,.T.);
#1210=FACE_BOUND('',#3209,.T.);
#1211=PLANE('',#15210);
#1212=PLANE('',#15231);
#1213=PLANE('',#15252);
#1214=PLANE('',#15298);
#1215=PLANE('',#15299);
#1216=PLANE('',#15300);
#1217=PLANE('',#15301);
#1218=PLANE('',#15302);
#1219=PLANE('',#15303);
#1220=PLANE('',#15304);
#1221=PLANE('',#15305);
#1222=PLANE('',#15306);
#1223=PLANE('',#15307);
#1224=PLANE('',#15308);
#1225=PLANE('',#15309);
#1226=PLANE('',#15310);
#1227=PLANE('',#15311);
#1228=PLANE('',#15312);
#1229=PLANE('',#15313);
#1230=PLANE('',#15314);
#1231=PLANE('',#15315);
#1232=PLANE('',#15316);
#1233=PLANE('',#15317);
#1234=PLANE('',#15318);
#1235=PLANE('',#15319);
#1236=PLANE('',#15320);
#1237=PLANE('',#15321);
#1238=PLANE('',#15322);
#1239=PLANE('',#15323);
#1240=PLANE('',#15324);
#1241=PLANE('',#15325);
#1242=PLANE('',#15326);
#1243=PLANE('',#15358);
#1244=PLANE('',#15365);
#1245=PLANE('',#15367);
#1246=PLANE('',#15369);
#1247=PLANE('',#15407);
#1248=PLANE('',#15414);
#1249=PLANE('',#15416);
#1250=PLANE('',#15418);
#1251=PLANE('',#15429);
#1252=PLANE('',#15458);
#1253=PLANE('',#15487);
#1254=PLANE('',#15561);
#1255=PLANE('',#15563);
#1256=PLANE('',#15565);
#1257=PLANE('',#15567);
#1258=PLANE('',#15569);
#1259=PLANE('',#15571);
#1260=PLANE('',#15573);
#1261=PLANE('',#15575);
#1262=PLANE('',#15593);
#1263=PLANE('',#15594);
#1264=PLANE('',#15595);
#1265=PLANE('',#15596);
#1266=PLANE('',#15597);
#1267=PLANE('',#15598);
#1268=PLANE('',#15599);
#1269=PLANE('',#15600);
#1270=PLANE('',#15601);
#1271=PLANE('',#15602);
#1272=PLANE('',#15603);
#1273=PLANE('',#15604);
#1274=PLANE('',#15605);
#1275=PLANE('',#15606);
#1276=PLANE('',#15607);
#1277=PLANE('',#15608);
#1278=PLANE('',#15609);
#1279=PLANE('',#15610);
#1280=PLANE('',#15611);
#1281=PLANE('',#15612);
#1282=PLANE('',#15613);
#1283=PLANE('',#15618);
#1284=PLANE('',#15626);
#1285=PLANE('',#15634);
#1286=PLANE('',#15671);
#1287=PLANE('',#15672);
#1288=PLANE('',#15673);
#1289=PLANE('',#15674);
#1290=PLANE('',#15675);
#1291=PLANE('',#15676);
#1292=PLANE('',#15677);
#1293=PLANE('',#15678);
#1294=PLANE('',#15679);
#1295=PLANE('',#15680);
#1296=PLANE('',#15681);
#1297=PLANE('',#15682);
#1298=PLANE('',#15683);
#1299=PLANE('',#15684);
#1300=PLANE('',#15685);
#1301=PLANE('',#15686);
#1302=PLANE('',#15687);
#1303=PLANE('',#15688);
#1304=PLANE('',#15689);
#1305=PLANE('',#15690);
#1306=PLANE('',#15691);
#1307=PLANE('',#15692);
#1308=PLANE('',#15693);
#1309=PLANE('',#15694);
#1310=PLANE('',#15695);
#1311=PLANE('',#15696);
#1312=PLANE('',#15697);
#1313=PLANE('',#15698);
#1314=PLANE('',#15699);
#1315=PLANE('',#15700);
#1316=PLANE('',#15701);
#1317=PLANE('',#15702);
#1318=PLANE('',#15703);
#1319=PLANE('',#15704);
#1320=PLANE('',#15710);
#1321=PLANE('',#15719);
#1322=PLANE('',#15727);
#1323=PLANE('',#15777);
#1324=PLANE('',#15778);
#1325=PLANE('',#15779);
#1326=PLANE('',#15780);
#1327=PLANE('',#15781);
#1328=PLANE('',#15782);
#1329=PLANE('',#15783);
#1330=PLANE('',#15784);
#1331=PLANE('',#15785);
#1332=PLANE('',#15786);
#1333=PLANE('',#15787);
#1334=PLANE('',#15788);
#1335=PLANE('',#15789);
#1336=PLANE('',#15790);
#1337=PLANE('',#15791);
#1338=PLANE('',#15792);
#1339=PLANE('',#15793);
#1340=PLANE('',#15794);
#1341=PLANE('',#15795);
#1342=PLANE('',#15796);
#1343=PLANE('',#15797);
#1344=PLANE('',#15798);
#1345=PLANE('',#15799);
#1346=PLANE('',#15800);
#1347=PLANE('',#15801);
#1348=PLANE('',#15802);
#1349=PLANE('',#15803);
#1350=PLANE('',#15804);
#1351=PLANE('',#15805);
#1352=PLANE('',#15806);
#1353=PLANE('',#15807);
#1354=PLANE('',#15808);
#1355=PLANE('',#15809);
#1356=PLANE('',#15810);
#1357=PLANE('',#15811);
#1358=PLANE('',#15812);
#1359=PLANE('',#15813);
#1360=PLANE('',#15814);
#1361=PLANE('',#15815);
#1362=PLANE('',#15817);
#1363=PLANE('',#15821);
#1364=PLANE('',#15825);
#1365=PLANE('',#15829);
#1366=PLANE('',#15833);
#1367=PLANE('',#15837);
#1368=PLANE('',#15841);
#1369=PLANE('',#15845);
#1370=PLANE('',#15849);
#1371=PLANE('',#15853);
#1372=PLANE('',#15857);
#1373=PLANE('',#15861);
#1374=PLANE('',#15865);
#1375=PLANE('',#15869);
#1376=PLANE('',#15873);
#1377=PLANE('',#15877);
#1378=PLANE('',#15881);
#1379=PLANE('',#15885);
#1380=PLANE('',#15889);
#1381=PLANE('',#15893);
#1382=PLANE('',#15897);
#1383=PLANE('',#15901);
#1384=PLANE('',#15905);
#1385=PLANE('',#15909);
#1386=PLANE('',#15913);
#1387=PLANE('',#15917);
#1388=PLANE('',#15921);
#1389=PLANE('',#15925);
#1390=PLANE('',#15929);
#1391=PLANE('',#15933);
#1392=PLANE('',#15937);
#1393=PLANE('',#15941);
#1394=PLANE('',#15945);
#1395=PLANE('',#15949);
#1396=PLANE('',#15953);
#1397=PLANE('',#15957);
#1398=PLANE('',#15961);
#1399=PLANE('',#15965);
#1400=PLANE('',#15969);
#1401=PLANE('',#15973);
#1402=PLANE('',#15977);
#1403=PLANE('',#15981);
#1404=PLANE('',#15985);
#1405=PLANE('',#15989);
#1406=PLANE('',#15993);
#1407=PLANE('',#15997);
#1408=PLANE('',#16001);
#1409=PLANE('',#16005);
#1410=PLANE('',#16009);
#1411=PLANE('',#16013);
#1412=PLANE('',#16017);
#1413=PLANE('',#16021);
#1414=PLANE('',#16025);
#1415=PLANE('',#16029);
#1416=PLANE('',#16033);
#1417=PLANE('',#16037);
#1418=PLANE('',#16041);
#1419=PLANE('',#16045);
#1420=PLANE('',#16049);
#1421=PLANE('',#16053);
#1422=PLANE('',#16057);
#1423=PLANE('',#16061);
#1424=PLANE('',#16065);
#1425=PLANE('',#16069);
#1426=PLANE('',#16073);
#1427=PLANE('',#16074);
#1428=PLANE('',#16076);
#1429=PLANE('',#16084);
#1430=PLANE('',#16116);
#1431=PLANE('',#16119);
#1432=PLANE('',#16125);
#1433=PLANE('',#16129);
#1434=PLANE('',#16130);
#1435=PLANE('',#16132);
#1436=PLANE('',#16133);
#1437=PLANE('',#16208);
#1438=PLANE('',#16209);
#1439=PLANE('',#16210);
#1440=PLANE('',#16213);
#1441=PLANE('',#16214);
#1442=PLANE('',#16215);
#1443=PLANE('',#16216);
#1444=PLANE('',#16217);
#1445=PLANE('',#16218);
#1446=PLANE('',#16219);
#1447=PLANE('',#16220);
#1448=PLANE('',#16221);
#1449=PLANE('',#16222);
#1450=PLANE('',#16223);
#1451=PLANE('',#16224);
#1452=PLANE('',#16225);
#1453=PLANE('',#16226);
#1454=PLANE('',#16227);
#1455=PLANE('',#16228);
#1456=PLANE('',#16229);
#1457=PLANE('',#16230);
#1458=PLANE('',#16231);
#1459=PLANE('',#16232);
#1460=PLANE('',#16233);
#1461=PLANE('',#16234);
#1462=PLANE('',#16235);
#1463=PLANE('',#16236);
#1464=PLANE('',#16237);
#1465=PLANE('',#16238);
#1466=PLANE('',#16239);
#1467=PLANE('',#16240);
#1468=PLANE('',#16241);
#1469=PLANE('',#16242);
#1470=PLANE('',#16243);
#1471=PLANE('',#16244);
#1472=PLANE('',#16245);
#1473=PLANE('',#16246);
#1474=PLANE('',#16247);
#1475=PLANE('',#16248);
#1476=PLANE('',#16249);
#1477=PLANE('',#16250);
#1478=PLANE('',#16251);
#1479=PLANE('',#16252);
#1480=PLANE('',#16253);
#1481=PLANE('',#16254);
#1482=PLANE('',#16255);
#1483=PLANE('',#16256);
#1484=PLANE('',#16257);
#1485=PLANE('',#16258);
#1486=PLANE('',#16259);
#1487=PLANE('',#16260);
#1488=PLANE('',#16261);
#1489=PLANE('',#16262);
#1490=PLANE('',#16263);
#1491=PLANE('',#16264);
#1492=PLANE('',#16265);
#1493=PLANE('',#16266);
#1494=PLANE('',#16267);
#1495=PLANE('',#16268);
#1496=PLANE('',#16269);
#1497=PLANE('',#16270);
#1498=PLANE('',#16271);
#1499=PLANE('',#16272);
#1500=PLANE('',#16273);
#1501=PLANE('',#16274);
#1502=PLANE('',#16275);
#1503=PLANE('',#16276);
#1504=PLANE('',#16277);
#1505=PLANE('',#16278);
#1506=PLANE('',#16279);
#1507=PLANE('',#16280);
#1508=PLANE('',#16281);
#1509=PLANE('',#16282);
#1510=PLANE('',#16283);
#1511=PLANE('',#16284);
#1512=PLANE('',#16285);
#1513=PLANE('',#16286);
#1514=PLANE('',#16287);
#1515=PLANE('',#16288);
#1516=PLANE('',#16289);
#1517=PLANE('',#16290);
#1518=PLANE('',#16291);
#1519=PLANE('',#16292);
#1520=PLANE('',#16293);
#1521=PLANE('',#16294);
#1522=PLANE('',#16295);
#1523=PLANE('',#16296);
#1524=PLANE('',#16297);
#1525=PLANE('',#16298);
#1526=PLANE('',#16299);
#1527=PLANE('',#16300);
#1528=PLANE('',#16301);
#1529=PLANE('',#16302);
#1530=PLANE('',#16303);
#1531=PLANE('',#16304);
#1532=PLANE('',#16305);
#1533=PLANE('',#16306);
#1534=PLANE('',#16307);
#1535=PLANE('',#16308);
#1536=PLANE('',#16309);
#1537=PLANE('',#16310);
#1538=PLANE('',#16311);
#1539=PLANE('',#16312);
#1540=PLANE('',#16313);
#1541=PLANE('',#16314);
#1542=PLANE('',#16317);
#1543=PLANE('',#16338);
#1544=PLANE('',#16339);
#1545=PLANE('',#16340);
#1546=PLANE('',#16341);
#1547=PLANE('',#16342);
#1548=PLANE('',#16343);
#1549=PLANE('',#16344);
#1550=PLANE('',#16345);
#1551=PLANE('',#16346);
#1552=PLANE('',#16347);
#1553=PLANE('',#16349);
#1554=PLANE('',#16351);
#1555=PLANE('',#16353);
#1556=PLANE('',#16355);
#1557=PLANE('',#16357);
#1558=PLANE('',#16360);
#1559=PLANE('',#16361);
#1560=PLANE('',#16362);
#1561=PLANE('',#16393);
#1562=PLANE('',#16396);
#1563=PLANE('',#16419);
#1564=PLANE('',#16420);
#1565=PLANE('',#16421);
#1566=PLANE('',#16422);
#1567=PLANE('',#16423);
#1568=PLANE('',#16424);
#1569=PLANE('',#16425);
#1570=PLANE('',#16426);
#1571=PLANE('',#16427);
#1572=PLANE('',#16428);
#1573=PLANE('',#16430);
#1574=PLANE('',#16432);
#1575=PLANE('',#16434);
#1576=PLANE('',#16436);
#1577=PLANE('',#16438);
#1578=PLANE('',#16441);
#1579=PLANE('',#16442);
#1580=PLANE('',#16443);
#1581=PLANE('',#16444);
#1582=PLANE('',#16449);
#1583=PLANE('',#16474);
#1584=PLANE('',#16477);
#1585=PLANE('',#16481);
#1586=PLANE('',#16483);
#1587=PLANE('',#16485);
#1588=PLANE('',#16487);
#1589=PLANE('',#16489);
#1590=PLANE('',#16491);
#1591=PLANE('',#16493);
#1592=PLANE('',#16496);
#1593=PLANE('',#16498);
#1594=PLANE('',#16500);
#1595=PLANE('',#16502);
#1596=PLANE('',#16504);
#1597=PLANE('',#16506);
#1598=PLANE('',#16532);
#1599=PLANE('',#16538);
#1600=PLANE('',#16540);
#1601=PLANE('',#16544);
#1602=PLANE('',#16545);
#1603=PLANE('',#16549);
#1604=PLANE('',#16551);
#1605=PLANE('',#16554);
#1606=FACE_OUTER_BOUND('',#2349,.T.);
#1607=FACE_OUTER_BOUND('',#2350,.T.);
#1608=FACE_OUTER_BOUND('',#2355,.T.);
#1609=FACE_OUTER_BOUND('',#2356,.T.);
#1610=FACE_OUTER_BOUND('',#2357,.T.);
#1611=FACE_OUTER_BOUND('',#2358,.T.);
#1612=FACE_OUTER_BOUND('',#2359,.T.);
#1613=FACE_OUTER_BOUND('',#2360,.T.);
#1614=FACE_OUTER_BOUND('',#2361,.T.);
#1615=FACE_OUTER_BOUND('',#2362,.T.);
#1616=FACE_OUTER_BOUND('',#2363,.T.);
#1617=FACE_OUTER_BOUND('',#2368,.T.);
#1618=FACE_OUTER_BOUND('',#2369,.T.);
#1619=FACE_OUTER_BOUND('',#2370,.T.);
#1620=FACE_OUTER_BOUND('',#2371,.T.);
#1621=FACE_OUTER_BOUND('',#2372,.T.);
#1622=FACE_OUTER_BOUND('',#2373,.T.);
#1623=FACE_OUTER_BOUND('',#2374,.T.);
#1624=FACE_OUTER_BOUND('',#2375,.T.);
#1625=FACE_OUTER_BOUND('',#2376,.T.);
#1626=FACE_OUTER_BOUND('',#2385,.T.);
#1627=FACE_OUTER_BOUND('',#2386,.T.);
#1628=FACE_OUTER_BOUND('',#2387,.T.);
#1629=FACE_OUTER_BOUND('',#2388,.T.);
#1630=FACE_OUTER_BOUND('',#2389,.T.);
#1631=FACE_OUTER_BOUND('',#2390,.T.);
#1632=FACE_OUTER_BOUND('',#2391,.T.);
#1633=FACE_OUTER_BOUND('',#2392,.T.);
#1634=FACE_OUTER_BOUND('',#2393,.T.);
#1635=FACE_OUTER_BOUND('',#2394,.T.);
#1636=FACE_OUTER_BOUND('',#2395,.T.);
#1637=FACE_OUTER_BOUND('',#2396,.T.);
#1638=FACE_OUTER_BOUND('',#2397,.T.);
#1639=FACE_OUTER_BOUND('',#2398,.T.);
#1640=FACE_OUTER_BOUND('',#2399,.T.);
#1641=FACE_OUTER_BOUND('',#2400,.T.);
#1642=FACE_OUTER_BOUND('',#2401,.T.);
#1643=FACE_OUTER_BOUND('',#2402,.T.);
#1644=FACE_OUTER_BOUND('',#2403,.T.);
#1645=FACE_OUTER_BOUND('',#2404,.T.);
#1646=FACE_OUTER_BOUND('',#2405,.T.);
#1647=FACE_OUTER_BOUND('',#2406,.T.);
#1648=FACE_OUTER_BOUND('',#2407,.T.);
#1649=FACE_OUTER_BOUND('',#2408,.T.);
#1650=FACE_OUTER_BOUND('',#2409,.T.);
#1651=FACE_OUTER_BOUND('',#2410,.T.);
#1652=FACE_OUTER_BOUND('',#2411,.T.);
#1653=FACE_OUTER_BOUND('',#2412,.T.);
#1654=FACE_OUTER_BOUND('',#2413,.T.);
#1655=FACE_OUTER_BOUND('',#2414,.T.);
#1656=FACE_OUTER_BOUND('',#2415,.T.);
#1657=FACE_OUTER_BOUND('',#2416,.T.);
#1658=FACE_OUTER_BOUND('',#2417,.T.);
#1659=FACE_OUTER_BOUND('',#2418,.T.);
#1660=FACE_OUTER_BOUND('',#2419,.T.);
#1661=FACE_OUTER_BOUND('',#2420,.T.);
#1662=FACE_OUTER_BOUND('',#2421,.T.);
#1663=FACE_OUTER_BOUND('',#2422,.T.);
#1664=FACE_OUTER_BOUND('',#2423,.T.);
#1665=FACE_OUTER_BOUND('',#2424,.T.);
#1666=FACE_OUTER_BOUND('',#2425,.T.);
#1667=FACE_OUTER_BOUND('',#2426,.T.);
#1668=FACE_OUTER_BOUND('',#2431,.T.);
#1669=FACE_OUTER_BOUND('',#2432,.T.);
#1670=FACE_OUTER_BOUND('',#2433,.T.);
#1671=FACE_OUTER_BOUND('',#2434,.T.);
#1672=FACE_OUTER_BOUND('',#2435,.T.);
#1673=FACE_OUTER_BOUND('',#2436,.T.);
#1674=FACE_OUTER_BOUND('',#2437,.T.);
#1675=FACE_OUTER_BOUND('',#2438,.T.);
#1676=FACE_OUTER_BOUND('',#2443,.T.);
#1677=FACE_OUTER_BOUND('',#2444,.T.);
#1678=FACE_OUTER_BOUND('',#2445,.T.);
#1679=FACE_OUTER_BOUND('',#2446,.T.);
#1680=FACE_OUTER_BOUND('',#2447,.T.);
#1681=FACE_OUTER_BOUND('',#2448,.T.);
#1682=FACE_OUTER_BOUND('',#2449,.T.);
#1683=FACE_OUTER_BOUND('',#2450,.T.);
#1684=FACE_OUTER_BOUND('',#2451,.T.);
#1685=FACE_OUTER_BOUND('',#2452,.T.);
#1686=FACE_OUTER_BOUND('',#2453,.T.);
#1687=FACE_OUTER_BOUND('',#2454,.T.);
#1688=FACE_OUTER_BOUND('',#2458,.T.);
#1689=FACE_OUTER_BOUND('',#2459,.T.);
#1690=FACE_OUTER_BOUND('',#2460,.T.);
#1691=FACE_OUTER_BOUND('',#2461,.T.);
#1692=FACE_OUTER_BOUND('',#2463,.T.);
#1693=FACE_OUTER_BOUND('',#2465,.T.);
#1694=FACE_OUTER_BOUND('',#2467,.T.);
#1695=FACE_OUTER_BOUND('',#2468,.T.);
#1696=FACE_OUTER_BOUND('',#2469,.T.);
#1697=FACE_OUTER_BOUND('',#2470,.T.);
#1698=FACE_OUTER_BOUND('',#2471,.T.);
#1699=FACE_OUTER_BOUND('',#2472,.T.);
#1700=FACE_OUTER_BOUND('',#2473,.T.);
#1701=FACE_OUTER_BOUND('',#2474,.T.);
#1702=FACE_OUTER_BOUND('',#2475,.T.);
#1703=FACE_OUTER_BOUND('',#2476,.T.);
#1704=FACE_OUTER_BOUND('',#2477,.T.);
#1705=FACE_OUTER_BOUND('',#2478,.T.);
#1706=FACE_OUTER_BOUND('',#2479,.T.);
#1707=FACE_OUTER_BOUND('',#2483,.T.);
#1708=FACE_OUTER_BOUND('',#2484,.T.);
#1709=FACE_OUTER_BOUND('',#2485,.T.);
#1710=FACE_OUTER_BOUND('',#2486,.T.);
#1711=FACE_OUTER_BOUND('',#2488,.T.);
#1712=FACE_OUTER_BOUND('',#2490,.T.);
#1713=FACE_OUTER_BOUND('',#2492,.T.);
#1714=FACE_OUTER_BOUND('',#2493,.T.);
#1715=FACE_OUTER_BOUND('',#2494,.T.);
#1716=FACE_OUTER_BOUND('',#2495,.T.);
#1717=FACE_OUTER_BOUND('',#2496,.T.);
#1718=FACE_OUTER_BOUND('',#2501,.T.);
#1719=FACE_OUTER_BOUND('',#2502,.T.);
#1720=FACE_OUTER_BOUND('',#2503,.T.);
#1721=FACE_OUTER_BOUND('',#2504,.T.);
#1722=FACE_OUTER_BOUND('',#2505,.T.);
#1723=FACE_OUTER_BOUND('',#2506,.T.);
#1724=FACE_OUTER_BOUND('',#2507,.T.);
#1725=FACE_OUTER_BOUND('',#2508,.T.);
#1726=FACE_OUTER_BOUND('',#2509,.T.);
#1727=FACE_OUTER_BOUND('',#2510,.T.);
#1728=FACE_OUTER_BOUND('',#2511,.T.);
#1729=FACE_OUTER_BOUND('',#2512,.T.);
#1730=FACE_OUTER_BOUND('',#2513,.T.);
#1731=FACE_OUTER_BOUND('',#2518,.T.);
#1732=FACE_OUTER_BOUND('',#2519,.T.);
#1733=FACE_OUTER_BOUND('',#2520,.T.);
#1734=FACE_OUTER_BOUND('',#2521,.T.);
#1735=FACE_OUTER_BOUND('',#2522,.T.);
#1736=FACE_OUTER_BOUND('',#2523,.T.);
#1737=FACE_OUTER_BOUND('',#2524,.T.);
#1738=FACE_OUTER_BOUND('',#2525,.T.);
#1739=FACE_OUTER_BOUND('',#2526,.T.);
#1740=FACE_OUTER_BOUND('',#2527,.T.);
#1741=FACE_OUTER_BOUND('',#2528,.T.);
#1742=FACE_OUTER_BOUND('',#2529,.T.);
#1743=FACE_OUTER_BOUND('',#2530,.T.);
#1744=FACE_OUTER_BOUND('',#2545,.T.);
#1745=FACE_OUTER_BOUND('',#2546,.T.);
#1746=FACE_OUTER_BOUND('',#2547,.T.);
#1747=FACE_OUTER_BOUND('',#2548,.T.);
#1748=FACE_OUTER_BOUND('',#2549,.T.);
#1749=FACE_OUTER_BOUND('',#2550,.T.);
#1750=FACE_OUTER_BOUND('',#2551,.T.);
#1751=FACE_OUTER_BOUND('',#2552,.T.);
#1752=FACE_OUTER_BOUND('',#2553,.T.);
#1753=FACE_OUTER_BOUND('',#2554,.T.);
#1754=FACE_OUTER_BOUND('',#2555,.T.);
#1755=FACE_OUTER_BOUND('',#2556,.T.);
#1756=FACE_OUTER_BOUND('',#2557,.T.);
#1757=FACE_OUTER_BOUND('',#2558,.T.);
#1758=FACE_OUTER_BOUND('',#2559,.T.);
#1759=FACE_OUTER_BOUND('',#2560,.T.);
#1760=FACE_OUTER_BOUND('',#2561,.T.);
#1761=FACE_OUTER_BOUND('',#2562,.T.);
#1762=FACE_OUTER_BOUND('',#2563,.T.);
#1763=FACE_OUTER_BOUND('',#2564,.T.);
#1764=FACE_OUTER_BOUND('',#2565,.T.);
#1765=FACE_OUTER_BOUND('',#2566,.T.);
#1766=FACE_OUTER_BOUND('',#2567,.T.);
#1767=FACE_OUTER_BOUND('',#2568,.T.);
#1768=FACE_OUTER_BOUND('',#2569,.T.);
#1769=FACE_OUTER_BOUND('',#2570,.T.);
#1770=FACE_OUTER_BOUND('',#2571,.T.);
#1771=FACE_OUTER_BOUND('',#2572,.T.);
#1772=FACE_OUTER_BOUND('',#2573,.T.);
#1773=FACE_OUTER_BOUND('',#2574,.T.);
#1774=FACE_OUTER_BOUND('',#2575,.T.);
#1775=FACE_OUTER_BOUND('',#2576,.T.);
#1776=FACE_OUTER_BOUND('',#2577,.T.);
#1777=FACE_OUTER_BOUND('',#2578,.T.);
#1778=FACE_OUTER_BOUND('',#2580,.T.);
#1779=FACE_OUTER_BOUND('',#2582,.T.);
#1780=FACE_OUTER_BOUND('',#2584,.T.);
#1781=FACE_OUTER_BOUND('',#2586,.T.);
#1782=FACE_OUTER_BOUND('',#2588,.T.);
#1783=FACE_OUTER_BOUND('',#2590,.T.);
#1784=FACE_OUTER_BOUND('',#2592,.T.);
#1785=FACE_OUTER_BOUND('',#2594,.T.);
#1786=FACE_OUTER_BOUND('',#2595,.T.);
#1787=FACE_OUTER_BOUND('',#2596,.T.);
#1788=FACE_OUTER_BOUND('',#2597,.T.);
#1789=FACE_OUTER_BOUND('',#2598,.T.);
#1790=FACE_OUTER_BOUND('',#2599,.T.);
#1791=FACE_OUTER_BOUND('',#2600,.T.);
#1792=FACE_OUTER_BOUND('',#2601,.T.);
#1793=FACE_OUTER_BOUND('',#2602,.T.);
#1794=FACE_OUTER_BOUND('',#2603,.T.);
#1795=FACE_OUTER_BOUND('',#2604,.T.);
#1796=FACE_OUTER_BOUND('',#2605,.T.);
#1797=FACE_OUTER_BOUND('',#2606,.T.);
#1798=FACE_OUTER_BOUND('',#2607,.T.);
#1799=FACE_OUTER_BOUND('',#2608,.T.);
#1800=FACE_OUTER_BOUND('',#2609,.T.);
#1801=FACE_OUTER_BOUND('',#2610,.T.);
#1802=FACE_OUTER_BOUND('',#2611,.T.);
#1803=FACE_OUTER_BOUND('',#2612,.T.);
#1804=FACE_OUTER_BOUND('',#2617,.T.);
#1805=FACE_OUTER_BOUND('',#2618,.T.);
#1806=FACE_OUTER_BOUND('',#2625,.T.);
#1807=FACE_OUTER_BOUND('',#2626,.T.);
#1808=FACE_OUTER_BOUND('',#2631,.T.);
#1809=FACE_OUTER_BOUND('',#2638,.T.);
#1810=FACE_OUTER_BOUND('',#2639,.T.);
#1811=FACE_OUTER_BOUND('',#2640,.T.);
#1812=FACE_OUTER_BOUND('',#2641,.T.);
#1813=FACE_OUTER_BOUND('',#2642,.T.);
#1814=FACE_OUTER_BOUND('',#2643,.T.);
#1815=FACE_OUTER_BOUND('',#2644,.T.);
#1816=FACE_OUTER_BOUND('',#2645,.T.);
#1817=FACE_OUTER_BOUND('',#2646,.T.);
#1818=FACE_OUTER_BOUND('',#2647,.T.);
#1819=FACE_OUTER_BOUND('',#2648,.T.);
#1820=FACE_OUTER_BOUND('',#2649,.T.);
#1821=FACE_OUTER_BOUND('',#2650,.T.);
#1822=FACE_OUTER_BOUND('',#2651,.T.);
#1823=FACE_OUTER_BOUND('',#2652,.T.);
#1824=FACE_OUTER_BOUND('',#2656,.T.);
#1825=FACE_OUTER_BOUND('',#2657,.T.);
#1826=FACE_OUTER_BOUND('',#2658,.T.);
#1827=FACE_OUTER_BOUND('',#2659,.T.);
#1828=FACE_OUTER_BOUND('',#2660,.T.);
#1829=FACE_OUTER_BOUND('',#2661,.T.);
#1830=FACE_OUTER_BOUND('',#2662,.T.);
#1831=FACE_OUTER_BOUND('',#2663,.T.);
#1832=FACE_OUTER_BOUND('',#2664,.T.);
#1833=FACE_OUTER_BOUND('',#2665,.T.);
#1834=FACE_OUTER_BOUND('',#2666,.T.);
#1835=FACE_OUTER_BOUND('',#2667,.T.);
#1836=FACE_OUTER_BOUND('',#2668,.T.);
#1837=FACE_OUTER_BOUND('',#2669,.T.);
#1838=FACE_OUTER_BOUND('',#2670,.T.);
#1839=FACE_OUTER_BOUND('',#2671,.T.);
#1840=FACE_OUTER_BOUND('',#2672,.T.);
#1841=FACE_OUTER_BOUND('',#2673,.T.);
#1842=FACE_OUTER_BOUND('',#2674,.T.);
#1843=FACE_OUTER_BOUND('',#2675,.T.);
#1844=FACE_OUTER_BOUND('',#2676,.T.);
#1845=FACE_OUTER_BOUND('',#2677,.T.);
#1846=FACE_OUTER_BOUND('',#2678,.T.);
#1847=FACE_OUTER_BOUND('',#2679,.T.);
#1848=FACE_OUTER_BOUND('',#2680,.T.);
#1849=FACE_OUTER_BOUND('',#2681,.T.);
#1850=FACE_OUTER_BOUND('',#2682,.T.);
#1851=FACE_OUTER_BOUND('',#2683,.T.);
#1852=FACE_OUTER_BOUND('',#2684,.T.);
#1853=FACE_OUTER_BOUND('',#2685,.T.);
#1854=FACE_OUTER_BOUND('',#2686,.T.);
#1855=FACE_OUTER_BOUND('',#2687,.T.);
#1856=FACE_OUTER_BOUND('',#2688,.T.);
#1857=FACE_OUTER_BOUND('',#2689,.T.);
#1858=FACE_OUTER_BOUND('',#2690,.T.);
#1859=FACE_OUTER_BOUND('',#2691,.T.);
#1860=FACE_OUTER_BOUND('',#2692,.T.);
#1861=FACE_OUTER_BOUND('',#2693,.T.);
#1862=FACE_OUTER_BOUND('',#2694,.T.);
#1863=FACE_OUTER_BOUND('',#2695,.T.);
#1864=FACE_OUTER_BOUND('',#2696,.T.);
#1865=FACE_OUTER_BOUND('',#2697,.T.);
#1866=FACE_OUTER_BOUND('',#2698,.T.);
#1867=FACE_OUTER_BOUND('',#2699,.T.);
#1868=FACE_OUTER_BOUND('',#2700,.T.);
#1869=FACE_OUTER_BOUND('',#2701,.T.);
#1870=FACE_OUTER_BOUND('',#2702,.T.);
#1871=FACE_OUTER_BOUND('',#2703,.T.);
#1872=FACE_OUTER_BOUND('',#2704,.T.);
#1873=FACE_OUTER_BOUND('',#2709,.T.);
#1874=FACE_OUTER_BOUND('',#2710,.T.);
#1875=FACE_OUTER_BOUND('',#2711,.T.);
#1876=FACE_OUTER_BOUND('',#2712,.T.);
#1877=FACE_OUTER_BOUND('',#2713,.T.);
#1878=FACE_OUTER_BOUND('',#2714,.T.);
#1879=FACE_OUTER_BOUND('',#2715,.T.);
#1880=FACE_OUTER_BOUND('',#2716,.T.);
#1881=FACE_OUTER_BOUND('',#2717,.T.);
#1882=FACE_OUTER_BOUND('',#2718,.T.);
#1883=FACE_OUTER_BOUND('',#2719,.T.);
#1884=FACE_OUTER_BOUND('',#2720,.T.);
#1885=FACE_OUTER_BOUND('',#2721,.T.);
#1886=FACE_OUTER_BOUND('',#2722,.T.);
#1887=FACE_OUTER_BOUND('',#2723,.T.);
#1888=FACE_OUTER_BOUND('',#2724,.T.);
#1889=FACE_OUTER_BOUND('',#2725,.T.);
#1890=FACE_OUTER_BOUND('',#2726,.T.);
#1891=FACE_OUTER_BOUND('',#2727,.T.);
#1892=FACE_OUTER_BOUND('',#2728,.T.);
#1893=FACE_OUTER_BOUND('',#2729,.T.);
#1894=FACE_OUTER_BOUND('',#2730,.T.);
#1895=FACE_OUTER_BOUND('',#2731,.T.);
#1896=FACE_OUTER_BOUND('',#2732,.T.);
#1897=FACE_OUTER_BOUND('',#2733,.T.);
#1898=FACE_OUTER_BOUND('',#2734,.T.);
#1899=FACE_OUTER_BOUND('',#2735,.T.);
#1900=FACE_OUTER_BOUND('',#2736,.T.);
#1901=FACE_OUTER_BOUND('',#2737,.T.);
#1902=FACE_OUTER_BOUND('',#2738,.T.);
#1903=FACE_OUTER_BOUND('',#2739,.T.);
#1904=FACE_OUTER_BOUND('',#2740,.T.);
#1905=FACE_OUTER_BOUND('',#2741,.T.);
#1906=FACE_OUTER_BOUND('',#2742,.T.);
#1907=FACE_OUTER_BOUND('',#2743,.T.);
#1908=FACE_OUTER_BOUND('',#2744,.T.);
#1909=FACE_OUTER_BOUND('',#2745,.T.);
#1910=FACE_OUTER_BOUND('',#2746,.T.);
#1911=FACE_OUTER_BOUND('',#2747,.T.);
#1912=FACE_OUTER_BOUND('',#2748,.T.);
#1913=FACE_OUTER_BOUND('',#2749,.T.);
#1914=FACE_OUTER_BOUND('',#2750,.T.);
#1915=FACE_OUTER_BOUND('',#2751,.T.);
#1916=FACE_OUTER_BOUND('',#2752,.T.);
#1917=FACE_OUTER_BOUND('',#2753,.T.);
#1918=FACE_OUTER_BOUND('',#2754,.T.);
#1919=FACE_OUTER_BOUND('',#2755,.T.);
#1920=FACE_OUTER_BOUND('',#2756,.T.);
#1921=FACE_OUTER_BOUND('',#2757,.T.);
#1922=FACE_OUTER_BOUND('',#2758,.T.);
#1923=FACE_OUTER_BOUND('',#2759,.T.);
#1924=FACE_OUTER_BOUND('',#2760,.T.);
#1925=FACE_OUTER_BOUND('',#2761,.T.);
#1926=FACE_OUTER_BOUND('',#2762,.T.);
#1927=FACE_OUTER_BOUND('',#2763,.T.);
#1928=FACE_OUTER_BOUND('',#2764,.T.);
#1929=FACE_OUTER_BOUND('',#2765,.T.);
#1930=FACE_OUTER_BOUND('',#2766,.T.);
#1931=FACE_OUTER_BOUND('',#2767,.T.);
#1932=FACE_OUTER_BOUND('',#2768,.T.);
#1933=FACE_OUTER_BOUND('',#2769,.T.);
#1934=FACE_OUTER_BOUND('',#2770,.T.);
#1935=FACE_OUTER_BOUND('',#2771,.T.);
#1936=FACE_OUTER_BOUND('',#2772,.T.);
#1937=FACE_OUTER_BOUND('',#2773,.T.);
#1938=FACE_OUTER_BOUND('',#2774,.T.);
#1939=FACE_OUTER_BOUND('',#2775,.T.);
#1940=FACE_OUTER_BOUND('',#2776,.T.);
#1941=FACE_OUTER_BOUND('',#2777,.T.);
#1942=FACE_OUTER_BOUND('',#2778,.T.);
#1943=FACE_OUTER_BOUND('',#2779,.T.);
#1944=FACE_OUTER_BOUND('',#2780,.T.);
#1945=FACE_OUTER_BOUND('',#2781,.T.);
#1946=FACE_OUTER_BOUND('',#2782,.T.);
#1947=FACE_OUTER_BOUND('',#2783,.T.);
#1948=FACE_OUTER_BOUND('',#2784,.T.);
#1949=FACE_OUTER_BOUND('',#2785,.T.);
#1950=FACE_OUTER_BOUND('',#2786,.T.);
#1951=FACE_OUTER_BOUND('',#2787,.T.);
#1952=FACE_OUTER_BOUND('',#2788,.T.);
#1953=FACE_OUTER_BOUND('',#2789,.T.);
#1954=FACE_OUTER_BOUND('',#2790,.T.);
#1955=FACE_OUTER_BOUND('',#2791,.T.);
#1956=FACE_OUTER_BOUND('',#2792,.T.);
#1957=FACE_OUTER_BOUND('',#2793,.T.);
#1958=FACE_OUTER_BOUND('',#2794,.T.);
#1959=FACE_OUTER_BOUND('',#2795,.T.);
#1960=FACE_OUTER_BOUND('',#2796,.T.);
#1961=FACE_OUTER_BOUND('',#2797,.T.);
#1962=FACE_OUTER_BOUND('',#2798,.T.);
#1963=FACE_OUTER_BOUND('',#2799,.T.);
#1964=FACE_OUTER_BOUND('',#2800,.T.);
#1965=FACE_OUTER_BOUND('',#2801,.T.);
#1966=FACE_OUTER_BOUND('',#2802,.T.);
#1967=FACE_OUTER_BOUND('',#2803,.T.);
#1968=FACE_OUTER_BOUND('',#2804,.T.);
#1969=FACE_OUTER_BOUND('',#2805,.T.);
#1970=FACE_OUTER_BOUND('',#2806,.T.);
#1971=FACE_OUTER_BOUND('',#2807,.T.);
#1972=FACE_OUTER_BOUND('',#2808,.T.);
#1973=FACE_OUTER_BOUND('',#2809,.T.);
#1974=FACE_OUTER_BOUND('',#2810,.T.);
#1975=FACE_OUTER_BOUND('',#2811,.T.);
#1976=FACE_OUTER_BOUND('',#2812,.T.);
#1977=FACE_OUTER_BOUND('',#2813,.T.);
#1978=FACE_OUTER_BOUND('',#2814,.T.);
#1979=FACE_OUTER_BOUND('',#2815,.T.);
#1980=FACE_OUTER_BOUND('',#2816,.T.);
#1981=FACE_OUTER_BOUND('',#2817,.T.);
#1982=FACE_OUTER_BOUND('',#2818,.T.);
#1983=FACE_OUTER_BOUND('',#2819,.T.);
#1984=FACE_OUTER_BOUND('',#2820,.T.);
#1985=FACE_OUTER_BOUND('',#2821,.T.);
#1986=FACE_OUTER_BOUND('',#2822,.T.);
#1987=FACE_OUTER_BOUND('',#2823,.T.);
#1988=FACE_OUTER_BOUND('',#2824,.T.);
#1989=FACE_OUTER_BOUND('',#2825,.T.);
#1990=FACE_OUTER_BOUND('',#2826,.T.);
#1991=FACE_OUTER_BOUND('',#2827,.T.);
#1992=FACE_OUTER_BOUND('',#2828,.T.);
#1993=FACE_OUTER_BOUND('',#2829,.T.);
#1994=FACE_OUTER_BOUND('',#2830,.T.);
#1995=FACE_OUTER_BOUND('',#2831,.T.);
#1996=FACE_OUTER_BOUND('',#2832,.T.);
#1997=FACE_OUTER_BOUND('',#2833,.T.);
#1998=FACE_OUTER_BOUND('',#2834,.T.);
#1999=FACE_OUTER_BOUND('',#2835,.T.);
#2000=FACE_OUTER_BOUND('',#2836,.T.);
#2001=FACE_OUTER_BOUND('',#2837,.T.);
#2002=FACE_OUTER_BOUND('',#2838,.T.);
#2003=FACE_OUTER_BOUND('',#2839,.T.);
#2004=FACE_OUTER_BOUND('',#2840,.T.);
#2005=FACE_OUTER_BOUND('',#2841,.T.);
#2006=FACE_OUTER_BOUND('',#2842,.T.);
#2007=FACE_OUTER_BOUND('',#2843,.T.);
#2008=FACE_OUTER_BOUND('',#2844,.T.);
#2009=FACE_OUTER_BOUND('',#2845,.T.);
#2010=FACE_OUTER_BOUND('',#2846,.T.);
#2011=FACE_OUTER_BOUND('',#2847,.T.);
#2012=FACE_OUTER_BOUND('',#2848,.T.);
#2013=FACE_OUTER_BOUND('',#2849,.T.);
#2014=FACE_OUTER_BOUND('',#2850,.T.);
#2015=FACE_OUTER_BOUND('',#2851,.T.);
#2016=FACE_OUTER_BOUND('',#2852,.T.);
#2017=FACE_OUTER_BOUND('',#2853,.T.);
#2018=FACE_OUTER_BOUND('',#2854,.T.);
#2019=FACE_OUTER_BOUND('',#2855,.T.);
#2020=FACE_OUTER_BOUND('',#2856,.T.);
#2021=FACE_OUTER_BOUND('',#2857,.T.);
#2022=FACE_OUTER_BOUND('',#2858,.T.);
#2023=FACE_OUTER_BOUND('',#2859,.T.);
#2024=FACE_OUTER_BOUND('',#2860,.T.);
#2025=FACE_OUTER_BOUND('',#2861,.T.);
#2026=FACE_OUTER_BOUND('',#2862,.T.);
#2027=FACE_OUTER_BOUND('',#2863,.T.);
#2028=FACE_OUTER_BOUND('',#2864,.T.);
#2029=FACE_OUTER_BOUND('',#2865,.T.);
#2030=FACE_OUTER_BOUND('',#2866,.T.);
#2031=FACE_OUTER_BOUND('',#2867,.T.);
#2032=FACE_OUTER_BOUND('',#2868,.T.);
#2033=FACE_OUTER_BOUND('',#2869,.T.);
#2034=FACE_OUTER_BOUND('',#2870,.T.);
#2035=FACE_OUTER_BOUND('',#2871,.T.);
#2036=FACE_OUTER_BOUND('',#2872,.T.);
#2037=FACE_OUTER_BOUND('',#2873,.T.);
#2038=FACE_OUTER_BOUND('',#2874,.T.);
#2039=FACE_OUTER_BOUND('',#2875,.T.);
#2040=FACE_OUTER_BOUND('',#2876,.T.);
#2041=FACE_OUTER_BOUND('',#2877,.T.);
#2042=FACE_OUTER_BOUND('',#2878,.T.);
#2043=FACE_OUTER_BOUND('',#2879,.T.);
#2044=FACE_OUTER_BOUND('',#2880,.T.);
#2045=FACE_OUTER_BOUND('',#2881,.T.);
#2046=FACE_OUTER_BOUND('',#2882,.T.);
#2047=FACE_OUTER_BOUND('',#2883,.T.);
#2048=FACE_OUTER_BOUND('',#2899,.T.);
#2049=FACE_OUTER_BOUND('',#2915,.T.);
#2050=FACE_OUTER_BOUND('',#2916,.T.);
#2051=FACE_OUTER_BOUND('',#2917,.T.);
#2052=FACE_OUTER_BOUND('',#2918,.T.);
#2053=FACE_OUTER_BOUND('',#2919,.T.);
#2054=FACE_OUTER_BOUND('',#2920,.T.);
#2055=FACE_OUTER_BOUND('',#2921,.T.);
#2056=FACE_OUTER_BOUND('',#2922,.T.);
#2057=FACE_OUTER_BOUND('',#2923,.T.);
#2058=FACE_OUTER_BOUND('',#2924,.T.);
#2059=FACE_OUTER_BOUND('',#2925,.T.);
#2060=FACE_OUTER_BOUND('',#2926,.T.);
#2061=FACE_OUTER_BOUND('',#2927,.T.);
#2062=FACE_OUTER_BOUND('',#2928,.T.);
#2063=FACE_OUTER_BOUND('',#2929,.T.);
#2064=FACE_OUTER_BOUND('',#2930,.T.);
#2065=FACE_OUTER_BOUND('',#2931,.T.);
#2066=FACE_OUTER_BOUND('',#2932,.T.);
#2067=FACE_OUTER_BOUND('',#2933,.T.);
#2068=FACE_OUTER_BOUND('',#2934,.T.);
#2069=FACE_OUTER_BOUND('',#2935,.T.);
#2070=FACE_OUTER_BOUND('',#2936,.T.);
#2071=FACE_OUTER_BOUND('',#2937,.T.);
#2072=FACE_OUTER_BOUND('',#2938,.T.);
#2073=FACE_OUTER_BOUND('',#2939,.T.);
#2074=FACE_OUTER_BOUND('',#2940,.T.);
#2075=FACE_OUTER_BOUND('',#2941,.T.);
#2076=FACE_OUTER_BOUND('',#2942,.T.);
#2077=FACE_OUTER_BOUND('',#2943,.T.);
#2078=FACE_OUTER_BOUND('',#2944,.T.);
#2079=FACE_OUTER_BOUND('',#2945,.T.);
#2080=FACE_OUTER_BOUND('',#2946,.T.);
#2081=FACE_OUTER_BOUND('',#2947,.T.);
#2082=FACE_OUTER_BOUND('',#2948,.T.);
#2083=FACE_OUTER_BOUND('',#2949,.T.);
#2084=FACE_OUTER_BOUND('',#2950,.T.);
#2085=FACE_OUTER_BOUND('',#2951,.T.);
#2086=FACE_OUTER_BOUND('',#2953,.T.);
#2087=FACE_OUTER_BOUND('',#2954,.T.);
#2088=FACE_OUTER_BOUND('',#2955,.T.);
#2089=FACE_OUTER_BOUND('',#2956,.T.);
#2090=FACE_OUTER_BOUND('',#2957,.T.);
#2091=FACE_OUTER_BOUND('',#2958,.T.);
#2092=FACE_OUTER_BOUND('',#2959,.T.);
#2093=FACE_OUTER_BOUND('',#2960,.T.);
#2094=FACE_OUTER_BOUND('',#2961,.T.);
#2095=FACE_OUTER_BOUND('',#2962,.T.);
#2096=FACE_OUTER_BOUND('',#2963,.T.);
#2097=FACE_OUTER_BOUND('',#2964,.T.);
#2098=FACE_OUTER_BOUND('',#2965,.T.);
#2099=FACE_OUTER_BOUND('',#2966,.T.);
#2100=FACE_OUTER_BOUND('',#2967,.T.);
#2101=FACE_OUTER_BOUND('',#2968,.T.);
#2102=FACE_OUTER_BOUND('',#2969,.T.);
#2103=FACE_OUTER_BOUND('',#2970,.T.);
#2104=FACE_OUTER_BOUND('',#2971,.T.);
#2105=FACE_OUTER_BOUND('',#2972,.T.);
#2106=FACE_OUTER_BOUND('',#2973,.T.);
#2107=FACE_OUTER_BOUND('',#2974,.T.);
#2108=FACE_OUTER_BOUND('',#2975,.T.);
#2109=FACE_OUTER_BOUND('',#2976,.T.);
#2110=FACE_OUTER_BOUND('',#2977,.T.);
#2111=FACE_OUTER_BOUND('',#2978,.T.);
#2112=FACE_OUTER_BOUND('',#2979,.T.);
#2113=FACE_OUTER_BOUND('',#2980,.T.);
#2114=FACE_OUTER_BOUND('',#2981,.T.);
#2115=FACE_OUTER_BOUND('',#2982,.T.);
#2116=FACE_OUTER_BOUND('',#2983,.T.);
#2117=FACE_OUTER_BOUND('',#2984,.T.);
#2118=FACE_OUTER_BOUND('',#2985,.T.);
#2119=FACE_OUTER_BOUND('',#2986,.T.);
#2120=FACE_OUTER_BOUND('',#2987,.T.);
#2121=FACE_OUTER_BOUND('',#2988,.T.);
#2122=FACE_OUTER_BOUND('',#2989,.T.);
#2123=FACE_OUTER_BOUND('',#2990,.T.);
#2124=FACE_OUTER_BOUND('',#2991,.T.);
#2125=FACE_OUTER_BOUND('',#2992,.T.);
#2126=FACE_OUTER_BOUND('',#2993,.T.);
#2127=FACE_OUTER_BOUND('',#2994,.T.);
#2128=FACE_OUTER_BOUND('',#2995,.T.);
#2129=FACE_OUTER_BOUND('',#2996,.T.);
#2130=FACE_OUTER_BOUND('',#2997,.T.);
#2131=FACE_OUTER_BOUND('',#2998,.T.);
#2132=FACE_OUTER_BOUND('',#2999,.T.);
#2133=FACE_OUTER_BOUND('',#3000,.T.);
#2134=FACE_OUTER_BOUND('',#3001,.T.);
#2135=FACE_OUTER_BOUND('',#3002,.T.);
#2136=FACE_OUTER_BOUND('',#3003,.T.);
#2137=FACE_OUTER_BOUND('',#3004,.T.);
#2138=FACE_OUTER_BOUND('',#3005,.T.);
#2139=FACE_OUTER_BOUND('',#3006,.T.);
#2140=FACE_OUTER_BOUND('',#3007,.T.);
#2141=FACE_OUTER_BOUND('',#3008,.T.);
#2142=FACE_OUTER_BOUND('',#3009,.T.);
#2143=FACE_OUTER_BOUND('',#3010,.T.);
#2144=FACE_OUTER_BOUND('',#3011,.T.);
#2145=FACE_OUTER_BOUND('',#3012,.T.);
#2146=FACE_OUTER_BOUND('',#3013,.T.);
#2147=FACE_OUTER_BOUND('',#3014,.T.);
#2148=FACE_OUTER_BOUND('',#3015,.T.);
#2149=FACE_OUTER_BOUND('',#3016,.T.);
#2150=FACE_OUTER_BOUND('',#3017,.T.);
#2151=FACE_OUTER_BOUND('',#3018,.T.);
#2152=FACE_OUTER_BOUND('',#3019,.T.);
#2153=FACE_OUTER_BOUND('',#3020,.T.);
#2154=FACE_OUTER_BOUND('',#3021,.T.);
#2155=FACE_OUTER_BOUND('',#3022,.T.);
#2156=FACE_OUTER_BOUND('',#3023,.T.);
#2157=FACE_OUTER_BOUND('',#3024,.T.);
#2158=FACE_OUTER_BOUND('',#3025,.T.);
#2159=FACE_OUTER_BOUND('',#3026,.T.);
#2160=FACE_OUTER_BOUND('',#3027,.T.);
#2161=FACE_OUTER_BOUND('',#3028,.T.);
#2162=FACE_OUTER_BOUND('',#3029,.T.);
#2163=FACE_OUTER_BOUND('',#3030,.T.);
#2164=FACE_OUTER_BOUND('',#3031,.T.);
#2165=FACE_OUTER_BOUND('',#3032,.T.);
#2166=FACE_OUTER_BOUND('',#3033,.T.);
#2167=FACE_OUTER_BOUND('',#3034,.T.);
#2168=FACE_OUTER_BOUND('',#3035,.T.);
#2169=FACE_OUTER_BOUND('',#3036,.T.);
#2170=FACE_OUTER_BOUND('',#3037,.T.);
#2171=FACE_OUTER_BOUND('',#3038,.T.);
#2172=FACE_OUTER_BOUND('',#3039,.T.);
#2173=FACE_OUTER_BOUND('',#3040,.T.);
#2174=FACE_OUTER_BOUND('',#3041,.T.);
#2175=FACE_OUTER_BOUND('',#3042,.T.);
#2176=FACE_OUTER_BOUND('',#3043,.T.);
#2177=FACE_OUTER_BOUND('',#3044,.T.);
#2178=FACE_OUTER_BOUND('',#3045,.T.);
#2179=FACE_OUTER_BOUND('',#3046,.T.);
#2180=FACE_OUTER_BOUND('',#3047,.T.);
#2181=FACE_OUTER_BOUND('',#3048,.T.);
#2182=FACE_OUTER_BOUND('',#3049,.T.);
#2183=FACE_OUTER_BOUND('',#3050,.T.);
#2184=FACE_OUTER_BOUND('',#3051,.T.);
#2185=FACE_OUTER_BOUND('',#3052,.T.);
#2186=FACE_OUTER_BOUND('',#3053,.T.);
#2187=FACE_OUTER_BOUND('',#3054,.T.);
#2188=FACE_OUTER_BOUND('',#3055,.T.);
#2189=FACE_OUTER_BOUND('',#3056,.T.);
#2190=FACE_OUTER_BOUND('',#3057,.T.);
#2191=FACE_OUTER_BOUND('',#3058,.T.);
#2192=FACE_OUTER_BOUND('',#3059,.T.);
#2193=FACE_OUTER_BOUND('',#3060,.T.);
#2194=FACE_OUTER_BOUND('',#3061,.T.);
#2195=FACE_OUTER_BOUND('',#3062,.T.);
#2196=FACE_OUTER_BOUND('',#3063,.T.);
#2197=FACE_OUTER_BOUND('',#3064,.T.);
#2198=FACE_OUTER_BOUND('',#3065,.T.);
#2199=FACE_OUTER_BOUND('',#3066,.T.);
#2200=FACE_OUTER_BOUND('',#3068,.T.);
#2201=FACE_OUTER_BOUND('',#3069,.T.);
#2202=FACE_OUTER_BOUND('',#3070,.T.);
#2203=FACE_OUTER_BOUND('',#3071,.T.);
#2204=FACE_OUTER_BOUND('',#3072,.T.);
#2205=FACE_OUTER_BOUND('',#3073,.T.);
#2206=FACE_OUTER_BOUND('',#3074,.T.);
#2207=FACE_OUTER_BOUND('',#3075,.T.);
#2208=FACE_OUTER_BOUND('',#3076,.T.);
#2209=FACE_OUTER_BOUND('',#3077,.T.);
#2210=FACE_OUTER_BOUND('',#3078,.T.);
#2211=FACE_OUTER_BOUND('',#3079,.T.);
#2212=FACE_OUTER_BOUND('',#3080,.T.);
#2213=FACE_OUTER_BOUND('',#3081,.T.);
#2214=FACE_OUTER_BOUND('',#3082,.T.);
#2215=FACE_OUTER_BOUND('',#3083,.T.);
#2216=FACE_OUTER_BOUND('',#3084,.T.);
#2217=FACE_OUTER_BOUND('',#3085,.T.);
#2218=FACE_OUTER_BOUND('',#3086,.T.);
#2219=FACE_OUTER_BOUND('',#3087,.T.);
#2220=FACE_OUTER_BOUND('',#3088,.T.);
#2221=FACE_OUTER_BOUND('',#3089,.T.);
#2222=FACE_OUTER_BOUND('',#3090,.T.);
#2223=FACE_OUTER_BOUND('',#3091,.T.);
#2224=FACE_OUTER_BOUND('',#3092,.T.);
#2225=FACE_OUTER_BOUND('',#3093,.T.);
#2226=FACE_OUTER_BOUND('',#3094,.T.);
#2227=FACE_OUTER_BOUND('',#3095,.T.);
#2228=FACE_OUTER_BOUND('',#3096,.T.);
#2229=FACE_OUTER_BOUND('',#3097,.T.);
#2230=FACE_OUTER_BOUND('',#3098,.T.);
#2231=FACE_OUTER_BOUND('',#3099,.T.);
#2232=FACE_OUTER_BOUND('',#3100,.T.);
#2233=FACE_OUTER_BOUND('',#3101,.T.);
#2234=FACE_OUTER_BOUND('',#3102,.T.);
#2235=FACE_OUTER_BOUND('',#3103,.T.);
#2236=FACE_OUTER_BOUND('',#3104,.T.);
#2237=FACE_OUTER_BOUND('',#3105,.T.);
#2238=FACE_OUTER_BOUND('',#3106,.T.);
#2239=FACE_OUTER_BOUND('',#3107,.T.);
#2240=FACE_OUTER_BOUND('',#3108,.T.);
#2241=FACE_OUTER_BOUND('',#3109,.T.);
#2242=FACE_OUTER_BOUND('',#3110,.T.);
#2243=FACE_OUTER_BOUND('',#3111,.T.);
#2244=FACE_OUTER_BOUND('',#3112,.T.);
#2245=FACE_OUTER_BOUND('',#3113,.T.);
#2246=FACE_OUTER_BOUND('',#3114,.T.);
#2247=FACE_OUTER_BOUND('',#3115,.T.);
#2248=FACE_OUTER_BOUND('',#3116,.T.);
#2249=FACE_OUTER_BOUND('',#3117,.T.);
#2250=FACE_OUTER_BOUND('',#3118,.T.);
#2251=FACE_OUTER_BOUND('',#3119,.T.);
#2252=FACE_OUTER_BOUND('',#3120,.T.);
#2253=FACE_OUTER_BOUND('',#3121,.T.);
#2254=FACE_OUTER_BOUND('',#3122,.T.);
#2255=FACE_OUTER_BOUND('',#3123,.T.);
#2256=FACE_OUTER_BOUND('',#3124,.T.);
#2257=FACE_OUTER_BOUND('',#3125,.T.);
#2258=FACE_OUTER_BOUND('',#3126,.T.);
#2259=FACE_OUTER_BOUND('',#3127,.T.);
#2260=FACE_OUTER_BOUND('',#3128,.T.);
#2261=FACE_OUTER_BOUND('',#3129,.T.);
#2262=FACE_OUTER_BOUND('',#3130,.T.);
#2263=FACE_OUTER_BOUND('',#3131,.T.);
#2264=FACE_OUTER_BOUND('',#3132,.T.);
#2265=FACE_OUTER_BOUND('',#3133,.T.);
#2266=FACE_OUTER_BOUND('',#3134,.T.);
#2267=FACE_OUTER_BOUND('',#3135,.T.);
#2268=FACE_OUTER_BOUND('',#3136,.T.);
#2269=FACE_OUTER_BOUND('',#3137,.T.);
#2270=FACE_OUTER_BOUND('',#3138,.T.);
#2271=FACE_OUTER_BOUND('',#3139,.T.);
#2272=FACE_OUTER_BOUND('',#3140,.T.);
#2273=FACE_OUTER_BOUND('',#3141,.T.);
#2274=FACE_OUTER_BOUND('',#3142,.T.);
#2275=FACE_OUTER_BOUND('',#3143,.T.);
#2276=FACE_OUTER_BOUND('',#3144,.T.);
#2277=FACE_OUTER_BOUND('',#3145,.T.);
#2278=FACE_OUTER_BOUND('',#3146,.T.);
#2279=FACE_OUTER_BOUND('',#3147,.T.);
#2280=FACE_OUTER_BOUND('',#3148,.T.);
#2281=FACE_OUTER_BOUND('',#3149,.T.);
#2282=FACE_OUTER_BOUND('',#3151,.T.);
#2283=FACE_OUTER_BOUND('',#3152,.T.);
#2284=FACE_OUTER_BOUND('',#3153,.T.);
#2285=FACE_OUTER_BOUND('',#3154,.T.);
#2286=FACE_OUTER_BOUND('',#3155,.T.);
#2287=FACE_OUTER_BOUND('',#3156,.T.);
#2288=FACE_OUTER_BOUND('',#3157,.T.);
#2289=FACE_OUTER_BOUND('',#3158,.T.);
#2290=FACE_OUTER_BOUND('',#3159,.T.);
#2291=FACE_OUTER_BOUND('',#3160,.T.);
#2292=FACE_OUTER_BOUND('',#3161,.T.);
#2293=FACE_OUTER_BOUND('',#3162,.T.);
#2294=FACE_OUTER_BOUND('',#3163,.T.);
#2295=FACE_OUTER_BOUND('',#3164,.T.);
#2296=FACE_OUTER_BOUND('',#3165,.T.);
#2297=FACE_OUTER_BOUND('',#3166,.T.);
#2298=FACE_OUTER_BOUND('',#3167,.T.);
#2299=FACE_OUTER_BOUND('',#3168,.T.);
#2300=FACE_OUTER_BOUND('',#3169,.T.);
#2301=FACE_OUTER_BOUND('',#3170,.T.);
#2302=FACE_OUTER_BOUND('',#3171,.T.);
#2303=FACE_OUTER_BOUND('',#3172,.T.);
#2304=FACE_OUTER_BOUND('',#3173,.T.);
#2305=FACE_OUTER_BOUND('',#3175,.T.);
#2306=FACE_OUTER_BOUND('',#3176,.T.);
#2307=FACE_OUTER_BOUND('',#3177,.T.);
#2308=FACE_OUTER_BOUND('',#3178,.T.);
#2309=FACE_OUTER_BOUND('',#3179,.T.);
#2310=FACE_OUTER_BOUND('',#3180,.T.);
#2311=FACE_OUTER_BOUND('',#3181,.T.);
#2312=FACE_OUTER_BOUND('',#3182,.T.);
#2313=FACE_OUTER_BOUND('',#3183,.T.);
#2314=FACE_OUTER_BOUND('',#3184,.T.);
#2315=FACE_OUTER_BOUND('',#3185,.T.);
#2316=FACE_OUTER_BOUND('',#3186,.T.);
#2317=FACE_OUTER_BOUND('',#3187,.T.);
#2318=FACE_OUTER_BOUND('',#3188,.T.);
#2319=FACE_OUTER_BOUND('',#3189,.T.);
#2320=FACE_OUTER_BOUND('',#3190,.T.);
#2321=FACE_OUTER_BOUND('',#3191,.T.);
#2322=FACE_OUTER_BOUND('',#3192,.T.);
#2323=FACE_OUTER_BOUND('',#3193,.T.);
#2324=FACE_OUTER_BOUND('',#3194,.T.);
#2325=FACE_OUTER_BOUND('',#3195,.T.);
#2326=FACE_OUTER_BOUND('',#3196,.T.);
#2327=FACE_OUTER_BOUND('',#3197,.T.);
#2328=FACE_OUTER_BOUND('',#3198,.T.);
#2329=FACE_OUTER_BOUND('',#3199,.T.);
#2330=FACE_OUTER_BOUND('',#3200,.T.);
#2331=FACE_OUTER_BOUND('',#3201,.T.);
#2332=FACE_OUTER_BOUND('',#3202,.T.);
#2333=FACE_OUTER_BOUND('',#3203,.T.);
#2334=FACE_OUTER_BOUND('',#3204,.T.);
#2335=FACE_OUTER_BOUND('',#3205,.T.);
#2336=FACE_OUTER_BOUND('',#3206,.T.);
#2337=FACE_OUTER_BOUND('',#3207,.T.);
#2338=FACE_OUTER_BOUND('',#3208,.T.);
#2339=FACE_OUTER_BOUND('',#3210,.T.);
#2340=FACE_OUTER_BOUND('',#3211,.T.);
#2341=FACE_OUTER_BOUND('',#3212,.T.);
#2342=FACE_OUTER_BOUND('',#3213,.T.);
#2343=FACE_OUTER_BOUND('',#3214,.T.);
#2344=FACE_OUTER_BOUND('',#3215,.T.);
#2345=FACE_OUTER_BOUND('',#3216,.T.);
#2346=FACE_OUTER_BOUND('',#3217,.T.);
#2347=FACE_OUTER_BOUND('',#3218,.T.);
#2348=FACE_OUTER_BOUND('',#3219,.T.);
#2349=EDGE_LOOP('',(#9782,#9783,#9784,#9785));
#2350=EDGE_LOOP('',(#9786,#9787,#9788,#9789));
#2351=EDGE_LOOP('',(#9790));
#2352=EDGE_LOOP('',(#9791));
#2353=EDGE_LOOP('',(#9792));
#2354=EDGE_LOOP('',(#9793));
#2355=EDGE_LOOP('',(#9794,#9795,#9796,#9797));
#2356=EDGE_LOOP('',(#9798,#9799,#9800,#9801));
#2357=EDGE_LOOP('',(#9802,#9803,#9804,#9805));
#2358=EDGE_LOOP('',(#9806,#9807,#9808,#9809));
#2359=EDGE_LOOP('',(#9810,#9811,#9812,#9813));
#2360=EDGE_LOOP('',(#9814,#9815,#9816,#9817));
#2361=EDGE_LOOP('',(#9818,#9819,#9820,#9821));
#2362=EDGE_LOOP('',(#9822,#9823,#9824,#9825));
#2363=EDGE_LOOP('',(#9826,#9827,#9828,#9829));
#2364=EDGE_LOOP('',(#9830));
#2365=EDGE_LOOP('',(#9831));
#2366=EDGE_LOOP('',(#9832));
#2367=EDGE_LOOP('',(#9833));
#2368=EDGE_LOOP('',(#9834,#9835,#9836,#9837));
#2369=EDGE_LOOP('',(#9838,#9839,#9840,#9841));
#2370=EDGE_LOOP('',(#9842,#9843,#9844,#9845));
#2371=EDGE_LOOP('',(#9846,#9847,#9848,#9849));
#2372=EDGE_LOOP('',(#9850,#9851,#9852,#9853));
#2373=EDGE_LOOP('',(#9854,#9855,#9856,#9857));
#2374=EDGE_LOOP('',(#9858,#9859,#9860,#9861));
#2375=EDGE_LOOP('',(#9862,#9863,#9864,#9865));
#2376=EDGE_LOOP('',(#9866,#9867,#9868,#9869));
#2377=EDGE_LOOP('',(#9870));
#2378=EDGE_LOOP('',(#9871));
#2379=EDGE_LOOP('',(#9872));
#2380=EDGE_LOOP('',(#9873));
#2381=EDGE_LOOP('',(#9874));
#2382=EDGE_LOOP('',(#9875));
#2383=EDGE_LOOP('',(#9876));
#2384=EDGE_LOOP('',(#9877));
#2385=EDGE_LOOP('',(#9878,#9879,#9880,#9881));
#2386=EDGE_LOOP('',(#9882,#9883,#9884,#9885));
#2387=EDGE_LOOP('',(#9886,#9887,#9888,#9889));
#2388=EDGE_LOOP('',(#9890,#9891,#9892,#9893));
#2389=EDGE_LOOP('',(#9894,#9895,#9896,#9897));
#2390=EDGE_LOOP('',(#9898,#9899,#9900,#9901));
#2391=EDGE_LOOP('',(#9902,#9903,#9904,#9905));
#2392=EDGE_LOOP('',(#9906,#9907,#9908,#9909));
#2393=EDGE_LOOP('',(#9910,#9911,#9912,#9913));
#2394=EDGE_LOOP('',(#9914,#9915,#9916,#9917));
#2395=EDGE_LOOP('',(#9918,#9919,#9920,#9921));
#2396=EDGE_LOOP('',(#9922,#9923,#9924,#9925));
#2397=EDGE_LOOP('',(#9926,#9927,#9928,#9929));
#2398=EDGE_LOOP('',(#9930,#9931,#9932,#9933));
#2399=EDGE_LOOP('',(#9934,#9935,#9936,#9937));
#2400=EDGE_LOOP('',(#9938,#9939,#9940));
#2401=EDGE_LOOP('',(#9941,#9942,#9943));
#2402=EDGE_LOOP('',(#9944,#9945,#9946));
#2403=EDGE_LOOP('',(#9947,#9948,#9949));
#2404=EDGE_LOOP('',(#9950,#9951,#9952));
#2405=EDGE_LOOP('',(#9953,#9954,#9955));
#2406=EDGE_LOOP('',(#9956,#9957,#9958));
#2407=EDGE_LOOP('',(#9959,#9960,#9961));
#2408=EDGE_LOOP('',(#9962,#9963,#9964,#9965,#9966));
#2409=EDGE_LOOP('',(#9967,#9968,#9969,#9970,#9971,#9972));
#2410=EDGE_LOOP('',(#9973,#9974,#9975,#9976,#9977,#9978,#9979,#9980,#9981,
#9982,#9983,#9984,#9985,#9986,#9987,#9988,#9989,#9990,#9991,#9992));
#2411=EDGE_LOOP('',(#9993,#9994,#9995,#9996));
#2412=EDGE_LOOP('',(#9997,#9998,#9999,#10000,#10001,#10002));
#2413=EDGE_LOOP('',(#10003,#10004,#10005,#10006,#10007));
#2414=EDGE_LOOP('',(#10008,#10009,#10010,#10011));
#2415=EDGE_LOOP('',(#10012,#10013,#10014,#10015,#10016));
#2416=EDGE_LOOP('',(#10017,#10018,#10019,#10020,#10021,#10022));
#2417=EDGE_LOOP('',(#10023,#10024,#10025,#10026,#10027,#10028));
#2418=EDGE_LOOP('',(#10029,#10030,#10031,#10032,#10033));
#2419=EDGE_LOOP('',(#10034,#10035,#10036,#10037,#10038,#10039,#10040,#10041,
#10042,#10043,#10044,#10045,#10046,#10047,#10048,#10049,#10050,#10051,#10052,
#10053));
#2420=EDGE_LOOP('',(#10054,#10055,#10056,#10057));
#2421=EDGE_LOOP('',(#10058,#10059,#10060,#10061));
#2422=EDGE_LOOP('',(#10062,#10063,#10064,#10065));
#2423=EDGE_LOOP('',(#10066,#10067,#10068,#10069));
#2424=EDGE_LOOP('',(#10070,#10071,#10072,#10073));
#2425=EDGE_LOOP('',(#10074,#10075,#10076,#10077));
#2426=EDGE_LOOP('',(#10078,#10079,#10080,#10081));
#2427=EDGE_LOOP('',(#10082));
#2428=EDGE_LOOP('',(#10083));
#2429=EDGE_LOOP('',(#10084));
#2430=EDGE_LOOP('',(#10085));
#2431=EDGE_LOOP('',(#10086,#10087,#10088,#10089));
#2432=EDGE_LOOP('',(#10090,#10091,#10092,#10093));
#2433=EDGE_LOOP('',(#10094,#10095,#10096,#10097));
#2434=EDGE_LOOP('',(#10098,#10099,#10100,#10101));
#2435=EDGE_LOOP('',(#10102,#10103,#10104,#10105));
#2436=EDGE_LOOP('',(#10106,#10107,#10108,#10109));
#2437=EDGE_LOOP('',(#10110,#10111,#10112,#10113));
#2438=EDGE_LOOP('',(#10114,#10115,#10116,#10117));
#2439=EDGE_LOOP('',(#10118));
#2440=EDGE_LOOP('',(#10119));
#2441=EDGE_LOOP('',(#10120));
#2442=EDGE_LOOP('',(#10121));
#2443=EDGE_LOOP('',(#10122,#10123,#10124,#10125));
#2444=EDGE_LOOP('',(#10126,#10127,#10128,#10129));
#2445=EDGE_LOOP('',(#10130,#10131,#10132,#10133,#10134,#10135));
#2446=EDGE_LOOP('',(#10136,#10137,#10138,#10139,#10140,#10141));
#2447=EDGE_LOOP('',(#10142,#10143,#10144,#10145));
#2448=EDGE_LOOP('',(#10146,#10147,#10148,#10149,#10150,#10151));
#2449=EDGE_LOOP('',(#10152,#10153,#10154,#10155,#10156,#10157));
#2450=EDGE_LOOP('',(#10158,#10159,#10160,#10161));
#2451=EDGE_LOOP('',(#10162,#10163,#10164,#10165,#10166,#10167));
#2452=EDGE_LOOP('',(#10168,#10169,#10170,#10171,#10172,#10173));
#2453=EDGE_LOOP('',(#10174,#10175,#10176,#10177));
#2454=EDGE_LOOP('',(#10178,#10179,#10180,#10181));
#2455=EDGE_LOOP('',(#10182,#10183,#10184,#10185));
#2456=EDGE_LOOP('',(#10186,#10187,#10188,#10189));
#2457=EDGE_LOOP('',(#10190,#10191,#10192,#10193));
#2458=EDGE_LOOP('',(#10194,#10195,#10196,#10197));
#2459=EDGE_LOOP('',(#10198,#10199,#10200,#10201));
#2460=EDGE_LOOP('',(#10202,#10203,#10204,#10205));
#2461=EDGE_LOOP('',(#10206));
#2462=EDGE_LOOP('',(#10207));
#2463=EDGE_LOOP('',(#10208));
#2464=EDGE_LOOP('',(#10209));
#2465=EDGE_LOOP('',(#10210));
#2466=EDGE_LOOP('',(#10211));
#2467=EDGE_LOOP('',(#10212,#10213,#10214,#10215));
#2468=EDGE_LOOP('',(#10216,#10217,#10218,#10219));
#2469=EDGE_LOOP('',(#10220,#10221,#10222,#10223));
#2470=EDGE_LOOP('',(#10224,#10225,#10226,#10227,#10228,#10229));
#2471=EDGE_LOOP('',(#10230,#10231,#10232,#10233,#10234,#10235));
#2472=EDGE_LOOP('',(#10236,#10237,#10238,#10239));
#2473=EDGE_LOOP('',(#10240,#10241,#10242,#10243,#10244,#10245));
#2474=EDGE_LOOP('',(#10246,#10247,#10248,#10249,#10250,#10251));
#2475=EDGE_LOOP('',(#10252,#10253,#10254,#10255));
#2476=EDGE_LOOP('',(#10256,#10257,#10258,#10259,#10260,#10261));
#2477=EDGE_LOOP('',(#10262,#10263,#10264,#10265,#10266,#10267));
#2478=EDGE_LOOP('',(#10268,#10269,#10270,#10271));
#2479=EDGE_LOOP('',(#10272,#10273,#10274,#10275));
#2480=EDGE_LOOP('',(#10276,#10277,#10278,#10279));
#2481=EDGE_LOOP('',(#10280,#10281,#10282,#10283));
#2482=EDGE_LOOP('',(#10284,#10285,#10286,#10287));
#2483=EDGE_LOOP('',(#10288,#10289,#10290,#10291));
#2484=EDGE_LOOP('',(#10292,#10293,#10294,#10295));
#2485=EDGE_LOOP('',(#10296,#10297,#10298,#10299));
#2486=EDGE_LOOP('',(#10300));
#2487=EDGE_LOOP('',(#10301));
#2488=EDGE_LOOP('',(#10302));
#2489=EDGE_LOOP('',(#10303));
#2490=EDGE_LOOP('',(#10304));
#2491=EDGE_LOOP('',(#10305));
#2492=EDGE_LOOP('',(#10306,#10307,#10308,#10309));
#2493=EDGE_LOOP('',(#10310,#10311,#10312,#10313));
#2494=EDGE_LOOP('',(#10314,#10315,#10316,#10317));
#2495=EDGE_LOOP('',(#10318,#10319,#10320,#10321));
#2496=EDGE_LOOP('',(#10322,#10323,#10324,#10325,#10326,#10327,#10328,#10329,
#10330,#10331,#10332,#10333,#10334,#10335));
#2497=EDGE_LOOP('',(#10336));
#2498=EDGE_LOOP('',(#10337));
#2499=EDGE_LOOP('',(#10338));
#2500=EDGE_LOOP('',(#10339));
#2501=EDGE_LOOP('',(#10340,#10341,#10342,#10343,#10344));
#2502=EDGE_LOOP('',(#10345,#10346,#10347,#10348));
#2503=EDGE_LOOP('',(#10349,#10350,#10351,#10352,#10353));
#2504=EDGE_LOOP('',(#10354,#10355,#10356,#10357));
#2505=EDGE_LOOP('',(#10358,#10359,#10360,#10361,#10362));
#2506=EDGE_LOOP('',(#10363,#10364,#10365,#10366));
#2507=EDGE_LOOP('',(#10367,#10368,#10369,#10370,#10371));
#2508=EDGE_LOOP('',(#10372,#10373,#10374,#10375));
#2509=EDGE_LOOP('',(#10376,#10377,#10378,#10379));
#2510=EDGE_LOOP('',(#10380,#10381,#10382,#10383));
#2511=EDGE_LOOP('',(#10384,#10385,#10386,#10387));
#2512=EDGE_LOOP('',(#10388,#10389,#10390,#10391));
#2513=EDGE_LOOP('',(#10392,#10393,#10394,#10395,#10396,#10397,#10398,#10399,
#10400,#10401,#10402,#10403,#10404,#10405));
#2514=EDGE_LOOP('',(#10406));
#2515=EDGE_LOOP('',(#10407));
#2516=EDGE_LOOP('',(#10408));
#2517=EDGE_LOOP('',(#10409));
#2518=EDGE_LOOP('',(#10410,#10411,#10412,#10413,#10414));
#2519=EDGE_LOOP('',(#10415,#10416,#10417,#10418));
#2520=EDGE_LOOP('',(#10419,#10420,#10421,#10422,#10423));
#2521=EDGE_LOOP('',(#10424,#10425,#10426,#10427));
#2522=EDGE_LOOP('',(#10428,#10429,#10430,#10431,#10432));
#2523=EDGE_LOOP('',(#10433,#10434,#10435,#10436));
#2524=EDGE_LOOP('',(#10437,#10438,#10439,#10440,#10441));
#2525=EDGE_LOOP('',(#10442,#10443,#10444,#10445));
#2526=EDGE_LOOP('',(#10446,#10447,#10448,#10449));
#2527=EDGE_LOOP('',(#10450,#10451,#10452,#10453));
#2528=EDGE_LOOP('',(#10454,#10455,#10456,#10457));
#2529=EDGE_LOOP('',(#10458,#10459,#10460,#10461));
#2530=EDGE_LOOP('',(#10462,#10463,#10464,#10465));
#2531=EDGE_LOOP('',(#10466));
#2532=EDGE_LOOP('',(#10467));
#2533=EDGE_LOOP('',(#10468));
#2534=EDGE_LOOP('',(#10469));
#2535=EDGE_LOOP('',(#10470));
#2536=EDGE_LOOP('',(#10471));
#2537=EDGE_LOOP('',(#10472));
#2538=EDGE_LOOP('',(#10473));
#2539=EDGE_LOOP('',(#10474));
#2540=EDGE_LOOP('',(#10475));
#2541=EDGE_LOOP('',(#10476));
#2542=EDGE_LOOP('',(#10477));
#2543=EDGE_LOOP('',(#10478));
#2544=EDGE_LOOP('',(#10479));
#2545=EDGE_LOOP('',(#10480,#10481,#10482,#10483));
#2546=EDGE_LOOP('',(#10484,#10485,#10486,#10487));
#2547=EDGE_LOOP('',(#10488,#10489,#10490,#10491));
#2548=EDGE_LOOP('',(#10492,#10493,#10494,#10495));
#2549=EDGE_LOOP('',(#10496,#10497,#10498,#10499));
#2550=EDGE_LOOP('',(#10500,#10501,#10502,#10503));
#2551=EDGE_LOOP('',(#10504,#10505,#10506,#10507));
#2552=EDGE_LOOP('',(#10508,#10509,#10510,#10511));
#2553=EDGE_LOOP('',(#10512,#10513,#10514,#10515));
#2554=EDGE_LOOP('',(#10516,#10517,#10518,#10519));
#2555=EDGE_LOOP('',(#10520,#10521,#10522,#10523));
#2556=EDGE_LOOP('',(#10524,#10525,#10526));
#2557=EDGE_LOOP('',(#10527,#10528,#10529));
#2558=EDGE_LOOP('',(#10530,#10531,#10532));
#2559=EDGE_LOOP('',(#10533,#10534,#10535));
#2560=EDGE_LOOP('',(#10536,#10537,#10538));
#2561=EDGE_LOOP('',(#10539,#10540,#10541));
#2562=EDGE_LOOP('',(#10542,#10543,#10544,#10545));
#2563=EDGE_LOOP('',(#10546,#10547,#10548,#10549));
#2564=EDGE_LOOP('',(#10550,#10551,#10552,#10553));
#2565=EDGE_LOOP('',(#10554,#10555,#10556,#10557));
#2566=EDGE_LOOP('',(#10558,#10559,#10560,#10561));
#2567=EDGE_LOOP('',(#10562,#10563,#10564,#10565));
#2568=EDGE_LOOP('',(#10566,#10567,#10568,#10569));
#2569=EDGE_LOOP('',(#10570,#10571,#10572,#10573));
#2570=EDGE_LOOP('',(#10574,#10575,#10576,#10577));
#2571=EDGE_LOOP('',(#10578,#10579,#10580,#10581));
#2572=EDGE_LOOP('',(#10582,#10583,#10584,#10585));
#2573=EDGE_LOOP('',(#10586,#10587,#10588,#10589));
#2574=EDGE_LOOP('',(#10590,#10591,#10592,#10593));
#2575=EDGE_LOOP('',(#10594,#10595,#10596,#10597));
#2576=EDGE_LOOP('',(#10598,#10599,#10600,#10601));
#2577=EDGE_LOOP('',(#10602,#10603,#10604,#10605));
#2578=EDGE_LOOP('',(#10606));
#2579=EDGE_LOOP('',(#10607));
#2580=EDGE_LOOP('',(#10608));
#2581=EDGE_LOOP('',(#10609));
#2582=EDGE_LOOP('',(#10610));
#2583=EDGE_LOOP('',(#10611));
#2584=EDGE_LOOP('',(#10612));
#2585=EDGE_LOOP('',(#10613));
#2586=EDGE_LOOP('',(#10614));
#2587=EDGE_LOOP('',(#10615));
#2588=EDGE_LOOP('',(#10616));
#2589=EDGE_LOOP('',(#10617));
#2590=EDGE_LOOP('',(#10618));
#2591=EDGE_LOOP('',(#10619));
#2592=EDGE_LOOP('',(#10620));
#2593=EDGE_LOOP('',(#10621));
#2594=EDGE_LOOP('',(#10622,#10623,#10624,#10625));
#2595=EDGE_LOOP('',(#10626,#10627,#10628,#10629));
#2596=EDGE_LOOP('',(#10630,#10631,#10632,#10633));
#2597=EDGE_LOOP('',(#10634,#10635,#10636,#10637));
#2598=EDGE_LOOP('',(#10638,#10639,#10640,#10641));
#2599=EDGE_LOOP('',(#10642,#10643,#10644,#10645));
#2600=EDGE_LOOP('',(#10646,#10647,#10648,#10649));
#2601=EDGE_LOOP('',(#10650,#10651,#10652,#10653));
#2602=EDGE_LOOP('',(#10654,#10655,#10656,#10657,#10658));
#2603=EDGE_LOOP('',(#10659,#10660,#10661,#10662,#10663,#10664));
#2604=EDGE_LOOP('',(#10665,#10666,#10667,#10668));
#2605=EDGE_LOOP('',(#10669,#10670,#10671,#10672,#10673,#10674));
#2606=EDGE_LOOP('',(#10675,#10676,#10677,#10678,#10679));
#2607=EDGE_LOOP('',(#10680,#10681,#10682,#10683,#10684));
#2608=EDGE_LOOP('',(#10685,#10686,#10687,#10688,#10689,#10690));
#2609=EDGE_LOOP('',(#10691,#10692,#10693,#10694,#10695,#10696));
#2610=EDGE_LOOP('',(#10697,#10698,#10699,#10700,#10701));
#2611=EDGE_LOOP('',(#10702,#10703,#10704,#10705));
#2612=EDGE_LOOP('',(#10706,#10707,#10708,#10709));
#2613=EDGE_LOOP('',(#10710));
#2614=EDGE_LOOP('',(#10711));
#2615=EDGE_LOOP('',(#10712));
#2616=EDGE_LOOP('',(#10713));
#2617=EDGE_LOOP('',(#10714,#10715,#10716,#10717));
#2618=EDGE_LOOP('',(#10718,#10719,#10720,#10721));
#2619=EDGE_LOOP('',(#10722));
#2620=EDGE_LOOP('',(#10723));
#2621=EDGE_LOOP('',(#10724));
#2622=EDGE_LOOP('',(#10725));
#2623=EDGE_LOOP('',(#10726));
#2624=EDGE_LOOP('',(#10727));
#2625=EDGE_LOOP('',(#10728,#10729,#10730,#10731));
#2626=EDGE_LOOP('',(#10732,#10733,#10734,#10735));
#2627=EDGE_LOOP('',(#10736));
#2628=EDGE_LOOP('',(#10737));
#2629=EDGE_LOOP('',(#10738));
#2630=EDGE_LOOP('',(#10739));
#2631=EDGE_LOOP('',(#10740,#10741,#10742,#10743));
#2632=EDGE_LOOP('',(#10744));
#2633=EDGE_LOOP('',(#10745));
#2634=EDGE_LOOP('',(#10746));
#2635=EDGE_LOOP('',(#10747));
#2636=EDGE_LOOP('',(#10748));
#2637=EDGE_LOOP('',(#10749));
#2638=EDGE_LOOP('',(#10750,#10751,#10752,#10753));
#2639=EDGE_LOOP('',(#10754,#10755,#10756,#10757));
#2640=EDGE_LOOP('',(#10758,#10759,#10760,#10761));
#2641=EDGE_LOOP('',(#10762,#10763,#10764,#10765));
#2642=EDGE_LOOP('',(#10766,#10767,#10768,#10769));
#2643=EDGE_LOOP('',(#10770,#10771,#10772,#10773));
#2644=EDGE_LOOP('',(#10774,#10775,#10776,#10777,#10778,#10779,#10780,#10781,
#10782,#10783,#10784,#10785,#10786,#10787,#10788,#10789,#10790,#10791));
#2645=EDGE_LOOP('',(#10792,#10793,#10794,#10795,#10796));
#2646=EDGE_LOOP('',(#10797,#10798,#10799,#10800));
#2647=EDGE_LOOP('',(#10801,#10802,#10803,#10804));
#2648=EDGE_LOOP('',(#10805,#10806,#10807,#10808,#10809,#10810,#10811,#10812,
#10813,#10814,#10815,#10816,#10817,#10818,#10819,#10820,#10821,#10822));
#2649=EDGE_LOOP('',(#10823,#10824,#10825,#10826,#10827));
#2650=EDGE_LOOP('',(#10828,#10829,#10830,#10831));
#2651=EDGE_LOOP('',(#10832,#10833,#10834,#10835));
#2652=EDGE_LOOP('',(#10836,#10837,#10838,#10839));
#2653=EDGE_LOOP('',(#10840));
#2654=EDGE_LOOP('',(#10841));
#2655=EDGE_LOOP('',(#10842));
#2656=EDGE_LOOP('',(#10843,#10844,#10845,#10846,#10847,#10848,#10849,#10850,
#10851,#10852,#10853,#10854,#10855,#10856,#10857,#10858));
#2657=EDGE_LOOP('',(#10859,#10860,#10861,#10862));
#2658=EDGE_LOOP('',(#10863,#10864,#10865,#10866,#10867,#10868,#10869,#10870,
#10871,#10872,#10873,#10874,#10875,#10876,#10877,#10878));
#2659=EDGE_LOOP('',(#10879,#10880,#10881,#10882));
#2660=EDGE_LOOP('',(#10883,#10884,#10885,#10886,#10887,#10888,#10889,#10890,
#10891,#10892,#10893,#10894,#10895,#10896,#10897,#10898));
#2661=EDGE_LOOP('',(#10899,#10900));
#2662=EDGE_LOOP('',(#10901,#10902));
#2663=EDGE_LOOP('',(#10903,#10904));
#2664=EDGE_LOOP('',(#10905,#10906));
#2665=EDGE_LOOP('',(#10907,#10908));
#2666=EDGE_LOOP('',(#10909,#10910));
#2667=EDGE_LOOP('',(#10911,#10912,#10913,#10914,#10915,#10916,#10917,#10918,
#10919,#10920,#10921,#10922,#10923,#10924,#10925,#10926));
#2668=EDGE_LOOP('',(#10927,#10928,#10929,#10930));
#2669=EDGE_LOOP('',(#10931,#10932,#10933,#10934));
#2670=EDGE_LOOP('',(#10935,#10936,#10937,#10938));
#2671=EDGE_LOOP('',(#10939,#10940,#10941,#10942));
#2672=EDGE_LOOP('',(#10943,#10944,#10945,#10946,#10947));
#2673=EDGE_LOOP('',(#10948,#10949,#10950,#10951,#10952));
#2674=EDGE_LOOP('',(#10953,#10954,#10955,#10956));
#2675=EDGE_LOOP('',(#10957,#10958,#10959,#10960));
#2676=EDGE_LOOP('',(#10961,#10962,#10963,#10964));
#2677=EDGE_LOOP('',(#10965,#10966,#10967,#10968));
#2678=EDGE_LOOP('',(#10969,#10970,#10971,#10972));
#2679=EDGE_LOOP('',(#10973,#10974,#10975,#10976,#10977,#10978));
#2680=EDGE_LOOP('',(#10979,#10980,#10981,#10982));
#2681=EDGE_LOOP('',(#10983,#10984,#10985,#10986,#10987,#10988));
#2682=EDGE_LOOP('',(#10989,#10990,#10991,#10992));
#2683=EDGE_LOOP('',(#10993,#10994,#10995,#10996));
#2684=EDGE_LOOP('',(#10997,#10998,#10999,#11000));
#2685=EDGE_LOOP('',(#11001,#11002,#11003,#11004));
#2686=EDGE_LOOP('',(#11005,#11006,#11007,#11008));
#2687=EDGE_LOOP('',(#11009,#11010,#11011,#11012));
#2688=EDGE_LOOP('',(#11013,#11014,#11015,#11016,#11017,#11018,#11019,#11020,
#11021,#11022,#11023,#11024,#11025,#11026,#11027,#11028));
#2689=EDGE_LOOP('',(#11029,#11030,#11031,#11032,#11033,#11034));
#2690=EDGE_LOOP('',(#11035,#11036,#11037,#11038,#11039,#11040));
#2691=EDGE_LOOP('',(#11041,#11042,#11043,#11044,#11045,#11046));
#2692=EDGE_LOOP('',(#11047,#11048,#11049,#11050));
#2693=EDGE_LOOP('',(#11051,#11052,#11053,#11054,#11055));
#2694=EDGE_LOOP('',(#11056,#11057,#11058,#11059));
#2695=EDGE_LOOP('',(#11060,#11061,#11062,#11063,#11064));
#2696=EDGE_LOOP('',(#11065,#11066,#11067,#11068,#11069,#11070,#11071,#11072,
#11073,#11074,#11075,#11076,#11077,#11078,#11079,#11080,#11081,#11082,#11083));
#2697=EDGE_LOOP('',(#11084,#11085,#11086,#11087,#11088));
#2698=EDGE_LOOP('',(#11089,#11090,#11091,#11092));
#2699=EDGE_LOOP('',(#11093,#11094,#11095,#11096,#11097));
#2700=EDGE_LOOP('',(#11098,#11099,#11100,#11101,#11102,#11103,#11104,#11105,
#11106,#11107,#11108,#11109,#11110,#11111,#11112,#11113,#11114,#11115,#11116));
#2701=EDGE_LOOP('',(#11117,#11118,#11119,#11120,#11121));
#2702=EDGE_LOOP('',(#11122,#11123,#11124,#11125));
#2703=EDGE_LOOP('',(#11126,#11127,#11128,#11129));
#2704=EDGE_LOOP('',(#11130,#11131,#11132,#11133));
#2705=EDGE_LOOP('',(#11134));
#2706=EDGE_LOOP('',(#11135));
#2707=EDGE_LOOP('',(#11136));
#2708=EDGE_LOOP('',(#11137));
#2709=EDGE_LOOP('',(#11138,#11139,#11140,#11141,#11142,#11143,#11144,#11145,
#11146,#11147,#11148,#11149,#11150,#11151,#11152,#11153));
#2710=EDGE_LOOP('',(#11154,#11155,#11156,#11157));
#2711=EDGE_LOOP('',(#11158,#11159,#11160,#11161,#11162,#11163,#11164,#11165,
#11166,#11167,#11168,#11169,#11170,#11171,#11172,#11173));
#2712=EDGE_LOOP('',(#11174,#11175,#11176,#11177));
#2713=EDGE_LOOP('',(#11178,#11179,#11180,#11181,#11182,#11183,#11184,#11185,
#11186,#11187,#11188,#11189,#11190,#11191,#11192,#11193));
#2714=EDGE_LOOP('',(#11194,#11195,#11196,#11197));
#2715=EDGE_LOOP('',(#11198,#11199,#11200,#11201,#11202,#11203,#11204,#11205,
#11206,#11207,#11208,#11209,#11210,#11211,#11212,#11213));
#2716=EDGE_LOOP('',(#11214,#11215));
#2717=EDGE_LOOP('',(#11216,#11217));
#2718=EDGE_LOOP('',(#11218,#11219));
#2719=EDGE_LOOP('',(#11220,#11221));
#2720=EDGE_LOOP('',(#11222,#11223));
#2721=EDGE_LOOP('',(#11224,#11225));
#2722=EDGE_LOOP('',(#11226,#11227));
#2723=EDGE_LOOP('',(#11228,#11229));
#2724=EDGE_LOOP('',(#11230,#11231,#11232,#11233,#11234,#11235,#11236,#11237,
#11238,#11239,#11240,#11241,#11242,#11243,#11244,#11245,#11246,#11247,#11248,
#11249));
#2725=EDGE_LOOP('',(#11250,#11251,#11252,#11253));
#2726=EDGE_LOOP('',(#11254,#11255,#11256,#11257));
#2727=EDGE_LOOP('',(#11258,#11259,#11260,#11261));
#2728=EDGE_LOOP('',(#11262,#11263,#11264,#11265));
#2729=EDGE_LOOP('',(#11266,#11267,#11268,#11269));
#2730=EDGE_LOOP('',(#11270,#11271,#11272,#11273,#11274));
#2731=EDGE_LOOP('',(#11275,#11276,#11277,#11278,#11279));
#2732=EDGE_LOOP('',(#11280,#11281,#11282,#11283,#11284));
#2733=EDGE_LOOP('',(#11285,#11286,#11287,#11288));
#2734=EDGE_LOOP('',(#11289,#11290,#11291,#11292));
#2735=EDGE_LOOP('',(#11293,#11294,#11295,#11296));
#2736=EDGE_LOOP('',(#11297,#11298,#11299,#11300));
#2737=EDGE_LOOP('',(#11301,#11302,#11303,#11304));
#2738=EDGE_LOOP('',(#11305,#11306,#11307,#11308,#11309,#11310));
#2739=EDGE_LOOP('',(#11311,#11312,#11313,#11314));
#2740=EDGE_LOOP('',(#11315,#11316,#11317,#11318,#11319,#11320));
#2741=EDGE_LOOP('',(#11321,#11322,#11323,#11324));
#2742=EDGE_LOOP('',(#11325,#11326,#11327,#11328));
#2743=EDGE_LOOP('',(#11329,#11330,#11331,#11332));
#2744=EDGE_LOOP('',(#11333,#11334,#11335,#11336));
#2745=EDGE_LOOP('',(#11337,#11338,#11339,#11340));
#2746=EDGE_LOOP('',(#11341,#11342,#11343,#11344,#11345,#11346,#11347,#11348,
#11349,#11350,#11351,#11352,#11353,#11354,#11355,#11356,#11357,#11358,#11359,
#11360));
#2747=EDGE_LOOP('',(#11361,#11362,#11363,#11364));
#2748=EDGE_LOOP('',(#11365,#11366,#11367,#11368,#11369,#11370));
#2749=EDGE_LOOP('',(#11371,#11372,#11373,#11374,#11375,#11376));
#2750=EDGE_LOOP('',(#11377,#11378,#11379,#11380,#11381,#11382));
#2751=EDGE_LOOP('',(#11383,#11384,#11385,#11386));
#2752=EDGE_LOOP('',(#11387,#11388,#11389,#11390));
#2753=EDGE_LOOP('',(#11391,#11392,#11393,#11394,#11395));
#2754=EDGE_LOOP('',(#11396,#11397,#11398,#11399));
#2755=EDGE_LOOP('',(#11400,#11401,#11402,#11403));
#2756=EDGE_LOOP('',(#11404,#11405,#11406,#11407));
#2757=EDGE_LOOP('',(#11408,#11409,#11410,#11411));
#2758=EDGE_LOOP('',(#11412,#11413,#11414,#11415));
#2759=EDGE_LOOP('',(#11416,#11417,#11418,#11419));
#2760=EDGE_LOOP('',(#11420,#11421,#11422,#11423));
#2761=EDGE_LOOP('',(#11424,#11425,#11426,#11427));
#2762=EDGE_LOOP('',(#11428,#11429,#11430,#11431));
#2763=EDGE_LOOP('',(#11432,#11433,#11434,#11435));
#2764=EDGE_LOOP('',(#11436,#11437,#11438,#11439));
#2765=EDGE_LOOP('',(#11440,#11441,#11442,#11443));
#2766=EDGE_LOOP('',(#11444,#11445,#11446,#11447));
#2767=EDGE_LOOP('',(#11448,#11449,#11450,#11451));
#2768=EDGE_LOOP('',(#11452,#11453,#11454,#11455));
#2769=EDGE_LOOP('',(#11456,#11457,#11458,#11459));
#2770=EDGE_LOOP('',(#11460,#11461,#11462,#11463));
#2771=EDGE_LOOP('',(#11464,#11465,#11466,#11467));
#2772=EDGE_LOOP('',(#11468,#11469,#11470,#11471));
#2773=EDGE_LOOP('',(#11472,#11473,#11474,#11475));
#2774=EDGE_LOOP('',(#11476,#11477,#11478,#11479));
#2775=EDGE_LOOP('',(#11480,#11481,#11482,#11483));
#2776=EDGE_LOOP('',(#11484,#11485,#11486,#11487));
#2777=EDGE_LOOP('',(#11488,#11489,#11490,#11491));
#2778=EDGE_LOOP('',(#11492,#11493,#11494,#11495));
#2779=EDGE_LOOP('',(#11496,#11497,#11498,#11499));
#2780=EDGE_LOOP('',(#11500,#11501,#11502,#11503));
#2781=EDGE_LOOP('',(#11504,#11505,#11506,#11507));
#2782=EDGE_LOOP('',(#11508,#11509,#11510,#11511));
#2783=EDGE_LOOP('',(#11512,#11513,#11514,#11515));
#2784=EDGE_LOOP('',(#11516,#11517,#11518,#11519));
#2785=EDGE_LOOP('',(#11520,#11521,#11522,#11523));
#2786=EDGE_LOOP('',(#11524,#11525,#11526,#11527));
#2787=EDGE_LOOP('',(#11528,#11529,#11530,#11531));
#2788=EDGE_LOOP('',(#11532,#11533,#11534,#11535));
#2789=EDGE_LOOP('',(#11536,#11537,#11538,#11539));
#2790=EDGE_LOOP('',(#11540,#11541,#11542,#11543));
#2791=EDGE_LOOP('',(#11544,#11545,#11546,#11547));
#2792=EDGE_LOOP('',(#11548,#11549,#11550,#11551));
#2793=EDGE_LOOP('',(#11552,#11553,#11554,#11555));
#2794=EDGE_LOOP('',(#11556,#11557,#11558,#11559));
#2795=EDGE_LOOP('',(#11560,#11561,#11562,#11563));
#2796=EDGE_LOOP('',(#11564,#11565,#11566,#11567));
#2797=EDGE_LOOP('',(#11568,#11569,#11570,#11571));
#2798=EDGE_LOOP('',(#11572,#11573,#11574,#11575));
#2799=EDGE_LOOP('',(#11576,#11577,#11578,#11579));
#2800=EDGE_LOOP('',(#11580,#11581,#11582,#11583));
#2801=EDGE_LOOP('',(#11584,#11585,#11586,#11587));
#2802=EDGE_LOOP('',(#11588,#11589,#11590,#11591));
#2803=EDGE_LOOP('',(#11592,#11593,#11594,#11595));
#2804=EDGE_LOOP('',(#11596,#11597,#11598,#11599));
#2805=EDGE_LOOP('',(#11600,#11601,#11602,#11603));
#2806=EDGE_LOOP('',(#11604,#11605,#11606,#11607));
#2807=EDGE_LOOP('',(#11608,#11609,#11610,#11611));
#2808=EDGE_LOOP('',(#11612,#11613,#11614,#11615));
#2809=EDGE_LOOP('',(#11616,#11617,#11618,#11619));
#2810=EDGE_LOOP('',(#11620,#11621,#11622,#11623));
#2811=EDGE_LOOP('',(#11624,#11625,#11626,#11627));
#2812=EDGE_LOOP('',(#11628,#11629,#11630,#11631));
#2813=EDGE_LOOP('',(#11632,#11633,#11634,#11635));
#2814=EDGE_LOOP('',(#11636,#11637,#11638,#11639));
#2815=EDGE_LOOP('',(#11640,#11641,#11642,#11643));
#2816=EDGE_LOOP('',(#11644,#11645,#11646,#11647));
#2817=EDGE_LOOP('',(#11648,#11649,#11650,#11651));
#2818=EDGE_LOOP('',(#11652,#11653,#11654,#11655));
#2819=EDGE_LOOP('',(#11656,#11657,#11658,#11659));
#2820=EDGE_LOOP('',(#11660,#11661,#11662,#11663));
#2821=EDGE_LOOP('',(#11664,#11665,#11666,#11667));
#2822=EDGE_LOOP('',(#11668,#11669,#11670,#11671));
#2823=EDGE_LOOP('',(#11672,#11673,#11674,#11675));
#2824=EDGE_LOOP('',(#11676,#11677,#11678,#11679));
#2825=EDGE_LOOP('',(#11680,#11681,#11682,#11683));
#2826=EDGE_LOOP('',(#11684,#11685,#11686,#11687));
#2827=EDGE_LOOP('',(#11688,#11689,#11690,#11691));
#2828=EDGE_LOOP('',(#11692,#11693,#11694,#11695));
#2829=EDGE_LOOP('',(#11696,#11697,#11698,#11699));
#2830=EDGE_LOOP('',(#11700,#11701,#11702,#11703));
#2831=EDGE_LOOP('',(#11704,#11705,#11706,#11707));
#2832=EDGE_LOOP('',(#11708,#11709,#11710,#11711));
#2833=EDGE_LOOP('',(#11712,#11713,#11714,#11715));
#2834=EDGE_LOOP('',(#11716,#11717,#11718,#11719));
#2835=EDGE_LOOP('',(#11720,#11721,#11722,#11723));
#2836=EDGE_LOOP('',(#11724,#11725,#11726,#11727));
#2837=EDGE_LOOP('',(#11728,#11729,#11730,#11731));
#2838=EDGE_LOOP('',(#11732,#11733,#11734,#11735));
#2839=EDGE_LOOP('',(#11736,#11737,#11738,#11739));
#2840=EDGE_LOOP('',(#11740,#11741,#11742,#11743));
#2841=EDGE_LOOP('',(#11744,#11745,#11746,#11747));
#2842=EDGE_LOOP('',(#11748,#11749,#11750,#11751));
#2843=EDGE_LOOP('',(#11752,#11753,#11754,#11755));
#2844=EDGE_LOOP('',(#11756,#11757,#11758,#11759));
#2845=EDGE_LOOP('',(#11760,#11761,#11762,#11763));
#2846=EDGE_LOOP('',(#11764,#11765,#11766,#11767));
#2847=EDGE_LOOP('',(#11768,#11769,#11770,#11771));
#2848=EDGE_LOOP('',(#11772,#11773,#11774,#11775));
#2849=EDGE_LOOP('',(#11776,#11777,#11778,#11779));
#2850=EDGE_LOOP('',(#11780,#11781,#11782,#11783));
#2851=EDGE_LOOP('',(#11784,#11785,#11786,#11787));
#2852=EDGE_LOOP('',(#11788,#11789,#11790,#11791));
#2853=EDGE_LOOP('',(#11792,#11793,#11794,#11795));
#2854=EDGE_LOOP('',(#11796,#11797,#11798,#11799));
#2855=EDGE_LOOP('',(#11800,#11801,#11802,#11803));
#2856=EDGE_LOOP('',(#11804,#11805,#11806,#11807));
#2857=EDGE_LOOP('',(#11808,#11809,#11810,#11811));
#2858=EDGE_LOOP('',(#11812,#11813,#11814,#11815));
#2859=EDGE_LOOP('',(#11816,#11817,#11818,#11819));
#2860=EDGE_LOOP('',(#11820,#11821,#11822,#11823));
#2861=EDGE_LOOP('',(#11824,#11825,#11826,#11827));
#2862=EDGE_LOOP('',(#11828,#11829,#11830,#11831));
#2863=EDGE_LOOP('',(#11832,#11833,#11834,#11835));
#2864=EDGE_LOOP('',(#11836,#11837,#11838,#11839));
#2865=EDGE_LOOP('',(#11840,#11841,#11842,#11843));
#2866=EDGE_LOOP('',(#11844,#11845,#11846,#11847));
#2867=EDGE_LOOP('',(#11848,#11849,#11850,#11851));
#2868=EDGE_LOOP('',(#11852,#11853,#11854,#11855));
#2869=EDGE_LOOP('',(#11856,#11857,#11858,#11859));
#2870=EDGE_LOOP('',(#11860,#11861,#11862,#11863));
#2871=EDGE_LOOP('',(#11864,#11865,#11866,#11867));
#2872=EDGE_LOOP('',(#11868,#11869,#11870,#11871));
#2873=EDGE_LOOP('',(#11872,#11873,#11874,#11875));
#2874=EDGE_LOOP('',(#11876,#11877,#11878,#11879));
#2875=EDGE_LOOP('',(#11880,#11881,#11882,#11883));
#2876=EDGE_LOOP('',(#11884,#11885,#11886,#11887));
#2877=EDGE_LOOP('',(#11888,#11889,#11890,#11891));
#2878=EDGE_LOOP('',(#11892,#11893,#11894,#11895));
#2879=EDGE_LOOP('',(#11896,#11897,#11898,#11899));
#2880=EDGE_LOOP('',(#11900,#11901,#11902,#11903));
#2881=EDGE_LOOP('',(#11904,#11905,#11906,#11907));
#2882=EDGE_LOOP('',(#11908,#11909,#11910,#11911));
#2883=EDGE_LOOP('',(#11912,#11913,#11914,#11915,#11916,#11917,#11918,#11919));
#2884=EDGE_LOOP('',(#11920,#11921,#11922,#11923,#11924,#11925,#11926,#11927));
#2885=EDGE_LOOP('',(#11928,#11929,#11930,#11931,#11932,#11933,#11934,#11935));
#2886=EDGE_LOOP('',(#11936,#11937,#11938,#11939,#11940,#11941,#11942,#11943));
#2887=EDGE_LOOP('',(#11944,#11945,#11946,#11947,#11948,#11949,#11950,#11951));
#2888=EDGE_LOOP('',(#11952,#11953,#11954,#11955,#11956,#11957,#11958,#11959));
#2889=EDGE_LOOP('',(#11960,#11961,#11962,#11963,#11964,#11965,#11966,#11967));
#2890=EDGE_LOOP('',(#11968,#11969,#11970,#11971,#11972,#11973,#11974,#11975));
#2891=EDGE_LOOP('',(#11976,#11977,#11978,#11979,#11980,#11981,#11982,#11983));
#2892=EDGE_LOOP('',(#11984,#11985,#11986,#11987,#11988,#11989,#11990,#11991));
#2893=EDGE_LOOP('',(#11992,#11993,#11994,#11995,#11996,#11997,#11998,#11999));
#2894=EDGE_LOOP('',(#12000,#12001,#12002,#12003,#12004,#12005,#12006,#12007));
#2895=EDGE_LOOP('',(#12008,#12009,#12010,#12011,#12012,#12013,#12014,#12015));
#2896=EDGE_LOOP('',(#12016,#12017,#12018,#12019,#12020,#12021,#12022,#12023));
#2897=EDGE_LOOP('',(#12024,#12025,#12026,#12027,#12028,#12029,#12030,#12031));
#2898=EDGE_LOOP('',(#12032,#12033,#12034,#12035,#12036,#12037,#12038,#12039));
#2899=EDGE_LOOP('',(#12040,#12041,#12042,#12043,#12044,#12045,#12046,#12047));
#2900=EDGE_LOOP('',(#12048,#12049,#12050,#12051,#12052,#12053,#12054,#12055));
#2901=EDGE_LOOP('',(#12056,#12057,#12058,#12059,#12060,#12061,#12062,#12063));
#2902=EDGE_LOOP('',(#12064,#12065,#12066,#12067,#12068,#12069,#12070,#12071));
#2903=EDGE_LOOP('',(#12072,#12073,#12074,#12075,#12076,#12077,#12078,#12079));
#2904=EDGE_LOOP('',(#12080,#12081,#12082,#12083,#12084,#12085,#12086,#12087));
#2905=EDGE_LOOP('',(#12088,#12089,#12090,#12091,#12092,#12093,#12094,#12095));
#2906=EDGE_LOOP('',(#12096,#12097,#12098,#12099,#12100,#12101,#12102,#12103));
#2907=EDGE_LOOP('',(#12104,#12105,#12106,#12107,#12108,#12109,#12110,#12111));
#2908=EDGE_LOOP('',(#12112,#12113,#12114,#12115,#12116,#12117,#12118,#12119));
#2909=EDGE_LOOP('',(#12120,#12121,#12122,#12123,#12124,#12125,#12126,#12127));
#2910=EDGE_LOOP('',(#12128,#12129,#12130,#12131,#12132,#12133,#12134,#12135));
#2911=EDGE_LOOP('',(#12136,#12137,#12138,#12139,#12140,#12141,#12142,#12143));
#2912=EDGE_LOOP('',(#12144,#12145,#12146,#12147,#12148,#12149,#12150,#12151));
#2913=EDGE_LOOP('',(#12152,#12153,#12154,#12155,#12156,#12157,#12158,#12159));
#2914=EDGE_LOOP('',(#12160,#12161,#12162,#12163,#12164,#12165,#12166,#12167));
#2915=EDGE_LOOP('',(#12168));
#2916=EDGE_LOOP('',(#12169,#12170,#12171,#12172));
#2917=EDGE_LOOP('',(#12173,#12174,#12175,#12176));
#2918=EDGE_LOOP('',(#12177,#12178,#12179,#12180));
#2919=EDGE_LOOP('',(#12181));
#2920=EDGE_LOOP('',(#12182,#12183,#12184,#12185));
#2921=EDGE_LOOP('',(#12186,#12187,#12188,#12189,#12190));
#2922=EDGE_LOOP('',(#12191,#12192,#12193,#12194,#12195));
#2923=EDGE_LOOP('',(#12196,#12197,#12198,#12199,#12200));
#2924=EDGE_LOOP('',(#12201,#12202,#12203,#12204,#12205));
#2925=EDGE_LOOP('',(#12206,#12207,#12208,#12209,#12210));
#2926=EDGE_LOOP('',(#12211,#12212,#12213,#12214,#12215));
#2927=EDGE_LOOP('',(#12216,#12217,#12218,#12219,#12220,#12221));
#2928=EDGE_LOOP('',(#12222,#12223,#12224,#12225));
#2929=EDGE_LOOP('',(#12226,#12227,#12228,#12229,#12230,#12231));
#2930=EDGE_LOOP('',(#12232,#12233,#12234,#12235,#12236,#12237));
#2931=EDGE_LOOP('',(#12238,#12239,#12240,#12241,#12242));
#2932=EDGE_LOOP('',(#12243,#12244,#12245,#12246,#12247));
#2933=EDGE_LOOP('',(#12248,#12249,#12250,#12251,#12252));
#2934=EDGE_LOOP('',(#12253,#12254,#12255,#12256,#12257));
#2935=EDGE_LOOP('',(#12258,#12259,#12260,#12261,#12262));
#2936=EDGE_LOOP('',(#12263,#12264,#12265,#12266,#12267));
#2937=EDGE_LOOP('',(#12268,#12269,#12270,#12271,#12272));
#2938=EDGE_LOOP('',(#12273,#12274,#12275,#12276,#12277));
#2939=EDGE_LOOP('',(#12278,#12279,#12280,#12281,#12282));
#2940=EDGE_LOOP('',(#12283,#12284,#12285,#12286,#12287));
#2941=EDGE_LOOP('',(#12288,#12289,#12290,#12291,#12292));
#2942=EDGE_LOOP('',(#12293,#12294,#12295,#12296,#12297));
#2943=EDGE_LOOP('',(#12298,#12299,#12300,#12301,#12302,#12303));
#2944=EDGE_LOOP('',(#12304,#12305,#12306,#12307,#12308,#12309,#12310,#12311,
#12312,#12313,#12314,#12315,#12316,#12317,#12318,#12319,#12320,#12321,#12322,
#12323,#12324,#12325,#12326,#12327,#12328,#12329,#12330,#12331,#12332,#12333,
#12334,#12335,#12336,#12337,#12338,#12339,#12340,#12341,#12342,#12343,#12344,
#12345,#12346,#12347,#12348,#12349,#12350,#12351,#12352,#12353,#12354,#12355));
#2945=EDGE_LOOP('',(#12356,#12357,#12358,#12359,#12360,#12361));
#2946=EDGE_LOOP('',(#12362,#12363,#12364,#12365,#12366));
#2947=EDGE_LOOP('',(#12367,#12368,#12369,#12370,#12371,#12372,#12373,#12374,
#12375,#12376,#12377,#12378,#12379,#12380,#12381,#12382,#12383,#12384,#12385,
#12386,#12387,#12388,#12389,#12390,#12391,#12392,#12393,#12394,#12395,#12396,
#12397,#12398,#12399,#12400,#12401,#12402,#12403,#12404,#12405,#12406,#12407,
#12408,#12409,#12410,#12411,#12412,#12413,#12414,#12415,#12416,#12417,#12418,
#12419,#12420,#12421,#12422,#12423,#12424,#12425,#12426,#12427,#12428,#12429,
#12430,#12431,#12432,#12433,#12434));
#2948=EDGE_LOOP('',(#12435,#12436,#12437,#12438,#12439,#12440));
#2949=EDGE_LOOP('',(#12441,#12442,#12443,#12444,#12445,#12446,#12447,#12448,
#12449,#12450,#12451,#12452,#12453,#12454,#12455,#12456,#12457,#12458,#12459,
#12460,#12461,#12462,#12463,#12464,#12465,#12466,#12467,#12468,#12469,#12470,
#12471,#12472,#12473,#12474,#12475,#12476,#12477,#12478,#12479,#12480,#12481,
#12482,#12483,#12484,#12485,#12486,#12487,#12488,#12489,#12490,#12491,#12492,
#12493,#12494,#12495,#12496,#12497,#12498,#12499,#12500,#12501,#12502,#12503,
#12504,#12505,#12506,#12507));
#2950=EDGE_LOOP('',(#12508,#12509,#12510,#12511,#12512,#12513,#12514));
#2951=EDGE_LOOP('',(#12515));
#2952=EDGE_LOOP('',(#12516));
#2953=EDGE_LOOP('',(#12517,#12518,#12519,#12520,#12521,#12522,#12523));
#2954=EDGE_LOOP('',(#12524));
#2955=EDGE_LOOP('',(#12525,#12526,#12527));
#2956=EDGE_LOOP('',(#12528,#12529,#12530,#12531));
#2957=EDGE_LOOP('',(#12532,#12533,#12534,#12535));
#2958=EDGE_LOOP('',(#12536,#12537,#12538,#12539,#12540,#12541,#12542,#12543,
#12544,#12545,#12546,#12547,#12548,#12549,#12550,#12551,#12552,#12553,#12554,
#12555,#12556,#12557,#12558,#12559,#12560,#12561,#12562,#12563,#12564,#12565,
#12566,#12567,#12568,#12569,#12570,#12571,#12572,#12573,#12574,#12575,#12576,
#12577,#12578,#12579,#12580,#12581,#12582,#12583,#12584,#12585,#12586,#12587,
#12588,#12589,#12590,#12591,#12592,#12593,#12594,#12595,#12596,#12597,#12598,
#12599,#12600,#12601,#12602,#12603,#12604,#12605,#12606,#12607,#12608,#12609,
#12610,#12611,#12612,#12613,#12614,#12615,#12616,#12617,#12618,#12619,#12620,
#12621,#12622,#12623,#12624,#12625,#12626,#12627,#12628,#12629,#12630,#12631,
#12632,#12633,#12634,#12635,#12636,#12637,#12638,#12639,#12640,#12641,#12642,
#12643,#12644,#12645,#12646,#12647,#12648,#12649,#12650,#12651,#12652,#12653,
#12654,#12655,#12656,#12657,#12658,#12659,#12660,#12661,#12662,#12663,#12664,
#12665,#12666,#12667,#12668,#12669,#12670,#12671,#12672,#12673,#12674,#12675,
#12676,#12677,#12678,#12679,#12680,#12681,#12682,#12683));
#2959=EDGE_LOOP('',(#12684,#12685,#12686,#12687));
#2960=EDGE_LOOP('',(#12688,#12689,#12690,#12691));
#2961=EDGE_LOOP('',(#12692,#12693,#12694));
#2962=EDGE_LOOP('',(#12695,#12696,#12697,#12698,#12699,#12700,#12701,#12702,
#12703,#12704,#12705,#12706,#12707,#12708,#12709,#12710,#12711,#12712,#12713,
#12714,#12715,#12716,#12717,#12718,#12719,#12720,#12721,#12722,#12723,#12724,
#12725,#12726,#12727,#12728,#12729,#12730,#12731,#12732,#12733,#12734,#12735,
#12736,#12737,#12738,#12739,#12740,#12741,#12742,#12743,#12744,#12745,#12746,
#12747,#12748,#12749,#12750,#12751,#12752,#12753,#12754,#12755,#12756,#12757,
#12758,#12759,#12760,#12761,#12762,#12763,#12764,#12765,#12766,#12767,#12768,
#12769,#12770,#12771,#12772,#12773,#12774,#12775,#12776,#12777,#12778,#12779,
#12780,#12781,#12782,#12783,#12784,#12785,#12786,#12787,#12788,#12789,#12790,
#12791,#12792,#12793,#12794,#12795,#12796,#12797,#12798,#12799,#12800,#12801,
#12802,#12803,#12804,#12805));
#2963=EDGE_LOOP('',(#12806,#12807,#12808));
#2964=EDGE_LOOP('',(#12809,#12810,#12811,#12812));
#2965=EDGE_LOOP('',(#12813,#12814,#12815,#12816));
#2966=EDGE_LOOP('',(#12817,#12818,#12819,#12820));
#2967=EDGE_LOOP('',(#12821,#12822,#12823,#12824));
#2968=EDGE_LOOP('',(#12825,#12826,#12827));
#2969=EDGE_LOOP('',(#12828,#12829,#12830));
#2970=EDGE_LOOP('',(#12831,#12832,#12833,#12834));
#2971=EDGE_LOOP('',(#12835,#12836,#12837,#12838));
#2972=EDGE_LOOP('',(#12839,#12840,#12841,#12842));
#2973=EDGE_LOOP('',(#12843,#12844,#12845,#12846));
#2974=EDGE_LOOP('',(#12847,#12848,#12849));
#2975=EDGE_LOOP('',(#12850,#12851,#12852));
#2976=EDGE_LOOP('',(#12853,#12854,#12855,#12856));
#2977=EDGE_LOOP('',(#12857,#12858,#12859,#12860));
#2978=EDGE_LOOP('',(#12861,#12862,#12863,#12864));
#2979=EDGE_LOOP('',(#12865,#12866,#12867,#12868));
#2980=EDGE_LOOP('',(#12869,#12870,#12871));
#2981=EDGE_LOOP('',(#12872,#12873,#12874));
#2982=EDGE_LOOP('',(#12875,#12876,#12877,#12878));
#2983=EDGE_LOOP('',(#12879,#12880,#12881,#12882));
#2984=EDGE_LOOP('',(#12883,#12884,#12885,#12886));
#2985=EDGE_LOOP('',(#12887,#12888,#12889,#12890));
#2986=EDGE_LOOP('',(#12891,#12892,#12893));
#2987=EDGE_LOOP('',(#12894,#12895,#12896));
#2988=EDGE_LOOP('',(#12897,#12898,#12899,#12900));
#2989=EDGE_LOOP('',(#12901,#12902,#12903,#12904));
#2990=EDGE_LOOP('',(#12905,#12906,#12907,#12908));
#2991=EDGE_LOOP('',(#12909,#12910,#12911,#12912));
#2992=EDGE_LOOP('',(#12913,#12914,#12915));
#2993=EDGE_LOOP('',(#12916,#12917,#12918));
#2994=EDGE_LOOP('',(#12919,#12920,#12921,#12922));
#2995=EDGE_LOOP('',(#12923,#12924,#12925,#12926));
#2996=EDGE_LOOP('',(#12927,#12928,#12929,#12930));
#2997=EDGE_LOOP('',(#12931,#12932,#12933,#12934));
#2998=EDGE_LOOP('',(#12935,#12936,#12937));
#2999=EDGE_LOOP('',(#12938,#12939,#12940));
#3000=EDGE_LOOP('',(#12941,#12942,#12943,#12944));
#3001=EDGE_LOOP('',(#12945,#12946,#12947,#12948));
#3002=EDGE_LOOP('',(#12949,#12950,#12951,#12952));
#3003=EDGE_LOOP('',(#12953,#12954,#12955,#12956));
#3004=EDGE_LOOP('',(#12957,#12958,#12959));
#3005=EDGE_LOOP('',(#12960,#12961,#12962));
#3006=EDGE_LOOP('',(#12963,#12964,#12965,#12966));
#3007=EDGE_LOOP('',(#12967,#12968,#12969,#12970));
#3008=EDGE_LOOP('',(#12971,#12972,#12973,#12974));
#3009=EDGE_LOOP('',(#12975,#12976,#12977,#12978));
#3010=EDGE_LOOP('',(#12979,#12980,#12981,#12982));
#3011=EDGE_LOOP('',(#12983,#12984,#12985));
#3012=EDGE_LOOP('',(#12986,#12987,#12988,#12989));
#3013=EDGE_LOOP('',(#12990,#12991,#12992,#12993));
#3014=EDGE_LOOP('',(#12994,#12995,#12996,#12997));
#3015=EDGE_LOOP('',(#12998,#12999,#13000,#13001));
#3016=EDGE_LOOP('',(#13002,#13003,#13004));
#3017=EDGE_LOOP('',(#13005,#13006,#13007));
#3018=EDGE_LOOP('',(#13008,#13009,#13010,#13011));
#3019=EDGE_LOOP('',(#13012,#13013,#13014,#13015));
#3020=EDGE_LOOP('',(#13016,#13017,#13018,#13019));
#3021=EDGE_LOOP('',(#13020,#13021,#13022,#13023));
#3022=EDGE_LOOP('',(#13024,#13025,#13026));
#3023=EDGE_LOOP('',(#13027,#13028,#13029));
#3024=EDGE_LOOP('',(#13030,#13031,#13032,#13033));
#3025=EDGE_LOOP('',(#13034,#13035,#13036,#13037));
#3026=EDGE_LOOP('',(#13038,#13039,#13040,#13041));
#3027=EDGE_LOOP('',(#13042,#13043,#13044,#13045));
#3028=EDGE_LOOP('',(#13046,#13047,#13048));
#3029=EDGE_LOOP('',(#13049,#13050,#13051));
#3030=EDGE_LOOP('',(#13052,#13053,#13054,#13055));
#3031=EDGE_LOOP('',(#13056,#13057,#13058,#13059));
#3032=EDGE_LOOP('',(#13060,#13061,#13062,#13063));
#3033=EDGE_LOOP('',(#13064,#13065,#13066,#13067));
#3034=EDGE_LOOP('',(#13068,#13069,#13070));
#3035=EDGE_LOOP('',(#13071,#13072,#13073));
#3036=EDGE_LOOP('',(#13074,#13075,#13076,#13077));
#3037=EDGE_LOOP('',(#13078,#13079,#13080,#13081));
#3038=EDGE_LOOP('',(#13082,#13083,#13084,#13085));
#3039=EDGE_LOOP('',(#13086,#13087,#13088,#13089));
#3040=EDGE_LOOP('',(#13090,#13091,#13092));
#3041=EDGE_LOOP('',(#13093,#13094,#13095));
#3042=EDGE_LOOP('',(#13096,#13097,#13098,#13099));
#3043=EDGE_LOOP('',(#13100,#13101,#13102,#13103));
#3044=EDGE_LOOP('',(#13104,#13105,#13106,#13107));
#3045=EDGE_LOOP('',(#13108,#13109,#13110,#13111));
#3046=EDGE_LOOP('',(#13112,#13113,#13114));
#3047=EDGE_LOOP('',(#13115,#13116,#13117));
#3048=EDGE_LOOP('',(#13118,#13119,#13120,#13121));
#3049=EDGE_LOOP('',(#13122,#13123,#13124,#13125));
#3050=EDGE_LOOP('',(#13126,#13127,#13128,#13129));
#3051=EDGE_LOOP('',(#13130,#13131,#13132,#13133));
#3052=EDGE_LOOP('',(#13134,#13135,#13136));
#3053=EDGE_LOOP('',(#13137,#13138,#13139));
#3054=EDGE_LOOP('',(#13140,#13141,#13142,#13143));
#3055=EDGE_LOOP('',(#13144,#13145,#13146,#13147));
#3056=EDGE_LOOP('',(#13148,#13149,#13150,#13151));
#3057=EDGE_LOOP('',(#13152,#13153,#13154,#13155));
#3058=EDGE_LOOP('',(#13156,#13157,#13158));
#3059=EDGE_LOOP('',(#13159,#13160,#13161));
#3060=EDGE_LOOP('',(#13162,#13163,#13164,#13165));
#3061=EDGE_LOOP('',(#13166,#13167,#13168,#13169));
#3062=EDGE_LOOP('',(#13170,#13171,#13172,#13173));
#3063=EDGE_LOOP('',(#13174,#13175,#13176,#13177));
#3064=EDGE_LOOP('',(#13178,#13179,#13180));
#3065=EDGE_LOOP('',(#13181,#13182,#13183,#13184));
#3066=EDGE_LOOP('',(#13185));
#3067=EDGE_LOOP('',(#13186));
#3068=EDGE_LOOP('',(#13187,#13188,#13189,#13190,#13191,#13192,#13193,#13194,
#13195,#13196,#13197,#13198,#13199,#13200,#13201,#13202,#13203,#13204,#13205,
#13206,#13207));
#3069=EDGE_LOOP('',(#13208,#13209,#13210,#13211));
#3070=EDGE_LOOP('',(#13212,#13213,#13214,#13215));
#3071=EDGE_LOOP('',(#13216,#13217,#13218,#13219));
#3072=EDGE_LOOP('',(#13220,#13221,#13222,#13223));
#3073=EDGE_LOOP('',(#13224,#13225,#13226,#13227));
#3074=EDGE_LOOP('',(#13228,#13229,#13230,#13231));
#3075=EDGE_LOOP('',(#13232,#13233,#13234,#13235,#13236,#13237,#13238,#13239));
#3076=EDGE_LOOP('',(#13240,#13241,#13242,#13243,#13244,#13245,#13246,#13247));
#3077=EDGE_LOOP('',(#13248,#13249,#13250,#13251,#13252,#13253,#13254,#13255));
#3078=EDGE_LOOP('',(#13256,#13257));
#3079=EDGE_LOOP('',(#13258,#13259));
#3080=EDGE_LOOP('',(#13260,#13261));
#3081=EDGE_LOOP('',(#13262,#13263));
#3082=EDGE_LOOP('',(#13264,#13265));
#3083=EDGE_LOOP('',(#13266,#13267));
#3084=EDGE_LOOP('',(#13268,#13269));
#3085=EDGE_LOOP('',(#13270,#13271));
#3086=EDGE_LOOP('',(#13272,#13273));
#3087=EDGE_LOOP('',(#13274,#13275));
#3088=EDGE_LOOP('',(#13276,#13277));
#3089=EDGE_LOOP('',(#13278,#13279));
#3090=EDGE_LOOP('',(#13280,#13281,#13282,#13283,#13284,#13285,#13286,#13287));
#3091=EDGE_LOOP('',(#13288,#13289,#13290,#13291,#13292,#13293,#13294,#13295));
#3092=EDGE_LOOP('',(#13296,#13297,#13298,#13299,#13300,#13301,#13302,#13303));
#3093=EDGE_LOOP('',(#13304,#13305,#13306,#13307,#13308,#13309,#13310,#13311));
#3094=EDGE_LOOP('',(#13312,#13313,#13314,#13315));
#3095=EDGE_LOOP('',(#13316,#13317,#13318,#13319,#13320));
#3096=EDGE_LOOP('',(#13321,#13322,#13323,#13324));
#3097=EDGE_LOOP('',(#13325,#13326,#13327,#13328,#13329));
#3098=EDGE_LOOP('',(#13330,#13331,#13332,#13333,#13334,#13335));
#3099=EDGE_LOOP('',(#13336,#13337,#13338,#13339));
#3100=EDGE_LOOP('',(#13340,#13341,#13342,#13343,#13344,#13345));
#3101=EDGE_LOOP('',(#13346,#13347,#13348,#13349));
#3102=EDGE_LOOP('',(#13350,#13351,#13352,#13353,#13354,#13355));
#3103=EDGE_LOOP('',(#13356,#13357,#13358,#13359));
#3104=EDGE_LOOP('',(#13360,#13361,#13362,#13363,#13364,#13365));
#3105=EDGE_LOOP('',(#13366,#13367,#13368,#13369,#13370));
#3106=EDGE_LOOP('',(#13371,#13372,#13373,#13374,#13375));
#3107=EDGE_LOOP('',(#13376,#13377,#13378,#13379,#13380));
#3108=EDGE_LOOP('',(#13381,#13382,#13383,#13384,#13385));
#3109=EDGE_LOOP('',(#13386,#13387,#13388,#13389,#13390));
#3110=EDGE_LOOP('',(#13391,#13392,#13393,#13394,#13395));
#3111=EDGE_LOOP('',(#13396,#13397,#13398,#13399,#13400));
#3112=EDGE_LOOP('',(#13401,#13402,#13403,#13404,#13405));
#3113=EDGE_LOOP('',(#13406,#13407,#13408,#13409,#13410));
#3114=EDGE_LOOP('',(#13411,#13412,#13413,#13414,#13415));
#3115=EDGE_LOOP('',(#13416,#13417,#13418,#13419,#13420));
#3116=EDGE_LOOP('',(#13421,#13422,#13423,#13424));
#3117=EDGE_LOOP('',(#13425,#13426,#13427,#13428,#13429,#13430,#13431,#13432,
#13433,#13434,#13435,#13436,#13437,#13438,#13439,#13440,#13441,#13442,#13443,
#13444,#13445,#13446,#13447,#13448,#13449,#13450,#13451,#13452,#13453,#13454,
#13455,#13456,#13457,#13458,#13459,#13460,#13461,#13462,#13463,#13464,#13465,
#13466,#13467,#13468,#13469,#13470,#13471,#13472,#13473,#13474,#13475,#13476));
#3118=EDGE_LOOP('',(#13477,#13478,#13479,#13480,#13481));
#3119=EDGE_LOOP('',(#13482,#13483,#13484,#13485,#13486,#13487));
#3120=EDGE_LOOP('',(#13488,#13489,#13490,#13491,#13492,#13493,#13494,#13495,
#13496,#13497,#13498,#13499,#13500,#13501,#13502,#13503,#13504,#13505,#13506,
#13507,#13508,#13509,#13510,#13511,#13512,#13513,#13514,#13515,#13516,#13517,
#13518,#13519,#13520,#13521,#13522,#13523,#13524,#13525,#13526,#13527,#13528,
#13529,#13530,#13531,#13532,#13533,#13534,#13535,#13536,#13537,#13538,#13539,
#13540,#13541,#13542,#13543,#13544,#13545,#13546,#13547,#13548,#13549,#13550,
#13551));
#3121=EDGE_LOOP('',(#13552,#13553,#13554,#13555,#13556,#13557));
#3122=EDGE_LOOP('',(#13558,#13559,#13560,#13561,#13562,#13563,#13564,#13565,
#13566,#13567,#13568,#13569,#13570,#13571,#13572,#13573,#13574,#13575,#13576,
#13577,#13578,#13579,#13580,#13581,#13582,#13583,#13584,#13585,#13586,#13587,
#13588,#13589,#13590,#13591,#13592,#13593,#13594,#13595,#13596,#13597,#13598,
#13599,#13600,#13601,#13602,#13603,#13604,#13605,#13606,#13607,#13608,#13609,
#13610,#13611,#13612,#13613,#13614,#13615,#13616,#13617,#13618,#13619,#13620,
#13621));
#3123=EDGE_LOOP('',(#13622,#13623,#13624,#13625,#13626,#13627,#13628,#13629,
#13630,#13631,#13632,#13633,#13634,#13635,#13636,#13637,#13638,#13639,#13640,
#13641,#13642));
#3124=EDGE_LOOP('',(#13643,#13644,#13645,#13646));
#3125=EDGE_LOOP('',(#13647,#13648,#13649,#13650));
#3126=EDGE_LOOP('',(#13651,#13652,#13653,#13654));
#3127=EDGE_LOOP('',(#13655,#13656,#13657,#13658));
#3128=EDGE_LOOP('',(#13659,#13660,#13661,#13662));
#3129=EDGE_LOOP('',(#13663,#13664,#13665,#13666));
#3130=EDGE_LOOP('',(#13667,#13668,#13669,#13670,#13671,#13672,#13673,#13674));
#3131=EDGE_LOOP('',(#13675,#13676,#13677,#13678,#13679,#13680,#13681,#13682));
#3132=EDGE_LOOP('',(#13683,#13684,#13685,#13686,#13687,#13688,#13689,#13690));
#3133=EDGE_LOOP('',(#13691,#13692));
#3134=EDGE_LOOP('',(#13693,#13694));
#3135=EDGE_LOOP('',(#13695,#13696));
#3136=EDGE_LOOP('',(#13697,#13698));
#3137=EDGE_LOOP('',(#13699,#13700));
#3138=EDGE_LOOP('',(#13701,#13702));
#3139=EDGE_LOOP('',(#13703,#13704));
#3140=EDGE_LOOP('',(#13705,#13706));
#3141=EDGE_LOOP('',(#13707,#13708));
#3142=EDGE_LOOP('',(#13709,#13710));
#3143=EDGE_LOOP('',(#13711,#13712));
#3144=EDGE_LOOP('',(#13713,#13714));
#3145=EDGE_LOOP('',(#13715,#13716,#13717,#13718,#13719,#13720,#13721,#13722));
#3146=EDGE_LOOP('',(#13723,#13724,#13725,#13726,#13727,#13728,#13729,#13730));
#3147=EDGE_LOOP('',(#13731,#13732,#13733,#13734,#13735,#13736,#13737,#13738));
#3148=EDGE_LOOP('',(#13739,#13740,#13741,#13742,#13743,#13744,#13745,#13746));
#3149=EDGE_LOOP('',(#13747));
#3150=EDGE_LOOP('',(#13748));
#3151=EDGE_LOOP('',(#13749,#13750,#13751,#13752,#13753,#13754,#13755));
#3152=EDGE_LOOP('',(#13756,#13757,#13758,#13759,#13760,#13761,#13762));
#3153=EDGE_LOOP('',(#13763));
#3154=EDGE_LOOP('',(#13764,#13765,#13766));
#3155=EDGE_LOOP('',(#13767,#13768,#13769,#13770,#13771,#13772,#13773));
#3156=EDGE_LOOP('',(#13774,#13775,#13776,#13777,#13778));
#3157=EDGE_LOOP('',(#13779,#13780,#13781,#13782,#13783,#13784));
#3158=EDGE_LOOP('',(#13785,#13786,#13787,#13788,#13789));
#3159=EDGE_LOOP('',(#13790,#13791,#13792,#13793,#13794,#13795));
#3160=EDGE_LOOP('',(#13796,#13797,#13798,#13799,#13800));
#3161=EDGE_LOOP('',(#13801,#13802,#13803,#13804,#13805,#13806));
#3162=EDGE_LOOP('',(#13807,#13808,#13809,#13810,#13811));
#3163=EDGE_LOOP('',(#13812,#13813,#13814,#13815,#13816,#13817));
#3164=EDGE_LOOP('',(#13818,#13819,#13820));
#3165=EDGE_LOOP('',(#13821,#13822,#13823,#13824,#13825));
#3166=EDGE_LOOP('',(#13826,#13827,#13828,#13829,#13830,#13831,#13832,#13833,
#13834,#13835,#13836,#13837,#13838,#13839,#13840,#13841,#13842,#13843,#13844,
#13845,#13846,#13847,#13848,#13849,#13850,#13851));
#3167=EDGE_LOOP('',(#13852,#13853,#13854,#13855,#13856));
#3168=EDGE_LOOP('',(#13857,#13858,#13859,#13860,#13861,#13862,#13863,#13864,
#13865,#13866,#13867,#13868,#13869,#13870,#13871,#13872,#13873,#13874,#13875,
#13876,#13877,#13878,#13879,#13880,#13881,#13882,#13883,#13884,#13885,#13886,
#13887,#13888,#13889,#13890));
#3169=EDGE_LOOP('',(#13891,#13892,#13893,#13894));
#3170=EDGE_LOOP('',(#13895,#13896,#13897,#13898,#13899,#13900,#13901,#13902,
#13903,#13904,#13905,#13906,#13907,#13908,#13909,#13910,#13911,#13912,#13913,
#13914,#13915,#13916,#13917,#13918,#13919,#13920,#13921,#13922,#13923,#13924,
#13925,#13926,#13927));
#3171=EDGE_LOOP('',(#13928,#13929,#13930,#13931,#13932,#13933));
#3172=EDGE_LOOP('',(#13934,#13935,#13936,#13937,#13938,#13939,#13940));
#3173=EDGE_LOOP('',(#13941));
#3174=EDGE_LOOP('',(#13942));
#3175=EDGE_LOOP('',(#13943,#13944));
#3176=EDGE_LOOP('',(#13945,#13946));
#3177=EDGE_LOOP('',(#13947,#13948));
#3178=EDGE_LOOP('',(#13949,#13950));
#3179=EDGE_LOOP('',(#13951,#13952));
#3180=EDGE_LOOP('',(#13953,#13954));
#3181=EDGE_LOOP('',(#13955,#13956,#13957,#13958,#13959,#13960,#13961,#13962));
#3182=EDGE_LOOP('',(#13963,#13964,#13965,#13966));
#3183=EDGE_LOOP('',(#13967,#13968,#13969,#13970));
#3184=EDGE_LOOP('',(#13971,#13972,#13973,#13974));
#3185=EDGE_LOOP('',(#13975,#13976,#13977,#13978));
#3186=EDGE_LOOP('',(#13979,#13980,#13981,#13982));
#3187=EDGE_LOOP('',(#13983,#13984,#13985,#13986));
#3188=EDGE_LOOP('',(#13987,#13988,#13989,#13990));
#3189=EDGE_LOOP('',(#13991,#13992,#13993,#13994,#13995,#13996,#13997,#13998,
#13999));
#3190=EDGE_LOOP('',(#14000,#14001,#14002));
#3191=EDGE_LOOP('',(#14003,#14004,#14005,#14006,#14007,#14008));
#3192=EDGE_LOOP('',(#14009,#14010,#14011,#14012,#14013));
#3193=EDGE_LOOP('',(#14014,#14015,#14016,#14017,#14018));
#3194=EDGE_LOOP('',(#14019,#14020,#14021,#14022,#14023));
#3195=EDGE_LOOP('',(#14024,#14025,#14026,#14027,#14028,#14029));
#3196=EDGE_LOOP('',(#14030,#14031,#14032,#14033,#14034));
#3197=EDGE_LOOP('',(#14035,#14036,#14037,#14038,#14039,#14040));
#3198=EDGE_LOOP('',(#14041,#14042,#14043,#14044,#14045));
#3199=EDGE_LOOP('',(#14046,#14047,#14048,#14049,#14050,#14051));
#3200=EDGE_LOOP('',(#14052,#14053,#14054,#14055,#14056));
#3201=EDGE_LOOP('',(#14057,#14058,#14059,#14060,#14061,#14062));
#3202=EDGE_LOOP('',(#14063,#14064,#14065,#14066,#14067,#14068,#14069,#14070,
#14071,#14072,#14073,#14074,#14075,#14076,#14077,#14078,#14079,#14080,#14081,
#14082,#14083,#14084,#14085,#14086,#14087,#14088,#14089,#14090,#14091,#14092));
#3203=EDGE_LOOP('',(#14093,#14094,#14095,#14096,#14097));
#3204=EDGE_LOOP('',(#14098,#14099,#14100,#14101,#14102,#14103,#14104,#14105,
#14106,#14107,#14108,#14109,#14110,#14111,#14112,#14113,#14114,#14115,#14116,
#14117,#14118,#14119,#14120,#14121,#14122,#14123,#14124,#14125,#14126,#14127,
#14128,#14129,#14130,#14131,#14132));
#3205=EDGE_LOOP('',(#14133,#14134,#14135,#14136,#14137));
#3206=EDGE_LOOP('',(#14138,#14139,#14140,#14141,#14142,#14143,#14144,#14145,
#14146,#14147,#14148,#14149,#14150,#14151,#14152,#14153,#14154,#14155,#14156,
#14157,#14158,#14159,#14160,#14161,#14162,#14163,#14164,#14165,#14166,#14167,
#14168,#14169,#14170,#14171,#14172,#14173,#14174,#14175,#14176,#14177));
#3207=EDGE_LOOP('',(#14178,#14179,#14180,#14181,#14182,#14183,#14184));
#3208=EDGE_LOOP('',(#14185));
#3209=EDGE_LOOP('',(#14186));
#3210=EDGE_LOOP('',(#14187,#14188,#14189,#14190,#14191));
#3211=EDGE_LOOP('',(#14192,#14193,#14194,#14195,#14196,#14197));
#3212=EDGE_LOOP('',(#14198,#14199,#14200,#14201,#14202,#14203));
#3213=EDGE_LOOP('',(#14204,#14205,#14206,#14207,#14208,#14209,#14210,#14211,
#14212,#14213,#14214,#14215));
#3214=EDGE_LOOP('',(#14216,#14217));
#3215=EDGE_LOOP('',(#14218,#14219));
#3216=EDGE_LOOP('',(#14220,#14221,#14222,#14223));
#3217=EDGE_LOOP('',(#14224));
#3218=EDGE_LOOP('',(#14225,#14226,#14227,#14228,#14229,#14230,#14231,#14232,
#14233));
#3219=EDGE_LOOP('',(#14234,#14235,#14236,#14237));
#3220=LINE('',#20568,#4332);
#3221=LINE('',#20573,#4333);
#3222=LINE('',#20575,#4334);
#3223=LINE('',#20577,#4335);
#3224=LINE('',#20578,#4336);
#3225=LINE('',#20587,#4337);
#3226=LINE('',#20592,#4338);
#3227=LINE('',#20595,#4339);
#3228=LINE('',#20600,#4340);
#3229=LINE('',#20603,#4341);
#3230=LINE('',#20608,#4342);
#3231=LINE('',#20611,#4343);
#3232=LINE('',#20617,#4344);
#3233=LINE('',#20622,#4345);
#3234=LINE('',#20624,#4346);
#3235=LINE('',#20626,#4347);
#3236=LINE('',#20627,#4348);
#3237=LINE('',#20636,#4349);
#3238=LINE('',#20641,#4350);
#3239=LINE('',#20644,#4351);
#3240=LINE('',#20649,#4352);
#3241=LINE('',#20652,#4353);
#3242=LINE('',#20657,#4354);
#3243=LINE('',#20660,#4355);
#3244=LINE('',#20666,#4356);
#3245=LINE('',#20671,#4357);
#3246=LINE('',#20673,#4358);
#3247=LINE('',#20675,#4359);
#3248=LINE('',#20676,#4360);
#3249=LINE('',#20693,#4361);
#3250=LINE('',#20698,#4362);
#3251=LINE('',#20701,#4363);
#3252=LINE('',#20706,#4364);
#3253=LINE('',#20709,#4365);
#3254=LINE('',#20714,#4366);
#3255=LINE('',#20717,#4367);
#3256=LINE('',#20722,#4368);
#3257=LINE('',#20725,#4369);
#3258=LINE('',#20730,#4370);
#3259=LINE('',#20733,#4371);
#3260=LINE('',#20738,#4372);
#3261=LINE('',#20741,#4373);
#3262=LINE('',#20746,#4374);
#3263=LINE('',#20749,#4375);
#3264=LINE('',#20753,#4376);
#3265=LINE('',#20756,#4377);
#3266=LINE('',#20759,#4378);
#3267=LINE('',#20762,#4379);
#3268=LINE('',#20765,#4380);
#3269=LINE('',#20768,#4381);
#3270=LINE('',#20771,#4382);
#3271=LINE('',#20774,#4383);
#3272=LINE('',#20778,#4384);
#3273=LINE('',#20780,#4385);
#3274=LINE('',#20782,#4386);
#3275=LINE('',#20784,#4387);
#3276=LINE('',#20785,#4388);
#3277=LINE('',#20788,#4389);
#3278=LINE('',#20790,#4390);
#3279=LINE('',#20791,#4391);
#3280=LINE('',#20792,#4392);
#3281=LINE('',#20795,#4393);
#3282=LINE('',#20797,#4394);
#3283=LINE('',#20799,#4395);
#3284=LINE('',#20801,#4396);
#3285=LINE('',#20803,#4397);
#3286=LINE('',#20805,#4398);
#3287=LINE('',#20806,#4399);
#3288=LINE('',#20807,#4400);
#3289=LINE('',#20809,#4401);
#3290=LINE('',#20811,#4402);
#3291=LINE('',#20813,#4403);
#3292=LINE('',#20815,#4404);
#3293=LINE('',#20817,#4405);
#3294=LINE('',#20819,#4406);
#3295=LINE('',#20821,#4407);
#3296=LINE('',#20822,#4408);
#3297=LINE('',#20825,#4409);
#3298=LINE('',#20827,#4410);
#3299=LINE('',#20828,#4411);
#3300=LINE('',#20831,#4412);
#3301=LINE('',#20833,#4413);
#3302=LINE('',#20835,#4414);
#3303=LINE('',#20836,#4415);
#3304=LINE('',#20839,#4416);
#3305=LINE('',#20840,#4417);
#3306=LINE('',#20843,#4418);
#3307=LINE('',#20844,#4419);
#3308=LINE('',#20847,#4420);
#3309=LINE('',#20849,#4421);
#3310=LINE('',#20850,#4422);
#3311=LINE('',#20853,#4423);
#3312=LINE('',#20855,#4424);
#3313=LINE('',#20856,#4425);
#3314=LINE('',#20859,#4426);
#3315=LINE('',#20860,#4427);
#3316=LINE('',#20862,#4428);
#3317=LINE('',#20863,#4429);
#3318=LINE('',#20866,#4430);
#3319=LINE('',#20868,#4431);
#3320=LINE('',#20870,#4432);
#3321=LINE('',#20872,#4433);
#3322=LINE('',#20874,#4434);
#3323=LINE('',#20876,#4435);
#3324=LINE('',#20877,#4436);
#3325=LINE('',#20878,#4437);
#3326=LINE('',#20880,#4438);
#3327=LINE('',#20882,#4439);
#3328=LINE('',#20884,#4440);
#3329=LINE('',#20886,#4441);
#3330=LINE('',#20888,#4442);
#3331=LINE('',#20890,#4443);
#3332=LINE('',#20891,#4444);
#3333=LINE('',#20893,#4445);
#3334=LINE('',#20894,#4446);
#3335=LINE('',#20896,#4447);
#3336=LINE('',#20899,#4448);
#3337=LINE('',#20901,#4449);
#3338=LINE('',#20903,#4450);
#3339=LINE('',#20905,#4451);
#3340=LINE('',#20907,#4452);
#3341=LINE('',#20909,#4453);
#3342=LINE('',#20912,#4454);
#3343=LINE('',#20914,#4455);
#3344=LINE('',#20918,#4456);
#3345=LINE('',#20920,#4457);
#3346=LINE('',#20927,#4458);
#3347=LINE('',#20942,#4459);
#3348=LINE('',#20947,#4460);
#3349=LINE('',#20953,#4461);
#3350=LINE('',#20968,#4462);
#3351=LINE('',#20973,#4463);
#3352=LINE('',#20979,#4464);
#3353=LINE('',#20994,#4465);
#3354=LINE('',#20999,#4466);
#3355=LINE('',#21004,#4467);
#3356=LINE('',#21006,#4468);
#3357=LINE('',#21008,#4469);
#3358=LINE('',#21009,#4470);
#3359=LINE('',#21012,#4471);
#3360=LINE('',#21016,#4472);
#3361=LINE('',#21020,#4473);
#3362=LINE('',#21033,#4474);
#3363=LINE('',#21037,#4475);
#3364=LINE('',#21041,#4476);
#3365=LINE('',#21047,#4477);
#3366=LINE('',#21062,#4478);
#3367=LINE('',#21067,#4479);
#3368=LINE('',#21073,#4480);
#3369=LINE('',#21088,#4481);
#3370=LINE('',#21093,#4482);
#3371=LINE('',#21099,#4483);
#3372=LINE('',#21114,#4484);
#3373=LINE('',#21119,#4485);
#3374=LINE('',#21124,#4486);
#3375=LINE('',#21126,#4487);
#3376=LINE('',#21128,#4488);
#3377=LINE('',#21129,#4489);
#3378=LINE('',#21132,#4490);
#3379=LINE('',#21136,#4491);
#3380=LINE('',#21140,#4492);
#3381=LINE('',#21153,#4493);
#3382=LINE('',#21157,#4494);
#3383=LINE('',#21161,#4495);
#3384=LINE('',#21167,#4496);
#3385=LINE('',#21172,#4497);
#3386=LINE('',#21174,#4498);
#3387=LINE('',#21176,#4499);
#3388=LINE('',#21178,#4500);
#3389=LINE('',#21180,#4501);
#3390=LINE('',#21182,#4502);
#3391=LINE('',#21184,#4503);
#3392=LINE('',#21186,#4504);
#3393=LINE('',#21188,#4505);
#3394=LINE('',#21190,#4506);
#3395=LINE('',#21192,#4507);
#3396=LINE('',#21194,#4508);
#3397=LINE('',#21196,#4509);
#3398=LINE('',#21197,#4510);
#3399=LINE('',#21206,#4511);
#3400=LINE('',#21213,#4512);
#3401=LINE('',#21216,#4513);
#3402=LINE('',#21223,#4514);
#3403=LINE('',#21226,#4515);
#3404=LINE('',#21233,#4516);
#3405=LINE('',#21236,#4517);
#3406=LINE('',#21242,#4518);
#3407=LINE('',#21245,#4519);
#3408=LINE('',#21248,#4520);
#3409=LINE('',#21251,#4521);
#3410=LINE('',#21256,#4522);
#3411=LINE('',#21261,#4523);
#3412=LINE('',#21263,#4524);
#3413=LINE('',#21265,#4525);
#3414=LINE('',#21267,#4526);
#3415=LINE('',#21269,#4527);
#3416=LINE('',#21271,#4528);
#3417=LINE('',#21273,#4529);
#3418=LINE('',#21275,#4530);
#3419=LINE('',#21277,#4531);
#3420=LINE('',#21279,#4532);
#3421=LINE('',#21281,#4533);
#3422=LINE('',#21283,#4534);
#3423=LINE('',#21285,#4535);
#3424=LINE('',#21286,#4536);
#3425=LINE('',#21295,#4537);
#3426=LINE('',#21302,#4538);
#3427=LINE('',#21305,#4539);
#3428=LINE('',#21312,#4540);
#3429=LINE('',#21315,#4541);
#3430=LINE('',#21322,#4542);
#3431=LINE('',#21325,#4543);
#3432=LINE('',#21331,#4544);
#3433=LINE('',#21334,#4545);
#3434=LINE('',#21337,#4546);
#3435=LINE('',#21340,#4547);
#3436=LINE('',#21345,#4548);
#3437=LINE('',#21350,#4549);
#3438=LINE('',#21352,#4550);
#3439=LINE('',#21354,#4551);
#3440=LINE('',#21355,#4552);
#3441=LINE('',#21384,#4553);
#3442=LINE('',#21389,#4554);
#3443=LINE('',#21392,#4555);
#3444=LINE('',#21397,#4556);
#3445=LINE('',#21400,#4557);
#3446=LINE('',#21405,#4558);
#3447=LINE('',#21408,#4559);
#3448=LINE('',#21413,#4560);
#3449=LINE('',#21416,#4561);
#3450=LINE('',#21421,#4562);
#3451=LINE('',#21424,#4563);
#3452=LINE('',#21428,#4564);
#3453=LINE('',#21431,#4565);
#3454=LINE('',#21434,#4566);
#3455=LINE('',#21437,#4567);
#3456=LINE('',#21440,#4568);
#3457=LINE('',#21443,#4569);
#3458=LINE('',#21447,#4570);
#3459=LINE('',#21450,#4571);
#3460=LINE('',#21455,#4572);
#3461=LINE('',#21458,#4573);
#3462=LINE('',#21463,#4574);
#3463=LINE('',#21466,#4575);
#3464=LINE('',#21471,#4576);
#3465=LINE('',#21474,#4577);
#3466=LINE('',#21479,#4578);
#3467=LINE('',#21482,#4579);
#3468=LINE('',#21487,#4580);
#3469=LINE('',#21490,#4581);
#3470=LINE('',#21495,#4582);
#3471=LINE('',#21498,#4583);
#3472=LINE('',#21503,#4584);
#3473=LINE('',#21506,#4585);
#3474=LINE('',#21534,#4586);
#3475=LINE('',#21538,#4587);
#3476=LINE('',#21542,#4588);
#3477=LINE('',#21546,#4589);
#3478=LINE('',#21550,#4590);
#3479=LINE('',#21554,#4591);
#3480=LINE('',#21558,#4592);
#3481=LINE('',#21562,#4593);
#3482=LINE('',#21565,#4594);
#3483=LINE('',#21567,#4595);
#3484=LINE('',#21568,#4596);
#3485=LINE('',#21571,#4597);
#3486=LINE('',#21572,#4598);
#3487=LINE('',#21573,#4599);
#3488=LINE('',#21575,#4600);
#3489=LINE('',#21576,#4601);
#3490=LINE('',#21578,#4602);
#3491=LINE('',#21580,#4603);
#3492=LINE('',#21581,#4604);
#3493=LINE('',#21583,#4605);
#3494=LINE('',#21585,#4606);
#3495=LINE('',#21586,#4607);
#3496=LINE('',#21589,#4608);
#3497=LINE('',#21590,#4609);
#3498=LINE('',#21592,#4610);
#3499=LINE('',#21595,#4611);
#3500=LINE('',#21596,#4612);
#3501=LINE('',#21598,#4613);
#3502=LINE('',#21600,#4614);
#3503=LINE('',#21601,#4615);
#3504=LINE('',#21603,#4616);
#3505=LINE('',#21607,#4617);
#3506=LINE('',#21609,#4618);
#3507=LINE('',#21611,#4619);
#3508=LINE('',#21613,#4620);
#3509=LINE('',#21615,#4621);
#3510=LINE('',#21622,#4622);
#3511=LINE('',#21627,#4623);
#3512=LINE('',#21629,#4624);
#3513=LINE('',#21631,#4625);
#3514=LINE('',#21633,#4626);
#3515=LINE('',#21635,#4627);
#3516=LINE('',#21637,#4628);
#3517=LINE('',#21639,#4629);
#3518=LINE('',#21641,#4630);
#3519=LINE('',#21643,#4631);
#3520=LINE('',#21645,#4632);
#3521=LINE('',#21647,#4633);
#3522=LINE('',#21649,#4634);
#3523=LINE('',#21651,#4635);
#3524=LINE('',#21653,#4636);
#3525=LINE('',#21654,#4637);
#3526=LINE('',#21656,#4638);
#3527=LINE('',#21657,#4639);
#3528=LINE('',#21660,#4640);
#3529=LINE('',#21666,#4641);
#3530=LINE('',#21671,#4642);
#3531=LINE('',#21676,#4643);
#3532=LINE('',#21678,#4644);
#3533=LINE('',#21679,#4645);
#3534=LINE('',#21681,#4646);
#3535=LINE('',#21683,#4647);
#3536=LINE('',#21685,#4648);
#3537=LINE('',#21687,#4649);
#3538=LINE('',#21689,#4650);
#3539=LINE('',#21691,#4651);
#3540=LINE('',#21693,#4652);
#3541=LINE('',#21695,#4653);
#3542=LINE('',#21697,#4654);
#3543=LINE('',#21699,#4655);
#3544=LINE('',#21701,#4656);
#3545=LINE('',#21703,#4657);
#3546=LINE('',#21705,#4658);
#3547=LINE('',#21706,#4659);
#3548=LINE('',#21709,#4660);
#3549=LINE('',#21715,#4661);
#3550=LINE('',#21720,#4662);
#3551=LINE('',#21723,#4663);
#3552=LINE('',#21724,#4664);
#3553=LINE('',#21731,#4665);
#3554=LINE('',#21735,#4666);
#3555=LINE('',#21743,#4667);
#3556=LINE('',#21747,#4668);
#3557=LINE('',#21755,#4669);
#3558=LINE('',#21760,#4670);
#3559=LINE('',#21763,#4671);
#3560=LINE('',#21767,#4672);
#3561=LINE('',#21775,#4673);
#3562=LINE('',#21779,#4674);
#3563=LINE('',#21787,#4675);
#3564=LINE('',#21792,#4676);
#3565=LINE('',#21795,#4677);
#3566=LINE('',#21799,#4678);
#3567=LINE('',#21807,#4679);
#3568=LINE('',#21811,#4680);
#3569=LINE('',#21819,#4681);
#3570=LINE('',#21822,#4682);
#3571=LINE('',#21824,#4683);
#3572=LINE('',#21826,#4684);
#3573=LINE('',#21828,#4685);
#3574=LINE('',#21830,#4686);
#3575=LINE('',#21832,#4687);
#3576=LINE('',#21834,#4688);
#3577=LINE('',#21835,#4689);
#3578=LINE('',#21836,#4690);
#3579=LINE('',#21837,#4691);
#3580=LINE('',#21838,#4692);
#3581=LINE('',#21840,#4693);
#3582=LINE('',#21842,#4694);
#3583=LINE('',#21844,#4695);
#3584=LINE('',#21846,#4696);
#3585=LINE('',#21848,#4697);
#3586=LINE('',#21850,#4698);
#3587=LINE('',#21852,#4699);
#3588=LINE('',#21854,#4700);
#3589=LINE('',#21856,#4701);
#3590=LINE('',#21859,#4702);
#3591=LINE('',#21861,#4703);
#3592=LINE('',#21862,#4704);
#3593=LINE('',#21865,#4705);
#3594=LINE('',#21867,#4706);
#3595=LINE('',#21868,#4707);
#3596=LINE('',#21870,#4708);
#3597=LINE('',#21871,#4709);
#3598=LINE('',#21874,#4710);
#3599=LINE('',#21876,#4711);
#3600=LINE('',#21877,#4712);
#3601=LINE('',#21880,#4713);
#3602=LINE('',#21881,#4714);
#3603=LINE('',#21882,#4715);
#3604=LINE('',#21885,#4716);
#3605=LINE('',#21886,#4717);
#3606=LINE('',#21888,#4718);
#3607=LINE('',#21890,#4719);
#3608=LINE('',#21892,#4720);
#3609=LINE('',#21895,#4721);
#3610=LINE('',#21896,#4722);
#3611=LINE('',#21898,#4723);
#3612=LINE('',#21903,#4724);
#3613=LINE('',#21905,#4725);
#3614=LINE('',#21912,#4726);
#3615=LINE('',#21919,#4727);
#3616=LINE('',#21921,#4728);
#3617=LINE('',#21923,#4729);
#3618=LINE('',#21925,#4730);
#3619=LINE('',#21927,#4731);
#3620=LINE('',#21929,#4732);
#3621=LINE('',#21931,#4733);
#3622=LINE('',#21933,#4734);
#3623=LINE('',#21935,#4735);
#3624=LINE('',#21937,#4736);
#3625=LINE('',#21938,#4737);
#3626=LINE('',#21940,#4738);
#3627=LINE('',#21942,#4739);
#3628=LINE('',#21944,#4740);
#3629=LINE('',#21946,#4741);
#3630=LINE('',#21948,#4742);
#3631=LINE('',#21949,#4743);
#3632=LINE('',#21952,#4744);
#3633=LINE('',#21958,#4745);
#3634=LINE('',#21963,#4746);
#3635=LINE('',#21970,#4747);
#3636=LINE('',#21972,#4748);
#3637=LINE('',#21973,#4749);
#3638=LINE('',#21975,#4750);
#3639=LINE('',#21977,#4751);
#3640=LINE('',#21979,#4752);
#3641=LINE('',#21981,#4753);
#3642=LINE('',#21983,#4754);
#3643=LINE('',#21985,#4755);
#3644=LINE('',#21987,#4756);
#3645=LINE('',#21989,#4757);
#3646=LINE('',#21991,#4758);
#3647=LINE('',#21993,#4759);
#3648=LINE('',#21995,#4760);
#3649=LINE('',#21997,#4761);
#3650=LINE('',#21999,#4762);
#3651=LINE('',#22000,#4763);
#3652=LINE('',#22003,#4764);
#3653=LINE('',#22009,#4765);
#3654=LINE('',#22014,#4766);
#3655=LINE('',#22017,#4767);
#3656=LINE('',#22018,#4768);
#3657=LINE('',#22027,#4769);
#3658=LINE('',#22031,#4770);
#3659=LINE('',#22039,#4771);
#3660=LINE('',#22043,#4772);
#3661=LINE('',#22051,#4773);
#3662=LINE('',#22056,#4774);
#3663=LINE('',#22059,#4775);
#3664=LINE('',#22063,#4776);
#3665=LINE('',#22071,#4777);
#3666=LINE('',#22075,#4778);
#3667=LINE('',#22083,#4779);
#3668=LINE('',#22088,#4780);
#3669=LINE('',#22091,#4781);
#3670=LINE('',#22095,#4782);
#3671=LINE('',#22103,#4783);
#3672=LINE('',#22107,#4784);
#3673=LINE('',#22115,#4785);
#3674=LINE('',#22120,#4786);
#3675=LINE('',#22123,#4787);
#3676=LINE('',#22127,#4788);
#3677=LINE('',#22135,#4789);
#3678=LINE('',#22139,#4790);
#3679=LINE('',#22147,#4791);
#3680=LINE('',#22150,#4792);
#3681=LINE('',#22152,#4793);
#3682=LINE('',#22154,#4794);
#3683=LINE('',#22156,#4795);
#3684=LINE('',#22158,#4796);
#3685=LINE('',#22160,#4797);
#3686=LINE('',#22162,#4798);
#3687=LINE('',#22164,#4799);
#3688=LINE('',#22166,#4800);
#3689=LINE('',#22167,#4801);
#3690=LINE('',#22168,#4802);
#3691=LINE('',#22169,#4803);
#3692=LINE('',#22170,#4804);
#3693=LINE('',#22171,#4805);
#3694=LINE('',#22173,#4806);
#3695=LINE('',#22175,#4807);
#3696=LINE('',#22177,#4808);
#3697=LINE('',#22179,#4809);
#3698=LINE('',#22181,#4810);
#3699=LINE('',#22183,#4811);
#3700=LINE('',#22185,#4812);
#3701=LINE('',#22187,#4813);
#3702=LINE('',#22189,#4814);
#3703=LINE('',#22191,#4815);
#3704=LINE('',#22193,#4816);
#3705=LINE('',#22195,#4817);
#3706=LINE('',#22198,#4818);
#3707=LINE('',#22200,#4819);
#3708=LINE('',#22201,#4820);
#3709=LINE('',#22204,#4821);
#3710=LINE('',#22205,#4822);
#3711=LINE('',#22208,#4823);
#3712=LINE('',#22210,#4824);
#3713=LINE('',#22211,#4825);
#3714=LINE('',#22214,#4826);
#3715=LINE('',#22215,#4827);
#3716=LINE('',#22218,#4828);
#3717=LINE('',#22219,#4829);
#3718=LINE('',#22222,#4830);
#3719=LINE('',#22223,#4831);
#3720=LINE('',#22225,#4832);
#3721=LINE('',#22227,#4833);
#3722=LINE('',#22229,#4834);
#3723=LINE('',#22230,#4835);
#3724=LINE('',#22232,#4836);
#3725=LINE('',#22234,#4837);
#3726=LINE('',#22237,#4838);
#3727=LINE('',#22238,#4839);
#3728=LINE('',#22242,#4840);
#3729=LINE('',#22244,#4841);
#3730=LINE('',#22250,#4842);
#3731=LINE('',#22252,#4843);
#3732=LINE('',#22254,#4844);
#3733=LINE('',#22255,#4845);
#3734=LINE('',#22260,#4846);
#3735=LINE('',#22264,#4847);
#3736=LINE('',#22266,#4848);
#3737=LINE('',#22267,#4849);
#3738=LINE('',#22272,#4850);
#3739=LINE('',#22276,#4851);
#3740=LINE('',#22278,#4852);
#3741=LINE('',#22279,#4853);
#3742=LINE('',#22284,#4854);
#3743=LINE('',#22288,#4855);
#3744=LINE('',#22290,#4856);
#3745=LINE('',#22291,#4857);
#3746=LINE('',#22298,#4858);
#3747=LINE('',#22300,#4859);
#3748=LINE('',#22302,#4860);
#3749=LINE('',#22303,#4861);
#3750=LINE('',#22308,#4862);
#3751=LINE('',#22312,#4863);
#3752=LINE('',#22314,#4864);
#3753=LINE('',#22315,#4865);
#3754=LINE('',#22320,#4866);
#3755=LINE('',#22324,#4867);
#3756=LINE('',#22326,#4868);
#3757=LINE('',#22327,#4869);
#3758=LINE('',#22332,#4870);
#3759=LINE('',#22336,#4871);
#3760=LINE('',#22338,#4872);
#3761=LINE('',#22339,#4873);
#3762=LINE('',#22346,#4874);
#3763=LINE('',#22348,#4875);
#3764=LINE('',#22350,#4876);
#3765=LINE('',#22351,#4877);
#3766=LINE('',#22356,#4878);
#3767=LINE('',#22360,#4879);
#3768=LINE('',#22362,#4880);
#3769=LINE('',#22363,#4881);
#3770=LINE('',#22368,#4882);
#3771=LINE('',#22372,#4883);
#3772=LINE('',#22374,#4884);
#3773=LINE('',#22375,#4885);
#3774=LINE('',#22380,#4886);
#3775=LINE('',#22384,#4887);
#3776=LINE('',#22386,#4888);
#3777=LINE('',#22387,#4889);
#3778=LINE('',#22394,#4890);
#3779=LINE('',#22396,#4891);
#3780=LINE('',#22398,#4892);
#3781=LINE('',#22399,#4893);
#3782=LINE('',#22404,#4894);
#3783=LINE('',#22408,#4895);
#3784=LINE('',#22410,#4896);
#3785=LINE('',#22411,#4897);
#3786=LINE('',#22416,#4898);
#3787=LINE('',#22420,#4899);
#3788=LINE('',#22422,#4900);
#3789=LINE('',#22423,#4901);
#3790=LINE('',#22428,#4902);
#3791=LINE('',#22432,#4903);
#3792=LINE('',#22434,#4904);
#3793=LINE('',#22435,#4905);
#3794=LINE('',#22442,#4906);
#3795=LINE('',#22444,#4907);
#3796=LINE('',#22446,#4908);
#3797=LINE('',#22447,#4909);
#3798=LINE('',#22452,#4910);
#3799=LINE('',#22456,#4911);
#3800=LINE('',#22458,#4912);
#3801=LINE('',#22459,#4913);
#3802=LINE('',#22464,#4914);
#3803=LINE('',#22468,#4915);
#3804=LINE('',#22470,#4916);
#3805=LINE('',#22471,#4917);
#3806=LINE('',#22476,#4918);
#3807=LINE('',#22480,#4919);
#3808=LINE('',#22482,#4920);
#3809=LINE('',#22483,#4921);
#3810=LINE('',#22490,#4922);
#3811=LINE('',#22492,#4923);
#3812=LINE('',#22494,#4924);
#3813=LINE('',#22495,#4925);
#3814=LINE('',#22500,#4926);
#3815=LINE('',#22504,#4927);
#3816=LINE('',#22506,#4928);
#3817=LINE('',#22507,#4929);
#3818=LINE('',#22512,#4930);
#3819=LINE('',#22516,#4931);
#3820=LINE('',#22518,#4932);
#3821=LINE('',#22519,#4933);
#3822=LINE('',#22524,#4934);
#3823=LINE('',#22528,#4935);
#3824=LINE('',#22530,#4936);
#3825=LINE('',#22531,#4937);
#3826=LINE('',#22538,#4938);
#3827=LINE('',#22540,#4939);
#3828=LINE('',#22542,#4940);
#3829=LINE('',#22543,#4941);
#3830=LINE('',#22548,#4942);
#3831=LINE('',#22552,#4943);
#3832=LINE('',#22554,#4944);
#3833=LINE('',#22555,#4945);
#3834=LINE('',#22560,#4946);
#3835=LINE('',#22564,#4947);
#3836=LINE('',#22566,#4948);
#3837=LINE('',#22567,#4949);
#3838=LINE('',#22572,#4950);
#3839=LINE('',#22576,#4951);
#3840=LINE('',#22578,#4952);
#3841=LINE('',#22579,#4953);
#3842=LINE('',#22586,#4954);
#3843=LINE('',#22588,#4955);
#3844=LINE('',#22590,#4956);
#3845=LINE('',#22591,#4957);
#3846=LINE('',#22596,#4958);
#3847=LINE('',#22600,#4959);
#3848=LINE('',#22602,#4960);
#3849=LINE('',#22603,#4961);
#3850=LINE('',#22608,#4962);
#3851=LINE('',#22612,#4963);
#3852=LINE('',#22614,#4964);
#3853=LINE('',#22615,#4965);
#3854=LINE('',#22620,#4966);
#3855=LINE('',#22624,#4967);
#3856=LINE('',#22626,#4968);
#3857=LINE('',#22627,#4969);
#3858=LINE('',#22634,#4970);
#3859=LINE('',#22636,#4971);
#3860=LINE('',#22638,#4972);
#3861=LINE('',#22639,#4973);
#3862=LINE('',#22644,#4974);
#3863=LINE('',#22648,#4975);
#3864=LINE('',#22650,#4976);
#3865=LINE('',#22651,#4977);
#3866=LINE('',#22656,#4978);
#3867=LINE('',#22660,#4979);
#3868=LINE('',#22662,#4980);
#3869=LINE('',#22663,#4981);
#3870=LINE('',#22668,#4982);
#3871=LINE('',#22672,#4983);
#3872=LINE('',#22674,#4984);
#3873=LINE('',#22675,#4985);
#3874=LINE('',#22682,#4986);
#3875=LINE('',#22684,#4987);
#3876=LINE('',#22686,#4988);
#3877=LINE('',#22687,#4989);
#3878=LINE('',#22692,#4990);
#3879=LINE('',#22696,#4991);
#3880=LINE('',#22698,#4992);
#3881=LINE('',#22699,#4993);
#3882=LINE('',#22704,#4994);
#3883=LINE('',#22708,#4995);
#3884=LINE('',#22710,#4996);
#3885=LINE('',#22711,#4997);
#3886=LINE('',#22716,#4998);
#3887=LINE('',#22720,#4999);
#3888=LINE('',#22722,#5000);
#3889=LINE('',#22723,#5001);
#3890=LINE('',#22730,#5002);
#3891=LINE('',#22732,#5003);
#3892=LINE('',#22734,#5004);
#3893=LINE('',#22735,#5005);
#3894=LINE('',#22740,#5006);
#3895=LINE('',#22744,#5007);
#3896=LINE('',#22746,#5008);
#3897=LINE('',#22747,#5009);
#3898=LINE('',#22752,#5010);
#3899=LINE('',#22756,#5011);
#3900=LINE('',#22758,#5012);
#3901=LINE('',#22759,#5013);
#3902=LINE('',#22764,#5014);
#3903=LINE('',#22768,#5015);
#3904=LINE('',#22770,#5016);
#3905=LINE('',#22771,#5017);
#3906=LINE('',#22778,#5018);
#3907=LINE('',#22780,#5019);
#3908=LINE('',#22782,#5020);
#3909=LINE('',#22783,#5021);
#3910=LINE('',#22788,#5022);
#3911=LINE('',#22792,#5023);
#3912=LINE('',#22794,#5024);
#3913=LINE('',#22795,#5025);
#3914=LINE('',#22800,#5026);
#3915=LINE('',#22804,#5027);
#3916=LINE('',#22806,#5028);
#3917=LINE('',#22807,#5029);
#3918=LINE('',#22812,#5030);
#3919=LINE('',#22816,#5031);
#3920=LINE('',#22818,#5032);
#3921=LINE('',#22819,#5033);
#3922=LINE('',#22826,#5034);
#3923=LINE('',#22828,#5035);
#3924=LINE('',#22830,#5036);
#3925=LINE('',#22831,#5037);
#3926=LINE('',#22836,#5038);
#3927=LINE('',#22840,#5039);
#3928=LINE('',#22842,#5040);
#3929=LINE('',#22843,#5041);
#3930=LINE('',#22848,#5042);
#3931=LINE('',#22852,#5043);
#3932=LINE('',#22854,#5044);
#3933=LINE('',#22855,#5045);
#3934=LINE('',#22860,#5046);
#3935=LINE('',#22864,#5047);
#3936=LINE('',#22866,#5048);
#3937=LINE('',#22867,#5049);
#3938=LINE('',#22874,#5050);
#3939=LINE('',#22876,#5051);
#3940=LINE('',#22878,#5052);
#3941=LINE('',#22879,#5053);
#3942=LINE('',#22884,#5054);
#3943=LINE('',#22888,#5055);
#3944=LINE('',#22890,#5056);
#3945=LINE('',#22891,#5057);
#3946=LINE('',#22896,#5058);
#3947=LINE('',#22900,#5059);
#3948=LINE('',#22902,#5060);
#3949=LINE('',#22903,#5061);
#3950=LINE('',#22908,#5062);
#3951=LINE('',#22912,#5063);
#3952=LINE('',#22914,#5064);
#3953=LINE('',#22915,#5065);
#3954=LINE('',#22922,#5066);
#3955=LINE('',#22924,#5067);
#3956=LINE('',#22926,#5068);
#3957=LINE('',#22927,#5069);
#3958=LINE('',#22932,#5070);
#3959=LINE('',#22936,#5071);
#3960=LINE('',#22938,#5072);
#3961=LINE('',#22939,#5073);
#3962=LINE('',#22944,#5074);
#3963=LINE('',#22948,#5075);
#3964=LINE('',#22950,#5076);
#3965=LINE('',#22951,#5077);
#3966=LINE('',#22956,#5078);
#3967=LINE('',#22960,#5079);
#3968=LINE('',#22962,#5080);
#3969=LINE('',#22963,#5081);
#3970=LINE('',#22970,#5082);
#3971=LINE('',#22972,#5083);
#3972=LINE('',#22974,#5084);
#3973=LINE('',#22975,#5085);
#3974=LINE('',#22981,#5086);
#3975=LINE('',#22984,#5087);
#3976=LINE('',#22986,#5088);
#3977=LINE('',#22987,#5089);
#3978=LINE('',#22993,#5090);
#3979=LINE('',#22996,#5091);
#3980=LINE('',#22998,#5092);
#3981=LINE('',#22999,#5093);
#3982=LINE('',#23005,#5094);
#3983=LINE('',#23008,#5095);
#3984=LINE('',#23010,#5096);
#3985=LINE('',#23011,#5097);
#3986=LINE('',#23024,#5098);
#3987=LINE('',#23028,#5099);
#3988=LINE('',#23031,#5100);
#3989=LINE('',#23038,#5101);
#3990=LINE('',#23279,#5102);
#3991=LINE('',#23718,#5103);
#3992=LINE('',#24155,#5104);
#3993=LINE('',#24596,#5105);
#3994=LINE('',#25079,#5106);
#3995=LINE('',#25510,#5107);
#3996=LINE('',#25798,#5108);
#3997=LINE('',#26266,#5109);
#3998=LINE('',#26700,#5110);
#3999=LINE('',#26872,#5111);
#4000=LINE('',#27194,#5112);
#4001=LINE('',#27647,#5113);
#4002=LINE('',#28096,#5114);
#4003=LINE('',#28531,#5115);
#4004=LINE('',#28990,#5116);
#4005=LINE('',#29435,#5117);
#4006=LINE('',#29914,#5118);
#4007=LINE('',#30399,#5119);
#4008=LINE('',#30846,#5120);
#4009=LINE('',#31293,#5121);
#4010=LINE('',#31726,#5122);
#4011=LINE('',#32243,#5123);
#4012=LINE('',#32694,#5124);
#4013=LINE('',#42247,#5125);
#4014=LINE('',#42255,#5126);
#4015=LINE('',#42256,#5127);
#4016=LINE('',#42259,#5128);
#4017=LINE('',#42261,#5129);
#4018=LINE('',#42267,#5130);
#4019=LINE('',#42276,#5131);
#4020=LINE('',#42281,#5132);
#4021=LINE('',#42285,#5133);
#4022=LINE('',#42289,#5134);
#4023=LINE('',#42293,#5135);
#4024=LINE('',#42297,#5136);
#4025=LINE('',#42301,#5137);
#4026=LINE('',#42305,#5138);
#4027=LINE('',#42309,#5139);
#4028=LINE('',#42313,#5140);
#4029=LINE('',#42317,#5141);
#4030=LINE('',#42321,#5142);
#4031=LINE('',#42325,#5143);
#4032=LINE('',#42329,#5144);
#4033=LINE('',#42333,#5145);
#4034=LINE('',#42337,#5146);
#4035=LINE('',#42341,#5147);
#4036=LINE('',#42345,#5148);
#4037=LINE('',#42349,#5149);
#4038=LINE('',#42353,#5150);
#4039=LINE('',#42357,#5151);
#4040=LINE('',#42361,#5152);
#4041=LINE('',#42365,#5153);
#4042=LINE('',#42369,#5154);
#4043=LINE('',#42373,#5155);
#4044=LINE('',#42377,#5156);
#4045=LINE('',#42381,#5157);
#4046=LINE('',#42385,#5158);
#4047=LINE('',#42389,#5159);
#4048=LINE('',#42393,#5160);
#4049=LINE('',#42397,#5161);
#4050=LINE('',#42401,#5162);
#4051=LINE('',#42405,#5163);
#4052=LINE('',#42409,#5164);
#4053=LINE('',#42414,#5165);
#4054=LINE('',#42418,#5166);
#4055=LINE('',#42422,#5167);
#4056=LINE('',#42426,#5168);
#4057=LINE('',#42430,#5169);
#4058=LINE('',#42434,#5170);
#4059=LINE('',#42438,#5171);
#4060=LINE('',#42442,#5172);
#4061=LINE('',#42446,#5173);
#4062=LINE('',#42450,#5174);
#4063=LINE('',#42454,#5175);
#4064=LINE('',#42458,#5176);
#4065=LINE('',#42462,#5177);
#4066=LINE('',#42466,#5178);
#4067=LINE('',#42470,#5179);
#4068=LINE('',#42474,#5180);
#4069=LINE('',#42478,#5181);
#4070=LINE('',#42482,#5182);
#4071=LINE('',#42486,#5183);
#4072=LINE('',#42490,#5184);
#4073=LINE('',#42494,#5185);
#4074=LINE('',#42498,#5186);
#4075=LINE('',#42502,#5187);
#4076=LINE('',#42506,#5188);
#4077=LINE('',#42510,#5189);
#4078=LINE('',#42514,#5190);
#4079=LINE('',#42518,#5191);
#4080=LINE('',#42522,#5192);
#4081=LINE('',#42526,#5193);
#4082=LINE('',#42530,#5194);
#4083=LINE('',#42534,#5195);
#4084=LINE('',#42538,#5196);
#4085=LINE('',#42542,#5197);
#4086=LINE('',#42546,#5198);
#4087=LINE('',#42550,#5199);
#4088=LINE('',#42554,#5200);
#4089=LINE('',#42557,#5201);
#4090=LINE('',#42560,#5202);
#4091=LINE('',#42562,#5203);
#4092=LINE('',#42570,#5204);
#4093=LINE('',#42812,#5205);
#4094=LINE('',#42816,#5206);
#4095=LINE('',#42817,#5207);
#4096=LINE('',#42819,#5208);
#4097=LINE('',#42823,#5209);
#4098=LINE('',#42824,#5210);
#4099=LINE('',#42826,#5211);
#4100=LINE('',#42830,#5212);
#4101=LINE('',#42831,#5213);
#4102=LINE('',#42833,#5214);
#4103=LINE('',#42837,#5215);
#4104=LINE('',#42838,#5216);
#4105=LINE('',#42840,#5217);
#4106=LINE('',#42844,#5218);
#4107=LINE('',#42845,#5219);
#4108=LINE('',#42847,#5220);
#4109=LINE('',#42851,#5221);
#4110=LINE('',#42852,#5222);
#4111=LINE('',#42854,#5223);
#4112=LINE('',#42858,#5224);
#4113=LINE('',#42859,#5225);
#4114=LINE('',#42861,#5226);
#4115=LINE('',#42865,#5227);
#4116=LINE('',#42866,#5228);
#4117=LINE('',#42868,#5229);
#4118=LINE('',#42872,#5230);
#4119=LINE('',#42873,#5231);
#4120=LINE('',#42875,#5232);
#4121=LINE('',#42879,#5233);
#4122=LINE('',#42880,#5234);
#4123=LINE('',#42882,#5235);
#4124=LINE('',#42886,#5236);
#4125=LINE('',#42887,#5237);
#4126=LINE('',#42889,#5238);
#4127=LINE('',#42893,#5239);
#4128=LINE('',#42894,#5240);
#4129=LINE('',#42896,#5241);
#4130=LINE('',#42900,#5242);
#4131=LINE('',#42901,#5243);
#4132=LINE('',#42903,#5244);
#4133=LINE('',#42907,#5245);
#4134=LINE('',#42908,#5246);
#4135=LINE('',#42910,#5247);
#4136=LINE('',#42914,#5248);
#4137=LINE('',#42915,#5249);
#4138=LINE('',#42917,#5250);
#4139=LINE('',#42921,#5251);
#4140=LINE('',#42922,#5252);
#4141=LINE('',#42924,#5253);
#4142=LINE('',#42928,#5254);
#4143=LINE('',#42929,#5255);
#4144=LINE('',#42931,#5256);
#4145=LINE('',#42935,#5257);
#4146=LINE('',#42936,#5258);
#4147=LINE('',#42938,#5259);
#4148=LINE('',#42942,#5260);
#4149=LINE('',#42943,#5261);
#4150=LINE('',#42945,#5262);
#4151=LINE('',#42949,#5263);
#4152=LINE('',#42950,#5264);
#4153=LINE('',#42952,#5265);
#4154=LINE('',#42956,#5266);
#4155=LINE('',#42957,#5267);
#4156=LINE('',#42959,#5268);
#4157=LINE('',#42963,#5269);
#4158=LINE('',#42964,#5270);
#4159=LINE('',#42966,#5271);
#4160=LINE('',#42970,#5272);
#4161=LINE('',#42971,#5273);
#4162=LINE('',#42973,#5274);
#4163=LINE('',#42977,#5275);
#4164=LINE('',#42978,#5276);
#4165=LINE('',#42980,#5277);
#4166=LINE('',#42984,#5278);
#4167=LINE('',#42985,#5279);
#4168=LINE('',#42987,#5280);
#4169=LINE('',#42991,#5281);
#4170=LINE('',#42992,#5282);
#4171=LINE('',#42994,#5283);
#4172=LINE('',#42998,#5284);
#4173=LINE('',#42999,#5285);
#4174=LINE('',#43001,#5286);
#4175=LINE('',#43005,#5287);
#4176=LINE('',#43006,#5288);
#4177=LINE('',#43008,#5289);
#4178=LINE('',#43012,#5290);
#4179=LINE('',#43013,#5291);
#4180=LINE('',#43015,#5292);
#4181=LINE('',#43019,#5293);
#4182=LINE('',#43020,#5294);
#4183=LINE('',#43022,#5295);
#4184=LINE('',#43026,#5296);
#4185=LINE('',#43027,#5297);
#4186=LINE('',#43029,#5298);
#4187=LINE('',#43033,#5299);
#4188=LINE('',#43034,#5300);
#4189=LINE('',#43036,#5301);
#4190=LINE('',#43040,#5302);
#4191=LINE('',#43041,#5303);
#4192=LINE('',#43043,#5304);
#4193=LINE('',#43047,#5305);
#4194=LINE('',#43048,#5306);
#4195=LINE('',#43050,#5307);
#4196=LINE('',#43118,#5308);
#4197=LINE('',#43121,#5309);
#4198=LINE('',#43123,#5310);
#4199=LINE('',#43127,#5311);
#4200=LINE('',#43129,#5312);
#4201=LINE('',#43133,#5313);
#4202=LINE('',#43136,#5314);
#4203=LINE('',#43139,#5315);
#4204=LINE('',#43141,#5316);
#4205=LINE('',#43145,#5317);
#4206=LINE('',#43148,#5318);
#4207=LINE('',#43151,#5319);
#4208=LINE('',#43154,#5320);
#4209=LINE('',#43156,#5321);
#4210=LINE('',#43158,#5322);
#4211=LINE('',#43160,#5323);
#4212=LINE('',#43161,#5324);
#4213=LINE('',#43163,#5325);
#4214=LINE('',#43165,#5326);
#4215=LINE('',#43166,#5327);
#4216=LINE('',#43168,#5328);
#4217=LINE('',#43170,#5329);
#4218=LINE('',#43171,#5330);
#4219=LINE('',#43175,#5331);
#4220=LINE('',#43178,#5332);
#4221=LINE('',#43180,#5333);
#4222=LINE('',#43183,#5334);
#4223=LINE('',#43193,#5335);
#4224=LINE('',#43196,#5336);
#4225=LINE('',#43200,#5337);
#4226=LINE('',#43202,#5338);
#4227=LINE('',#43204,#5339);
#4228=LINE('',#43210,#5340);
#4229=LINE('',#43509,#5341);
#4230=LINE('',#43953,#5342);
#4231=LINE('',#44385,#5343);
#4232=LINE('',#44805,#5344);
#4233=LINE('',#45307,#5345);
#4234=LINE('',#45737,#5346);
#4235=LINE('',#46191,#5347);
#4236=LINE('',#46635,#5348);
#4237=LINE('',#47117,#5349);
#4238=LINE('',#47583,#5350);
#4239=LINE('',#48007,#5351);
#4240=LINE('',#48471,#5352);
#4241=LINE('',#48910,#5353);
#4242=LINE('',#49349,#5354);
#4243=LINE('',#49798,#5355);
#4244=LINE('',#50301,#5356);
#4245=LINE('',#50804,#5357);
#4246=LINE('',#51283,#5358);
#4247=LINE('',#51716,#5359);
#4248=LINE('',#52161,#5360);
#4249=LINE('',#52610,#5361);
#4250=LINE('',#53053,#5362);
#4251=LINE('',#63245,#5363);
#4252=LINE('',#63249,#5364);
#4253=LINE('',#63251,#5365);
#4254=LINE('',#63255,#5366);
#4255=LINE('',#63257,#5367);
#4256=LINE('',#63261,#5368);
#4257=LINE('',#63264,#5369);
#4258=LINE('',#63267,#5370);
#4259=LINE('',#63269,#5371);
#4260=LINE('',#63273,#5372);
#4261=LINE('',#63276,#5373);
#4262=LINE('',#63279,#5374);
#4263=LINE('',#63282,#5375);
#4264=LINE('',#63284,#5376);
#4265=LINE('',#63286,#5377);
#4266=LINE('',#63288,#5378);
#4267=LINE('',#63289,#5379);
#4268=LINE('',#63291,#5380);
#4269=LINE('',#63293,#5381);
#4270=LINE('',#63294,#5382);
#4271=LINE('',#63296,#5383);
#4272=LINE('',#63298,#5384);
#4273=LINE('',#63299,#5385);
#4274=LINE('',#63303,#5386);
#4275=LINE('',#63306,#5387);
#4276=LINE('',#63308,#5388);
#4277=LINE('',#63311,#5389);
#4278=LINE('',#63321,#5390);
#4279=LINE('',#63324,#5391);
#4280=LINE('',#63328,#5392);
#4281=LINE('',#63330,#5393);
#4282=LINE('',#63332,#5394);
#4283=LINE('',#63338,#5395);
#4284=LINE('',#63341,#5396);
#4285=LINE('',#63348,#5397);
#4286=LINE('',#63379,#5398);
#4287=LINE('',#63754,#5399);
#4288=LINE('',#64126,#5400);
#4289=LINE('',#64510,#5401);
#4290=LINE('',#64893,#5402);
#4291=LINE('',#65270,#5403);
#4292=LINE('',#65649,#5404);
#4293=LINE('',#65877,#5405);
#4294=LINE('',#66229,#5406);
#4295=LINE('',#66611,#5407);
#4296=LINE('',#71404,#5408);
#4297=LINE('',#71408,#5409);
#4298=LINE('',#71412,#5410);
#4299=LINE('',#71416,#5411);
#4300=LINE('',#71420,#5412);
#4301=LINE('',#71423,#5413);
#4302=LINE('',#71427,#5414);
#4303=LINE('',#71432,#5415);
#4304=LINE('',#71433,#5416);
#4305=LINE('',#71437,#5417);
#4306=LINE('',#71441,#5418);
#4307=LINE('',#71445,#5419);
#4308=LINE('',#71449,#5420);
#4309=LINE('',#71455,#5421);
#4310=LINE('',#71462,#5422);
#4311=LINE('',#71518,#5423);
#4312=LINE('',#71886,#5424);
#4313=LINE('',#72252,#5425);
#4314=LINE('',#72618,#5426);
#4315=LINE('',#72992,#5427);
#4316=LINE('',#73367,#5428);
#4317=LINE('',#73718,#5429);
#4318=LINE('',#73946,#5430);
#4319=LINE('',#74318,#5431);
#4320=LINE('',#74693,#5432);
#4321=LINE('',#75067,#5433);
#4322=LINE('',#80906,#5434);
#4323=LINE('',#80910,#5435);
#4324=LINE('',#80914,#5436);
#4325=LINE('',#80916,#5437);
#4326=LINE('',#80922,#5438);
#4327=LINE('',#80928,#5439);
#4328=LINE('',#80934,#5440);
#4329=LINE('',#80939,#5441);
#4330=LINE('',#80941,#5442);
#4331=LINE('',#80953,#5443);
#4332=VECTOR('',#16628,2.89999999999999);
#4333=VECTOR('',#16633,10.);
#4334=VECTOR('',#16634,10.);
#4335=VECTOR('',#16635,10.);
#4336=VECTOR('',#16636,10.);
#4337=VECTOR('',#16645,2.74999999999999);
#4338=VECTOR('',#16652,2.9);
#4339=VECTOR('',#16655,2.75);
#4340=VECTOR('',#16662,2.9);
#4341=VECTOR('',#16665,2.75);
#4342=VECTOR('',#16672,2.9);
#4343=VECTOR('',#16675,2.75);
#4344=VECTOR('',#16682,2.89999999999999);
#4345=VECTOR('',#16687,10.);
#4346=VECTOR('',#16688,10.);
#4347=VECTOR('',#16689,10.);
#4348=VECTOR('',#16690,10.);
#4349=VECTOR('',#16699,2.74999999999999);
#4350=VECTOR('',#16706,2.9);
#4351=VECTOR('',#16709,2.75);
#4352=VECTOR('',#16716,2.9);
#4353=VECTOR('',#16719,2.75);
#4354=VECTOR('',#16726,2.9);
#4355=VECTOR('',#16729,2.75);
#4356=VECTOR('',#16736,3.24999999999999);
#4357=VECTOR('',#16741,10.);
#4358=VECTOR('',#16742,10.);
#4359=VECTOR('',#16743,10.);
#4360=VECTOR('',#16744,10.);
#4361=VECTOR('',#16761,3.05);
#4362=VECTOR('',#16768,3.24999999999999);
#4363=VECTOR('',#16771,3.05);
#4364=VECTOR('',#16778,3.25);
#4365=VECTOR('',#16781,3.05);
#4366=VECTOR('',#16788,3.25);
#4367=VECTOR('',#16791,3.05);
#4368=VECTOR('',#16798,3.25);
#4369=VECTOR('',#16801,3.05);
#4370=VECTOR('',#16808,3.25);
#4371=VECTOR('',#16811,3.05);
#4372=VECTOR('',#16818,3.24999999999999);
#4373=VECTOR('',#16821,3.05);
#4374=VECTOR('',#16828,3.24999999999999);
#4375=VECTOR('',#16831,3.05);
#4376=VECTOR('',#16836,1.525);
#4377=VECTOR('',#16839,1.525);
#4378=VECTOR('',#16842,1.525);
#4379=VECTOR('',#16845,1.525);
#4380=VECTOR('',#16848,1.525);
#4381=VECTOR('',#16851,1.525);
#4382=VECTOR('',#16854,1.525);
#4383=VECTOR('',#16857,1.525);
#4384=VECTOR('',#16860,10.);
#4385=VECTOR('',#16861,10.);
#4386=VECTOR('',#16862,10.);
#4387=VECTOR('',#16863,10.);
#4388=VECTOR('',#16864,10.);
#4389=VECTOR('',#16867,10.);
#4390=VECTOR('',#16868,10.);
#4391=VECTOR('',#16869,10.);
#4392=VECTOR('',#16870,10.);
#4393=VECTOR('',#16873,10.);
#4394=VECTOR('',#16874,10.);
#4395=VECTOR('',#16875,10.);
#4396=VECTOR('',#16876,10.);
#4397=VECTOR('',#16877,10.);
#4398=VECTOR('',#16878,10.);
#4399=VECTOR('',#16879,10.);
#4400=VECTOR('',#16880,10.);
#4401=VECTOR('',#16881,10.);
#4402=VECTOR('',#16882,10.);
#4403=VECTOR('',#16883,10.);
#4404=VECTOR('',#16884,10.);
#4405=VECTOR('',#16885,10.);
#4406=VECTOR('',#16886,10.);
#4407=VECTOR('',#16887,10.);
#4408=VECTOR('',#16888,10.);
#4409=VECTOR('',#16891,10.);
#4410=VECTOR('',#16892,10.);
#4411=VECTOR('',#16893,10.);
#4412=VECTOR('',#16896,10.);
#4413=VECTOR('',#16897,10.);
#4414=VECTOR('',#16898,10.);
#4415=VECTOR('',#16899,10.);
#4416=VECTOR('',#16902,10.);
#4417=VECTOR('',#16903,10.);
#4418=VECTOR('',#16906,10.);
#4419=VECTOR('',#16907,10.);
#4420=VECTOR('',#16910,10.);
#4421=VECTOR('',#16911,10.);
#4422=VECTOR('',#16912,10.);
#4423=VECTOR('',#16915,10.);
#4424=VECTOR('',#16916,10.);
#4425=VECTOR('',#16917,10.);
#4426=VECTOR('',#16920,10.);
#4427=VECTOR('',#16921,10.);
#4428=VECTOR('',#16924,10.);
#4429=VECTOR('',#16925,10.);
#4430=VECTOR('',#16928,10.);
#4431=VECTOR('',#16929,10.);
#4432=VECTOR('',#16930,10.);
#4433=VECTOR('',#16931,10.);
#4434=VECTOR('',#16932,10.);
#4435=VECTOR('',#16933,10.);
#4436=VECTOR('',#16934,10.);
#4437=VECTOR('',#16935,10.);
#4438=VECTOR('',#16936,10.);
#4439=VECTOR('',#16937,10.);
#4440=VECTOR('',#16938,10.);
#4441=VECTOR('',#16939,10.);
#4442=VECTOR('',#16940,10.);
#4443=VECTOR('',#16941,10.);
#4444=VECTOR('',#16942,10.);
#4445=VECTOR('',#16945,10.);
#4446=VECTOR('',#16946,10.);
#4447=VECTOR('',#16949,10.);
#4448=VECTOR('',#16954,10.);
#4449=VECTOR('',#16957,10.);
#4450=VECTOR('',#16960,10.);
#4451=VECTOR('',#16963,10.);
#4452=VECTOR('',#16966,10.);
#4453=VECTOR('',#16969,10.);
#4454=VECTOR('',#16974,10.);
#4455=VECTOR('',#16977,10.);
#4456=VECTOR('',#16984,10.);
#4457=VECTOR('',#16987,10.);
#4458=VECTOR('',#16996,2.7);
#4459=VECTOR('',#17005,5.15000000000001);
#4460=VECTOR('',#17012,2.55000000000001);
#4461=VECTOR('',#17019,2.7);
#4462=VECTOR('',#17028,5.15);
#4463=VECTOR('',#17035,2.55000000000001);
#4464=VECTOR('',#17042,2.7);
#4465=VECTOR('',#17051,5.15);
#4466=VECTOR('',#17058,2.55);
#4467=VECTOR('',#17063,10.);
#4468=VECTOR('',#17064,10.);
#4469=VECTOR('',#17065,10.);
#4470=VECTOR('',#17066,10.);
#4471=VECTOR('',#17069,5.);
#4472=VECTOR('',#17074,5.);
#4473=VECTOR('',#17079,5.);
#4474=VECTOR('',#17096,3.);
#4475=VECTOR('',#17101,3.00000000000001);
#4476=VECTOR('',#17106,3.00000000000001);
#4477=VECTOR('',#17113,2.7);
#4478=VECTOR('',#17122,5.15000000000001);
#4479=VECTOR('',#17129,2.55000000000001);
#4480=VECTOR('',#17136,2.7);
#4481=VECTOR('',#17145,5.15);
#4482=VECTOR('',#17152,2.55000000000001);
#4483=VECTOR('',#17159,2.7);
#4484=VECTOR('',#17168,5.15);
#4485=VECTOR('',#17175,2.55);
#4486=VECTOR('',#17180,10.);
#4487=VECTOR('',#17181,10.);
#4488=VECTOR('',#17182,10.);
#4489=VECTOR('',#17183,10.);
#4490=VECTOR('',#17186,5.);
#4491=VECTOR('',#17191,5.);
#4492=VECTOR('',#17196,5.);
#4493=VECTOR('',#17213,3.);
#4494=VECTOR('',#17218,3.00000000000001);
#4495=VECTOR('',#17223,3.00000000000001);
#4496=VECTOR('',#17230,2.2);
#4497=VECTOR('',#17235,10.);
#4498=VECTOR('',#17236,10.);
#4499=VECTOR('',#17237,10.);
#4500=VECTOR('',#17238,10.);
#4501=VECTOR('',#17239,10.);
#4502=VECTOR('',#17240,10.);
#4503=VECTOR('',#17241,10.);
#4504=VECTOR('',#17242,10.);
#4505=VECTOR('',#17243,10.);
#4506=VECTOR('',#17244,10.);
#4507=VECTOR('',#17245,10.);
#4508=VECTOR('',#17246,10.);
#4509=VECTOR('',#17247,10.);
#4510=VECTOR('',#17248,10.);
#4511=VECTOR('',#17257,2.05);
#4512=VECTOR('',#17266,2.2);
#4513=VECTOR('',#17269,2.05);
#4514=VECTOR('',#17278,2.2);
#4515=VECTOR('',#17281,2.05);
#4516=VECTOR('',#17290,2.2);
#4517=VECTOR('',#17293,2.05);
#4518=VECTOR('',#17300,1.025);
#4519=VECTOR('',#17303,1.025);
#4520=VECTOR('',#17306,1.025);
#4521=VECTOR('',#17309,1.025);
#4522=VECTOR('',#17314,2.2);
#4523=VECTOR('',#17319,10.);
#4524=VECTOR('',#17320,10.);
#4525=VECTOR('',#17321,10.);
#4526=VECTOR('',#17322,10.);
#4527=VECTOR('',#17323,10.);
#4528=VECTOR('',#17324,10.);
#4529=VECTOR('',#17325,10.);
#4530=VECTOR('',#17326,10.);
#4531=VECTOR('',#17327,10.);
#4532=VECTOR('',#17328,10.);
#4533=VECTOR('',#17329,10.);
#4534=VECTOR('',#17330,10.);
#4535=VECTOR('',#17331,10.);
#4536=VECTOR('',#17332,10.);
#4537=VECTOR('',#17341,2.05);
#4538=VECTOR('',#17350,2.2);
#4539=VECTOR('',#17353,2.05);
#4540=VECTOR('',#17362,2.2);
#4541=VECTOR('',#17365,2.05);
#4542=VECTOR('',#17374,2.2);
#4543=VECTOR('',#17377,2.05);
#4544=VECTOR('',#17384,2.05);
#4545=VECTOR('',#17387,2.05);
#4546=VECTOR('',#17390,2.05);
#4547=VECTOR('',#17393,2.05);
#4548=VECTOR('',#17398,3.24999999999999);
#4549=VECTOR('',#17403,10.);
#4550=VECTOR('',#17404,10.);
#4551=VECTOR('',#17405,10.);
#4552=VECTOR('',#17406,10.);
#4553=VECTOR('',#17435,3.05);
#4554=VECTOR('',#17442,3.24999999999999);
#4555=VECTOR('',#17445,3.05);
#4556=VECTOR('',#17452,3.24999999999999);
#4557=VECTOR('',#17455,3.05);
#4558=VECTOR('',#17462,3.25);
#4559=VECTOR('',#17465,3.05);
#4560=VECTOR('',#17472,3.25);
#4561=VECTOR('',#17475,3.05);
#4562=VECTOR('',#17482,3.24999999999999);
#4563=VECTOR('',#17485,3.05);
#4564=VECTOR('',#17490,3.05000000000001);
#4565=VECTOR('',#17493,3.05000000000001);
#4566=VECTOR('',#17496,3.05);
#4567=VECTOR('',#17499,3.05);
#4568=VECTOR('',#17502,3.05);
#4569=VECTOR('',#17505,3.05);
#4570=VECTOR('',#17510,5.65000000000001);
#4571=VECTOR('',#17513,5.50000000000001);
#4572=VECTOR('',#17520,5.65);
#4573=VECTOR('',#17523,5.50000000000001);
#4574=VECTOR('',#17530,5.65);
#4575=VECTOR('',#17533,5.5);
#4576=VECTOR('',#17540,5.65);
#4577=VECTOR('',#17543,5.50000000000001);
#4578=VECTOR('',#17550,5.65);
#4579=VECTOR('',#17553,5.5);
#4580=VECTOR('',#17560,5.65);
#4581=VECTOR('',#17563,5.50000000000001);
#4582=VECTOR('',#17570,5.65);
#4583=VECTOR('',#17573,5.50000000000001);
#4584=VECTOR('',#17580,5.65000000000001);
#4585=VECTOR('',#17583,5.50000000000001);
#4586=VECTOR('',#17620,3.50000000000001);
#4587=VECTOR('',#17625,3.5);
#4588=VECTOR('',#17630,3.5);
#4589=VECTOR('',#17635,3.5);
#4590=VECTOR('',#17640,3.5);
#4591=VECTOR('',#17645,3.5);
#4592=VECTOR('',#17650,3.5);
#4593=VECTOR('',#17655,3.50000000000001);
#4594=VECTOR('',#17660,10.);
#4595=VECTOR('',#17661,10.);
#4596=VECTOR('',#17662,10.);
#4597=VECTOR('',#17665,10.);
#4598=VECTOR('',#17666,10.);
#4599=VECTOR('',#17667,10.);
#4600=VECTOR('',#17670,10.);
#4601=VECTOR('',#17671,10.);
#4602=VECTOR('',#17674,9.99999999999999);
#4603=VECTOR('',#17675,10.);
#4604=VECTOR('',#17676,9.99999999999999);
#4605=VECTOR('',#17679,10.);
#4606=VECTOR('',#17682,10.);
#4607=VECTOR('',#17683,10.);
#4608=VECTOR('',#17686,10.);
#4609=VECTOR('',#17687,10.);
#4610=VECTOR('',#17690,10.);
#4611=VECTOR('',#17695,10.);
#4612=VECTOR('',#17696,10.);
#4613=VECTOR('',#17699,10.);
#4614=VECTOR('',#17702,10.);
#4615=VECTOR('',#17703,10.);
#4616=VECTOR('',#17706,10.);
#4617=VECTOR('',#17713,10.);
#4618=VECTOR('',#17716,10.);
#4619=VECTOR('',#17719,10.);
#4620=VECTOR('',#17722,10.);
#4621=VECTOR('',#17725,10.);
#4622=VECTOR('',#17734,1.65);
#4623=VECTOR('',#17739,10.);
#4624=VECTOR('',#17740,10.);
#4625=VECTOR('',#17741,10.);
#4626=VECTOR('',#17742,10.);
#4627=VECTOR('',#17743,10.);
#4628=VECTOR('',#17744,10.);
#4629=VECTOR('',#17745,10.);
#4630=VECTOR('',#17746,10.);
#4631=VECTOR('',#17747,9.99999999999999);
#4632=VECTOR('',#17748,10.);
#4633=VECTOR('',#17749,10.);
#4634=VECTOR('',#17750,10.);
#4635=VECTOR('',#17751,10.);
#4636=VECTOR('',#17752,9.99999999999999);
#4637=VECTOR('',#17753,10.);
#4638=VECTOR('',#17754,10.);
#4639=VECTOR('',#17755,10.);
#4640=VECTOR('',#17758,1.55);
#4641=VECTOR('',#17765,0.775000000000001);
#4642=VECTOR('',#17770,1.65);
#4643=VECTOR('',#17775,10.);
#4644=VECTOR('',#17776,10.);
#4645=VECTOR('',#17777,10.);
#4646=VECTOR('',#17778,10.);
#4647=VECTOR('',#17779,9.99999999999999);
#4648=VECTOR('',#17780,10.);
#4649=VECTOR('',#17781,10.);
#4650=VECTOR('',#17782,10.);
#4651=VECTOR('',#17783,10.);
#4652=VECTOR('',#17784,9.99999999999999);
#4653=VECTOR('',#17785,10.);
#4654=VECTOR('',#17786,10.);
#4655=VECTOR('',#17787,10.);
#4656=VECTOR('',#17788,10.);
#4657=VECTOR('',#17789,10.);
#4658=VECTOR('',#17790,10.);
#4659=VECTOR('',#17791,10.);
#4660=VECTOR('',#17794,1.55);
#4661=VECTOR('',#17801,1.55);
#4662=VECTOR('',#17806,2.7);
#4663=VECTOR('',#17811,10.);
#4664=VECTOR('',#17812,10.);
#4665=VECTOR('',#17819,2.55000000000001);
#4666=VECTOR('',#17822,10.);
#4667=VECTOR('',#17829,10.);
#4668=VECTOR('',#17832,10.);
#4669=VECTOR('',#17839,10.);
#4670=VECTOR('',#17846,2.7);
#4671=VECTOR('',#17849,2.55000000000001);
#4672=VECTOR('',#17852,10.);
#4673=VECTOR('',#17859,10.);
#4674=VECTOR('',#17862,10.);
#4675=VECTOR('',#17869,10.);
#4676=VECTOR('',#17876,2.7);
#4677=VECTOR('',#17879,2.55);
#4678=VECTOR('',#17882,10.);
#4679=VECTOR('',#17889,10.);
#4680=VECTOR('',#17892,10.);
#4681=VECTOR('',#17899,10.);
#4682=VECTOR('',#17904,10.);
#4683=VECTOR('',#17907,10.);
#4684=VECTOR('',#17910,10.);
#4685=VECTOR('',#17913,10.);
#4686=VECTOR('',#17916,10.);
#4687=VECTOR('',#17919,10.);
#4688=VECTOR('',#17922,10.);
#4689=VECTOR('',#17923,10.);
#4690=VECTOR('',#17924,10.);
#4691=VECTOR('',#17925,10.);
#4692=VECTOR('',#17926,10.);
#4693=VECTOR('',#17929,10.);
#4694=VECTOR('',#17932,10.);
#4695=VECTOR('',#17935,10.);
#4696=VECTOR('',#17938,10.);
#4697=VECTOR('',#17941,10.);
#4698=VECTOR('',#17944,10.);
#4699=VECTOR('',#17947,10.);
#4700=VECTOR('',#17950,10.);
#4701=VECTOR('',#17953,10.);
#4702=VECTOR('',#17956,10.);
#4703=VECTOR('',#17957,10.);
#4704=VECTOR('',#17958,10.);
#4705=VECTOR('',#17961,10.);
#4706=VECTOR('',#17962,10.);
#4707=VECTOR('',#17963,10.);
#4708=VECTOR('',#17966,10.);
#4709=VECTOR('',#17967,10.);
#4710=VECTOR('',#17970,10.);
#4711=VECTOR('',#17971,10.);
#4712=VECTOR('',#17972,10.);
#4713=VECTOR('',#17975,10.);
#4714=VECTOR('',#17976,10.);
#4715=VECTOR('',#17977,10.);
#4716=VECTOR('',#17980,10.);
#4717=VECTOR('',#17981,10.);
#4718=VECTOR('',#17984,10.);
#4719=VECTOR('',#17987,10.);
#4720=VECTOR('',#17990,10.);
#4721=VECTOR('',#17995,10.);
#4722=VECTOR('',#17996,10.);
#4723=VECTOR('',#17999,10.);
#4724=VECTOR('',#18008,10.);
#4725=VECTOR('',#18011,10.);
#4726=VECTOR('',#18020,1.65);
#4727=VECTOR('',#18027,10.);
#4728=VECTOR('',#18028,10.);
#4729=VECTOR('',#18029,10.);
#4730=VECTOR('',#18030,9.99999999999999);
#4731=VECTOR('',#18031,10.);
#4732=VECTOR('',#18032,10.);
#4733=VECTOR('',#18033,10.);
#4734=VECTOR('',#18034,10.);
#4735=VECTOR('',#18035,10.);
#4736=VECTOR('',#18036,9.99999999999999);
#4737=VECTOR('',#18037,10.);
#4738=VECTOR('',#18038,10.);
#4739=VECTOR('',#18039,10.);
#4740=VECTOR('',#18040,10.);
#4741=VECTOR('',#18041,10.);
#4742=VECTOR('',#18042,10.);
#4743=VECTOR('',#18043,10.);
#4744=VECTOR('',#18046,1.55);
#4745=VECTOR('',#18053,0.775000000000001);
#4746=VECTOR('',#18058,1.65);
#4747=VECTOR('',#18065,10.);
#4748=VECTOR('',#18066,10.);
#4749=VECTOR('',#18067,10.);
#4750=VECTOR('',#18068,10.);
#4751=VECTOR('',#18069,9.99999999999999);
#4752=VECTOR('',#18070,10.);
#4753=VECTOR('',#18071,10.);
#4754=VECTOR('',#18072,10.);
#4755=VECTOR('',#18073,10.);
#4756=VECTOR('',#18074,10.);
#4757=VECTOR('',#18075,9.99999999999999);
#4758=VECTOR('',#18076,10.);
#4759=VECTOR('',#18077,10.);
#4760=VECTOR('',#18078,10.);
#4761=VECTOR('',#18079,10.);
#4762=VECTOR('',#18080,10.);
#4763=VECTOR('',#18081,10.);
#4764=VECTOR('',#18084,1.55);
#4765=VECTOR('',#18091,1.55);
#4766=VECTOR('',#18096,2.7);
#4767=VECTOR('',#18101,10.);
#4768=VECTOR('',#18102,10.);
#4769=VECTOR('',#18111,2.54999999999999);
#4770=VECTOR('',#18114,10.);
#4771=VECTOR('',#18121,10.);
#4772=VECTOR('',#18124,10.);
#4773=VECTOR('',#18131,10.);
#4774=VECTOR('',#18138,2.7);
#4775=VECTOR('',#18141,2.55);
#4776=VECTOR('',#18144,10.);
#4777=VECTOR('',#18151,10.);
#4778=VECTOR('',#18154,10.);
#4779=VECTOR('',#18161,10.);
#4780=VECTOR('',#18168,2.7);
#4781=VECTOR('',#18171,2.55000000000001);
#4782=VECTOR('',#18174,10.);
#4783=VECTOR('',#18181,10.);
#4784=VECTOR('',#18184,10.);
#4785=VECTOR('',#18191,10.);
#4786=VECTOR('',#18198,2.7);
#4787=VECTOR('',#18201,2.55000000000001);
#4788=VECTOR('',#18204,10.);
#4789=VECTOR('',#18211,10.);
#4790=VECTOR('',#18214,10.);
#4791=VECTOR('',#18221,10.);
#4792=VECTOR('',#18226,10.);
#4793=VECTOR('',#18229,10.);
#4794=VECTOR('',#18232,10.);
#4795=VECTOR('',#18235,10.);
#4796=VECTOR('',#18238,10.);
#4797=VECTOR('',#18241,10.);
#4798=VECTOR('',#18244,10.);
#4799=VECTOR('',#18247,10.);
#4800=VECTOR('',#18250,10.);
#4801=VECTOR('',#18251,10.);
#4802=VECTOR('',#18252,10.);
#4803=VECTOR('',#18253,10.);
#4804=VECTOR('',#18254,10.);
#4805=VECTOR('',#18255,10.);
#4806=VECTOR('',#18258,10.);
#4807=VECTOR('',#18261,10.);
#4808=VECTOR('',#18264,10.);
#4809=VECTOR('',#18267,10.);
#4810=VECTOR('',#18270,10.);
#4811=VECTOR('',#18273,10.);
#4812=VECTOR('',#18276,10.);
#4813=VECTOR('',#18279,10.);
#4814=VECTOR('',#18282,10.);
#4815=VECTOR('',#18285,10.);
#4816=VECTOR('',#18288,10.);
#4817=VECTOR('',#18291,10.);
#4818=VECTOR('',#18294,10.);
#4819=VECTOR('',#18295,10.);
#4820=VECTOR('',#18296,10.);
#4821=VECTOR('',#18299,10.);
#4822=VECTOR('',#18300,10.);
#4823=VECTOR('',#18303,10.);
#4824=VECTOR('',#18304,10.);
#4825=VECTOR('',#18305,10.);
#4826=VECTOR('',#18308,10.);
#4827=VECTOR('',#18309,10.);
#4828=VECTOR('',#18312,10.);
#4829=VECTOR('',#18313,10.);
#4830=VECTOR('',#18316,10.);
#4831=VECTOR('',#18317,10.);
#4832=VECTOR('',#18320,10.);
#4833=VECTOR('',#18323,10.);
#4834=VECTOR('',#18326,10.);
#4835=VECTOR('',#18327,10.);
#4836=VECTOR('',#18330,10.);
#4837=VECTOR('',#18333,10.);
#4838=VECTOR('',#18338,10.);
#4839=VECTOR('',#18339,10.);
#4840=VECTOR('',#18346,10.);
#4841=VECTOR('',#18349,10.);
#4842=VECTOR('',#18356,10.);
#4843=VECTOR('',#18357,10.);
#4844=VECTOR('',#18358,10.);
#4845=VECTOR('',#18359,10.);
#4846=VECTOR('',#18364,10.);
#4847=VECTOR('',#18369,10.);
#4848=VECTOR('',#18370,10.);
#4849=VECTOR('',#18371,10.);
#4850=VECTOR('',#18376,10.);
#4851=VECTOR('',#18381,10.);
#4852=VECTOR('',#18382,10.);
#4853=VECTOR('',#18383,10.);
#4854=VECTOR('',#18388,10.);
#4855=VECTOR('',#18393,10.);
#4856=VECTOR('',#18394,10.);
#4857=VECTOR('',#18395,10.);
#4858=VECTOR('',#18404,10.);
#4859=VECTOR('',#18405,10.);
#4860=VECTOR('',#18406,10.);
#4861=VECTOR('',#18407,10.);
#4862=VECTOR('',#18412,10.);
#4863=VECTOR('',#18417,10.);
#4864=VECTOR('',#18418,10.);
#4865=VECTOR('',#18419,10.);
#4866=VECTOR('',#18424,10.);
#4867=VECTOR('',#18429,10.);
#4868=VECTOR('',#18430,10.);
#4869=VECTOR('',#18431,10.);
#4870=VECTOR('',#18436,10.);
#4871=VECTOR('',#18441,10.);
#4872=VECTOR('',#18442,10.);
#4873=VECTOR('',#18443,10.);
#4874=VECTOR('',#18452,10.);
#4875=VECTOR('',#18453,10.);
#4876=VECTOR('',#18454,10.);
#4877=VECTOR('',#18455,10.);
#4878=VECTOR('',#18460,10.);
#4879=VECTOR('',#18465,10.);
#4880=VECTOR('',#18466,10.);
#4881=VECTOR('',#18467,10.);
#4882=VECTOR('',#18472,10.);
#4883=VECTOR('',#18477,10.);
#4884=VECTOR('',#18478,10.);
#4885=VECTOR('',#18479,10.);
#4886=VECTOR('',#18484,10.);
#4887=VECTOR('',#18489,10.);
#4888=VECTOR('',#18490,10.);
#4889=VECTOR('',#18491,10.);
#4890=VECTOR('',#18500,10.);
#4891=VECTOR('',#18501,10.);
#4892=VECTOR('',#18502,10.);
#4893=VECTOR('',#18503,10.);
#4894=VECTOR('',#18508,10.);
#4895=VECTOR('',#18513,10.);
#4896=VECTOR('',#18514,10.);
#4897=VECTOR('',#18515,10.);
#4898=VECTOR('',#18520,10.);
#4899=VECTOR('',#18525,10.);
#4900=VECTOR('',#18526,10.);
#4901=VECTOR('',#18527,10.);
#4902=VECTOR('',#18532,10.);
#4903=VECTOR('',#18537,10.);
#4904=VECTOR('',#18538,10.);
#4905=VECTOR('',#18539,10.);
#4906=VECTOR('',#18548,10.);
#4907=VECTOR('',#18549,10.);
#4908=VECTOR('',#18550,10.);
#4909=VECTOR('',#18551,10.);
#4910=VECTOR('',#18556,10.);
#4911=VECTOR('',#18561,10.);
#4912=VECTOR('',#18562,10.);
#4913=VECTOR('',#18563,10.);
#4914=VECTOR('',#18568,10.);
#4915=VECTOR('',#18573,10.);
#4916=VECTOR('',#18574,10.);
#4917=VECTOR('',#18575,10.);
#4918=VECTOR('',#18580,10.);
#4919=VECTOR('',#18585,10.);
#4920=VECTOR('',#18586,10.);
#4921=VECTOR('',#18587,10.);
#4922=VECTOR('',#18596,10.);
#4923=VECTOR('',#18597,10.);
#4924=VECTOR('',#18598,10.);
#4925=VECTOR('',#18599,10.);
#4926=VECTOR('',#18604,10.);
#4927=VECTOR('',#18609,10.);
#4928=VECTOR('',#18610,10.);
#4929=VECTOR('',#18611,10.);
#4930=VECTOR('',#18616,10.);
#4931=VECTOR('',#18621,10.);
#4932=VECTOR('',#18622,10.);
#4933=VECTOR('',#18623,10.);
#4934=VECTOR('',#18628,10.);
#4935=VECTOR('',#18633,10.);
#4936=VECTOR('',#18634,10.);
#4937=VECTOR('',#18635,10.);
#4938=VECTOR('',#18644,10.);
#4939=VECTOR('',#18645,10.);
#4940=VECTOR('',#18646,10.);
#4941=VECTOR('',#18647,10.);
#4942=VECTOR('',#18652,10.);
#4943=VECTOR('',#18657,10.);
#4944=VECTOR('',#18658,10.);
#4945=VECTOR('',#18659,10.);
#4946=VECTOR('',#18664,10.);
#4947=VECTOR('',#18669,10.);
#4948=VECTOR('',#18670,10.);
#4949=VECTOR('',#18671,10.);
#4950=VECTOR('',#18676,10.);
#4951=VECTOR('',#18681,10.);
#4952=VECTOR('',#18682,10.);
#4953=VECTOR('',#18683,10.);
#4954=VECTOR('',#18692,10.);
#4955=VECTOR('',#18693,10.);
#4956=VECTOR('',#18694,10.);
#4957=VECTOR('',#18695,10.);
#4958=VECTOR('',#18700,10.);
#4959=VECTOR('',#18705,10.);
#4960=VECTOR('',#18706,10.);
#4961=VECTOR('',#18707,10.);
#4962=VECTOR('',#18712,10.);
#4963=VECTOR('',#18717,10.);
#4964=VECTOR('',#18718,10.);
#4965=VECTOR('',#18719,10.);
#4966=VECTOR('',#18724,10.);
#4967=VECTOR('',#18729,10.);
#4968=VECTOR('',#18730,10.);
#4969=VECTOR('',#18731,10.);
#4970=VECTOR('',#18740,10.);
#4971=VECTOR('',#18741,10.);
#4972=VECTOR('',#18742,10.);
#4973=VECTOR('',#18743,10.);
#4974=VECTOR('',#18748,10.);
#4975=VECTOR('',#18753,10.);
#4976=VECTOR('',#18754,10.);
#4977=VECTOR('',#18755,10.);
#4978=VECTOR('',#18760,10.);
#4979=VECTOR('',#18765,10.);
#4980=VECTOR('',#18766,10.);
#4981=VECTOR('',#18767,10.);
#4982=VECTOR('',#18772,10.);
#4983=VECTOR('',#18777,10.);
#4984=VECTOR('',#18778,10.);
#4985=VECTOR('',#18779,10.);
#4986=VECTOR('',#18788,10.);
#4987=VECTOR('',#18789,10.);
#4988=VECTOR('',#18790,10.);
#4989=VECTOR('',#18791,10.);
#4990=VECTOR('',#18796,10.);
#4991=VECTOR('',#18801,10.);
#4992=VECTOR('',#18802,10.);
#4993=VECTOR('',#18803,10.);
#4994=VECTOR('',#18808,10.);
#4995=VECTOR('',#18813,10.);
#4996=VECTOR('',#18814,10.);
#4997=VECTOR('',#18815,10.);
#4998=VECTOR('',#18820,10.);
#4999=VECTOR('',#18825,10.);
#5000=VECTOR('',#18826,10.);
#5001=VECTOR('',#18827,10.);
#5002=VECTOR('',#18836,10.);
#5003=VECTOR('',#18837,10.);
#5004=VECTOR('',#18838,10.);
#5005=VECTOR('',#18839,10.);
#5006=VECTOR('',#18844,10.);
#5007=VECTOR('',#18849,10.);
#5008=VECTOR('',#18850,10.);
#5009=VECTOR('',#18851,10.);
#5010=VECTOR('',#18856,10.);
#5011=VECTOR('',#18861,10.);
#5012=VECTOR('',#18862,10.);
#5013=VECTOR('',#18863,10.);
#5014=VECTOR('',#18868,10.);
#5015=VECTOR('',#18873,10.);
#5016=VECTOR('',#18874,10.);
#5017=VECTOR('',#18875,10.);
#5018=VECTOR('',#18884,10.);
#5019=VECTOR('',#18885,10.);
#5020=VECTOR('',#18886,10.);
#5021=VECTOR('',#18887,10.);
#5022=VECTOR('',#18892,10.);
#5023=VECTOR('',#18897,10.);
#5024=VECTOR('',#18898,10.);
#5025=VECTOR('',#18899,10.);
#5026=VECTOR('',#18904,10.);
#5027=VECTOR('',#18909,10.);
#5028=VECTOR('',#18910,10.);
#5029=VECTOR('',#18911,10.);
#5030=VECTOR('',#18916,10.);
#5031=VECTOR('',#18921,10.);
#5032=VECTOR('',#18922,10.);
#5033=VECTOR('',#18923,10.);
#5034=VECTOR('',#18932,10.);
#5035=VECTOR('',#18933,10.);
#5036=VECTOR('',#18934,10.);
#5037=VECTOR('',#18935,10.);
#5038=VECTOR('',#18940,10.);
#5039=VECTOR('',#18945,10.);
#5040=VECTOR('',#18946,10.);
#5041=VECTOR('',#18947,10.);
#5042=VECTOR('',#18952,10.);
#5043=VECTOR('',#18957,10.);
#5044=VECTOR('',#18958,10.);
#5045=VECTOR('',#18959,10.);
#5046=VECTOR('',#18964,10.);
#5047=VECTOR('',#18969,10.);
#5048=VECTOR('',#18970,10.);
#5049=VECTOR('',#18971,10.);
#5050=VECTOR('',#18980,10.);
#5051=VECTOR('',#18981,10.);
#5052=VECTOR('',#18982,10.);
#5053=VECTOR('',#18983,10.);
#5054=VECTOR('',#18988,10.);
#5055=VECTOR('',#18993,10.);
#5056=VECTOR('',#18994,10.);
#5057=VECTOR('',#18995,10.);
#5058=VECTOR('',#19000,10.);
#5059=VECTOR('',#19005,10.);
#5060=VECTOR('',#19006,10.);
#5061=VECTOR('',#19007,10.);
#5062=VECTOR('',#19012,10.);
#5063=VECTOR('',#19017,10.);
#5064=VECTOR('',#19018,10.);
#5065=VECTOR('',#19019,10.);
#5066=VECTOR('',#19028,10.);
#5067=VECTOR('',#19029,10.);
#5068=VECTOR('',#19030,10.);
#5069=VECTOR('',#19031,10.);
#5070=VECTOR('',#19036,10.);
#5071=VECTOR('',#19041,10.);
#5072=VECTOR('',#19042,10.);
#5073=VECTOR('',#19043,10.);
#5074=VECTOR('',#19048,10.);
#5075=VECTOR('',#19053,10.);
#5076=VECTOR('',#19054,10.);
#5077=VECTOR('',#19055,10.);
#5078=VECTOR('',#19060,10.);
#5079=VECTOR('',#19065,10.);
#5080=VECTOR('',#19066,10.);
#5081=VECTOR('',#19067,10.);
#5082=VECTOR('',#19076,10.);
#5083=VECTOR('',#19077,10.);
#5084=VECTOR('',#19078,10.);
#5085=VECTOR('',#19079,10.);
#5086=VECTOR('',#19086,10.);
#5087=VECTOR('',#19089,10.);
#5088=VECTOR('',#19090,10.);
#5089=VECTOR('',#19091,10.);
#5090=VECTOR('',#19098,10.);
#5091=VECTOR('',#19101,10.);
#5092=VECTOR('',#19102,10.);
#5093=VECTOR('',#19103,10.);
#5094=VECTOR('',#19110,10.);
#5095=VECTOR('',#19113,10.);
#5096=VECTOR('',#19114,10.);
#5097=VECTOR('',#19115,10.);
#5098=VECTOR('',#19136,2.85);
#5099=VECTOR('',#19141,3.);
#5100=VECTOR('',#19144,2.85);
#5101=VECTOR('',#19153,1.99475);
#5102=VECTOR('',#19158,1.99475);
#5103=VECTOR('',#19161,1.99475);
#5104=VECTOR('',#19164,1.99475);
#5105=VECTOR('',#19167,1.99475);
#5106=VECTOR('',#19170,1.99475);
#5107=VECTOR('',#19173,1.99475);
#5108=VECTOR('',#19176,1.99475);
#5109=VECTOR('',#19179,1.99475);
#5110=VECTOR('',#19182,1.99475);
#5111=VECTOR('',#19185,1.99475);
#5112=VECTOR('',#19188,1.99475);
#5113=VECTOR('',#19191,1.99475);
#5114=VECTOR('',#19194,1.99475);
#5115=VECTOR('',#19197,1.99475);
#5116=VECTOR('',#19200,1.99475);
#5117=VECTOR('',#19203,1.99475);
#5118=VECTOR('',#19206,1.99475);
#5119=VECTOR('',#19209,1.99475);
#5120=VECTOR('',#19212,1.99475);
#5121=VECTOR('',#19215,1.99475);
#5122=VECTOR('',#19218,1.99475);
#5123=VECTOR('',#19221,1.99475);
#5124=VECTOR('',#19224,1.99475);
#5125=VECTOR('',#19259,2.2005);
#5126=VECTOR('',#19268,10.);
#5127=VECTOR('',#19269,10.);
#5128=VECTOR('',#19272,10.);
#5129=VECTOR('',#19273,10.);
#5130=VECTOR('',#19276,10.);
#5131=VECTOR('',#19281,4.25);
#5132=VECTOR('',#19286,10.);
#5133=VECTOR('',#19289,10.);
#5134=VECTOR('',#19292,10.);
#5135=VECTOR('',#19295,10.);
#5136=VECTOR('',#19298,10.);
#5137=VECTOR('',#19301,10.);
#5138=VECTOR('',#19304,10.);
#5139=VECTOR('',#19307,10.);
#5140=VECTOR('',#19310,10.);
#5141=VECTOR('',#19313,10.);
#5142=VECTOR('',#19316,10.);
#5143=VECTOR('',#19319,10.);
#5144=VECTOR('',#19322,10.);
#5145=VECTOR('',#19325,10.);
#5146=VECTOR('',#19328,10.);
#5147=VECTOR('',#19331,10.);
#5148=VECTOR('',#19334,10.);
#5149=VECTOR('',#19337,10.);
#5150=VECTOR('',#19340,10.);
#5151=VECTOR('',#19343,10.);
#5152=VECTOR('',#19346,10.);
#5153=VECTOR('',#19349,10.);
#5154=VECTOR('',#19352,10.);
#5155=VECTOR('',#19355,10.);
#5156=VECTOR('',#19358,10.);
#5157=VECTOR('',#19361,10.);
#5158=VECTOR('',#19364,10.);
#5159=VECTOR('',#19367,10.);
#5160=VECTOR('',#19370,10.);
#5161=VECTOR('',#19373,10.);
#5162=VECTOR('',#19376,10.);
#5163=VECTOR('',#19379,10.);
#5164=VECTOR('',#19382,10.);
#5165=VECTOR('',#19387,10.);
#5166=VECTOR('',#19390,10.);
#5167=VECTOR('',#19393,10.);
#5168=VECTOR('',#19396,10.);
#5169=VECTOR('',#19399,10.);
#5170=VECTOR('',#19402,10.);
#5171=VECTOR('',#19405,10.);
#5172=VECTOR('',#19408,10.);
#5173=VECTOR('',#19411,10.);
#5174=VECTOR('',#19414,10.);
#5175=VECTOR('',#19417,10.);
#5176=VECTOR('',#19420,10.);
#5177=VECTOR('',#19423,10.);
#5178=VECTOR('',#19426,10.);
#5179=VECTOR('',#19429,10.);
#5180=VECTOR('',#19432,10.);
#5181=VECTOR('',#19435,10.);
#5182=VECTOR('',#19438,10.);
#5183=VECTOR('',#19441,10.);
#5184=VECTOR('',#19444,10.);
#5185=VECTOR('',#19447,10.);
#5186=VECTOR('',#19450,10.);
#5187=VECTOR('',#19453,10.);
#5188=VECTOR('',#19456,10.);
#5189=VECTOR('',#19459,10.);
#5190=VECTOR('',#19462,10.);
#5191=VECTOR('',#19465,10.);
#5192=VECTOR('',#19468,10.);
#5193=VECTOR('',#19471,10.);
#5194=VECTOR('',#19474,10.);
#5195=VECTOR('',#19477,10.);
#5196=VECTOR('',#19480,10.);
#5197=VECTOR('',#19483,10.);
#5198=VECTOR('',#19486,10.);
#5199=VECTOR('',#19489,10.);
#5200=VECTOR('',#19492,10.);
#5201=VECTOR('',#19495,10.);
#5202=VECTOR('',#19498,10.);
#5203=VECTOR('',#19499,10.);
#5204=VECTOR('',#19502,10.);
#5205=VECTOR('',#19507,4.05);
#5206=VECTOR('',#19512,10.);
#5207=VECTOR('',#19513,10.);
#5208=VECTOR('',#19516,10.);
#5209=VECTOR('',#19521,10.);
#5210=VECTOR('',#19522,10.);
#5211=VECTOR('',#19525,10.);
#5212=VECTOR('',#19530,10.);
#5213=VECTOR('',#19531,10.);
#5214=VECTOR('',#19534,10.);
#5215=VECTOR('',#19539,10.);
#5216=VECTOR('',#19540,10.);
#5217=VECTOR('',#19543,10.);
#5218=VECTOR('',#19548,10.);
#5219=VECTOR('',#19549,9.99999999999999);
#5220=VECTOR('',#19552,10.);
#5221=VECTOR('',#19557,10.);
#5222=VECTOR('',#19558,10.);
#5223=VECTOR('',#19561,10.);
#5224=VECTOR('',#19566,10.);
#5225=VECTOR('',#19567,10.);
#5226=VECTOR('',#19570,10.);
#5227=VECTOR('',#19575,10.);
#5228=VECTOR('',#19576,10.);
#5229=VECTOR('',#19579,10.);
#5230=VECTOR('',#19584,10.);
#5231=VECTOR('',#19585,10.);
#5232=VECTOR('',#19588,10.);
#5233=VECTOR('',#19593,10.);
#5234=VECTOR('',#19594,10.);
#5235=VECTOR('',#19597,10.);
#5236=VECTOR('',#19602,10.);
#5237=VECTOR('',#19603,10.);
#5238=VECTOR('',#19606,10.);
#5239=VECTOR('',#19611,10.);
#5240=VECTOR('',#19612,10.);
#5241=VECTOR('',#19615,10.);
#5242=VECTOR('',#19620,10.);
#5243=VECTOR('',#19621,10.);
#5244=VECTOR('',#19624,10.);
#5245=VECTOR('',#19629,10.);
#5246=VECTOR('',#19630,10.);
#5247=VECTOR('',#19633,10.);
#5248=VECTOR('',#19638,10.);
#5249=VECTOR('',#19639,10.);
#5250=VECTOR('',#19642,10.);
#5251=VECTOR('',#19647,10.);
#5252=VECTOR('',#19648,10.);
#5253=VECTOR('',#19651,10.);
#5254=VECTOR('',#19656,10.);
#5255=VECTOR('',#19657,10.);
#5256=VECTOR('',#19660,10.);
#5257=VECTOR('',#19665,10.);
#5258=VECTOR('',#19666,10.);
#5259=VECTOR('',#19669,10.);
#5260=VECTOR('',#19674,10.);
#5261=VECTOR('',#19675,10.);
#5262=VECTOR('',#19678,10.);
#5263=VECTOR('',#19683,10.);
#5264=VECTOR('',#19684,10.);
#5265=VECTOR('',#19687,10.);
#5266=VECTOR('',#19692,10.);
#5267=VECTOR('',#19693,10.);
#5268=VECTOR('',#19696,10.);
#5269=VECTOR('',#19701,10.);
#5270=VECTOR('',#19702,10.);
#5271=VECTOR('',#19705,10.);
#5272=VECTOR('',#19710,10.);
#5273=VECTOR('',#19711,10.);
#5274=VECTOR('',#19714,10.);
#5275=VECTOR('',#19719,10.);
#5276=VECTOR('',#19720,10.);
#5277=VECTOR('',#19723,10.);
#5278=VECTOR('',#19728,10.);
#5279=VECTOR('',#19729,10.);
#5280=VECTOR('',#19732,10.);
#5281=VECTOR('',#19737,10.);
#5282=VECTOR('',#19738,10.);
#5283=VECTOR('',#19741,10.);
#5284=VECTOR('',#19746,10.);
#5285=VECTOR('',#19747,10.);
#5286=VECTOR('',#19750,10.);
#5287=VECTOR('',#19755,10.);
#5288=VECTOR('',#19756,10.);
#5289=VECTOR('',#19759,10.);
#5290=VECTOR('',#19764,10.);
#5291=VECTOR('',#19765,10.);
#5292=VECTOR('',#19768,10.);
#5293=VECTOR('',#19773,10.);
#5294=VECTOR('',#19774,10.);
#5295=VECTOR('',#19777,10.);
#5296=VECTOR('',#19782,10.);
#5297=VECTOR('',#19783,10.);
#5298=VECTOR('',#19786,10.);
#5299=VECTOR('',#19791,10.);
#5300=VECTOR('',#19792,10.);
#5301=VECTOR('',#19795,10.);
#5302=VECTOR('',#19800,10.);
#5303=VECTOR('',#19801,10.);
#5304=VECTOR('',#19804,10.);
#5305=VECTOR('',#19809,10.);
#5306=VECTOR('',#19810,10.);
#5307=VECTOR('',#19813,10.);
#5308=VECTOR('',#19838,2.40940107675851);
#5309=VECTOR('',#19841,10.);
#5310=VECTOR('',#19842,10.);
#5311=VECTOR('',#19847,10.);
#5312=VECTOR('',#19848,10.);
#5313=VECTOR('',#19853,10.);
#5314=VECTOR('',#19856,10.);
#5315=VECTOR('',#19859,10.);
#5316=VECTOR('',#19860,10.);
#5317=VECTOR('',#19865,10.);
#5318=VECTOR('',#19868,10.);
#5319=VECTOR('',#19871,10.);
#5320=VECTOR('',#19874,10.);
#5321=VECTOR('',#19877,10.);
#5322=VECTOR('',#19878,10.);
#5323=VECTOR('',#19879,10.);
#5324=VECTOR('',#19880,10.);
#5325=VECTOR('',#19883,10.);
#5326=VECTOR('',#19884,10.);
#5327=VECTOR('',#19885,10.);
#5328=VECTOR('',#19888,10.);
#5329=VECTOR('',#19889,10.);
#5330=VECTOR('',#19890,10.);
#5331=VECTOR('',#19897,10.);
#5332=VECTOR('',#19902,10.);
#5333=VECTOR('',#19905,10.);
#5334=VECTOR('',#19908,10.);
#5335=VECTOR('',#19925,10.);
#5336=VECTOR('',#19930,10.);
#5337=VECTOR('',#19935,2.30940107675851);
#5338=VECTOR('',#19938,10.);
#5339=VECTOR('',#19941,10.);
#5340=VECTOR('',#19948,1.99475);
#5341=VECTOR('',#19953,1.99475);
#5342=VECTOR('',#19956,1.99475);
#5343=VECTOR('',#19959,1.99475);
#5344=VECTOR('',#19962,1.99475);
#5345=VECTOR('',#19965,1.99475);
#5346=VECTOR('',#19968,1.99475);
#5347=VECTOR('',#19971,1.99475);
#5348=VECTOR('',#19974,1.99475);
#5349=VECTOR('',#19977,1.99475);
#5350=VECTOR('',#19980,1.99475);
#5351=VECTOR('',#19983,1.99475);
#5352=VECTOR('',#19986,1.99475);
#5353=VECTOR('',#19989,1.99475);
#5354=VECTOR('',#19992,1.99475);
#5355=VECTOR('',#19995,1.99475);
#5356=VECTOR('',#19998,1.99475);
#5357=VECTOR('',#20001,1.99475);
#5358=VECTOR('',#20004,1.99475);
#5359=VECTOR('',#20007,1.99475);
#5360=VECTOR('',#20010,1.99475);
#5361=VECTOR('',#20013,1.99475);
#5362=VECTOR('',#20016,1.99475);
#5363=VECTOR('',#20053,1.49337567297406);
#5364=VECTOR('',#20058,10.);
#5365=VECTOR('',#20059,10.);
#5366=VECTOR('',#20064,10.);
#5367=VECTOR('',#20065,10.);
#5368=VECTOR('',#20070,10.);
#5369=VECTOR('',#20073,10.);
#5370=VECTOR('',#20076,10.);
#5371=VECTOR('',#20077,10.);
#5372=VECTOR('',#20082,10.);
#5373=VECTOR('',#20085,10.);
#5374=VECTOR('',#20088,10.);
#5375=VECTOR('',#20091,10.);
#5376=VECTOR('',#20094,10.);
#5377=VECTOR('',#20095,10.);
#5378=VECTOR('',#20096,10.);
#5379=VECTOR('',#20097,10.);
#5380=VECTOR('',#20100,10.);
#5381=VECTOR('',#20101,10.);
#5382=VECTOR('',#20102,10.);
#5383=VECTOR('',#20105,10.);
#5384=VECTOR('',#20106,10.);
#5385=VECTOR('',#20107,10.);
#5386=VECTOR('',#20114,10.);
#5387=VECTOR('',#20119,10.);
#5388=VECTOR('',#20122,10.);
#5389=VECTOR('',#20125,10.);
#5390=VECTOR('',#20142,10.);
#5391=VECTOR('',#20147,10.);
#5392=VECTOR('',#20152,1.44337567297407);
#5393=VECTOR('',#20155,10.);
#5394=VECTOR('',#20158,10.);
#5395=VECTOR('',#20167,2.26);
#5396=VECTOR('',#20170,2.125);
#5397=VECTOR('',#20179,1.99475);
#5398=VECTOR('',#20184,1.99475);
#5399=VECTOR('',#20189,1.99475);
#5400=VECTOR('',#20192,1.99475);
#5401=VECTOR('',#20195,1.99475);
#5402=VECTOR('',#20198,1.99475);
#5403=VECTOR('',#20201,1.99475);
#5404=VECTOR('',#20204,1.99475);
#5405=VECTOR('',#20207,1.99475);
#5406=VECTOR('',#20210,1.99475);
#5407=VECTOR('',#20213,2.25);
#5408=VECTOR('',#20254,10.);
#5409=VECTOR('',#20259,10.);
#5410=VECTOR('',#20264,10.);
#5411=VECTOR('',#20269,10.);
#5412=VECTOR('',#20274,10.);
#5413=VECTOR('',#20279,10.);
#5414=VECTOR('',#20284,0.866025403784438);
#5415=VECTOR('',#20289,10.);
#5416=VECTOR('',#20290,10.);
#5417=VECTOR('',#20295,10.);
#5418=VECTOR('',#20300,10.);
#5419=VECTOR('',#20305,10.);
#5420=VECTOR('',#20310,10.);
#5421=VECTOR('',#20319,4.75);
#5422=VECTOR('',#20328,1.17775);
#5423=VECTOR('',#20333,1.17775);
#5424=VECTOR('',#20338,1.17775);
#5425=VECTOR('',#20341,1.17775);
#5426=VECTOR('',#20344,1.17775);
#5427=VECTOR('',#20347,1.17775);
#5428=VECTOR('',#20350,1.17775);
#5429=VECTOR('',#20353,1.17775);
#5430=VECTOR('',#20356,1.17775);
#5431=VECTOR('',#20359,1.17775);
#5432=VECTOR('',#20362,1.17775);
#5433=VECTOR('',#20365,1.17775);
#5434=VECTOR('',#20396,10.);
#5435=VECTOR('',#20399,10.);
#5436=VECTOR('',#20404,10.);
#5437=VECTOR('',#20405,10.);
#5438=VECTOR('',#20406,10.);
#5439=VECTOR('',#20409,10.);
#5440=VECTOR('',#20410,10.);
#5441=VECTOR('',#20411,10.);
#5442=VECTOR('',#20414,2.75);
#5443=VECTOR('',#20435,1.325);
#5444=CIRCLE('',#15208,2.74999999999999);
#5445=CIRCLE('',#15209,3.05);
#5446=CIRCLE('',#15211,3.05);
#5447=CIRCLE('',#15212,3.05);
#5448=CIRCLE('',#15213,3.05);
#5449=CIRCLE('',#15215,2.74999999999999);
#5450=CIRCLE('',#15217,2.75);
#5451=CIRCLE('',#15219,2.75);
#5452=CIRCLE('',#15221,2.75);
#5453=CIRCLE('',#15223,2.75);
#5454=CIRCLE('',#15225,2.75);
#5455=CIRCLE('',#15227,2.75);
#5456=CIRCLE('',#15229,2.74999999999999);
#5457=CIRCLE('',#15230,3.05);
#5458=CIRCLE('',#15232,3.05);
#5459=CIRCLE('',#15233,3.05);
#5460=CIRCLE('',#15234,3.05);
#5461=CIRCLE('',#15236,2.74999999999999);
#5462=CIRCLE('',#15238,2.75);
#5463=CIRCLE('',#15240,2.75);
#5464=CIRCLE('',#15242,2.75);
#5465=CIRCLE('',#15244,2.75);
#5466=CIRCLE('',#15246,2.75);
#5467=CIRCLE('',#15248,2.75);
#5468=CIRCLE('',#15250,3.05);
#5469=CIRCLE('',#15251,3.44999999999999);
#5470=CIRCLE('',#15253,3.44999999999999);
#5471=CIRCLE('',#15254,3.45);
#5472=CIRCLE('',#15255,3.45);
#5473=CIRCLE('',#15256,3.44999999999999);
#5474=CIRCLE('',#15257,3.44999999999999);
#5475=CIRCLE('',#15258,3.45);
#5476=CIRCLE('',#15259,3.45);
#5477=CIRCLE('',#15261,3.05);
#5478=CIRCLE('',#15263,3.05);
#5479=CIRCLE('',#15265,3.05);
#5480=CIRCLE('',#15267,3.05);
#5481=CIRCLE('',#15269,3.05);
#5482=CIRCLE('',#15271,3.05);
#5483=CIRCLE('',#15273,3.05);
#5484=CIRCLE('',#15275,3.05);
#5485=CIRCLE('',#15277,3.05);
#5486=CIRCLE('',#15279,3.05);
#5487=CIRCLE('',#15281,3.05);
#5488=CIRCLE('',#15283,3.05);
#5489=CIRCLE('',#15285,3.05);
#5490=CIRCLE('',#15287,3.05);
#5491=CIRCLE('',#15289,3.05);
#5492=CIRCLE('',#15329,2.55000000000001);
#5493=CIRCLE('',#15330,2.85);
#5494=CIRCLE('',#15331,2.85);
#5495=CIRCLE('',#15333,5.);
#5496=CIRCLE('',#15334,5.30000000000001);
#5497=CIRCLE('',#15335,5.30000000000001);
#5498=CIRCLE('',#15337,2.55000000000001);
#5499=CIRCLE('',#15339,2.55000000000001);
#5500=CIRCLE('',#15340,2.85);
#5501=CIRCLE('',#15341,2.85);
#5502=CIRCLE('',#15343,5.);
#5503=CIRCLE('',#15344,5.29999999999999);
#5504=CIRCLE('',#15345,5.29999999999999);
#5505=CIRCLE('',#15347,2.55000000000001);
#5506=CIRCLE('',#15349,2.55);
#5507=CIRCLE('',#15350,2.85);
#5508=CIRCLE('',#15351,2.85);
#5509=CIRCLE('',#15353,5.);
#5510=CIRCLE('',#15354,5.3);
#5511=CIRCLE('',#15355,5.3);
#5512=CIRCLE('',#15357,2.55);
#5513=CIRCLE('',#15360,5.);
#5514=CIRCLE('',#15362,5.);
#5515=CIRCLE('',#15364,5.);
#5516=CIRCLE('',#15366,3.);
#5517=CIRCLE('',#15368,3.00000000000001);
#5518=CIRCLE('',#15370,3.00000000000001);
#5519=CIRCLE('',#15372,3.);
#5520=CIRCLE('',#15374,3.00000000000001);
#5521=CIRCLE('',#15376,3.00000000000001);
#5522=CIRCLE('',#15378,2.55000000000001);
#5523=CIRCLE('',#15379,2.85);
#5524=CIRCLE('',#15380,2.85);
#5525=CIRCLE('',#15382,5.);
#5526=CIRCLE('',#15383,5.30000000000001);
#5527=CIRCLE('',#15384,5.30000000000001);
#5528=CIRCLE('',#15386,2.55000000000001);
#5529=CIRCLE('',#15388,2.55000000000001);
#5530=CIRCLE('',#15389,2.85);
#5531=CIRCLE('',#15390,2.85);
#5532=CIRCLE('',#15392,5.);
#5533=CIRCLE('',#15393,5.29999999999999);
#5534=CIRCLE('',#15394,5.29999999999999);
#5535=CIRCLE('',#15396,2.55000000000001);
#5536=CIRCLE('',#15398,2.55);
#5537=CIRCLE('',#15399,2.85);
#5538=CIRCLE('',#15400,2.85);
#5539=CIRCLE('',#15402,5.);
#5540=CIRCLE('',#15403,5.3);
#5541=CIRCLE('',#15404,5.3);
#5542=CIRCLE('',#15406,2.55);
#5543=CIRCLE('',#15409,5.);
#5544=CIRCLE('',#15411,5.);
#5545=CIRCLE('',#15413,5.);
#5546=CIRCLE('',#15415,3.);
#5547=CIRCLE('',#15417,3.00000000000001);
#5548=CIRCLE('',#15419,3.00000000000001);
#5549=CIRCLE('',#15421,3.);
#5550=CIRCLE('',#15423,3.00000000000001);
#5551=CIRCLE('',#15425,3.00000000000001);
#5552=CIRCLE('',#15427,2.05);
#5553=CIRCLE('',#15428,2.34999999999999);
#5554=CIRCLE('',#15430,2.35);
#5555=CIRCLE('',#15431,2.35);
#5556=CIRCLE('',#15432,2.35);
#5557=CIRCLE('',#15434,2.05);
#5558=CIRCLE('',#15435,2.05);
#5559=CIRCLE('',#15437,2.05);
#5560=CIRCLE('',#15439,2.05);
#5561=CIRCLE('',#15440,2.05);
#5562=CIRCLE('',#15442,2.05);
#5563=CIRCLE('',#15444,2.05);
#5564=CIRCLE('',#15445,2.05);
#5565=CIRCLE('',#15447,2.05);
#5566=CIRCLE('',#15449,2.05);
#5567=CIRCLE('',#15450,2.05);
#5568=CIRCLE('',#15456,2.05);
#5569=CIRCLE('',#15457,2.34999999999999);
#5570=CIRCLE('',#15459,2.35);
#5571=CIRCLE('',#15460,2.35);
#5572=CIRCLE('',#15461,2.35);
#5573=CIRCLE('',#15463,2.05);
#5574=CIRCLE('',#15464,2.05);
#5575=CIRCLE('',#15466,2.05);
#5576=CIRCLE('',#15468,2.05);
#5577=CIRCLE('',#15469,2.05);
#5578=CIRCLE('',#15471,2.05);
#5579=CIRCLE('',#15473,2.05);
#5580=CIRCLE('',#15474,2.05);
#5581=CIRCLE('',#15476,2.05);
#5582=CIRCLE('',#15478,2.05);
#5583=CIRCLE('',#15479,2.05);
#5584=CIRCLE('',#15485,3.05);
#5585=CIRCLE('',#15486,3.44999999999999);
#5586=CIRCLE('',#15488,3.44999999999999);
#5587=CIRCLE('',#15489,3.45);
#5588=CIRCLE('',#15490,3.44999999999999);
#5589=CIRCLE('',#15491,5.80000000000002);
#5590=CIRCLE('',#15492,5.8);
#5591=CIRCLE('',#15493,5.8);
#5592=CIRCLE('',#15494,5.8);
#5593=CIRCLE('',#15495,5.80000000000002);
#5594=CIRCLE('',#15496,5.8);
#5595=CIRCLE('',#15497,5.8);
#5596=CIRCLE('',#15498,5.8);
#5597=CIRCLE('',#15499,3.45);
#5598=CIRCLE('',#15500,3.44999999999999);
#5599=CIRCLE('',#15502,3.05);
#5600=CIRCLE('',#15504,3.05);
#5601=CIRCLE('',#15506,3.05);
#5602=CIRCLE('',#15508,3.05);
#5603=CIRCLE('',#15510,3.05);
#5604=CIRCLE('',#15512,3.05);
#5605=CIRCLE('',#15514,3.05);
#5606=CIRCLE('',#15516,3.05);
#5607=CIRCLE('',#15518,3.05);
#5608=CIRCLE('',#15520,3.05);
#5609=CIRCLE('',#15522,3.05);
#5610=CIRCLE('',#15530,5.50000000000001);
#5611=CIRCLE('',#15532,5.50000000000001);
#5612=CIRCLE('',#15534,5.50000000000001);
#5613=CIRCLE('',#15536,5.50000000000001);
#5614=CIRCLE('',#15538,5.5);
#5615=CIRCLE('',#15540,5.5);
#5616=CIRCLE('',#15542,5.50000000000001);
#5617=CIRCLE('',#15544,5.50000000000001);
#5618=CIRCLE('',#15546,5.5);
#5619=CIRCLE('',#15548,5.5);
#5620=CIRCLE('',#15550,5.50000000000001);
#5621=CIRCLE('',#15552,5.50000000000001);
#5622=CIRCLE('',#15554,5.50000000000001);
#5623=CIRCLE('',#15556,5.50000000000001);
#5624=CIRCLE('',#15558,5.50000000000001);
#5625=CIRCLE('',#15560,5.50000000000001);
#5626=CIRCLE('',#15562,3.50000000000001);
#5627=CIRCLE('',#15564,3.5);
#5628=CIRCLE('',#15566,3.5);
#5629=CIRCLE('',#15568,3.5);
#5630=CIRCLE('',#15570,3.5);
#5631=CIRCLE('',#15572,3.5);
#5632=CIRCLE('',#15574,3.5);
#5633=CIRCLE('',#15576,3.50000000000001);
#5634=CIRCLE('',#15578,3.50000000000001);
#5635=CIRCLE('',#15580,3.5);
#5636=CIRCLE('',#15582,3.5);
#5637=CIRCLE('',#15584,3.5);
#5638=CIRCLE('',#15586,3.5);
#5639=CIRCLE('',#15588,3.5);
#5640=CIRCLE('',#15590,3.5);
#5641=CIRCLE('',#15592,3.50000000000001);
#5642=CIRCLE('',#15616,1.55);
#5643=CIRCLE('',#15617,1.75);
#5644=CIRCLE('',#15620,1.55);
#5645=CIRCLE('',#15621,1.55);
#5646=CIRCLE('',#15624,1.55);
#5647=CIRCLE('',#15625,1.75);
#5648=CIRCLE('',#15628,1.55);
#5649=CIRCLE('',#15629,1.55);
#5650=CIRCLE('',#15632,2.55000000000001);
#5651=CIRCLE('',#15633,2.85);
#5652=CIRCLE('',#15635,2.85);
#5653=CIRCLE('',#15636,2.85);
#5654=CIRCLE('',#15638,2.55000000000001);
#5655=CIRCLE('',#15640,2.55000000000001);
#5656=CIRCLE('',#15642,2.55000000000001);
#5657=CIRCLE('',#15644,2.55000000000001);
#5658=CIRCLE('',#15646,2.55000000000001);
#5659=CIRCLE('',#15648,2.55000000000001);
#5660=CIRCLE('',#15650,2.55000000000001);
#5661=CIRCLE('',#15652,2.55000000000001);
#5662=CIRCLE('',#15654,2.55000000000001);
#5663=CIRCLE('',#15656,2.55000000000001);
#5664=CIRCLE('',#15658,2.55000000000001);
#5665=CIRCLE('',#15660,2.55);
#5666=CIRCLE('',#15662,2.55);
#5667=CIRCLE('',#15664,2.55);
#5668=CIRCLE('',#15666,2.55);
#5669=CIRCLE('',#15668,2.55);
#5670=CIRCLE('',#15670,2.55);
#5671=CIRCLE('',#15707,1.55);
#5672=CIRCLE('',#15708,1.75);
#5673=CIRCLE('',#15709,1.75);
#5674=CIRCLE('',#15712,1.55);
#5675=CIRCLE('',#15713,1.55);
#5676=CIRCLE('',#15716,1.55);
#5677=CIRCLE('',#15717,1.75);
#5678=CIRCLE('',#15718,1.75);
#5679=CIRCLE('',#15721,1.55);
#5680=CIRCLE('',#15722,1.55);
#5681=CIRCLE('',#15725,2.54999999999999);
#5682=CIRCLE('',#15726,2.85);
#5683=CIRCLE('',#15728,2.85);
#5684=CIRCLE('',#15729,2.85);
#5685=CIRCLE('',#15730,2.85);
#5686=CIRCLE('',#15732,2.54999999999999);
#5687=CIRCLE('',#15734,2.54999999999999);
#5688=CIRCLE('',#15736,2.54999999999999);
#5689=CIRCLE('',#15738,2.54999999999999);
#5690=CIRCLE('',#15740,2.54999999999999);
#5691=CIRCLE('',#15742,2.55);
#5692=CIRCLE('',#15744,2.55);
#5693=CIRCLE('',#15746,2.55);
#5694=CIRCLE('',#15748,2.55);
#5695=CIRCLE('',#15750,2.55);
#5696=CIRCLE('',#15752,2.55);
#5697=CIRCLE('',#15754,2.55000000000001);
#5698=CIRCLE('',#15756,2.55000000000001);
#5699=CIRCLE('',#15758,2.55000000000001);
#5700=CIRCLE('',#15760,2.55000000000001);
#5701=CIRCLE('',#15762,2.55000000000001);
#5702=CIRCLE('',#15764,2.55000000000001);
#5703=CIRCLE('',#15766,2.55000000000001);
#5704=CIRCLE('',#15768,2.55000000000001);
#5705=CIRCLE('',#15770,2.55000000000001);
#5706=CIRCLE('',#15772,2.55000000000001);
#5707=CIRCLE('',#15774,2.55000000000001);
#5708=CIRCLE('',#15776,2.55000000000001);
#5709=CIRCLE('',#15819,0.400000000000027);
#5710=CIRCLE('',#15820,0.400000000000027);
#5711=CIRCLE('',#15823,0.399999999999956);
#5712=CIRCLE('',#15824,0.399999999999956);
#5713=CIRCLE('',#15827,0.399999999999945);
#5714=CIRCLE('',#15828,0.399999999999945);
#5715=CIRCLE('',#15831,0.400000000000027);
#5716=CIRCLE('',#15832,0.400000000000027);
#5717=CIRCLE('',#15835,0.399999999999996);
#5718=CIRCLE('',#15836,0.399999999999996);
#5719=CIRCLE('',#15839,0.4);
#5720=CIRCLE('',#15840,0.4);
#5721=CIRCLE('',#15843,0.399999999999996);
#5722=CIRCLE('',#15844,0.399999999999996);
#5723=CIRCLE('',#15847,0.399999999999996);
#5724=CIRCLE('',#15848,0.399999999999996);
#5725=CIRCLE('',#15851,0.600000000000005);
#5726=CIRCLE('',#15852,0.600000000000005);
#5727=CIRCLE('',#15855,0.600000000000005);
#5728=CIRCLE('',#15856,0.600000000000005);
#5729=CIRCLE('',#15859,0.600000000000005);
#5730=CIRCLE('',#15860,0.600000000000005);
#5731=CIRCLE('',#15863,0.600000000000005);
#5732=CIRCLE('',#15864,0.600000000000005);
#5733=CIRCLE('',#15867,0.600000000000005);
#5734=CIRCLE('',#15868,0.600000000000005);
#5735=CIRCLE('',#15871,0.600000000000005);
#5736=CIRCLE('',#15872,0.600000000000005);
#5737=CIRCLE('',#15875,0.600000000000005);
#5738=CIRCLE('',#15876,0.600000000000005);
#5739=CIRCLE('',#15879,0.600000000000005);
#5740=CIRCLE('',#15880,0.600000000000005);
#5741=CIRCLE('',#15883,0.599999999999987);
#5742=CIRCLE('',#15884,0.599999999999987);
#5743=CIRCLE('',#15887,0.599999999999987);
#5744=CIRCLE('',#15888,0.599999999999987);
#5745=CIRCLE('',#15891,0.599999999999987);
#5746=CIRCLE('',#15892,0.599999999999987);
#5747=CIRCLE('',#15895,0.599999999999987);
#5748=CIRCLE('',#15896,0.599999999999987);
#5749=CIRCLE('',#15899,0.599999999999987);
#5750=CIRCLE('',#15900,0.599999999999987);
#5751=CIRCLE('',#15903,0.599999999999987);
#5752=CIRCLE('',#15904,0.599999999999987);
#5753=CIRCLE('',#15907,0.599999999999987);
#5754=CIRCLE('',#15908,0.599999999999987);
#5755=CIRCLE('',#15911,0.599999999999987);
#5756=CIRCLE('',#15912,0.599999999999987);
#5757=CIRCLE('',#15915,0.599999999999987);
#5758=CIRCLE('',#15916,0.599999999999987);
#5759=CIRCLE('',#15919,0.599999999999987);
#5760=CIRCLE('',#15920,0.599999999999987);
#5761=CIRCLE('',#15923,0.599999999999987);
#5762=CIRCLE('',#15924,0.599999999999987);
#5763=CIRCLE('',#15927,0.599999999999987);
#5764=CIRCLE('',#15928,0.599999999999987);
#5765=CIRCLE('',#15931,0.600000000000001);
#5766=CIRCLE('',#15932,0.600000000000001);
#5767=CIRCLE('',#15935,0.600000000000005);
#5768=CIRCLE('',#15936,0.600000000000005);
#5769=CIRCLE('',#15939,0.599999999999998);
#5770=CIRCLE('',#15940,0.599999999999998);
#5771=CIRCLE('',#15943,0.600000000000005);
#5772=CIRCLE('',#15944,0.600000000000005);
#5773=CIRCLE('',#15947,0.600000000000001);
#5774=CIRCLE('',#15948,0.600000000000001);
#5775=CIRCLE('',#15951,0.600000000000005);
#5776=CIRCLE('',#15952,0.600000000000005);
#5777=CIRCLE('',#15955,0.600000000000003);
#5778=CIRCLE('',#15956,0.600000000000003);
#5779=CIRCLE('',#15959,0.600000000000005);
#5780=CIRCLE('',#15960,0.600000000000005);
#5781=CIRCLE('',#15963,0.599999999999996);
#5782=CIRCLE('',#15964,0.599999999999996);
#5783=CIRCLE('',#15967,0.600000000000005);
#5784=CIRCLE('',#15968,0.600000000000005);
#5785=CIRCLE('',#15971,0.599999999999998);
#5786=CIRCLE('',#15972,0.599999999999998);
#5787=CIRCLE('',#15975,0.600000000000005);
#5788=CIRCLE('',#15976,0.600000000000005);
#5789=CIRCLE('',#15979,0.599999999999987);
#5790=CIRCLE('',#15980,0.599999999999987);
#5791=CIRCLE('',#15983,0.599999999999987);
#5792=CIRCLE('',#15984,0.599999999999987);
#5793=CIRCLE('',#15987,0.599999999999987);
#5794=CIRCLE('',#15988,0.599999999999987);
#5795=CIRCLE('',#15991,0.599999999999987);
#5796=CIRCLE('',#15992,0.599999999999987);
#5797=CIRCLE('',#15995,0.600000000000001);
#5798=CIRCLE('',#15996,0.600000000000001);
#5799=CIRCLE('',#15999,0.600000000000005);
#5800=CIRCLE('',#16000,0.600000000000005);
#5801=CIRCLE('',#16003,0.600000000000003);
#5802=CIRCLE('',#16004,0.600000000000003);
#5803=CIRCLE('',#16007,0.600000000000005);
#5804=CIRCLE('',#16008,0.600000000000005);
#5805=CIRCLE('',#16011,0.599999999999987);
#5806=CIRCLE('',#16012,0.599999999999987);
#5807=CIRCLE('',#16015,0.600000000000005);
#5808=CIRCLE('',#16016,0.600000000000005);
#5809=CIRCLE('',#16019,0.600000000000005);
#5810=CIRCLE('',#16020,0.600000000000005);
#5811=CIRCLE('',#16023,0.599999999999987);
#5812=CIRCLE('',#16024,0.599999999999987);
#5813=CIRCLE('',#16027,0.600000000000005);
#5814=CIRCLE('',#16028,0.600000000000005);
#5815=CIRCLE('',#16031,0.600000000000005);
#5816=CIRCLE('',#16032,0.600000000000005);
#5817=CIRCLE('',#16035,0.600000000000005);
#5818=CIRCLE('',#16036,0.600000000000005);
#5819=CIRCLE('',#16039,0.600000000000005);
#5820=CIRCLE('',#16040,0.600000000000005);
#5821=CIRCLE('',#16043,0.600000000000027);
#5822=CIRCLE('',#16044,0.600000000000027);
#5823=CIRCLE('',#16047,0.600000000000023);
#5824=CIRCLE('',#16048,0.600000000000023);
#5825=CIRCLE('',#16051,0.600000000000025);
#5826=CIRCLE('',#16052,0.600000000000025);
#5827=CIRCLE('',#16055,0.600000000000023);
#5828=CIRCLE('',#16056,0.600000000000023);
#5829=CIRCLE('',#16059,1.);
#5830=CIRCLE('',#16060,1.);
#5831=CIRCLE('',#16063,1.00000000000001);
#5832=CIRCLE('',#16064,1.00000000000001);
#5833=CIRCLE('',#16067,1.00000000000001);
#5834=CIRCLE('',#16068,1.00000000000001);
#5835=CIRCLE('',#16071,1.);
#5836=CIRCLE('',#16072,1.);
#5837=CIRCLE('',#16077,2.7);
#5838=CIRCLE('',#16079,3.);
#5839=CIRCLE('',#16081,3.);
#5840=CIRCLE('',#16083,2.7);
#5841=CIRCLE('',#16087,1.99475);
#5842=CIRCLE('',#16112,2.4505);
#5843=CIRCLE('',#16113,2.4505);
#5844=CIRCLE('',#16115,1.99475);
#5845=CIRCLE('',#16117,2.4505);
#5846=CIRCLE('',#16118,2.4505);
#5847=CIRCLE('',#16120,2.4505);
#5848=CIRCLE('',#16121,2.4505);
#5849=CIRCLE('',#16123,2.6505);
#5850=CIRCLE('',#16124,0.2);
#5851=CIRCLE('',#16126,4.05);
#5852=CIRCLE('',#16128,1.9505);
#5853=CIRCLE('',#16131,4.25);
#5854=CIRCLE('',#16135,4.25);
#5855=CIRCLE('',#16136,4.25);
#5856=CIRCLE('',#16137,4.25);
#5857=CIRCLE('',#16138,4.25);
#5858=CIRCLE('',#16139,4.25);
#5859=CIRCLE('',#16140,4.25);
#5860=CIRCLE('',#16141,4.25);
#5861=CIRCLE('',#16142,4.25);
#5862=CIRCLE('',#16143,4.25);
#5863=CIRCLE('',#16144,4.25);
#5864=CIRCLE('',#16145,4.25);
#5865=CIRCLE('',#16146,4.25);
#5866=CIRCLE('',#16147,4.25);
#5867=CIRCLE('',#16148,4.25);
#5868=CIRCLE('',#16149,4.25);
#5869=CIRCLE('',#16150,4.25);
#5870=CIRCLE('',#16151,4.25);
#5871=CIRCLE('',#16152,4.25);
#5872=CIRCLE('',#16153,4.25);
#5873=CIRCLE('',#16154,4.25);
#5874=CIRCLE('',#16155,4.25);
#5875=CIRCLE('',#16156,4.25);
#5876=CIRCLE('',#16157,4.25);
#5877=CIRCLE('',#16158,4.25);
#5878=CIRCLE('',#16159,4.25);
#5879=CIRCLE('',#16160,4.25);
#5880=CIRCLE('',#16161,4.25);
#5881=CIRCLE('',#16162,4.25);
#5882=CIRCLE('',#16163,4.25);
#5883=CIRCLE('',#16164,4.25);
#5884=CIRCLE('',#16165,4.25);
#5885=CIRCLE('',#16166,4.25);
#5886=CIRCLE('',#16167,4.25);
#5887=CIRCLE('',#16168,4.25);
#5888=CIRCLE('',#16169,4.25);
#5889=CIRCLE('',#16170,4.25);
#5890=CIRCLE('',#16171,4.25);
#5891=CIRCLE('',#16172,4.25);
#5892=CIRCLE('',#16173,4.25);
#5893=CIRCLE('',#16174,4.25);
#5894=CIRCLE('',#16175,4.25);
#5895=CIRCLE('',#16176,4.25);
#5896=CIRCLE('',#16177,4.25);
#5897=CIRCLE('',#16178,4.25);
#5898=CIRCLE('',#16179,4.25);
#5899=CIRCLE('',#16180,4.25);
#5900=CIRCLE('',#16181,4.25);
#5901=CIRCLE('',#16182,4.25);
#5902=CIRCLE('',#16183,4.25);
#5903=CIRCLE('',#16184,4.25);
#5904=CIRCLE('',#16185,4.25);
#5905=CIRCLE('',#16186,4.25);
#5906=CIRCLE('',#16187,4.25);
#5907=CIRCLE('',#16188,4.25);
#5908=CIRCLE('',#16189,4.25);
#5909=CIRCLE('',#16190,4.25);
#5910=CIRCLE('',#16191,4.25);
#5911=CIRCLE('',#16192,4.25);
#5912=CIRCLE('',#16193,4.25);
#5913=CIRCLE('',#16194,4.25);
#5914=CIRCLE('',#16195,4.25);
#5915=CIRCLE('',#16196,4.25);
#5916=CIRCLE('',#16197,4.25);
#5917=CIRCLE('',#16198,4.25);
#5918=CIRCLE('',#16199,4.25);
#5919=CIRCLE('',#16200,4.25);
#5920=CIRCLE('',#16201,4.25);
#5921=CIRCLE('',#16202,4.25);
#5922=CIRCLE('',#16203,4.25);
#5923=CIRCLE('',#16204,4.25);
#5924=CIRCLE('',#16205,4.25);
#5925=CIRCLE('',#16206,4.25);
#5926=CIRCLE('',#16207,4.25);
#5927=CIRCLE('',#16212,3.85);
#5928=CIRCLE('',#16316,0.2);
#5929=CIRCLE('',#16318,2.55940107675851);
#5930=CIRCLE('',#16320,2.2594010767585);
#5931=CIRCLE('',#16321,2.2594010767585);
#5932=CIRCLE('',#16322,2.2594010767585);
#5933=CIRCLE('',#16323,2.2594010767585);
#5934=CIRCLE('',#16324,2.2594010767585);
#5935=CIRCLE('',#16325,2.2594010767585);
#5936=CIRCLE('',#16327,2.2594010767585);
#5937=CIRCLE('',#16329,2.2594010767585);
#5938=CIRCLE('',#16331,2.2594010767585);
#5939=CIRCLE('',#16333,2.2594010767585);
#5940=CIRCLE('',#16335,2.2594010767585);
#5941=CIRCLE('',#16337,2.2594010767585);
#5942=CIRCLE('',#16348,2.30940107675851);
#5943=CIRCLE('',#16350,2.30940107675851);
#5944=CIRCLE('',#16352,2.30940107675851);
#5945=CIRCLE('',#16354,2.30940107675851);
#5946=CIRCLE('',#16356,2.30940107675851);
#5947=CIRCLE('',#16358,2.30940107675851);
#5948=CIRCLE('',#16365,1.99475);
#5949=CIRCLE('',#16389,2.4505);
#5950=CIRCLE('',#16390,2.4505);
#5951=CIRCLE('',#16392,1.99475);
#5952=CIRCLE('',#16394,2.4505);
#5953=CIRCLE('',#16395,2.4505);
#5954=CIRCLE('',#16397,2.4505);
#5955=CIRCLE('',#16398,2.4505);
#5956=CIRCLE('',#16400,1.39337567297407);
#5957=CIRCLE('',#16401,1.39337567297407);
#5958=CIRCLE('',#16402,1.39337567297407);
#5959=CIRCLE('',#16403,1.39337567297407);
#5960=CIRCLE('',#16404,1.39337567297407);
#5961=CIRCLE('',#16405,1.39337567297407);
#5962=CIRCLE('',#16406,1.59337567297406);
#5963=CIRCLE('',#16408,1.39337567297407);
#5964=CIRCLE('',#16410,1.39337567297407);
#5965=CIRCLE('',#16412,1.39337567297407);
#5966=CIRCLE('',#16414,1.39337567297407);
#5967=CIRCLE('',#16416,1.39337567297407);
#5968=CIRCLE('',#16418,1.39337567297407);
#5969=CIRCLE('',#16429,1.44337567297407);
#5970=CIRCLE('',#16431,1.44337567297407);
#5971=CIRCLE('',#16433,1.44337567297407);
#5972=CIRCLE('',#16435,1.44337567297407);
#5973=CIRCLE('',#16437,1.44337567297407);
#5974=CIRCLE('',#16439,1.44337567297407);
#5975=CIRCLE('',#16445,2.02);
#5976=CIRCLE('',#16448,1.75);
#5977=CIRCLE('',#16452,1.99475);
#5978=CIRCLE('',#16454,1.99475);
#5979=CIRCLE('',#16464,2.);
#5980=CIRCLE('',#16466,2.4505);
#5981=CIRCLE('',#16467,2.);
#5982=CIRCLE('',#16469,2.4505);
#5983=CIRCLE('',#16470,2.4505);
#5984=CIRCLE('',#16472,1.99475);
#5985=CIRCLE('',#16475,2.4505);
#5986=CIRCLE('',#16479,2.6505);
#5987=CIRCLE('',#16480,0.2);
#5988=CIRCLE('',#16482,4.75);
#5989=CIRCLE('',#16484,1.73205080756888);
#5990=CIRCLE('',#16486,1.73205080756888);
#5991=CIRCLE('',#16488,1.73205080756888);
#5992=CIRCLE('',#16490,1.73205080756888);
#5993=CIRCLE('',#16492,1.73205080756888);
#5994=CIRCLE('',#16494,1.73205080756888);
#5995=CIRCLE('',#16497,5.86614939355167);
#5996=CIRCLE('',#16499,5.86614939355167);
#5997=CIRCLE('',#16501,5.86614939355168);
#5998=CIRCLE('',#16503,5.86614939355169);
#5999=CIRCLE('',#16505,5.86614939355168);
#6000=CIRCLE('',#16507,5.86614939355169);
#6001=CIRCLE('',#16509,4.75);
#6002=CIRCLE('',#16511,6.05489130434781);
#6003=CIRCLE('',#16514,1.17775);
#6004=CIRCLE('',#16516,1.17775);
#6005=CIRCLE('',#16528,1.4635);
#6006=CIRCLE('',#16529,1.4635);
#6007=CIRCLE('',#16531,1.17775);
#6008=CIRCLE('',#16533,1.4635);
#6009=CIRCLE('',#16534,1.4635);
#6010=CIRCLE('',#16536,1.5635);
#6011=CIRCLE('',#16537,0.1);
#6012=CIRCLE('',#16539,2.75);
#6013=CIRCLE('',#16541,2.75);
#6014=CIRCLE('',#16542,2.75);
#6015=CIRCLE('',#16543,2.75);
#6016=CIRCLE('',#16547,2.75);
#6017=CIRCLE('',#16548,2.75);
#6018=CIRCLE('',#16550,2.35);
#6019=CIRCLE('',#16552,2.35);
#6020=CIRCLE('',#16555,1.15);
#6021=VERTEX_POINT('',#20565);
#6022=VERTEX_POINT('',#20567);
#6023=VERTEX_POINT('',#20571);
#6024=VERTEX_POINT('',#20572);
#6025=VERTEX_POINT('',#20574);
#6026=VERTEX_POINT('',#20576);
#6027=VERTEX_POINT('',#20579);
#6028=VERTEX_POINT('',#20581);
#6029=VERTEX_POINT('',#20583);
#6030=VERTEX_POINT('',#20586);
#6031=VERTEX_POINT('',#20590);
#6032=VERTEX_POINT('',#20594);
#6033=VERTEX_POINT('',#20598);
#6034=VERTEX_POINT('',#20602);
#6035=VERTEX_POINT('',#20606);
#6036=VERTEX_POINT('',#20610);
#6037=VERTEX_POINT('',#20614);
#6038=VERTEX_POINT('',#20616);
#6039=VERTEX_POINT('',#20620);
#6040=VERTEX_POINT('',#20621);
#6041=VERTEX_POINT('',#20623);
#6042=VERTEX_POINT('',#20625);
#6043=VERTEX_POINT('',#20628);
#6044=VERTEX_POINT('',#20630);
#6045=VERTEX_POINT('',#20632);
#6046=VERTEX_POINT('',#20635);
#6047=VERTEX_POINT('',#20639);
#6048=VERTEX_POINT('',#20643);
#6049=VERTEX_POINT('',#20647);
#6050=VERTEX_POINT('',#20651);
#6051=VERTEX_POINT('',#20655);
#6052=VERTEX_POINT('',#20659);
#6053=VERTEX_POINT('',#20663);
#6054=VERTEX_POINT('',#20665);
#6055=VERTEX_POINT('',#20669);
#6056=VERTEX_POINT('',#20670);
#6057=VERTEX_POINT('',#20672);
#6058=VERTEX_POINT('',#20674);
#6059=VERTEX_POINT('',#20677);
#6060=VERTEX_POINT('',#20679);
#6061=VERTEX_POINT('',#20681);
#6062=VERTEX_POINT('',#20683);
#6063=VERTEX_POINT('',#20685);
#6064=VERTEX_POINT('',#20687);
#6065=VERTEX_POINT('',#20689);
#6066=VERTEX_POINT('',#20692);
#6067=VERTEX_POINT('',#20696);
#6068=VERTEX_POINT('',#20700);
#6069=VERTEX_POINT('',#20704);
#6070=VERTEX_POINT('',#20708);
#6071=VERTEX_POINT('',#20712);
#6072=VERTEX_POINT('',#20716);
#6073=VERTEX_POINT('',#20720);
#6074=VERTEX_POINT('',#20724);
#6075=VERTEX_POINT('',#20728);
#6076=VERTEX_POINT('',#20732);
#6077=VERTEX_POINT('',#20736);
#6078=VERTEX_POINT('',#20740);
#6079=VERTEX_POINT('',#20744);
#6080=VERTEX_POINT('',#20748);
#6081=VERTEX_POINT('',#20752);
#6082=VERTEX_POINT('',#20755);
#6083=VERTEX_POINT('',#20758);
#6084=VERTEX_POINT('',#20761);
#6085=VERTEX_POINT('',#20764);
#6086=VERTEX_POINT('',#20767);
#6087=VERTEX_POINT('',#20770);
#6088=VERTEX_POINT('',#20773);
#6089=VERTEX_POINT('',#20776);
#6090=VERTEX_POINT('',#20777);
#6091=VERTEX_POINT('',#20779);
#6092=VERTEX_POINT('',#20781);
#6093=VERTEX_POINT('',#20783);
#6094=VERTEX_POINT('',#20787);
#6095=VERTEX_POINT('',#20789);
#6096=VERTEX_POINT('',#20794);
#6097=VERTEX_POINT('',#20796);
#6098=VERTEX_POINT('',#20798);
#6099=VERTEX_POINT('',#20800);
#6100=VERTEX_POINT('',#20802);
#6101=VERTEX_POINT('',#20804);
#6102=VERTEX_POINT('',#20808);
#6103=VERTEX_POINT('',#20810);
#6104=VERTEX_POINT('',#20812);
#6105=VERTEX_POINT('',#20814);
#6106=VERTEX_POINT('',#20816);
#6107=VERTEX_POINT('',#20818);
#6108=VERTEX_POINT('',#20820);
#6109=VERTEX_POINT('',#20824);
#6110=VERTEX_POINT('',#20826);
#6111=VERTEX_POINT('',#20830);
#6112=VERTEX_POINT('',#20832);
#6113=VERTEX_POINT('',#20834);
#6114=VERTEX_POINT('',#20838);
#6115=VERTEX_POINT('',#20842);
#6116=VERTEX_POINT('',#20846);
#6117=VERTEX_POINT('',#20848);
#6118=VERTEX_POINT('',#20852);
#6119=VERTEX_POINT('',#20854);
#6120=VERTEX_POINT('',#20858);
#6121=VERTEX_POINT('',#20865);
#6122=VERTEX_POINT('',#20867);
#6123=VERTEX_POINT('',#20869);
#6124=VERTEX_POINT('',#20871);
#6125=VERTEX_POINT('',#20873);
#6126=VERTEX_POINT('',#20875);
#6127=VERTEX_POINT('',#20879);
#6128=VERTEX_POINT('',#20881);
#6129=VERTEX_POINT('',#20883);
#6130=VERTEX_POINT('',#20885);
#6131=VERTEX_POINT('',#20887);
#6132=VERTEX_POINT('',#20889);
#6133=VERTEX_POINT('',#20924);
#6134=VERTEX_POINT('',#20926);
#6135=VERTEX_POINT('',#20928);
#6136=VERTEX_POINT('',#20930);
#6137=VERTEX_POINT('',#20939);
#6138=VERTEX_POINT('',#20941);
#6139=VERTEX_POINT('',#20946);
#6140=VERTEX_POINT('',#20950);
#6141=VERTEX_POINT('',#20952);
#6142=VERTEX_POINT('',#20954);
#6143=VERTEX_POINT('',#20956);
#6144=VERTEX_POINT('',#20965);
#6145=VERTEX_POINT('',#20967);
#6146=VERTEX_POINT('',#20972);
#6147=VERTEX_POINT('',#20976);
#6148=VERTEX_POINT('',#20978);
#6149=VERTEX_POINT('',#20980);
#6150=VERTEX_POINT('',#20982);
#6151=VERTEX_POINT('',#20991);
#6152=VERTEX_POINT('',#20993);
#6153=VERTEX_POINT('',#20998);
#6154=VERTEX_POINT('',#21002);
#6155=VERTEX_POINT('',#21003);
#6156=VERTEX_POINT('',#21005);
#6157=VERTEX_POINT('',#21007);
#6158=VERTEX_POINT('',#21011);
#6159=VERTEX_POINT('',#21015);
#6160=VERTEX_POINT('',#21019);
#6161=VERTEX_POINT('',#21023);
#6162=VERTEX_POINT('',#21026);
#6163=VERTEX_POINT('',#21029);
#6164=VERTEX_POINT('',#21032);
#6165=VERTEX_POINT('',#21036);
#6166=VERTEX_POINT('',#21040);
#6167=VERTEX_POINT('',#21044);
#6168=VERTEX_POINT('',#21046);
#6169=VERTEX_POINT('',#21048);
#6170=VERTEX_POINT('',#21050);
#6171=VERTEX_POINT('',#21059);
#6172=VERTEX_POINT('',#21061);
#6173=VERTEX_POINT('',#21066);
#6174=VERTEX_POINT('',#21070);
#6175=VERTEX_POINT('',#21072);
#6176=VERTEX_POINT('',#21074);
#6177=VERTEX_POINT('',#21076);
#6178=VERTEX_POINT('',#21085);
#6179=VERTEX_POINT('',#21087);
#6180=VERTEX_POINT('',#21092);
#6181=VERTEX_POINT('',#21096);
#6182=VERTEX_POINT('',#21098);
#6183=VERTEX_POINT('',#21100);
#6184=VERTEX_POINT('',#21102);
#6185=VERTEX_POINT('',#21111);
#6186=VERTEX_POINT('',#21113);
#6187=VERTEX_POINT('',#21118);
#6188=VERTEX_POINT('',#21122);
#6189=VERTEX_POINT('',#21123);
#6190=VERTEX_POINT('',#21125);
#6191=VERTEX_POINT('',#21127);
#6192=VERTEX_POINT('',#21131);
#6193=VERTEX_POINT('',#21135);
#6194=VERTEX_POINT('',#21139);
#6195=VERTEX_POINT('',#21143);
#6196=VERTEX_POINT('',#21146);
#6197=VERTEX_POINT('',#21149);
#6198=VERTEX_POINT('',#21152);
#6199=VERTEX_POINT('',#21156);
#6200=VERTEX_POINT('',#21160);
#6201=VERTEX_POINT('',#21164);
#6202=VERTEX_POINT('',#21166);
#6203=VERTEX_POINT('',#21170);
#6204=VERTEX_POINT('',#21171);
#6205=VERTEX_POINT('',#21173);
#6206=VERTEX_POINT('',#21175);
#6207=VERTEX_POINT('',#21177);
#6208=VERTEX_POINT('',#21179);
#6209=VERTEX_POINT('',#21181);
#6210=VERTEX_POINT('',#21183);
#6211=VERTEX_POINT('',#21185);
#6212=VERTEX_POINT('',#21187);
#6213=VERTEX_POINT('',#21189);
#6214=VERTEX_POINT('',#21191);
#6215=VERTEX_POINT('',#21193);
#6216=VERTEX_POINT('',#21195);
#6217=VERTEX_POINT('',#21198);
#6218=VERTEX_POINT('',#21200);
#6219=VERTEX_POINT('',#21202);
#6220=VERTEX_POINT('',#21205);
#6221=VERTEX_POINT('',#21207);
#6222=VERTEX_POINT('',#21211);
#6223=VERTEX_POINT('',#21215);
#6224=VERTEX_POINT('',#21217);
#6225=VERTEX_POINT('',#21221);
#6226=VERTEX_POINT('',#21225);
#6227=VERTEX_POINT('',#21227);
#6228=VERTEX_POINT('',#21231);
#6229=VERTEX_POINT('',#21235);
#6230=VERTEX_POINT('',#21237);
#6231=VERTEX_POINT('',#21241);
#6232=VERTEX_POINT('',#21244);
#6233=VERTEX_POINT('',#21247);
#6234=VERTEX_POINT('',#21250);
#6235=VERTEX_POINT('',#21253);
#6236=VERTEX_POINT('',#21255);
#6237=VERTEX_POINT('',#21259);
#6238=VERTEX_POINT('',#21260);
#6239=VERTEX_POINT('',#21262);
#6240=VERTEX_POINT('',#21264);
#6241=VERTEX_POINT('',#21266);
#6242=VERTEX_POINT('',#21268);
#6243=VERTEX_POINT('',#21270);
#6244=VERTEX_POINT('',#21272);
#6245=VERTEX_POINT('',#21274);
#6246=VERTEX_POINT('',#21276);
#6247=VERTEX_POINT('',#21278);
#6248=VERTEX_POINT('',#21280);
#6249=VERTEX_POINT('',#21282);
#6250=VERTEX_POINT('',#21284);
#6251=VERTEX_POINT('',#21287);
#6252=VERTEX_POINT('',#21289);
#6253=VERTEX_POINT('',#21291);
#6254=VERTEX_POINT('',#21294);
#6255=VERTEX_POINT('',#21296);
#6256=VERTEX_POINT('',#21300);
#6257=VERTEX_POINT('',#21304);
#6258=VERTEX_POINT('',#21306);
#6259=VERTEX_POINT('',#21310);
#6260=VERTEX_POINT('',#21314);
#6261=VERTEX_POINT('',#21316);
#6262=VERTEX_POINT('',#21320);
#6263=VERTEX_POINT('',#21324);
#6264=VERTEX_POINT('',#21326);
#6265=VERTEX_POINT('',#21330);
#6266=VERTEX_POINT('',#21333);
#6267=VERTEX_POINT('',#21336);
#6268=VERTEX_POINT('',#21339);
#6269=VERTEX_POINT('',#21342);
#6270=VERTEX_POINT('',#21344);
#6271=VERTEX_POINT('',#21348);
#6272=VERTEX_POINT('',#21349);
#6273=VERTEX_POINT('',#21351);
#6274=VERTEX_POINT('',#21353);
#6275=VERTEX_POINT('',#21356);
#6276=VERTEX_POINT('',#21358);
#6277=VERTEX_POINT('',#21360);
#6278=VERTEX_POINT('',#21362);
#6279=VERTEX_POINT('',#21364);
#6280=VERTEX_POINT('',#21366);
#6281=VERTEX_POINT('',#21368);
#6282=VERTEX_POINT('',#21370);
#6283=VERTEX_POINT('',#21372);
#6284=VERTEX_POINT('',#21374);
#6285=VERTEX_POINT('',#21376);
#6286=VERTEX_POINT('',#21378);
#6287=VERTEX_POINT('',#21380);
#6288=VERTEX_POINT('',#21383);
#6289=VERTEX_POINT('',#21387);
#6290=VERTEX_POINT('',#21391);
#6291=VERTEX_POINT('',#21395);
#6292=VERTEX_POINT('',#21399);
#6293=VERTEX_POINT('',#21403);
#6294=VERTEX_POINT('',#21407);
#6295=VERTEX_POINT('',#21411);
#6296=VERTEX_POINT('',#21415);
#6297=VERTEX_POINT('',#21419);
#6298=VERTEX_POINT('',#21423);
#6299=VERTEX_POINT('',#21427);
#6300=VERTEX_POINT('',#21430);
#6301=VERTEX_POINT('',#21433);
#6302=VERTEX_POINT('',#21436);
#6303=VERTEX_POINT('',#21439);
#6304=VERTEX_POINT('',#21442);
#6305=VERTEX_POINT('',#21445);
#6306=VERTEX_POINT('',#21449);
#6307=VERTEX_POINT('',#21453);
#6308=VERTEX_POINT('',#21457);
#6309=VERTEX_POINT('',#21461);
#6310=VERTEX_POINT('',#21465);
#6311=VERTEX_POINT('',#21469);
#6312=VERTEX_POINT('',#21473);
#6313=VERTEX_POINT('',#21477);
#6314=VERTEX_POINT('',#21481);
#6315=VERTEX_POINT('',#21485);
#6316=VERTEX_POINT('',#21489);
#6317=VERTEX_POINT('',#21493);
#6318=VERTEX_POINT('',#21497);
#6319=VERTEX_POINT('',#21501);
#6320=VERTEX_POINT('',#21505);
#6321=VERTEX_POINT('',#21509);
#6322=VERTEX_POINT('',#21512);
#6323=VERTEX_POINT('',#21515);
#6324=VERTEX_POINT('',#21518);
#6325=VERTEX_POINT('',#21521);
#6326=VERTEX_POINT('',#21524);
#6327=VERTEX_POINT('',#21527);
#6328=VERTEX_POINT('',#21530);
#6329=VERTEX_POINT('',#21533);
#6330=VERTEX_POINT('',#21537);
#6331=VERTEX_POINT('',#21541);
#6332=VERTEX_POINT('',#21545);
#6333=VERTEX_POINT('',#21549);
#6334=VERTEX_POINT('',#21553);
#6335=VERTEX_POINT('',#21557);
#6336=VERTEX_POINT('',#21561);
#6337=VERTEX_POINT('',#21566);
#6338=VERTEX_POINT('',#21570);
#6339=VERTEX_POINT('',#21579);
#6340=VERTEX_POINT('',#21588);
#6341=VERTEX_POINT('',#21619);
#6342=VERTEX_POINT('',#21621);
#6343=VERTEX_POINT('',#21625);
#6344=VERTEX_POINT('',#21626);
#6345=VERTEX_POINT('',#21628);
#6346=VERTEX_POINT('',#21630);
#6347=VERTEX_POINT('',#21632);
#6348=VERTEX_POINT('',#21634);
#6349=VERTEX_POINT('',#21636);
#6350=VERTEX_POINT('',#21638);
#6351=VERTEX_POINT('',#21640);
#6352=VERTEX_POINT('',#21642);
#6353=VERTEX_POINT('',#21644);
#6354=VERTEX_POINT('',#21646);
#6355=VERTEX_POINT('',#21648);
#6356=VERTEX_POINT('',#21650);
#6357=VERTEX_POINT('',#21652);
#6358=VERTEX_POINT('',#21655);
#6359=VERTEX_POINT('',#21659);
#6360=VERTEX_POINT('',#21661);
#6361=VERTEX_POINT('',#21665);
#6362=VERTEX_POINT('',#21668);
#6363=VERTEX_POINT('',#21670);
#6364=VERTEX_POINT('',#21674);
#6365=VERTEX_POINT('',#21675);
#6366=VERTEX_POINT('',#21677);
#6367=VERTEX_POINT('',#21680);
#6368=VERTEX_POINT('',#21682);
#6369=VERTEX_POINT('',#21684);
#6370=VERTEX_POINT('',#21686);
#6371=VERTEX_POINT('',#21688);
#6372=VERTEX_POINT('',#21690);
#6373=VERTEX_POINT('',#21692);
#6374=VERTEX_POINT('',#21694);
#6375=VERTEX_POINT('',#21696);
#6376=VERTEX_POINT('',#21698);
#6377=VERTEX_POINT('',#21700);
#6378=VERTEX_POINT('',#21702);
#6379=VERTEX_POINT('',#21704);
#6380=VERTEX_POINT('',#21708);
#6381=VERTEX_POINT('',#21710);
#6382=VERTEX_POINT('',#21714);
#6383=VERTEX_POINT('',#21717);
#6384=VERTEX_POINT('',#21719);
#6385=VERTEX_POINT('',#21725);
#6386=VERTEX_POINT('',#21727);
#6387=VERTEX_POINT('',#21730);
#6388=VERTEX_POINT('',#21732);
#6389=VERTEX_POINT('',#21734);
#6390=VERTEX_POINT('',#21736);
#6391=VERTEX_POINT('',#21738);
#6392=VERTEX_POINT('',#21740);
#6393=VERTEX_POINT('',#21742);
#6394=VERTEX_POINT('',#21744);
#6395=VERTEX_POINT('',#21746);
#6396=VERTEX_POINT('',#21748);
#6397=VERTEX_POINT('',#21750);
#6398=VERTEX_POINT('',#21752);
#6399=VERTEX_POINT('',#21754);
#6400=VERTEX_POINT('',#21758);
#6401=VERTEX_POINT('',#21762);
#6402=VERTEX_POINT('',#21764);
#6403=VERTEX_POINT('',#21766);
#6404=VERTEX_POINT('',#21768);
#6405=VERTEX_POINT('',#21770);
#6406=VERTEX_POINT('',#21772);
#6407=VERTEX_POINT('',#21774);
#6408=VERTEX_POINT('',#21776);
#6409=VERTEX_POINT('',#21778);
#6410=VERTEX_POINT('',#21780);
#6411=VERTEX_POINT('',#21782);
#6412=VERTEX_POINT('',#21784);
#6413=VERTEX_POINT('',#21786);
#6414=VERTEX_POINT('',#21790);
#6415=VERTEX_POINT('',#21794);
#6416=VERTEX_POINT('',#21796);
#6417=VERTEX_POINT('',#21798);
#6418=VERTEX_POINT('',#21800);
#6419=VERTEX_POINT('',#21802);
#6420=VERTEX_POINT('',#21804);
#6421=VERTEX_POINT('',#21806);
#6422=VERTEX_POINT('',#21808);
#6423=VERTEX_POINT('',#21810);
#6424=VERTEX_POINT('',#21812);
#6425=VERTEX_POINT('',#21814);
#6426=VERTEX_POINT('',#21816);
#6427=VERTEX_POINT('',#21818);
#6428=VERTEX_POINT('',#21858);
#6429=VERTEX_POINT('',#21860);
#6430=VERTEX_POINT('',#21864);
#6431=VERTEX_POINT('',#21866);
#6432=VERTEX_POINT('',#21873);
#6433=VERTEX_POINT('',#21875);
#6434=VERTEX_POINT('',#21879);
#6435=VERTEX_POINT('',#21884);
#6436=VERTEX_POINT('',#21909);
#6437=VERTEX_POINT('',#21911);
#6438=VERTEX_POINT('',#21913);
#6439=VERTEX_POINT('',#21917);
#6440=VERTEX_POINT('',#21918);
#6441=VERTEX_POINT('',#21920);
#6442=VERTEX_POINT('',#21922);
#6443=VERTEX_POINT('',#21924);
#6444=VERTEX_POINT('',#21926);
#6445=VERTEX_POINT('',#21928);
#6446=VERTEX_POINT('',#21930);
#6447=VERTEX_POINT('',#21932);
#6448=VERTEX_POINT('',#21934);
#6449=VERTEX_POINT('',#21936);
#6450=VERTEX_POINT('',#21939);
#6451=VERTEX_POINT('',#21941);
#6452=VERTEX_POINT('',#21943);
#6453=VERTEX_POINT('',#21945);
#6454=VERTEX_POINT('',#21947);
#6455=VERTEX_POINT('',#21951);
#6456=VERTEX_POINT('',#21953);
#6457=VERTEX_POINT('',#21957);
#6458=VERTEX_POINT('',#21960);
#6459=VERTEX_POINT('',#21962);
#6460=VERTEX_POINT('',#21964);
#6461=VERTEX_POINT('',#21968);
#6462=VERTEX_POINT('',#21969);
#6463=VERTEX_POINT('',#21971);
#6464=VERTEX_POINT('',#21974);
#6465=VERTEX_POINT('',#21976);
#6466=VERTEX_POINT('',#21978);
#6467=VERTEX_POINT('',#21980);
#6468=VERTEX_POINT('',#21982);
#6469=VERTEX_POINT('',#21984);
#6470=VERTEX_POINT('',#21986);
#6471=VERTEX_POINT('',#21988);
#6472=VERTEX_POINT('',#21990);
#6473=VERTEX_POINT('',#21992);
#6474=VERTEX_POINT('',#21994);
#6475=VERTEX_POINT('',#21996);
#6476=VERTEX_POINT('',#21998);
#6477=VERTEX_POINT('',#22002);
#6478=VERTEX_POINT('',#22004);
#6479=VERTEX_POINT('',#22008);
#6480=VERTEX_POINT('',#22011);
#6481=VERTEX_POINT('',#22013);
#6482=VERTEX_POINT('',#22019);
#6483=VERTEX_POINT('',#22021);
#6484=VERTEX_POINT('',#22023);
#6485=VERTEX_POINT('',#22026);
#6486=VERTEX_POINT('',#22028);
#6487=VERTEX_POINT('',#22030);
#6488=VERTEX_POINT('',#22032);
#6489=VERTEX_POINT('',#22034);
#6490=VERTEX_POINT('',#22036);
#6491=VERTEX_POINT('',#22038);
#6492=VERTEX_POINT('',#22040);
#6493=VERTEX_POINT('',#22042);
#6494=VERTEX_POINT('',#22044);
#6495=VERTEX_POINT('',#22046);
#6496=VERTEX_POINT('',#22048);
#6497=VERTEX_POINT('',#22050);
#6498=VERTEX_POINT('',#22054);
#6499=VERTEX_POINT('',#22058);
#6500=VERTEX_POINT('',#22060);
#6501=VERTEX_POINT('',#22062);
#6502=VERTEX_POINT('',#22064);
#6503=VERTEX_POINT('',#22066);
#6504=VERTEX_POINT('',#22068);
#6505=VERTEX_POINT('',#22070);
#6506=VERTEX_POINT('',#22072);
#6507=VERTEX_POINT('',#22074);
#6508=VERTEX_POINT('',#22076);
#6509=VERTEX_POINT('',#22078);
#6510=VERTEX_POINT('',#22080);
#6511=VERTEX_POINT('',#22082);
#6512=VERTEX_POINT('',#22086);
#6513=VERTEX_POINT('',#22090);
#6514=VERTEX_POINT('',#22092);
#6515=VERTEX_POINT('',#22094);
#6516=VERTEX_POINT('',#22096);
#6517=VERTEX_POINT('',#22098);
#6518=VERTEX_POINT('',#22100);
#6519=VERTEX_POINT('',#22102);
#6520=VERTEX_POINT('',#22104);
#6521=VERTEX_POINT('',#22106);
#6522=VERTEX_POINT('',#22108);
#6523=VERTEX_POINT('',#22110);
#6524=VERTEX_POINT('',#22112);
#6525=VERTEX_POINT('',#22114);
#6526=VERTEX_POINT('',#22118);
#6527=VERTEX_POINT('',#22122);
#6528=VERTEX_POINT('',#22124);
#6529=VERTEX_POINT('',#22126);
#6530=VERTEX_POINT('',#22128);
#6531=VERTEX_POINT('',#22130);
#6532=VERTEX_POINT('',#22132);
#6533=VERTEX_POINT('',#22134);
#6534=VERTEX_POINT('',#22136);
#6535=VERTEX_POINT('',#22138);
#6536=VERTEX_POINT('',#22140);
#6537=VERTEX_POINT('',#22142);
#6538=VERTEX_POINT('',#22144);
#6539=VERTEX_POINT('',#22146);
#6540=VERTEX_POINT('',#22197);
#6541=VERTEX_POINT('',#22199);
#6542=VERTEX_POINT('',#22203);
#6543=VERTEX_POINT('',#22207);
#6544=VERTEX_POINT('',#22209);
#6545=VERTEX_POINT('',#22213);
#6546=VERTEX_POINT('',#22217);
#6547=VERTEX_POINT('',#22221);
#6548=VERTEX_POINT('',#22248);
#6549=VERTEX_POINT('',#22249);
#6550=VERTEX_POINT('',#22251);
#6551=VERTEX_POINT('',#22253);
#6552=VERTEX_POINT('',#22257);
#6553=VERTEX_POINT('',#22259);
#6554=VERTEX_POINT('',#22263);
#6555=VERTEX_POINT('',#22265);
#6556=VERTEX_POINT('',#22269);
#6557=VERTEX_POINT('',#22271);
#6558=VERTEX_POINT('',#22275);
#6559=VERTEX_POINT('',#22277);
#6560=VERTEX_POINT('',#22281);
#6561=VERTEX_POINT('',#22283);
#6562=VERTEX_POINT('',#22287);
#6563=VERTEX_POINT('',#22289);
#6564=VERTEX_POINT('',#22296);
#6565=VERTEX_POINT('',#22297);
#6566=VERTEX_POINT('',#22299);
#6567=VERTEX_POINT('',#22301);
#6568=VERTEX_POINT('',#22305);
#6569=VERTEX_POINT('',#22307);
#6570=VERTEX_POINT('',#22311);
#6571=VERTEX_POINT('',#22313);
#6572=VERTEX_POINT('',#22317);
#6573=VERTEX_POINT('',#22319);
#6574=VERTEX_POINT('',#22323);
#6575=VERTEX_POINT('',#22325);
#6576=VERTEX_POINT('',#22329);
#6577=VERTEX_POINT('',#22331);
#6578=VERTEX_POINT('',#22335);
#6579=VERTEX_POINT('',#22337);
#6580=VERTEX_POINT('',#22344);
#6581=VERTEX_POINT('',#22345);
#6582=VERTEX_POINT('',#22347);
#6583=VERTEX_POINT('',#22349);
#6584=VERTEX_POINT('',#22353);
#6585=VERTEX_POINT('',#22355);
#6586=VERTEX_POINT('',#22359);
#6587=VERTEX_POINT('',#22361);
#6588=VERTEX_POINT('',#22365);
#6589=VERTEX_POINT('',#22367);
#6590=VERTEX_POINT('',#22371);
#6591=VERTEX_POINT('',#22373);
#6592=VERTEX_POINT('',#22377);
#6593=VERTEX_POINT('',#22379);
#6594=VERTEX_POINT('',#22383);
#6595=VERTEX_POINT('',#22385);
#6596=VERTEX_POINT('',#22392);
#6597=VERTEX_POINT('',#22393);
#6598=VERTEX_POINT('',#22395);
#6599=VERTEX_POINT('',#22397);
#6600=VERTEX_POINT('',#22401);
#6601=VERTEX_POINT('',#22403);
#6602=VERTEX_POINT('',#22407);
#6603=VERTEX_POINT('',#22409);
#6604=VERTEX_POINT('',#22413);
#6605=VERTEX_POINT('',#22415);
#6606=VERTEX_POINT('',#22419);
#6607=VERTEX_POINT('',#22421);
#6608=VERTEX_POINT('',#22425);
#6609=VERTEX_POINT('',#22427);
#6610=VERTEX_POINT('',#22431);
#6611=VERTEX_POINT('',#22433);
#6612=VERTEX_POINT('',#22440);
#6613=VERTEX_POINT('',#22441);
#6614=VERTEX_POINT('',#22443);
#6615=VERTEX_POINT('',#22445);
#6616=VERTEX_POINT('',#22449);
#6617=VERTEX_POINT('',#22451);
#6618=VERTEX_POINT('',#22455);
#6619=VERTEX_POINT('',#22457);
#6620=VERTEX_POINT('',#22461);
#6621=VERTEX_POINT('',#22463);
#6622=VERTEX_POINT('',#22467);
#6623=VERTEX_POINT('',#22469);
#6624=VERTEX_POINT('',#22473);
#6625=VERTEX_POINT('',#22475);
#6626=VERTEX_POINT('',#22479);
#6627=VERTEX_POINT('',#22481);
#6628=VERTEX_POINT('',#22488);
#6629=VERTEX_POINT('',#22489);
#6630=VERTEX_POINT('',#22491);
#6631=VERTEX_POINT('',#22493);
#6632=VERTEX_POINT('',#22497);
#6633=VERTEX_POINT('',#22499);
#6634=VERTEX_POINT('',#22503);
#6635=VERTEX_POINT('',#22505);
#6636=VERTEX_POINT('',#22509);
#6637=VERTEX_POINT('',#22511);
#6638=VERTEX_POINT('',#22515);
#6639=VERTEX_POINT('',#22517);
#6640=VERTEX_POINT('',#22521);
#6641=VERTEX_POINT('',#22523);
#6642=VERTEX_POINT('',#22527);
#6643=VERTEX_POINT('',#22529);
#6644=VERTEX_POINT('',#22536);
#6645=VERTEX_POINT('',#22537);
#6646=VERTEX_POINT('',#22539);
#6647=VERTEX_POINT('',#22541);
#6648=VERTEX_POINT('',#22545);
#6649=VERTEX_POINT('',#22547);
#6650=VERTEX_POINT('',#22551);
#6651=VERTEX_POINT('',#22553);
#6652=VERTEX_POINT('',#22557);
#6653=VERTEX_POINT('',#22559);
#6654=VERTEX_POINT('',#22563);
#6655=VERTEX_POINT('',#22565);
#6656=VERTEX_POINT('',#22569);
#6657=VERTEX_POINT('',#22571);
#6658=VERTEX_POINT('',#22575);
#6659=VERTEX_POINT('',#22577);
#6660=VERTEX_POINT('',#22584);
#6661=VERTEX_POINT('',#22585);
#6662=VERTEX_POINT('',#22587);
#6663=VERTEX_POINT('',#22589);
#6664=VERTEX_POINT('',#22593);
#6665=VERTEX_POINT('',#22595);
#6666=VERTEX_POINT('',#22599);
#6667=VERTEX_POINT('',#22601);
#6668=VERTEX_POINT('',#22605);
#6669=VERTEX_POINT('',#22607);
#6670=VERTEX_POINT('',#22611);
#6671=VERTEX_POINT('',#22613);
#6672=VERTEX_POINT('',#22617);
#6673=VERTEX_POINT('',#22619);
#6674=VERTEX_POINT('',#22623);
#6675=VERTEX_POINT('',#22625);
#6676=VERTEX_POINT('',#22632);
#6677=VERTEX_POINT('',#22633);
#6678=VERTEX_POINT('',#22635);
#6679=VERTEX_POINT('',#22637);
#6680=VERTEX_POINT('',#22641);
#6681=VERTEX_POINT('',#22643);
#6682=VERTEX_POINT('',#22647);
#6683=VERTEX_POINT('',#22649);
#6684=VERTEX_POINT('',#22653);
#6685=VERTEX_POINT('',#22655);
#6686=VERTEX_POINT('',#22659);
#6687=VERTEX_POINT('',#22661);
#6688=VERTEX_POINT('',#22665);
#6689=VERTEX_POINT('',#22667);
#6690=VERTEX_POINT('',#22671);
#6691=VERTEX_POINT('',#22673);
#6692=VERTEX_POINT('',#22680);
#6693=VERTEX_POINT('',#22681);
#6694=VERTEX_POINT('',#22683);
#6695=VERTEX_POINT('',#22685);
#6696=VERTEX_POINT('',#22689);
#6697=VERTEX_POINT('',#22691);
#6698=VERTEX_POINT('',#22695);
#6699=VERTEX_POINT('',#22697);
#6700=VERTEX_POINT('',#22701);
#6701=VERTEX_POINT('',#22703);
#6702=VERTEX_POINT('',#22707);
#6703=VERTEX_POINT('',#22709);
#6704=VERTEX_POINT('',#22713);
#6705=VERTEX_POINT('',#22715);
#6706=VERTEX_POINT('',#22719);
#6707=VERTEX_POINT('',#22721);
#6708=VERTEX_POINT('',#22728);
#6709=VERTEX_POINT('',#22729);
#6710=VERTEX_POINT('',#22731);
#6711=VERTEX_POINT('',#22733);
#6712=VERTEX_POINT('',#22737);
#6713=VERTEX_POINT('',#22739);
#6714=VERTEX_POINT('',#22743);
#6715=VERTEX_POINT('',#22745);
#6716=VERTEX_POINT('',#22749);
#6717=VERTEX_POINT('',#22751);
#6718=VERTEX_POINT('',#22755);
#6719=VERTEX_POINT('',#22757);
#6720=VERTEX_POINT('',#22761);
#6721=VERTEX_POINT('',#22763);
#6722=VERTEX_POINT('',#22767);
#6723=VERTEX_POINT('',#22769);
#6724=VERTEX_POINT('',#22776);
#6725=VERTEX_POINT('',#22777);
#6726=VERTEX_POINT('',#22779);
#6727=VERTEX_POINT('',#22781);
#6728=VERTEX_POINT('',#22785);
#6729=VERTEX_POINT('',#22787);
#6730=VERTEX_POINT('',#22791);
#6731=VERTEX_POINT('',#22793);
#6732=VERTEX_POINT('',#22797);
#6733=VERTEX_POINT('',#22799);
#6734=VERTEX_POINT('',#22803);
#6735=VERTEX_POINT('',#22805);
#6736=VERTEX_POINT('',#22809);
#6737=VERTEX_POINT('',#22811);
#6738=VERTEX_POINT('',#22815);
#6739=VERTEX_POINT('',#22817);
#6740=VERTEX_POINT('',#22824);
#6741=VERTEX_POINT('',#22825);
#6742=VERTEX_POINT('',#22827);
#6743=VERTEX_POINT('',#22829);
#6744=VERTEX_POINT('',#22833);
#6745=VERTEX_POINT('',#22835);
#6746=VERTEX_POINT('',#22839);
#6747=VERTEX_POINT('',#22841);
#6748=VERTEX_POINT('',#22845);
#6749=VERTEX_POINT('',#22847);
#6750=VERTEX_POINT('',#22851);
#6751=VERTEX_POINT('',#22853);
#6752=VERTEX_POINT('',#22857);
#6753=VERTEX_POINT('',#22859);
#6754=VERTEX_POINT('',#22863);
#6755=VERTEX_POINT('',#22865);
#6756=VERTEX_POINT('',#22872);
#6757=VERTEX_POINT('',#22873);
#6758=VERTEX_POINT('',#22875);
#6759=VERTEX_POINT('',#22877);
#6760=VERTEX_POINT('',#22881);
#6761=VERTEX_POINT('',#22883);
#6762=VERTEX_POINT('',#22887);
#6763=VERTEX_POINT('',#22889);
#6764=VERTEX_POINT('',#22893);
#6765=VERTEX_POINT('',#22895);
#6766=VERTEX_POINT('',#22899);
#6767=VERTEX_POINT('',#22901);
#6768=VERTEX_POINT('',#22905);
#6769=VERTEX_POINT('',#22907);
#6770=VERTEX_POINT('',#22911);
#6771=VERTEX_POINT('',#22913);
#6772=VERTEX_POINT('',#22920);
#6773=VERTEX_POINT('',#22921);
#6774=VERTEX_POINT('',#22923);
#6775=VERTEX_POINT('',#22925);
#6776=VERTEX_POINT('',#22929);
#6777=VERTEX_POINT('',#22931);
#6778=VERTEX_POINT('',#22935);
#6779=VERTEX_POINT('',#22937);
#6780=VERTEX_POINT('',#22941);
#6781=VERTEX_POINT('',#22943);
#6782=VERTEX_POINT('',#22947);
#6783=VERTEX_POINT('',#22949);
#6784=VERTEX_POINT('',#22953);
#6785=VERTEX_POINT('',#22955);
#6786=VERTEX_POINT('',#22959);
#6787=VERTEX_POINT('',#22961);
#6788=VERTEX_POINT('',#22968);
#6789=VERTEX_POINT('',#22969);
#6790=VERTEX_POINT('',#22971);
#6791=VERTEX_POINT('',#22973);
#6792=VERTEX_POINT('',#22977);
#6793=VERTEX_POINT('',#22979);
#6794=VERTEX_POINT('',#22983);
#6795=VERTEX_POINT('',#22985);
#6796=VERTEX_POINT('',#22989);
#6797=VERTEX_POINT('',#22991);
#6798=VERTEX_POINT('',#22995);
#6799=VERTEX_POINT('',#22997);
#6800=VERTEX_POINT('',#23001);
#6801=VERTEX_POINT('',#23003);
#6802=VERTEX_POINT('',#23007);
#6803=VERTEX_POINT('',#23009);
#6804=VERTEX_POINT('',#23019);
#6805=VERTEX_POINT('',#23022);
#6806=VERTEX_POINT('',#23026);
#6807=VERTEX_POINT('',#23030);
#6808=VERTEX_POINT('',#23036);
#6809=VERTEX_POINT('',#23037);
#6810=VERTEX_POINT('',#23039);
#6811=VERTEX_POINT('',#23198);
#6812=VERTEX_POINT('',#23277);
#6813=VERTEX_POINT('',#23278);
#6814=VERTEX_POINT('',#23502);
#6815=VERTEX_POINT('',#23716);
#6816=VERTEX_POINT('',#23717);
#6817=VERTEX_POINT('',#23719);
#6818=VERTEX_POINT('',#24153);
#6819=VERTEX_POINT('',#24154);
#6820=VERTEX_POINT('',#24372);
#6821=VERTEX_POINT('',#24594);
#6822=VERTEX_POINT('',#24595);
#6823=VERTEX_POINT('',#24597);
#6824=VERTEX_POINT('',#25077);
#6825=VERTEX_POINT('',#25078);
#6826=VERTEX_POINT('',#25294);
#6827=VERTEX_POINT('',#25508);
#6828=VERTEX_POINT('',#25509);
#6829=VERTEX_POINT('',#25511);
#6830=VERTEX_POINT('',#25796);
#6831=VERTEX_POINT('',#25797);
#6832=VERTEX_POINT('',#25799);
#6833=VERTEX_POINT('',#25960);
#6834=VERTEX_POINT('',#26264);
#6835=VERTEX_POINT('',#26265);
#6836=VERTEX_POINT('',#26698);
#6837=VERTEX_POINT('',#26699);
#6838=VERTEX_POINT('',#26701);
#6839=VERTEX_POINT('',#26767);
#6840=VERTEX_POINT('',#26870);
#6841=VERTEX_POINT('',#26871);
#6842=VERTEX_POINT('',#26873);
#6843=VERTEX_POINT('',#27019);
#6844=VERTEX_POINT('',#27192);
#6845=VERTEX_POINT('',#27193);
#6846=VERTEX_POINT('',#27195);
#6847=VERTEX_POINT('',#27645);
#6848=VERTEX_POINT('',#27646);
#6849=VERTEX_POINT('',#27852);
#6850=VERTEX_POINT('',#28094);
#6851=VERTEX_POINT('',#28095);
#6852=VERTEX_POINT('',#28097);
#6853=VERTEX_POINT('',#28529);
#6854=VERTEX_POINT('',#28530);
#6855=VERTEX_POINT('',#28734);
#6856=VERTEX_POINT('',#28988);
#6857=VERTEX_POINT('',#28989);
#6858=VERTEX_POINT('',#28991);
#6859=VERTEX_POINT('',#29433);
#6860=VERTEX_POINT('',#29434);
#6861=VERTEX_POINT('',#29652);
#6862=VERTEX_POINT('',#29912);
#6863=VERTEX_POINT('',#29913);
#6864=VERTEX_POINT('',#29915);
#6865=VERTEX_POINT('',#30397);
#6866=VERTEX_POINT('',#30398);
#6867=VERTEX_POINT('',#30622);
#6868=VERTEX_POINT('',#30844);
#6869=VERTEX_POINT('',#30845);
#6870=VERTEX_POINT('',#30847);
#6871=VERTEX_POINT('',#31291);
#6872=VERTEX_POINT('',#31292);
#6873=VERTEX_POINT('',#31510);
#6874=VERTEX_POINT('',#31724);
#6875=VERTEX_POINT('',#31725);
#6876=VERTEX_POINT('',#31727);
#6877=VERTEX_POINT('',#32241);
#6878=VERTEX_POINT('',#32242);
#6879=VERTEX_POINT('',#32462);
#6880=VERTEX_POINT('',#32692);
#6881=VERTEX_POINT('',#32693);
#6882=VERTEX_POINT('',#32695);
#6883=VERTEX_POINT('',#32910);
#6884=VERTEX_POINT('',#32976);
#6885=VERTEX_POINT('',#32977);
#6886=VERTEX_POINT('',#32984);
#6887=VERTEX_POINT('',#32986);
#6888=VERTEX_POINT('',#32992);
#6889=VERTEX_POINT('',#33183);
#6890=VERTEX_POINT('',#33377);
#6891=VERTEX_POINT('',#33571);
#6892=VERTEX_POINT('',#33762);
#6893=VERTEX_POINT('',#33773);
#6894=VERTEX_POINT('',#33967);
#6895=VERTEX_POINT('',#34158);
#6896=VERTEX_POINT('',#34169);
#6897=VERTEX_POINT('',#34360);
#6898=VERTEX_POINT('',#34551);
#6899=VERTEX_POINT('',#34745);
#6900=VERTEX_POINT('',#34756);
#6901=VERTEX_POINT('',#34947);
#6902=VERTEX_POINT('',#35141);
#6903=VERTEX_POINT('',#35335);
#6904=VERTEX_POINT('',#35526);
#6905=VERTEX_POINT('',#35538);
#6906=VERTEX_POINT('',#35732);
#6907=VERTEX_POINT('',#35923);
#6908=VERTEX_POINT('',#35935);
#6909=VERTEX_POINT('',#36129);
#6910=VERTEX_POINT('',#36323);
#6911=VERTEX_POINT('',#36334);
#6912=VERTEX_POINT('',#36519);
#6913=VERTEX_POINT('',#36521);
#6914=VERTEX_POINT('',#36531);
#6915=VERTEX_POINT('',#36722);
#6916=VERTEX_POINT('',#36916);
#6917=VERTEX_POINT('',#37107);
#6918=VERTEX_POINT('',#37298);
#6919=VERTEX_POINT('',#37309);
#6920=VERTEX_POINT('',#37503);
#6921=VERTEX_POINT('',#37691);
#6922=VERTEX_POINT('',#37702);
#6923=VERTEX_POINT('',#37896);
#6924=VERTEX_POINT('',#38090);
#6925=VERTEX_POINT('',#38281);
#6926=VERTEX_POINT('',#38475);
#6927=VERTEX_POINT('',#38669);
#6928=VERTEX_POINT('',#38860);
#6929=VERTEX_POINT('',#39051);
#6930=VERTEX_POINT('',#39245);
#6931=VERTEX_POINT('',#39436);
#6932=VERTEX_POINT('',#39627);
#6933=VERTEX_POINT('',#39821);
#6934=VERTEX_POINT('',#40015);
#6935=VERTEX_POINT('',#40206);
#6936=VERTEX_POINT('',#40408);
#6937=VERTEX_POINT('',#40414);
#6938=VERTEX_POINT('',#40506);
#6939=VERTEX_POINT('',#40508);
#6940=VERTEX_POINT('',#40614);
#6941=VERTEX_POINT('',#40615);
#6942=VERTEX_POINT('',#41423);
#6943=VERTEX_POINT('',#41514);
#6944=VERTEX_POINT('',#41515);
#6945=VERTEX_POINT('',#42239);
#6946=VERTEX_POINT('',#42243);
#6947=VERTEX_POINT('',#42246);
#6948=VERTEX_POINT('',#42251);
#6949=VERTEX_POINT('',#42252);
#6950=VERTEX_POINT('',#42254);
#6951=VERTEX_POINT('',#42258);
#6952=VERTEX_POINT('',#42260);
#6953=VERTEX_POINT('',#42266);
#6954=VERTEX_POINT('',#42272);
#6955=VERTEX_POINT('',#42273);
#6956=VERTEX_POINT('',#42275);
#6957=VERTEX_POINT('',#42278);
#6958=VERTEX_POINT('',#42280);
#6959=VERTEX_POINT('',#42282);
#6960=VERTEX_POINT('',#42284);
#6961=VERTEX_POINT('',#42286);
#6962=VERTEX_POINT('',#42288);
#6963=VERTEX_POINT('',#42290);
#6964=VERTEX_POINT('',#42292);
#6965=VERTEX_POINT('',#42294);
#6966=VERTEX_POINT('',#42296);
#6967=VERTEX_POINT('',#42298);
#6968=VERTEX_POINT('',#42300);
#6969=VERTEX_POINT('',#42302);
#6970=VERTEX_POINT('',#42304);
#6971=VERTEX_POINT('',#42306);
#6972=VERTEX_POINT('',#42308);
#6973=VERTEX_POINT('',#42310);
#6974=VERTEX_POINT('',#42312);
#6975=VERTEX_POINT('',#42314);
#6976=VERTEX_POINT('',#42316);
#6977=VERTEX_POINT('',#42318);
#6978=VERTEX_POINT('',#42320);
#6979=VERTEX_POINT('',#42322);
#6980=VERTEX_POINT('',#42324);
#6981=VERTEX_POINT('',#42326);
#6982=VERTEX_POINT('',#42328);
#6983=VERTEX_POINT('',#42330);
#6984=VERTEX_POINT('',#42332);
#6985=VERTEX_POINT('',#42334);
#6986=VERTEX_POINT('',#42336);
#6987=VERTEX_POINT('',#42338);
#6988=VERTEX_POINT('',#42340);
#6989=VERTEX_POINT('',#42342);
#6990=VERTEX_POINT('',#42344);
#6991=VERTEX_POINT('',#42346);
#6992=VERTEX_POINT('',#42348);
#6993=VERTEX_POINT('',#42350);
#6994=VERTEX_POINT('',#42352);
#6995=VERTEX_POINT('',#42354);
#6996=VERTEX_POINT('',#42356);
#6997=VERTEX_POINT('',#42358);
#6998=VERTEX_POINT('',#42360);
#6999=VERTEX_POINT('',#42362);
#7000=VERTEX_POINT('',#42364);
#7001=VERTEX_POINT('',#42366);
#7002=VERTEX_POINT('',#42368);
#7003=VERTEX_POINT('',#42370);
#7004=VERTEX_POINT('',#42372);
#7005=VERTEX_POINT('',#42374);
#7006=VERTEX_POINT('',#42376);
#7007=VERTEX_POINT('',#42378);
#7008=VERTEX_POINT('',#42380);
#7009=VERTEX_POINT('',#42382);
#7010=VERTEX_POINT('',#42384);
#7011=VERTEX_POINT('',#42386);
#7012=VERTEX_POINT('',#42388);
#7013=VERTEX_POINT('',#42390);
#7014=VERTEX_POINT('',#42392);
#7015=VERTEX_POINT('',#42394);
#7016=VERTEX_POINT('',#42396);
#7017=VERTEX_POINT('',#42398);
#7018=VERTEX_POINT('',#42400);
#7019=VERTEX_POINT('',#42402);
#7020=VERTEX_POINT('',#42404);
#7021=VERTEX_POINT('',#42406);
#7022=VERTEX_POINT('',#42408);
#7023=VERTEX_POINT('',#42411);
#7024=VERTEX_POINT('',#42413);
#7025=VERTEX_POINT('',#42415);
#7026=VERTEX_POINT('',#42417);
#7027=VERTEX_POINT('',#42419);
#7028=VERTEX_POINT('',#42421);
#7029=VERTEX_POINT('',#42423);
#7030=VERTEX_POINT('',#42425);
#7031=VERTEX_POINT('',#42427);
#7032=VERTEX_POINT('',#42429);
#7033=VERTEX_POINT('',#42431);
#7034=VERTEX_POINT('',#42433);
#7035=VERTEX_POINT('',#42435);
#7036=VERTEX_POINT('',#42437);
#7037=VERTEX_POINT('',#42439);
#7038=VERTEX_POINT('',#42441);
#7039=VERTEX_POINT('',#42443);
#7040=VERTEX_POINT('',#42445);
#7041=VERTEX_POINT('',#42447);
#7042=VERTEX_POINT('',#42449);
#7043=VERTEX_POINT('',#42451);
#7044=VERTEX_POINT('',#42453);
#7045=VERTEX_POINT('',#42455);
#7046=VERTEX_POINT('',#42457);
#7047=VERTEX_POINT('',#42459);
#7048=VERTEX_POINT('',#42461);
#7049=VERTEX_POINT('',#42463);
#7050=VERTEX_POINT('',#42465);
#7051=VERTEX_POINT('',#42467);
#7052=VERTEX_POINT('',#42469);
#7053=VERTEX_POINT('',#42471);
#7054=VERTEX_POINT('',#42473);
#7055=VERTEX_POINT('',#42475);
#7056=VERTEX_POINT('',#42477);
#7057=VERTEX_POINT('',#42479);
#7058=VERTEX_POINT('',#42481);
#7059=VERTEX_POINT('',#42483);
#7060=VERTEX_POINT('',#42485);
#7061=VERTEX_POINT('',#42487);
#7062=VERTEX_POINT('',#42489);
#7063=VERTEX_POINT('',#42491);
#7064=VERTEX_POINT('',#42493);
#7065=VERTEX_POINT('',#42495);
#7066=VERTEX_POINT('',#42497);
#7067=VERTEX_POINT('',#42499);
#7068=VERTEX_POINT('',#42501);
#7069=VERTEX_POINT('',#42503);
#7070=VERTEX_POINT('',#42505);
#7071=VERTEX_POINT('',#42507);
#7072=VERTEX_POINT('',#42509);
#7073=VERTEX_POINT('',#42511);
#7074=VERTEX_POINT('',#42513);
#7075=VERTEX_POINT('',#42515);
#7076=VERTEX_POINT('',#42517);
#7077=VERTEX_POINT('',#42519);
#7078=VERTEX_POINT('',#42521);
#7079=VERTEX_POINT('',#42523);
#7080=VERTEX_POINT('',#42525);
#7081=VERTEX_POINT('',#42527);
#7082=VERTEX_POINT('',#42529);
#7083=VERTEX_POINT('',#42531);
#7084=VERTEX_POINT('',#42533);
#7085=VERTEX_POINT('',#42535);
#7086=VERTEX_POINT('',#42537);
#7087=VERTEX_POINT('',#42539);
#7088=VERTEX_POINT('',#42541);
#7089=VERTEX_POINT('',#42543);
#7090=VERTEX_POINT('',#42545);
#7091=VERTEX_POINT('',#42547);
#7092=VERTEX_POINT('',#42549);
#7093=VERTEX_POINT('',#42551);
#7094=VERTEX_POINT('',#42553);
#7095=VERTEX_POINT('',#42555);
#7096=VERTEX_POINT('',#42559);
#7097=VERTEX_POINT('',#42561);
#7098=VERTEX_POINT('',#42573);
#7099=VERTEX_POINT('',#42577);
#7100=VERTEX_POINT('',#42584);
#7101=VERTEX_POINT('',#42591);
#7102=VERTEX_POINT('',#42598);
#7103=VERTEX_POINT('',#42605);
#7104=VERTEX_POINT('',#42612);
#7105=VERTEX_POINT('',#42619);
#7106=VERTEX_POINT('',#42626);
#7107=VERTEX_POINT('',#42633);
#7108=VERTEX_POINT('',#42640);
#7109=VERTEX_POINT('',#42647);
#7110=VERTEX_POINT('',#42654);
#7111=VERTEX_POINT('',#42661);
#7112=VERTEX_POINT('',#42668);
#7113=VERTEX_POINT('',#42675);
#7114=VERTEX_POINT('',#42682);
#7115=VERTEX_POINT('',#42689);
#7116=VERTEX_POINT('',#42696);
#7117=VERTEX_POINT('',#42703);
#7118=VERTEX_POINT('',#42710);
#7119=VERTEX_POINT('',#42717);
#7120=VERTEX_POINT('',#42724);
#7121=VERTEX_POINT('',#42731);
#7122=VERTEX_POINT('',#42738);
#7123=VERTEX_POINT('',#42745);
#7124=VERTEX_POINT('',#42752);
#7125=VERTEX_POINT('',#42759);
#7126=VERTEX_POINT('',#42766);
#7127=VERTEX_POINT('',#42773);
#7128=VERTEX_POINT('',#42780);
#7129=VERTEX_POINT('',#42787);
#7130=VERTEX_POINT('',#42794);
#7131=VERTEX_POINT('',#42801);
#7132=VERTEX_POINT('',#42811);
#7133=VERTEX_POINT('',#42815);
#7134=VERTEX_POINT('',#42822);
#7135=VERTEX_POINT('',#42829);
#7136=VERTEX_POINT('',#42836);
#7137=VERTEX_POINT('',#42843);
#7138=VERTEX_POINT('',#42850);
#7139=VERTEX_POINT('',#42857);
#7140=VERTEX_POINT('',#42864);
#7141=VERTEX_POINT('',#42871);
#7142=VERTEX_POINT('',#42878);
#7143=VERTEX_POINT('',#42885);
#7144=VERTEX_POINT('',#42892);
#7145=VERTEX_POINT('',#42899);
#7146=VERTEX_POINT('',#42906);
#7147=VERTEX_POINT('',#42913);
#7148=VERTEX_POINT('',#42920);
#7149=VERTEX_POINT('',#42927);
#7150=VERTEX_POINT('',#42934);
#7151=VERTEX_POINT('',#42941);
#7152=VERTEX_POINT('',#42948);
#7153=VERTEX_POINT('',#42955);
#7154=VERTEX_POINT('',#42962);
#7155=VERTEX_POINT('',#42969);
#7156=VERTEX_POINT('',#42976);
#7157=VERTEX_POINT('',#42983);
#7158=VERTEX_POINT('',#42990);
#7159=VERTEX_POINT('',#42997);
#7160=VERTEX_POINT('',#43004);
#7161=VERTEX_POINT('',#43011);
#7162=VERTEX_POINT('',#43018);
#7163=VERTEX_POINT('',#43025);
#7164=VERTEX_POINT('',#43032);
#7165=VERTEX_POINT('',#43039);
#7166=VERTEX_POINT('',#43046);
#7167=VERTEX_POINT('',#43055);
#7168=VERTEX_POINT('',#43058);
#7169=VERTEX_POINT('',#43059);
#7170=VERTEX_POINT('',#43063);
#7171=VERTEX_POINT('',#43065);
#7172=VERTEX_POINT('',#43069);
#7173=VERTEX_POINT('',#43073);
#7174=VERTEX_POINT('',#43075);
#7175=VERTEX_POINT('',#43079);
#7176=VERTEX_POINT('',#43083);
#7177=VERTEX_POINT('',#43085);
#7178=VERTEX_POINT('',#43089);
#7179=VERTEX_POINT('',#43093);
#7180=VERTEX_POINT('',#43095);
#7181=VERTEX_POINT('',#43099);
#7182=VERTEX_POINT('',#43103);
#7183=VERTEX_POINT('',#43105);
#7184=VERTEX_POINT('',#43109);
#7185=VERTEX_POINT('',#43113);
#7186=VERTEX_POINT('',#43120);
#7187=VERTEX_POINT('',#43122);
#7188=VERTEX_POINT('',#43126);
#7189=VERTEX_POINT('',#43128);
#7190=VERTEX_POINT('',#43132);
#7191=VERTEX_POINT('',#43134);
#7192=VERTEX_POINT('',#43138);
#7193=VERTEX_POINT('',#43140);
#7194=VERTEX_POINT('',#43144);
#7195=VERTEX_POINT('',#43146);
#7196=VERTEX_POINT('',#43150);
#7197=VERTEX_POINT('',#43152);
#7198=VERTEX_POINT('',#43157);
#7199=VERTEX_POINT('',#43159);
#7200=VERTEX_POINT('',#43164);
#7201=VERTEX_POINT('',#43169);
#7202=VERTEX_POINT('',#43182);
#7203=VERTEX_POINT('',#43192);
#7204=VERTEX_POINT('',#43199);
#7205=VERTEX_POINT('',#43208);
#7206=VERTEX_POINT('',#43209);
#7207=VERTEX_POINT('',#43211);
#7208=VERTEX_POINT('',#43386);
#7209=VERTEX_POINT('',#43507);
#7210=VERTEX_POINT('',#43508);
#7211=VERTEX_POINT('',#43728);
#7212=VERTEX_POINT('',#43951);
#7213=VERTEX_POINT('',#43952);
#7214=VERTEX_POINT('',#44383);
#7215=VERTEX_POINT('',#44384);
#7216=VERTEX_POINT('',#44614);
#7217=VERTEX_POINT('',#44803);
#7218=VERTEX_POINT('',#44804);
#7219=VERTEX_POINT('',#44806);
#7220=VERTEX_POINT('',#45067);
#7221=VERTEX_POINT('',#45305);
#7222=VERTEX_POINT('',#45306);
#7223=VERTEX_POINT('',#45735);
#7224=VERTEX_POINT('',#45736);
#7225=VERTEX_POINT('',#45738);
#7226=VERTEX_POINT('',#45967);
#7227=VERTEX_POINT('',#46189);
#7228=VERTEX_POINT('',#46190);
#7229=VERTEX_POINT('',#46633);
#7230=VERTEX_POINT('',#46634);
#7231=VERTEX_POINT('',#46636);
#7232=VERTEX_POINT('',#46869);
#7233=VERTEX_POINT('',#47115);
#7234=VERTEX_POINT('',#47116);
#7235=VERTEX_POINT('',#47581);
#7236=VERTEX_POINT('',#47582);
#7237=VERTEX_POINT('',#47584);
#7238=VERTEX_POINT('',#47773);
#7239=VERTEX_POINT('',#48005);
#7240=VERTEX_POINT('',#48006);
#7241=VERTEX_POINT('',#48008);
#7242=VERTEX_POINT('',#48469);
#7243=VERTEX_POINT('',#48470);
#7244=VERTEX_POINT('',#48684);
#7245=VERTEX_POINT('',#48908);
#7246=VERTEX_POINT('',#48909);
#7247=VERTEX_POINT('',#48911);
#7248=VERTEX_POINT('',#49347);
#7249=VERTEX_POINT('',#49348);
#7250=VERTEX_POINT('',#49572);
#7251=VERTEX_POINT('',#49796);
#7252=VERTEX_POINT('',#49797);
#7253=VERTEX_POINT('',#49799);
#7254=VERTEX_POINT('',#50299);
#7255=VERTEX_POINT('',#50300);
#7256=VERTEX_POINT('',#50534);
#7257=VERTEX_POINT('',#50802);
#7258=VERTEX_POINT('',#50803);
#7259=VERTEX_POINT('',#50805);
#7260=VERTEX_POINT('',#51281);
#7261=VERTEX_POINT('',#51282);
#7262=VERTEX_POINT('',#51488);
#7263=VERTEX_POINT('',#51714);
#7264=VERTEX_POINT('',#51715);
#7265=VERTEX_POINT('',#51717);
#7266=VERTEX_POINT('',#52159);
#7267=VERTEX_POINT('',#52160);
#7268=VERTEX_POINT('',#52378);
#7269=VERTEX_POINT('',#52608);
#7270=VERTEX_POINT('',#52609);
#7271=VERTEX_POINT('',#52611);
#7272=VERTEX_POINT('',#53051);
#7273=VERTEX_POINT('',#53052);
#7274=VERTEX_POINT('',#53517);
#7275=VERTEX_POINT('',#53518);
#7276=VERTEX_POINT('',#53525);
#7277=VERTEX_POINT('',#53527);
#7278=VERTEX_POINT('',#53533);
#7279=VERTEX_POINT('',#53724);
#7280=VERTEX_POINT('',#53918);
#7281=VERTEX_POINT('',#54109);
#7282=VERTEX_POINT('',#54303);
#7283=VERTEX_POINT('',#54497);
#7284=VERTEX_POINT('',#54691);
#7285=VERTEX_POINT('',#54882);
#7286=VERTEX_POINT('',#55076);
#7287=VERTEX_POINT('',#55270);
#7288=VERTEX_POINT('',#55461);
#7289=VERTEX_POINT('',#55655);
#7290=VERTEX_POINT('',#55846);
#7291=VERTEX_POINT('',#56037);
#7292=VERTEX_POINT('',#56228);
#7293=VERTEX_POINT('',#56422);
#7294=VERTEX_POINT('',#56613);
#7295=VERTEX_POINT('',#56807);
#7296=VERTEX_POINT('',#57001);
#7297=VERTEX_POINT('',#57192);
#7298=VERTEX_POINT('',#57386);
#7299=VERTEX_POINT('',#57580);
#7300=VERTEX_POINT('',#57592);
#7301=VERTEX_POINT('',#57783);
#7302=VERTEX_POINT('',#57866);
#7303=VERTEX_POINT('',#57868);
#7304=VERTEX_POINT('',#57874);
#7305=VERTEX_POINT('',#58065);
#7306=VERTEX_POINT('',#58259);
#7307=VERTEX_POINT('',#58270);
#7308=VERTEX_POINT('',#58281);
#7309=VERTEX_POINT('',#58293);
#7310=VERTEX_POINT('',#58304);
#7311=VERTEX_POINT('',#58315);
#7312=VERTEX_POINT('',#58327);
#7313=VERTEX_POINT('',#58521);
#7314=VERTEX_POINT('',#58715);
#7315=VERTEX_POINT('',#58906);
#7316=VERTEX_POINT('',#59097);
#7317=VERTEX_POINT('',#59291);
#7318=VERTEX_POINT('',#59482);
#7319=VERTEX_POINT('',#59676);
#7320=VERTEX_POINT('',#59870);
#7321=VERTEX_POINT('',#60064);
#7322=VERTEX_POINT('',#60255);
#7323=VERTEX_POINT('',#60449);
#7324=VERTEX_POINT('',#60643);
#7325=VERTEX_POINT('',#60834);
#7326=VERTEX_POINT('',#61219);
#7327=VERTEX_POINT('',#61428);
#7328=VERTEX_POINT('',#61430);
#7329=VERTEX_POINT('',#61578);
#7330=VERTEX_POINT('',#61579);
#7331=VERTEX_POINT('',#61669);
#7332=VERTEX_POINT('',#62380);
#7333=VERTEX_POINT('',#62471);
#7334=VERTEX_POINT('',#62473);
#7335=VERTEX_POINT('',#63184);
#7336=VERTEX_POINT('',#63185);
#7337=VERTEX_POINT('',#63189);
#7338=VERTEX_POINT('',#63191);
#7339=VERTEX_POINT('',#63195);
#7340=VERTEX_POINT('',#63199);
#7341=VERTEX_POINT('',#63201);
#7342=VERTEX_POINT('',#63205);
#7343=VERTEX_POINT('',#63209);
#7344=VERTEX_POINT('',#63211);
#7345=VERTEX_POINT('',#63215);
#7346=VERTEX_POINT('',#63219);
#7347=VERTEX_POINT('',#63221);
#7348=VERTEX_POINT('',#63225);
#7349=VERTEX_POINT('',#63229);
#7350=VERTEX_POINT('',#63231);
#7351=VERTEX_POINT('',#63235);
#7352=VERTEX_POINT('',#63239);
#7353=VERTEX_POINT('',#63244);
#7354=VERTEX_POINT('',#63248);
#7355=VERTEX_POINT('',#63250);
#7356=VERTEX_POINT('',#63254);
#7357=VERTEX_POINT('',#63256);
#7358=VERTEX_POINT('',#63260);
#7359=VERTEX_POINT('',#63262);
#7360=VERTEX_POINT('',#63266);
#7361=VERTEX_POINT('',#63268);
#7362=VERTEX_POINT('',#63272);
#7363=VERTEX_POINT('',#63274);
#7364=VERTEX_POINT('',#63278);
#7365=VERTEX_POINT('',#63280);
#7366=VERTEX_POINT('',#63285);
#7367=VERTEX_POINT('',#63287);
#7368=VERTEX_POINT('',#63292);
#7369=VERTEX_POINT('',#63297);
#7370=VERTEX_POINT('',#63310);
#7371=VERTEX_POINT('',#63320);
#7372=VERTEX_POINT('',#63327);
#7373=VERTEX_POINT('',#63335);
#7374=VERTEX_POINT('',#63340);
#7375=VERTEX_POINT('',#63346);
#7376=VERTEX_POINT('',#63347);
#7377=VERTEX_POINT('',#63349);
#7378=VERTEX_POINT('',#63377);
#7379=VERTEX_POINT('',#63378);
#7380=VERTEX_POINT('',#63380);
#7381=VERTEX_POINT('',#63569);
#7382=VERTEX_POINT('',#63571);
#7383=VERTEX_POINT('',#63752);
#7384=VERTEX_POINT('',#63753);
#7385=VERTEX_POINT('',#63931);
#7386=VERTEX_POINT('',#64124);
#7387=VERTEX_POINT('',#64125);
#7388=VERTEX_POINT('',#64127);
#7389=VERTEX_POINT('',#64318);
#7390=VERTEX_POINT('',#64508);
#7391=VERTEX_POINT('',#64509);
#7392=VERTEX_POINT('',#64695);
#7393=VERTEX_POINT('',#64891);
#7394=VERTEX_POINT('',#64892);
#7395=VERTEX_POINT('',#64894);
#7396=VERTEX_POINT('',#65075);
#7397=VERTEX_POINT('',#65268);
#7398=VERTEX_POINT('',#65269);
#7399=VERTEX_POINT('',#65457);
#7400=VERTEX_POINT('',#65647);
#7401=VERTEX_POINT('',#65648);
#7402=VERTEX_POINT('',#65650);
#7403=VERTEX_POINT('',#65829);
#7404=VERTEX_POINT('',#65875);
#7405=VERTEX_POINT('',#65876);
#7406=VERTEX_POINT('',#66060);
#7407=VERTEX_POINT('',#66227);
#7408=VERTEX_POINT('',#66228);
#7409=VERTEX_POINT('',#66230);
#7410=VERTEX_POINT('',#66419);
#7411=VERTEX_POINT('',#66609);
#7412=VERTEX_POINT('',#66610);
#7413=VERTEX_POINT('',#66612);
#7414=VERTEX_POINT('',#66643);
#7415=VERTEX_POINT('',#66654);
#7416=VERTEX_POINT('',#66656);
#7417=VERTEX_POINT('',#66673);
#7418=VERTEX_POINT('',#66680);
#7419=VERTEX_POINT('',#66686);
#7420=VERTEX_POINT('',#66877);
#7421=VERTEX_POINT('',#67071);
#7422=VERTEX_POINT('',#67265);
#7423=VERTEX_POINT('',#67456);
#7424=VERTEX_POINT('',#67647);
#7425=VERTEX_POINT('',#67838);
#7426=VERTEX_POINT('',#68029);
#7427=VERTEX_POINT('',#68223);
#7428=VERTEX_POINT('',#68414);
#7429=VERTEX_POINT('',#68605);
#7430=VERTEX_POINT('',#68634);
#7431=VERTEX_POINT('',#68636);
#7432=VERTEX_POINT('',#68638);
#7433=VERTEX_POINT('',#68649);
#7434=VERTEX_POINT('',#68843);
#7435=VERTEX_POINT('',#69037);
#7436=VERTEX_POINT('',#69225);
#7437=VERTEX_POINT('',#69419);
#7438=VERTEX_POINT('',#69613);
#7439=VERTEX_POINT('',#69804);
#7440=VERTEX_POINT('',#69998);
#7441=VERTEX_POINT('',#70383);
#7442=VERTEX_POINT('',#70418);
#7443=VERTEX_POINT('',#70543);
#7444=VERTEX_POINT('',#71018);
#7445=VERTEX_POINT('',#71395);
#7446=VERTEX_POINT('',#71399);
#7447=VERTEX_POINT('',#71402);
#7448=VERTEX_POINT('',#71403);
#7449=VERTEX_POINT('',#71407);
#7450=VERTEX_POINT('',#71411);
#7451=VERTEX_POINT('',#71415);
#7452=VERTEX_POINT('',#71419);
#7453=VERTEX_POINT('',#71426);
#7454=VERTEX_POINT('',#71429);
#7455=VERTEX_POINT('',#71430);
#7456=VERTEX_POINT('',#71435);
#7457=VERTEX_POINT('',#71439);
#7458=VERTEX_POINT('',#71443);
#7459=VERTEX_POINT('',#71447);
#7460=VERTEX_POINT('',#71453);
#7461=VERTEX_POINT('',#71460);
#7462=VERTEX_POINT('',#71461);
#7463=VERTEX_POINT('',#71463);
#7464=VERTEX_POINT('',#71516);
#7465=VERTEX_POINT('',#71517);
#7466=VERTEX_POINT('',#71713);
#7467=VERTEX_POINT('',#71715);
#7468=VERTEX_POINT('',#71884);
#7469=VERTEX_POINT('',#71885);
#7470=VERTEX_POINT('',#72075);
#7471=VERTEX_POINT('',#72250);
#7472=VERTEX_POINT('',#72251);
#7473=VERTEX_POINT('',#72441);
#7474=VERTEX_POINT('',#72616);
#7475=VERTEX_POINT('',#72617);
#7476=VERTEX_POINT('',#72815);
#7477=VERTEX_POINT('',#72990);
#7478=VERTEX_POINT('',#72991);
#7479=VERTEX_POINT('',#72993);
#7480=VERTEX_POINT('',#73190);
#7481=VERTEX_POINT('',#73365);
#7482=VERTEX_POINT('',#73366);
#7483=VERTEX_POINT('',#73544);
#7484=VERTEX_POINT('',#73716);
#7485=VERTEX_POINT('',#73717);
#7486=VERTEX_POINT('',#73719);
#7487=VERTEX_POINT('',#73914);
#7488=VERTEX_POINT('',#73944);
#7489=VERTEX_POINT('',#73945);
#7490=VERTEX_POINT('',#74155);
#7491=VERTEX_POINT('',#74316);
#7492=VERTEX_POINT('',#74317);
#7493=VERTEX_POINT('',#74319);
#7494=VERTEX_POINT('',#74516);
#7495=VERTEX_POINT('',#74691);
#7496=VERTEX_POINT('',#74692);
#7497=VERTEX_POINT('',#74890);
#7498=VERTEX_POINT('',#75065);
#7499=VERTEX_POINT('',#75066);
#7500=VERTEX_POINT('',#75068);
#7501=VERTEX_POINT('',#75269);
#7502=VERTEX_POINT('',#75444);
#7503=VERTEX_POINT('',#75445);
#7504=VERTEX_POINT('',#75453);
#7505=VERTEX_POINT('',#75455);
#7506=VERTEX_POINT('',#75461);
#7507=VERTEX_POINT('',#75634);
#7508=VERTEX_POINT('',#75810);
#7509=VERTEX_POINT('',#75983);
#7510=VERTEX_POINT('',#76159);
#7511=VERTEX_POINT('',#76332);
#7512=VERTEX_POINT('',#76505);
#7513=VERTEX_POINT('',#76678);
#7514=VERTEX_POINT('',#76854);
#7515=VERTEX_POINT('',#77027);
#7516=VERTEX_POINT('',#77203);
#7517=VERTEX_POINT('',#77376);
#7518=VERTEX_POINT('',#77552);
#7519=VERTEX_POINT('',#77596);
#7520=VERTEX_POINT('',#77598);
#7521=VERTEX_POINT('',#77618);
#7522=VERTEX_POINT('',#77794);
#7523=VERTEX_POINT('',#77967);
#7524=VERTEX_POINT('',#78143);
#7525=VERTEX_POINT('',#78316);
#7526=VERTEX_POINT('',#78489);
#7527=VERTEX_POINT('',#78665);
#7528=VERTEX_POINT('',#78838);
#7529=VERTEX_POINT('',#79014);
#7530=VERTEX_POINT('',#79187);
#7531=VERTEX_POINT('',#79360);
#7532=VERTEX_POINT('',#79712);
#7533=VERTEX_POINT('',#79732);
#7534=VERTEX_POINT('',#79869);
#7535=VERTEX_POINT('',#80337);
#7536=VERTEX_POINT('',#80366);
#7537=VERTEX_POINT('',#80464);
#7538=VERTEX_POINT('',#80895);
#7539=VERTEX_POINT('',#80899);
#7540=VERTEX_POINT('',#80902);
#7541=VERTEX_POINT('',#80903);
#7542=VERTEX_POINT('',#80905);
#7543=VERTEX_POINT('',#80907);
#7544=VERTEX_POINT('',#80909);
#7545=VERTEX_POINT('',#80913);
#7546=VERTEX_POINT('',#80915);
#7547=VERTEX_POINT('',#80917);
#7548=VERTEX_POINT('',#80921);
#7549=VERTEX_POINT('',#80927);
#7550=VERTEX_POINT('',#80929);
#7551=VERTEX_POINT('',#80933);
#7552=VERTEX_POINT('',#80935);
#7553=VERTEX_POINT('',#80950);
#7554=EDGE_CURVE('',#6021,#6021,#5444,.T.);
#7555=EDGE_CURVE('',#6021,#6022,#3220,.T.);
#7556=EDGE_CURVE('',#6022,#6022,#5445,.T.);
#7557=EDGE_CURVE('',#6023,#6024,#3221,.T.);
#7558=EDGE_CURVE('',#6025,#6023,#3222,.T.);
#7559=EDGE_CURVE('',#6026,#6025,#3223,.T.);
#7560=EDGE_CURVE('',#6024,#6026,#3224,.T.);
#7561=EDGE_CURVE('',#6027,#6027,#5446,.T.);
#7562=EDGE_CURVE('',#6028,#6028,#5447,.T.);
#7563=EDGE_CURVE('',#6029,#6029,#5448,.T.);
#7564=EDGE_CURVE('',#6021,#6030,#3225,.T.);
#7565=EDGE_CURVE('',#6030,#6030,#5449,.T.);
#7566=EDGE_CURVE('',#6031,#6031,#5450,.T.);
#7567=EDGE_CURVE('',#6031,#6027,#3226,.T.);
#7568=EDGE_CURVE('',#6031,#6032,#3227,.T.);
#7569=EDGE_CURVE('',#6032,#6032,#5451,.T.);
#7570=EDGE_CURVE('',#6033,#6033,#5452,.T.);
#7571=EDGE_CURVE('',#6033,#6029,#3228,.T.);
#7572=EDGE_CURVE('',#6033,#6034,#3229,.T.);
#7573=EDGE_CURVE('',#6034,#6034,#5453,.T.);
#7574=EDGE_CURVE('',#6035,#6035,#5454,.T.);
#7575=EDGE_CURVE('',#6035,#6028,#3230,.T.);
#7576=EDGE_CURVE('',#6035,#6036,#3231,.T.);
#7577=EDGE_CURVE('',#6036,#6036,#5455,.T.);
#7578=EDGE_CURVE('',#6037,#6037,#5456,.T.);
#7579=EDGE_CURVE('',#6037,#6038,#3232,.T.);
#7580=EDGE_CURVE('',#6038,#6038,#5457,.T.);
#7581=EDGE_CURVE('',#6039,#6040,#3233,.T.);
#7582=EDGE_CURVE('',#6041,#6039,#3234,.T.);
#7583=EDGE_CURVE('',#6041,#6042,#3235,.T.);
#7584=EDGE_CURVE('',#6040,#6042,#3236,.T.);
#7585=EDGE_CURVE('',#6043,#6043,#5458,.T.);
#7586=EDGE_CURVE('',#6044,#6044,#5459,.T.);
#7587=EDGE_CURVE('',#6045,#6045,#5460,.T.);
#7588=EDGE_CURVE('',#6037,#6046,#3237,.T.);
#7589=EDGE_CURVE('',#6046,#6046,#5461,.T.);
#7590=EDGE_CURVE('',#6047,#6047,#5462,.T.);
#7591=EDGE_CURVE('',#6047,#6043,#3238,.T.);
#7592=EDGE_CURVE('',#6047,#6048,#3239,.T.);
#7593=EDGE_CURVE('',#6048,#6048,#5463,.T.);
#7594=EDGE_CURVE('',#6049,#6049,#5464,.T.);
#7595=EDGE_CURVE('',#6049,#6045,#3240,.T.);
#7596=EDGE_CURVE('',#6049,#6050,#3241,.T.);
#7597=EDGE_CURVE('',#6050,#6050,#5465,.T.);
#7598=EDGE_CURVE('',#6051,#6051,#5466,.T.);
#7599=EDGE_CURVE('',#6051,#6044,#3242,.T.);
#7600=EDGE_CURVE('',#6051,#6052,#3243,.T.);
#7601=EDGE_CURVE('',#6052,#6052,#5467,.T.);
#7602=EDGE_CURVE('',#6053,#6053,#5468,.T.);
#7603=EDGE_CURVE('',#6053,#6054,#3244,.T.);
#7604=EDGE_CURVE('',#6054,#6054,#5469,.T.);
#7605=EDGE_CURVE('',#6055,#6056,#3245,.T.);
#7606=EDGE_CURVE('',#6057,#6055,#3246,.T.);
#7607=EDGE_CURVE('',#6058,#6057,#3247,.T.);
#7608=EDGE_CURVE('',#6056,#6058,#3248,.T.);
#7609=EDGE_CURVE('',#6059,#6059,#5470,.T.);
#7610=EDGE_CURVE('',#6060,#6060,#5471,.T.);
#7611=EDGE_CURVE('',#6061,#6061,#5472,.T.);
#7612=EDGE_CURVE('',#6062,#6062,#5473,.T.);
#7613=EDGE_CURVE('',#6063,#6063,#5474,.T.);
#7614=EDGE_CURVE('',#6064,#6064,#5475,.T.);
#7615=EDGE_CURVE('',#6065,#6065,#5476,.T.);
#7616=EDGE_CURVE('',#6053,#6066,#3249,.T.);
#7617=EDGE_CURVE('',#6066,#6066,#5477,.T.);
#7618=EDGE_CURVE('',#6067,#6067,#5478,.T.);
#7619=EDGE_CURVE('',#6067,#6059,#3250,.T.);
#7620=EDGE_CURVE('',#6067,#6068,#3251,.T.);
#7621=EDGE_CURVE('',#6068,#6068,#5479,.T.);
#7622=EDGE_CURVE('',#6069,#6069,#5480,.T.);
#7623=EDGE_CURVE('',#6069,#6065,#3252,.T.);
#7624=EDGE_CURVE('',#6069,#6070,#3253,.T.);
#7625=EDGE_CURVE('',#6070,#6070,#5481,.T.);
#7626=EDGE_CURVE('',#6071,#6071,#5482,.T.);
#7627=EDGE_CURVE('',#6071,#6060,#3254,.T.);
#7628=EDGE_CURVE('',#6071,#6072,#3255,.T.);
#7629=EDGE_CURVE('',#6072,#6072,#5483,.T.);
#7630=EDGE_CURVE('',#6073,#6073,#5484,.T.);
#7631=EDGE_CURVE('',#6073,#6064,#3256,.T.);
#7632=EDGE_CURVE('',#6073,#6074,#3257,.T.);
#7633=EDGE_CURVE('',#6074,#6074,#5485,.T.);
#7634=EDGE_CURVE('',#6075,#6075,#5486,.T.);
#7635=EDGE_CURVE('',#6075,#6061,#3258,.T.);
#7636=EDGE_CURVE('',#6075,#6076,#3259,.T.);
#7637=EDGE_CURVE('',#6076,#6076,#5487,.T.);
#7638=EDGE_CURVE('',#6077,#6077,#5488,.T.);
#7639=EDGE_CURVE('',#6077,#6063,#3260,.T.);
#7640=EDGE_CURVE('',#6077,#6078,#3261,.T.);
#7641=EDGE_CURVE('',#6078,#6078,#5489,.T.);
#7642=EDGE_CURVE('',#6079,#6079,#5490,.T.);
#7643=EDGE_CURVE('',#6079,#6062,#3262,.T.);
#7644=EDGE_CURVE('',#6079,#6080,#3263,.T.);
#7645=EDGE_CURVE('',#6080,#6080,#5491,.T.);
#7646=EDGE_CURVE('',#6081,#6066,#3264,.T.);
#7647=EDGE_CURVE('',#6082,#6080,#3265,.T.);
#7648=EDGE_CURVE('',#6083,#6068,#3266,.T.);
#7649=EDGE_CURVE('',#6084,#6078,#3267,.T.);
#7650=EDGE_CURVE('',#6085,#6076,#3268,.T.);
#7651=EDGE_CURVE('',#6086,#6072,#3269,.T.);
#7652=EDGE_CURVE('',#6087,#6074,#3270,.T.);
#7653=EDGE_CURVE('',#6088,#6070,#3271,.T.);
#7654=EDGE_CURVE('',#6089,#6090,#3272,.T.);
#7655=EDGE_CURVE('',#6090,#6091,#3273,.T.);
#7656=EDGE_CURVE('',#6091,#6092,#3274,.T.);
#7657=EDGE_CURVE('',#6092,#6093,#3275,.T.);
#7658=EDGE_CURVE('',#6093,#6089,#3276,.T.);
#7659=EDGE_CURVE('',#6091,#6094,#3277,.T.);
#7660=EDGE_CURVE('',#6094,#6095,#3278,.T.);
#7661=EDGE_CURVE('',#6095,#6055,#3279,.T.);
#7662=EDGE_CURVE('',#6056,#6092,#3280,.T.);
#7663=EDGE_CURVE('',#6090,#6096,#3281,.T.);
#7664=EDGE_CURVE('',#6096,#6097,#3282,.T.);
#7665=EDGE_CURVE('',#6097,#6098,#3283,.T.);
#7666=EDGE_CURVE('',#6098,#6099,#3284,.T.);
#7667=EDGE_CURVE('',#6100,#6099,#3285,.T.);
#7668=EDGE_CURVE('',#6100,#6101,#3286,.T.);
#7669=EDGE_CURVE('',#6040,#6101,#3287,.T.);
#7670=EDGE_CURVE('',#6042,#6025,#3288,.T.);
#7671=EDGE_CURVE('',#6102,#6023,#3289,.T.);
#7672=EDGE_CURVE('',#6102,#6103,#3290,.T.);
#7673=EDGE_CURVE('',#6104,#6103,#3291,.T.);
#7674=EDGE_CURVE('',#6104,#6105,#3292,.T.);
#7675=EDGE_CURVE('',#6105,#6106,#3293,.T.);
#7676=EDGE_CURVE('',#6106,#6107,#3294,.T.);
#7677=EDGE_CURVE('',#6107,#6108,#3295,.T.);
#7678=EDGE_CURVE('',#6094,#6108,#3296,.T.);
#7679=EDGE_CURVE('',#6089,#6109,#3297,.T.);
#7680=EDGE_CURVE('',#6110,#6109,#3298,.T.);
#7681=EDGE_CURVE('',#6110,#6090,#3299,.T.);
#7682=EDGE_CURVE('',#6111,#6095,#3300,.T.);
#7683=EDGE_CURVE('',#6111,#6112,#3301,.T.);
#7684=EDGE_CURVE('',#6113,#6112,#3302,.T.);
#7685=EDGE_CURVE('',#6057,#6113,#3303,.T.);
#7686=EDGE_CURVE('',#6108,#6114,#3304,.T.);
#7687=EDGE_CURVE('',#6114,#6111,#3305,.T.);
#7688=EDGE_CURVE('',#6115,#6114,#3306,.T.);
#7689=EDGE_CURVE('',#6112,#6115,#3307,.T.);
#7690=EDGE_CURVE('',#6115,#6116,#3308,.T.);
#7691=EDGE_CURVE('',#6116,#6117,#3309,.T.);
#7692=EDGE_CURVE('',#6117,#6113,#3310,.T.);
#7693=EDGE_CURVE('',#6117,#6118,#3311,.T.);
#7694=EDGE_CURVE('',#6118,#6119,#3312,.T.);
#7695=EDGE_CURVE('',#6119,#6058,#3313,.T.);
#7696=EDGE_CURVE('',#6120,#6119,#3314,.T.);
#7697=EDGE_CURVE('',#6120,#6093,#3315,.T.);
#7698=EDGE_CURVE('',#6118,#6110,#3316,.T.);
#7699=EDGE_CURVE('',#6109,#6120,#3317,.T.);
#7700=EDGE_CURVE('',#6116,#6121,#3318,.T.);
#7701=EDGE_CURVE('',#6121,#6122,#3319,.T.);
#7702=EDGE_CURVE('',#6122,#6123,#3320,.T.);
#7703=EDGE_CURVE('',#6123,#6124,#3321,.T.);
#7704=EDGE_CURVE('',#6125,#6124,#3322,.T.);
#7705=EDGE_CURVE('',#6125,#6126,#3323,.T.);
#7706=EDGE_CURVE('',#6024,#6126,#3324,.T.);
#7707=EDGE_CURVE('',#6026,#6041,#3325,.T.);
#7708=EDGE_CURVE('',#6127,#6039,#3326,.T.);
#7709=EDGE_CURVE('',#6127,#6128,#3327,.T.);
#7710=EDGE_CURVE('',#6129,#6128,#3328,.T.);
#7711=EDGE_CURVE('',#6129,#6130,#3329,.T.);
#7712=EDGE_CURVE('',#6130,#6131,#3330,.T.);
#7713=EDGE_CURVE('',#6131,#6132,#3331,.T.);
#7714=EDGE_CURVE('',#6132,#6110,#3332,.T.);
#7715=EDGE_CURVE('',#6099,#6129,#3333,.T.);
#7716=EDGE_CURVE('',#6128,#6100,#3334,.T.);
#7717=EDGE_CURVE('',#6101,#6127,#3335,.T.);
#7718=EDGE_CURVE('',#6126,#6102,#3336,.T.);
#7719=EDGE_CURVE('',#6103,#6125,#3337,.T.);
#7720=EDGE_CURVE('',#6124,#6104,#3338,.T.);
#7721=EDGE_CURVE('',#6123,#6105,#3339,.T.);
#7722=EDGE_CURVE('',#6108,#6116,#3340,.T.);
#7723=EDGE_CURVE('',#6132,#6096,#3341,.T.);
#7724=EDGE_CURVE('',#6121,#6107,#3342,.T.);
#7725=EDGE_CURVE('',#6122,#6106,#3343,.T.);
#7726=EDGE_CURVE('',#6130,#6098,#3344,.T.);
#7727=EDGE_CURVE('',#6131,#6097,#3345,.T.);
#7728=EDGE_CURVE('',#6133,#6133,#5492,.T.);
#7729=EDGE_CURVE('',#6133,#6134,#3346,.T.);
#7730=EDGE_CURVE('',#6134,#6135,#5493,.T.);
#7731=EDGE_CURVE('',#6135,#6136,#402,.T.);
#7732=EDGE_CURVE('',#6136,#6134,#5494,.T.);
#7733=EDGE_CURVE('',#6137,#6137,#5495,.T.);
#7734=EDGE_CURVE('',#6137,#6138,#3347,.T.);
#7735=EDGE_CURVE('',#6138,#6136,#5496,.T.);
#7736=EDGE_CURVE('',#6135,#6138,#5497,.T.);
#7737=EDGE_CURVE('',#6133,#6139,#3348,.T.);
#7738=EDGE_CURVE('',#6139,#6139,#5498,.T.);
#7739=EDGE_CURVE('',#6140,#6140,#5499,.T.);
#7740=EDGE_CURVE('',#6140,#6141,#3349,.T.);
#7741=EDGE_CURVE('',#6141,#6142,#5500,.T.);
#7742=EDGE_CURVE('',#6142,#6143,#403,.T.);
#7743=EDGE_CURVE('',#6143,#6141,#5501,.T.);
#7744=EDGE_CURVE('',#6144,#6144,#5502,.T.);
#7745=EDGE_CURVE('',#6144,#6145,#3350,.T.);
#7746=EDGE_CURVE('',#6145,#6143,#5503,.T.);
#7747=EDGE_CURVE('',#6142,#6145,#5504,.T.);
#7748=EDGE_CURVE('',#6140,#6146,#3351,.T.);
#7749=EDGE_CURVE('',#6146,#6146,#5505,.T.);
#7750=EDGE_CURVE('',#6147,#6147,#5506,.T.);
#7751=EDGE_CURVE('',#6147,#6148,#3352,.T.);
#7752=EDGE_CURVE('',#6148,#6149,#5507,.T.);
#7753=EDGE_CURVE('',#6149,#6150,#404,.T.);
#7754=EDGE_CURVE('',#6150,#6148,#5508,.T.);
#7755=EDGE_CURVE('',#6151,#6151,#5509,.T.);
#7756=EDGE_CURVE('',#6151,#6152,#3353,.T.);
#7757=EDGE_CURVE('',#6152,#6150,#5510,.T.);
#7758=EDGE_CURVE('',#6149,#6152,#5511,.T.);
#7759=EDGE_CURVE('',#6147,#6153,#3354,.T.);
#7760=EDGE_CURVE('',#6153,#6153,#5512,.T.);
#7761=EDGE_CURVE('',#6154,#6155,#3355,.T.);
#7762=EDGE_CURVE('',#6156,#6154,#3356,.T.);
#7763=EDGE_CURVE('',#6157,#6156,#3357,.T.);
#7764=EDGE_CURVE('',#6155,#6157,#3358,.T.);
#7765=EDGE_CURVE('',#6137,#6158,#3359,.T.);
#7766=EDGE_CURVE('',#6158,#6158,#5513,.T.);
#7767=EDGE_CURVE('',#6144,#6159,#3360,.T.);
#7768=EDGE_CURVE('',#6159,#6159,#5514,.T.);
#7769=EDGE_CURVE('',#6151,#6160,#3361,.T.);
#7770=EDGE_CURVE('',#6160,#6160,#5515,.T.);
#7771=EDGE_CURVE('',#6161,#6161,#5516,.T.);
#7772=EDGE_CURVE('',#6162,#6162,#5517,.T.);
#7773=EDGE_CURVE('',#6163,#6163,#5518,.T.);
#7774=EDGE_CURVE('',#6161,#6164,#3362,.T.);
#7775=EDGE_CURVE('',#6164,#6164,#5519,.T.);
#7776=EDGE_CURVE('',#6162,#6165,#3363,.T.);
#7777=EDGE_CURVE('',#6165,#6165,#5520,.T.);
#7778=EDGE_CURVE('',#6163,#6166,#3364,.T.);
#7779=EDGE_CURVE('',#6166,#6166,#5521,.T.);
#7780=EDGE_CURVE('',#6167,#6167,#5522,.T.);
#7781=EDGE_CURVE('',#6167,#6168,#3365,.T.);
#7782=EDGE_CURVE('',#6168,#6169,#5523,.T.);
#7783=EDGE_CURVE('',#6169,#6170,#405,.T.);
#7784=EDGE_CURVE('',#6170,#6168,#5524,.T.);
#7785=EDGE_CURVE('',#6171,#6171,#5525,.T.);
#7786=EDGE_CURVE('',#6171,#6172,#3366,.T.);
#7787=EDGE_CURVE('',#6172,#6170,#5526,.T.);
#7788=EDGE_CURVE('',#6169,#6172,#5527,.T.);
#7789=EDGE_CURVE('',#6167,#6173,#3367,.T.);
#7790=EDGE_CURVE('',#6173,#6173,#5528,.T.);
#7791=EDGE_CURVE('',#6174,#6174,#5529,.T.);
#7792=EDGE_CURVE('',#6174,#6175,#3368,.T.);
#7793=EDGE_CURVE('',#6175,#6176,#5530,.T.);
#7794=EDGE_CURVE('',#6176,#6177,#406,.T.);
#7795=EDGE_CURVE('',#6177,#6175,#5531,.T.);
#7796=EDGE_CURVE('',#6178,#6178,#5532,.T.);
#7797=EDGE_CURVE('',#6178,#6179,#3369,.T.);
#7798=EDGE_CURVE('',#6179,#6177,#5533,.T.);
#7799=EDGE_CURVE('',#6176,#6179,#5534,.T.);
#7800=EDGE_CURVE('',#6174,#6180,#3370,.T.);
#7801=EDGE_CURVE('',#6180,#6180,#5535,.T.);
#7802=EDGE_CURVE('',#6181,#6181,#5536,.T.);
#7803=EDGE_CURVE('',#6181,#6182,#3371,.T.);
#7804=EDGE_CURVE('',#6182,#6183,#5537,.T.);
#7805=EDGE_CURVE('',#6183,#6184,#407,.T.);
#7806=EDGE_CURVE('',#6184,#6182,#5538,.T.);
#7807=EDGE_CURVE('',#6185,#6185,#5539,.T.);
#7808=EDGE_CURVE('',#6185,#6186,#3372,.T.);
#7809=EDGE_CURVE('',#6186,#6184,#5540,.T.);
#7810=EDGE_CURVE('',#6183,#6186,#5541,.T.);
#7811=EDGE_CURVE('',#6181,#6187,#3373,.T.);
#7812=EDGE_CURVE('',#6187,#6187,#5542,.T.);
#7813=EDGE_CURVE('',#6188,#6189,#3374,.T.);
#7814=EDGE_CURVE('',#6190,#6188,#3375,.T.);
#7815=EDGE_CURVE('',#6191,#6190,#3376,.T.);
#7816=EDGE_CURVE('',#6189,#6191,#3377,.T.);
#7817=EDGE_CURVE('',#6171,#6192,#3378,.T.);
#7818=EDGE_CURVE('',#6192,#6192,#5543,.T.);
#7819=EDGE_CURVE('',#6178,#6193,#3379,.T.);
#7820=EDGE_CURVE('',#6193,#6193,#5544,.T.);
#7821=EDGE_CURVE('',#6185,#6194,#3380,.T.);
#7822=EDGE_CURVE('',#6194,#6194,#5545,.T.);
#7823=EDGE_CURVE('',#6195,#6195,#5546,.T.);
#7824=EDGE_CURVE('',#6196,#6196,#5547,.T.);
#7825=EDGE_CURVE('',#6197,#6197,#5548,.T.);
#7826=EDGE_CURVE('',#6195,#6198,#3381,.T.);
#7827=EDGE_CURVE('',#6198,#6198,#5549,.T.);
#7828=EDGE_CURVE('',#6196,#6199,#3382,.T.);
#7829=EDGE_CURVE('',#6199,#6199,#5550,.T.);
#7830=EDGE_CURVE('',#6197,#6200,#3383,.T.);
#7831=EDGE_CURVE('',#6200,#6200,#5551,.T.);
#7832=EDGE_CURVE('',#6201,#6201,#5552,.T.);
#7833=EDGE_CURVE('',#6201,#6202,#3384,.T.);
#7834=EDGE_CURVE('',#6202,#6202,#5553,.T.);
#7835=EDGE_CURVE('',#6203,#6204,#3385,.T.);
#7836=EDGE_CURVE('',#6203,#6205,#3386,.T.);
#7837=EDGE_CURVE('',#6206,#6205,#3387,.T.);
#7838=EDGE_CURVE('',#6206,#6207,#3388,.T.);
#7839=EDGE_CURVE('',#6207,#6208,#3389,.T.);
#7840=EDGE_CURVE('',#6208,#6209,#3390,.T.);
#7841=EDGE_CURVE('',#6209,#6210,#3391,.T.);
#7842=EDGE_CURVE('',#6210,#6211,#3392,.T.);
#7843=EDGE_CURVE('',#6211,#6212,#3393,.T.);
#7844=EDGE_CURVE('',#6212,#6213,#3394,.T.);
#7845=EDGE_CURVE('',#6214,#6213,#3395,.T.);
#7846=EDGE_CURVE('',#6214,#6215,#3396,.T.);
#7847=EDGE_CURVE('',#6216,#6215,#3397,.T.);
#7848=EDGE_CURVE('',#6204,#6216,#3398,.T.);
#7849=EDGE_CURVE('',#6217,#6217,#5554,.T.);
#7850=EDGE_CURVE('',#6218,#6218,#5555,.T.);
#7851=EDGE_CURVE('',#6219,#6219,#5556,.T.);
#7852=EDGE_CURVE('',#6201,#6220,#3399,.T.);
#7853=EDGE_CURVE('',#6220,#6221,#5557,.T.);
#7854=EDGE_CURVE('',#6221,#6220,#5558,.T.);
#7855=EDGE_CURVE('',#6222,#6222,#5559,.T.);
#7856=EDGE_CURVE('',#6222,#6217,#3400,.T.);
#7857=EDGE_CURVE('',#6222,#6223,#3401,.T.);
#7858=EDGE_CURVE('',#6223,#6224,#5560,.T.);
#7859=EDGE_CURVE('',#6224,#6223,#5561,.T.);
#7860=EDGE_CURVE('',#6225,#6225,#5562,.T.);
#7861=EDGE_CURVE('',#6225,#6219,#3402,.T.);
#7862=EDGE_CURVE('',#6225,#6226,#3403,.T.);
#7863=EDGE_CURVE('',#6226,#6227,#5563,.T.);
#7864=EDGE_CURVE('',#6227,#6226,#5564,.T.);
#7865=EDGE_CURVE('',#6228,#6228,#5565,.T.);
#7866=EDGE_CURVE('',#6228,#6218,#3404,.T.);
#7867=EDGE_CURVE('',#6228,#6229,#3405,.T.);
#7868=EDGE_CURVE('',#6229,#6230,#5566,.T.);
#7869=EDGE_CURVE('',#6230,#6229,#5567,.T.);
#7870=EDGE_CURVE('',#6231,#6221,#3406,.T.);
#7871=EDGE_CURVE('',#6232,#6230,#3407,.T.);
#7872=EDGE_CURVE('',#6233,#6227,#3408,.T.);
#7873=EDGE_CURVE('',#6234,#6224,#3409,.T.);
#7874=EDGE_CURVE('',#6235,#6235,#5568,.T.);
#7875=EDGE_CURVE('',#6235,#6236,#3410,.T.);
#7876=EDGE_CURVE('',#6236,#6236,#5569,.T.);
#7877=EDGE_CURVE('',#6237,#6238,#3411,.T.);
#7878=EDGE_CURVE('',#6239,#6237,#3412,.T.);
#7879=EDGE_CURVE('',#6240,#6239,#3413,.T.);
#7880=EDGE_CURVE('',#6241,#6240,#3414,.T.);
#7881=EDGE_CURVE('',#6242,#6241,#3415,.T.);
#7882=EDGE_CURVE('',#6243,#6242,#3416,.T.);
#7883=EDGE_CURVE('',#6244,#6243,#3417,.T.);
#7884=EDGE_CURVE('',#6245,#6244,#3418,.T.);
#7885=EDGE_CURVE('',#6246,#6245,#3419,.T.);
#7886=EDGE_CURVE('',#6247,#6246,#3420,.T.);
#7887=EDGE_CURVE('',#6248,#6247,#3421,.T.);
#7888=EDGE_CURVE('',#6249,#6248,#3422,.T.);
#7889=EDGE_CURVE('',#6250,#6249,#3423,.T.);
#7890=EDGE_CURVE('',#6238,#6250,#3424,.T.);
#7891=EDGE_CURVE('',#6251,#6251,#5570,.T.);
#7892=EDGE_CURVE('',#6252,#6252,#5571,.T.);
#7893=EDGE_CURVE('',#6253,#6253,#5572,.T.);
#7894=EDGE_CURVE('',#6235,#6254,#3425,.T.);
#7895=EDGE_CURVE('',#6254,#6255,#5573,.T.);
#7896=EDGE_CURVE('',#6255,#6254,#5574,.T.);
#7897=EDGE_CURVE('',#6256,#6256,#5575,.T.);
#7898=EDGE_CURVE('',#6256,#6251,#3426,.T.);
#7899=EDGE_CURVE('',#6256,#6257,#3427,.T.);
#7900=EDGE_CURVE('',#6257,#6258,#5576,.T.);
#7901=EDGE_CURVE('',#6258,#6257,#5577,.T.);
#7902=EDGE_CURVE('',#6259,#6259,#5578,.T.);
#7903=EDGE_CURVE('',#6259,#6253,#3428,.T.);
#7904=EDGE_CURVE('',#6259,#6260,#3429,.T.);
#7905=EDGE_CURVE('',#6260,#6261,#5579,.T.);
#7906=EDGE_CURVE('',#6261,#6260,#5580,.T.);
#7907=EDGE_CURVE('',#6262,#6262,#5581,.T.);
#7908=EDGE_CURVE('',#6262,#6252,#3430,.T.);
#7909=EDGE_CURVE('',#6262,#6263,#3431,.T.);
#7910=EDGE_CURVE('',#6263,#6264,#5582,.T.);
#7911=EDGE_CURVE('',#6264,#6263,#5583,.T.);
#7912=EDGE_CURVE('',#6265,#6255,#3432,.T.);
#7913=EDGE_CURVE('',#6266,#6264,#3433,.T.);
#7914=EDGE_CURVE('',#6267,#6261,#3434,.T.);
#7915=EDGE_CURVE('',#6268,#6258,#3435,.T.);
#7916=EDGE_CURVE('',#6269,#6269,#5584,.T.);
#7917=EDGE_CURVE('',#6269,#6270,#3436,.T.);
#7918=EDGE_CURVE('',#6270,#6270,#5585,.T.);
#7919=EDGE_CURVE('',#6271,#6272,#3437,.T.);
#7920=EDGE_CURVE('',#6273,#6271,#3438,.T.);
#7921=EDGE_CURVE('',#6274,#6273,#3439,.T.);
#7922=EDGE_CURVE('',#6272,#6274,#3440,.T.);
#7923=EDGE_CURVE('',#6275,#6275,#5586,.T.);
#7924=EDGE_CURVE('',#6276,#6276,#5587,.T.);
#7925=EDGE_CURVE('',#6277,#6277,#5588,.T.);
#7926=EDGE_CURVE('',#6278,#6278,#5589,.T.);
#7927=EDGE_CURVE('',#6279,#6279,#5590,.T.);
#7928=EDGE_CURVE('',#6280,#6280,#5591,.T.);
#7929=EDGE_CURVE('',#6281,#6281,#5592,.T.);
#7930=EDGE_CURVE('',#6282,#6282,#5593,.T.);
#7931=EDGE_CURVE('',#6283,#6283,#5594,.T.);
#7932=EDGE_CURVE('',#6284,#6284,#5595,.T.);
#7933=EDGE_CURVE('',#6285,#6285,#5596,.T.);
#7934=EDGE_CURVE('',#6286,#6286,#5597,.T.);
#7935=EDGE_CURVE('',#6287,#6287,#5598,.T.);
#7936=EDGE_CURVE('',#6269,#6288,#3441,.T.);
#7937=EDGE_CURVE('',#6288,#6288,#5599,.T.);
#7938=EDGE_CURVE('',#6289,#6289,#5600,.T.);
#7939=EDGE_CURVE('',#6289,#6275,#3442,.T.);
#7940=EDGE_CURVE('',#6289,#6290,#3443,.T.);
#7941=EDGE_CURVE('',#6290,#6290,#5601,.T.);
#7942=EDGE_CURVE('',#6291,#6291,#5602,.T.);
#7943=EDGE_CURVE('',#6291,#6287,#3444,.T.);
#7944=EDGE_CURVE('',#6291,#6292,#3445,.T.);
#7945=EDGE_CURVE('',#6292,#6292,#5603,.T.);
#7946=EDGE_CURVE('',#6293,#6293,#5604,.T.);
#7947=EDGE_CURVE('',#6293,#6276,#3446,.T.);
#7948=EDGE_CURVE('',#6293,#6294,#3447,.T.);
#7949=EDGE_CURVE('',#6294,#6294,#5605,.T.);
#7950=EDGE_CURVE('',#6295,#6295,#5606,.T.);
#7951=EDGE_CURVE('',#6295,#6286,#3448,.T.);
#7952=EDGE_CURVE('',#6295,#6296,#3449,.T.);
#7953=EDGE_CURVE('',#6296,#6296,#5607,.T.);
#7954=EDGE_CURVE('',#6297,#6297,#5608,.T.);
#7955=EDGE_CURVE('',#6297,#6277,#3450,.T.);
#7956=EDGE_CURVE('',#6297,#6298,#3451,.T.);
#7957=EDGE_CURVE('',#6298,#6298,#5609,.T.);
#7958=EDGE_CURVE('',#6299,#6288,#3452,.T.);
#7959=EDGE_CURVE('',#6300,#6298,#3453,.T.);
#7960=EDGE_CURVE('',#6301,#6290,#3454,.T.);
#7961=EDGE_CURVE('',#6302,#6292,#3455,.T.);
#7962=EDGE_CURVE('',#6303,#6294,#3456,.T.);
#7963=EDGE_CURVE('',#6304,#6296,#3457,.T.);
#7964=EDGE_CURVE('',#6305,#6305,#5610,.T.);
#7965=EDGE_CURVE('',#6305,#6278,#3458,.T.);
#7966=EDGE_CURVE('',#6305,#6306,#3459,.T.);
#7967=EDGE_CURVE('',#6306,#6306,#5611,.T.);
#7968=EDGE_CURVE('',#6307,#6307,#5612,.T.);
#7969=EDGE_CURVE('',#6307,#6285,#3460,.T.);
#7970=EDGE_CURVE('',#6307,#6308,#3461,.T.);
#7971=EDGE_CURVE('',#6308,#6308,#5613,.T.);
#7972=EDGE_CURVE('',#6309,#6309,#5614,.T.);
#7973=EDGE_CURVE('',#6309,#6279,#3462,.T.);
#7974=EDGE_CURVE('',#6309,#6310,#3463,.T.);
#7975=EDGE_CURVE('',#6310,#6310,#5615,.T.);
#7976=EDGE_CURVE('',#6311,#6311,#5616,.T.);
#7977=EDGE_CURVE('',#6311,#6284,#3464,.T.);
#7978=EDGE_CURVE('',#6311,#6312,#3465,.T.);
#7979=EDGE_CURVE('',#6312,#6312,#5617,.T.);
#7980=EDGE_CURVE('',#6313,#6313,#5618,.T.);
#7981=EDGE_CURVE('',#6313,#6280,#3466,.T.);
#7982=EDGE_CURVE('',#6313,#6314,#3467,.T.);
#7983=EDGE_CURVE('',#6314,#6314,#5619,.T.);
#7984=EDGE_CURVE('',#6315,#6315,#5620,.T.);
#7985=EDGE_CURVE('',#6315,#6283,#3468,.T.);
#7986=EDGE_CURVE('',#6315,#6316,#3469,.T.);
#7987=EDGE_CURVE('',#6316,#6316,#5621,.T.);
#7988=EDGE_CURVE('',#6317,#6317,#5622,.T.);
#7989=EDGE_CURVE('',#6317,#6281,#3470,.T.);
#7990=EDGE_CURVE('',#6317,#6318,#3471,.T.);
#7991=EDGE_CURVE('',#6318,#6318,#5623,.T.);
#7992=EDGE_CURVE('',#6319,#6319,#5624,.T.);
#7993=EDGE_CURVE('',#6319,#6282,#3472,.T.);
#7994=EDGE_CURVE('',#6319,#6320,#3473,.T.);
#7995=EDGE_CURVE('',#6320,#6320,#5625,.T.);
#7996=EDGE_CURVE('',#6321,#6321,#5626,.T.);
#7997=EDGE_CURVE('',#6322,#6322,#5627,.T.);
#7998=EDGE_CURVE('',#6323,#6323,#5628,.T.);
#7999=EDGE_CURVE('',#6324,#6324,#5629,.T.);
#8000=EDGE_CURVE('',#6325,#6325,#5630,.T.);
#8001=EDGE_CURVE('',#6326,#6326,#5631,.T.);
#8002=EDGE_CURVE('',#6327,#6327,#5632,.T.);
#8003=EDGE_CURVE('',#6328,#6328,#5633,.T.);
#8004=EDGE_CURVE('',#6321,#6329,#3474,.T.);
#8005=EDGE_CURVE('',#6329,#6329,#5634,.T.);
#8006=EDGE_CURVE('',#6322,#6330,#3475,.T.);
#8007=EDGE_CURVE('',#6330,#6330,#5635,.T.);
#8008=EDGE_CURVE('',#6323,#6331,#3476,.T.);
#8009=EDGE_CURVE('',#6331,#6331,#5636,.T.);
#8010=EDGE_CURVE('',#6324,#6332,#3477,.T.);
#8011=EDGE_CURVE('',#6332,#6332,#5637,.T.);
#8012=EDGE_CURVE('',#6325,#6333,#3478,.T.);
#8013=EDGE_CURVE('',#6333,#6333,#5638,.T.);
#8014=EDGE_CURVE('',#6326,#6334,#3479,.T.);
#8015=EDGE_CURVE('',#6334,#6334,#5639,.T.);
#8016=EDGE_CURVE('',#6327,#6335,#3480,.T.);
#8017=EDGE_CURVE('',#6335,#6335,#5640,.T.);
#8018=EDGE_CURVE('',#6328,#6336,#3481,.T.);
#8019=EDGE_CURVE('',#6336,#6336,#5641,.T.);
#8020=EDGE_CURVE('',#6155,#6203,#3482,.T.);
#8021=EDGE_CURVE('',#6204,#6337,#3483,.T.);
#8022=EDGE_CURVE('',#6337,#6154,#3484,.T.);
#8023=EDGE_CURVE('',#6216,#6338,#3485,.T.);
#8024=EDGE_CURVE('',#6338,#6271,#3486,.T.);
#8025=EDGE_CURVE('',#6272,#6337,#3487,.T.);
#8026=EDGE_CURVE('',#6249,#6157,#3488,.T.);
#8027=EDGE_CURVE('',#6249,#6203,#3489,.T.);
#8028=EDGE_CURVE('',#6189,#6338,#3490,.T.);
#8029=EDGE_CURVE('',#6339,#6191,#3491,.T.);
#8030=EDGE_CURVE('',#6273,#6339,#3492,.T.);
#8031=EDGE_CURVE('',#6215,#6188,#3493,.T.);
#8032=EDGE_CURVE('',#6190,#6237,#3494,.T.);
#8033=EDGE_CURVE('',#6238,#6339,#3495,.T.);
#8034=EDGE_CURVE('',#6250,#6340,#3496,.T.);
#8035=EDGE_CURVE('',#6340,#6274,#3497,.T.);
#8036=EDGE_CURVE('',#6156,#6340,#3498,.T.);
#8037=EDGE_CURVE('',#6213,#6240,#3499,.T.);
#8038=EDGE_CURVE('',#6239,#6214,#3500,.T.);
#8039=EDGE_CURVE('',#6215,#6237,#3501,.T.);
#8040=EDGE_CURVE('',#6205,#6248,#3502,.T.);
#8041=EDGE_CURVE('',#6247,#6206,#3503,.T.);
#8042=EDGE_CURVE('',#6246,#6207,#3504,.T.);
#8043=EDGE_CURVE('',#6241,#6212,#3505,.T.);
#8044=EDGE_CURVE('',#6242,#6211,#3506,.T.);
#8045=EDGE_CURVE('',#6243,#6210,#3507,.T.);
#8046=EDGE_CURVE('',#6244,#6209,#3508,.T.);
#8047=EDGE_CURVE('',#6245,#6208,#3509,.T.);
#8048=EDGE_CURVE('',#6341,#6341,#5642,.T.);
#8049=EDGE_CURVE('',#6341,#6342,#3510,.T.);
#8050=EDGE_CURVE('',#6342,#6342,#5643,.T.);
#8051=EDGE_CURVE('',#6343,#6344,#3511,.T.);
#8052=EDGE_CURVE('',#6345,#6343,#3512,.T.);
#8053=EDGE_CURVE('',#6345,#6346,#3513,.T.);
#8054=EDGE_CURVE('',#6347,#6346,#3514,.T.);
#8055=EDGE_CURVE('',#6348,#6347,#3515,.T.);
#8056=EDGE_CURVE('',#6349,#6348,#3516,.T.);
#8057=EDGE_CURVE('',#6349,#6350,#3517,.T.);
#8058=EDGE_CURVE('',#6351,#6350,#3518,.T.);
#8059=EDGE_CURVE('',#6351,#6352,#3519,.T.);
#8060=EDGE_CURVE('',#6352,#6353,#3520,.T.);
#8061=EDGE_CURVE('',#6353,#6354,#3521,.T.);
#8062=EDGE_CURVE('',#6354,#6355,#3522,.T.);
#8063=EDGE_CURVE('',#6355,#6356,#3523,.T.);
#8064=EDGE_CURVE('',#6357,#6356,#3524,.T.);
#8065=EDGE_CURVE('',#6357,#6342,#3525,.T.);
#8066=EDGE_CURVE('',#6342,#6358,#3526,.T.);
#8067=EDGE_CURVE('',#6344,#6358,#3527,.T.);
#8068=EDGE_CURVE('',#6341,#6359,#3528,.T.);
#8069=EDGE_CURVE('',#6359,#6360,#5644,.T.);
#8070=EDGE_CURVE('',#6360,#6359,#5645,.T.);
#8071=EDGE_CURVE('',#6361,#6360,#3529,.T.);
#8072=EDGE_CURVE('',#6362,#6362,#5646,.T.);
#8073=EDGE_CURVE('',#6362,#6363,#3530,.T.);
#8074=EDGE_CURVE('',#6363,#6363,#5647,.T.);
#8075=EDGE_CURVE('',#6364,#6365,#3531,.T.);
#8076=EDGE_CURVE('',#6366,#6364,#3532,.T.);
#8077=EDGE_CURVE('',#6366,#6363,#3533,.T.);
#8078=EDGE_CURVE('',#6363,#6367,#3534,.T.);
#8079=EDGE_CURVE('',#6368,#6367,#3535,.T.);
#8080=EDGE_CURVE('',#6368,#6369,#3536,.T.);
#8081=EDGE_CURVE('',#6369,#6370,#3537,.T.);
#8082=EDGE_CURVE('',#6370,#6371,#3538,.T.);
#8083=EDGE_CURVE('',#6371,#6372,#3539,.T.);
#8084=EDGE_CURVE('',#6372,#6373,#3540,.T.);
#8085=EDGE_CURVE('',#6374,#6373,#3541,.T.);
#8086=EDGE_CURVE('',#6374,#6375,#3542,.T.);
#8087=EDGE_CURVE('',#6376,#6375,#3543,.T.);
#8088=EDGE_CURVE('',#6377,#6376,#3544,.T.);
#8089=EDGE_CURVE('',#6378,#6377,#3545,.T.);
#8090=EDGE_CURVE('',#6378,#6379,#3546,.T.);
#8091=EDGE_CURVE('',#6365,#6379,#3547,.T.);
#8092=EDGE_CURVE('',#6362,#6380,#3548,.T.);
#8093=EDGE_CURVE('',#6380,#6381,#5648,.T.);
#8094=EDGE_CURVE('',#6381,#6380,#5649,.T.);
#8095=EDGE_CURVE('',#6382,#6381,#3549,.T.);
#8096=EDGE_CURVE('',#6383,#6383,#5650,.T.);
#8097=EDGE_CURVE('',#6383,#6384,#3550,.T.);
#8098=EDGE_CURVE('',#6384,#6384,#5651,.T.);
#8099=EDGE_CURVE('',#6379,#6345,#3551,.T.);
#8100=EDGE_CURVE('',#6346,#6378,#3552,.T.);
#8101=EDGE_CURVE('',#6385,#6385,#5652,.T.);
#8102=EDGE_CURVE('',#6386,#6386,#5653,.T.);
#8103=EDGE_CURVE('',#6383,#6387,#3553,.T.);
#8104=EDGE_CURVE('',#6388,#6387,#5654,.T.);
#8105=EDGE_CURVE('',#6389,#6388,#3554,.T.);
#8106=EDGE_CURVE('',#6390,#6389,#372,.T.);
#8107=EDGE_CURVE('',#6390,#6391,#5655,.T.);
#8108=EDGE_CURVE('',#6392,#6391,#373,.T.);
#8109=EDGE_CURVE('',#6393,#6392,#3555,.T.);
#8110=EDGE_CURVE('',#6394,#6393,#5656,.T.);
#8111=EDGE_CURVE('',#6395,#6394,#3556,.T.);
#8112=EDGE_CURVE('',#6396,#6395,#374,.T.);
#8113=EDGE_CURVE('',#6396,#6397,#5657,.T.);
#8114=EDGE_CURVE('',#6398,#6397,#375,.T.);
#8115=EDGE_CURVE('',#6399,#6398,#3557,.T.);
#8116=EDGE_CURVE('',#6387,#6399,#5658,.T.);
#8117=EDGE_CURVE('',#6400,#6400,#5659,.T.);
#8118=EDGE_CURVE('',#6400,#6385,#3558,.T.);
#8119=EDGE_CURVE('',#6400,#6401,#3559,.T.);
#8120=EDGE_CURVE('',#6402,#6401,#5660,.T.);
#8121=EDGE_CURVE('',#6403,#6402,#3560,.T.);
#8122=EDGE_CURVE('',#6404,#6403,#376,.T.);
#8123=EDGE_CURVE('',#6404,#6405,#5661,.T.);
#8124=EDGE_CURVE('',#6406,#6405,#377,.T.);
#8125=EDGE_CURVE('',#6407,#6406,#3561,.T.);
#8126=EDGE_CURVE('',#6408,#6407,#5662,.T.);
#8127=EDGE_CURVE('',#6409,#6408,#3562,.T.);
#8128=EDGE_CURVE('',#6410,#6409,#378,.T.);
#8129=EDGE_CURVE('',#6410,#6411,#5663,.T.);
#8130=EDGE_CURVE('',#6412,#6411,#379,.T.);
#8131=EDGE_CURVE('',#6413,#6412,#3563,.T.);
#8132=EDGE_CURVE('',#6401,#6413,#5664,.T.);
#8133=EDGE_CURVE('',#6414,#6414,#5665,.T.);
#8134=EDGE_CURVE('',#6414,#6386,#3564,.T.);
#8135=EDGE_CURVE('',#6414,#6415,#3565,.T.);
#8136=EDGE_CURVE('',#6416,#6415,#5666,.T.);
#8137=EDGE_CURVE('',#6417,#6416,#3566,.T.);
#8138=EDGE_CURVE('',#6418,#6417,#380,.T.);
#8139=EDGE_CURVE('',#6418,#6419,#5667,.T.);
#8140=EDGE_CURVE('',#6420,#6419,#381,.T.);
#8141=EDGE_CURVE('',#6421,#6420,#3567,.T.);
#8142=EDGE_CURVE('',#6422,#6421,#5668,.T.);
#8143=EDGE_CURVE('',#6423,#6422,#3568,.T.);
#8144=EDGE_CURVE('',#6424,#6423,#382,.T.);
#8145=EDGE_CURVE('',#6424,#6425,#5669,.T.);
#8146=EDGE_CURVE('',#6426,#6425,#383,.T.);
#8147=EDGE_CURVE('',#6427,#6426,#3569,.T.);
#8148=EDGE_CURVE('',#6415,#6427,#5670,.T.);
#8149=EDGE_CURVE('',#6419,#6418,#3570,.T.);
#8150=EDGE_CURVE('',#6425,#6424,#3571,.T.);
#8151=EDGE_CURVE('',#6405,#6404,#3572,.T.);
#8152=EDGE_CURVE('',#6411,#6410,#3573,.T.);
#8153=EDGE_CURVE('',#6391,#6390,#3574,.T.);
#8154=EDGE_CURVE('',#6397,#6396,#3575,.T.);
#8155=EDGE_CURVE('',#6423,#6412,#3576,.T.);
#8156=EDGE_CURVE('',#6409,#6398,#3577,.T.);
#8157=EDGE_CURVE('',#6395,#6352,#3578,.T.);
#8158=EDGE_CURVE('',#6373,#6351,#3579,.T.);
#8159=EDGE_CURVE('',#6372,#6426,#3580,.T.);
#8160=EDGE_CURVE('',#6394,#6353,#3581,.T.);
#8161=EDGE_CURVE('',#6408,#6399,#3582,.T.);
#8162=EDGE_CURVE('',#6422,#6413,#3583,.T.);
#8163=EDGE_CURVE('',#6393,#6354,#3584,.T.);
#8164=EDGE_CURVE('',#6407,#6388,#3585,.T.);
#8165=EDGE_CURVE('',#6421,#6402,#3586,.T.);
#8166=EDGE_CURVE('',#6392,#6355,#3587,.T.);
#8167=EDGE_CURVE('',#6406,#6389,#3588,.T.);
#8168=EDGE_CURVE('',#6420,#6403,#3589,.T.);
#8169=EDGE_CURVE('',#6428,#6343,#3590,.T.);
#8170=EDGE_CURVE('',#6344,#6429,#3591,.T.);
#8171=EDGE_CURVE('',#6429,#6428,#3592,.T.);
#8172=EDGE_CURVE('',#6430,#6429,#3593,.T.);
#8173=EDGE_CURVE('',#6431,#6430,#3594,.T.);
#8174=EDGE_CURVE('',#6428,#6431,#3595,.T.);
#8175=EDGE_CURVE('',#6358,#6366,#3596,.T.);
#8176=EDGE_CURVE('',#6430,#6364,#3597,.T.);
#8177=EDGE_CURVE('',#6432,#6348,#3598,.T.);
#8178=EDGE_CURVE('',#6347,#6433,#3599,.T.);
#8179=EDGE_CURVE('',#6433,#6432,#3600,.T.);
#8180=EDGE_CURVE('',#6432,#6434,#3601,.T.);
#8181=EDGE_CURVE('',#6376,#6434,#3602,.T.);
#8182=EDGE_CURVE('',#6375,#6349,#3603,.T.);
#8183=EDGE_CURVE('',#6435,#6433,#3604,.T.);
#8184=EDGE_CURVE('',#6434,#6435,#3605,.T.);
#8185=EDGE_CURVE('',#6365,#6431,#3606,.T.);
#8186=EDGE_CURVE('',#6435,#6377,#3607,.T.);
#8187=EDGE_CURVE('',#6350,#6374,#3608,.T.);
#8188=EDGE_CURVE('',#6356,#6368,#3609,.T.);
#8189=EDGE_CURVE('',#6367,#6357,#3610,.T.);
#8190=EDGE_CURVE('',#6369,#6417,#3611,.T.);
#8191=EDGE_CURVE('',#6370,#6416,#3612,.T.);
#8192=EDGE_CURVE('',#6371,#6427,#3613,.T.);
#8193=EDGE_CURVE('',#6436,#6436,#5671,.T.);
#8194=EDGE_CURVE('',#6436,#6437,#3614,.T.);
#8195=EDGE_CURVE('',#6437,#6438,#5672,.T.);
#8196=EDGE_CURVE('',#6438,#6437,#5673,.T.);
#8197=EDGE_CURVE('',#6439,#6440,#3615,.T.);
#8198=EDGE_CURVE('',#6441,#6439,#3616,.T.);
#8199=EDGE_CURVE('',#6441,#6442,#3617,.T.);
#8200=EDGE_CURVE('',#6443,#6442,#3618,.T.);
#8201=EDGE_CURVE('',#6443,#6444,#3619,.T.);
#8202=EDGE_CURVE('',#6444,#6445,#3620,.T.);
#8203=EDGE_CURVE('',#6445,#6446,#3621,.T.);
#8204=EDGE_CURVE('',#6446,#6447,#3622,.T.);
#8205=EDGE_CURVE('',#6447,#6448,#3623,.T.);
#8206=EDGE_CURVE('',#6449,#6448,#3624,.T.);
#8207=EDGE_CURVE('',#6449,#6438,#3625,.T.);
#8208=EDGE_CURVE('',#6438,#6450,#3626,.T.);
#8209=EDGE_CURVE('',#6451,#6450,#3627,.T.);
#8210=EDGE_CURVE('',#6452,#6451,#3628,.T.);
#8211=EDGE_CURVE('',#6453,#6452,#3629,.T.);
#8212=EDGE_CURVE('',#6453,#6454,#3630,.T.);
#8213=EDGE_CURVE('',#6440,#6454,#3631,.T.);
#8214=EDGE_CURVE('',#6436,#6455,#3632,.T.);
#8215=EDGE_CURVE('',#6455,#6456,#5674,.T.);
#8216=EDGE_CURVE('',#6456,#6455,#5675,.T.);
#8217=EDGE_CURVE('',#6457,#6456,#3633,.T.);
#8218=EDGE_CURVE('',#6458,#6458,#5676,.T.);
#8219=EDGE_CURVE('',#6458,#6459,#3634,.T.);
#8220=EDGE_CURVE('',#6459,#6460,#5677,.T.);
#8221=EDGE_CURVE('',#6460,#6459,#5678,.T.);
#8222=EDGE_CURVE('',#6461,#6462,#3635,.T.);
#8223=EDGE_CURVE('',#6463,#6461,#3636,.T.);
#8224=EDGE_CURVE('',#6460,#6463,#3637,.T.);
#8225=EDGE_CURVE('',#6464,#6460,#3638,.T.);
#8226=EDGE_CURVE('',#6465,#6464,#3639,.T.);
#8227=EDGE_CURVE('',#6466,#6465,#3640,.T.);
#8228=EDGE_CURVE('',#6467,#6466,#3641,.T.);
#8229=EDGE_CURVE('',#6468,#6467,#3642,.T.);
#8230=EDGE_CURVE('',#6469,#6468,#3643,.T.);
#8231=EDGE_CURVE('',#6470,#6469,#3644,.T.);
#8232=EDGE_CURVE('',#6471,#6470,#3645,.T.);
#8233=EDGE_CURVE('',#6472,#6471,#3646,.T.);
#8234=EDGE_CURVE('',#6473,#6472,#3647,.T.);
#8235=EDGE_CURVE('',#6474,#6473,#3648,.T.);
#8236=EDGE_CURVE('',#6475,#6474,#3649,.T.);
#8237=EDGE_CURVE('',#6476,#6475,#3650,.T.);
#8238=EDGE_CURVE('',#6462,#6476,#3651,.T.);
#8239=EDGE_CURVE('',#6458,#6477,#3652,.T.);
#8240=EDGE_CURVE('',#6477,#6478,#5679,.T.);
#8241=EDGE_CURVE('',#6478,#6477,#5680,.T.);
#8242=EDGE_CURVE('',#6479,#6478,#3653,.T.);
#8243=EDGE_CURVE('',#6480,#6480,#5681,.T.);
#8244=EDGE_CURVE('',#6480,#6481,#3654,.T.);
#8245=EDGE_CURVE('',#6481,#6481,#5682,.T.);
#8246=EDGE_CURVE('',#6454,#6475,#3655,.T.);
#8247=EDGE_CURVE('',#6476,#6453,#3656,.T.);
#8248=EDGE_CURVE('',#6482,#6482,#5683,.T.);
#8249=EDGE_CURVE('',#6483,#6483,#5684,.T.);
#8250=EDGE_CURVE('',#6484,#6484,#5685,.T.);
#8251=EDGE_CURVE('',#6480,#6485,#3657,.T.);
#8252=EDGE_CURVE('',#6486,#6485,#5686,.T.);
#8253=EDGE_CURVE('',#6487,#6486,#3658,.T.);
#8254=EDGE_CURVE('',#6488,#6487,#384,.T.);
#8255=EDGE_CURVE('',#6488,#6489,#5687,.T.);
#8256=EDGE_CURVE('',#6490,#6489,#385,.T.);
#8257=EDGE_CURVE('',#6491,#6490,#3659,.T.);
#8258=EDGE_CURVE('',#6492,#6491,#5688,.T.);
#8259=EDGE_CURVE('',#6493,#6492,#3660,.T.);
#8260=EDGE_CURVE('',#6494,#6493,#386,.T.);
#8261=EDGE_CURVE('',#6494,#6495,#5689,.T.);
#8262=EDGE_CURVE('',#6496,#6495,#387,.T.);
#8263=EDGE_CURVE('',#6497,#6496,#3661,.T.);
#8264=EDGE_CURVE('',#6485,#6497,#5690,.T.);
#8265=EDGE_CURVE('',#6498,#6498,#5691,.T.);
#8266=EDGE_CURVE('',#6498,#6482,#3662,.T.);
#8267=EDGE_CURVE('',#6498,#6499,#3663,.T.);
#8268=EDGE_CURVE('',#6500,#6499,#5692,.T.);
#8269=EDGE_CURVE('',#6501,#6500,#3664,.T.);
#8270=EDGE_CURVE('',#6502,#6501,#388,.T.);
#8271=EDGE_CURVE('',#6502,#6503,#5693,.T.);
#8272=EDGE_CURVE('',#6504,#6503,#389,.T.);
#8273=EDGE_CURVE('',#6505,#6504,#3665,.T.);
#8274=EDGE_CURVE('',#6506,#6505,#5694,.T.);
#8275=EDGE_CURVE('',#6507,#6506,#3666,.T.);
#8276=EDGE_CURVE('',#6508,#6507,#390,.T.);
#8277=EDGE_CURVE('',#6508,#6509,#5695,.T.);
#8278=EDGE_CURVE('',#6510,#6509,#391,.T.);
#8279=EDGE_CURVE('',#6511,#6510,#3667,.T.);
#8280=EDGE_CURVE('',#6499,#6511,#5696,.T.);
#8281=EDGE_CURVE('',#6512,#6512,#5697,.T.);
#8282=EDGE_CURVE('',#6512,#6484,#3668,.T.);
#8283=EDGE_CURVE('',#6512,#6513,#3669,.T.);
#8284=EDGE_CURVE('',#6514,#6513,#5698,.T.);
#8285=EDGE_CURVE('',#6515,#6514,#3670,.T.);
#8286=EDGE_CURVE('',#6516,#6515,#392,.T.);
#8287=EDGE_CURVE('',#6516,#6517,#5699,.T.);
#8288=EDGE_CURVE('',#6518,#6517,#393,.T.);
#8289=EDGE_CURVE('',#6519,#6518,#3671,.T.);
#8290=EDGE_CURVE('',#6520,#6519,#5700,.T.);
#8291=EDGE_CURVE('',#6521,#6520,#3672,.T.);
#8292=EDGE_CURVE('',#6522,#6521,#394,.T.);
#8293=EDGE_CURVE('',#6522,#6523,#5701,.T.);
#8294=EDGE_CURVE('',#6524,#6523,#395,.T.);
#8295=EDGE_CURVE('',#6525,#6524,#3673,.T.);
#8296=EDGE_CURVE('',#6513,#6525,#5702,.T.);
#8297=EDGE_CURVE('',#6526,#6526,#5703,.T.);
#8298=EDGE_CURVE('',#6526,#6483,#3674,.T.);
#8299=EDGE_CURVE('',#6526,#6527,#3675,.T.);
#8300=EDGE_CURVE('',#6528,#6527,#5704,.T.);
#8301=EDGE_CURVE('',#6529,#6528,#3676,.T.);
#8302=EDGE_CURVE('',#6530,#6529,#396,.T.);
#8303=EDGE_CURVE('',#6530,#6531,#5705,.T.);
#8304=EDGE_CURVE('',#6532,#6531,#397,.T.);
#8305=EDGE_CURVE('',#6533,#6532,#3677,.T.);
#8306=EDGE_CURVE('',#6534,#6533,#5706,.T.);
#8307=EDGE_CURVE('',#6535,#6534,#3678,.T.);
#8308=EDGE_CURVE('',#6536,#6535,#398,.T.);
#8309=EDGE_CURVE('',#6536,#6537,#5707,.T.);
#8310=EDGE_CURVE('',#6538,#6537,#399,.T.);
#8311=EDGE_CURVE('',#6539,#6538,#3679,.T.);
#8312=EDGE_CURVE('',#6527,#6539,#5708,.T.);
#8313=EDGE_CURVE('',#6531,#6530,#3680,.T.);
#8314=EDGE_CURVE('',#6537,#6536,#3681,.T.);
#8315=EDGE_CURVE('',#6517,#6516,#3682,.T.);
#8316=EDGE_CURVE('',#6523,#6522,#3683,.T.);
#8317=EDGE_CURVE('',#6503,#6502,#3684,.T.);
#8318=EDGE_CURVE('',#6509,#6508,#3685,.T.);
#8319=EDGE_CURVE('',#6489,#6488,#3686,.T.);
#8320=EDGE_CURVE('',#6495,#6494,#3687,.T.);
#8321=EDGE_CURVE('',#6535,#6496,#3688,.T.);
#8322=EDGE_CURVE('',#6493,#6444,#3689,.T.);
#8323=EDGE_CURVE('',#6470,#6443,#3690,.T.);
#8324=EDGE_CURVE('',#6469,#6510,#3691,.T.);
#8325=EDGE_CURVE('',#6507,#6524,#3692,.T.);
#8326=EDGE_CURVE('',#6521,#6538,#3693,.T.);
#8327=EDGE_CURVE('',#6492,#6445,#3694,.T.);
#8328=EDGE_CURVE('',#6534,#6497,#3695,.T.);
#8329=EDGE_CURVE('',#6468,#6511,#3696,.T.);
#8330=EDGE_CURVE('',#6506,#6525,#3697,.T.);
#8331=EDGE_CURVE('',#6491,#6446,#3698,.T.);
#8332=EDGE_CURVE('',#6533,#6486,#3699,.T.);
#8333=EDGE_CURVE('',#6467,#6500,#3700,.T.);
#8334=EDGE_CURVE('',#6505,#6514,#3701,.T.);
#8335=EDGE_CURVE('',#6490,#6447,#3702,.T.);
#8336=EDGE_CURVE('',#6532,#6487,#3703,.T.);
#8337=EDGE_CURVE('',#6466,#6501,#3704,.T.);
#8338=EDGE_CURVE('',#6504,#6515,#3705,.T.);
#8339=EDGE_CURVE('',#6540,#6439,#3706,.T.);
#8340=EDGE_CURVE('',#6440,#6541,#3707,.T.);
#8341=EDGE_CURVE('',#6541,#6540,#3708,.T.);
#8342=EDGE_CURVE('',#6542,#6474,#3709,.T.);
#8343=EDGE_CURVE('',#6542,#6541,#3710,.T.);
#8344=EDGE_CURVE('',#6543,#6452,#3711,.T.);
#8345=EDGE_CURVE('',#6451,#6544,#3712,.T.);
#8346=EDGE_CURVE('',#6544,#6543,#3713,.T.);
#8347=EDGE_CURVE('',#6543,#6545,#3714,.T.);
#8348=EDGE_CURVE('',#6462,#6545,#3715,.T.);
#8349=EDGE_CURVE('',#6545,#6546,#3716,.T.);
#8350=EDGE_CURVE('',#6546,#6461,#3717,.T.);
#8351=EDGE_CURVE('',#6473,#6547,#3718,.T.);
#8352=EDGE_CURVE('',#6547,#6542,#3719,.T.);
#8353=EDGE_CURVE('',#6442,#6471,#3720,.T.);
#8354=EDGE_CURVE('',#6472,#6441,#3721,.T.);
#8355=EDGE_CURVE('',#6448,#6465,#3722,.T.);
#8356=EDGE_CURVE('',#6464,#6449,#3723,.T.);
#8357=EDGE_CURVE('',#6518,#6529,#3724,.T.);
#8358=EDGE_CURVE('',#6540,#6547,#3725,.T.);
#8359=EDGE_CURVE('',#6450,#6463,#3726,.T.);
#8360=EDGE_CURVE('',#6546,#6544,#3727,.T.);
#8361=EDGE_CURVE('',#6519,#6528,#3728,.T.);
#8362=EDGE_CURVE('',#6520,#6539,#3729,.T.);
#8363=EDGE_CURVE('',#6548,#6549,#3730,.T.);
#8364=EDGE_CURVE('',#6548,#6550,#3731,.T.);
#8365=EDGE_CURVE('',#6551,#6550,#3732,.T.);
#8366=EDGE_CURVE('',#6549,#6551,#3733,.T.);
#8367=EDGE_CURVE('',#6552,#6548,#5709,.T.);
#8368=EDGE_CURVE('',#6552,#6553,#3734,.T.);
#8369=EDGE_CURVE('',#6550,#6553,#5710,.T.);
#8370=EDGE_CURVE('',#6554,#6552,#3735,.T.);
#8371=EDGE_CURVE('',#6554,#6555,#3736,.T.);
#8372=EDGE_CURVE('',#6553,#6555,#3737,.T.);
#8373=EDGE_CURVE('',#6556,#6554,#5711,.T.);
#8374=EDGE_CURVE('',#6556,#6557,#3738,.T.);
#8375=EDGE_CURVE('',#6555,#6557,#5712,.T.);
#8376=EDGE_CURVE('',#6558,#6556,#3739,.T.);
#8377=EDGE_CURVE('',#6558,#6559,#3740,.T.);
#8378=EDGE_CURVE('',#6557,#6559,#3741,.T.);
#8379=EDGE_CURVE('',#6560,#6558,#5713,.T.);
#8380=EDGE_CURVE('',#6560,#6561,#3742,.T.);
#8381=EDGE_CURVE('',#6559,#6561,#5714,.T.);
#8382=EDGE_CURVE('',#6562,#6560,#3743,.T.);
#8383=EDGE_CURVE('',#6562,#6563,#3744,.T.);
#8384=EDGE_CURVE('',#6561,#6563,#3745,.T.);
#8385=EDGE_CURVE('',#6549,#6562,#5715,.T.);
#8386=EDGE_CURVE('',#6563,#6551,#5716,.T.);
#8387=EDGE_CURVE('',#6564,#6565,#3746,.T.);
#8388=EDGE_CURVE('',#6564,#6566,#3747,.T.);
#8389=EDGE_CURVE('',#6567,#6566,#3748,.T.);
#8390=EDGE_CURVE('',#6565,#6567,#3749,.T.);
#8391=EDGE_CURVE('',#6568,#6564,#5717,.T.);
#8392=EDGE_CURVE('',#6568,#6569,#3750,.T.);
#8393=EDGE_CURVE('',#6566,#6569,#5718,.T.);
#8394=EDGE_CURVE('',#6570,#6568,#3751,.T.);
#8395=EDGE_CURVE('',#6570,#6571,#3752,.T.);
#8396=EDGE_CURVE('',#6569,#6571,#3753,.T.);
#8397=EDGE_CURVE('',#6572,#6570,#5719,.T.);
#8398=EDGE_CURVE('',#6572,#6573,#3754,.T.);
#8399=EDGE_CURVE('',#6571,#6573,#5720,.T.);
#8400=EDGE_CURVE('',#6574,#6572,#3755,.T.);
#8401=EDGE_CURVE('',#6574,#6575,#3756,.T.);
#8402=EDGE_CURVE('',#6573,#6575,#3757,.T.);
#8403=EDGE_CURVE('',#6576,#6574,#5721,.T.);
#8404=EDGE_CURVE('',#6576,#6577,#3758,.T.);
#8405=EDGE_CURVE('',#6575,#6577,#5722,.T.);
#8406=EDGE_CURVE('',#6578,#6576,#3759,.T.);
#8407=EDGE_CURVE('',#6578,#6579,#3760,.T.);
#8408=EDGE_CURVE('',#6577,#6579,#3761,.T.);
#8409=EDGE_CURVE('',#6565,#6578,#5723,.T.);
#8410=EDGE_CURVE('',#6579,#6567,#5724,.T.);
#8411=EDGE_CURVE('',#6580,#6581,#3762,.T.);
#8412=EDGE_CURVE('',#6580,#6582,#3763,.T.);
#8413=EDGE_CURVE('',#6583,#6582,#3764,.T.);
#8414=EDGE_CURVE('',#6581,#6583,#3765,.T.);
#8415=EDGE_CURVE('',#6584,#6580,#5725,.T.);
#8416=EDGE_CURVE('',#6584,#6585,#3766,.T.);
#8417=EDGE_CURVE('',#6582,#6585,#5726,.T.);
#8418=EDGE_CURVE('',#6586,#6584,#3767,.T.);
#8419=EDGE_CURVE('',#6586,#6587,#3768,.T.);
#8420=EDGE_CURVE('',#6585,#6587,#3769,.T.);
#8421=EDGE_CURVE('',#6588,#6586,#5727,.T.);
#8422=EDGE_CURVE('',#6588,#6589,#3770,.T.);
#8423=EDGE_CURVE('',#6587,#6589,#5728,.T.);
#8424=EDGE_CURVE('',#6590,#6588,#3771,.T.);
#8425=EDGE_CURVE('',#6590,#6591,#3772,.T.);
#8426=EDGE_CURVE('',#6589,#6591,#3773,.T.);
#8427=EDGE_CURVE('',#6592,#6590,#5729,.T.);
#8428=EDGE_CURVE('',#6592,#6593,#3774,.T.);
#8429=EDGE_CURVE('',#6591,#6593,#5730,.T.);
#8430=EDGE_CURVE('',#6594,#6592,#3775,.T.);
#8431=EDGE_CURVE('',#6594,#6595,#3776,.T.);
#8432=EDGE_CURVE('',#6593,#6595,#3777,.T.);
#8433=EDGE_CURVE('',#6581,#6594,#5731,.T.);
#8434=EDGE_CURVE('',#6595,#6583,#5732,.T.);
#8435=EDGE_CURVE('',#6596,#6597,#3778,.T.);
#8436=EDGE_CURVE('',#6596,#6598,#3779,.T.);
#8437=EDGE_CURVE('',#6599,#6598,#3780,.T.);
#8438=EDGE_CURVE('',#6597,#6599,#3781,.T.);
#8439=EDGE_CURVE('',#6600,#6596,#5733,.T.);
#8440=EDGE_CURVE('',#6600,#6601,#3782,.T.);
#8441=EDGE_CURVE('',#6598,#6601,#5734,.T.);
#8442=EDGE_CURVE('',#6602,#6600,#3783,.T.);
#8443=EDGE_CURVE('',#6602,#6603,#3784,.T.);
#8444=EDGE_CURVE('',#6601,#6603,#3785,.T.);
#8445=EDGE_CURVE('',#6604,#6602,#5735,.T.);
#8446=EDGE_CURVE('',#6604,#6605,#3786,.T.);
#8447=EDGE_CURVE('',#6603,#6605,#5736,.T.);
#8448=EDGE_CURVE('',#6606,#6604,#3787,.T.);
#8449=EDGE_CURVE('',#6606,#6607,#3788,.T.);
#8450=EDGE_CURVE('',#6605,#6607,#3789,.T.);
#8451=EDGE_CURVE('',#6608,#6606,#5737,.T.);
#8452=EDGE_CURVE('',#6608,#6609,#3790,.T.);
#8453=EDGE_CURVE('',#6607,#6609,#5738,.T.);
#8454=EDGE_CURVE('',#6610,#6608,#3791,.T.);
#8455=EDGE_CURVE('',#6610,#6611,#3792,.T.);
#8456=EDGE_CURVE('',#6609,#6611,#3793,.T.);
#8457=EDGE_CURVE('',#6597,#6610,#5739,.T.);
#8458=EDGE_CURVE('',#6611,#6599,#5740,.T.);
#8459=EDGE_CURVE('',#6612,#6613,#3794,.T.);
#8460=EDGE_CURVE('',#6612,#6614,#3795,.T.);
#8461=EDGE_CURVE('',#6615,#6614,#3796,.T.);
#8462=EDGE_CURVE('',#6613,#6615,#3797,.T.);
#8463=EDGE_CURVE('',#6616,#6612,#5741,.T.);
#8464=EDGE_CURVE('',#6616,#6617,#3798,.T.);
#8465=EDGE_CURVE('',#6614,#6617,#5742,.T.);
#8466=EDGE_CURVE('',#6618,#6616,#3799,.T.);
#8467=EDGE_CURVE('',#6618,#6619,#3800,.T.);
#8468=EDGE_CURVE('',#6617,#6619,#3801,.T.);
#8469=EDGE_CURVE('',#6620,#6618,#5743,.T.);
#8470=EDGE_CURVE('',#6620,#6621,#3802,.T.);
#8471=EDGE_CURVE('',#6619,#6621,#5744,.T.);
#8472=EDGE_CURVE('',#6622,#6620,#3803,.T.);
#8473=EDGE_CURVE('',#6622,#6623,#3804,.T.);
#8474=EDGE_CURVE('',#6621,#6623,#3805,.T.);
#8475=EDGE_CURVE('',#6624,#6622,#5745,.T.);
#8476=EDGE_CURVE('',#6624,#6625,#3806,.T.);
#8477=EDGE_CURVE('',#6623,#6625,#5746,.T.);
#8478=EDGE_CURVE('',#6626,#6624,#3807,.T.);
#8479=EDGE_CURVE('',#6626,#6627,#3808,.T.);
#8480=EDGE_CURVE('',#6625,#6627,#3809,.T.);
#8481=EDGE_CURVE('',#6613,#6626,#5747,.T.);
#8482=EDGE_CURVE('',#6627,#6615,#5748,.T.);
#8483=EDGE_CURVE('',#6628,#6629,#3810,.T.);
#8484=EDGE_CURVE('',#6628,#6630,#3811,.T.);
#8485=EDGE_CURVE('',#6631,#6630,#3812,.T.);
#8486=EDGE_CURVE('',#6629,#6631,#3813,.T.);
#8487=EDGE_CURVE('',#6632,#6628,#5749,.T.);
#8488=EDGE_CURVE('',#6632,#6633,#3814,.T.);
#8489=EDGE_CURVE('',#6630,#6633,#5750,.T.);
#8490=EDGE_CURVE('',#6634,#6632,#3815,.T.);
#8491=EDGE_CURVE('',#6634,#6635,#3816,.T.);
#8492=EDGE_CURVE('',#6633,#6635,#3817,.T.);
#8493=EDGE_CURVE('',#6636,#6634,#5751,.T.);
#8494=EDGE_CURVE('',#6636,#6637,#3818,.T.);
#8495=EDGE_CURVE('',#6635,#6637,#5752,.T.);
#8496=EDGE_CURVE('',#6638,#6636,#3819,.T.);
#8497=EDGE_CURVE('',#6638,#6639,#3820,.T.);
#8498=EDGE_CURVE('',#6637,#6639,#3821,.T.);
#8499=EDGE_CURVE('',#6640,#6638,#5753,.T.);
#8500=EDGE_CURVE('',#6640,#6641,#3822,.T.);
#8501=EDGE_CURVE('',#6639,#6641,#5754,.T.);
#8502=EDGE_CURVE('',#6642,#6640,#3823,.T.);
#8503=EDGE_CURVE('',#6642,#6643,#3824,.T.);
#8504=EDGE_CURVE('',#6641,#6643,#3825,.T.);
#8505=EDGE_CURVE('',#6629,#6642,#5755,.T.);
#8506=EDGE_CURVE('',#6643,#6631,#5756,.T.);
#8507=EDGE_CURVE('',#6644,#6645,#3826,.T.);
#8508=EDGE_CURVE('',#6644,#6646,#3827,.T.);
#8509=EDGE_CURVE('',#6647,#6646,#3828,.T.);
#8510=EDGE_CURVE('',#6645,#6647,#3829,.T.);
#8511=EDGE_CURVE('',#6648,#6644,#5757,.T.);
#8512=EDGE_CURVE('',#6648,#6649,#3830,.T.);
#8513=EDGE_CURVE('',#6646,#6649,#5758,.T.);
#8514=EDGE_CURVE('',#6650,#6648,#3831,.T.);
#8515=EDGE_CURVE('',#6650,#6651,#3832,.T.);
#8516=EDGE_CURVE('',#6649,#6651,#3833,.T.);
#8517=EDGE_CURVE('',#6652,#6650,#5759,.T.);
#8518=EDGE_CURVE('',#6652,#6653,#3834,.T.);
#8519=EDGE_CURVE('',#6651,#6653,#5760,.T.);
#8520=EDGE_CURVE('',#6654,#6652,#3835,.T.);
#8521=EDGE_CURVE('',#6654,#6655,#3836,.T.);
#8522=EDGE_CURVE('',#6653,#6655,#3837,.T.);
#8523=EDGE_CURVE('',#6656,#6654,#5761,.T.);
#8524=EDGE_CURVE('',#6656,#6657,#3838,.T.);
#8525=EDGE_CURVE('',#6655,#6657,#5762,.T.);
#8526=EDGE_CURVE('',#6658,#6656,#3839,.T.);
#8527=EDGE_CURVE('',#6658,#6659,#3840,.T.);
#8528=EDGE_CURVE('',#6657,#6659,#3841,.T.);
#8529=EDGE_CURVE('',#6645,#6658,#5763,.T.);
#8530=EDGE_CURVE('',#6659,#6647,#5764,.T.);
#8531=EDGE_CURVE('',#6660,#6661,#3842,.T.);
#8532=EDGE_CURVE('',#6660,#6662,#3843,.T.);
#8533=EDGE_CURVE('',#6663,#6662,#3844,.T.);
#8534=EDGE_CURVE('',#6661,#6663,#3845,.T.);
#8535=EDGE_CURVE('',#6664,#6660,#5765,.T.);
#8536=EDGE_CURVE('',#6664,#6665,#3846,.T.);
#8537=EDGE_CURVE('',#6662,#6665,#5766,.T.);
#8538=EDGE_CURVE('',#6666,#6664,#3847,.T.);
#8539=EDGE_CURVE('',#6666,#6667,#3848,.T.);
#8540=EDGE_CURVE('',#6665,#6667,#3849,.T.);
#8541=EDGE_CURVE('',#6668,#6666,#5767,.T.);
#8542=EDGE_CURVE('',#6668,#6669,#3850,.T.);
#8543=EDGE_CURVE('',#6667,#6669,#5768,.T.);
#8544=EDGE_CURVE('',#6670,#6668,#3851,.T.);
#8545=EDGE_CURVE('',#6670,#6671,#3852,.T.);
#8546=EDGE_CURVE('',#6669,#6671,#3853,.T.);
#8547=EDGE_CURVE('',#6672,#6670,#5769,.T.);
#8548=EDGE_CURVE('',#6672,#6673,#3854,.T.);
#8549=EDGE_CURVE('',#6671,#6673,#5770,.T.);
#8550=EDGE_CURVE('',#6674,#6672,#3855,.T.);
#8551=EDGE_CURVE('',#6674,#6675,#3856,.T.);
#8552=EDGE_CURVE('',#6673,#6675,#3857,.T.);
#8553=EDGE_CURVE('',#6661,#6674,#5771,.T.);
#8554=EDGE_CURVE('',#6675,#6663,#5772,.T.);
#8555=EDGE_CURVE('',#6676,#6677,#3858,.T.);
#8556=EDGE_CURVE('',#6676,#6678,#3859,.T.);
#8557=EDGE_CURVE('',#6679,#6678,#3860,.T.);
#8558=EDGE_CURVE('',#6677,#6679,#3861,.T.);
#8559=EDGE_CURVE('',#6680,#6676,#5773,.T.);
#8560=EDGE_CURVE('',#6680,#6681,#3862,.T.);
#8561=EDGE_CURVE('',#6678,#6681,#5774,.T.);
#8562=EDGE_CURVE('',#6682,#6680,#3863,.T.);
#8563=EDGE_CURVE('',#6682,#6683,#3864,.T.);
#8564=EDGE_CURVE('',#6681,#6683,#3865,.T.);
#8565=EDGE_CURVE('',#6684,#6682,#5775,.T.);
#8566=EDGE_CURVE('',#6684,#6685,#3866,.T.);
#8567=EDGE_CURVE('',#6683,#6685,#5776,.T.);
#8568=EDGE_CURVE('',#6686,#6684,#3867,.T.);
#8569=EDGE_CURVE('',#6686,#6687,#3868,.T.);
#8570=EDGE_CURVE('',#6685,#6687,#3869,.T.);
#8571=EDGE_CURVE('',#6688,#6686,#5777,.T.);
#8572=EDGE_CURVE('',#6688,#6689,#3870,.T.);
#8573=EDGE_CURVE('',#6687,#6689,#5778,.T.);
#8574=EDGE_CURVE('',#6690,#6688,#3871,.T.);
#8575=EDGE_CURVE('',#6690,#6691,#3872,.T.);
#8576=EDGE_CURVE('',#6689,#6691,#3873,.T.);
#8577=EDGE_CURVE('',#6677,#6690,#5779,.T.);
#8578=EDGE_CURVE('',#6691,#6679,#5780,.T.);
#8579=EDGE_CURVE('',#6692,#6693,#3874,.T.);
#8580=EDGE_CURVE('',#6692,#6694,#3875,.T.);
#8581=EDGE_CURVE('',#6695,#6694,#3876,.T.);
#8582=EDGE_CURVE('',#6693,#6695,#3877,.T.);
#8583=EDGE_CURVE('',#6696,#6692,#5781,.T.);
#8584=EDGE_CURVE('',#6696,#6697,#3878,.T.);
#8585=EDGE_CURVE('',#6694,#6697,#5782,.T.);
#8586=EDGE_CURVE('',#6698,#6696,#3879,.T.);
#8587=EDGE_CURVE('',#6698,#6699,#3880,.T.);
#8588=EDGE_CURVE('',#6697,#6699,#3881,.T.);
#8589=EDGE_CURVE('',#6700,#6698,#5783,.T.);
#8590=EDGE_CURVE('',#6700,#6701,#3882,.T.);
#8591=EDGE_CURVE('',#6699,#6701,#5784,.T.);
#8592=EDGE_CURVE('',#6702,#6700,#3883,.T.);
#8593=EDGE_CURVE('',#6702,#6703,#3884,.T.);
#8594=EDGE_CURVE('',#6701,#6703,#3885,.T.);
#8595=EDGE_CURVE('',#6704,#6702,#5785,.T.);
#8596=EDGE_CURVE('',#6704,#6705,#3886,.T.);
#8597=EDGE_CURVE('',#6703,#6705,#5786,.T.);
#8598=EDGE_CURVE('',#6706,#6704,#3887,.T.);
#8599=EDGE_CURVE('',#6706,#6707,#3888,.T.);
#8600=EDGE_CURVE('',#6705,#6707,#3889,.T.);
#8601=EDGE_CURVE('',#6693,#6706,#5787,.T.);
#8602=EDGE_CURVE('',#6707,#6695,#5788,.T.);
#8603=EDGE_CURVE('',#6708,#6709,#3890,.T.);
#8604=EDGE_CURVE('',#6708,#6710,#3891,.T.);
#8605=EDGE_CURVE('',#6711,#6710,#3892,.T.);
#8606=EDGE_CURVE('',#6709,#6711,#3893,.T.);
#8607=EDGE_CURVE('',#6712,#6708,#5789,.T.);
#8608=EDGE_CURVE('',#6712,#6713,#3894,.T.);
#8609=EDGE_CURVE('',#6710,#6713,#5790,.T.);
#8610=EDGE_CURVE('',#6714,#6712,#3895,.T.);
#8611=EDGE_CURVE('',#6714,#6715,#3896,.T.);
#8612=EDGE_CURVE('',#6713,#6715,#3897,.T.);
#8613=EDGE_CURVE('',#6716,#6714,#5791,.T.);
#8614=EDGE_CURVE('',#6716,#6717,#3898,.T.);
#8615=EDGE_CURVE('',#6715,#6717,#5792,.T.);
#8616=EDGE_CURVE('',#6718,#6716,#3899,.T.);
#8617=EDGE_CURVE('',#6718,#6719,#3900,.T.);
#8618=EDGE_CURVE('',#6717,#6719,#3901,.T.);
#8619=EDGE_CURVE('',#6720,#6718,#5793,.T.);
#8620=EDGE_CURVE('',#6720,#6721,#3902,.T.);
#8621=EDGE_CURVE('',#6719,#6721,#5794,.T.);
#8622=EDGE_CURVE('',#6722,#6720,#3903,.T.);
#8623=EDGE_CURVE('',#6722,#6723,#3904,.T.);
#8624=EDGE_CURVE('',#6721,#6723,#3905,.T.);
#8625=EDGE_CURVE('',#6709,#6722,#5795,.T.);
#8626=EDGE_CURVE('',#6723,#6711,#5796,.T.);
#8627=EDGE_CURVE('',#6724,#6725,#3906,.T.);
#8628=EDGE_CURVE('',#6724,#6726,#3907,.T.);
#8629=EDGE_CURVE('',#6727,#6726,#3908,.T.);
#8630=EDGE_CURVE('',#6725,#6727,#3909,.T.);
#8631=EDGE_CURVE('',#6728,#6724,#5797,.T.);
#8632=EDGE_CURVE('',#6728,#6729,#3910,.T.);
#8633=EDGE_CURVE('',#6726,#6729,#5798,.T.);
#8634=EDGE_CURVE('',#6730,#6728,#3911,.T.);
#8635=EDGE_CURVE('',#6730,#6731,#3912,.T.);
#8636=EDGE_CURVE('',#6729,#6731,#3913,.T.);
#8637=EDGE_CURVE('',#6732,#6730,#5799,.T.);
#8638=EDGE_CURVE('',#6732,#6733,#3914,.T.);
#8639=EDGE_CURVE('',#6731,#6733,#5800,.T.);
#8640=EDGE_CURVE('',#6734,#6732,#3915,.T.);
#8641=EDGE_CURVE('',#6734,#6735,#3916,.T.);
#8642=EDGE_CURVE('',#6733,#6735,#3917,.T.);
#8643=EDGE_CURVE('',#6736,#6734,#5801,.T.);
#8644=EDGE_CURVE('',#6736,#6737,#3918,.T.);
#8645=EDGE_CURVE('',#6735,#6737,#5802,.T.);
#8646=EDGE_CURVE('',#6738,#6736,#3919,.T.);
#8647=EDGE_CURVE('',#6738,#6739,#3920,.T.);
#8648=EDGE_CURVE('',#6737,#6739,#3921,.T.);
#8649=EDGE_CURVE('',#6725,#6738,#5803,.T.);
#8650=EDGE_CURVE('',#6739,#6727,#5804,.T.);
#8651=EDGE_CURVE('',#6740,#6741,#3922,.T.);
#8652=EDGE_CURVE('',#6740,#6742,#3923,.T.);
#8653=EDGE_CURVE('',#6743,#6742,#3924,.T.);
#8654=EDGE_CURVE('',#6741,#6743,#3925,.T.);
#8655=EDGE_CURVE('',#6744,#6740,#5805,.T.);
#8656=EDGE_CURVE('',#6744,#6745,#3926,.T.);
#8657=EDGE_CURVE('',#6742,#6745,#5806,.T.);
#8658=EDGE_CURVE('',#6746,#6744,#3927,.T.);
#8659=EDGE_CURVE('',#6746,#6747,#3928,.T.);
#8660=EDGE_CURVE('',#6745,#6747,#3929,.T.);
#8661=EDGE_CURVE('',#6748,#6746,#5807,.T.);
#8662=EDGE_CURVE('',#6748,#6749,#3930,.T.);
#8663=EDGE_CURVE('',#6747,#6749,#5808,.T.);
#8664=EDGE_CURVE('',#6750,#6748,#3931,.T.);
#8665=EDGE_CURVE('',#6750,#6751,#3932,.T.);
#8666=EDGE_CURVE('',#6749,#6751,#3933,.T.);
#8667=EDGE_CURVE('',#6752,#6750,#5809,.T.);
#8668=EDGE_CURVE('',#6752,#6753,#3934,.T.);
#8669=EDGE_CURVE('',#6751,#6753,#5810,.T.);
#8670=EDGE_CURVE('',#6754,#6752,#3935,.T.);
#8671=EDGE_CURVE('',#6754,#6755,#3936,.T.);
#8672=EDGE_CURVE('',#6753,#6755,#3937,.T.);
#8673=EDGE_CURVE('',#6741,#6754,#5811,.T.);
#8674=EDGE_CURVE('',#6755,#6743,#5812,.T.);
#8675=EDGE_CURVE('',#6756,#6757,#3938,.T.);
#8676=EDGE_CURVE('',#6756,#6758,#3939,.T.);
#8677=EDGE_CURVE('',#6759,#6758,#3940,.T.);
#8678=EDGE_CURVE('',#6757,#6759,#3941,.T.);
#8679=EDGE_CURVE('',#6760,#6756,#5813,.T.);
#8680=EDGE_CURVE('',#6760,#6761,#3942,.T.);
#8681=EDGE_CURVE('',#6758,#6761,#5814,.T.);
#8682=EDGE_CURVE('',#6762,#6760,#3943,.T.);
#8683=EDGE_CURVE('',#6762,#6763,#3944,.T.);
#8684=EDGE_CURVE('',#6761,#6763,#3945,.T.);
#8685=EDGE_CURVE('',#6764,#6762,#5815,.T.);
#8686=EDGE_CURVE('',#6764,#6765,#3946,.T.);
#8687=EDGE_CURVE('',#6763,#6765,#5816,.T.);
#8688=EDGE_CURVE('',#6766,#6764,#3947,.T.);
#8689=EDGE_CURVE('',#6766,#6767,#3948,.T.);
#8690=EDGE_CURVE('',#6765,#6767,#3949,.T.);
#8691=EDGE_CURVE('',#6768,#6766,#5817,.T.);
#8692=EDGE_CURVE('',#6768,#6769,#3950,.T.);
#8693=EDGE_CURVE('',#6767,#6769,#5818,.T.);
#8694=EDGE_CURVE('',#6770,#6768,#3951,.T.);
#8695=EDGE_CURVE('',#6770,#6771,#3952,.T.);
#8696=EDGE_CURVE('',#6769,#6771,#3953,.T.);
#8697=EDGE_CURVE('',#6757,#6770,#5819,.T.);
#8698=EDGE_CURVE('',#6771,#6759,#5820,.T.);
#8699=EDGE_CURVE('',#6772,#6773,#3954,.T.);
#8700=EDGE_CURVE('',#6772,#6774,#3955,.T.);
#8701=EDGE_CURVE('',#6775,#6774,#3956,.T.);
#8702=EDGE_CURVE('',#6773,#6775,#3957,.T.);
#8703=EDGE_CURVE('',#6776,#6772,#5821,.T.);
#8704=EDGE_CURVE('',#6776,#6777,#3958,.T.);
#8705=EDGE_CURVE('',#6774,#6777,#5822,.T.);
#8706=EDGE_CURVE('',#6778,#6776,#3959,.T.);
#8707=EDGE_CURVE('',#6778,#6779,#3960,.T.);
#8708=EDGE_CURVE('',#6777,#6779,#3961,.T.);
#8709=EDGE_CURVE('',#6780,#6778,#5823,.T.);
#8710=EDGE_CURVE('',#6780,#6781,#3962,.T.);
#8711=EDGE_CURVE('',#6779,#6781,#5824,.T.);
#8712=EDGE_CURVE('',#6782,#6780,#3963,.T.);
#8713=EDGE_CURVE('',#6782,#6783,#3964,.T.);
#8714=EDGE_CURVE('',#6781,#6783,#3965,.T.);
#8715=EDGE_CURVE('',#6784,#6782,#5825,.T.);
#8716=EDGE_CURVE('',#6784,#6785,#3966,.T.);
#8717=EDGE_CURVE('',#6783,#6785,#5826,.T.);
#8718=EDGE_CURVE('',#6786,#6784,#3967,.T.);
#8719=EDGE_CURVE('',#6786,#6787,#3968,.T.);
#8720=EDGE_CURVE('',#6785,#6787,#3969,.T.);
#8721=EDGE_CURVE('',#6773,#6786,#5827,.T.);
#8722=EDGE_CURVE('',#6787,#6775,#5828,.T.);
#8723=EDGE_CURVE('',#6788,#6789,#3970,.T.);
#8724=EDGE_CURVE('',#6789,#6790,#3971,.T.);
#8725=EDGE_CURVE('',#6791,#6790,#3972,.T.);
#8726=EDGE_CURVE('',#6788,#6791,#3973,.T.);
#8727=EDGE_CURVE('',#6792,#6788,#5829,.T.);
#8728=EDGE_CURVE('',#6793,#6791,#5830,.T.);
#8729=EDGE_CURVE('',#6792,#6793,#3974,.T.);
#8730=EDGE_CURVE('',#6794,#6792,#3975,.T.);
#8731=EDGE_CURVE('',#6795,#6793,#3976,.T.);
#8732=EDGE_CURVE('',#6794,#6795,#3977,.T.);
#8733=EDGE_CURVE('',#6796,#6794,#5831,.T.);
#8734=EDGE_CURVE('',#6797,#6795,#5832,.T.);
#8735=EDGE_CURVE('',#6796,#6797,#3978,.T.);
#8736=EDGE_CURVE('',#6798,#6796,#3979,.T.);
#8737=EDGE_CURVE('',#6799,#6797,#3980,.T.);
#8738=EDGE_CURVE('',#6798,#6799,#3981,.T.);
#8739=EDGE_CURVE('',#6800,#6798,#5833,.T.);
#8740=EDGE_CURVE('',#6801,#6799,#5834,.T.);
#8741=EDGE_CURVE('',#6800,#6801,#3982,.T.);
#8742=EDGE_CURVE('',#6802,#6800,#3983,.T.);
#8743=EDGE_CURVE('',#6803,#6801,#3984,.T.);
#8744=EDGE_CURVE('',#6802,#6803,#3985,.T.);
#8745=EDGE_CURVE('',#6789,#6802,#5835,.T.);
#8746=EDGE_CURVE('',#6790,#6803,#5836,.T.);
#8747=EDGE_CURVE('',#6804,#6804,#5837,.T.);
#8748=EDGE_CURVE('',#6805,#6805,#5838,.T.);
#8749=EDGE_CURVE('',#6805,#6804,#3986,.T.);
#8750=EDGE_CURVE('',#6806,#6806,#5839,.T.);
#8751=EDGE_CURVE('',#6806,#6805,#3987,.T.);
#8752=EDGE_CURVE('',#6806,#6807,#3988,.T.);
#8753=EDGE_CURVE('',#6807,#6807,#5840,.T.);
#8754=EDGE_CURVE('',#6808,#6809,#3989,.T.);
#8755=EDGE_CURVE('',#6810,#6808,#408,.F.);
#8756=EDGE_CURVE('',#6811,#6810,#5841,.T.);
#8757=EDGE_CURVE('',#6811,#6809,#409,.T.);
#8758=EDGE_CURVE('',#6812,#6813,#3990,.T.);
#8759=EDGE_CURVE('',#6808,#6812,#410,.F.);
#8760=EDGE_CURVE('',#6809,#6814,#411,.T.);
#8761=EDGE_CURVE('',#6814,#6813,#412,.T.);
#8762=EDGE_CURVE('',#6815,#6816,#3991,.T.);
#8763=EDGE_CURVE('',#6817,#6815,#413,.F.);
#8764=EDGE_CURVE('',#6812,#6817,#414,.F.);
#8765=EDGE_CURVE('',#6813,#6816,#415,.T.);
#8766=EDGE_CURVE('',#6818,#6819,#3992,.T.);
#8767=EDGE_CURVE('',#6815,#6818,#416,.F.);
#8768=EDGE_CURVE('',#6816,#6820,#417,.T.);
#8769=EDGE_CURVE('',#6820,#6819,#418,.T.);
#8770=EDGE_CURVE('',#6821,#6822,#3993,.T.);
#8771=EDGE_CURVE('',#6823,#6821,#419,.F.);
#8772=EDGE_CURVE('',#6818,#6823,#420,.F.);
#8773=EDGE_CURVE('',#6819,#6822,#421,.T.);
#8774=EDGE_CURVE('',#6824,#6825,#3994,.T.);
#8775=EDGE_CURVE('',#6821,#6824,#422,.F.);
#8776=EDGE_CURVE('',#6822,#6826,#423,.T.);
#8777=EDGE_CURVE('',#6826,#6825,#424,.T.);
#8778=EDGE_CURVE('',#6827,#6828,#3995,.T.);
#8779=EDGE_CURVE('',#6829,#6827,#425,.T.);
#8780=EDGE_CURVE('',#6824,#6829,#426,.F.);
#8781=EDGE_CURVE('',#6825,#6828,#427,.T.);
#8782=EDGE_CURVE('',#6830,#6831,#3996,.T.);
#8783=EDGE_CURVE('',#6832,#6830,#428,.F.);
#8784=EDGE_CURVE('',#6827,#6832,#429,.T.);
#8785=EDGE_CURVE('',#6828,#6833,#430,.T.);
#8786=EDGE_CURVE('',#6833,#6831,#431,.T.);
#8787=EDGE_CURVE('',#6834,#6835,#3997,.T.);
#8788=EDGE_CURVE('',#6830,#6834,#432,.F.);
#8789=EDGE_CURVE('',#6831,#6835,#433,.T.);
#8790=EDGE_CURVE('',#6836,#6837,#3998,.T.);
#8791=EDGE_CURVE('',#6838,#6836,#434,.T.);
#8792=EDGE_CURVE('',#6834,#6838,#435,.F.);
#8793=EDGE_CURVE('',#6835,#6839,#436,.T.);
#8794=EDGE_CURVE('',#6839,#6837,#437,.T.);
#8795=EDGE_CURVE('',#6840,#6841,#3999,.T.);
#8796=EDGE_CURVE('',#6842,#6840,#438,.T.);
#8797=EDGE_CURVE('',#6836,#6842,#439,.T.);
#8798=EDGE_CURVE('',#6837,#6843,#440,.T.);
#8799=EDGE_CURVE('',#6843,#6841,#441,.T.);
#8800=EDGE_CURVE('',#6844,#6845,#4000,.T.);
#8801=EDGE_CURVE('',#6846,#6844,#442,.F.);
#8802=EDGE_CURVE('',#6840,#6846,#443,.T.);
#8803=EDGE_CURVE('',#6841,#6845,#444,.T.);
#8804=EDGE_CURVE('',#6847,#6848,#4001,.T.);
#8805=EDGE_CURVE('',#6844,#6847,#445,.F.);
#8806=EDGE_CURVE('',#6845,#6849,#446,.T.);
#8807=EDGE_CURVE('',#6849,#6848,#447,.T.);
#8808=EDGE_CURVE('',#6850,#6851,#4002,.T.);
#8809=EDGE_CURVE('',#6852,#6850,#448,.F.);
#8810=EDGE_CURVE('',#6847,#6852,#449,.F.);
#8811=EDGE_CURVE('',#6848,#6851,#450,.T.);
#8812=EDGE_CURVE('',#6853,#6854,#4003,.T.);
#8813=EDGE_CURVE('',#6850,#6853,#451,.F.);
#8814=EDGE_CURVE('',#6851,#6855,#452,.T.);
#8815=EDGE_CURVE('',#6855,#6854,#453,.T.);
#8816=EDGE_CURVE('',#6856,#6857,#4004,.T.);
#8817=EDGE_CURVE('',#6858,#6856,#454,.F.);
#8818=EDGE_CURVE('',#6853,#6858,#455,.F.);
#8819=EDGE_CURVE('',#6854,#6857,#456,.T.);
#8820=EDGE_CURVE('',#6859,#6860,#4005,.T.);
#8821=EDGE_CURVE('',#6856,#6859,#457,.F.);
#8822=EDGE_CURVE('',#6857,#6861,#458,.T.);
#8823=EDGE_CURVE('',#6861,#6860,#459,.T.);
#8824=EDGE_CURVE('',#6862,#6863,#4006,.T.);
#8825=EDGE_CURVE('',#6864,#6862,#460,.F.);
#8826=EDGE_CURVE('',#6859,#6864,#461,.F.);
#8827=EDGE_CURVE('',#6860,#6863,#462,.T.);
#8828=EDGE_CURVE('',#6865,#6866,#4007,.T.);
#8829=EDGE_CURVE('',#6862,#6865,#463,.F.);
#8830=EDGE_CURVE('',#6863,#6867,#464,.T.);
#8831=EDGE_CURVE('',#6867,#6866,#465,.T.);
#8832=EDGE_CURVE('',#6868,#6869,#4008,.T.);
#8833=EDGE_CURVE('',#6870,#6868,#466,.F.);
#8834=EDGE_CURVE('',#6865,#6870,#467,.F.);
#8835=EDGE_CURVE('',#6866,#6869,#468,.T.);
#8836=EDGE_CURVE('',#6871,#6872,#4009,.T.);
#8837=EDGE_CURVE('',#6868,#6871,#469,.F.);
#8838=EDGE_CURVE('',#6869,#6873,#470,.T.);
#8839=EDGE_CURVE('',#6873,#6872,#471,.T.);
#8840=EDGE_CURVE('',#6874,#6875,#4010,.T.);
#8841=EDGE_CURVE('',#6876,#6874,#472,.F.);
#8842=EDGE_CURVE('',#6871,#6876,#473,.F.);
#8843=EDGE_CURVE('',#6872,#6875,#474,.T.);
#8844=EDGE_CURVE('',#6877,#6878,#4011,.T.);
#8845=EDGE_CURVE('',#6874,#6877,#475,.F.);
#8846=EDGE_CURVE('',#6875,#6879,#476,.T.);
#8847=EDGE_CURVE('',#6879,#6878,#477,.T.);
#8848=EDGE_CURVE('',#6880,#6881,#4012,.T.);
#8849=EDGE_CURVE('',#6882,#6880,#478,.T.);
#8850=EDGE_CURVE('',#6877,#6882,#479,.F.);
#8851=EDGE_CURVE('',#6878,#6883,#480,.T.);
#8852=EDGE_CURVE('',#6883,#6881,#481,.T.);
#8853=EDGE_CURVE('',#6884,#6885,#482,.T.);
#8854=EDGE_CURVE('',#6886,#6885,#5842,.T.);
#8855=EDGE_CURVE('',#6886,#6887,#483,.T.);
#8856=EDGE_CURVE('',#6887,#6888,#484,.T.);
#8857=EDGE_CURVE('',#6888,#6889,#485,.T.);
#8858=EDGE_CURVE('',#6889,#6890,#486,.T.);
#8859=EDGE_CURVE('',#6890,#6891,#487,.T.);
#8860=EDGE_CURVE('',#6891,#6892,#488,.T.);
#8861=EDGE_CURVE('',#6892,#6893,#489,.T.);
#8862=EDGE_CURVE('',#6893,#6894,#490,.T.);
#8863=EDGE_CURVE('',#6894,#6895,#491,.T.);
#8864=EDGE_CURVE('',#6895,#6896,#492,.T.);
#8865=EDGE_CURVE('',#6896,#6897,#493,.T.);
#8866=EDGE_CURVE('',#6897,#6898,#494,.T.);
#8867=EDGE_CURVE('',#6898,#6899,#495,.T.);
#8868=EDGE_CURVE('',#6899,#6900,#496,.T.);
#8869=EDGE_CURVE('',#6900,#6901,#497,.T.);
#8870=EDGE_CURVE('',#6901,#6902,#498,.T.);
#8871=EDGE_CURVE('',#6902,#6903,#499,.T.);
#8872=EDGE_CURVE('',#6903,#6904,#500,.T.);
#8873=EDGE_CURVE('',#6904,#6905,#501,.T.);
#8874=EDGE_CURVE('',#6905,#6906,#502,.T.);
#8875=EDGE_CURVE('',#6906,#6907,#503,.T.);
#8876=EDGE_CURVE('',#6907,#6908,#504,.T.);
#8877=EDGE_CURVE('',#6908,#6909,#505,.T.);
#8878=EDGE_CURVE('',#6909,#6910,#506,.T.);
#8879=EDGE_CURVE('',#6910,#6911,#507,.T.);
#8880=EDGE_CURVE('',#6912,#6911,#5843,.T.);
#8881=EDGE_CURVE('',#6912,#6913,#508,.T.);
#8882=EDGE_CURVE('',#6913,#6914,#509,.T.);
#8883=EDGE_CURVE('',#6914,#6915,#510,.T.);
#8884=EDGE_CURVE('',#6915,#6916,#511,.T.);
#8885=EDGE_CURVE('',#6916,#6917,#512,.T.);
#8886=EDGE_CURVE('',#6917,#6918,#513,.T.);
#8887=EDGE_CURVE('',#6918,#6919,#514,.T.);
#8888=EDGE_CURVE('',#6919,#6920,#515,.T.);
#8889=EDGE_CURVE('',#6920,#6921,#516,.T.);
#8890=EDGE_CURVE('',#6921,#6922,#517,.T.);
#8891=EDGE_CURVE('',#6922,#6923,#518,.T.);
#8892=EDGE_CURVE('',#6923,#6924,#519,.T.);
#8893=EDGE_CURVE('',#6924,#6925,#520,.T.);
#8894=EDGE_CURVE('',#6925,#6926,#521,.T.);
#8895=EDGE_CURVE('',#6926,#6927,#522,.T.);
#8896=EDGE_CURVE('',#6927,#6928,#523,.T.);
#8897=EDGE_CURVE('',#6928,#6929,#524,.T.);
#8898=EDGE_CURVE('',#6929,#6930,#525,.T.);
#8899=EDGE_CURVE('',#6930,#6931,#526,.T.);
#8900=EDGE_CURVE('',#6931,#6932,#527,.T.);
#8901=EDGE_CURVE('',#6932,#6933,#528,.T.);
#8902=EDGE_CURVE('',#6933,#6934,#529,.T.);
#8903=EDGE_CURVE('',#6934,#6935,#530,.T.);
#8904=EDGE_CURVE('',#6935,#6884,#531,.T.);
#8905=EDGE_CURVE('',#6881,#6936,#532,.T.);
#8906=EDGE_CURVE('',#6936,#6937,#533,.T.);
#8907=EDGE_CURVE('',#6938,#6937,#5844,.T.);
#8908=EDGE_CURVE('',#6939,#6938,#534,.T.);
#8909=EDGE_CURVE('',#6880,#6939,#535,.T.);
#8910=EDGE_CURVE('',#6940,#6941,#5845,.T.);
#8911=EDGE_CURVE('',#6940,#6938,#536,.T.);
#8912=EDGE_CURVE('',#6937,#6912,#537,.T.);
#8913=EDGE_CURVE('',#6941,#6912,#5846,.T.);
#8914=EDGE_CURVE('',#6911,#6940,#538,.T.);
#8915=EDGE_CURVE('',#6942,#6886,#539,.T.);
#8916=EDGE_CURVE('',#6942,#6810,#540,.T.);
#8917=EDGE_CURVE('',#6943,#6944,#5847,.T.);
#8918=EDGE_CURVE('',#6943,#6811,#541,.T.);
#8919=EDGE_CURVE('',#6944,#6886,#5848,.T.);
#8920=EDGE_CURVE('',#6885,#6943,#542,.T.);
#8921=EDGE_CURVE('',#6945,#6945,#5849,.T.);
#8922=EDGE_CURVE('',#6945,#6944,#5850,.T.);
#8923=EDGE_CURVE('',#6946,#6946,#5851,.T.);
#8924=EDGE_CURVE('',#6941,#6947,#4013,.T.);
#8925=EDGE_CURVE('',#6947,#6947,#5852,.T.);
#8926=EDGE_CURVE('',#6948,#6949,#5853,.T.);
#8927=EDGE_CURVE('',#6950,#6948,#4014,.T.);
#8928=EDGE_CURVE('',#6949,#6950,#4015,.T.);
#8929=EDGE_CURVE('',#6949,#6951,#4016,.T.);
#8930=EDGE_CURVE('',#6952,#6950,#4017,.T.);
#8931=EDGE_CURVE('',#6951,#6952,#260,.T.);
#8932=EDGE_CURVE('',#6953,#6948,#4018,.T.);
#8933=EDGE_CURVE('',#6952,#6953,#261,.T.);
#8934=EDGE_CURVE('',#6954,#6955,#5854,.T.);
#8935=EDGE_CURVE('',#6955,#6956,#4019,.T.);
#8936=EDGE_CURVE('',#6956,#6956,#5855,.T.);
#8937=EDGE_CURVE('',#6955,#6957,#5856,.T.);
#8938=EDGE_CURVE('',#6957,#6958,#4020,.T.);
#8939=EDGE_CURVE('',#6959,#6958,#5857,.T.);
#8940=EDGE_CURVE('',#6959,#6960,#4021,.T.);
#8941=EDGE_CURVE('',#6960,#6961,#5858,.T.);
#8942=EDGE_CURVE('',#6961,#6962,#4022,.T.);
#8943=EDGE_CURVE('',#6963,#6962,#5859,.T.);
#8944=EDGE_CURVE('',#6963,#6964,#4023,.T.);
#8945=EDGE_CURVE('',#6964,#6965,#5860,.T.);
#8946=EDGE_CURVE('',#6965,#6966,#4024,.T.);
#8947=EDGE_CURVE('',#6967,#6966,#5861,.T.);
#8948=EDGE_CURVE('',#6967,#6968,#4025,.T.);
#8949=EDGE_CURVE('',#6968,#6969,#5862,.T.);
#8950=EDGE_CURVE('',#6969,#6970,#4026,.T.);
#8951=EDGE_CURVE('',#6971,#6970,#5863,.T.);
#8952=EDGE_CURVE('',#6971,#6972,#4027,.T.);
#8953=EDGE_CURVE('',#6972,#6973,#5864,.T.);
#8954=EDGE_CURVE('',#6973,#6974,#4028,.T.);
#8955=EDGE_CURVE('',#6975,#6974,#5865,.T.);
#8956=EDGE_CURVE('',#6975,#6976,#4029,.T.);
#8957=EDGE_CURVE('',#6976,#6977,#5866,.T.);
#8958=EDGE_CURVE('',#6977,#6978,#4030,.T.);
#8959=EDGE_CURVE('',#6979,#6978,#5867,.T.);
#8960=EDGE_CURVE('',#6979,#6980,#4031,.T.);
#8961=EDGE_CURVE('',#6980,#6981,#5868,.T.);
#8962=EDGE_CURVE('',#6981,#6982,#4032,.T.);
#8963=EDGE_CURVE('',#6983,#6982,#5869,.T.);
#8964=EDGE_CURVE('',#6983,#6984,#4033,.T.);
#8965=EDGE_CURVE('',#6984,#6985,#5870,.T.);
#8966=EDGE_CURVE('',#6985,#6986,#4034,.T.);
#8967=EDGE_CURVE('',#6987,#6986,#5871,.T.);
#8968=EDGE_CURVE('',#6987,#6988,#4035,.T.);
#8969=EDGE_CURVE('',#6988,#6989,#5872,.T.);
#8970=EDGE_CURVE('',#6989,#6990,#4036,.T.);
#8971=EDGE_CURVE('',#6991,#6990,#5873,.T.);
#8972=EDGE_CURVE('',#6991,#6992,#4037,.T.);
#8973=EDGE_CURVE('',#6992,#6993,#5874,.T.);
#8974=EDGE_CURVE('',#6993,#6994,#4038,.T.);
#8975=EDGE_CURVE('',#6995,#6994,#5875,.T.);
#8976=EDGE_CURVE('',#6995,#6996,#4039,.T.);
#8977=EDGE_CURVE('',#6996,#6997,#5876,.T.);
#8978=EDGE_CURVE('',#6997,#6998,#4040,.T.);
#8979=EDGE_CURVE('',#6999,#6998,#5877,.T.);
#8980=EDGE_CURVE('',#6999,#7000,#4041,.T.);
#8981=EDGE_CURVE('',#7000,#7001,#5878,.T.);
#8982=EDGE_CURVE('',#7001,#7002,#4042,.T.);
#8983=EDGE_CURVE('',#7003,#7002,#5879,.T.);
#8984=EDGE_CURVE('',#7003,#7004,#4043,.T.);
#8985=EDGE_CURVE('',#7004,#7005,#5880,.T.);
#8986=EDGE_CURVE('',#7005,#7006,#4044,.T.);
#8987=EDGE_CURVE('',#7007,#7006,#5881,.T.);
#8988=EDGE_CURVE('',#7007,#7008,#4045,.T.);
#8989=EDGE_CURVE('',#7008,#7009,#5882,.T.);
#8990=EDGE_CURVE('',#7009,#7010,#4046,.T.);
#8991=EDGE_CURVE('',#7011,#7010,#5883,.T.);
#8992=EDGE_CURVE('',#7011,#7012,#4047,.T.);
#8993=EDGE_CURVE('',#7012,#7013,#5884,.T.);
#8994=EDGE_CURVE('',#7013,#7014,#4048,.T.);
#8995=EDGE_CURVE('',#7015,#7014,#5885,.T.);
#8996=EDGE_CURVE('',#7015,#7016,#4049,.T.);
#8997=EDGE_CURVE('',#7016,#7017,#5886,.T.);
#8998=EDGE_CURVE('',#7017,#7018,#4050,.T.);
#8999=EDGE_CURVE('',#7019,#7018,#5887,.T.);
#9000=EDGE_CURVE('',#7019,#7020,#4051,.T.);
#9001=EDGE_CURVE('',#7020,#7021,#5888,.T.);
#9002=EDGE_CURVE('',#7021,#7022,#4052,.T.);
#9003=EDGE_CURVE('',#6953,#7022,#5889,.T.);
#9004=EDGE_CURVE('',#7023,#6951,#5890,.T.);
#9005=EDGE_CURVE('',#7023,#7024,#4053,.T.);
#9006=EDGE_CURVE('',#7024,#7025,#5891,.T.);
#9007=EDGE_CURVE('',#7025,#7026,#4054,.T.);
#9008=EDGE_CURVE('',#7027,#7026,#5892,.T.);
#9009=EDGE_CURVE('',#7027,#7028,#4055,.T.);
#9010=EDGE_CURVE('',#7028,#7029,#5893,.T.);
#9011=EDGE_CURVE('',#7029,#7030,#4056,.T.);
#9012=EDGE_CURVE('',#7031,#7030,#5894,.T.);
#9013=EDGE_CURVE('',#7031,#7032,#4057,.T.);
#9014=EDGE_CURVE('',#7032,#7033,#5895,.T.);
#9015=EDGE_CURVE('',#7033,#7034,#4058,.T.);
#9016=EDGE_CURVE('',#7035,#7034,#5896,.T.);
#9017=EDGE_CURVE('',#7035,#7036,#4059,.T.);
#9018=EDGE_CURVE('',#7036,#7037,#5897,.T.);
#9019=EDGE_CURVE('',#7037,#7038,#4060,.T.);
#9020=EDGE_CURVE('',#7039,#7038,#5898,.T.);
#9021=EDGE_CURVE('',#7039,#7040,#4061,.T.);
#9022=EDGE_CURVE('',#7040,#7041,#5899,.T.);
#9023=EDGE_CURVE('',#7041,#7042,#4062,.T.);
#9024=EDGE_CURVE('',#7043,#7042,#5900,.T.);
#9025=EDGE_CURVE('',#7043,#7044,#4063,.T.);
#9026=EDGE_CURVE('',#7044,#7045,#5901,.T.);
#9027=EDGE_CURVE('',#7045,#7046,#4064,.T.);
#9028=EDGE_CURVE('',#7047,#7046,#5902,.T.);
#9029=EDGE_CURVE('',#7047,#7048,#4065,.T.);
#9030=EDGE_CURVE('',#7048,#7049,#5903,.T.);
#9031=EDGE_CURVE('',#7049,#7050,#4066,.T.);
#9032=EDGE_CURVE('',#7051,#7050,#5904,.T.);
#9033=EDGE_CURVE('',#7051,#7052,#4067,.T.);
#9034=EDGE_CURVE('',#7052,#7053,#5905,.T.);
#9035=EDGE_CURVE('',#7053,#7054,#4068,.T.);
#9036=EDGE_CURVE('',#7055,#7054,#5906,.T.);
#9037=EDGE_CURVE('',#7055,#7056,#4069,.T.);
#9038=EDGE_CURVE('',#7056,#7057,#5907,.T.);
#9039=EDGE_CURVE('',#7057,#7058,#4070,.T.);
#9040=EDGE_CURVE('',#7059,#7058,#5908,.T.);
#9041=EDGE_CURVE('',#7059,#7060,#4071,.T.);
#9042=EDGE_CURVE('',#7060,#7061,#5909,.T.);
#9043=EDGE_CURVE('',#7061,#7062,#4072,.T.);
#9044=EDGE_CURVE('',#7063,#7062,#5910,.T.);
#9045=EDGE_CURVE('',#7063,#7064,#4073,.T.);
#9046=EDGE_CURVE('',#7064,#7065,#5911,.T.);
#9047=EDGE_CURVE('',#7065,#7066,#4074,.T.);
#9048=EDGE_CURVE('',#7067,#7066,#5912,.T.);
#9049=EDGE_CURVE('',#7067,#7068,#4075,.T.);
#9050=EDGE_CURVE('',#7068,#7069,#5913,.T.);
#9051=EDGE_CURVE('',#7069,#7070,#4076,.T.);
#9052=EDGE_CURVE('',#7071,#7070,#5914,.T.);
#9053=EDGE_CURVE('',#7071,#7072,#4077,.T.);
#9054=EDGE_CURVE('',#7072,#7073,#5915,.T.);
#9055=EDGE_CURVE('',#7073,#7074,#4078,.T.);
#9056=EDGE_CURVE('',#7075,#7074,#5916,.T.);
#9057=EDGE_CURVE('',#7075,#7076,#4079,.T.);
#9058=EDGE_CURVE('',#7076,#7077,#5917,.T.);
#9059=EDGE_CURVE('',#7077,#7078,#4080,.T.);
#9060=EDGE_CURVE('',#7079,#7078,#5918,.T.);
#9061=EDGE_CURVE('',#7079,#7080,#4081,.T.);
#9062=EDGE_CURVE('',#7080,#7081,#5919,.T.);
#9063=EDGE_CURVE('',#7081,#7082,#4082,.T.);
#9064=EDGE_CURVE('',#7083,#7082,#5920,.T.);
#9065=EDGE_CURVE('',#7083,#7084,#4083,.T.);
#9066=EDGE_CURVE('',#7084,#7085,#5921,.T.);
#9067=EDGE_CURVE('',#7085,#7086,#4084,.T.);
#9068=EDGE_CURVE('',#7087,#7086,#5922,.T.);
#9069=EDGE_CURVE('',#7087,#7088,#4085,.T.);
#9070=EDGE_CURVE('',#7088,#7089,#5923,.T.);
#9071=EDGE_CURVE('',#7089,#7090,#4086,.T.);
#9072=EDGE_CURVE('',#7091,#7090,#5924,.T.);
#9073=EDGE_CURVE('',#7091,#7092,#4087,.T.);
#9074=EDGE_CURVE('',#7092,#7093,#5925,.T.);
#9075=EDGE_CURVE('',#7093,#7094,#4088,.T.);
#9076=EDGE_CURVE('',#7095,#7094,#5926,.T.);
#9077=EDGE_CURVE('',#7095,#6954,#4089,.T.);
#9078=EDGE_CURVE('',#7021,#7096,#4090,.T.);
#9079=EDGE_CURVE('',#7097,#7096,#4091,.T.);
#9080=EDGE_CURVE('',#7022,#7097,#262,.T.);
#9081=EDGE_CURVE('',#7097,#7019,#263,.T.);
#9082=EDGE_CURVE('',#7096,#7020,#4092,.T.);
#9083=EDGE_CURVE('',#7098,#7095,#264,.T.);
#9084=EDGE_CURVE('',#7094,#7099,#265,.T.);
#9085=EDGE_CURVE('',#7099,#7091,#266,.T.);
#9086=EDGE_CURVE('',#7090,#7100,#267,.T.);
#9087=EDGE_CURVE('',#7100,#7087,#268,.T.);
#9088=EDGE_CURVE('',#7086,#7101,#269,.T.);
#9089=EDGE_CURVE('',#7101,#7083,#270,.T.);
#9090=EDGE_CURVE('',#7082,#7102,#271,.T.);
#9091=EDGE_CURVE('',#7102,#7079,#272,.T.);
#9092=EDGE_CURVE('',#7078,#7103,#273,.T.);
#9093=EDGE_CURVE('',#7103,#7075,#274,.T.);
#9094=EDGE_CURVE('',#7074,#7104,#275,.T.);
#9095=EDGE_CURVE('',#7104,#7071,#276,.T.);
#9096=EDGE_CURVE('',#7070,#7105,#277,.T.);
#9097=EDGE_CURVE('',#7105,#7067,#278,.T.);
#9098=EDGE_CURVE('',#7066,#7106,#279,.T.);
#9099=EDGE_CURVE('',#7106,#7063,#280,.T.);
#9100=EDGE_CURVE('',#7062,#7107,#281,.T.);
#9101=EDGE_CURVE('',#7107,#7059,#282,.T.);
#9102=EDGE_CURVE('',#7058,#7108,#283,.T.);
#9103=EDGE_CURVE('',#7108,#7055,#284,.T.);
#9104=EDGE_CURVE('',#7054,#7109,#285,.T.);
#9105=EDGE_CURVE('',#7109,#7051,#286,.T.);
#9106=EDGE_CURVE('',#7050,#7110,#287,.T.);
#9107=EDGE_CURVE('',#7110,#7047,#288,.T.);
#9108=EDGE_CURVE('',#7046,#7111,#289,.T.);
#9109=EDGE_CURVE('',#7111,#7043,#290,.T.);
#9110=EDGE_CURVE('',#7042,#7112,#291,.T.);
#9111=EDGE_CURVE('',#7112,#7039,#292,.T.);
#9112=EDGE_CURVE('',#7038,#7113,#293,.T.);
#9113=EDGE_CURVE('',#7113,#7035,#294,.T.);
#9114=EDGE_CURVE('',#7034,#7114,#295,.T.);
#9115=EDGE_CURVE('',#7114,#7031,#296,.T.);
#9116=EDGE_CURVE('',#7030,#7115,#297,.T.);
#9117=EDGE_CURVE('',#7115,#7027,#298,.T.);
#9118=EDGE_CURVE('',#7026,#7116,#299,.T.);
#9119=EDGE_CURVE('',#7116,#7023,#300,.T.);
#9120=EDGE_CURVE('',#7018,#7117,#301,.T.);
#9121=EDGE_CURVE('',#7117,#7015,#302,.T.);
#9122=EDGE_CURVE('',#7014,#7118,#303,.T.);
#9123=EDGE_CURVE('',#7118,#7011,#304,.T.);
#9124=EDGE_CURVE('',#7010,#7119,#305,.T.);
#9125=EDGE_CURVE('',#7119,#7007,#306,.T.);
#9126=EDGE_CURVE('',#7006,#7120,#307,.T.);
#9127=EDGE_CURVE('',#7120,#7003,#308,.T.);
#9128=EDGE_CURVE('',#7002,#7121,#309,.T.);
#9129=EDGE_CURVE('',#7121,#6999,#310,.T.);
#9130=EDGE_CURVE('',#6998,#7122,#311,.T.);
#9131=EDGE_CURVE('',#7122,#6995,#312,.T.);
#9132=EDGE_CURVE('',#6994,#7123,#313,.T.);
#9133=EDGE_CURVE('',#7123,#6991,#314,.T.);
#9134=EDGE_CURVE('',#6990,#7124,#315,.T.);
#9135=EDGE_CURVE('',#7124,#6987,#316,.T.);
#9136=EDGE_CURVE('',#6986,#7125,#317,.T.);
#9137=EDGE_CURVE('',#7125,#6983,#318,.T.);
#9138=EDGE_CURVE('',#6982,#7126,#319,.T.);
#9139=EDGE_CURVE('',#7126,#6979,#320,.T.);
#9140=EDGE_CURVE('',#6978,#7127,#321,.T.);
#9141=EDGE_CURVE('',#7127,#6975,#322,.T.);
#9142=EDGE_CURVE('',#6974,#7128,#323,.T.);
#9143=EDGE_CURVE('',#7128,#6971,#324,.T.);
#9144=EDGE_CURVE('',#6970,#7129,#325,.T.);
#9145=EDGE_CURVE('',#7129,#6967,#326,.T.);
#9146=EDGE_CURVE('',#6966,#7130,#327,.T.);
#9147=EDGE_CURVE('',#7130,#6963,#328,.T.);
#9148=EDGE_CURVE('',#6962,#7131,#329,.T.);
#9149=EDGE_CURVE('',#7131,#6959,#330,.T.);
#9150=EDGE_CURVE('',#6958,#7098,#331,.T.);
#9151=EDGE_CURVE('',#7098,#7132,#4093,.T.);
#9152=EDGE_CURVE('',#7132,#7132,#5927,.T.);
#9153=EDGE_CURVE('',#7133,#7016,#4094,.T.);
#9154=EDGE_CURVE('',#7017,#7133,#4095,.T.);
#9155=EDGE_CURVE('',#7117,#7133,#4096,.T.);
#9156=EDGE_CURVE('',#7013,#7134,#4097,.T.);
#9157=EDGE_CURVE('',#7118,#7134,#4098,.T.);
#9158=EDGE_CURVE('',#7134,#7012,#4099,.T.);
#9159=EDGE_CURVE('',#7135,#7008,#4100,.T.);
#9160=EDGE_CURVE('',#7009,#7135,#4101,.T.);
#9161=EDGE_CURVE('',#7119,#7135,#4102,.T.);
#9162=EDGE_CURVE('',#7005,#7136,#4103,.T.);
#9163=EDGE_CURVE('',#7120,#7136,#4104,.T.);
#9164=EDGE_CURVE('',#7136,#7004,#4105,.T.);
#9165=EDGE_CURVE('',#7137,#7000,#4106,.T.);
#9166=EDGE_CURVE('',#7001,#7137,#4107,.T.);
#9167=EDGE_CURVE('',#7121,#7137,#4108,.T.);
#9168=EDGE_CURVE('',#6997,#7138,#4109,.T.);
#9169=EDGE_CURVE('',#7122,#7138,#4110,.T.);
#9170=EDGE_CURVE('',#7138,#6996,#4111,.T.);
#9171=EDGE_CURVE('',#7139,#6992,#4112,.T.);
#9172=EDGE_CURVE('',#6993,#7139,#4113,.T.);
#9173=EDGE_CURVE('',#7123,#7139,#4114,.T.);
#9174=EDGE_CURVE('',#6989,#7140,#4115,.T.);
#9175=EDGE_CURVE('',#7124,#7140,#4116,.T.);
#9176=EDGE_CURVE('',#7140,#6988,#4117,.T.);
#9177=EDGE_CURVE('',#7141,#6984,#4118,.T.);
#9178=EDGE_CURVE('',#6985,#7141,#4119,.T.);
#9179=EDGE_CURVE('',#7125,#7141,#4120,.T.);
#9180=EDGE_CURVE('',#6981,#7142,#4121,.T.);
#9181=EDGE_CURVE('',#7126,#7142,#4122,.T.);
#9182=EDGE_CURVE('',#7142,#6980,#4123,.T.);
#9183=EDGE_CURVE('',#7143,#6976,#4124,.T.);
#9184=EDGE_CURVE('',#6977,#7143,#4125,.T.);
#9185=EDGE_CURVE('',#7127,#7143,#4126,.T.);
#9186=EDGE_CURVE('',#6973,#7144,#4127,.T.);
#9187=EDGE_CURVE('',#7128,#7144,#4128,.T.);
#9188=EDGE_CURVE('',#7144,#6972,#4129,.T.);
#9189=EDGE_CURVE('',#7145,#6968,#4130,.T.);
#9190=EDGE_CURVE('',#6969,#7145,#4131,.T.);
#9191=EDGE_CURVE('',#7129,#7145,#4132,.T.);
#9192=EDGE_CURVE('',#6965,#7146,#4133,.T.);
#9193=EDGE_CURVE('',#7130,#7146,#4134,.T.);
#9194=EDGE_CURVE('',#7146,#6964,#4135,.T.);
#9195=EDGE_CURVE('',#7147,#6960,#4136,.T.);
#9196=EDGE_CURVE('',#6961,#7147,#4137,.T.);
#9197=EDGE_CURVE('',#7131,#7147,#4138,.T.);
#9198=EDGE_CURVE('',#6957,#7148,#4139,.T.);
#9199=EDGE_CURVE('',#7098,#7148,#4140,.T.);
#9200=EDGE_CURVE('',#7148,#6954,#4141,.T.);
#9201=EDGE_CURVE('',#7149,#7092,#4142,.T.);
#9202=EDGE_CURVE('',#7093,#7149,#4143,.T.);
#9203=EDGE_CURVE('',#7099,#7149,#4144,.T.);
#9204=EDGE_CURVE('',#7089,#7150,#4145,.T.);
#9205=EDGE_CURVE('',#7100,#7150,#4146,.T.);
#9206=EDGE_CURVE('',#7150,#7088,#4147,.T.);
#9207=EDGE_CURVE('',#7151,#7084,#4148,.T.);
#9208=EDGE_CURVE('',#7085,#7151,#4149,.T.);
#9209=EDGE_CURVE('',#7101,#7151,#4150,.T.);
#9210=EDGE_CURVE('',#7081,#7152,#4151,.T.);
#9211=EDGE_CURVE('',#7102,#7152,#4152,.T.);
#9212=EDGE_CURVE('',#7152,#7080,#4153,.T.);
#9213=EDGE_CURVE('',#7153,#7076,#4154,.T.);
#9214=EDGE_CURVE('',#7077,#7153,#4155,.T.);
#9215=EDGE_CURVE('',#7103,#7153,#4156,.T.);
#9216=EDGE_CURVE('',#7073,#7154,#4157,.T.);
#9217=EDGE_CURVE('',#7104,#7154,#4158,.T.);
#9218=EDGE_CURVE('',#7154,#7072,#4159,.T.);
#9219=EDGE_CURVE('',#7155,#7068,#4160,.T.);
#9220=EDGE_CURVE('',#7069,#7155,#4161,.T.);
#9221=EDGE_CURVE('',#7105,#7155,#4162,.T.);
#9222=EDGE_CURVE('',#7065,#7156,#4163,.T.);
#9223=EDGE_CURVE('',#7106,#7156,#4164,.T.);
#9224=EDGE_CURVE('',#7156,#7064,#4165,.T.);
#9225=EDGE_CURVE('',#7157,#7060,#4166,.T.);
#9226=EDGE_CURVE('',#7061,#7157,#4167,.T.);
#9227=EDGE_CURVE('',#7107,#7157,#4168,.T.);
#9228=EDGE_CURVE('',#7057,#7158,#4169,.T.);
#9229=EDGE_CURVE('',#7108,#7158,#4170,.T.);
#9230=EDGE_CURVE('',#7158,#7056,#4171,.T.);
#9231=EDGE_CURVE('',#7159,#7052,#4172,.T.);
#9232=EDGE_CURVE('',#7053,#7159,#4173,.T.);
#9233=EDGE_CURVE('',#7109,#7159,#4174,.T.);
#9234=EDGE_CURVE('',#7049,#7160,#4175,.T.);
#9235=EDGE_CURVE('',#7110,#7160,#4176,.T.);
#9236=EDGE_CURVE('',#7160,#7048,#4177,.T.);
#9237=EDGE_CURVE('',#7161,#7044,#4178,.T.);
#9238=EDGE_CURVE('',#7045,#7161,#4179,.T.);
#9239=EDGE_CURVE('',#7111,#7161,#4180,.T.);
#9240=EDGE_CURVE('',#7041,#7162,#4181,.T.);
#9241=EDGE_CURVE('',#7112,#7162,#4182,.T.);
#9242=EDGE_CURVE('',#7162,#7040,#4183,.T.);
#9243=EDGE_CURVE('',#7163,#7036,#4184,.T.);
#9244=EDGE_CURVE('',#7037,#7163,#4185,.T.);
#9245=EDGE_CURVE('',#7113,#7163,#4186,.T.);
#9246=EDGE_CURVE('',#7033,#7164,#4187,.T.);
#9247=EDGE_CURVE('',#7114,#7164,#4188,.T.);
#9248=EDGE_CURVE('',#7164,#7032,#4189,.T.);
#9249=EDGE_CURVE('',#7165,#7028,#4190,.T.);
#9250=EDGE_CURVE('',#7029,#7165,#4191,.T.);
#9251=EDGE_CURVE('',#7115,#7165,#4192,.T.);
#9252=EDGE_CURVE('',#7025,#7166,#4193,.T.);
#9253=EDGE_CURVE('',#7116,#7166,#4194,.T.);
#9254=EDGE_CURVE('',#7166,#7024,#4195,.T.);
#9255=EDGE_CURVE('',#6946,#6956,#5928,.T.);
#9256=EDGE_CURVE('',#7167,#7167,#5929,.T.);
#9257=EDGE_CURVE('',#7168,#7169,#332,.T.);
#9258=EDGE_CURVE('',#7168,#7170,#5930,.T.);
#9259=EDGE_CURVE('',#7171,#7170,#333,.T.);
#9260=EDGE_CURVE('',#7172,#7171,#334,.T.);
#9261=EDGE_CURVE('',#7172,#7173,#5931,.T.);
#9262=EDGE_CURVE('',#7174,#7173,#335,.T.);
#9263=EDGE_CURVE('',#7175,#7174,#336,.T.);
#9264=EDGE_CURVE('',#7175,#7176,#5932,.T.);
#9265=EDGE_CURVE('',#7177,#7176,#337,.T.);
#9266=EDGE_CURVE('',#7178,#7177,#338,.T.);
#9267=EDGE_CURVE('',#7178,#7179,#5933,.T.);
#9268=EDGE_CURVE('',#7180,#7179,#339,.T.);
#9269=EDGE_CURVE('',#7181,#7180,#340,.T.);
#9270=EDGE_CURVE('',#7181,#7182,#5934,.T.);
#9271=EDGE_CURVE('',#7183,#7182,#341,.T.);
#9272=EDGE_CURVE('',#7184,#7183,#342,.T.);
#9273=EDGE_CURVE('',#7184,#7185,#5935,.T.);
#9274=EDGE_CURVE('',#7169,#7185,#343,.T.);
#9275=EDGE_CURVE('',#7169,#7167,#4196,.T.);
#9276=EDGE_CURVE('',#7176,#7186,#4197,.T.);
#9277=EDGE_CURVE('',#7187,#7175,#4198,.T.);
#9278=EDGE_CURVE('',#7186,#7187,#5936,.T.);
#9279=EDGE_CURVE('',#7179,#7188,#4199,.T.);
#9280=EDGE_CURVE('',#7189,#7178,#4200,.T.);
#9281=EDGE_CURVE('',#7188,#7189,#5937,.T.);
#9282=EDGE_CURVE('',#7190,#7172,#4201,.T.);
#9283=EDGE_CURVE('',#7191,#7190,#5938,.T.);
#9284=EDGE_CURVE('',#7173,#7191,#4202,.T.);
#9285=EDGE_CURVE('',#7182,#7192,#4203,.T.);
#9286=EDGE_CURVE('',#7193,#7181,#4204,.T.);
#9287=EDGE_CURVE('',#7192,#7193,#5939,.T.);
#9288=EDGE_CURVE('',#7194,#7168,#4205,.T.);
#9289=EDGE_CURVE('',#7195,#7194,#5940,.T.);
#9290=EDGE_CURVE('',#7170,#7195,#4206,.T.);
#9291=EDGE_CURVE('',#7196,#7184,#4207,.T.);
#9292=EDGE_CURVE('',#7197,#7196,#5941,.T.);
#9293=EDGE_CURVE('',#7185,#7197,#4208,.T.);
#9294=EDGE_CURVE('',#7193,#7192,#4209,.T.);
#9295=EDGE_CURVE('',#7180,#7198,#4210,.T.);
#9296=EDGE_CURVE('',#7198,#7199,#4211,.T.);
#9297=EDGE_CURVE('',#7183,#7199,#4212,.T.);
#9298=EDGE_CURVE('',#7189,#7188,#4213,.T.);
#9299=EDGE_CURVE('',#7177,#7200,#4214,.T.);
#9300=EDGE_CURVE('',#7200,#7198,#4215,.T.);
#9301=EDGE_CURVE('',#7187,#7186,#4216,.T.);
#9302=EDGE_CURVE('',#7174,#7201,#4217,.T.);
#9303=EDGE_CURVE('',#7201,#7200,#4218,.T.);
#9304=EDGE_CURVE('',#7190,#7191,#4219,.T.);
#9305=EDGE_CURVE('',#7194,#7195,#4220,.T.);
#9306=EDGE_CURVE('',#7196,#7197,#4221,.T.);
#9307=EDGE_CURVE('',#7202,#7201,#4222,.T.);
#9308=EDGE_CURVE('',#7202,#7201,#5942,.T.);
#9309=EDGE_CURVE('',#7201,#7200,#5943,.T.);
#9310=EDGE_CURVE('',#7200,#7198,#5944,.T.);
#9311=EDGE_CURVE('',#7198,#7199,#5945,.T.);
#9312=EDGE_CURVE('',#7199,#7203,#4223,.T.);
#9313=EDGE_CURVE('',#7199,#7203,#5946,.T.);
#9314=EDGE_CURVE('',#7203,#7202,#4224,.T.);
#9315=EDGE_CURVE('',#7203,#7202,#5947,.T.);
#9316=EDGE_CURVE('',#7204,#7203,#4225,.T.);
#9317=EDGE_CURVE('',#7171,#7202,#4226,.T.);
#9318=EDGE_CURVE('',#7169,#7203,#4227,.T.);
#9319=EDGE_CURVE('',#7205,#7206,#4228,.T.);
#9320=EDGE_CURVE('',#7207,#7205,#543,.F.);
#9321=EDGE_CURVE('',#7208,#7207,#5948,.T.);
#9322=EDGE_CURVE('',#7208,#7206,#544,.T.);
#9323=EDGE_CURVE('',#7209,#7210,#4229,.T.);
#9324=EDGE_CURVE('',#7205,#7209,#545,.F.);
#9325=EDGE_CURVE('',#7206,#7211,#546,.T.);
#9326=EDGE_CURVE('',#7211,#7210,#547,.T.);
#9327=EDGE_CURVE('',#7212,#7213,#4230,.T.);
#9328=EDGE_CURVE('',#7209,#7212,#548,.F.);
#9329=EDGE_CURVE('',#7210,#7213,#549,.T.);
#9330=EDGE_CURVE('',#7214,#7215,#4231,.T.);
#9331=EDGE_CURVE('',#7212,#7214,#550,.F.);
#9332=EDGE_CURVE('',#7213,#7216,#551,.T.);
#9333=EDGE_CURVE('',#7216,#7215,#552,.T.);
#9334=EDGE_CURVE('',#7217,#7218,#4232,.T.);
#9335=EDGE_CURVE('',#7219,#7217,#553,.F.);
#9336=EDGE_CURVE('',#7214,#7219,#554,.F.);
#9337=EDGE_CURVE('',#7215,#7220,#555,.T.);
#9338=EDGE_CURVE('',#7220,#7218,#556,.T.);
#9339=EDGE_CURVE('',#7221,#7222,#4233,.T.);
#9340=EDGE_CURVE('',#7217,#7221,#557,.F.);
#9341=EDGE_CURVE('',#7218,#7222,#558,.T.);
#9342=EDGE_CURVE('',#7223,#7224,#4234,.T.);
#9343=EDGE_CURVE('',#7225,#7223,#559,.F.);
#9344=EDGE_CURVE('',#7221,#7225,#560,.F.);
#9345=EDGE_CURVE('',#7222,#7226,#561,.T.);
#9346=EDGE_CURVE('',#7226,#7224,#562,.T.);
#9347=EDGE_CURVE('',#7227,#7228,#4235,.T.);
#9348=EDGE_CURVE('',#7223,#7227,#563,.F.);
#9349=EDGE_CURVE('',#7224,#7228,#564,.T.);
#9350=EDGE_CURVE('',#7229,#7230,#4236,.T.);
#9351=EDGE_CURVE('',#7231,#7229,#565,.F.);
#9352=EDGE_CURVE('',#7227,#7231,#566,.F.);
#9353=EDGE_CURVE('',#7228,#7232,#567,.T.);
#9354=EDGE_CURVE('',#7232,#7230,#568,.T.);
#9355=EDGE_CURVE('',#7233,#7234,#4237,.T.);
#9356=EDGE_CURVE('',#7229,#7233,#569,.F.);
#9357=EDGE_CURVE('',#7230,#7234,#570,.T.);
#9358=EDGE_CURVE('',#7235,#7236,#4238,.T.);
#9359=EDGE_CURVE('',#7237,#7235,#571,.T.);
#9360=EDGE_CURVE('',#7233,#7237,#572,.F.);
#9361=EDGE_CURVE('',#7234,#7238,#573,.T.);
#9362=EDGE_CURVE('',#7238,#7236,#574,.T.);
#9363=EDGE_CURVE('',#7239,#7240,#4239,.T.);
#9364=EDGE_CURVE('',#7241,#7239,#575,.F.);
#9365=EDGE_CURVE('',#7235,#7241,#576,.T.);
#9366=EDGE_CURVE('',#7236,#7240,#577,.T.);
#9367=EDGE_CURVE('',#7242,#7243,#4240,.T.);
#9368=EDGE_CURVE('',#7239,#7242,#578,.F.);
#9369=EDGE_CURVE('',#7240,#7244,#579,.T.);
#9370=EDGE_CURVE('',#7244,#7243,#580,.T.);
#9371=EDGE_CURVE('',#7245,#7246,#4241,.T.);
#9372=EDGE_CURVE('',#7247,#7245,#581,.F.);
#9373=EDGE_CURVE('',#7242,#7247,#582,.F.);
#9374=EDGE_CURVE('',#7243,#7246,#583,.T.);
#9375=EDGE_CURVE('',#7248,#7249,#4242,.T.);
#9376=EDGE_CURVE('',#7245,#7248,#584,.F.);
#9377=EDGE_CURVE('',#7246,#7250,#585,.T.);
#9378=EDGE_CURVE('',#7250,#7249,#586,.T.);
#9379=EDGE_CURVE('',#7251,#7252,#4243,.T.);
#9380=EDGE_CURVE('',#7253,#7251,#587,.F.);
#9381=EDGE_CURVE('',#7248,#7253,#588,.F.);
#9382=EDGE_CURVE('',#7249,#7252,#589,.T.);
#9383=EDGE_CURVE('',#7254,#7255,#4244,.T.);
#9384=EDGE_CURVE('',#7251,#7254,#590,.F.);
#9385=EDGE_CURVE('',#7252,#7256,#591,.T.);
#9386=EDGE_CURVE('',#7256,#7255,#592,.T.);
#9387=EDGE_CURVE('',#7257,#7258,#4245,.T.);
#9388=EDGE_CURVE('',#7259,#7257,#593,.F.);
#9389=EDGE_CURVE('',#7254,#7259,#594,.F.);
#9390=EDGE_CURVE('',#7255,#7258,#595,.T.);
#9391=EDGE_CURVE('',#7260,#7261,#4246,.T.);
#9392=EDGE_CURVE('',#7257,#7260,#596,.F.);
#9393=EDGE_CURVE('',#7258,#7262,#597,.T.);
#9394=EDGE_CURVE('',#7262,#7261,#598,.T.);
#9395=EDGE_CURVE('',#7263,#7264,#4247,.T.);
#9396=EDGE_CURVE('',#7265,#7263,#599,.F.);
#9397=EDGE_CURVE('',#7260,#7265,#600,.F.);
#9398=EDGE_CURVE('',#7261,#7264,#601,.T.);
#9399=EDGE_CURVE('',#7266,#7267,#4248,.T.);
#9400=EDGE_CURVE('',#7263,#7266,#602,.F.);
#9401=EDGE_CURVE('',#7264,#7268,#603,.T.);
#9402=EDGE_CURVE('',#7268,#7267,#604,.T.);
#9403=EDGE_CURVE('',#7269,#7270,#4249,.T.);
#9404=EDGE_CURVE('',#7271,#7269,#605,.F.);
#9405=EDGE_CURVE('',#7266,#7271,#606,.F.);
#9406=EDGE_CURVE('',#7267,#7270,#607,.T.);
#9407=EDGE_CURVE('',#7272,#7273,#4250,.T.);
#9408=EDGE_CURVE('',#7269,#7272,#608,.F.);
#9409=EDGE_CURVE('',#7270,#7273,#609,.T.);
#9410=EDGE_CURVE('',#7274,#7275,#610,.T.);
#9411=EDGE_CURVE('',#7275,#7276,#5949,.T.);
#9412=EDGE_CURVE('',#7276,#7277,#611,.T.);
#9413=EDGE_CURVE('',#7277,#7278,#612,.T.);
#9414=EDGE_CURVE('',#7278,#7279,#613,.T.);
#9415=EDGE_CURVE('',#7279,#7280,#614,.T.);
#9416=EDGE_CURVE('',#7280,#7281,#615,.T.);
#9417=EDGE_CURVE('',#7281,#7282,#616,.T.);
#9418=EDGE_CURVE('',#7282,#7283,#617,.T.);
#9419=EDGE_CURVE('',#7283,#7284,#618,.T.);
#9420=EDGE_CURVE('',#7284,#7285,#619,.T.);
#9421=EDGE_CURVE('',#7285,#7286,#620,.T.);
#9422=EDGE_CURVE('',#7286,#7287,#621,.T.);
#9423=EDGE_CURVE('',#7287,#7288,#622,.T.);
#9424=EDGE_CURVE('',#7288,#7289,#623,.T.);
#9425=EDGE_CURVE('',#7289,#7290,#624,.T.);
#9426=EDGE_CURVE('',#7290,#7291,#625,.T.);
#9427=EDGE_CURVE('',#7291,#7292,#626,.T.);
#9428=EDGE_CURVE('',#7292,#7293,#627,.T.);
#9429=EDGE_CURVE('',#7293,#7294,#628,.T.);
#9430=EDGE_CURVE('',#7294,#7295,#629,.T.);
#9431=EDGE_CURVE('',#7295,#7296,#630,.T.);
#9432=EDGE_CURVE('',#7296,#7297,#631,.T.);
#9433=EDGE_CURVE('',#7297,#7298,#632,.T.);
#9434=EDGE_CURVE('',#7298,#7299,#633,.T.);
#9435=EDGE_CURVE('',#7299,#7300,#634,.T.);
#9436=EDGE_CURVE('',#7300,#7301,#635,.T.);
#9437=EDGE_CURVE('',#7302,#7301,#5950,.F.);
#9438=EDGE_CURVE('',#7302,#7303,#636,.T.);
#9439=EDGE_CURVE('',#7303,#7304,#637,.T.);
#9440=EDGE_CURVE('',#7304,#7305,#638,.T.);
#9441=EDGE_CURVE('',#7305,#7306,#639,.T.);
#9442=EDGE_CURVE('',#7306,#7307,#640,.T.);
#9443=EDGE_CURVE('',#7307,#7308,#641,.T.);
#9444=EDGE_CURVE('',#7308,#7309,#642,.T.);
#9445=EDGE_CURVE('',#7309,#7310,#643,.T.);
#9446=EDGE_CURVE('',#7310,#7311,#644,.T.);
#9447=EDGE_CURVE('',#7311,#7312,#645,.T.);
#9448=EDGE_CURVE('',#7312,#7313,#646,.T.);
#9449=EDGE_CURVE('',#7313,#7314,#647,.T.);
#9450=EDGE_CURVE('',#7314,#7315,#648,.T.);
#9451=EDGE_CURVE('',#7315,#7316,#649,.T.);
#9452=EDGE_CURVE('',#7316,#7317,#650,.T.);
#9453=EDGE_CURVE('',#7317,#7318,#651,.T.);
#9454=EDGE_CURVE('',#7318,#7319,#652,.T.);
#9455=EDGE_CURVE('',#7319,#7320,#653,.T.);
#9456=EDGE_CURVE('',#7320,#7321,#654,.T.);
#9457=EDGE_CURVE('',#7321,#7322,#655,.T.);
#9458=EDGE_CURVE('',#7322,#7323,#656,.T.);
#9459=EDGE_CURVE('',#7323,#7324,#657,.T.);
#9460=EDGE_CURVE('',#7324,#7325,#658,.T.);
#9461=EDGE_CURVE('',#7325,#7274,#659,.T.);
#9462=EDGE_CURVE('',#7273,#7326,#660,.T.);
#9463=EDGE_CURVE('',#7327,#7326,#5951,.T.);
#9464=EDGE_CURVE('',#7328,#7327,#661,.T.);
#9465=EDGE_CURVE('',#7272,#7328,#662,.F.);
#9466=EDGE_CURVE('',#7329,#7330,#5952,.F.);
#9467=EDGE_CURVE('',#7329,#7327,#663,.T.);
#9468=EDGE_CURVE('',#7326,#7331,#664,.T.);
#9469=EDGE_CURVE('',#7331,#7302,#665,.T.);
#9470=EDGE_CURVE('',#7330,#7302,#5953,.F.);
#9471=EDGE_CURVE('',#7301,#7329,#666,.T.);
#9472=EDGE_CURVE('',#7332,#7276,#667,.T.);
#9473=EDGE_CURVE('',#7332,#7207,#668,.T.);
#9474=EDGE_CURVE('',#7276,#7333,#5954,.T.);
#9475=EDGE_CURVE('',#7333,#7334,#5955,.T.);
#9476=EDGE_CURVE('',#7334,#7208,#669,.T.);
#9477=EDGE_CURVE('',#7334,#7275,#670,.T.);
#9478=EDGE_CURVE('',#7335,#7336,#344,.T.);
#9479=EDGE_CURVE('',#7335,#7337,#5956,.T.);
#9480=EDGE_CURVE('',#7338,#7337,#345,.T.);
#9481=EDGE_CURVE('',#7339,#7338,#346,.T.);
#9482=EDGE_CURVE('',#7339,#7340,#5957,.T.);
#9483=EDGE_CURVE('',#7341,#7340,#347,.T.);
#9484=EDGE_CURVE('',#7342,#7341,#348,.T.);
#9485=EDGE_CURVE('',#7342,#7343,#5958,.T.);
#9486=EDGE_CURVE('',#7344,#7343,#349,.T.);
#9487=EDGE_CURVE('',#7345,#7344,#350,.T.);
#9488=EDGE_CURVE('',#7345,#7346,#5959,.T.);
#9489=EDGE_CURVE('',#7347,#7346,#351,.T.);
#9490=EDGE_CURVE('',#7348,#7347,#352,.T.);
#9491=EDGE_CURVE('',#7348,#7349,#5960,.T.);
#9492=EDGE_CURVE('',#7350,#7349,#353,.T.);
#9493=EDGE_CURVE('',#7351,#7350,#354,.T.);
#9494=EDGE_CURVE('',#7351,#7352,#5961,.T.);
#9495=EDGE_CURVE('',#7336,#7352,#355,.T.);
#9496=EDGE_CURVE('',#7336,#7353,#4251,.T.);
#9497=EDGE_CURVE('',#7353,#7353,#5962,.T.);
#9498=EDGE_CURVE('',#7343,#7354,#4252,.T.);
#9499=EDGE_CURVE('',#7355,#7342,#4253,.T.);
#9500=EDGE_CURVE('',#7354,#7355,#5963,.T.);
#9501=EDGE_CURVE('',#7346,#7356,#4254,.T.);
#9502=EDGE_CURVE('',#7357,#7345,#4255,.T.);
#9503=EDGE_CURVE('',#7356,#7357,#5964,.T.);
#9504=EDGE_CURVE('',#7358,#7339,#4256,.T.);
#9505=EDGE_CURVE('',#7359,#7358,#5965,.T.);
#9506=EDGE_CURVE('',#7340,#7359,#4257,.T.);
#9507=EDGE_CURVE('',#7349,#7360,#4258,.T.);
#9508=EDGE_CURVE('',#7361,#7348,#4259,.T.);
#9509=EDGE_CURVE('',#7360,#7361,#5966,.T.);
#9510=EDGE_CURVE('',#7362,#7335,#4260,.T.);
#9511=EDGE_CURVE('',#7363,#7362,#5967,.T.);
#9512=EDGE_CURVE('',#7337,#7363,#4261,.T.);
#9513=EDGE_CURVE('',#7364,#7351,#4262,.T.);
#9514=EDGE_CURVE('',#7365,#7364,#5968,.T.);
#9515=EDGE_CURVE('',#7352,#7365,#4263,.T.);
#9516=EDGE_CURVE('',#7361,#7360,#4264,.T.);
#9517=EDGE_CURVE('',#7347,#7366,#4265,.T.);
#9518=EDGE_CURVE('',#7366,#7367,#4266,.T.);
#9519=EDGE_CURVE('',#7350,#7367,#4267,.T.);
#9520=EDGE_CURVE('',#7357,#7356,#4268,.T.);
#9521=EDGE_CURVE('',#7344,#7368,#4269,.T.);
#9522=EDGE_CURVE('',#7368,#7366,#4270,.T.);
#9523=EDGE_CURVE('',#7355,#7354,#4271,.T.);
#9524=EDGE_CURVE('',#7341,#7369,#4272,.T.);
#9525=EDGE_CURVE('',#7369,#7368,#4273,.T.);
#9526=EDGE_CURVE('',#7358,#7359,#4274,.T.);
#9527=EDGE_CURVE('',#7362,#7363,#4275,.T.);
#9528=EDGE_CURVE('',#7364,#7365,#4276,.T.);
#9529=EDGE_CURVE('',#7370,#7369,#4277,.T.);
#9530=EDGE_CURVE('',#7370,#7369,#5969,.T.);
#9531=EDGE_CURVE('',#7369,#7368,#5970,.T.);
#9532=EDGE_CURVE('',#7368,#7366,#5971,.T.);
#9533=EDGE_CURVE('',#7366,#7367,#5972,.T.);
#9534=EDGE_CURVE('',#7367,#7371,#4278,.T.);
#9535=EDGE_CURVE('',#7367,#7371,#5973,.T.);
#9536=EDGE_CURVE('',#7371,#7370,#4279,.T.);
#9537=EDGE_CURVE('',#7371,#7370,#5974,.T.);
#9538=EDGE_CURVE('',#7372,#7371,#4280,.T.);
#9539=EDGE_CURVE('',#7338,#7370,#4281,.T.);
#9540=EDGE_CURVE('',#7336,#7371,#4282,.T.);
#9541=EDGE_CURVE('',#7373,#7373,#5975,.T.);
#9542=EDGE_CURVE('',#7333,#7373,#4283,.T.);
#9543=EDGE_CURVE('',#7330,#7374,#4284,.T.);
#9544=EDGE_CURVE('',#7374,#7374,#5976,.T.);
#9545=EDGE_CURVE('',#7375,#7376,#4285,.T.);
#9546=EDGE_CURVE('',#7377,#7375,#671,.T.);
#9547=EDGE_CURVE('',#7376,#7377,#5977,.T.);
#9548=EDGE_CURVE('',#7378,#7379,#4286,.T.);
#9549=EDGE_CURVE('',#7380,#7378,#672,.F.);
#9550=EDGE_CURVE('',#7375,#7380,#673,.T.);
#9551=EDGE_CURVE('',#7381,#7376,#5978,.T.);
#9552=EDGE_CURVE('',#7381,#7382,#674,.T.);
#9553=EDGE_CURVE('',#7382,#7379,#675,.T.);
#9554=EDGE_CURVE('',#7383,#7384,#4287,.T.);
#9555=EDGE_CURVE('',#7378,#7383,#676,.F.);
#9556=EDGE_CURVE('',#7379,#7385,#677,.T.);
#9557=EDGE_CURVE('',#7385,#7384,#678,.T.);
#9558=EDGE_CURVE('',#7386,#7387,#4288,.T.);
#9559=EDGE_CURVE('',#7388,#7386,#679,.F.);
#9560=EDGE_CURVE('',#7383,#7388,#680,.F.);
#9561=EDGE_CURVE('',#7384,#7389,#681,.T.);
#9562=EDGE_CURVE('',#7389,#7387,#682,.T.);
#9563=EDGE_CURVE('',#7390,#7391,#4289,.T.);
#9564=EDGE_CURVE('',#7386,#7390,#683,.F.);
#9565=EDGE_CURVE('',#7387,#7392,#684,.T.);
#9566=EDGE_CURVE('',#7392,#7391,#685,.T.);
#9567=EDGE_CURVE('',#7393,#7394,#4290,.T.);
#9568=EDGE_CURVE('',#7395,#7393,#686,.F.);
#9569=EDGE_CURVE('',#7390,#7395,#687,.F.);
#9570=EDGE_CURVE('',#7391,#7396,#688,.T.);
#9571=EDGE_CURVE('',#7396,#7394,#689,.T.);
#9572=EDGE_CURVE('',#7397,#7398,#4291,.T.);
#9573=EDGE_CURVE('',#7393,#7397,#690,.F.);
#9574=EDGE_CURVE('',#7394,#7399,#691,.T.);
#9575=EDGE_CURVE('',#7399,#7398,#692,.T.);
#9576=EDGE_CURVE('',#7400,#7401,#4292,.T.);
#9577=EDGE_CURVE('',#7402,#7400,#693,.F.);
#9578=EDGE_CURVE('',#7397,#7402,#694,.F.);
#9579=EDGE_CURVE('',#7398,#7403,#695,.T.);
#9580=EDGE_CURVE('',#7403,#7401,#696,.T.);
#9581=EDGE_CURVE('',#7404,#7405,#4293,.T.);
#9582=EDGE_CURVE('',#7400,#7404,#697,.F.);
#9583=EDGE_CURVE('',#7401,#7406,#698,.T.);
#9584=EDGE_CURVE('',#7406,#7405,#699,.T.);
#9585=EDGE_CURVE('',#7407,#7408,#4294,.T.);
#9586=EDGE_CURVE('',#7409,#7407,#700,.F.);
#9587=EDGE_CURVE('',#7404,#7409,#701,.F.);
#9588=EDGE_CURVE('',#7405,#7410,#702,.T.);
#9589=EDGE_CURVE('',#7410,#7408,#703,.T.);
#9590=EDGE_CURVE('',#7411,#7412,#4295,.T.);
#9591=EDGE_CURVE('',#7411,#7413,#5979,.T.);
#9592=EDGE_CURVE('',#7413,#7412,#704,.T.);
#9593=EDGE_CURVE('',#7412,#7414,#705,.T.);
#9594=EDGE_CURVE('',#7415,#7414,#5980,.T.);
#9595=EDGE_CURVE('',#7415,#7416,#706,.T.);
#9596=EDGE_CURVE('',#7416,#7411,#5981,.T.);
#9597=EDGE_CURVE('',#7417,#7415,#707,.T.);
#9598=EDGE_CURVE('',#7414,#7418,#708,.T.);
#9599=EDGE_CURVE('',#7418,#7419,#709,.T.);
#9600=EDGE_CURVE('',#7419,#7420,#710,.T.);
#9601=EDGE_CURVE('',#7420,#7421,#711,.T.);
#9602=EDGE_CURVE('',#7421,#7422,#712,.T.);
#9603=EDGE_CURVE('',#7422,#7423,#713,.T.);
#9604=EDGE_CURVE('',#7423,#7424,#714,.T.);
#9605=EDGE_CURVE('',#7424,#7425,#715,.T.);
#9606=EDGE_CURVE('',#7425,#7426,#716,.T.);
#9607=EDGE_CURVE('',#7426,#7427,#717,.T.);
#9608=EDGE_CURVE('',#7427,#7428,#718,.T.);
#9609=EDGE_CURVE('',#7428,#7429,#719,.T.);
#9610=EDGE_CURVE('',#7430,#7429,#5982,.T.);
#9611=EDGE_CURVE('',#7431,#7430,#5983,.T.);
#9612=EDGE_CURVE('',#7431,#7432,#720,.T.);
#9613=EDGE_CURVE('',#7432,#7433,#721,.T.);
#9614=EDGE_CURVE('',#7433,#7434,#722,.T.);
#9615=EDGE_CURVE('',#7434,#7435,#723,.T.);
#9616=EDGE_CURVE('',#7435,#7436,#724,.T.);
#9617=EDGE_CURVE('',#7436,#7437,#725,.T.);
#9618=EDGE_CURVE('',#7437,#7438,#726,.T.);
#9619=EDGE_CURVE('',#7438,#7439,#727,.T.);
#9620=EDGE_CURVE('',#7439,#7440,#728,.T.);
#9621=EDGE_CURVE('',#7440,#7417,#729,.T.);
#9622=EDGE_CURVE('',#7408,#7441,#730,.T.);
#9623=EDGE_CURVE('',#7441,#7442,#731,.T.);
#9624=EDGE_CURVE('',#7443,#7442,#5984,.T.);
#9625=EDGE_CURVE('',#7407,#7443,#732,.F.);
#9626=EDGE_CURVE('',#7442,#7431,#733,.T.);
#9627=EDGE_CURVE('',#7416,#7381,#400,.T.);
#9628=EDGE_CURVE('',#7444,#7431,#5985,.T.);
#9629=EDGE_CURVE('',#7444,#7443,#734,.T.);
#9630=EDGE_CURVE('',#7377,#7413,#401,.T.);
#9631=EDGE_CURVE('',#7429,#7444,#735,.T.);
#9632=EDGE_CURVE('',#7445,#7445,#5986,.T.);
#9633=EDGE_CURVE('',#7445,#7430,#5987,.T.);
#9634=EDGE_CURVE('',#7446,#7446,#5988,.T.);
#9635=EDGE_CURVE('',#7447,#7448,#4296,.T.);
#9636=EDGE_CURVE('',#7448,#7447,#5989,.T.);
#9637=EDGE_CURVE('',#7448,#7449,#4297,.T.);
#9638=EDGE_CURVE('',#7449,#7448,#5990,.T.);
#9639=EDGE_CURVE('',#7449,#7450,#4298,.T.);
#9640=EDGE_CURVE('',#7450,#7449,#5991,.T.);
#9641=EDGE_CURVE('',#7450,#7451,#4299,.T.);
#9642=EDGE_CURVE('',#7451,#7450,#5992,.T.);
#9643=EDGE_CURVE('',#7451,#7452,#4300,.T.);
#9644=EDGE_CURVE('',#7452,#7451,#5993,.T.);
#9645=EDGE_CURVE('',#7452,#7447,#4301,.T.);
#9646=EDGE_CURVE('',#7447,#7452,#5994,.T.);
#9647=EDGE_CURVE('',#7453,#7448,#4302,.T.);
#9648=EDGE_CURVE('',#7454,#7455,#5995,.T.);
#9649=EDGE_CURVE('',#7454,#7447,#4303,.T.);
#9650=EDGE_CURVE('',#7455,#7448,#4304,.T.);
#9651=EDGE_CURVE('',#7455,#7456,#5996,.T.);
#9652=EDGE_CURVE('',#7456,#7449,#4305,.T.);
#9653=EDGE_CURVE('',#7456,#7457,#5997,.T.);
#9654=EDGE_CURVE('',#7457,#7450,#4306,.T.);
#9655=EDGE_CURVE('',#7457,#7458,#5998,.T.);
#9656=EDGE_CURVE('',#7458,#7451,#4307,.T.);
#9657=EDGE_CURVE('',#7459,#7454,#5999,.T.);
#9658=EDGE_CURVE('',#7459,#7452,#4308,.T.);
#9659=EDGE_CURVE('',#7458,#7459,#6000,.T.);
#9660=EDGE_CURVE('',#7460,#7460,#6001,.T.);
#9661=EDGE_CURVE('',#7460,#7446,#4309,.T.);
#9662=EDGE_CURVE('',#7455,#7460,#6002,.T.);
#9663=EDGE_CURVE('',#7461,#7462,#4310,.T.);
#9664=EDGE_CURVE('',#7463,#7461,#736,.F.);
#9665=EDGE_CURVE('',#7462,#7463,#6003,.T.);
#9666=EDGE_CURVE('',#7464,#7465,#4311,.T.);
#9667=EDGE_CURVE('',#7461,#7464,#737,.F.);
#9668=EDGE_CURVE('',#7466,#7462,#6004,.T.);
#9669=EDGE_CURVE('',#7466,#7467,#738,.T.);
#9670=EDGE_CURVE('',#7467,#7465,#739,.T.);
#9671=EDGE_CURVE('',#7468,#7469,#4312,.T.);
#9672=EDGE_CURVE('',#7464,#7468,#740,.F.);
#9673=EDGE_CURVE('',#7465,#7470,#741,.T.);
#9674=EDGE_CURVE('',#7470,#7469,#742,.T.);
#9675=EDGE_CURVE('',#7471,#7472,#4313,.T.);
#9676=EDGE_CURVE('',#7468,#7471,#743,.F.);
#9677=EDGE_CURVE('',#7469,#7473,#744,.T.);
#9678=EDGE_CURVE('',#7473,#7472,#745,.T.);
#9679=EDGE_CURVE('',#7474,#7475,#4314,.T.);
#9680=EDGE_CURVE('',#7471,#7474,#746,.F.);
#9681=EDGE_CURVE('',#7472,#7476,#747,.T.);
#9682=EDGE_CURVE('',#7476,#7475,#748,.T.);
#9683=EDGE_CURVE('',#7477,#7478,#4315,.T.);
#9684=EDGE_CURVE('',#7479,#7477,#749,.F.);
#9685=EDGE_CURVE('',#7474,#7479,#750,.F.);
#9686=EDGE_CURVE('',#7475,#7480,#751,.T.);
#9687=EDGE_CURVE('',#7480,#7478,#752,.T.);
#9688=EDGE_CURVE('',#7481,#7482,#4316,.T.);
#9689=EDGE_CURVE('',#7477,#7481,#753,.F.);
#9690=EDGE_CURVE('',#7478,#7483,#754,.T.);
#9691=EDGE_CURVE('',#7483,#7482,#755,.T.);
#9692=EDGE_CURVE('',#7484,#7485,#4317,.T.);
#9693=EDGE_CURVE('',#7486,#7484,#756,.F.);
#9694=EDGE_CURVE('',#7481,#7486,#757,.F.);
#9695=EDGE_CURVE('',#7482,#7487,#758,.T.);
#9696=EDGE_CURVE('',#7487,#7485,#759,.T.);
#9697=EDGE_CURVE('',#7488,#7489,#4318,.T.);
#9698=EDGE_CURVE('',#7484,#7488,#760,.F.);
#9699=EDGE_CURVE('',#7485,#7490,#761,.T.);
#9700=EDGE_CURVE('',#7490,#7489,#762,.T.);
#9701=EDGE_CURVE('',#7491,#7492,#4319,.T.);
#9702=EDGE_CURVE('',#7493,#7491,#763,.F.);
#9703=EDGE_CURVE('',#7488,#7493,#764,.F.);
#9704=EDGE_CURVE('',#7489,#7494,#765,.T.);
#9705=EDGE_CURVE('',#7494,#7492,#766,.T.);
#9706=EDGE_CURVE('',#7495,#7496,#4320,.T.);
#9707=EDGE_CURVE('',#7491,#7495,#767,.F.);
#9708=EDGE_CURVE('',#7492,#7497,#768,.T.);
#9709=EDGE_CURVE('',#7497,#7496,#769,.T.);
#9710=EDGE_CURVE('',#7498,#7499,#4321,.T.);
#9711=EDGE_CURVE('',#7500,#7498,#770,.F.);
#9712=EDGE_CURVE('',#7495,#7500,#771,.F.);
#9713=EDGE_CURVE('',#7496,#7501,#772,.T.);
#9714=EDGE_CURVE('',#7501,#7499,#773,.T.);
#9715=EDGE_CURVE('',#7502,#7503,#774,.T.);
#9716=EDGE_CURVE('',#7503,#7504,#6005,.T.);
#9717=EDGE_CURVE('',#7504,#7505,#775,.T.);
#9718=EDGE_CURVE('',#7505,#7506,#776,.T.);
#9719=EDGE_CURVE('',#7506,#7507,#777,.T.);
#9720=EDGE_CURVE('',#7507,#7508,#778,.T.);
#9721=EDGE_CURVE('',#7508,#7509,#779,.T.);
#9722=EDGE_CURVE('',#7509,#7510,#780,.T.);
#9723=EDGE_CURVE('',#7510,#7511,#781,.T.);
#9724=EDGE_CURVE('',#7511,#7512,#782,.T.);
#9725=EDGE_CURVE('',#7512,#7513,#783,.T.);
#9726=EDGE_CURVE('',#7513,#7514,#784,.T.);
#9727=EDGE_CURVE('',#7514,#7515,#785,.T.);
#9728=EDGE_CURVE('',#7515,#7516,#786,.T.);
#9729=EDGE_CURVE('',#7516,#7517,#787,.T.);
#9730=EDGE_CURVE('',#7517,#7518,#788,.T.);
#9731=EDGE_CURVE('',#7519,#7518,#6006,.T.);
#9732=EDGE_CURVE('',#7519,#7520,#789,.T.);
#9733=EDGE_CURVE('',#7520,#7521,#790,.T.);
#9734=EDGE_CURVE('',#7521,#7522,#791,.T.);
#9735=EDGE_CURVE('',#7522,#7523,#792,.T.);
#9736=EDGE_CURVE('',#7523,#7524,#793,.T.);
#9737=EDGE_CURVE('',#7524,#7525,#794,.T.);
#9738=EDGE_CURVE('',#7525,#7526,#795,.T.);
#9739=EDGE_CURVE('',#7526,#7527,#796,.T.);
#9740=EDGE_CURVE('',#7527,#7528,#797,.T.);
#9741=EDGE_CURVE('',#7528,#7529,#798,.T.);
#9742=EDGE_CURVE('',#7529,#7530,#799,.T.);
#9743=EDGE_CURVE('',#7530,#7531,#800,.T.);
#9744=EDGE_CURVE('',#7531,#7502,#801,.T.);
#9745=EDGE_CURVE('',#7499,#7532,#802,.T.);
#9746=EDGE_CURVE('',#7532,#7533,#803,.T.);
#9747=EDGE_CURVE('',#7534,#7533,#6007,.T.);
#9748=EDGE_CURVE('',#7498,#7534,#804,.F.);
#9749=EDGE_CURVE('',#7463,#7535,#805,.T.);
#9750=EDGE_CURVE('',#7536,#7534,#806,.T.);
#9751=EDGE_CURVE('',#7518,#7536,#807,.T.);
#9752=EDGE_CURVE('',#7535,#7504,#808,.T.);
#9753=EDGE_CURVE('',#7536,#7537,#6008,.T.);
#9754=EDGE_CURVE('',#7533,#7519,#809,.T.);
#9755=EDGE_CURVE('',#7537,#7519,#6009,.T.);
#9756=EDGE_CURVE('',#7503,#7466,#810,.T.);
#9757=EDGE_CURVE('',#7538,#7538,#6010,.T.);
#9758=EDGE_CURVE('',#7538,#7537,#6011,.T.);
#9759=EDGE_CURVE('',#7539,#7539,#6012,.T.);
#9760=EDGE_CURVE('',#7540,#7541,#6013,.T.);
#9761=EDGE_CURVE('',#7542,#7540,#4322,.T.);
#9762=EDGE_CURVE('',#7543,#7542,#6014,.T.);
#9763=EDGE_CURVE('',#7544,#7543,#4323,.T.);
#9764=EDGE_CURVE('',#7541,#7544,#6015,.T.);
#9765=EDGE_CURVE('',#7544,#7545,#4324,.T.);
#9766=EDGE_CURVE('',#7546,#7543,#4325,.T.);
#9767=EDGE_CURVE('',#7547,#7546,#356,.T.);
#9768=EDGE_CURVE('',#7548,#7547,#4326,.T.);
#9769=EDGE_CURVE('',#7545,#7548,#357,.T.);
#9770=EDGE_CURVE('',#7549,#7540,#4327,.T.);
#9771=EDGE_CURVE('',#7550,#7549,#358,.T.);
#9772=EDGE_CURVE('',#7551,#7550,#4328,.T.);
#9773=EDGE_CURVE('',#7552,#7551,#359,.T.);
#9774=EDGE_CURVE('',#7542,#7552,#4329,.T.);
#9775=EDGE_CURVE('',#7541,#7539,#4330,.T.);
#9776=EDGE_CURVE('',#7546,#7545,#6016,.T.);
#9777=EDGE_CURVE('',#7549,#7552,#6017,.T.);
#9778=EDGE_CURVE('',#7547,#7548,#6018,.T.);
#9779=EDGE_CURVE('',#7550,#7551,#6019,.T.);
#9780=EDGE_CURVE('',#7553,#7553,#6020,.T.);
#9781=EDGE_CURVE('',#7553,#7535,#4331,.T.);
#9782=ORIENTED_EDGE('',*,*,#7554,.T.);
#9783=ORIENTED_EDGE('',*,*,#7555,.T.);
#9784=ORIENTED_EDGE('',*,*,#7556,.T.);
#9785=ORIENTED_EDGE('',*,*,#7555,.F.);
#9786=ORIENTED_EDGE('',*,*,#7557,.F.);
#9787=ORIENTED_EDGE('',*,*,#7558,.F.);
#9788=ORIENTED_EDGE('',*,*,#7559,.F.);
#9789=ORIENTED_EDGE('',*,*,#7560,.F.);
#9790=ORIENTED_EDGE('',*,*,#7561,.F.);
#9791=ORIENTED_EDGE('',*,*,#7562,.F.);
#9792=ORIENTED_EDGE('',*,*,#7563,.F.);
#9793=ORIENTED_EDGE('',*,*,#7556,.F.);
#9794=ORIENTED_EDGE('',*,*,#7554,.F.);
#9795=ORIENTED_EDGE('',*,*,#7564,.T.);
#9796=ORIENTED_EDGE('',*,*,#7565,.F.);
#9797=ORIENTED_EDGE('',*,*,#7564,.F.);
#9798=ORIENTED_EDGE('',*,*,#7566,.T.);
#9799=ORIENTED_EDGE('',*,*,#7567,.T.);
#9800=ORIENTED_EDGE('',*,*,#7561,.T.);
#9801=ORIENTED_EDGE('',*,*,#7567,.F.);
#9802=ORIENTED_EDGE('',*,*,#7566,.F.);
#9803=ORIENTED_EDGE('',*,*,#7568,.T.);
#9804=ORIENTED_EDGE('',*,*,#7569,.F.);
#9805=ORIENTED_EDGE('',*,*,#7568,.F.);
#9806=ORIENTED_EDGE('',*,*,#7570,.T.);
#9807=ORIENTED_EDGE('',*,*,#7571,.T.);
#9808=ORIENTED_EDGE('',*,*,#7563,.T.);
#9809=ORIENTED_EDGE('',*,*,#7571,.F.);
#9810=ORIENTED_EDGE('',*,*,#7570,.F.);
#9811=ORIENTED_EDGE('',*,*,#7572,.T.);
#9812=ORIENTED_EDGE('',*,*,#7573,.F.);
#9813=ORIENTED_EDGE('',*,*,#7572,.F.);
#9814=ORIENTED_EDGE('',*,*,#7574,.T.);
#9815=ORIENTED_EDGE('',*,*,#7575,.T.);
#9816=ORIENTED_EDGE('',*,*,#7562,.T.);
#9817=ORIENTED_EDGE('',*,*,#7575,.F.);
#9818=ORIENTED_EDGE('',*,*,#7574,.F.);
#9819=ORIENTED_EDGE('',*,*,#7576,.T.);
#9820=ORIENTED_EDGE('',*,*,#7577,.F.);
#9821=ORIENTED_EDGE('',*,*,#7576,.F.);
#9822=ORIENTED_EDGE('',*,*,#7578,.T.);
#9823=ORIENTED_EDGE('',*,*,#7579,.T.);
#9824=ORIENTED_EDGE('',*,*,#7580,.T.);
#9825=ORIENTED_EDGE('',*,*,#7579,.F.);
#9826=ORIENTED_EDGE('',*,*,#7581,.F.);
#9827=ORIENTED_EDGE('',*,*,#7582,.F.);
#9828=ORIENTED_EDGE('',*,*,#7583,.T.);
#9829=ORIENTED_EDGE('',*,*,#7584,.F.);
#9830=ORIENTED_EDGE('',*,*,#7585,.F.);
#9831=ORIENTED_EDGE('',*,*,#7586,.F.);
#9832=ORIENTED_EDGE('',*,*,#7587,.F.);
#9833=ORIENTED_EDGE('',*,*,#7580,.F.);
#9834=ORIENTED_EDGE('',*,*,#7578,.F.);
#9835=ORIENTED_EDGE('',*,*,#7588,.T.);
#9836=ORIENTED_EDGE('',*,*,#7589,.F.);
#9837=ORIENTED_EDGE('',*,*,#7588,.F.);
#9838=ORIENTED_EDGE('',*,*,#7590,.T.);
#9839=ORIENTED_EDGE('',*,*,#7591,.T.);
#9840=ORIENTED_EDGE('',*,*,#7585,.T.);
#9841=ORIENTED_EDGE('',*,*,#7591,.F.);
#9842=ORIENTED_EDGE('',*,*,#7590,.F.);
#9843=ORIENTED_EDGE('',*,*,#7592,.T.);
#9844=ORIENTED_EDGE('',*,*,#7593,.F.);
#9845=ORIENTED_EDGE('',*,*,#7592,.F.);
#9846=ORIENTED_EDGE('',*,*,#7594,.T.);
#9847=ORIENTED_EDGE('',*,*,#7595,.T.);
#9848=ORIENTED_EDGE('',*,*,#7587,.T.);
#9849=ORIENTED_EDGE('',*,*,#7595,.F.);
#9850=ORIENTED_EDGE('',*,*,#7594,.F.);
#9851=ORIENTED_EDGE('',*,*,#7596,.T.);
#9852=ORIENTED_EDGE('',*,*,#7597,.F.);
#9853=ORIENTED_EDGE('',*,*,#7596,.F.);
#9854=ORIENTED_EDGE('',*,*,#7598,.T.);
#9855=ORIENTED_EDGE('',*,*,#7599,.T.);
#9856=ORIENTED_EDGE('',*,*,#7586,.T.);
#9857=ORIENTED_EDGE('',*,*,#7599,.F.);
#9858=ORIENTED_EDGE('',*,*,#7598,.F.);
#9859=ORIENTED_EDGE('',*,*,#7600,.T.);
#9860=ORIENTED_EDGE('',*,*,#7601,.F.);
#9861=ORIENTED_EDGE('',*,*,#7600,.F.);
#9862=ORIENTED_EDGE('',*,*,#7602,.T.);
#9863=ORIENTED_EDGE('',*,*,#7603,.T.);
#9864=ORIENTED_EDGE('',*,*,#7604,.T.);
#9865=ORIENTED_EDGE('',*,*,#7603,.F.);
#9866=ORIENTED_EDGE('',*,*,#7605,.F.);
#9867=ORIENTED_EDGE('',*,*,#7606,.F.);
#9868=ORIENTED_EDGE('',*,*,#7607,.F.);
#9869=ORIENTED_EDGE('',*,*,#7608,.F.);
#9870=ORIENTED_EDGE('',*,*,#7609,.F.);
#9871=ORIENTED_EDGE('',*,*,#7610,.F.);
#9872=ORIENTED_EDGE('',*,*,#7611,.F.);
#9873=ORIENTED_EDGE('',*,*,#7612,.F.);
#9874=ORIENTED_EDGE('',*,*,#7613,.F.);
#9875=ORIENTED_EDGE('',*,*,#7614,.F.);
#9876=ORIENTED_EDGE('',*,*,#7615,.F.);
#9877=ORIENTED_EDGE('',*,*,#7604,.F.);
#9878=ORIENTED_EDGE('',*,*,#7602,.F.);
#9879=ORIENTED_EDGE('',*,*,#7616,.T.);
#9880=ORIENTED_EDGE('',*,*,#7617,.T.);
#9881=ORIENTED_EDGE('',*,*,#7616,.F.);
#9882=ORIENTED_EDGE('',*,*,#7618,.T.);
#9883=ORIENTED_EDGE('',*,*,#7619,.T.);
#9884=ORIENTED_EDGE('',*,*,#7609,.T.);
#9885=ORIENTED_EDGE('',*,*,#7619,.F.);
#9886=ORIENTED_EDGE('',*,*,#7618,.F.);
#9887=ORIENTED_EDGE('',*,*,#7620,.T.);
#9888=ORIENTED_EDGE('',*,*,#7621,.T.);
#9889=ORIENTED_EDGE('',*,*,#7620,.F.);
#9890=ORIENTED_EDGE('',*,*,#7622,.T.);
#9891=ORIENTED_EDGE('',*,*,#7623,.T.);
#9892=ORIENTED_EDGE('',*,*,#7615,.T.);
#9893=ORIENTED_EDGE('',*,*,#7623,.F.);
#9894=ORIENTED_EDGE('',*,*,#7622,.F.);
#9895=ORIENTED_EDGE('',*,*,#7624,.T.);
#9896=ORIENTED_EDGE('',*,*,#7625,.T.);
#9897=ORIENTED_EDGE('',*,*,#7624,.F.);
#9898=ORIENTED_EDGE('',*,*,#7626,.T.);
#9899=ORIENTED_EDGE('',*,*,#7627,.T.);
#9900=ORIENTED_EDGE('',*,*,#7610,.T.);
#9901=ORIENTED_EDGE('',*,*,#7627,.F.);
#9902=ORIENTED_EDGE('',*,*,#7626,.F.);
#9903=ORIENTED_EDGE('',*,*,#7628,.T.);
#9904=ORIENTED_EDGE('',*,*,#7629,.T.);
#9905=ORIENTED_EDGE('',*,*,#7628,.F.);
#9906=ORIENTED_EDGE('',*,*,#7630,.T.);
#9907=ORIENTED_EDGE('',*,*,#7631,.T.);
#9908=ORIENTED_EDGE('',*,*,#7614,.T.);
#9909=ORIENTED_EDGE('',*,*,#7631,.F.);
#9910=ORIENTED_EDGE('',*,*,#7630,.F.);
#9911=ORIENTED_EDGE('',*,*,#7632,.T.);
#9912=ORIENTED_EDGE('',*,*,#7633,.T.);
#9913=ORIENTED_EDGE('',*,*,#7632,.F.);
#9914=ORIENTED_EDGE('',*,*,#7634,.T.);
#9915=ORIENTED_EDGE('',*,*,#7635,.T.);
#9916=ORIENTED_EDGE('',*,*,#7611,.T.);
#9917=ORIENTED_EDGE('',*,*,#7635,.F.);
#9918=ORIENTED_EDGE('',*,*,#7634,.F.);
#9919=ORIENTED_EDGE('',*,*,#7636,.T.);
#9920=ORIENTED_EDGE('',*,*,#7637,.T.);
#9921=ORIENTED_EDGE('',*,*,#7636,.F.);
#9922=ORIENTED_EDGE('',*,*,#7638,.T.);
#9923=ORIENTED_EDGE('',*,*,#7639,.T.);
#9924=ORIENTED_EDGE('',*,*,#7613,.T.);
#9925=ORIENTED_EDGE('',*,*,#7639,.F.);
#9926=ORIENTED_EDGE('',*,*,#7638,.F.);
#9927=ORIENTED_EDGE('',*,*,#7640,.T.);
#9928=ORIENTED_EDGE('',*,*,#7641,.T.);
#9929=ORIENTED_EDGE('',*,*,#7640,.F.);
#9930=ORIENTED_EDGE('',*,*,#7642,.T.);
#9931=ORIENTED_EDGE('',*,*,#7643,.T.);
#9932=ORIENTED_EDGE('',*,*,#7612,.T.);
#9933=ORIENTED_EDGE('',*,*,#7643,.F.);
#9934=ORIENTED_EDGE('',*,*,#7642,.F.);
#9935=ORIENTED_EDGE('',*,*,#7644,.T.);
#9936=ORIENTED_EDGE('',*,*,#7645,.T.);
#9937=ORIENTED_EDGE('',*,*,#7644,.F.);
#9938=ORIENTED_EDGE('',*,*,#7646,.T.);
#9939=ORIENTED_EDGE('',*,*,#7617,.F.);
#9940=ORIENTED_EDGE('',*,*,#7646,.F.);
#9941=ORIENTED_EDGE('',*,*,#7647,.T.);
#9942=ORIENTED_EDGE('',*,*,#7645,.F.);
#9943=ORIENTED_EDGE('',*,*,#7647,.F.);
#9944=ORIENTED_EDGE('',*,*,#7648,.T.);
#9945=ORIENTED_EDGE('',*,*,#7621,.F.);
#9946=ORIENTED_EDGE('',*,*,#7648,.F.);
#9947=ORIENTED_EDGE('',*,*,#7649,.T.);
#9948=ORIENTED_EDGE('',*,*,#7641,.F.);
#9949=ORIENTED_EDGE('',*,*,#7649,.F.);
#9950=ORIENTED_EDGE('',*,*,#7650,.T.);
#9951=ORIENTED_EDGE('',*,*,#7637,.F.);
#9952=ORIENTED_EDGE('',*,*,#7650,.F.);
#9953=ORIENTED_EDGE('',*,*,#7651,.T.);
#9954=ORIENTED_EDGE('',*,*,#7629,.F.);
#9955=ORIENTED_EDGE('',*,*,#7651,.F.);
#9956=ORIENTED_EDGE('',*,*,#7652,.T.);
#9957=ORIENTED_EDGE('',*,*,#7633,.F.);
#9958=ORIENTED_EDGE('',*,*,#7652,.F.);
#9959=ORIENTED_EDGE('',*,*,#7653,.T.);
#9960=ORIENTED_EDGE('',*,*,#7625,.F.);
#9961=ORIENTED_EDGE('',*,*,#7653,.F.);
#9962=ORIENTED_EDGE('',*,*,#7654,.T.);
#9963=ORIENTED_EDGE('',*,*,#7655,.T.);
#9964=ORIENTED_EDGE('',*,*,#7656,.T.);
#9965=ORIENTED_EDGE('',*,*,#7657,.T.);
#9966=ORIENTED_EDGE('',*,*,#7658,.T.);
#9967=ORIENTED_EDGE('',*,*,#7656,.F.);
#9968=ORIENTED_EDGE('',*,*,#7659,.T.);
#9969=ORIENTED_EDGE('',*,*,#7660,.T.);
#9970=ORIENTED_EDGE('',*,*,#7661,.T.);
#9971=ORIENTED_EDGE('',*,*,#7605,.T.);
#9972=ORIENTED_EDGE('',*,*,#7662,.T.);
#9973=ORIENTED_EDGE('',*,*,#7655,.F.);
#9974=ORIENTED_EDGE('',*,*,#7663,.T.);
#9975=ORIENTED_EDGE('',*,*,#7664,.T.);
#9976=ORIENTED_EDGE('',*,*,#7665,.T.);
#9977=ORIENTED_EDGE('',*,*,#7666,.T.);
#9978=ORIENTED_EDGE('',*,*,#7667,.F.);
#9979=ORIENTED_EDGE('',*,*,#7668,.T.);
#9980=ORIENTED_EDGE('',*,*,#7669,.F.);
#9981=ORIENTED_EDGE('',*,*,#7584,.T.);
#9982=ORIENTED_EDGE('',*,*,#7670,.T.);
#9983=ORIENTED_EDGE('',*,*,#7558,.T.);
#9984=ORIENTED_EDGE('',*,*,#7671,.F.);
#9985=ORIENTED_EDGE('',*,*,#7672,.T.);
#9986=ORIENTED_EDGE('',*,*,#7673,.F.);
#9987=ORIENTED_EDGE('',*,*,#7674,.T.);
#9988=ORIENTED_EDGE('',*,*,#7675,.T.);
#9989=ORIENTED_EDGE('',*,*,#7676,.T.);
#9990=ORIENTED_EDGE('',*,*,#7677,.T.);
#9991=ORIENTED_EDGE('',*,*,#7678,.F.);
#9992=ORIENTED_EDGE('',*,*,#7659,.F.);
#9993=ORIENTED_EDGE('',*,*,#7654,.F.);
#9994=ORIENTED_EDGE('',*,*,#7679,.T.);
#9995=ORIENTED_EDGE('',*,*,#7680,.F.);
#9996=ORIENTED_EDGE('',*,*,#7681,.T.);
#9997=ORIENTED_EDGE('',*,*,#7661,.F.);
#9998=ORIENTED_EDGE('',*,*,#7682,.F.);
#9999=ORIENTED_EDGE('',*,*,#7683,.T.);
#10000=ORIENTED_EDGE('',*,*,#7684,.F.);
#10001=ORIENTED_EDGE('',*,*,#7685,.F.);
#10002=ORIENTED_EDGE('',*,*,#7606,.T.);
#10003=ORIENTED_EDGE('',*,*,#7660,.F.);
#10004=ORIENTED_EDGE('',*,*,#7678,.T.);
#10005=ORIENTED_EDGE('',*,*,#7686,.T.);
#10006=ORIENTED_EDGE('',*,*,#7687,.T.);
#10007=ORIENTED_EDGE('',*,*,#7682,.T.);
#10008=ORIENTED_EDGE('',*,*,#7687,.F.);
#10009=ORIENTED_EDGE('',*,*,#7688,.F.);
#10010=ORIENTED_EDGE('',*,*,#7689,.F.);
#10011=ORIENTED_EDGE('',*,*,#7683,.F.);
#10012=ORIENTED_EDGE('',*,*,#7690,.T.);
#10013=ORIENTED_EDGE('',*,*,#7691,.T.);
#10014=ORIENTED_EDGE('',*,*,#7692,.T.);
#10015=ORIENTED_EDGE('',*,*,#7684,.T.);
#10016=ORIENTED_EDGE('',*,*,#7689,.T.);
#10017=ORIENTED_EDGE('',*,*,#7692,.F.);
#10018=ORIENTED_EDGE('',*,*,#7693,.T.);
#10019=ORIENTED_EDGE('',*,*,#7694,.T.);
#10020=ORIENTED_EDGE('',*,*,#7695,.T.);
#10021=ORIENTED_EDGE('',*,*,#7607,.T.);
#10022=ORIENTED_EDGE('',*,*,#7685,.T.);
#10023=ORIENTED_EDGE('',*,*,#7657,.F.);
#10024=ORIENTED_EDGE('',*,*,#7662,.F.);
#10025=ORIENTED_EDGE('',*,*,#7608,.T.);
#10026=ORIENTED_EDGE('',*,*,#7695,.F.);
#10027=ORIENTED_EDGE('',*,*,#7696,.F.);
#10028=ORIENTED_EDGE('',*,*,#7697,.T.);
#10029=ORIENTED_EDGE('',*,*,#7694,.F.);
#10030=ORIENTED_EDGE('',*,*,#7698,.T.);
#10031=ORIENTED_EDGE('',*,*,#7680,.T.);
#10032=ORIENTED_EDGE('',*,*,#7699,.T.);
#10033=ORIENTED_EDGE('',*,*,#7696,.T.);
#10034=ORIENTED_EDGE('',*,*,#7691,.F.);
#10035=ORIENTED_EDGE('',*,*,#7700,.T.);
#10036=ORIENTED_EDGE('',*,*,#7701,.T.);
#10037=ORIENTED_EDGE('',*,*,#7702,.T.);
#10038=ORIENTED_EDGE('',*,*,#7703,.T.);
#10039=ORIENTED_EDGE('',*,*,#7704,.F.);
#10040=ORIENTED_EDGE('',*,*,#7705,.T.);
#10041=ORIENTED_EDGE('',*,*,#7706,.F.);
#10042=ORIENTED_EDGE('',*,*,#7560,.T.);
#10043=ORIENTED_EDGE('',*,*,#7707,.T.);
#10044=ORIENTED_EDGE('',*,*,#7582,.T.);
#10045=ORIENTED_EDGE('',*,*,#7708,.F.);
#10046=ORIENTED_EDGE('',*,*,#7709,.T.);
#10047=ORIENTED_EDGE('',*,*,#7710,.F.);
#10048=ORIENTED_EDGE('',*,*,#7711,.T.);
#10049=ORIENTED_EDGE('',*,*,#7712,.T.);
#10050=ORIENTED_EDGE('',*,*,#7713,.T.);
#10051=ORIENTED_EDGE('',*,*,#7714,.T.);
#10052=ORIENTED_EDGE('',*,*,#7698,.F.);
#10053=ORIENTED_EDGE('',*,*,#7693,.F.);
#10054=ORIENTED_EDGE('',*,*,#7667,.T.);
#10055=ORIENTED_EDGE('',*,*,#7715,.T.);
#10056=ORIENTED_EDGE('',*,*,#7710,.T.);
#10057=ORIENTED_EDGE('',*,*,#7716,.T.);
#10058=ORIENTED_EDGE('',*,*,#7716,.F.);
#10059=ORIENTED_EDGE('',*,*,#7709,.F.);
#10060=ORIENTED_EDGE('',*,*,#7717,.F.);
#10061=ORIENTED_EDGE('',*,*,#7668,.F.);
#10062=ORIENTED_EDGE('',*,*,#7669,.T.);
#10063=ORIENTED_EDGE('',*,*,#7717,.T.);
#10064=ORIENTED_EDGE('',*,*,#7708,.T.);
#10065=ORIENTED_EDGE('',*,*,#7581,.T.);
#10066=ORIENTED_EDGE('',*,*,#7671,.T.);
#10067=ORIENTED_EDGE('',*,*,#7557,.T.);
#10068=ORIENTED_EDGE('',*,*,#7706,.T.);
#10069=ORIENTED_EDGE('',*,*,#7718,.T.);
#10070=ORIENTED_EDGE('',*,*,#7718,.F.);
#10071=ORIENTED_EDGE('',*,*,#7705,.F.);
#10072=ORIENTED_EDGE('',*,*,#7719,.F.);
#10073=ORIENTED_EDGE('',*,*,#7672,.F.);
#10074=ORIENTED_EDGE('',*,*,#7673,.T.);
#10075=ORIENTED_EDGE('',*,*,#7719,.T.);
#10076=ORIENTED_EDGE('',*,*,#7704,.T.);
#10077=ORIENTED_EDGE('',*,*,#7720,.T.);
#10078=ORIENTED_EDGE('',*,*,#7720,.F.);
#10079=ORIENTED_EDGE('',*,*,#7703,.F.);
#10080=ORIENTED_EDGE('',*,*,#7721,.T.);
#10081=ORIENTED_EDGE('',*,*,#7674,.F.);
#10082=ORIENTED_EDGE('',*,*,#7577,.T.);
#10083=ORIENTED_EDGE('',*,*,#7573,.T.);
#10084=ORIENTED_EDGE('',*,*,#7569,.T.);
#10085=ORIENTED_EDGE('',*,*,#7565,.T.);
#10086=ORIENTED_EDGE('',*,*,#7686,.F.);
#10087=ORIENTED_EDGE('',*,*,#7722,.T.);
#10088=ORIENTED_EDGE('',*,*,#7690,.F.);
#10089=ORIENTED_EDGE('',*,*,#7688,.T.);
#10090=ORIENTED_EDGE('',*,*,#7681,.F.);
#10091=ORIENTED_EDGE('',*,*,#7714,.F.);
#10092=ORIENTED_EDGE('',*,*,#7723,.T.);
#10093=ORIENTED_EDGE('',*,*,#7663,.F.);
#10094=ORIENTED_EDGE('',*,*,#7658,.F.);
#10095=ORIENTED_EDGE('',*,*,#7697,.F.);
#10096=ORIENTED_EDGE('',*,*,#7699,.F.);
#10097=ORIENTED_EDGE('',*,*,#7679,.F.);
#10098=ORIENTED_EDGE('',*,*,#7722,.F.);
#10099=ORIENTED_EDGE('',*,*,#7677,.F.);
#10100=ORIENTED_EDGE('',*,*,#7724,.F.);
#10101=ORIENTED_EDGE('',*,*,#7700,.F.);
#10102=ORIENTED_EDGE('',*,*,#7701,.F.);
#10103=ORIENTED_EDGE('',*,*,#7724,.T.);
#10104=ORIENTED_EDGE('',*,*,#7676,.F.);
#10105=ORIENTED_EDGE('',*,*,#7725,.F.);
#10106=ORIENTED_EDGE('',*,*,#7702,.F.);
#10107=ORIENTED_EDGE('',*,*,#7725,.T.);
#10108=ORIENTED_EDGE('',*,*,#7675,.F.);
#10109=ORIENTED_EDGE('',*,*,#7721,.F.);
#10110=ORIENTED_EDGE('',*,*,#7707,.F.);
#10111=ORIENTED_EDGE('',*,*,#7559,.T.);
#10112=ORIENTED_EDGE('',*,*,#7670,.F.);
#10113=ORIENTED_EDGE('',*,*,#7583,.F.);
#10114=ORIENTED_EDGE('',*,*,#7715,.F.);
#10115=ORIENTED_EDGE('',*,*,#7666,.F.);
#10116=ORIENTED_EDGE('',*,*,#7726,.F.);
#10117=ORIENTED_EDGE('',*,*,#7711,.F.);
#10118=ORIENTED_EDGE('',*,*,#7601,.T.);
#10119=ORIENTED_EDGE('',*,*,#7597,.T.);
#10120=ORIENTED_EDGE('',*,*,#7593,.T.);
#10121=ORIENTED_EDGE('',*,*,#7589,.T.);
#10122=ORIENTED_EDGE('',*,*,#7712,.F.);
#10123=ORIENTED_EDGE('',*,*,#7726,.T.);
#10124=ORIENTED_EDGE('',*,*,#7665,.F.);
#10125=ORIENTED_EDGE('',*,*,#7727,.F.);
#10126=ORIENTED_EDGE('',*,*,#7713,.F.);
#10127=ORIENTED_EDGE('',*,*,#7727,.T.);
#10128=ORIENTED_EDGE('',*,*,#7664,.F.);
#10129=ORIENTED_EDGE('',*,*,#7723,.F.);
#10130=ORIENTED_EDGE('',*,*,#7728,.T.);
#10131=ORIENTED_EDGE('',*,*,#7729,.T.);
#10132=ORIENTED_EDGE('',*,*,#7730,.T.);
#10133=ORIENTED_EDGE('',*,*,#7731,.T.);
#10134=ORIENTED_EDGE('',*,*,#7732,.T.);
#10135=ORIENTED_EDGE('',*,*,#7729,.F.);
#10136=ORIENTED_EDGE('',*,*,#7733,.T.);
#10137=ORIENTED_EDGE('',*,*,#7734,.T.);
#10138=ORIENTED_EDGE('',*,*,#7735,.T.);
#10139=ORIENTED_EDGE('',*,*,#7731,.F.);
#10140=ORIENTED_EDGE('',*,*,#7736,.T.);
#10141=ORIENTED_EDGE('',*,*,#7734,.F.);
#10142=ORIENTED_EDGE('',*,*,#7728,.F.);
#10143=ORIENTED_EDGE('',*,*,#7737,.T.);
#10144=ORIENTED_EDGE('',*,*,#7738,.F.);
#10145=ORIENTED_EDGE('',*,*,#7737,.F.);
#10146=ORIENTED_EDGE('',*,*,#7739,.T.);
#10147=ORIENTED_EDGE('',*,*,#7740,.T.);
#10148=ORIENTED_EDGE('',*,*,#7741,.T.);
#10149=ORIENTED_EDGE('',*,*,#7742,.T.);
#10150=ORIENTED_EDGE('',*,*,#7743,.T.);
#10151=ORIENTED_EDGE('',*,*,#7740,.F.);
#10152=ORIENTED_EDGE('',*,*,#7744,.T.);
#10153=ORIENTED_EDGE('',*,*,#7745,.T.);
#10154=ORIENTED_EDGE('',*,*,#7746,.T.);
#10155=ORIENTED_EDGE('',*,*,#7742,.F.);
#10156=ORIENTED_EDGE('',*,*,#7747,.T.);
#10157=ORIENTED_EDGE('',*,*,#7745,.F.);
#10158=ORIENTED_EDGE('',*,*,#7739,.F.);
#10159=ORIENTED_EDGE('',*,*,#7748,.T.);
#10160=ORIENTED_EDGE('',*,*,#7749,.F.);
#10161=ORIENTED_EDGE('',*,*,#7748,.F.);
#10162=ORIENTED_EDGE('',*,*,#7750,.T.);
#10163=ORIENTED_EDGE('',*,*,#7751,.T.);
#10164=ORIENTED_EDGE('',*,*,#7752,.T.);
#10165=ORIENTED_EDGE('',*,*,#7753,.T.);
#10166=ORIENTED_EDGE('',*,*,#7754,.T.);
#10167=ORIENTED_EDGE('',*,*,#7751,.F.);
#10168=ORIENTED_EDGE('',*,*,#7755,.T.);
#10169=ORIENTED_EDGE('',*,*,#7756,.T.);
#10170=ORIENTED_EDGE('',*,*,#7757,.T.);
#10171=ORIENTED_EDGE('',*,*,#7753,.F.);
#10172=ORIENTED_EDGE('',*,*,#7758,.T.);
#10173=ORIENTED_EDGE('',*,*,#7756,.F.);
#10174=ORIENTED_EDGE('',*,*,#7750,.F.);
#10175=ORIENTED_EDGE('',*,*,#7759,.T.);
#10176=ORIENTED_EDGE('',*,*,#7760,.F.);
#10177=ORIENTED_EDGE('',*,*,#7759,.F.);
#10178=ORIENTED_EDGE('',*,*,#7761,.F.);
#10179=ORIENTED_EDGE('',*,*,#7762,.F.);
#10180=ORIENTED_EDGE('',*,*,#7763,.F.);
#10181=ORIENTED_EDGE('',*,*,#7764,.F.);
#10182=ORIENTED_EDGE('',*,*,#7732,.F.);
#10183=ORIENTED_EDGE('',*,*,#7735,.F.);
#10184=ORIENTED_EDGE('',*,*,#7736,.F.);
#10185=ORIENTED_EDGE('',*,*,#7730,.F.);
#10186=ORIENTED_EDGE('',*,*,#7743,.F.);
#10187=ORIENTED_EDGE('',*,*,#7746,.F.);
#10188=ORIENTED_EDGE('',*,*,#7747,.F.);
#10189=ORIENTED_EDGE('',*,*,#7741,.F.);
#10190=ORIENTED_EDGE('',*,*,#7754,.F.);
#10191=ORIENTED_EDGE('',*,*,#7757,.F.);
#10192=ORIENTED_EDGE('',*,*,#7758,.F.);
#10193=ORIENTED_EDGE('',*,*,#7752,.F.);
#10194=ORIENTED_EDGE('',*,*,#7733,.F.);
#10195=ORIENTED_EDGE('',*,*,#7765,.T.);
#10196=ORIENTED_EDGE('',*,*,#7766,.T.);
#10197=ORIENTED_EDGE('',*,*,#7765,.F.);
#10198=ORIENTED_EDGE('',*,*,#7744,.F.);
#10199=ORIENTED_EDGE('',*,*,#7767,.T.);
#10200=ORIENTED_EDGE('',*,*,#7768,.T.);
#10201=ORIENTED_EDGE('',*,*,#7767,.F.);
#10202=ORIENTED_EDGE('',*,*,#7755,.F.);
#10203=ORIENTED_EDGE('',*,*,#7769,.T.);
#10204=ORIENTED_EDGE('',*,*,#7770,.T.);
#10205=ORIENTED_EDGE('',*,*,#7769,.F.);
#10206=ORIENTED_EDGE('',*,*,#7770,.F.);
#10207=ORIENTED_EDGE('',*,*,#7771,.F.);
#10208=ORIENTED_EDGE('',*,*,#7768,.F.);
#10209=ORIENTED_EDGE('',*,*,#7772,.F.);
#10210=ORIENTED_EDGE('',*,*,#7766,.F.);
#10211=ORIENTED_EDGE('',*,*,#7773,.F.);
#10212=ORIENTED_EDGE('',*,*,#7771,.T.);
#10213=ORIENTED_EDGE('',*,*,#7774,.T.);
#10214=ORIENTED_EDGE('',*,*,#7775,.F.);
#10215=ORIENTED_EDGE('',*,*,#7774,.F.);
#10216=ORIENTED_EDGE('',*,*,#7772,.T.);
#10217=ORIENTED_EDGE('',*,*,#7776,.T.);
#10218=ORIENTED_EDGE('',*,*,#7777,.F.);
#10219=ORIENTED_EDGE('',*,*,#7776,.F.);
#10220=ORIENTED_EDGE('',*,*,#7773,.T.);
#10221=ORIENTED_EDGE('',*,*,#7778,.T.);
#10222=ORIENTED_EDGE('',*,*,#7779,.F.);
#10223=ORIENTED_EDGE('',*,*,#7778,.F.);
#10224=ORIENTED_EDGE('',*,*,#7780,.T.);
#10225=ORIENTED_EDGE('',*,*,#7781,.T.);
#10226=ORIENTED_EDGE('',*,*,#7782,.T.);
#10227=ORIENTED_EDGE('',*,*,#7783,.T.);
#10228=ORIENTED_EDGE('',*,*,#7784,.T.);
#10229=ORIENTED_EDGE('',*,*,#7781,.F.);
#10230=ORIENTED_EDGE('',*,*,#7785,.T.);
#10231=ORIENTED_EDGE('',*,*,#7786,.T.);
#10232=ORIENTED_EDGE('',*,*,#7787,.T.);
#10233=ORIENTED_EDGE('',*,*,#7783,.F.);
#10234=ORIENTED_EDGE('',*,*,#7788,.T.);
#10235=ORIENTED_EDGE('',*,*,#7786,.F.);
#10236=ORIENTED_EDGE('',*,*,#7780,.F.);
#10237=ORIENTED_EDGE('',*,*,#7789,.T.);
#10238=ORIENTED_EDGE('',*,*,#7790,.F.);
#10239=ORIENTED_EDGE('',*,*,#7789,.F.);
#10240=ORIENTED_EDGE('',*,*,#7791,.T.);
#10241=ORIENTED_EDGE('',*,*,#7792,.T.);
#10242=ORIENTED_EDGE('',*,*,#7793,.T.);
#10243=ORIENTED_EDGE('',*,*,#7794,.T.);
#10244=ORIENTED_EDGE('',*,*,#7795,.T.);
#10245=ORIENTED_EDGE('',*,*,#7792,.F.);
#10246=ORIENTED_EDGE('',*,*,#7796,.T.);
#10247=ORIENTED_EDGE('',*,*,#7797,.T.);
#10248=ORIENTED_EDGE('',*,*,#7798,.T.);
#10249=ORIENTED_EDGE('',*,*,#7794,.F.);
#10250=ORIENTED_EDGE('',*,*,#7799,.T.);
#10251=ORIENTED_EDGE('',*,*,#7797,.F.);
#10252=ORIENTED_EDGE('',*,*,#7791,.F.);
#10253=ORIENTED_EDGE('',*,*,#7800,.T.);
#10254=ORIENTED_EDGE('',*,*,#7801,.F.);
#10255=ORIENTED_EDGE('',*,*,#7800,.F.);
#10256=ORIENTED_EDGE('',*,*,#7802,.T.);
#10257=ORIENTED_EDGE('',*,*,#7803,.T.);
#10258=ORIENTED_EDGE('',*,*,#7804,.T.);
#10259=ORIENTED_EDGE('',*,*,#7805,.T.);
#10260=ORIENTED_EDGE('',*,*,#7806,.T.);
#10261=ORIENTED_EDGE('',*,*,#7803,.F.);
#10262=ORIENTED_EDGE('',*,*,#7807,.T.);
#10263=ORIENTED_EDGE('',*,*,#7808,.T.);
#10264=ORIENTED_EDGE('',*,*,#7809,.T.);
#10265=ORIENTED_EDGE('',*,*,#7805,.F.);
#10266=ORIENTED_EDGE('',*,*,#7810,.T.);
#10267=ORIENTED_EDGE('',*,*,#7808,.F.);
#10268=ORIENTED_EDGE('',*,*,#7802,.F.);
#10269=ORIENTED_EDGE('',*,*,#7811,.T.);
#10270=ORIENTED_EDGE('',*,*,#7812,.F.);
#10271=ORIENTED_EDGE('',*,*,#7811,.F.);
#10272=ORIENTED_EDGE('',*,*,#7813,.F.);
#10273=ORIENTED_EDGE('',*,*,#7814,.F.);
#10274=ORIENTED_EDGE('',*,*,#7815,.F.);
#10275=ORIENTED_EDGE('',*,*,#7816,.F.);
#10276=ORIENTED_EDGE('',*,*,#7784,.F.);
#10277=ORIENTED_EDGE('',*,*,#7787,.F.);
#10278=ORIENTED_EDGE('',*,*,#7788,.F.);
#10279=ORIENTED_EDGE('',*,*,#7782,.F.);
#10280=ORIENTED_EDGE('',*,*,#7795,.F.);
#10281=ORIENTED_EDGE('',*,*,#7798,.F.);
#10282=ORIENTED_EDGE('',*,*,#7799,.F.);
#10283=ORIENTED_EDGE('',*,*,#7793,.F.);
#10284=ORIENTED_EDGE('',*,*,#7806,.F.);
#10285=ORIENTED_EDGE('',*,*,#7809,.F.);
#10286=ORIENTED_EDGE('',*,*,#7810,.F.);
#10287=ORIENTED_EDGE('',*,*,#7804,.F.);
#10288=ORIENTED_EDGE('',*,*,#7785,.F.);
#10289=ORIENTED_EDGE('',*,*,#7817,.T.);
#10290=ORIENTED_EDGE('',*,*,#7818,.T.);
#10291=ORIENTED_EDGE('',*,*,#7817,.F.);
#10292=ORIENTED_EDGE('',*,*,#7796,.F.);
#10293=ORIENTED_EDGE('',*,*,#7819,.T.);
#10294=ORIENTED_EDGE('',*,*,#7820,.T.);
#10295=ORIENTED_EDGE('',*,*,#7819,.F.);
#10296=ORIENTED_EDGE('',*,*,#7807,.F.);
#10297=ORIENTED_EDGE('',*,*,#7821,.T.);
#10298=ORIENTED_EDGE('',*,*,#7822,.T.);
#10299=ORIENTED_EDGE('',*,*,#7821,.F.);
#10300=ORIENTED_EDGE('',*,*,#7822,.F.);
#10301=ORIENTED_EDGE('',*,*,#7823,.F.);
#10302=ORIENTED_EDGE('',*,*,#7820,.F.);
#10303=ORIENTED_EDGE('',*,*,#7824,.F.);
#10304=ORIENTED_EDGE('',*,*,#7818,.F.);
#10305=ORIENTED_EDGE('',*,*,#7825,.F.);
#10306=ORIENTED_EDGE('',*,*,#7823,.T.);
#10307=ORIENTED_EDGE('',*,*,#7826,.T.);
#10308=ORIENTED_EDGE('',*,*,#7827,.F.);
#10309=ORIENTED_EDGE('',*,*,#7826,.F.);
#10310=ORIENTED_EDGE('',*,*,#7824,.T.);
#10311=ORIENTED_EDGE('',*,*,#7828,.T.);
#10312=ORIENTED_EDGE('',*,*,#7829,.F.);
#10313=ORIENTED_EDGE('',*,*,#7828,.F.);
#10314=ORIENTED_EDGE('',*,*,#7825,.T.);
#10315=ORIENTED_EDGE('',*,*,#7830,.T.);
#10316=ORIENTED_EDGE('',*,*,#7831,.F.);
#10317=ORIENTED_EDGE('',*,*,#7830,.F.);
#10318=ORIENTED_EDGE('',*,*,#7832,.T.);
#10319=ORIENTED_EDGE('',*,*,#7833,.T.);
#10320=ORIENTED_EDGE('',*,*,#7834,.T.);
#10321=ORIENTED_EDGE('',*,*,#7833,.F.);
#10322=ORIENTED_EDGE('',*,*,#7835,.F.);
#10323=ORIENTED_EDGE('',*,*,#7836,.T.);
#10324=ORIENTED_EDGE('',*,*,#7837,.F.);
#10325=ORIENTED_EDGE('',*,*,#7838,.T.);
#10326=ORIENTED_EDGE('',*,*,#7839,.T.);
#10327=ORIENTED_EDGE('',*,*,#7840,.T.);
#10328=ORIENTED_EDGE('',*,*,#7841,.T.);
#10329=ORIENTED_EDGE('',*,*,#7842,.T.);
#10330=ORIENTED_EDGE('',*,*,#7843,.T.);
#10331=ORIENTED_EDGE('',*,*,#7844,.T.);
#10332=ORIENTED_EDGE('',*,*,#7845,.F.);
#10333=ORIENTED_EDGE('',*,*,#7846,.T.);
#10334=ORIENTED_EDGE('',*,*,#7847,.F.);
#10335=ORIENTED_EDGE('',*,*,#7848,.F.);
#10336=ORIENTED_EDGE('',*,*,#7849,.F.);
#10337=ORIENTED_EDGE('',*,*,#7850,.F.);
#10338=ORIENTED_EDGE('',*,*,#7851,.F.);
#10339=ORIENTED_EDGE('',*,*,#7834,.F.);
#10340=ORIENTED_EDGE('',*,*,#7832,.F.);
#10341=ORIENTED_EDGE('',*,*,#7852,.T.);
#10342=ORIENTED_EDGE('',*,*,#7853,.T.);
#10343=ORIENTED_EDGE('',*,*,#7854,.T.);
#10344=ORIENTED_EDGE('',*,*,#7852,.F.);
#10345=ORIENTED_EDGE('',*,*,#7855,.T.);
#10346=ORIENTED_EDGE('',*,*,#7856,.T.);
#10347=ORIENTED_EDGE('',*,*,#7849,.T.);
#10348=ORIENTED_EDGE('',*,*,#7856,.F.);
#10349=ORIENTED_EDGE('',*,*,#7855,.F.);
#10350=ORIENTED_EDGE('',*,*,#7857,.T.);
#10351=ORIENTED_EDGE('',*,*,#7858,.T.);
#10352=ORIENTED_EDGE('',*,*,#7859,.T.);
#10353=ORIENTED_EDGE('',*,*,#7857,.F.);
#10354=ORIENTED_EDGE('',*,*,#7860,.T.);
#10355=ORIENTED_EDGE('',*,*,#7861,.T.);
#10356=ORIENTED_EDGE('',*,*,#7851,.T.);
#10357=ORIENTED_EDGE('',*,*,#7861,.F.);
#10358=ORIENTED_EDGE('',*,*,#7860,.F.);
#10359=ORIENTED_EDGE('',*,*,#7862,.T.);
#10360=ORIENTED_EDGE('',*,*,#7863,.T.);
#10361=ORIENTED_EDGE('',*,*,#7864,.T.);
#10362=ORIENTED_EDGE('',*,*,#7862,.F.);
#10363=ORIENTED_EDGE('',*,*,#7865,.T.);
#10364=ORIENTED_EDGE('',*,*,#7866,.T.);
#10365=ORIENTED_EDGE('',*,*,#7850,.T.);
#10366=ORIENTED_EDGE('',*,*,#7866,.F.);
#10367=ORIENTED_EDGE('',*,*,#7865,.F.);
#10368=ORIENTED_EDGE('',*,*,#7867,.T.);
#10369=ORIENTED_EDGE('',*,*,#7868,.T.);
#10370=ORIENTED_EDGE('',*,*,#7869,.T.);
#10371=ORIENTED_EDGE('',*,*,#7867,.F.);
#10372=ORIENTED_EDGE('',*,*,#7870,.T.);
#10373=ORIENTED_EDGE('',*,*,#7853,.F.);
#10374=ORIENTED_EDGE('',*,*,#7854,.F.);
#10375=ORIENTED_EDGE('',*,*,#7870,.F.);
#10376=ORIENTED_EDGE('',*,*,#7871,.T.);
#10377=ORIENTED_EDGE('',*,*,#7868,.F.);
#10378=ORIENTED_EDGE('',*,*,#7869,.F.);
#10379=ORIENTED_EDGE('',*,*,#7871,.F.);
#10380=ORIENTED_EDGE('',*,*,#7872,.T.);
#10381=ORIENTED_EDGE('',*,*,#7863,.F.);
#10382=ORIENTED_EDGE('',*,*,#7864,.F.);
#10383=ORIENTED_EDGE('',*,*,#7872,.F.);
#10384=ORIENTED_EDGE('',*,*,#7873,.T.);
#10385=ORIENTED_EDGE('',*,*,#7858,.F.);
#10386=ORIENTED_EDGE('',*,*,#7859,.F.);
#10387=ORIENTED_EDGE('',*,*,#7873,.F.);
#10388=ORIENTED_EDGE('',*,*,#7874,.T.);
#10389=ORIENTED_EDGE('',*,*,#7875,.T.);
#10390=ORIENTED_EDGE('',*,*,#7876,.T.);
#10391=ORIENTED_EDGE('',*,*,#7875,.F.);
#10392=ORIENTED_EDGE('',*,*,#7877,.F.);
#10393=ORIENTED_EDGE('',*,*,#7878,.F.);
#10394=ORIENTED_EDGE('',*,*,#7879,.F.);
#10395=ORIENTED_EDGE('',*,*,#7880,.F.);
#10396=ORIENTED_EDGE('',*,*,#7881,.F.);
#10397=ORIENTED_EDGE('',*,*,#7882,.F.);
#10398=ORIENTED_EDGE('',*,*,#7883,.F.);
#10399=ORIENTED_EDGE('',*,*,#7884,.F.);
#10400=ORIENTED_EDGE('',*,*,#7885,.F.);
#10401=ORIENTED_EDGE('',*,*,#7886,.F.);
#10402=ORIENTED_EDGE('',*,*,#7887,.F.);
#10403=ORIENTED_EDGE('',*,*,#7888,.F.);
#10404=ORIENTED_EDGE('',*,*,#7889,.F.);
#10405=ORIENTED_EDGE('',*,*,#7890,.F.);
#10406=ORIENTED_EDGE('',*,*,#7891,.F.);
#10407=ORIENTED_EDGE('',*,*,#7892,.F.);
#10408=ORIENTED_EDGE('',*,*,#7893,.F.);
#10409=ORIENTED_EDGE('',*,*,#7876,.F.);
#10410=ORIENTED_EDGE('',*,*,#7874,.F.);
#10411=ORIENTED_EDGE('',*,*,#7894,.T.);
#10412=ORIENTED_EDGE('',*,*,#7895,.T.);
#10413=ORIENTED_EDGE('',*,*,#7896,.T.);
#10414=ORIENTED_EDGE('',*,*,#7894,.F.);
#10415=ORIENTED_EDGE('',*,*,#7897,.T.);
#10416=ORIENTED_EDGE('',*,*,#7898,.T.);
#10417=ORIENTED_EDGE('',*,*,#7891,.T.);
#10418=ORIENTED_EDGE('',*,*,#7898,.F.);
#10419=ORIENTED_EDGE('',*,*,#7897,.F.);
#10420=ORIENTED_EDGE('',*,*,#7899,.T.);
#10421=ORIENTED_EDGE('',*,*,#7900,.T.);
#10422=ORIENTED_EDGE('',*,*,#7901,.T.);
#10423=ORIENTED_EDGE('',*,*,#7899,.F.);
#10424=ORIENTED_EDGE('',*,*,#7902,.T.);
#10425=ORIENTED_EDGE('',*,*,#7903,.T.);
#10426=ORIENTED_EDGE('',*,*,#7893,.T.);
#10427=ORIENTED_EDGE('',*,*,#7903,.F.);
#10428=ORIENTED_EDGE('',*,*,#7902,.F.);
#10429=ORIENTED_EDGE('',*,*,#7904,.T.);
#10430=ORIENTED_EDGE('',*,*,#7905,.T.);
#10431=ORIENTED_EDGE('',*,*,#7906,.T.);
#10432=ORIENTED_EDGE('',*,*,#7904,.F.);
#10433=ORIENTED_EDGE('',*,*,#7907,.T.);
#10434=ORIENTED_EDGE('',*,*,#7908,.T.);
#10435=ORIENTED_EDGE('',*,*,#7892,.T.);
#10436=ORIENTED_EDGE('',*,*,#7908,.F.);
#10437=ORIENTED_EDGE('',*,*,#7907,.F.);
#10438=ORIENTED_EDGE('',*,*,#7909,.T.);
#10439=ORIENTED_EDGE('',*,*,#7910,.T.);
#10440=ORIENTED_EDGE('',*,*,#7911,.T.);
#10441=ORIENTED_EDGE('',*,*,#7909,.F.);
#10442=ORIENTED_EDGE('',*,*,#7912,.T.);
#10443=ORIENTED_EDGE('',*,*,#7895,.F.);
#10444=ORIENTED_EDGE('',*,*,#7896,.F.);
#10445=ORIENTED_EDGE('',*,*,#7912,.F.);
#10446=ORIENTED_EDGE('',*,*,#7913,.T.);
#10447=ORIENTED_EDGE('',*,*,#7910,.F.);
#10448=ORIENTED_EDGE('',*,*,#7911,.F.);
#10449=ORIENTED_EDGE('',*,*,#7913,.F.);
#10450=ORIENTED_EDGE('',*,*,#7914,.T.);
#10451=ORIENTED_EDGE('',*,*,#7905,.F.);
#10452=ORIENTED_EDGE('',*,*,#7906,.F.);
#10453=ORIENTED_EDGE('',*,*,#7914,.F.);
#10454=ORIENTED_EDGE('',*,*,#7915,.T.);
#10455=ORIENTED_EDGE('',*,*,#7900,.F.);
#10456=ORIENTED_EDGE('',*,*,#7901,.F.);
#10457=ORIENTED_EDGE('',*,*,#7915,.F.);
#10458=ORIENTED_EDGE('',*,*,#7916,.T.);
#10459=ORIENTED_EDGE('',*,*,#7917,.T.);
#10460=ORIENTED_EDGE('',*,*,#7918,.T.);
#10461=ORIENTED_EDGE('',*,*,#7917,.F.);
#10462=ORIENTED_EDGE('',*,*,#7919,.F.);
#10463=ORIENTED_EDGE('',*,*,#7920,.F.);
#10464=ORIENTED_EDGE('',*,*,#7921,.F.);
#10465=ORIENTED_EDGE('',*,*,#7922,.F.);
#10466=ORIENTED_EDGE('',*,*,#7923,.F.);
#10467=ORIENTED_EDGE('',*,*,#7924,.F.);
#10468=ORIENTED_EDGE('',*,*,#7925,.F.);
#10469=ORIENTED_EDGE('',*,*,#7926,.F.);
#10470=ORIENTED_EDGE('',*,*,#7927,.F.);
#10471=ORIENTED_EDGE('',*,*,#7928,.F.);
#10472=ORIENTED_EDGE('',*,*,#7929,.F.);
#10473=ORIENTED_EDGE('',*,*,#7930,.F.);
#10474=ORIENTED_EDGE('',*,*,#7931,.F.);
#10475=ORIENTED_EDGE('',*,*,#7932,.F.);
#10476=ORIENTED_EDGE('',*,*,#7933,.F.);
#10477=ORIENTED_EDGE('',*,*,#7934,.F.);
#10478=ORIENTED_EDGE('',*,*,#7935,.F.);
#10479=ORIENTED_EDGE('',*,*,#7918,.F.);
#10480=ORIENTED_EDGE('',*,*,#7916,.F.);
#10481=ORIENTED_EDGE('',*,*,#7936,.T.);
#10482=ORIENTED_EDGE('',*,*,#7937,.T.);
#10483=ORIENTED_EDGE('',*,*,#7936,.F.);
#10484=ORIENTED_EDGE('',*,*,#7938,.T.);
#10485=ORIENTED_EDGE('',*,*,#7939,.T.);
#10486=ORIENTED_EDGE('',*,*,#7923,.T.);
#10487=ORIENTED_EDGE('',*,*,#7939,.F.);
#10488=ORIENTED_EDGE('',*,*,#7938,.F.);
#10489=ORIENTED_EDGE('',*,*,#7940,.T.);
#10490=ORIENTED_EDGE('',*,*,#7941,.T.);
#10491=ORIENTED_EDGE('',*,*,#7940,.F.);
#10492=ORIENTED_EDGE('',*,*,#7942,.T.);
#10493=ORIENTED_EDGE('',*,*,#7943,.T.);
#10494=ORIENTED_EDGE('',*,*,#7935,.T.);
#10495=ORIENTED_EDGE('',*,*,#7943,.F.);
#10496=ORIENTED_EDGE('',*,*,#7942,.F.);
#10497=ORIENTED_EDGE('',*,*,#7944,.T.);
#10498=ORIENTED_EDGE('',*,*,#7945,.T.);
#10499=ORIENTED_EDGE('',*,*,#7944,.F.);
#10500=ORIENTED_EDGE('',*,*,#7946,.T.);
#10501=ORIENTED_EDGE('',*,*,#7947,.T.);
#10502=ORIENTED_EDGE('',*,*,#7924,.T.);
#10503=ORIENTED_EDGE('',*,*,#7947,.F.);
#10504=ORIENTED_EDGE('',*,*,#7946,.F.);
#10505=ORIENTED_EDGE('',*,*,#7948,.T.);
#10506=ORIENTED_EDGE('',*,*,#7949,.T.);
#10507=ORIENTED_EDGE('',*,*,#7948,.F.);
#10508=ORIENTED_EDGE('',*,*,#7950,.T.);
#10509=ORIENTED_EDGE('',*,*,#7951,.T.);
#10510=ORIENTED_EDGE('',*,*,#7934,.T.);
#10511=ORIENTED_EDGE('',*,*,#7951,.F.);
#10512=ORIENTED_EDGE('',*,*,#7950,.F.);
#10513=ORIENTED_EDGE('',*,*,#7952,.T.);
#10514=ORIENTED_EDGE('',*,*,#7953,.T.);
#10515=ORIENTED_EDGE('',*,*,#7952,.F.);
#10516=ORIENTED_EDGE('',*,*,#7954,.T.);
#10517=ORIENTED_EDGE('',*,*,#7955,.T.);
#10518=ORIENTED_EDGE('',*,*,#7925,.T.);
#10519=ORIENTED_EDGE('',*,*,#7955,.F.);
#10520=ORIENTED_EDGE('',*,*,#7954,.F.);
#10521=ORIENTED_EDGE('',*,*,#7956,.T.);
#10522=ORIENTED_EDGE('',*,*,#7957,.T.);
#10523=ORIENTED_EDGE('',*,*,#7956,.F.);
#10524=ORIENTED_EDGE('',*,*,#7958,.T.);
#10525=ORIENTED_EDGE('',*,*,#7937,.F.);
#10526=ORIENTED_EDGE('',*,*,#7958,.F.);
#10527=ORIENTED_EDGE('',*,*,#7959,.T.);
#10528=ORIENTED_EDGE('',*,*,#7957,.F.);
#10529=ORIENTED_EDGE('',*,*,#7959,.F.);
#10530=ORIENTED_EDGE('',*,*,#7960,.T.);
#10531=ORIENTED_EDGE('',*,*,#7941,.F.);
#10532=ORIENTED_EDGE('',*,*,#7960,.F.);
#10533=ORIENTED_EDGE('',*,*,#7961,.T.);
#10534=ORIENTED_EDGE('',*,*,#7945,.F.);
#10535=ORIENTED_EDGE('',*,*,#7961,.F.);
#10536=ORIENTED_EDGE('',*,*,#7962,.T.);
#10537=ORIENTED_EDGE('',*,*,#7949,.F.);
#10538=ORIENTED_EDGE('',*,*,#7962,.F.);
#10539=ORIENTED_EDGE('',*,*,#7963,.T.);
#10540=ORIENTED_EDGE('',*,*,#7953,.F.);
#10541=ORIENTED_EDGE('',*,*,#7963,.F.);
#10542=ORIENTED_EDGE('',*,*,#7964,.T.);
#10543=ORIENTED_EDGE('',*,*,#7965,.T.);
#10544=ORIENTED_EDGE('',*,*,#7926,.T.);
#10545=ORIENTED_EDGE('',*,*,#7965,.F.);
#10546=ORIENTED_EDGE('',*,*,#7964,.F.);
#10547=ORIENTED_EDGE('',*,*,#7966,.T.);
#10548=ORIENTED_EDGE('',*,*,#7967,.T.);
#10549=ORIENTED_EDGE('',*,*,#7966,.F.);
#10550=ORIENTED_EDGE('',*,*,#7968,.T.);
#10551=ORIENTED_EDGE('',*,*,#7969,.T.);
#10552=ORIENTED_EDGE('',*,*,#7933,.T.);
#10553=ORIENTED_EDGE('',*,*,#7969,.F.);
#10554=ORIENTED_EDGE('',*,*,#7968,.F.);
#10555=ORIENTED_EDGE('',*,*,#7970,.T.);
#10556=ORIENTED_EDGE('',*,*,#7971,.T.);
#10557=ORIENTED_EDGE('',*,*,#7970,.F.);
#10558=ORIENTED_EDGE('',*,*,#7972,.T.);
#10559=ORIENTED_EDGE('',*,*,#7973,.T.);
#10560=ORIENTED_EDGE('',*,*,#7927,.T.);
#10561=ORIENTED_EDGE('',*,*,#7973,.F.);
#10562=ORIENTED_EDGE('',*,*,#7972,.F.);
#10563=ORIENTED_EDGE('',*,*,#7974,.T.);
#10564=ORIENTED_EDGE('',*,*,#7975,.T.);
#10565=ORIENTED_EDGE('',*,*,#7974,.F.);
#10566=ORIENTED_EDGE('',*,*,#7976,.T.);
#10567=ORIENTED_EDGE('',*,*,#7977,.T.);
#10568=ORIENTED_EDGE('',*,*,#7932,.T.);
#10569=ORIENTED_EDGE('',*,*,#7977,.F.);
#10570=ORIENTED_EDGE('',*,*,#7976,.F.);
#10571=ORIENTED_EDGE('',*,*,#7978,.T.);
#10572=ORIENTED_EDGE('',*,*,#7979,.T.);
#10573=ORIENTED_EDGE('',*,*,#7978,.F.);
#10574=ORIENTED_EDGE('',*,*,#7980,.T.);
#10575=ORIENTED_EDGE('',*,*,#7981,.T.);
#10576=ORIENTED_EDGE('',*,*,#7928,.T.);
#10577=ORIENTED_EDGE('',*,*,#7981,.F.);
#10578=ORIENTED_EDGE('',*,*,#7980,.F.);
#10579=ORIENTED_EDGE('',*,*,#7982,.T.);
#10580=ORIENTED_EDGE('',*,*,#7983,.T.);
#10581=ORIENTED_EDGE('',*,*,#7982,.F.);
#10582=ORIENTED_EDGE('',*,*,#7984,.T.);
#10583=ORIENTED_EDGE('',*,*,#7985,.T.);
#10584=ORIENTED_EDGE('',*,*,#7931,.T.);
#10585=ORIENTED_EDGE('',*,*,#7985,.F.);
#10586=ORIENTED_EDGE('',*,*,#7984,.F.);
#10587=ORIENTED_EDGE('',*,*,#7986,.T.);
#10588=ORIENTED_EDGE('',*,*,#7987,.T.);
#10589=ORIENTED_EDGE('',*,*,#7986,.F.);
#10590=ORIENTED_EDGE('',*,*,#7988,.T.);
#10591=ORIENTED_EDGE('',*,*,#7989,.T.);
#10592=ORIENTED_EDGE('',*,*,#7929,.T.);
#10593=ORIENTED_EDGE('',*,*,#7989,.F.);
#10594=ORIENTED_EDGE('',*,*,#7988,.F.);
#10595=ORIENTED_EDGE('',*,*,#7990,.T.);
#10596=ORIENTED_EDGE('',*,*,#7991,.T.);
#10597=ORIENTED_EDGE('',*,*,#7990,.F.);
#10598=ORIENTED_EDGE('',*,*,#7992,.T.);
#10599=ORIENTED_EDGE('',*,*,#7993,.T.);
#10600=ORIENTED_EDGE('',*,*,#7930,.T.);
#10601=ORIENTED_EDGE('',*,*,#7993,.F.);
#10602=ORIENTED_EDGE('',*,*,#7992,.F.);
#10603=ORIENTED_EDGE('',*,*,#7994,.T.);
#10604=ORIENTED_EDGE('',*,*,#7995,.T.);
#10605=ORIENTED_EDGE('',*,*,#7994,.F.);
#10606=ORIENTED_EDGE('',*,*,#7995,.F.);
#10607=ORIENTED_EDGE('',*,*,#7996,.F.);
#10608=ORIENTED_EDGE('',*,*,#7991,.F.);
#10609=ORIENTED_EDGE('',*,*,#7997,.F.);
#10610=ORIENTED_EDGE('',*,*,#7987,.F.);
#10611=ORIENTED_EDGE('',*,*,#7998,.F.);
#10612=ORIENTED_EDGE('',*,*,#7983,.F.);
#10613=ORIENTED_EDGE('',*,*,#7999,.F.);
#10614=ORIENTED_EDGE('',*,*,#7979,.F.);
#10615=ORIENTED_EDGE('',*,*,#8000,.F.);
#10616=ORIENTED_EDGE('',*,*,#7975,.F.);
#10617=ORIENTED_EDGE('',*,*,#8001,.F.);
#10618=ORIENTED_EDGE('',*,*,#7971,.F.);
#10619=ORIENTED_EDGE('',*,*,#8002,.F.);
#10620=ORIENTED_EDGE('',*,*,#7967,.F.);
#10621=ORIENTED_EDGE('',*,*,#8003,.F.);
#10622=ORIENTED_EDGE('',*,*,#7996,.T.);
#10623=ORIENTED_EDGE('',*,*,#8004,.T.);
#10624=ORIENTED_EDGE('',*,*,#8005,.F.);
#10625=ORIENTED_EDGE('',*,*,#8004,.F.);
#10626=ORIENTED_EDGE('',*,*,#7997,.T.);
#10627=ORIENTED_EDGE('',*,*,#8006,.T.);
#10628=ORIENTED_EDGE('',*,*,#8007,.F.);
#10629=ORIENTED_EDGE('',*,*,#8006,.F.);
#10630=ORIENTED_EDGE('',*,*,#7998,.T.);
#10631=ORIENTED_EDGE('',*,*,#8008,.T.);
#10632=ORIENTED_EDGE('',*,*,#8009,.F.);
#10633=ORIENTED_EDGE('',*,*,#8008,.F.);
#10634=ORIENTED_EDGE('',*,*,#7999,.T.);
#10635=ORIENTED_EDGE('',*,*,#8010,.T.);
#10636=ORIENTED_EDGE('',*,*,#8011,.F.);
#10637=ORIENTED_EDGE('',*,*,#8010,.F.);
#10638=ORIENTED_EDGE('',*,*,#8000,.T.);
#10639=ORIENTED_EDGE('',*,*,#8012,.T.);
#10640=ORIENTED_EDGE('',*,*,#8013,.F.);
#10641=ORIENTED_EDGE('',*,*,#8012,.F.);
#10642=ORIENTED_EDGE('',*,*,#8001,.T.);
#10643=ORIENTED_EDGE('',*,*,#8014,.T.);
#10644=ORIENTED_EDGE('',*,*,#8015,.F.);
#10645=ORIENTED_EDGE('',*,*,#8014,.F.);
#10646=ORIENTED_EDGE('',*,*,#8002,.T.);
#10647=ORIENTED_EDGE('',*,*,#8016,.T.);
#10648=ORIENTED_EDGE('',*,*,#8017,.F.);
#10649=ORIENTED_EDGE('',*,*,#8016,.F.);
#10650=ORIENTED_EDGE('',*,*,#8003,.T.);
#10651=ORIENTED_EDGE('',*,*,#8018,.T.);
#10652=ORIENTED_EDGE('',*,*,#8019,.F.);
#10653=ORIENTED_EDGE('',*,*,#8018,.F.);
#10654=ORIENTED_EDGE('',*,*,#8020,.T.);
#10655=ORIENTED_EDGE('',*,*,#7835,.T.);
#10656=ORIENTED_EDGE('',*,*,#8021,.T.);
#10657=ORIENTED_EDGE('',*,*,#8022,.T.);
#10658=ORIENTED_EDGE('',*,*,#7761,.T.);
#10659=ORIENTED_EDGE('',*,*,#8021,.F.);
#10660=ORIENTED_EDGE('',*,*,#7848,.T.);
#10661=ORIENTED_EDGE('',*,*,#8023,.T.);
#10662=ORIENTED_EDGE('',*,*,#8024,.T.);
#10663=ORIENTED_EDGE('',*,*,#7919,.T.);
#10664=ORIENTED_EDGE('',*,*,#8025,.T.);
#10665=ORIENTED_EDGE('',*,*,#8020,.F.);
#10666=ORIENTED_EDGE('',*,*,#7764,.T.);
#10667=ORIENTED_EDGE('',*,*,#8026,.F.);
#10668=ORIENTED_EDGE('',*,*,#8027,.T.);
#10669=ORIENTED_EDGE('',*,*,#8024,.F.);
#10670=ORIENTED_EDGE('',*,*,#8028,.F.);
#10671=ORIENTED_EDGE('',*,*,#7816,.T.);
#10672=ORIENTED_EDGE('',*,*,#8029,.F.);
#10673=ORIENTED_EDGE('',*,*,#8030,.F.);
#10674=ORIENTED_EDGE('',*,*,#7920,.T.);
#10675=ORIENTED_EDGE('',*,*,#8023,.F.);
#10676=ORIENTED_EDGE('',*,*,#7847,.T.);
#10677=ORIENTED_EDGE('',*,*,#8031,.T.);
#10678=ORIENTED_EDGE('',*,*,#7813,.T.);
#10679=ORIENTED_EDGE('',*,*,#8028,.T.);
#10680=ORIENTED_EDGE('',*,*,#8029,.T.);
#10681=ORIENTED_EDGE('',*,*,#7815,.T.);
#10682=ORIENTED_EDGE('',*,*,#8032,.T.);
#10683=ORIENTED_EDGE('',*,*,#7877,.T.);
#10684=ORIENTED_EDGE('',*,*,#8033,.T.);
#10685=ORIENTED_EDGE('',*,*,#8033,.F.);
#10686=ORIENTED_EDGE('',*,*,#7890,.T.);
#10687=ORIENTED_EDGE('',*,*,#8034,.T.);
#10688=ORIENTED_EDGE('',*,*,#8035,.T.);
#10689=ORIENTED_EDGE('',*,*,#7921,.T.);
#10690=ORIENTED_EDGE('',*,*,#8030,.T.);
#10691=ORIENTED_EDGE('',*,*,#8022,.F.);
#10692=ORIENTED_EDGE('',*,*,#8025,.F.);
#10693=ORIENTED_EDGE('',*,*,#7922,.T.);
#10694=ORIENTED_EDGE('',*,*,#8035,.F.);
#10695=ORIENTED_EDGE('',*,*,#8036,.F.);
#10696=ORIENTED_EDGE('',*,*,#7762,.T.);
#10697=ORIENTED_EDGE('',*,*,#8034,.F.);
#10698=ORIENTED_EDGE('',*,*,#7889,.T.);
#10699=ORIENTED_EDGE('',*,*,#8026,.T.);
#10700=ORIENTED_EDGE('',*,*,#7763,.T.);
#10701=ORIENTED_EDGE('',*,*,#8036,.T.);
#10702=ORIENTED_EDGE('',*,*,#7845,.T.);
#10703=ORIENTED_EDGE('',*,*,#8037,.T.);
#10704=ORIENTED_EDGE('',*,*,#7879,.T.);
#10705=ORIENTED_EDGE('',*,*,#8038,.T.);
#10706=ORIENTED_EDGE('',*,*,#8038,.F.);
#10707=ORIENTED_EDGE('',*,*,#7878,.T.);
#10708=ORIENTED_EDGE('',*,*,#8039,.F.);
#10709=ORIENTED_EDGE('',*,*,#7846,.F.);
#10710=ORIENTED_EDGE('',*,*,#8005,.T.);
#10711=ORIENTED_EDGE('',*,*,#8007,.T.);
#10712=ORIENTED_EDGE('',*,*,#8013,.T.);
#10713=ORIENTED_EDGE('',*,*,#8015,.T.);
#10714=ORIENTED_EDGE('',*,*,#7837,.T.);
#10715=ORIENTED_EDGE('',*,*,#8040,.T.);
#10716=ORIENTED_EDGE('',*,*,#7887,.T.);
#10717=ORIENTED_EDGE('',*,*,#8041,.T.);
#10718=ORIENTED_EDGE('',*,*,#8041,.F.);
#10719=ORIENTED_EDGE('',*,*,#7886,.T.);
#10720=ORIENTED_EDGE('',*,*,#8042,.T.);
#10721=ORIENTED_EDGE('',*,*,#7838,.F.);
#10722=ORIENTED_EDGE('',*,*,#7779,.T.);
#10723=ORIENTED_EDGE('',*,*,#7777,.T.);
#10724=ORIENTED_EDGE('',*,*,#7775,.T.);
#10725=ORIENTED_EDGE('',*,*,#7738,.T.);
#10726=ORIENTED_EDGE('',*,*,#7749,.T.);
#10727=ORIENTED_EDGE('',*,*,#7760,.T.);
#10728=ORIENTED_EDGE('',*,*,#8031,.F.);
#10729=ORIENTED_EDGE('',*,*,#8039,.T.);
#10730=ORIENTED_EDGE('',*,*,#8032,.F.);
#10731=ORIENTED_EDGE('',*,*,#7814,.T.);
#10732=ORIENTED_EDGE('',*,*,#8040,.F.);
#10733=ORIENTED_EDGE('',*,*,#7836,.F.);
#10734=ORIENTED_EDGE('',*,*,#8027,.F.);
#10735=ORIENTED_EDGE('',*,*,#7888,.T.);
#10736=ORIENTED_EDGE('',*,*,#8009,.T.);
#10737=ORIENTED_EDGE('',*,*,#8011,.T.);
#10738=ORIENTED_EDGE('',*,*,#8017,.T.);
#10739=ORIENTED_EDGE('',*,*,#8019,.T.);
#10740=ORIENTED_EDGE('',*,*,#8037,.F.);
#10741=ORIENTED_EDGE('',*,*,#7844,.F.);
#10742=ORIENTED_EDGE('',*,*,#8043,.F.);
#10743=ORIENTED_EDGE('',*,*,#7880,.T.);
#10744=ORIENTED_EDGE('',*,*,#7831,.T.);
#10745=ORIENTED_EDGE('',*,*,#7829,.T.);
#10746=ORIENTED_EDGE('',*,*,#7827,.T.);
#10747=ORIENTED_EDGE('',*,*,#7790,.T.);
#10748=ORIENTED_EDGE('',*,*,#7801,.T.);
#10749=ORIENTED_EDGE('',*,*,#7812,.T.);
#10750=ORIENTED_EDGE('',*,*,#7881,.T.);
#10751=ORIENTED_EDGE('',*,*,#8043,.T.);
#10752=ORIENTED_EDGE('',*,*,#7843,.F.);
#10753=ORIENTED_EDGE('',*,*,#8044,.F.);
#10754=ORIENTED_EDGE('',*,*,#7882,.T.);
#10755=ORIENTED_EDGE('',*,*,#8044,.T.);
#10756=ORIENTED_EDGE('',*,*,#7842,.F.);
#10757=ORIENTED_EDGE('',*,*,#8045,.F.);
#10758=ORIENTED_EDGE('',*,*,#7883,.T.);
#10759=ORIENTED_EDGE('',*,*,#8045,.T.);
#10760=ORIENTED_EDGE('',*,*,#7841,.F.);
#10761=ORIENTED_EDGE('',*,*,#8046,.F.);
#10762=ORIENTED_EDGE('',*,*,#7884,.T.);
#10763=ORIENTED_EDGE('',*,*,#8046,.T.);
#10764=ORIENTED_EDGE('',*,*,#7840,.F.);
#10765=ORIENTED_EDGE('',*,*,#8047,.F.);
#10766=ORIENTED_EDGE('',*,*,#7885,.T.);
#10767=ORIENTED_EDGE('',*,*,#8047,.T.);
#10768=ORIENTED_EDGE('',*,*,#7839,.F.);
#10769=ORIENTED_EDGE('',*,*,#8042,.F.);
#10770=ORIENTED_EDGE('',*,*,#8048,.T.);
#10771=ORIENTED_EDGE('',*,*,#8049,.T.);
#10772=ORIENTED_EDGE('',*,*,#8050,.T.);
#10773=ORIENTED_EDGE('',*,*,#8049,.F.);
#10774=ORIENTED_EDGE('',*,*,#8051,.F.);
#10775=ORIENTED_EDGE('',*,*,#8052,.F.);
#10776=ORIENTED_EDGE('',*,*,#8053,.T.);
#10777=ORIENTED_EDGE('',*,*,#8054,.F.);
#10778=ORIENTED_EDGE('',*,*,#8055,.F.);
#10779=ORIENTED_EDGE('',*,*,#8056,.F.);
#10780=ORIENTED_EDGE('',*,*,#8057,.T.);
#10781=ORIENTED_EDGE('',*,*,#8058,.F.);
#10782=ORIENTED_EDGE('',*,*,#8059,.T.);
#10783=ORIENTED_EDGE('',*,*,#8060,.T.);
#10784=ORIENTED_EDGE('',*,*,#8061,.T.);
#10785=ORIENTED_EDGE('',*,*,#8062,.T.);
#10786=ORIENTED_EDGE('',*,*,#8063,.T.);
#10787=ORIENTED_EDGE('',*,*,#8064,.F.);
#10788=ORIENTED_EDGE('',*,*,#8065,.T.);
#10789=ORIENTED_EDGE('',*,*,#8050,.F.);
#10790=ORIENTED_EDGE('',*,*,#8066,.T.);
#10791=ORIENTED_EDGE('',*,*,#8067,.F.);
#10792=ORIENTED_EDGE('',*,*,#8048,.F.);
#10793=ORIENTED_EDGE('',*,*,#8068,.T.);
#10794=ORIENTED_EDGE('',*,*,#8069,.T.);
#10795=ORIENTED_EDGE('',*,*,#8070,.T.);
#10796=ORIENTED_EDGE('',*,*,#8068,.F.);
#10797=ORIENTED_EDGE('',*,*,#8071,.T.);
#10798=ORIENTED_EDGE('',*,*,#8069,.F.);
#10799=ORIENTED_EDGE('',*,*,#8070,.F.);
#10800=ORIENTED_EDGE('',*,*,#8071,.F.);
#10801=ORIENTED_EDGE('',*,*,#8072,.T.);
#10802=ORIENTED_EDGE('',*,*,#8073,.T.);
#10803=ORIENTED_EDGE('',*,*,#8074,.T.);
#10804=ORIENTED_EDGE('',*,*,#8073,.F.);
#10805=ORIENTED_EDGE('',*,*,#8075,.F.);
#10806=ORIENTED_EDGE('',*,*,#8076,.F.);
#10807=ORIENTED_EDGE('',*,*,#8077,.T.);
#10808=ORIENTED_EDGE('',*,*,#8074,.F.);
#10809=ORIENTED_EDGE('',*,*,#8078,.T.);
#10810=ORIENTED_EDGE('',*,*,#8079,.F.);
#10811=ORIENTED_EDGE('',*,*,#8080,.T.);
#10812=ORIENTED_EDGE('',*,*,#8081,.T.);
#10813=ORIENTED_EDGE('',*,*,#8082,.T.);
#10814=ORIENTED_EDGE('',*,*,#8083,.T.);
#10815=ORIENTED_EDGE('',*,*,#8084,.T.);
#10816=ORIENTED_EDGE('',*,*,#8085,.F.);
#10817=ORIENTED_EDGE('',*,*,#8086,.T.);
#10818=ORIENTED_EDGE('',*,*,#8087,.F.);
#10819=ORIENTED_EDGE('',*,*,#8088,.F.);
#10820=ORIENTED_EDGE('',*,*,#8089,.F.);
#10821=ORIENTED_EDGE('',*,*,#8090,.T.);
#10822=ORIENTED_EDGE('',*,*,#8091,.F.);
#10823=ORIENTED_EDGE('',*,*,#8072,.F.);
#10824=ORIENTED_EDGE('',*,*,#8092,.T.);
#10825=ORIENTED_EDGE('',*,*,#8093,.T.);
#10826=ORIENTED_EDGE('',*,*,#8094,.T.);
#10827=ORIENTED_EDGE('',*,*,#8092,.F.);
#10828=ORIENTED_EDGE('',*,*,#8095,.T.);
#10829=ORIENTED_EDGE('',*,*,#8093,.F.);
#10830=ORIENTED_EDGE('',*,*,#8094,.F.);
#10831=ORIENTED_EDGE('',*,*,#8095,.F.);
#10832=ORIENTED_EDGE('',*,*,#8096,.T.);
#10833=ORIENTED_EDGE('',*,*,#8097,.T.);
#10834=ORIENTED_EDGE('',*,*,#8098,.T.);
#10835=ORIENTED_EDGE('',*,*,#8097,.F.);
#10836=ORIENTED_EDGE('',*,*,#8099,.F.);
#10837=ORIENTED_EDGE('',*,*,#8090,.F.);
#10838=ORIENTED_EDGE('',*,*,#8100,.F.);
#10839=ORIENTED_EDGE('',*,*,#8053,.F.);
#10840=ORIENTED_EDGE('',*,*,#8101,.F.);
#10841=ORIENTED_EDGE('',*,*,#8102,.F.);
#10842=ORIENTED_EDGE('',*,*,#8098,.F.);
#10843=ORIENTED_EDGE('',*,*,#8096,.F.);
#10844=ORIENTED_EDGE('',*,*,#8103,.T.);
#10845=ORIENTED_EDGE('',*,*,#8104,.F.);
#10846=ORIENTED_EDGE('',*,*,#8105,.F.);
#10847=ORIENTED_EDGE('',*,*,#8106,.F.);
#10848=ORIENTED_EDGE('',*,*,#8107,.T.);
#10849=ORIENTED_EDGE('',*,*,#8108,.F.);
#10850=ORIENTED_EDGE('',*,*,#8109,.F.);
#10851=ORIENTED_EDGE('',*,*,#8110,.F.);
#10852=ORIENTED_EDGE('',*,*,#8111,.F.);
#10853=ORIENTED_EDGE('',*,*,#8112,.F.);
#10854=ORIENTED_EDGE('',*,*,#8113,.T.);
#10855=ORIENTED_EDGE('',*,*,#8114,.F.);
#10856=ORIENTED_EDGE('',*,*,#8115,.F.);
#10857=ORIENTED_EDGE('',*,*,#8116,.F.);
#10858=ORIENTED_EDGE('',*,*,#8103,.F.);
#10859=ORIENTED_EDGE('',*,*,#8117,.T.);
#10860=ORIENTED_EDGE('',*,*,#8118,.T.);
#10861=ORIENTED_EDGE('',*,*,#8101,.T.);
#10862=ORIENTED_EDGE('',*,*,#8118,.F.);
#10863=ORIENTED_EDGE('',*,*,#8117,.F.);
#10864=ORIENTED_EDGE('',*,*,#8119,.T.);
#10865=ORIENTED_EDGE('',*,*,#8120,.F.);
#10866=ORIENTED_EDGE('',*,*,#8121,.F.);
#10867=ORIENTED_EDGE('',*,*,#8122,.F.);
#10868=ORIENTED_EDGE('',*,*,#8123,.T.);
#10869=ORIENTED_EDGE('',*,*,#8124,.F.);
#10870=ORIENTED_EDGE('',*,*,#8125,.F.);
#10871=ORIENTED_EDGE('',*,*,#8126,.F.);
#10872=ORIENTED_EDGE('',*,*,#8127,.F.);
#10873=ORIENTED_EDGE('',*,*,#8128,.F.);
#10874=ORIENTED_EDGE('',*,*,#8129,.T.);
#10875=ORIENTED_EDGE('',*,*,#8130,.F.);
#10876=ORIENTED_EDGE('',*,*,#8131,.F.);
#10877=ORIENTED_EDGE('',*,*,#8132,.F.);
#10878=ORIENTED_EDGE('',*,*,#8119,.F.);
#10879=ORIENTED_EDGE('',*,*,#8133,.T.);
#10880=ORIENTED_EDGE('',*,*,#8134,.T.);
#10881=ORIENTED_EDGE('',*,*,#8102,.T.);
#10882=ORIENTED_EDGE('',*,*,#8134,.F.);
#10883=ORIENTED_EDGE('',*,*,#8133,.F.);
#10884=ORIENTED_EDGE('',*,*,#8135,.T.);
#10885=ORIENTED_EDGE('',*,*,#8136,.F.);
#10886=ORIENTED_EDGE('',*,*,#8137,.F.);
#10887=ORIENTED_EDGE('',*,*,#8138,.F.);
#10888=ORIENTED_EDGE('',*,*,#8139,.T.);
#10889=ORIENTED_EDGE('',*,*,#8140,.F.);
#10890=ORIENTED_EDGE('',*,*,#8141,.F.);
#10891=ORIENTED_EDGE('',*,*,#8142,.F.);
#10892=ORIENTED_EDGE('',*,*,#8143,.F.);
#10893=ORIENTED_EDGE('',*,*,#8144,.F.);
#10894=ORIENTED_EDGE('',*,*,#8145,.T.);
#10895=ORIENTED_EDGE('',*,*,#8146,.F.);
#10896=ORIENTED_EDGE('',*,*,#8147,.F.);
#10897=ORIENTED_EDGE('',*,*,#8148,.F.);
#10898=ORIENTED_EDGE('',*,*,#8135,.F.);
#10899=ORIENTED_EDGE('',*,*,#8149,.F.);
#10900=ORIENTED_EDGE('',*,*,#8139,.F.);
#10901=ORIENTED_EDGE('',*,*,#8150,.F.);
#10902=ORIENTED_EDGE('',*,*,#8145,.F.);
#10903=ORIENTED_EDGE('',*,*,#8151,.F.);
#10904=ORIENTED_EDGE('',*,*,#8123,.F.);
#10905=ORIENTED_EDGE('',*,*,#8152,.F.);
#10906=ORIENTED_EDGE('',*,*,#8129,.F.);
#10907=ORIENTED_EDGE('',*,*,#8153,.F.);
#10908=ORIENTED_EDGE('',*,*,#8107,.F.);
#10909=ORIENTED_EDGE('',*,*,#8154,.F.);
#10910=ORIENTED_EDGE('',*,*,#8113,.F.);
#10911=ORIENTED_EDGE('',*,*,#8146,.T.);
#10912=ORIENTED_EDGE('',*,*,#8150,.T.);
#10913=ORIENTED_EDGE('',*,*,#8144,.T.);
#10914=ORIENTED_EDGE('',*,*,#8155,.T.);
#10915=ORIENTED_EDGE('',*,*,#8130,.T.);
#10916=ORIENTED_EDGE('',*,*,#8152,.T.);
#10917=ORIENTED_EDGE('',*,*,#8128,.T.);
#10918=ORIENTED_EDGE('',*,*,#8156,.T.);
#10919=ORIENTED_EDGE('',*,*,#8114,.T.);
#10920=ORIENTED_EDGE('',*,*,#8154,.T.);
#10921=ORIENTED_EDGE('',*,*,#8112,.T.);
#10922=ORIENTED_EDGE('',*,*,#8157,.T.);
#10923=ORIENTED_EDGE('',*,*,#8059,.F.);
#10924=ORIENTED_EDGE('',*,*,#8158,.F.);
#10925=ORIENTED_EDGE('',*,*,#8084,.F.);
#10926=ORIENTED_EDGE('',*,*,#8159,.T.);
#10927=ORIENTED_EDGE('',*,*,#8111,.T.);
#10928=ORIENTED_EDGE('',*,*,#8160,.T.);
#10929=ORIENTED_EDGE('',*,*,#8060,.F.);
#10930=ORIENTED_EDGE('',*,*,#8157,.F.);
#10931=ORIENTED_EDGE('',*,*,#8127,.T.);
#10932=ORIENTED_EDGE('',*,*,#8161,.T.);
#10933=ORIENTED_EDGE('',*,*,#8115,.T.);
#10934=ORIENTED_EDGE('',*,*,#8156,.F.);
#10935=ORIENTED_EDGE('',*,*,#8143,.T.);
#10936=ORIENTED_EDGE('',*,*,#8162,.T.);
#10937=ORIENTED_EDGE('',*,*,#8131,.T.);
#10938=ORIENTED_EDGE('',*,*,#8155,.F.);
#10939=ORIENTED_EDGE('',*,*,#8110,.T.);
#10940=ORIENTED_EDGE('',*,*,#8163,.T.);
#10941=ORIENTED_EDGE('',*,*,#8061,.F.);
#10942=ORIENTED_EDGE('',*,*,#8160,.F.);
#10943=ORIENTED_EDGE('',*,*,#8126,.T.);
#10944=ORIENTED_EDGE('',*,*,#8164,.T.);
#10945=ORIENTED_EDGE('',*,*,#8104,.T.);
#10946=ORIENTED_EDGE('',*,*,#8116,.T.);
#10947=ORIENTED_EDGE('',*,*,#8161,.F.);
#10948=ORIENTED_EDGE('',*,*,#8142,.T.);
#10949=ORIENTED_EDGE('',*,*,#8165,.T.);
#10950=ORIENTED_EDGE('',*,*,#8120,.T.);
#10951=ORIENTED_EDGE('',*,*,#8132,.T.);
#10952=ORIENTED_EDGE('',*,*,#8162,.F.);
#10953=ORIENTED_EDGE('',*,*,#8109,.T.);
#10954=ORIENTED_EDGE('',*,*,#8166,.T.);
#10955=ORIENTED_EDGE('',*,*,#8062,.F.);
#10956=ORIENTED_EDGE('',*,*,#8163,.F.);
#10957=ORIENTED_EDGE('',*,*,#8125,.T.);
#10958=ORIENTED_EDGE('',*,*,#8167,.T.);
#10959=ORIENTED_EDGE('',*,*,#8105,.T.);
#10960=ORIENTED_EDGE('',*,*,#8164,.F.);
#10961=ORIENTED_EDGE('',*,*,#8141,.T.);
#10962=ORIENTED_EDGE('',*,*,#8168,.T.);
#10963=ORIENTED_EDGE('',*,*,#8121,.T.);
#10964=ORIENTED_EDGE('',*,*,#8165,.F.);
#10965=ORIENTED_EDGE('',*,*,#8169,.T.);
#10966=ORIENTED_EDGE('',*,*,#8051,.T.);
#10967=ORIENTED_EDGE('',*,*,#8170,.T.);
#10968=ORIENTED_EDGE('',*,*,#8171,.T.);
#10969=ORIENTED_EDGE('',*,*,#8171,.F.);
#10970=ORIENTED_EDGE('',*,*,#8172,.F.);
#10971=ORIENTED_EDGE('',*,*,#8173,.F.);
#10972=ORIENTED_EDGE('',*,*,#8174,.F.);
#10973=ORIENTED_EDGE('',*,*,#8170,.F.);
#10974=ORIENTED_EDGE('',*,*,#8067,.T.);
#10975=ORIENTED_EDGE('',*,*,#8175,.T.);
#10976=ORIENTED_EDGE('',*,*,#8076,.T.);
#10977=ORIENTED_EDGE('',*,*,#8176,.F.);
#10978=ORIENTED_EDGE('',*,*,#8172,.T.);
#10979=ORIENTED_EDGE('',*,*,#8177,.T.);
#10980=ORIENTED_EDGE('',*,*,#8055,.T.);
#10981=ORIENTED_EDGE('',*,*,#8178,.T.);
#10982=ORIENTED_EDGE('',*,*,#8179,.T.);
#10983=ORIENTED_EDGE('',*,*,#8177,.F.);
#10984=ORIENTED_EDGE('',*,*,#8180,.T.);
#10985=ORIENTED_EDGE('',*,*,#8181,.F.);
#10986=ORIENTED_EDGE('',*,*,#8087,.T.);
#10987=ORIENTED_EDGE('',*,*,#8182,.T.);
#10988=ORIENTED_EDGE('',*,*,#8056,.T.);
#10989=ORIENTED_EDGE('',*,*,#8179,.F.);
#10990=ORIENTED_EDGE('',*,*,#8183,.F.);
#10991=ORIENTED_EDGE('',*,*,#8184,.F.);
#10992=ORIENTED_EDGE('',*,*,#8180,.F.);
#10993=ORIENTED_EDGE('',*,*,#8176,.T.);
#10994=ORIENTED_EDGE('',*,*,#8075,.T.);
#10995=ORIENTED_EDGE('',*,*,#8185,.T.);
#10996=ORIENTED_EDGE('',*,*,#8173,.T.);
#10997=ORIENTED_EDGE('',*,*,#8186,.T.);
#10998=ORIENTED_EDGE('',*,*,#8088,.T.);
#10999=ORIENTED_EDGE('',*,*,#8181,.T.);
#11000=ORIENTED_EDGE('',*,*,#8184,.T.);
#11001=ORIENTED_EDGE('',*,*,#8058,.T.);
#11002=ORIENTED_EDGE('',*,*,#8187,.T.);
#11003=ORIENTED_EDGE('',*,*,#8085,.T.);
#11004=ORIENTED_EDGE('',*,*,#8158,.T.);
#11005=ORIENTED_EDGE('',*,*,#8187,.F.);
#11006=ORIENTED_EDGE('',*,*,#8057,.F.);
#11007=ORIENTED_EDGE('',*,*,#8182,.F.);
#11008=ORIENTED_EDGE('',*,*,#8086,.F.);
#11009=ORIENTED_EDGE('',*,*,#8064,.T.);
#11010=ORIENTED_EDGE('',*,*,#8188,.T.);
#11011=ORIENTED_EDGE('',*,*,#8079,.T.);
#11012=ORIENTED_EDGE('',*,*,#8189,.T.);
#11013=ORIENTED_EDGE('',*,*,#8138,.T.);
#11014=ORIENTED_EDGE('',*,*,#8190,.F.);
#11015=ORIENTED_EDGE('',*,*,#8080,.F.);
#11016=ORIENTED_EDGE('',*,*,#8188,.F.);
#11017=ORIENTED_EDGE('',*,*,#8063,.F.);
#11018=ORIENTED_EDGE('',*,*,#8166,.F.);
#11019=ORIENTED_EDGE('',*,*,#8108,.T.);
#11020=ORIENTED_EDGE('',*,*,#8153,.T.);
#11021=ORIENTED_EDGE('',*,*,#8106,.T.);
#11022=ORIENTED_EDGE('',*,*,#8167,.F.);
#11023=ORIENTED_EDGE('',*,*,#8124,.T.);
#11024=ORIENTED_EDGE('',*,*,#8151,.T.);
#11025=ORIENTED_EDGE('',*,*,#8122,.T.);
#11026=ORIENTED_EDGE('',*,*,#8168,.F.);
#11027=ORIENTED_EDGE('',*,*,#8140,.T.);
#11028=ORIENTED_EDGE('',*,*,#8149,.T.);
#11029=ORIENTED_EDGE('',*,*,#8169,.F.);
#11030=ORIENTED_EDGE('',*,*,#8174,.T.);
#11031=ORIENTED_EDGE('',*,*,#8185,.F.);
#11032=ORIENTED_EDGE('',*,*,#8091,.T.);
#11033=ORIENTED_EDGE('',*,*,#8099,.T.);
#11034=ORIENTED_EDGE('',*,*,#8052,.T.);
#11035=ORIENTED_EDGE('',*,*,#8178,.F.);
#11036=ORIENTED_EDGE('',*,*,#8054,.T.);
#11037=ORIENTED_EDGE('',*,*,#8100,.T.);
#11038=ORIENTED_EDGE('',*,*,#8089,.T.);
#11039=ORIENTED_EDGE('',*,*,#8186,.F.);
#11040=ORIENTED_EDGE('',*,*,#8183,.T.);
#11041=ORIENTED_EDGE('',*,*,#8189,.F.);
#11042=ORIENTED_EDGE('',*,*,#8078,.F.);
#11043=ORIENTED_EDGE('',*,*,#8077,.F.);
#11044=ORIENTED_EDGE('',*,*,#8175,.F.);
#11045=ORIENTED_EDGE('',*,*,#8066,.F.);
#11046=ORIENTED_EDGE('',*,*,#8065,.F.);
#11047=ORIENTED_EDGE('',*,*,#8137,.T.);
#11048=ORIENTED_EDGE('',*,*,#8191,.F.);
#11049=ORIENTED_EDGE('',*,*,#8081,.F.);
#11050=ORIENTED_EDGE('',*,*,#8190,.T.);
#11051=ORIENTED_EDGE('',*,*,#8136,.T.);
#11052=ORIENTED_EDGE('',*,*,#8148,.T.);
#11053=ORIENTED_EDGE('',*,*,#8192,.F.);
#11054=ORIENTED_EDGE('',*,*,#8082,.F.);
#11055=ORIENTED_EDGE('',*,*,#8191,.T.);
#11056=ORIENTED_EDGE('',*,*,#8147,.T.);
#11057=ORIENTED_EDGE('',*,*,#8159,.F.);
#11058=ORIENTED_EDGE('',*,*,#8083,.F.);
#11059=ORIENTED_EDGE('',*,*,#8192,.T.);
#11060=ORIENTED_EDGE('',*,*,#8193,.T.);
#11061=ORIENTED_EDGE('',*,*,#8194,.T.);
#11062=ORIENTED_EDGE('',*,*,#8195,.T.);
#11063=ORIENTED_EDGE('',*,*,#8196,.T.);
#11064=ORIENTED_EDGE('',*,*,#8194,.F.);
#11065=ORIENTED_EDGE('',*,*,#8197,.F.);
#11066=ORIENTED_EDGE('',*,*,#8198,.F.);
#11067=ORIENTED_EDGE('',*,*,#8199,.T.);
#11068=ORIENTED_EDGE('',*,*,#8200,.F.);
#11069=ORIENTED_EDGE('',*,*,#8201,.T.);
#11070=ORIENTED_EDGE('',*,*,#8202,.T.);
#11071=ORIENTED_EDGE('',*,*,#8203,.T.);
#11072=ORIENTED_EDGE('',*,*,#8204,.T.);
#11073=ORIENTED_EDGE('',*,*,#8205,.T.);
#11074=ORIENTED_EDGE('',*,*,#8206,.F.);
#11075=ORIENTED_EDGE('',*,*,#8207,.T.);
#11076=ORIENTED_EDGE('',*,*,#8195,.F.);
#11077=ORIENTED_EDGE('',*,*,#8196,.F.);
#11078=ORIENTED_EDGE('',*,*,#8208,.T.);
#11079=ORIENTED_EDGE('',*,*,#8209,.F.);
#11080=ORIENTED_EDGE('',*,*,#8210,.F.);
#11081=ORIENTED_EDGE('',*,*,#8211,.F.);
#11082=ORIENTED_EDGE('',*,*,#8212,.T.);
#11083=ORIENTED_EDGE('',*,*,#8213,.F.);
#11084=ORIENTED_EDGE('',*,*,#8193,.F.);
#11085=ORIENTED_EDGE('',*,*,#8214,.T.);
#11086=ORIENTED_EDGE('',*,*,#8215,.T.);
#11087=ORIENTED_EDGE('',*,*,#8216,.T.);
#11088=ORIENTED_EDGE('',*,*,#8214,.F.);
#11089=ORIENTED_EDGE('',*,*,#8217,.T.);
#11090=ORIENTED_EDGE('',*,*,#8215,.F.);
#11091=ORIENTED_EDGE('',*,*,#8216,.F.);
#11092=ORIENTED_EDGE('',*,*,#8217,.F.);
#11093=ORIENTED_EDGE('',*,*,#8218,.T.);
#11094=ORIENTED_EDGE('',*,*,#8219,.T.);
#11095=ORIENTED_EDGE('',*,*,#8220,.T.);
#11096=ORIENTED_EDGE('',*,*,#8221,.T.);
#11097=ORIENTED_EDGE('',*,*,#8219,.F.);
#11098=ORIENTED_EDGE('',*,*,#8222,.F.);
#11099=ORIENTED_EDGE('',*,*,#8223,.F.);
#11100=ORIENTED_EDGE('',*,*,#8224,.F.);
#11101=ORIENTED_EDGE('',*,*,#8220,.F.);
#11102=ORIENTED_EDGE('',*,*,#8221,.F.);
#11103=ORIENTED_EDGE('',*,*,#8225,.F.);
#11104=ORIENTED_EDGE('',*,*,#8226,.F.);
#11105=ORIENTED_EDGE('',*,*,#8227,.F.);
#11106=ORIENTED_EDGE('',*,*,#8228,.F.);
#11107=ORIENTED_EDGE('',*,*,#8229,.F.);
#11108=ORIENTED_EDGE('',*,*,#8230,.F.);
#11109=ORIENTED_EDGE('',*,*,#8231,.F.);
#11110=ORIENTED_EDGE('',*,*,#8232,.F.);
#11111=ORIENTED_EDGE('',*,*,#8233,.F.);
#11112=ORIENTED_EDGE('',*,*,#8234,.F.);
#11113=ORIENTED_EDGE('',*,*,#8235,.F.);
#11114=ORIENTED_EDGE('',*,*,#8236,.F.);
#11115=ORIENTED_EDGE('',*,*,#8237,.F.);
#11116=ORIENTED_EDGE('',*,*,#8238,.F.);
#11117=ORIENTED_EDGE('',*,*,#8218,.F.);
#11118=ORIENTED_EDGE('',*,*,#8239,.T.);
#11119=ORIENTED_EDGE('',*,*,#8240,.T.);
#11120=ORIENTED_EDGE('',*,*,#8241,.T.);
#11121=ORIENTED_EDGE('',*,*,#8239,.F.);
#11122=ORIENTED_EDGE('',*,*,#8242,.T.);
#11123=ORIENTED_EDGE('',*,*,#8240,.F.);
#11124=ORIENTED_EDGE('',*,*,#8241,.F.);
#11125=ORIENTED_EDGE('',*,*,#8242,.F.);
#11126=ORIENTED_EDGE('',*,*,#8243,.T.);
#11127=ORIENTED_EDGE('',*,*,#8244,.T.);
#11128=ORIENTED_EDGE('',*,*,#8245,.T.);
#11129=ORIENTED_EDGE('',*,*,#8244,.F.);
#11130=ORIENTED_EDGE('',*,*,#8246,.F.);
#11131=ORIENTED_EDGE('',*,*,#8212,.F.);
#11132=ORIENTED_EDGE('',*,*,#8247,.F.);
#11133=ORIENTED_EDGE('',*,*,#8237,.T.);
#11134=ORIENTED_EDGE('',*,*,#8248,.F.);
#11135=ORIENTED_EDGE('',*,*,#8249,.F.);
#11136=ORIENTED_EDGE('',*,*,#8250,.F.);
#11137=ORIENTED_EDGE('',*,*,#8245,.F.);
#11138=ORIENTED_EDGE('',*,*,#8243,.F.);
#11139=ORIENTED_EDGE('',*,*,#8251,.T.);
#11140=ORIENTED_EDGE('',*,*,#8252,.F.);
#11141=ORIENTED_EDGE('',*,*,#8253,.F.);
#11142=ORIENTED_EDGE('',*,*,#8254,.F.);
#11143=ORIENTED_EDGE('',*,*,#8255,.T.);
#11144=ORIENTED_EDGE('',*,*,#8256,.F.);
#11145=ORIENTED_EDGE('',*,*,#8257,.F.);
#11146=ORIENTED_EDGE('',*,*,#8258,.F.);
#11147=ORIENTED_EDGE('',*,*,#8259,.F.);
#11148=ORIENTED_EDGE('',*,*,#8260,.F.);
#11149=ORIENTED_EDGE('',*,*,#8261,.T.);
#11150=ORIENTED_EDGE('',*,*,#8262,.F.);
#11151=ORIENTED_EDGE('',*,*,#8263,.F.);
#11152=ORIENTED_EDGE('',*,*,#8264,.F.);
#11153=ORIENTED_EDGE('',*,*,#8251,.F.);
#11154=ORIENTED_EDGE('',*,*,#8265,.T.);
#11155=ORIENTED_EDGE('',*,*,#8266,.T.);
#11156=ORIENTED_EDGE('',*,*,#8248,.T.);
#11157=ORIENTED_EDGE('',*,*,#8266,.F.);
#11158=ORIENTED_EDGE('',*,*,#8265,.F.);
#11159=ORIENTED_EDGE('',*,*,#8267,.T.);
#11160=ORIENTED_EDGE('',*,*,#8268,.F.);
#11161=ORIENTED_EDGE('',*,*,#8269,.F.);
#11162=ORIENTED_EDGE('',*,*,#8270,.F.);
#11163=ORIENTED_EDGE('',*,*,#8271,.T.);
#11164=ORIENTED_EDGE('',*,*,#8272,.F.);
#11165=ORIENTED_EDGE('',*,*,#8273,.F.);
#11166=ORIENTED_EDGE('',*,*,#8274,.F.);
#11167=ORIENTED_EDGE('',*,*,#8275,.F.);
#11168=ORIENTED_EDGE('',*,*,#8276,.F.);
#11169=ORIENTED_EDGE('',*,*,#8277,.T.);
#11170=ORIENTED_EDGE('',*,*,#8278,.F.);
#11171=ORIENTED_EDGE('',*,*,#8279,.F.);
#11172=ORIENTED_EDGE('',*,*,#8280,.F.);
#11173=ORIENTED_EDGE('',*,*,#8267,.F.);
#11174=ORIENTED_EDGE('',*,*,#8281,.T.);
#11175=ORIENTED_EDGE('',*,*,#8282,.T.);
#11176=ORIENTED_EDGE('',*,*,#8250,.T.);
#11177=ORIENTED_EDGE('',*,*,#8282,.F.);
#11178=ORIENTED_EDGE('',*,*,#8281,.F.);
#11179=ORIENTED_EDGE('',*,*,#8283,.T.);
#11180=ORIENTED_EDGE('',*,*,#8284,.F.);
#11181=ORIENTED_EDGE('',*,*,#8285,.F.);
#11182=ORIENTED_EDGE('',*,*,#8286,.F.);
#11183=ORIENTED_EDGE('',*,*,#8287,.T.);
#11184=ORIENTED_EDGE('',*,*,#8288,.F.);
#11185=ORIENTED_EDGE('',*,*,#8289,.F.);
#11186=ORIENTED_EDGE('',*,*,#8290,.F.);
#11187=ORIENTED_EDGE('',*,*,#8291,.F.);
#11188=ORIENTED_EDGE('',*,*,#8292,.F.);
#11189=ORIENTED_EDGE('',*,*,#8293,.T.);
#11190=ORIENTED_EDGE('',*,*,#8294,.F.);
#11191=ORIENTED_EDGE('',*,*,#8295,.F.);
#11192=ORIENTED_EDGE('',*,*,#8296,.F.);
#11193=ORIENTED_EDGE('',*,*,#8283,.F.);
#11194=ORIENTED_EDGE('',*,*,#8297,.T.);
#11195=ORIENTED_EDGE('',*,*,#8298,.T.);
#11196=ORIENTED_EDGE('',*,*,#8249,.T.);
#11197=ORIENTED_EDGE('',*,*,#8298,.F.);
#11198=ORIENTED_EDGE('',*,*,#8297,.F.);
#11199=ORIENTED_EDGE('',*,*,#8299,.T.);
#11200=ORIENTED_EDGE('',*,*,#8300,.F.);
#11201=ORIENTED_EDGE('',*,*,#8301,.F.);
#11202=ORIENTED_EDGE('',*,*,#8302,.F.);
#11203=ORIENTED_EDGE('',*,*,#8303,.T.);
#11204=ORIENTED_EDGE('',*,*,#8304,.F.);
#11205=ORIENTED_EDGE('',*,*,#8305,.F.);
#11206=ORIENTED_EDGE('',*,*,#8306,.F.);
#11207=ORIENTED_EDGE('',*,*,#8307,.F.);
#11208=ORIENTED_EDGE('',*,*,#8308,.F.);
#11209=ORIENTED_EDGE('',*,*,#8309,.T.);
#11210=ORIENTED_EDGE('',*,*,#8310,.F.);
#11211=ORIENTED_EDGE('',*,*,#8311,.F.);
#11212=ORIENTED_EDGE('',*,*,#8312,.F.);
#11213=ORIENTED_EDGE('',*,*,#8299,.F.);
#11214=ORIENTED_EDGE('',*,*,#8313,.F.);
#11215=ORIENTED_EDGE('',*,*,#8303,.F.);
#11216=ORIENTED_EDGE('',*,*,#8314,.F.);
#11217=ORIENTED_EDGE('',*,*,#8309,.F.);
#11218=ORIENTED_EDGE('',*,*,#8315,.F.);
#11219=ORIENTED_EDGE('',*,*,#8287,.F.);
#11220=ORIENTED_EDGE('',*,*,#8316,.F.);
#11221=ORIENTED_EDGE('',*,*,#8293,.F.);
#11222=ORIENTED_EDGE('',*,*,#8317,.F.);
#11223=ORIENTED_EDGE('',*,*,#8271,.F.);
#11224=ORIENTED_EDGE('',*,*,#8318,.F.);
#11225=ORIENTED_EDGE('',*,*,#8277,.F.);
#11226=ORIENTED_EDGE('',*,*,#8319,.F.);
#11227=ORIENTED_EDGE('',*,*,#8255,.F.);
#11228=ORIENTED_EDGE('',*,*,#8320,.F.);
#11229=ORIENTED_EDGE('',*,*,#8261,.F.);
#11230=ORIENTED_EDGE('',*,*,#8310,.T.);
#11231=ORIENTED_EDGE('',*,*,#8314,.T.);
#11232=ORIENTED_EDGE('',*,*,#8308,.T.);
#11233=ORIENTED_EDGE('',*,*,#8321,.T.);
#11234=ORIENTED_EDGE('',*,*,#8262,.T.);
#11235=ORIENTED_EDGE('',*,*,#8320,.T.);
#11236=ORIENTED_EDGE('',*,*,#8260,.T.);
#11237=ORIENTED_EDGE('',*,*,#8322,.T.);
#11238=ORIENTED_EDGE('',*,*,#8201,.F.);
#11239=ORIENTED_EDGE('',*,*,#8323,.F.);
#11240=ORIENTED_EDGE('',*,*,#8231,.T.);
#11241=ORIENTED_EDGE('',*,*,#8324,.T.);
#11242=ORIENTED_EDGE('',*,*,#8278,.T.);
#11243=ORIENTED_EDGE('',*,*,#8318,.T.);
#11244=ORIENTED_EDGE('',*,*,#8276,.T.);
#11245=ORIENTED_EDGE('',*,*,#8325,.T.);
#11246=ORIENTED_EDGE('',*,*,#8294,.T.);
#11247=ORIENTED_EDGE('',*,*,#8316,.T.);
#11248=ORIENTED_EDGE('',*,*,#8292,.T.);
#11249=ORIENTED_EDGE('',*,*,#8326,.T.);
#11250=ORIENTED_EDGE('',*,*,#8259,.T.);
#11251=ORIENTED_EDGE('',*,*,#8327,.T.);
#11252=ORIENTED_EDGE('',*,*,#8202,.F.);
#11253=ORIENTED_EDGE('',*,*,#8322,.F.);
#11254=ORIENTED_EDGE('',*,*,#8307,.T.);
#11255=ORIENTED_EDGE('',*,*,#8328,.T.);
#11256=ORIENTED_EDGE('',*,*,#8263,.T.);
#11257=ORIENTED_EDGE('',*,*,#8321,.F.);
#11258=ORIENTED_EDGE('',*,*,#8279,.T.);
#11259=ORIENTED_EDGE('',*,*,#8324,.F.);
#11260=ORIENTED_EDGE('',*,*,#8230,.T.);
#11261=ORIENTED_EDGE('',*,*,#8329,.T.);
#11262=ORIENTED_EDGE('',*,*,#8295,.T.);
#11263=ORIENTED_EDGE('',*,*,#8325,.F.);
#11264=ORIENTED_EDGE('',*,*,#8275,.T.);
#11265=ORIENTED_EDGE('',*,*,#8330,.T.);
#11266=ORIENTED_EDGE('',*,*,#8258,.T.);
#11267=ORIENTED_EDGE('',*,*,#8331,.T.);
#11268=ORIENTED_EDGE('',*,*,#8203,.F.);
#11269=ORIENTED_EDGE('',*,*,#8327,.F.);
#11270=ORIENTED_EDGE('',*,*,#8306,.T.);
#11271=ORIENTED_EDGE('',*,*,#8332,.T.);
#11272=ORIENTED_EDGE('',*,*,#8252,.T.);
#11273=ORIENTED_EDGE('',*,*,#8264,.T.);
#11274=ORIENTED_EDGE('',*,*,#8328,.F.);
#11275=ORIENTED_EDGE('',*,*,#8268,.T.);
#11276=ORIENTED_EDGE('',*,*,#8280,.T.);
#11277=ORIENTED_EDGE('',*,*,#8329,.F.);
#11278=ORIENTED_EDGE('',*,*,#8229,.T.);
#11279=ORIENTED_EDGE('',*,*,#8333,.T.);
#11280=ORIENTED_EDGE('',*,*,#8284,.T.);
#11281=ORIENTED_EDGE('',*,*,#8296,.T.);
#11282=ORIENTED_EDGE('',*,*,#8330,.F.);
#11283=ORIENTED_EDGE('',*,*,#8274,.T.);
#11284=ORIENTED_EDGE('',*,*,#8334,.T.);
#11285=ORIENTED_EDGE('',*,*,#8257,.T.);
#11286=ORIENTED_EDGE('',*,*,#8335,.T.);
#11287=ORIENTED_EDGE('',*,*,#8204,.F.);
#11288=ORIENTED_EDGE('',*,*,#8331,.F.);
#11289=ORIENTED_EDGE('',*,*,#8305,.T.);
#11290=ORIENTED_EDGE('',*,*,#8336,.T.);
#11291=ORIENTED_EDGE('',*,*,#8253,.T.);
#11292=ORIENTED_EDGE('',*,*,#8332,.F.);
#11293=ORIENTED_EDGE('',*,*,#8269,.T.);
#11294=ORIENTED_EDGE('',*,*,#8333,.F.);
#11295=ORIENTED_EDGE('',*,*,#8228,.T.);
#11296=ORIENTED_EDGE('',*,*,#8337,.T.);
#11297=ORIENTED_EDGE('',*,*,#8285,.T.);
#11298=ORIENTED_EDGE('',*,*,#8334,.F.);
#11299=ORIENTED_EDGE('',*,*,#8273,.T.);
#11300=ORIENTED_EDGE('',*,*,#8338,.T.);
#11301=ORIENTED_EDGE('',*,*,#8339,.T.);
#11302=ORIENTED_EDGE('',*,*,#8197,.T.);
#11303=ORIENTED_EDGE('',*,*,#8340,.T.);
#11304=ORIENTED_EDGE('',*,*,#8341,.T.);
#11305=ORIENTED_EDGE('',*,*,#8340,.F.);
#11306=ORIENTED_EDGE('',*,*,#8213,.T.);
#11307=ORIENTED_EDGE('',*,*,#8246,.T.);
#11308=ORIENTED_EDGE('',*,*,#8236,.T.);
#11309=ORIENTED_EDGE('',*,*,#8342,.F.);
#11310=ORIENTED_EDGE('',*,*,#8343,.T.);
#11311=ORIENTED_EDGE('',*,*,#8344,.T.);
#11312=ORIENTED_EDGE('',*,*,#8210,.T.);
#11313=ORIENTED_EDGE('',*,*,#8345,.T.);
#11314=ORIENTED_EDGE('',*,*,#8346,.T.);
#11315=ORIENTED_EDGE('',*,*,#8344,.F.);
#11316=ORIENTED_EDGE('',*,*,#8347,.T.);
#11317=ORIENTED_EDGE('',*,*,#8348,.F.);
#11318=ORIENTED_EDGE('',*,*,#8238,.T.);
#11319=ORIENTED_EDGE('',*,*,#8247,.T.);
#11320=ORIENTED_EDGE('',*,*,#8211,.T.);
#11321=ORIENTED_EDGE('',*,*,#8348,.T.);
#11322=ORIENTED_EDGE('',*,*,#8349,.T.);
#11323=ORIENTED_EDGE('',*,*,#8350,.T.);
#11324=ORIENTED_EDGE('',*,*,#8222,.T.);
#11325=ORIENTED_EDGE('',*,*,#8351,.T.);
#11326=ORIENTED_EDGE('',*,*,#8352,.T.);
#11327=ORIENTED_EDGE('',*,*,#8342,.T.);
#11328=ORIENTED_EDGE('',*,*,#8235,.T.);
#11329=ORIENTED_EDGE('',*,*,#8200,.T.);
#11330=ORIENTED_EDGE('',*,*,#8353,.T.);
#11331=ORIENTED_EDGE('',*,*,#8232,.T.);
#11332=ORIENTED_EDGE('',*,*,#8323,.T.);
#11333=ORIENTED_EDGE('',*,*,#8353,.F.);
#11334=ORIENTED_EDGE('',*,*,#8199,.F.);
#11335=ORIENTED_EDGE('',*,*,#8354,.F.);
#11336=ORIENTED_EDGE('',*,*,#8233,.T.);
#11337=ORIENTED_EDGE('',*,*,#8206,.T.);
#11338=ORIENTED_EDGE('',*,*,#8355,.T.);
#11339=ORIENTED_EDGE('',*,*,#8226,.T.);
#11340=ORIENTED_EDGE('',*,*,#8356,.T.);
#11341=ORIENTED_EDGE('',*,*,#8302,.T.);
#11342=ORIENTED_EDGE('',*,*,#8357,.F.);
#11343=ORIENTED_EDGE('',*,*,#8288,.T.);
#11344=ORIENTED_EDGE('',*,*,#8315,.T.);
#11345=ORIENTED_EDGE('',*,*,#8286,.T.);
#11346=ORIENTED_EDGE('',*,*,#8338,.F.);
#11347=ORIENTED_EDGE('',*,*,#8272,.T.);
#11348=ORIENTED_EDGE('',*,*,#8317,.T.);
#11349=ORIENTED_EDGE('',*,*,#8270,.T.);
#11350=ORIENTED_EDGE('',*,*,#8337,.F.);
#11351=ORIENTED_EDGE('',*,*,#8227,.T.);
#11352=ORIENTED_EDGE('',*,*,#8355,.F.);
#11353=ORIENTED_EDGE('',*,*,#8205,.F.);
#11354=ORIENTED_EDGE('',*,*,#8335,.F.);
#11355=ORIENTED_EDGE('',*,*,#8256,.T.);
#11356=ORIENTED_EDGE('',*,*,#8319,.T.);
#11357=ORIENTED_EDGE('',*,*,#8254,.T.);
#11358=ORIENTED_EDGE('',*,*,#8336,.F.);
#11359=ORIENTED_EDGE('',*,*,#8304,.T.);
#11360=ORIENTED_EDGE('',*,*,#8313,.T.);
#11361=ORIENTED_EDGE('',*,*,#8341,.F.);
#11362=ORIENTED_EDGE('',*,*,#8343,.F.);
#11363=ORIENTED_EDGE('',*,*,#8352,.F.);
#11364=ORIENTED_EDGE('',*,*,#8358,.F.);
#11365=ORIENTED_EDGE('',*,*,#8339,.F.);
#11366=ORIENTED_EDGE('',*,*,#8358,.T.);
#11367=ORIENTED_EDGE('',*,*,#8351,.F.);
#11368=ORIENTED_EDGE('',*,*,#8234,.T.);
#11369=ORIENTED_EDGE('',*,*,#8354,.T.);
#11370=ORIENTED_EDGE('',*,*,#8198,.T.);
#11371=ORIENTED_EDGE('',*,*,#8345,.F.);
#11372=ORIENTED_EDGE('',*,*,#8209,.T.);
#11373=ORIENTED_EDGE('',*,*,#8359,.T.);
#11374=ORIENTED_EDGE('',*,*,#8223,.T.);
#11375=ORIENTED_EDGE('',*,*,#8350,.F.);
#11376=ORIENTED_EDGE('',*,*,#8360,.T.);
#11377=ORIENTED_EDGE('',*,*,#8356,.F.);
#11378=ORIENTED_EDGE('',*,*,#8225,.T.);
#11379=ORIENTED_EDGE('',*,*,#8224,.T.);
#11380=ORIENTED_EDGE('',*,*,#8359,.F.);
#11381=ORIENTED_EDGE('',*,*,#8208,.F.);
#11382=ORIENTED_EDGE('',*,*,#8207,.F.);
#11383=ORIENTED_EDGE('',*,*,#8346,.F.);
#11384=ORIENTED_EDGE('',*,*,#8360,.F.);
#11385=ORIENTED_EDGE('',*,*,#8349,.F.);
#11386=ORIENTED_EDGE('',*,*,#8347,.F.);
#11387=ORIENTED_EDGE('',*,*,#8301,.T.);
#11388=ORIENTED_EDGE('',*,*,#8361,.F.);
#11389=ORIENTED_EDGE('',*,*,#8289,.T.);
#11390=ORIENTED_EDGE('',*,*,#8357,.T.);
#11391=ORIENTED_EDGE('',*,*,#8300,.T.);
#11392=ORIENTED_EDGE('',*,*,#8312,.T.);
#11393=ORIENTED_EDGE('',*,*,#8362,.F.);
#11394=ORIENTED_EDGE('',*,*,#8290,.T.);
#11395=ORIENTED_EDGE('',*,*,#8361,.T.);
#11396=ORIENTED_EDGE('',*,*,#8311,.T.);
#11397=ORIENTED_EDGE('',*,*,#8326,.F.);
#11398=ORIENTED_EDGE('',*,*,#8291,.T.);
#11399=ORIENTED_EDGE('',*,*,#8362,.T.);
#11400=ORIENTED_EDGE('',*,*,#8363,.F.);
#11401=ORIENTED_EDGE('',*,*,#8364,.T.);
#11402=ORIENTED_EDGE('',*,*,#8365,.F.);
#11403=ORIENTED_EDGE('',*,*,#8366,.F.);
#11404=ORIENTED_EDGE('',*,*,#8367,.F.);
#11405=ORIENTED_EDGE('',*,*,#8368,.T.);
#11406=ORIENTED_EDGE('',*,*,#8369,.F.);
#11407=ORIENTED_EDGE('',*,*,#8364,.F.);
#11408=ORIENTED_EDGE('',*,*,#8370,.F.);
#11409=ORIENTED_EDGE('',*,*,#8371,.T.);
#11410=ORIENTED_EDGE('',*,*,#8372,.F.);
#11411=ORIENTED_EDGE('',*,*,#8368,.F.);
#11412=ORIENTED_EDGE('',*,*,#8373,.F.);
#11413=ORIENTED_EDGE('',*,*,#8374,.T.);
#11414=ORIENTED_EDGE('',*,*,#8375,.F.);
#11415=ORIENTED_EDGE('',*,*,#8371,.F.);
#11416=ORIENTED_EDGE('',*,*,#8376,.F.);
#11417=ORIENTED_EDGE('',*,*,#8377,.T.);
#11418=ORIENTED_EDGE('',*,*,#8378,.F.);
#11419=ORIENTED_EDGE('',*,*,#8374,.F.);
#11420=ORIENTED_EDGE('',*,*,#8379,.F.);
#11421=ORIENTED_EDGE('',*,*,#8380,.T.);
#11422=ORIENTED_EDGE('',*,*,#8381,.F.);
#11423=ORIENTED_EDGE('',*,*,#8377,.F.);
#11424=ORIENTED_EDGE('',*,*,#8382,.F.);
#11425=ORIENTED_EDGE('',*,*,#8383,.T.);
#11426=ORIENTED_EDGE('',*,*,#8384,.F.);
#11427=ORIENTED_EDGE('',*,*,#8380,.F.);
#11428=ORIENTED_EDGE('',*,*,#8385,.F.);
#11429=ORIENTED_EDGE('',*,*,#8366,.T.);
#11430=ORIENTED_EDGE('',*,*,#8386,.F.);
#11431=ORIENTED_EDGE('',*,*,#8383,.F.);
#11432=ORIENTED_EDGE('',*,*,#8387,.F.);
#11433=ORIENTED_EDGE('',*,*,#8388,.T.);
#11434=ORIENTED_EDGE('',*,*,#8389,.F.);
#11435=ORIENTED_EDGE('',*,*,#8390,.F.);
#11436=ORIENTED_EDGE('',*,*,#8391,.F.);
#11437=ORIENTED_EDGE('',*,*,#8392,.T.);
#11438=ORIENTED_EDGE('',*,*,#8393,.F.);
#11439=ORIENTED_EDGE('',*,*,#8388,.F.);
#11440=ORIENTED_EDGE('',*,*,#8394,.F.);
#11441=ORIENTED_EDGE('',*,*,#8395,.T.);
#11442=ORIENTED_EDGE('',*,*,#8396,.F.);
#11443=ORIENTED_EDGE('',*,*,#8392,.F.);
#11444=ORIENTED_EDGE('',*,*,#8397,.F.);
#11445=ORIENTED_EDGE('',*,*,#8398,.T.);
#11446=ORIENTED_EDGE('',*,*,#8399,.F.);
#11447=ORIENTED_EDGE('',*,*,#8395,.F.);
#11448=ORIENTED_EDGE('',*,*,#8400,.F.);
#11449=ORIENTED_EDGE('',*,*,#8401,.T.);
#11450=ORIENTED_EDGE('',*,*,#8402,.F.);
#11451=ORIENTED_EDGE('',*,*,#8398,.F.);
#11452=ORIENTED_EDGE('',*,*,#8403,.F.);
#11453=ORIENTED_EDGE('',*,*,#8404,.T.);
#11454=ORIENTED_EDGE('',*,*,#8405,.F.);
#11455=ORIENTED_EDGE('',*,*,#8401,.F.);
#11456=ORIENTED_EDGE('',*,*,#8406,.F.);
#11457=ORIENTED_EDGE('',*,*,#8407,.T.);
#11458=ORIENTED_EDGE('',*,*,#8408,.F.);
#11459=ORIENTED_EDGE('',*,*,#8404,.F.);
#11460=ORIENTED_EDGE('',*,*,#8409,.F.);
#11461=ORIENTED_EDGE('',*,*,#8390,.T.);
#11462=ORIENTED_EDGE('',*,*,#8410,.F.);
#11463=ORIENTED_EDGE('',*,*,#8407,.F.);
#11464=ORIENTED_EDGE('',*,*,#8411,.F.);
#11465=ORIENTED_EDGE('',*,*,#8412,.T.);
#11466=ORIENTED_EDGE('',*,*,#8413,.F.);
#11467=ORIENTED_EDGE('',*,*,#8414,.F.);
#11468=ORIENTED_EDGE('',*,*,#8415,.F.);
#11469=ORIENTED_EDGE('',*,*,#8416,.T.);
#11470=ORIENTED_EDGE('',*,*,#8417,.F.);
#11471=ORIENTED_EDGE('',*,*,#8412,.F.);
#11472=ORIENTED_EDGE('',*,*,#8418,.F.);
#11473=ORIENTED_EDGE('',*,*,#8419,.T.);
#11474=ORIENTED_EDGE('',*,*,#8420,.F.);
#11475=ORIENTED_EDGE('',*,*,#8416,.F.);
#11476=ORIENTED_EDGE('',*,*,#8421,.F.);
#11477=ORIENTED_EDGE('',*,*,#8422,.T.);
#11478=ORIENTED_EDGE('',*,*,#8423,.F.);
#11479=ORIENTED_EDGE('',*,*,#8419,.F.);
#11480=ORIENTED_EDGE('',*,*,#8424,.F.);
#11481=ORIENTED_EDGE('',*,*,#8425,.T.);
#11482=ORIENTED_EDGE('',*,*,#8426,.F.);
#11483=ORIENTED_EDGE('',*,*,#8422,.F.);
#11484=ORIENTED_EDGE('',*,*,#8427,.F.);
#11485=ORIENTED_EDGE('',*,*,#8428,.T.);
#11486=ORIENTED_EDGE('',*,*,#8429,.F.);
#11487=ORIENTED_EDGE('',*,*,#8425,.F.);
#11488=ORIENTED_EDGE('',*,*,#8430,.F.);
#11489=ORIENTED_EDGE('',*,*,#8431,.T.);
#11490=ORIENTED_EDGE('',*,*,#8432,.F.);
#11491=ORIENTED_EDGE('',*,*,#8428,.F.);
#11492=ORIENTED_EDGE('',*,*,#8433,.F.);
#11493=ORIENTED_EDGE('',*,*,#8414,.T.);
#11494=ORIENTED_EDGE('',*,*,#8434,.F.);
#11495=ORIENTED_EDGE('',*,*,#8431,.F.);
#11496=ORIENTED_EDGE('',*,*,#8435,.F.);
#11497=ORIENTED_EDGE('',*,*,#8436,.T.);
#11498=ORIENTED_EDGE('',*,*,#8437,.F.);
#11499=ORIENTED_EDGE('',*,*,#8438,.F.);
#11500=ORIENTED_EDGE('',*,*,#8439,.F.);
#11501=ORIENTED_EDGE('',*,*,#8440,.T.);
#11502=ORIENTED_EDGE('',*,*,#8441,.F.);
#11503=ORIENTED_EDGE('',*,*,#8436,.F.);
#11504=ORIENTED_EDGE('',*,*,#8442,.F.);
#11505=ORIENTED_EDGE('',*,*,#8443,.T.);
#11506=ORIENTED_EDGE('',*,*,#8444,.F.);
#11507=ORIENTED_EDGE('',*,*,#8440,.F.);
#11508=ORIENTED_EDGE('',*,*,#8445,.F.);
#11509=ORIENTED_EDGE('',*,*,#8446,.T.);
#11510=ORIENTED_EDGE('',*,*,#8447,.F.);
#11511=ORIENTED_EDGE('',*,*,#8443,.F.);
#11512=ORIENTED_EDGE('',*,*,#8448,.F.);
#11513=ORIENTED_EDGE('',*,*,#8449,.T.);
#11514=ORIENTED_EDGE('',*,*,#8450,.F.);
#11515=ORIENTED_EDGE('',*,*,#8446,.F.);
#11516=ORIENTED_EDGE('',*,*,#8451,.F.);
#11517=ORIENTED_EDGE('',*,*,#8452,.T.);
#11518=ORIENTED_EDGE('',*,*,#8453,.F.);
#11519=ORIENTED_EDGE('',*,*,#8449,.F.);
#11520=ORIENTED_EDGE('',*,*,#8454,.F.);
#11521=ORIENTED_EDGE('',*,*,#8455,.T.);
#11522=ORIENTED_EDGE('',*,*,#8456,.F.);
#11523=ORIENTED_EDGE('',*,*,#8452,.F.);
#11524=ORIENTED_EDGE('',*,*,#8457,.F.);
#11525=ORIENTED_EDGE('',*,*,#8438,.T.);
#11526=ORIENTED_EDGE('',*,*,#8458,.F.);
#11527=ORIENTED_EDGE('',*,*,#8455,.F.);
#11528=ORIENTED_EDGE('',*,*,#8459,.F.);
#11529=ORIENTED_EDGE('',*,*,#8460,.T.);
#11530=ORIENTED_EDGE('',*,*,#8461,.F.);
#11531=ORIENTED_EDGE('',*,*,#8462,.F.);
#11532=ORIENTED_EDGE('',*,*,#8463,.F.);
#11533=ORIENTED_EDGE('',*,*,#8464,.T.);
#11534=ORIENTED_EDGE('',*,*,#8465,.F.);
#11535=ORIENTED_EDGE('',*,*,#8460,.F.);
#11536=ORIENTED_EDGE('',*,*,#8466,.F.);
#11537=ORIENTED_EDGE('',*,*,#8467,.T.);
#11538=ORIENTED_EDGE('',*,*,#8468,.F.);
#11539=ORIENTED_EDGE('',*,*,#8464,.F.);
#11540=ORIENTED_EDGE('',*,*,#8469,.F.);
#11541=ORIENTED_EDGE('',*,*,#8470,.T.);
#11542=ORIENTED_EDGE('',*,*,#8471,.F.);
#11543=ORIENTED_EDGE('',*,*,#8467,.F.);
#11544=ORIENTED_EDGE('',*,*,#8472,.F.);
#11545=ORIENTED_EDGE('',*,*,#8473,.T.);
#11546=ORIENTED_EDGE('',*,*,#8474,.F.);
#11547=ORIENTED_EDGE('',*,*,#8470,.F.);
#11548=ORIENTED_EDGE('',*,*,#8475,.F.);
#11549=ORIENTED_EDGE('',*,*,#8476,.T.);
#11550=ORIENTED_EDGE('',*,*,#8477,.F.);
#11551=ORIENTED_EDGE('',*,*,#8473,.F.);
#11552=ORIENTED_EDGE('',*,*,#8478,.F.);
#11553=ORIENTED_EDGE('',*,*,#8479,.T.);
#11554=ORIENTED_EDGE('',*,*,#8480,.F.);
#11555=ORIENTED_EDGE('',*,*,#8476,.F.);
#11556=ORIENTED_EDGE('',*,*,#8481,.F.);
#11557=ORIENTED_EDGE('',*,*,#8462,.T.);
#11558=ORIENTED_EDGE('',*,*,#8482,.F.);
#11559=ORIENTED_EDGE('',*,*,#8479,.F.);
#11560=ORIENTED_EDGE('',*,*,#8483,.F.);
#11561=ORIENTED_EDGE('',*,*,#8484,.T.);
#11562=ORIENTED_EDGE('',*,*,#8485,.F.);
#11563=ORIENTED_EDGE('',*,*,#8486,.F.);
#11564=ORIENTED_EDGE('',*,*,#8487,.F.);
#11565=ORIENTED_EDGE('',*,*,#8488,.T.);
#11566=ORIENTED_EDGE('',*,*,#8489,.F.);
#11567=ORIENTED_EDGE('',*,*,#8484,.F.);
#11568=ORIENTED_EDGE('',*,*,#8490,.F.);
#11569=ORIENTED_EDGE('',*,*,#8491,.T.);
#11570=ORIENTED_EDGE('',*,*,#8492,.F.);
#11571=ORIENTED_EDGE('',*,*,#8488,.F.);
#11572=ORIENTED_EDGE('',*,*,#8493,.F.);
#11573=ORIENTED_EDGE('',*,*,#8494,.T.);
#11574=ORIENTED_EDGE('',*,*,#8495,.F.);
#11575=ORIENTED_EDGE('',*,*,#8491,.F.);
#11576=ORIENTED_EDGE('',*,*,#8496,.F.);
#11577=ORIENTED_EDGE('',*,*,#8497,.T.);
#11578=ORIENTED_EDGE('',*,*,#8498,.F.);
#11579=ORIENTED_EDGE('',*,*,#8494,.F.);
#11580=ORIENTED_EDGE('',*,*,#8499,.F.);
#11581=ORIENTED_EDGE('',*,*,#8500,.T.);
#11582=ORIENTED_EDGE('',*,*,#8501,.F.);
#11583=ORIENTED_EDGE('',*,*,#8497,.F.);
#11584=ORIENTED_EDGE('',*,*,#8502,.F.);
#11585=ORIENTED_EDGE('',*,*,#8503,.T.);
#11586=ORIENTED_EDGE('',*,*,#8504,.F.);
#11587=ORIENTED_EDGE('',*,*,#8500,.F.);
#11588=ORIENTED_EDGE('',*,*,#8505,.F.);
#11589=ORIENTED_EDGE('',*,*,#8486,.T.);
#11590=ORIENTED_EDGE('',*,*,#8506,.F.);
#11591=ORIENTED_EDGE('',*,*,#8503,.F.);
#11592=ORIENTED_EDGE('',*,*,#8507,.F.);
#11593=ORIENTED_EDGE('',*,*,#8508,.T.);
#11594=ORIENTED_EDGE('',*,*,#8509,.F.);
#11595=ORIENTED_EDGE('',*,*,#8510,.F.);
#11596=ORIENTED_EDGE('',*,*,#8511,.F.);
#11597=ORIENTED_EDGE('',*,*,#8512,.T.);
#11598=ORIENTED_EDGE('',*,*,#8513,.F.);
#11599=ORIENTED_EDGE('',*,*,#8508,.F.);
#11600=ORIENTED_EDGE('',*,*,#8514,.F.);
#11601=ORIENTED_EDGE('',*,*,#8515,.T.);
#11602=ORIENTED_EDGE('',*,*,#8516,.F.);
#11603=ORIENTED_EDGE('',*,*,#8512,.F.);
#11604=ORIENTED_EDGE('',*,*,#8517,.F.);
#11605=ORIENTED_EDGE('',*,*,#8518,.T.);
#11606=ORIENTED_EDGE('',*,*,#8519,.F.);
#11607=ORIENTED_EDGE('',*,*,#8515,.F.);
#11608=ORIENTED_EDGE('',*,*,#8520,.F.);
#11609=ORIENTED_EDGE('',*,*,#8521,.T.);
#11610=ORIENTED_EDGE('',*,*,#8522,.F.);
#11611=ORIENTED_EDGE('',*,*,#8518,.F.);
#11612=ORIENTED_EDGE('',*,*,#8523,.F.);
#11613=ORIENTED_EDGE('',*,*,#8524,.T.);
#11614=ORIENTED_EDGE('',*,*,#8525,.F.);
#11615=ORIENTED_EDGE('',*,*,#8521,.F.);
#11616=ORIENTED_EDGE('',*,*,#8526,.F.);
#11617=ORIENTED_EDGE('',*,*,#8527,.T.);
#11618=ORIENTED_EDGE('',*,*,#8528,.F.);
#11619=ORIENTED_EDGE('',*,*,#8524,.F.);
#11620=ORIENTED_EDGE('',*,*,#8529,.F.);
#11621=ORIENTED_EDGE('',*,*,#8510,.T.);
#11622=ORIENTED_EDGE('',*,*,#8530,.F.);
#11623=ORIENTED_EDGE('',*,*,#8527,.F.);
#11624=ORIENTED_EDGE('',*,*,#8531,.F.);
#11625=ORIENTED_EDGE('',*,*,#8532,.T.);
#11626=ORIENTED_EDGE('',*,*,#8533,.F.);
#11627=ORIENTED_EDGE('',*,*,#8534,.F.);
#11628=ORIENTED_EDGE('',*,*,#8535,.F.);
#11629=ORIENTED_EDGE('',*,*,#8536,.T.);
#11630=ORIENTED_EDGE('',*,*,#8537,.F.);
#11631=ORIENTED_EDGE('',*,*,#8532,.F.);
#11632=ORIENTED_EDGE('',*,*,#8538,.F.);
#11633=ORIENTED_EDGE('',*,*,#8539,.T.);
#11634=ORIENTED_EDGE('',*,*,#8540,.F.);
#11635=ORIENTED_EDGE('',*,*,#8536,.F.);
#11636=ORIENTED_EDGE('',*,*,#8541,.F.);
#11637=ORIENTED_EDGE('',*,*,#8542,.T.);
#11638=ORIENTED_EDGE('',*,*,#8543,.F.);
#11639=ORIENTED_EDGE('',*,*,#8539,.F.);
#11640=ORIENTED_EDGE('',*,*,#8544,.F.);
#11641=ORIENTED_EDGE('',*,*,#8545,.T.);
#11642=ORIENTED_EDGE('',*,*,#8546,.F.);
#11643=ORIENTED_EDGE('',*,*,#8542,.F.);
#11644=ORIENTED_EDGE('',*,*,#8547,.F.);
#11645=ORIENTED_EDGE('',*,*,#8548,.T.);
#11646=ORIENTED_EDGE('',*,*,#8549,.F.);
#11647=ORIENTED_EDGE('',*,*,#8545,.F.);
#11648=ORIENTED_EDGE('',*,*,#8550,.F.);
#11649=ORIENTED_EDGE('',*,*,#8551,.T.);
#11650=ORIENTED_EDGE('',*,*,#8552,.F.);
#11651=ORIENTED_EDGE('',*,*,#8548,.F.);
#11652=ORIENTED_EDGE('',*,*,#8553,.F.);
#11653=ORIENTED_EDGE('',*,*,#8534,.T.);
#11654=ORIENTED_EDGE('',*,*,#8554,.F.);
#11655=ORIENTED_EDGE('',*,*,#8551,.F.);
#11656=ORIENTED_EDGE('',*,*,#8555,.F.);
#11657=ORIENTED_EDGE('',*,*,#8556,.T.);
#11658=ORIENTED_EDGE('',*,*,#8557,.F.);
#11659=ORIENTED_EDGE('',*,*,#8558,.F.);
#11660=ORIENTED_EDGE('',*,*,#8559,.F.);
#11661=ORIENTED_EDGE('',*,*,#8560,.T.);
#11662=ORIENTED_EDGE('',*,*,#8561,.F.);
#11663=ORIENTED_EDGE('',*,*,#8556,.F.);
#11664=ORIENTED_EDGE('',*,*,#8562,.F.);
#11665=ORIENTED_EDGE('',*,*,#8563,.T.);
#11666=ORIENTED_EDGE('',*,*,#8564,.F.);
#11667=ORIENTED_EDGE('',*,*,#8560,.F.);
#11668=ORIENTED_EDGE('',*,*,#8565,.F.);
#11669=ORIENTED_EDGE('',*,*,#8566,.T.);
#11670=ORIENTED_EDGE('',*,*,#8567,.F.);
#11671=ORIENTED_EDGE('',*,*,#8563,.F.);
#11672=ORIENTED_EDGE('',*,*,#8568,.F.);
#11673=ORIENTED_EDGE('',*,*,#8569,.T.);
#11674=ORIENTED_EDGE('',*,*,#8570,.F.);
#11675=ORIENTED_EDGE('',*,*,#8566,.F.);
#11676=ORIENTED_EDGE('',*,*,#8571,.F.);
#11677=ORIENTED_EDGE('',*,*,#8572,.T.);
#11678=ORIENTED_EDGE('',*,*,#8573,.F.);
#11679=ORIENTED_EDGE('',*,*,#8569,.F.);
#11680=ORIENTED_EDGE('',*,*,#8574,.F.);
#11681=ORIENTED_EDGE('',*,*,#8575,.T.);
#11682=ORIENTED_EDGE('',*,*,#8576,.F.);
#11683=ORIENTED_EDGE('',*,*,#8572,.F.);
#11684=ORIENTED_EDGE('',*,*,#8577,.F.);
#11685=ORIENTED_EDGE('',*,*,#8558,.T.);
#11686=ORIENTED_EDGE('',*,*,#8578,.F.);
#11687=ORIENTED_EDGE('',*,*,#8575,.F.);
#11688=ORIENTED_EDGE('',*,*,#8579,.F.);
#11689=ORIENTED_EDGE('',*,*,#8580,.T.);
#11690=ORIENTED_EDGE('',*,*,#8581,.F.);
#11691=ORIENTED_EDGE('',*,*,#8582,.F.);
#11692=ORIENTED_EDGE('',*,*,#8583,.F.);
#11693=ORIENTED_EDGE('',*,*,#8584,.T.);
#11694=ORIENTED_EDGE('',*,*,#8585,.F.);
#11695=ORIENTED_EDGE('',*,*,#8580,.F.);
#11696=ORIENTED_EDGE('',*,*,#8586,.F.);
#11697=ORIENTED_EDGE('',*,*,#8587,.T.);
#11698=ORIENTED_EDGE('',*,*,#8588,.F.);
#11699=ORIENTED_EDGE('',*,*,#8584,.F.);
#11700=ORIENTED_EDGE('',*,*,#8589,.F.);
#11701=ORIENTED_EDGE('',*,*,#8590,.T.);
#11702=ORIENTED_EDGE('',*,*,#8591,.F.);
#11703=ORIENTED_EDGE('',*,*,#8587,.F.);
#11704=ORIENTED_EDGE('',*,*,#8592,.F.);
#11705=ORIENTED_EDGE('',*,*,#8593,.T.);
#11706=ORIENTED_EDGE('',*,*,#8594,.F.);
#11707=ORIENTED_EDGE('',*,*,#8590,.F.);
#11708=ORIENTED_EDGE('',*,*,#8595,.F.);
#11709=ORIENTED_EDGE('',*,*,#8596,.T.);
#11710=ORIENTED_EDGE('',*,*,#8597,.F.);
#11711=ORIENTED_EDGE('',*,*,#8593,.F.);
#11712=ORIENTED_EDGE('',*,*,#8598,.F.);
#11713=ORIENTED_EDGE('',*,*,#8599,.T.);
#11714=ORIENTED_EDGE('',*,*,#8600,.F.);
#11715=ORIENTED_EDGE('',*,*,#8596,.F.);
#11716=ORIENTED_EDGE('',*,*,#8601,.F.);
#11717=ORIENTED_EDGE('',*,*,#8582,.T.);
#11718=ORIENTED_EDGE('',*,*,#8602,.F.);
#11719=ORIENTED_EDGE('',*,*,#8599,.F.);
#11720=ORIENTED_EDGE('',*,*,#8603,.F.);
#11721=ORIENTED_EDGE('',*,*,#8604,.T.);
#11722=ORIENTED_EDGE('',*,*,#8605,.F.);
#11723=ORIENTED_EDGE('',*,*,#8606,.F.);
#11724=ORIENTED_EDGE('',*,*,#8607,.F.);
#11725=ORIENTED_EDGE('',*,*,#8608,.T.);
#11726=ORIENTED_EDGE('',*,*,#8609,.F.);
#11727=ORIENTED_EDGE('',*,*,#8604,.F.);
#11728=ORIENTED_EDGE('',*,*,#8610,.F.);
#11729=ORIENTED_EDGE('',*,*,#8611,.T.);
#11730=ORIENTED_EDGE('',*,*,#8612,.F.);
#11731=ORIENTED_EDGE('',*,*,#8608,.F.);
#11732=ORIENTED_EDGE('',*,*,#8613,.F.);
#11733=ORIENTED_EDGE('',*,*,#8614,.T.);
#11734=ORIENTED_EDGE('',*,*,#8615,.F.);
#11735=ORIENTED_EDGE('',*,*,#8611,.F.);
#11736=ORIENTED_EDGE('',*,*,#8616,.F.);
#11737=ORIENTED_EDGE('',*,*,#8617,.T.);
#11738=ORIENTED_EDGE('',*,*,#8618,.F.);
#11739=ORIENTED_EDGE('',*,*,#8614,.F.);
#11740=ORIENTED_EDGE('',*,*,#8619,.F.);
#11741=ORIENTED_EDGE('',*,*,#8620,.T.);
#11742=ORIENTED_EDGE('',*,*,#8621,.F.);
#11743=ORIENTED_EDGE('',*,*,#8617,.F.);
#11744=ORIENTED_EDGE('',*,*,#8622,.F.);
#11745=ORIENTED_EDGE('',*,*,#8623,.T.);
#11746=ORIENTED_EDGE('',*,*,#8624,.F.);
#11747=ORIENTED_EDGE('',*,*,#8620,.F.);
#11748=ORIENTED_EDGE('',*,*,#8625,.F.);
#11749=ORIENTED_EDGE('',*,*,#8606,.T.);
#11750=ORIENTED_EDGE('',*,*,#8626,.F.);
#11751=ORIENTED_EDGE('',*,*,#8623,.F.);
#11752=ORIENTED_EDGE('',*,*,#8627,.F.);
#11753=ORIENTED_EDGE('',*,*,#8628,.T.);
#11754=ORIENTED_EDGE('',*,*,#8629,.F.);
#11755=ORIENTED_EDGE('',*,*,#8630,.F.);
#11756=ORIENTED_EDGE('',*,*,#8631,.F.);
#11757=ORIENTED_EDGE('',*,*,#8632,.T.);
#11758=ORIENTED_EDGE('',*,*,#8633,.F.);
#11759=ORIENTED_EDGE('',*,*,#8628,.F.);
#11760=ORIENTED_EDGE('',*,*,#8634,.F.);
#11761=ORIENTED_EDGE('',*,*,#8635,.T.);
#11762=ORIENTED_EDGE('',*,*,#8636,.F.);
#11763=ORIENTED_EDGE('',*,*,#8632,.F.);
#11764=ORIENTED_EDGE('',*,*,#8637,.F.);
#11765=ORIENTED_EDGE('',*,*,#8638,.T.);
#11766=ORIENTED_EDGE('',*,*,#8639,.F.);
#11767=ORIENTED_EDGE('',*,*,#8635,.F.);
#11768=ORIENTED_EDGE('',*,*,#8640,.F.);
#11769=ORIENTED_EDGE('',*,*,#8641,.T.);
#11770=ORIENTED_EDGE('',*,*,#8642,.F.);
#11771=ORIENTED_EDGE('',*,*,#8638,.F.);
#11772=ORIENTED_EDGE('',*,*,#8643,.F.);
#11773=ORIENTED_EDGE('',*,*,#8644,.T.);
#11774=ORIENTED_EDGE('',*,*,#8645,.F.);
#11775=ORIENTED_EDGE('',*,*,#8641,.F.);
#11776=ORIENTED_EDGE('',*,*,#8646,.F.);
#11777=ORIENTED_EDGE('',*,*,#8647,.T.);
#11778=ORIENTED_EDGE('',*,*,#8648,.F.);
#11779=ORIENTED_EDGE('',*,*,#8644,.F.);
#11780=ORIENTED_EDGE('',*,*,#8649,.F.);
#11781=ORIENTED_EDGE('',*,*,#8630,.T.);
#11782=ORIENTED_EDGE('',*,*,#8650,.F.);
#11783=ORIENTED_EDGE('',*,*,#8647,.F.);
#11784=ORIENTED_EDGE('',*,*,#8651,.F.);
#11785=ORIENTED_EDGE('',*,*,#8652,.T.);
#11786=ORIENTED_EDGE('',*,*,#8653,.F.);
#11787=ORIENTED_EDGE('',*,*,#8654,.F.);
#11788=ORIENTED_EDGE('',*,*,#8655,.F.);
#11789=ORIENTED_EDGE('',*,*,#8656,.T.);
#11790=ORIENTED_EDGE('',*,*,#8657,.F.);
#11791=ORIENTED_EDGE('',*,*,#8652,.F.);
#11792=ORIENTED_EDGE('',*,*,#8658,.F.);
#11793=ORIENTED_EDGE('',*,*,#8659,.T.);
#11794=ORIENTED_EDGE('',*,*,#8660,.F.);
#11795=ORIENTED_EDGE('',*,*,#8656,.F.);
#11796=ORIENTED_EDGE('',*,*,#8661,.F.);
#11797=ORIENTED_EDGE('',*,*,#8662,.T.);
#11798=ORIENTED_EDGE('',*,*,#8663,.F.);
#11799=ORIENTED_EDGE('',*,*,#8659,.F.);
#11800=ORIENTED_EDGE('',*,*,#8664,.F.);
#11801=ORIENTED_EDGE('',*,*,#8665,.T.);
#11802=ORIENTED_EDGE('',*,*,#8666,.F.);
#11803=ORIENTED_EDGE('',*,*,#8662,.F.);
#11804=ORIENTED_EDGE('',*,*,#8667,.F.);
#11805=ORIENTED_EDGE('',*,*,#8668,.T.);
#11806=ORIENTED_EDGE('',*,*,#8669,.F.);
#11807=ORIENTED_EDGE('',*,*,#8665,.F.);
#11808=ORIENTED_EDGE('',*,*,#8670,.F.);
#11809=ORIENTED_EDGE('',*,*,#8671,.T.);
#11810=ORIENTED_EDGE('',*,*,#8672,.F.);
#11811=ORIENTED_EDGE('',*,*,#8668,.F.);
#11812=ORIENTED_EDGE('',*,*,#8673,.F.);
#11813=ORIENTED_EDGE('',*,*,#8654,.T.);
#11814=ORIENTED_EDGE('',*,*,#8674,.F.);
#11815=ORIENTED_EDGE('',*,*,#8671,.F.);
#11816=ORIENTED_EDGE('',*,*,#8675,.F.);
#11817=ORIENTED_EDGE('',*,*,#8676,.T.);
#11818=ORIENTED_EDGE('',*,*,#8677,.F.);
#11819=ORIENTED_EDGE('',*,*,#8678,.F.);
#11820=ORIENTED_EDGE('',*,*,#8679,.F.);
#11821=ORIENTED_EDGE('',*,*,#8680,.T.);
#11822=ORIENTED_EDGE('',*,*,#8681,.F.);
#11823=ORIENTED_EDGE('',*,*,#8676,.F.);
#11824=ORIENTED_EDGE('',*,*,#8682,.F.);
#11825=ORIENTED_EDGE('',*,*,#8683,.T.);
#11826=ORIENTED_EDGE('',*,*,#8684,.F.);
#11827=ORIENTED_EDGE('',*,*,#8680,.F.);
#11828=ORIENTED_EDGE('',*,*,#8685,.F.);
#11829=ORIENTED_EDGE('',*,*,#8686,.T.);
#11830=ORIENTED_EDGE('',*,*,#8687,.F.);
#11831=ORIENTED_EDGE('',*,*,#8683,.F.);
#11832=ORIENTED_EDGE('',*,*,#8688,.F.);
#11833=ORIENTED_EDGE('',*,*,#8689,.T.);
#11834=ORIENTED_EDGE('',*,*,#8690,.F.);
#11835=ORIENTED_EDGE('',*,*,#8686,.F.);
#11836=ORIENTED_EDGE('',*,*,#8691,.F.);
#11837=ORIENTED_EDGE('',*,*,#8692,.T.);
#11838=ORIENTED_EDGE('',*,*,#8693,.F.);
#11839=ORIENTED_EDGE('',*,*,#8689,.F.);
#11840=ORIENTED_EDGE('',*,*,#8694,.F.);
#11841=ORIENTED_EDGE('',*,*,#8695,.T.);
#11842=ORIENTED_EDGE('',*,*,#8696,.F.);
#11843=ORIENTED_EDGE('',*,*,#8692,.F.);
#11844=ORIENTED_EDGE('',*,*,#8697,.F.);
#11845=ORIENTED_EDGE('',*,*,#8678,.T.);
#11846=ORIENTED_EDGE('',*,*,#8698,.F.);
#11847=ORIENTED_EDGE('',*,*,#8695,.F.);
#11848=ORIENTED_EDGE('',*,*,#8699,.F.);
#11849=ORIENTED_EDGE('',*,*,#8700,.T.);
#11850=ORIENTED_EDGE('',*,*,#8701,.F.);
#11851=ORIENTED_EDGE('',*,*,#8702,.F.);
#11852=ORIENTED_EDGE('',*,*,#8703,.F.);
#11853=ORIENTED_EDGE('',*,*,#8704,.T.);
#11854=ORIENTED_EDGE('',*,*,#8705,.F.);
#11855=ORIENTED_EDGE('',*,*,#8700,.F.);
#11856=ORIENTED_EDGE('',*,*,#8706,.F.);
#11857=ORIENTED_EDGE('',*,*,#8707,.T.);
#11858=ORIENTED_EDGE('',*,*,#8708,.F.);
#11859=ORIENTED_EDGE('',*,*,#8704,.F.);
#11860=ORIENTED_EDGE('',*,*,#8709,.F.);
#11861=ORIENTED_EDGE('',*,*,#8710,.T.);
#11862=ORIENTED_EDGE('',*,*,#8711,.F.);
#11863=ORIENTED_EDGE('',*,*,#8707,.F.);
#11864=ORIENTED_EDGE('',*,*,#8712,.F.);
#11865=ORIENTED_EDGE('',*,*,#8713,.T.);
#11866=ORIENTED_EDGE('',*,*,#8714,.F.);
#11867=ORIENTED_EDGE('',*,*,#8710,.F.);
#11868=ORIENTED_EDGE('',*,*,#8715,.F.);
#11869=ORIENTED_EDGE('',*,*,#8716,.T.);
#11870=ORIENTED_EDGE('',*,*,#8717,.F.);
#11871=ORIENTED_EDGE('',*,*,#8713,.F.);
#11872=ORIENTED_EDGE('',*,*,#8718,.F.);
#11873=ORIENTED_EDGE('',*,*,#8719,.T.);
#11874=ORIENTED_EDGE('',*,*,#8720,.F.);
#11875=ORIENTED_EDGE('',*,*,#8716,.F.);
#11876=ORIENTED_EDGE('',*,*,#8721,.F.);
#11877=ORIENTED_EDGE('',*,*,#8702,.T.);
#11878=ORIENTED_EDGE('',*,*,#8722,.F.);
#11879=ORIENTED_EDGE('',*,*,#8719,.F.);
#11880=ORIENTED_EDGE('',*,*,#8723,.T.);
#11881=ORIENTED_EDGE('',*,*,#8724,.T.);
#11882=ORIENTED_EDGE('',*,*,#8725,.F.);
#11883=ORIENTED_EDGE('',*,*,#8726,.F.);
#11884=ORIENTED_EDGE('',*,*,#8727,.T.);
#11885=ORIENTED_EDGE('',*,*,#8726,.T.);
#11886=ORIENTED_EDGE('',*,*,#8728,.F.);
#11887=ORIENTED_EDGE('',*,*,#8729,.F.);
#11888=ORIENTED_EDGE('',*,*,#8730,.T.);
#11889=ORIENTED_EDGE('',*,*,#8729,.T.);
#11890=ORIENTED_EDGE('',*,*,#8731,.F.);
#11891=ORIENTED_EDGE('',*,*,#8732,.F.);
#11892=ORIENTED_EDGE('',*,*,#8733,.T.);
#11893=ORIENTED_EDGE('',*,*,#8732,.T.);
#11894=ORIENTED_EDGE('',*,*,#8734,.F.);
#11895=ORIENTED_EDGE('',*,*,#8735,.F.);
#11896=ORIENTED_EDGE('',*,*,#8736,.T.);
#11897=ORIENTED_EDGE('',*,*,#8735,.T.);
#11898=ORIENTED_EDGE('',*,*,#8737,.F.);
#11899=ORIENTED_EDGE('',*,*,#8738,.F.);
#11900=ORIENTED_EDGE('',*,*,#8739,.T.);
#11901=ORIENTED_EDGE('',*,*,#8738,.T.);
#11902=ORIENTED_EDGE('',*,*,#8740,.F.);
#11903=ORIENTED_EDGE('',*,*,#8741,.F.);
#11904=ORIENTED_EDGE('',*,*,#8742,.T.);
#11905=ORIENTED_EDGE('',*,*,#8741,.T.);
#11906=ORIENTED_EDGE('',*,*,#8743,.F.);
#11907=ORIENTED_EDGE('',*,*,#8744,.F.);
#11908=ORIENTED_EDGE('',*,*,#8745,.T.);
#11909=ORIENTED_EDGE('',*,*,#8744,.T.);
#11910=ORIENTED_EDGE('',*,*,#8746,.F.);
#11911=ORIENTED_EDGE('',*,*,#8724,.F.);
#11912=ORIENTED_EDGE('',*,*,#8746,.T.);
#11913=ORIENTED_EDGE('',*,*,#8743,.T.);
#11914=ORIENTED_EDGE('',*,*,#8740,.T.);
#11915=ORIENTED_EDGE('',*,*,#8737,.T.);
#11916=ORIENTED_EDGE('',*,*,#8734,.T.);
#11917=ORIENTED_EDGE('',*,*,#8731,.T.);
#11918=ORIENTED_EDGE('',*,*,#8728,.T.);
#11919=ORIENTED_EDGE('',*,*,#8725,.T.);
#11920=ORIENTED_EDGE('',*,*,#8389,.T.);
#11921=ORIENTED_EDGE('',*,*,#8393,.T.);
#11922=ORIENTED_EDGE('',*,*,#8396,.T.);
#11923=ORIENTED_EDGE('',*,*,#8399,.T.);
#11924=ORIENTED_EDGE('',*,*,#8402,.T.);
#11925=ORIENTED_EDGE('',*,*,#8405,.T.);
#11926=ORIENTED_EDGE('',*,*,#8408,.T.);
#11927=ORIENTED_EDGE('',*,*,#8410,.T.);
#11928=ORIENTED_EDGE('',*,*,#8701,.T.);
#11929=ORIENTED_EDGE('',*,*,#8705,.T.);
#11930=ORIENTED_EDGE('',*,*,#8708,.T.);
#11931=ORIENTED_EDGE('',*,*,#8711,.T.);
#11932=ORIENTED_EDGE('',*,*,#8714,.T.);
#11933=ORIENTED_EDGE('',*,*,#8717,.T.);
#11934=ORIENTED_EDGE('',*,*,#8720,.T.);
#11935=ORIENTED_EDGE('',*,*,#8722,.T.);
#11936=ORIENTED_EDGE('',*,*,#8677,.T.);
#11937=ORIENTED_EDGE('',*,*,#8681,.T.);
#11938=ORIENTED_EDGE('',*,*,#8684,.T.);
#11939=ORIENTED_EDGE('',*,*,#8687,.T.);
#11940=ORIENTED_EDGE('',*,*,#8690,.T.);
#11941=ORIENTED_EDGE('',*,*,#8693,.T.);
#11942=ORIENTED_EDGE('',*,*,#8696,.T.);
#11943=ORIENTED_EDGE('',*,*,#8698,.T.);
#11944=ORIENTED_EDGE('',*,*,#8653,.T.);
#11945=ORIENTED_EDGE('',*,*,#8657,.T.);
#11946=ORIENTED_EDGE('',*,*,#8660,.T.);
#11947=ORIENTED_EDGE('',*,*,#8663,.T.);
#11948=ORIENTED_EDGE('',*,*,#8666,.T.);
#11949=ORIENTED_EDGE('',*,*,#8669,.T.);
#11950=ORIENTED_EDGE('',*,*,#8672,.T.);
#11951=ORIENTED_EDGE('',*,*,#8674,.T.);
#11952=ORIENTED_EDGE('',*,*,#8629,.T.);
#11953=ORIENTED_EDGE('',*,*,#8633,.T.);
#11954=ORIENTED_EDGE('',*,*,#8636,.T.);
#11955=ORIENTED_EDGE('',*,*,#8639,.T.);
#11956=ORIENTED_EDGE('',*,*,#8642,.T.);
#11957=ORIENTED_EDGE('',*,*,#8645,.T.);
#11958=ORIENTED_EDGE('',*,*,#8648,.T.);
#11959=ORIENTED_EDGE('',*,*,#8650,.T.);
#11960=ORIENTED_EDGE('',*,*,#8605,.T.);
#11961=ORIENTED_EDGE('',*,*,#8609,.T.);
#11962=ORIENTED_EDGE('',*,*,#8612,.T.);
#11963=ORIENTED_EDGE('',*,*,#8615,.T.);
#11964=ORIENTED_EDGE('',*,*,#8618,.T.);
#11965=ORIENTED_EDGE('',*,*,#8621,.T.);
#11966=ORIENTED_EDGE('',*,*,#8624,.T.);
#11967=ORIENTED_EDGE('',*,*,#8626,.T.);
#11968=ORIENTED_EDGE('',*,*,#8581,.T.);
#11969=ORIENTED_EDGE('',*,*,#8585,.T.);
#11970=ORIENTED_EDGE('',*,*,#8588,.T.);
#11971=ORIENTED_EDGE('',*,*,#8591,.T.);
#11972=ORIENTED_EDGE('',*,*,#8594,.T.);
#11973=ORIENTED_EDGE('',*,*,#8597,.T.);
#11974=ORIENTED_EDGE('',*,*,#8600,.T.);
#11975=ORIENTED_EDGE('',*,*,#8602,.T.);
#11976=ORIENTED_EDGE('',*,*,#8557,.T.);
#11977=ORIENTED_EDGE('',*,*,#8561,.T.);
#11978=ORIENTED_EDGE('',*,*,#8564,.T.);
#11979=ORIENTED_EDGE('',*,*,#8567,.T.);
#11980=ORIENTED_EDGE('',*,*,#8570,.T.);
#11981=ORIENTED_EDGE('',*,*,#8573,.T.);
#11982=ORIENTED_EDGE('',*,*,#8576,.T.);
#11983=ORIENTED_EDGE('',*,*,#8578,.T.);
#11984=ORIENTED_EDGE('',*,*,#8533,.T.);
#11985=ORIENTED_EDGE('',*,*,#8537,.T.);
#11986=ORIENTED_EDGE('',*,*,#8540,.T.);
#11987=ORIENTED_EDGE('',*,*,#8543,.T.);
#11988=ORIENTED_EDGE('',*,*,#8546,.T.);
#11989=ORIENTED_EDGE('',*,*,#8549,.T.);
#11990=ORIENTED_EDGE('',*,*,#8552,.T.);
#11991=ORIENTED_EDGE('',*,*,#8554,.T.);
#11992=ORIENTED_EDGE('',*,*,#8509,.T.);
#11993=ORIENTED_EDGE('',*,*,#8513,.T.);
#11994=ORIENTED_EDGE('',*,*,#8516,.T.);
#11995=ORIENTED_EDGE('',*,*,#8519,.T.);
#11996=ORIENTED_EDGE('',*,*,#8522,.T.);
#11997=ORIENTED_EDGE('',*,*,#8525,.T.);
#11998=ORIENTED_EDGE('',*,*,#8528,.T.);
#11999=ORIENTED_EDGE('',*,*,#8530,.T.);
#12000=ORIENTED_EDGE('',*,*,#8485,.T.);
#12001=ORIENTED_EDGE('',*,*,#8489,.T.);
#12002=ORIENTED_EDGE('',*,*,#8492,.T.);
#12003=ORIENTED_EDGE('',*,*,#8495,.T.);
#12004=ORIENTED_EDGE('',*,*,#8498,.T.);
#12005=ORIENTED_EDGE('',*,*,#8501,.T.);
#12006=ORIENTED_EDGE('',*,*,#8504,.T.);
#12007=ORIENTED_EDGE('',*,*,#8506,.T.);
#12008=ORIENTED_EDGE('',*,*,#8461,.T.);
#12009=ORIENTED_EDGE('',*,*,#8465,.T.);
#12010=ORIENTED_EDGE('',*,*,#8468,.T.);
#12011=ORIENTED_EDGE('',*,*,#8471,.T.);
#12012=ORIENTED_EDGE('',*,*,#8474,.T.);
#12013=ORIENTED_EDGE('',*,*,#8477,.T.);
#12014=ORIENTED_EDGE('',*,*,#8480,.T.);
#12015=ORIENTED_EDGE('',*,*,#8482,.T.);
#12016=ORIENTED_EDGE('',*,*,#8437,.T.);
#12017=ORIENTED_EDGE('',*,*,#8441,.T.);
#12018=ORIENTED_EDGE('',*,*,#8444,.T.);
#12019=ORIENTED_EDGE('',*,*,#8447,.T.);
#12020=ORIENTED_EDGE('',*,*,#8450,.T.);
#12021=ORIENTED_EDGE('',*,*,#8453,.T.);
#12022=ORIENTED_EDGE('',*,*,#8456,.T.);
#12023=ORIENTED_EDGE('',*,*,#8458,.T.);
#12024=ORIENTED_EDGE('',*,*,#8413,.T.);
#12025=ORIENTED_EDGE('',*,*,#8417,.T.);
#12026=ORIENTED_EDGE('',*,*,#8420,.T.);
#12027=ORIENTED_EDGE('',*,*,#8423,.T.);
#12028=ORIENTED_EDGE('',*,*,#8426,.T.);
#12029=ORIENTED_EDGE('',*,*,#8429,.T.);
#12030=ORIENTED_EDGE('',*,*,#8432,.T.);
#12031=ORIENTED_EDGE('',*,*,#8434,.T.);
#12032=ORIENTED_EDGE('',*,*,#8365,.T.);
#12033=ORIENTED_EDGE('',*,*,#8369,.T.);
#12034=ORIENTED_EDGE('',*,*,#8372,.T.);
#12035=ORIENTED_EDGE('',*,*,#8375,.T.);
#12036=ORIENTED_EDGE('',*,*,#8378,.T.);
#12037=ORIENTED_EDGE('',*,*,#8381,.T.);
#12038=ORIENTED_EDGE('',*,*,#8384,.T.);
#12039=ORIENTED_EDGE('',*,*,#8386,.T.);
#12040=ORIENTED_EDGE('',*,*,#8745,.F.);
#12041=ORIENTED_EDGE('',*,*,#8723,.F.);
#12042=ORIENTED_EDGE('',*,*,#8727,.F.);
#12043=ORIENTED_EDGE('',*,*,#8730,.F.);
#12044=ORIENTED_EDGE('',*,*,#8733,.F.);
#12045=ORIENTED_EDGE('',*,*,#8736,.F.);
#12046=ORIENTED_EDGE('',*,*,#8739,.F.);
#12047=ORIENTED_EDGE('',*,*,#8742,.F.);
#12048=ORIENTED_EDGE('',*,*,#8387,.T.);
#12049=ORIENTED_EDGE('',*,*,#8409,.T.);
#12050=ORIENTED_EDGE('',*,*,#8406,.T.);
#12051=ORIENTED_EDGE('',*,*,#8403,.T.);
#12052=ORIENTED_EDGE('',*,*,#8400,.T.);
#12053=ORIENTED_EDGE('',*,*,#8397,.T.);
#12054=ORIENTED_EDGE('',*,*,#8394,.T.);
#12055=ORIENTED_EDGE('',*,*,#8391,.T.);
#12056=ORIENTED_EDGE('',*,*,#8699,.T.);
#12057=ORIENTED_EDGE('',*,*,#8721,.T.);
#12058=ORIENTED_EDGE('',*,*,#8718,.T.);
#12059=ORIENTED_EDGE('',*,*,#8715,.T.);
#12060=ORIENTED_EDGE('',*,*,#8712,.T.);
#12061=ORIENTED_EDGE('',*,*,#8709,.T.);
#12062=ORIENTED_EDGE('',*,*,#8706,.T.);
#12063=ORIENTED_EDGE('',*,*,#8703,.T.);
#12064=ORIENTED_EDGE('',*,*,#8675,.T.);
#12065=ORIENTED_EDGE('',*,*,#8697,.T.);
#12066=ORIENTED_EDGE('',*,*,#8694,.T.);
#12067=ORIENTED_EDGE('',*,*,#8691,.T.);
#12068=ORIENTED_EDGE('',*,*,#8688,.T.);
#12069=ORIENTED_EDGE('',*,*,#8685,.T.);
#12070=ORIENTED_EDGE('',*,*,#8682,.T.);
#12071=ORIENTED_EDGE('',*,*,#8679,.T.);
#12072=ORIENTED_EDGE('',*,*,#8651,.T.);
#12073=ORIENTED_EDGE('',*,*,#8673,.T.);
#12074=ORIENTED_EDGE('',*,*,#8670,.T.);
#12075=ORIENTED_EDGE('',*,*,#8667,.T.);
#12076=ORIENTED_EDGE('',*,*,#8664,.T.);
#12077=ORIENTED_EDGE('',*,*,#8661,.T.);
#12078=ORIENTED_EDGE('',*,*,#8658,.T.);
#12079=ORIENTED_EDGE('',*,*,#8655,.T.);
#12080=ORIENTED_EDGE('',*,*,#8627,.T.);
#12081=ORIENTED_EDGE('',*,*,#8649,.T.);
#12082=ORIENTED_EDGE('',*,*,#8646,.T.);
#12083=ORIENTED_EDGE('',*,*,#8643,.T.);
#12084=ORIENTED_EDGE('',*,*,#8640,.T.);
#12085=ORIENTED_EDGE('',*,*,#8637,.T.);
#12086=ORIENTED_EDGE('',*,*,#8634,.T.);
#12087=ORIENTED_EDGE('',*,*,#8631,.T.);
#12088=ORIENTED_EDGE('',*,*,#8603,.T.);
#12089=ORIENTED_EDGE('',*,*,#8625,.T.);
#12090=ORIENTED_EDGE('',*,*,#8622,.T.);
#12091=ORIENTED_EDGE('',*,*,#8619,.T.);
#12092=ORIENTED_EDGE('',*,*,#8616,.T.);
#12093=ORIENTED_EDGE('',*,*,#8613,.T.);
#12094=ORIENTED_EDGE('',*,*,#8610,.T.);
#12095=ORIENTED_EDGE('',*,*,#8607,.T.);
#12096=ORIENTED_EDGE('',*,*,#8579,.T.);
#12097=ORIENTED_EDGE('',*,*,#8601,.T.);
#12098=ORIENTED_EDGE('',*,*,#8598,.T.);
#12099=ORIENTED_EDGE('',*,*,#8595,.T.);
#12100=ORIENTED_EDGE('',*,*,#8592,.T.);
#12101=ORIENTED_EDGE('',*,*,#8589,.T.);
#12102=ORIENTED_EDGE('',*,*,#8586,.T.);
#12103=ORIENTED_EDGE('',*,*,#8583,.T.);
#12104=ORIENTED_EDGE('',*,*,#8555,.T.);
#12105=ORIENTED_EDGE('',*,*,#8577,.T.);
#12106=ORIENTED_EDGE('',*,*,#8574,.T.);
#12107=ORIENTED_EDGE('',*,*,#8571,.T.);
#12108=ORIENTED_EDGE('',*,*,#8568,.T.);
#12109=ORIENTED_EDGE('',*,*,#8565,.T.);
#12110=ORIENTED_EDGE('',*,*,#8562,.T.);
#12111=ORIENTED_EDGE('',*,*,#8559,.T.);
#12112=ORIENTED_EDGE('',*,*,#8531,.T.);
#12113=ORIENTED_EDGE('',*,*,#8553,.T.);
#12114=ORIENTED_EDGE('',*,*,#8550,.T.);
#12115=ORIENTED_EDGE('',*,*,#8547,.T.);
#12116=ORIENTED_EDGE('',*,*,#8544,.T.);
#12117=ORIENTED_EDGE('',*,*,#8541,.T.);
#12118=ORIENTED_EDGE('',*,*,#8538,.T.);
#12119=ORIENTED_EDGE('',*,*,#8535,.T.);
#12120=ORIENTED_EDGE('',*,*,#8507,.T.);
#12121=ORIENTED_EDGE('',*,*,#8529,.T.);
#12122=ORIENTED_EDGE('',*,*,#8526,.T.);
#12123=ORIENTED_EDGE('',*,*,#8523,.T.);
#12124=ORIENTED_EDGE('',*,*,#8520,.T.);
#12125=ORIENTED_EDGE('',*,*,#8517,.T.);
#12126=ORIENTED_EDGE('',*,*,#8514,.T.);
#12127=ORIENTED_EDGE('',*,*,#8511,.T.);
#12128=ORIENTED_EDGE('',*,*,#8483,.T.);
#12129=ORIENTED_EDGE('',*,*,#8505,.T.);
#12130=ORIENTED_EDGE('',*,*,#8502,.T.);
#12131=ORIENTED_EDGE('',*,*,#8499,.T.);
#12132=ORIENTED_EDGE('',*,*,#8496,.T.);
#12133=ORIENTED_EDGE('',*,*,#8493,.T.);
#12134=ORIENTED_EDGE('',*,*,#8490,.T.);
#12135=ORIENTED_EDGE('',*,*,#8487,.T.);
#12136=ORIENTED_EDGE('',*,*,#8459,.T.);
#12137=ORIENTED_EDGE('',*,*,#8481,.T.);
#12138=ORIENTED_EDGE('',*,*,#8478,.T.);
#12139=ORIENTED_EDGE('',*,*,#8475,.T.);
#12140=ORIENTED_EDGE('',*,*,#8472,.T.);
#12141=ORIENTED_EDGE('',*,*,#8469,.T.);
#12142=ORIENTED_EDGE('',*,*,#8466,.T.);
#12143=ORIENTED_EDGE('',*,*,#8463,.T.);
#12144=ORIENTED_EDGE('',*,*,#8435,.T.);
#12145=ORIENTED_EDGE('',*,*,#8457,.T.);
#12146=ORIENTED_EDGE('',*,*,#8454,.T.);
#12147=ORIENTED_EDGE('',*,*,#8451,.T.);
#12148=ORIENTED_EDGE('',*,*,#8448,.T.);
#12149=ORIENTED_EDGE('',*,*,#8445,.T.);
#12150=ORIENTED_EDGE('',*,*,#8442,.T.);
#12151=ORIENTED_EDGE('',*,*,#8439,.T.);
#12152=ORIENTED_EDGE('',*,*,#8411,.T.);
#12153=ORIENTED_EDGE('',*,*,#8433,.T.);
#12154=ORIENTED_EDGE('',*,*,#8430,.T.);
#12155=ORIENTED_EDGE('',*,*,#8427,.T.);
#12156=ORIENTED_EDGE('',*,*,#8424,.T.);
#12157=ORIENTED_EDGE('',*,*,#8421,.T.);
#12158=ORIENTED_EDGE('',*,*,#8418,.T.);
#12159=ORIENTED_EDGE('',*,*,#8415,.T.);
#12160=ORIENTED_EDGE('',*,*,#8363,.T.);
#12161=ORIENTED_EDGE('',*,*,#8385,.T.);
#12162=ORIENTED_EDGE('',*,*,#8382,.T.);
#12163=ORIENTED_EDGE('',*,*,#8379,.T.);
#12164=ORIENTED_EDGE('',*,*,#8376,.T.);
#12165=ORIENTED_EDGE('',*,*,#8373,.T.);
#12166=ORIENTED_EDGE('',*,*,#8370,.T.);
#12167=ORIENTED_EDGE('',*,*,#8367,.T.);
#12168=ORIENTED_EDGE('',*,*,#8747,.F.);
#12169=ORIENTED_EDGE('',*,*,#8748,.F.);
#12170=ORIENTED_EDGE('',*,*,#8749,.T.);
#12171=ORIENTED_EDGE('',*,*,#8747,.T.);
#12172=ORIENTED_EDGE('',*,*,#8749,.F.);
#12173=ORIENTED_EDGE('',*,*,#8750,.F.);
#12174=ORIENTED_EDGE('',*,*,#8751,.T.);
#12175=ORIENTED_EDGE('',*,*,#8748,.T.);
#12176=ORIENTED_EDGE('',*,*,#8751,.F.);
#12177=ORIENTED_EDGE('',*,*,#8750,.T.);
#12178=ORIENTED_EDGE('',*,*,#8752,.T.);
#12179=ORIENTED_EDGE('',*,*,#8753,.F.);
#12180=ORIENTED_EDGE('',*,*,#8752,.F.);
#12181=ORIENTED_EDGE('',*,*,#8753,.T.);
#12182=ORIENTED_EDGE('',*,*,#8754,.F.);
#12183=ORIENTED_EDGE('',*,*,#8755,.F.);
#12184=ORIENTED_EDGE('',*,*,#8756,.F.);
#12185=ORIENTED_EDGE('',*,*,#8757,.T.);
#12186=ORIENTED_EDGE('',*,*,#8758,.F.);
#12187=ORIENTED_EDGE('',*,*,#8759,.F.);
#12188=ORIENTED_EDGE('',*,*,#8754,.T.);
#12189=ORIENTED_EDGE('',*,*,#8760,.T.);
#12190=ORIENTED_EDGE('',*,*,#8761,.T.);
#12191=ORIENTED_EDGE('',*,*,#8762,.F.);
#12192=ORIENTED_EDGE('',*,*,#8763,.F.);
#12193=ORIENTED_EDGE('',*,*,#8764,.F.);
#12194=ORIENTED_EDGE('',*,*,#8758,.T.);
#12195=ORIENTED_EDGE('',*,*,#8765,.T.);
#12196=ORIENTED_EDGE('',*,*,#8766,.F.);
#12197=ORIENTED_EDGE('',*,*,#8767,.F.);
#12198=ORIENTED_EDGE('',*,*,#8762,.T.);
#12199=ORIENTED_EDGE('',*,*,#8768,.T.);
#12200=ORIENTED_EDGE('',*,*,#8769,.T.);
#12201=ORIENTED_EDGE('',*,*,#8770,.F.);
#12202=ORIENTED_EDGE('',*,*,#8771,.F.);
#12203=ORIENTED_EDGE('',*,*,#8772,.F.);
#12204=ORIENTED_EDGE('',*,*,#8766,.T.);
#12205=ORIENTED_EDGE('',*,*,#8773,.T.);
#12206=ORIENTED_EDGE('',*,*,#8774,.F.);
#12207=ORIENTED_EDGE('',*,*,#8775,.F.);
#12208=ORIENTED_EDGE('',*,*,#8770,.T.);
#12209=ORIENTED_EDGE('',*,*,#8776,.T.);
#12210=ORIENTED_EDGE('',*,*,#8777,.T.);
#12211=ORIENTED_EDGE('',*,*,#8778,.F.);
#12212=ORIENTED_EDGE('',*,*,#8779,.F.);
#12213=ORIENTED_EDGE('',*,*,#8780,.F.);
#12214=ORIENTED_EDGE('',*,*,#8774,.T.);
#12215=ORIENTED_EDGE('',*,*,#8781,.T.);
#12216=ORIENTED_EDGE('',*,*,#8782,.F.);
#12217=ORIENTED_EDGE('',*,*,#8783,.F.);
#12218=ORIENTED_EDGE('',*,*,#8784,.F.);
#12219=ORIENTED_EDGE('',*,*,#8778,.T.);
#12220=ORIENTED_EDGE('',*,*,#8785,.T.);
#12221=ORIENTED_EDGE('',*,*,#8786,.T.);
#12222=ORIENTED_EDGE('',*,*,#8787,.F.);
#12223=ORIENTED_EDGE('',*,*,#8788,.F.);
#12224=ORIENTED_EDGE('',*,*,#8782,.T.);
#12225=ORIENTED_EDGE('',*,*,#8789,.T.);
#12226=ORIENTED_EDGE('',*,*,#8790,.F.);
#12227=ORIENTED_EDGE('',*,*,#8791,.F.);
#12228=ORIENTED_EDGE('',*,*,#8792,.F.);
#12229=ORIENTED_EDGE('',*,*,#8787,.T.);
#12230=ORIENTED_EDGE('',*,*,#8793,.T.);
#12231=ORIENTED_EDGE('',*,*,#8794,.T.);
#12232=ORIENTED_EDGE('',*,*,#8795,.F.);
#12233=ORIENTED_EDGE('',*,*,#8796,.F.);
#12234=ORIENTED_EDGE('',*,*,#8797,.F.);
#12235=ORIENTED_EDGE('',*,*,#8790,.T.);
#12236=ORIENTED_EDGE('',*,*,#8798,.T.);
#12237=ORIENTED_EDGE('',*,*,#8799,.T.);
#12238=ORIENTED_EDGE('',*,*,#8800,.F.);
#12239=ORIENTED_EDGE('',*,*,#8801,.F.);
#12240=ORIENTED_EDGE('',*,*,#8802,.F.);
#12241=ORIENTED_EDGE('',*,*,#8795,.T.);
#12242=ORIENTED_EDGE('',*,*,#8803,.T.);
#12243=ORIENTED_EDGE('',*,*,#8804,.F.);
#12244=ORIENTED_EDGE('',*,*,#8805,.F.);
#12245=ORIENTED_EDGE('',*,*,#8800,.T.);
#12246=ORIENTED_EDGE('',*,*,#8806,.T.);
#12247=ORIENTED_EDGE('',*,*,#8807,.T.);
#12248=ORIENTED_EDGE('',*,*,#8808,.F.);
#12249=ORIENTED_EDGE('',*,*,#8809,.F.);
#12250=ORIENTED_EDGE('',*,*,#8810,.F.);
#12251=ORIENTED_EDGE('',*,*,#8804,.T.);
#12252=ORIENTED_EDGE('',*,*,#8811,.T.);
#12253=ORIENTED_EDGE('',*,*,#8812,.F.);
#12254=ORIENTED_EDGE('',*,*,#8813,.F.);
#12255=ORIENTED_EDGE('',*,*,#8808,.T.);
#12256=ORIENTED_EDGE('',*,*,#8814,.T.);
#12257=ORIENTED_EDGE('',*,*,#8815,.T.);
#12258=ORIENTED_EDGE('',*,*,#8816,.F.);
#12259=ORIENTED_EDGE('',*,*,#8817,.F.);
#12260=ORIENTED_EDGE('',*,*,#8818,.F.);
#12261=ORIENTED_EDGE('',*,*,#8812,.T.);
#12262=ORIENTED_EDGE('',*,*,#8819,.T.);
#12263=ORIENTED_EDGE('',*,*,#8820,.F.);
#12264=ORIENTED_EDGE('',*,*,#8821,.F.);
#12265=ORIENTED_EDGE('',*,*,#8816,.T.);
#12266=ORIENTED_EDGE('',*,*,#8822,.T.);
#12267=ORIENTED_EDGE('',*,*,#8823,.T.);
#12268=ORIENTED_EDGE('',*,*,#8824,.F.);
#12269=ORIENTED_EDGE('',*,*,#8825,.F.);
#12270=ORIENTED_EDGE('',*,*,#8826,.F.);
#12271=ORIENTED_EDGE('',*,*,#8820,.T.);
#12272=ORIENTED_EDGE('',*,*,#8827,.T.);
#12273=ORIENTED_EDGE('',*,*,#8828,.F.);
#12274=ORIENTED_EDGE('',*,*,#8829,.F.);
#12275=ORIENTED_EDGE('',*,*,#8824,.T.);
#12276=ORIENTED_EDGE('',*,*,#8830,.T.);
#12277=ORIENTED_EDGE('',*,*,#8831,.T.);
#12278=ORIENTED_EDGE('',*,*,#8832,.F.);
#12279=ORIENTED_EDGE('',*,*,#8833,.F.);
#12280=ORIENTED_EDGE('',*,*,#8834,.F.);
#12281=ORIENTED_EDGE('',*,*,#8828,.T.);
#12282=ORIENTED_EDGE('',*,*,#8835,.T.);
#12283=ORIENTED_EDGE('',*,*,#8836,.F.);
#12284=ORIENTED_EDGE('',*,*,#8837,.F.);
#12285=ORIENTED_EDGE('',*,*,#8832,.T.);
#12286=ORIENTED_EDGE('',*,*,#8838,.T.);
#12287=ORIENTED_EDGE('',*,*,#8839,.T.);
#12288=ORIENTED_EDGE('',*,*,#8840,.F.);
#12289=ORIENTED_EDGE('',*,*,#8841,.F.);
#12290=ORIENTED_EDGE('',*,*,#8842,.F.);
#12291=ORIENTED_EDGE('',*,*,#8836,.T.);
#12292=ORIENTED_EDGE('',*,*,#8843,.T.);
#12293=ORIENTED_EDGE('',*,*,#8844,.F.);
#12294=ORIENTED_EDGE('',*,*,#8845,.F.);
#12295=ORIENTED_EDGE('',*,*,#8840,.T.);
#12296=ORIENTED_EDGE('',*,*,#8846,.T.);
#12297=ORIENTED_EDGE('',*,*,#8847,.T.);
#12298=ORIENTED_EDGE('',*,*,#8848,.F.);
#12299=ORIENTED_EDGE('',*,*,#8849,.F.);
#12300=ORIENTED_EDGE('',*,*,#8850,.F.);
#12301=ORIENTED_EDGE('',*,*,#8844,.T.);
#12302=ORIENTED_EDGE('',*,*,#8851,.T.);
#12303=ORIENTED_EDGE('',*,*,#8852,.T.);
#12304=ORIENTED_EDGE('',*,*,#8853,.T.);
#12305=ORIENTED_EDGE('',*,*,#8854,.F.);
#12306=ORIENTED_EDGE('',*,*,#8855,.T.);
#12307=ORIENTED_EDGE('',*,*,#8856,.T.);
#12308=ORIENTED_EDGE('',*,*,#8857,.T.);
#12309=ORIENTED_EDGE('',*,*,#8858,.T.);
#12310=ORIENTED_EDGE('',*,*,#8859,.T.);
#12311=ORIENTED_EDGE('',*,*,#8860,.T.);
#12312=ORIENTED_EDGE('',*,*,#8861,.T.);
#12313=ORIENTED_EDGE('',*,*,#8862,.T.);
#12314=ORIENTED_EDGE('',*,*,#8863,.T.);
#12315=ORIENTED_EDGE('',*,*,#8864,.T.);
#12316=ORIENTED_EDGE('',*,*,#8865,.T.);
#12317=ORIENTED_EDGE('',*,*,#8866,.T.);
#12318=ORIENTED_EDGE('',*,*,#8867,.T.);
#12319=ORIENTED_EDGE('',*,*,#8868,.T.);
#12320=ORIENTED_EDGE('',*,*,#8869,.T.);
#12321=ORIENTED_EDGE('',*,*,#8870,.T.);
#12322=ORIENTED_EDGE('',*,*,#8871,.T.);
#12323=ORIENTED_EDGE('',*,*,#8872,.T.);
#12324=ORIENTED_EDGE('',*,*,#8873,.T.);
#12325=ORIENTED_EDGE('',*,*,#8874,.T.);
#12326=ORIENTED_EDGE('',*,*,#8875,.T.);
#12327=ORIENTED_EDGE('',*,*,#8876,.T.);
#12328=ORIENTED_EDGE('',*,*,#8877,.T.);
#12329=ORIENTED_EDGE('',*,*,#8878,.T.);
#12330=ORIENTED_EDGE('',*,*,#8879,.T.);
#12331=ORIENTED_EDGE('',*,*,#8880,.F.);
#12332=ORIENTED_EDGE('',*,*,#8881,.T.);
#12333=ORIENTED_EDGE('',*,*,#8882,.T.);
#12334=ORIENTED_EDGE('',*,*,#8883,.T.);
#12335=ORIENTED_EDGE('',*,*,#8884,.T.);
#12336=ORIENTED_EDGE('',*,*,#8885,.T.);
#12337=ORIENTED_EDGE('',*,*,#8886,.T.);
#12338=ORIENTED_EDGE('',*,*,#8887,.T.);
#12339=ORIENTED_EDGE('',*,*,#8888,.T.);
#12340=ORIENTED_EDGE('',*,*,#8889,.T.);
#12341=ORIENTED_EDGE('',*,*,#8890,.T.);
#12342=ORIENTED_EDGE('',*,*,#8891,.T.);
#12343=ORIENTED_EDGE('',*,*,#8892,.T.);
#12344=ORIENTED_EDGE('',*,*,#8893,.T.);
#12345=ORIENTED_EDGE('',*,*,#8894,.T.);
#12346=ORIENTED_EDGE('',*,*,#8895,.T.);
#12347=ORIENTED_EDGE('',*,*,#8896,.T.);
#12348=ORIENTED_EDGE('',*,*,#8897,.T.);
#12349=ORIENTED_EDGE('',*,*,#8898,.T.);
#12350=ORIENTED_EDGE('',*,*,#8899,.T.);
#12351=ORIENTED_EDGE('',*,*,#8900,.T.);
#12352=ORIENTED_EDGE('',*,*,#8901,.T.);
#12353=ORIENTED_EDGE('',*,*,#8902,.T.);
#12354=ORIENTED_EDGE('',*,*,#8903,.T.);
#12355=ORIENTED_EDGE('',*,*,#8904,.T.);
#12356=ORIENTED_EDGE('',*,*,#8848,.T.);
#12357=ORIENTED_EDGE('',*,*,#8905,.T.);
#12358=ORIENTED_EDGE('',*,*,#8906,.T.);
#12359=ORIENTED_EDGE('',*,*,#8907,.F.);
#12360=ORIENTED_EDGE('',*,*,#8908,.F.);
#12361=ORIENTED_EDGE('',*,*,#8909,.F.);
#12362=ORIENTED_EDGE('',*,*,#8910,.F.);
#12363=ORIENTED_EDGE('',*,*,#8911,.T.);
#12364=ORIENTED_EDGE('',*,*,#8907,.T.);
#12365=ORIENTED_EDGE('',*,*,#8912,.T.);
#12366=ORIENTED_EDGE('',*,*,#8913,.F.);
#12367=ORIENTED_EDGE('',*,*,#8911,.F.);
#12368=ORIENTED_EDGE('',*,*,#8914,.F.);
#12369=ORIENTED_EDGE('',*,*,#8879,.F.);
#12370=ORIENTED_EDGE('',*,*,#8878,.F.);
#12371=ORIENTED_EDGE('',*,*,#8877,.F.);
#12372=ORIENTED_EDGE('',*,*,#8876,.F.);
#12373=ORIENTED_EDGE('',*,*,#8875,.F.);
#12374=ORIENTED_EDGE('',*,*,#8874,.F.);
#12375=ORIENTED_EDGE('',*,*,#8873,.F.);
#12376=ORIENTED_EDGE('',*,*,#8872,.F.);
#12377=ORIENTED_EDGE('',*,*,#8871,.F.);
#12378=ORIENTED_EDGE('',*,*,#8870,.F.);
#12379=ORIENTED_EDGE('',*,*,#8869,.F.);
#12380=ORIENTED_EDGE('',*,*,#8868,.F.);
#12381=ORIENTED_EDGE('',*,*,#8867,.F.);
#12382=ORIENTED_EDGE('',*,*,#8866,.F.);
#12383=ORIENTED_EDGE('',*,*,#8865,.F.);
#12384=ORIENTED_EDGE('',*,*,#8864,.F.);
#12385=ORIENTED_EDGE('',*,*,#8863,.F.);
#12386=ORIENTED_EDGE('',*,*,#8862,.F.);
#12387=ORIENTED_EDGE('',*,*,#8861,.F.);
#12388=ORIENTED_EDGE('',*,*,#8860,.F.);
#12389=ORIENTED_EDGE('',*,*,#8859,.F.);
#12390=ORIENTED_EDGE('',*,*,#8858,.F.);
#12391=ORIENTED_EDGE('',*,*,#8857,.F.);
#12392=ORIENTED_EDGE('',*,*,#8856,.F.);
#12393=ORIENTED_EDGE('',*,*,#8855,.F.);
#12394=ORIENTED_EDGE('',*,*,#8915,.F.);
#12395=ORIENTED_EDGE('',*,*,#8916,.T.);
#12396=ORIENTED_EDGE('',*,*,#8755,.T.);
#12397=ORIENTED_EDGE('',*,*,#8759,.T.);
#12398=ORIENTED_EDGE('',*,*,#8764,.T.);
#12399=ORIENTED_EDGE('',*,*,#8763,.T.);
#12400=ORIENTED_EDGE('',*,*,#8767,.T.);
#12401=ORIENTED_EDGE('',*,*,#8772,.T.);
#12402=ORIENTED_EDGE('',*,*,#8771,.T.);
#12403=ORIENTED_EDGE('',*,*,#8775,.T.);
#12404=ORIENTED_EDGE('',*,*,#8780,.T.);
#12405=ORIENTED_EDGE('',*,*,#8779,.T.);
#12406=ORIENTED_EDGE('',*,*,#8784,.T.);
#12407=ORIENTED_EDGE('',*,*,#8783,.T.);
#12408=ORIENTED_EDGE('',*,*,#8788,.T.);
#12409=ORIENTED_EDGE('',*,*,#8792,.T.);
#12410=ORIENTED_EDGE('',*,*,#8791,.T.);
#12411=ORIENTED_EDGE('',*,*,#8797,.T.);
#12412=ORIENTED_EDGE('',*,*,#8796,.T.);
#12413=ORIENTED_EDGE('',*,*,#8802,.T.);
#12414=ORIENTED_EDGE('',*,*,#8801,.T.);
#12415=ORIENTED_EDGE('',*,*,#8805,.T.);
#12416=ORIENTED_EDGE('',*,*,#8810,.T.);
#12417=ORIENTED_EDGE('',*,*,#8809,.T.);
#12418=ORIENTED_EDGE('',*,*,#8813,.T.);
#12419=ORIENTED_EDGE('',*,*,#8818,.T.);
#12420=ORIENTED_EDGE('',*,*,#8817,.T.);
#12421=ORIENTED_EDGE('',*,*,#8821,.T.);
#12422=ORIENTED_EDGE('',*,*,#8826,.T.);
#12423=ORIENTED_EDGE('',*,*,#8825,.T.);
#12424=ORIENTED_EDGE('',*,*,#8829,.T.);
#12425=ORIENTED_EDGE('',*,*,#8834,.T.);
#12426=ORIENTED_EDGE('',*,*,#8833,.T.);
#12427=ORIENTED_EDGE('',*,*,#8837,.T.);
#12428=ORIENTED_EDGE('',*,*,#8842,.T.);
#12429=ORIENTED_EDGE('',*,*,#8841,.T.);
#12430=ORIENTED_EDGE('',*,*,#8845,.T.);
#12431=ORIENTED_EDGE('',*,*,#8850,.T.);
#12432=ORIENTED_EDGE('',*,*,#8849,.T.);
#12433=ORIENTED_EDGE('',*,*,#8909,.T.);
#12434=ORIENTED_EDGE('',*,*,#8908,.T.);
#12435=ORIENTED_EDGE('',*,*,#8917,.F.);
#12436=ORIENTED_EDGE('',*,*,#8918,.T.);
#12437=ORIENTED_EDGE('',*,*,#8756,.T.);
#12438=ORIENTED_EDGE('',*,*,#8916,.F.);
#12439=ORIENTED_EDGE('',*,*,#8915,.T.);
#12440=ORIENTED_EDGE('',*,*,#8919,.F.);
#12441=ORIENTED_EDGE('',*,*,#8912,.F.);
#12442=ORIENTED_EDGE('',*,*,#8906,.F.);
#12443=ORIENTED_EDGE('',*,*,#8905,.F.);
#12444=ORIENTED_EDGE('',*,*,#8852,.F.);
#12445=ORIENTED_EDGE('',*,*,#8851,.F.);
#12446=ORIENTED_EDGE('',*,*,#8847,.F.);
#12447=ORIENTED_EDGE('',*,*,#8846,.F.);
#12448=ORIENTED_EDGE('',*,*,#8843,.F.);
#12449=ORIENTED_EDGE('',*,*,#8839,.F.);
#12450=ORIENTED_EDGE('',*,*,#8838,.F.);
#12451=ORIENTED_EDGE('',*,*,#8835,.F.);
#12452=ORIENTED_EDGE('',*,*,#8831,.F.);
#12453=ORIENTED_EDGE('',*,*,#8830,.F.);
#12454=ORIENTED_EDGE('',*,*,#8827,.F.);
#12455=ORIENTED_EDGE('',*,*,#8823,.F.);
#12456=ORIENTED_EDGE('',*,*,#8822,.F.);
#12457=ORIENTED_EDGE('',*,*,#8819,.F.);
#12458=ORIENTED_EDGE('',*,*,#8815,.F.);
#12459=ORIENTED_EDGE('',*,*,#8814,.F.);
#12460=ORIENTED_EDGE('',*,*,#8811,.F.);
#12461=ORIENTED_EDGE('',*,*,#8807,.F.);
#12462=ORIENTED_EDGE('',*,*,#8806,.F.);
#12463=ORIENTED_EDGE('',*,*,#8803,.F.);
#12464=ORIENTED_EDGE('',*,*,#8799,.F.);
#12465=ORIENTED_EDGE('',*,*,#8798,.F.);
#12466=ORIENTED_EDGE('',*,*,#8794,.F.);
#12467=ORIENTED_EDGE('',*,*,#8793,.F.);
#12468=ORIENTED_EDGE('',*,*,#8789,.F.);
#12469=ORIENTED_EDGE('',*,*,#8786,.F.);
#12470=ORIENTED_EDGE('',*,*,#8785,.F.);
#12471=ORIENTED_EDGE('',*,*,#8781,.F.);
#12472=ORIENTED_EDGE('',*,*,#8777,.F.);
#12473=ORIENTED_EDGE('',*,*,#8776,.F.);
#12474=ORIENTED_EDGE('',*,*,#8773,.F.);
#12475=ORIENTED_EDGE('',*,*,#8769,.F.);
#12476=ORIENTED_EDGE('',*,*,#8768,.F.);
#12477=ORIENTED_EDGE('',*,*,#8765,.F.);
#12478=ORIENTED_EDGE('',*,*,#8761,.F.);
#12479=ORIENTED_EDGE('',*,*,#8760,.F.);
#12480=ORIENTED_EDGE('',*,*,#8757,.F.);
#12481=ORIENTED_EDGE('',*,*,#8918,.F.);
#12482=ORIENTED_EDGE('',*,*,#8920,.F.);
#12483=ORIENTED_EDGE('',*,*,#8853,.F.);
#12484=ORIENTED_EDGE('',*,*,#8904,.F.);
#12485=ORIENTED_EDGE('',*,*,#8903,.F.);
#12486=ORIENTED_EDGE('',*,*,#8902,.F.);
#12487=ORIENTED_EDGE('',*,*,#8901,.F.);
#12488=ORIENTED_EDGE('',*,*,#8900,.F.);
#12489=ORIENTED_EDGE('',*,*,#8899,.F.);
#12490=ORIENTED_EDGE('',*,*,#8898,.F.);
#12491=ORIENTED_EDGE('',*,*,#8897,.F.);
#12492=ORIENTED_EDGE('',*,*,#8896,.F.);
#12493=ORIENTED_EDGE('',*,*,#8895,.F.);
#12494=ORIENTED_EDGE('',*,*,#8894,.F.);
#12495=ORIENTED_EDGE('',*,*,#8893,.F.);
#12496=ORIENTED_EDGE('',*,*,#8892,.F.);
#12497=ORIENTED_EDGE('',*,*,#8891,.F.);
#12498=ORIENTED_EDGE('',*,*,#8890,.F.);
#12499=ORIENTED_EDGE('',*,*,#8889,.F.);
#12500=ORIENTED_EDGE('',*,*,#8888,.F.);
#12501=ORIENTED_EDGE('',*,*,#8887,.F.);
#12502=ORIENTED_EDGE('',*,*,#8886,.F.);
#12503=ORIENTED_EDGE('',*,*,#8885,.F.);
#12504=ORIENTED_EDGE('',*,*,#8884,.F.);
#12505=ORIENTED_EDGE('',*,*,#8883,.F.);
#12506=ORIENTED_EDGE('',*,*,#8882,.F.);
#12507=ORIENTED_EDGE('',*,*,#8881,.F.);
#12508=ORIENTED_EDGE('',*,*,#8921,.T.);
#12509=ORIENTED_EDGE('',*,*,#8922,.T.);
#12510=ORIENTED_EDGE('',*,*,#8919,.T.);
#12511=ORIENTED_EDGE('',*,*,#8854,.T.);
#12512=ORIENTED_EDGE('',*,*,#8920,.T.);
#12513=ORIENTED_EDGE('',*,*,#8917,.T.);
#12514=ORIENTED_EDGE('',*,*,#8922,.F.);
#12515=ORIENTED_EDGE('',*,*,#8923,.F.);
#12516=ORIENTED_EDGE('',*,*,#8921,.F.);
#12517=ORIENTED_EDGE('',*,*,#8910,.T.);
#12518=ORIENTED_EDGE('',*,*,#8924,.T.);
#12519=ORIENTED_EDGE('',*,*,#8925,.T.);
#12520=ORIENTED_EDGE('',*,*,#8924,.F.);
#12521=ORIENTED_EDGE('',*,*,#8913,.T.);
#12522=ORIENTED_EDGE('',*,*,#8880,.T.);
#12523=ORIENTED_EDGE('',*,*,#8914,.T.);
#12524=ORIENTED_EDGE('',*,*,#8925,.F.);
#12525=ORIENTED_EDGE('',*,*,#8926,.F.);
#12526=ORIENTED_EDGE('',*,*,#8927,.F.);
#12527=ORIENTED_EDGE('',*,*,#8928,.F.);
#12528=ORIENTED_EDGE('',*,*,#8929,.F.);
#12529=ORIENTED_EDGE('',*,*,#8928,.T.);
#12530=ORIENTED_EDGE('',*,*,#8930,.F.);
#12531=ORIENTED_EDGE('',*,*,#8931,.F.);
#12532=ORIENTED_EDGE('',*,*,#8932,.F.);
#12533=ORIENTED_EDGE('',*,*,#8933,.F.);
#12534=ORIENTED_EDGE('',*,*,#8930,.T.);
#12535=ORIENTED_EDGE('',*,*,#8927,.T.);
#12536=ORIENTED_EDGE('',*,*,#8934,.T.);
#12537=ORIENTED_EDGE('',*,*,#8935,.T.);
#12538=ORIENTED_EDGE('',*,*,#8936,.F.);
#12539=ORIENTED_EDGE('',*,*,#8935,.F.);
#12540=ORIENTED_EDGE('',*,*,#8937,.T.);
#12541=ORIENTED_EDGE('',*,*,#8938,.T.);
#12542=ORIENTED_EDGE('',*,*,#8939,.F.);
#12543=ORIENTED_EDGE('',*,*,#8940,.T.);
#12544=ORIENTED_EDGE('',*,*,#8941,.T.);
#12545=ORIENTED_EDGE('',*,*,#8942,.T.);
#12546=ORIENTED_EDGE('',*,*,#8943,.F.);
#12547=ORIENTED_EDGE('',*,*,#8944,.T.);
#12548=ORIENTED_EDGE('',*,*,#8945,.T.);
#12549=ORIENTED_EDGE('',*,*,#8946,.T.);
#12550=ORIENTED_EDGE('',*,*,#8947,.F.);
#12551=ORIENTED_EDGE('',*,*,#8948,.T.);
#12552=ORIENTED_EDGE('',*,*,#8949,.T.);
#12553=ORIENTED_EDGE('',*,*,#8950,.T.);
#12554=ORIENTED_EDGE('',*,*,#8951,.F.);
#12555=ORIENTED_EDGE('',*,*,#8952,.T.);
#12556=ORIENTED_EDGE('',*,*,#8953,.T.);
#12557=ORIENTED_EDGE('',*,*,#8954,.T.);
#12558=ORIENTED_EDGE('',*,*,#8955,.F.);
#12559=ORIENTED_EDGE('',*,*,#8956,.T.);
#12560=ORIENTED_EDGE('',*,*,#8957,.T.);
#12561=ORIENTED_EDGE('',*,*,#8958,.T.);
#12562=ORIENTED_EDGE('',*,*,#8959,.F.);
#12563=ORIENTED_EDGE('',*,*,#8960,.T.);
#12564=ORIENTED_EDGE('',*,*,#8961,.T.);
#12565=ORIENTED_EDGE('',*,*,#8962,.T.);
#12566=ORIENTED_EDGE('',*,*,#8963,.F.);
#12567=ORIENTED_EDGE('',*,*,#8964,.T.);
#12568=ORIENTED_EDGE('',*,*,#8965,.T.);
#12569=ORIENTED_EDGE('',*,*,#8966,.T.);
#12570=ORIENTED_EDGE('',*,*,#8967,.F.);
#12571=ORIENTED_EDGE('',*,*,#8968,.T.);
#12572=ORIENTED_EDGE('',*,*,#8969,.T.);
#12573=ORIENTED_EDGE('',*,*,#8970,.T.);
#12574=ORIENTED_EDGE('',*,*,#8971,.F.);
#12575=ORIENTED_EDGE('',*,*,#8972,.T.);
#12576=ORIENTED_EDGE('',*,*,#8973,.T.);
#12577=ORIENTED_EDGE('',*,*,#8974,.T.);
#12578=ORIENTED_EDGE('',*,*,#8975,.F.);
#12579=ORIENTED_EDGE('',*,*,#8976,.T.);
#12580=ORIENTED_EDGE('',*,*,#8977,.T.);
#12581=ORIENTED_EDGE('',*,*,#8978,.T.);
#12582=ORIENTED_EDGE('',*,*,#8979,.F.);
#12583=ORIENTED_EDGE('',*,*,#8980,.T.);
#12584=ORIENTED_EDGE('',*,*,#8981,.T.);
#12585=ORIENTED_EDGE('',*,*,#8982,.T.);
#12586=ORIENTED_EDGE('',*,*,#8983,.F.);
#12587=ORIENTED_EDGE('',*,*,#8984,.T.);
#12588=ORIENTED_EDGE('',*,*,#8985,.T.);
#12589=ORIENTED_EDGE('',*,*,#8986,.T.);
#12590=ORIENTED_EDGE('',*,*,#8987,.F.);
#12591=ORIENTED_EDGE('',*,*,#8988,.T.);
#12592=ORIENTED_EDGE('',*,*,#8989,.T.);
#12593=ORIENTED_EDGE('',*,*,#8990,.T.);
#12594=ORIENTED_EDGE('',*,*,#8991,.F.);
#12595=ORIENTED_EDGE('',*,*,#8992,.T.);
#12596=ORIENTED_EDGE('',*,*,#8993,.T.);
#12597=ORIENTED_EDGE('',*,*,#8994,.T.);
#12598=ORIENTED_EDGE('',*,*,#8995,.F.);
#12599=ORIENTED_EDGE('',*,*,#8996,.T.);
#12600=ORIENTED_EDGE('',*,*,#8997,.T.);
#12601=ORIENTED_EDGE('',*,*,#8998,.T.);
#12602=ORIENTED_EDGE('',*,*,#8999,.F.);
#12603=ORIENTED_EDGE('',*,*,#9000,.T.);
#12604=ORIENTED_EDGE('',*,*,#9001,.T.);
#12605=ORIENTED_EDGE('',*,*,#9002,.T.);
#12606=ORIENTED_EDGE('',*,*,#9003,.F.);
#12607=ORIENTED_EDGE('',*,*,#8932,.T.);
#12608=ORIENTED_EDGE('',*,*,#8926,.T.);
#12609=ORIENTED_EDGE('',*,*,#8929,.T.);
#12610=ORIENTED_EDGE('',*,*,#9004,.F.);
#12611=ORIENTED_EDGE('',*,*,#9005,.T.);
#12612=ORIENTED_EDGE('',*,*,#9006,.T.);
#12613=ORIENTED_EDGE('',*,*,#9007,.T.);
#12614=ORIENTED_EDGE('',*,*,#9008,.F.);
#12615=ORIENTED_EDGE('',*,*,#9009,.T.);
#12616=ORIENTED_EDGE('',*,*,#9010,.T.);
#12617=ORIENTED_EDGE('',*,*,#9011,.T.);
#12618=ORIENTED_EDGE('',*,*,#9012,.F.);
#12619=ORIENTED_EDGE('',*,*,#9013,.T.);
#12620=ORIENTED_EDGE('',*,*,#9014,.T.);
#12621=ORIENTED_EDGE('',*,*,#9015,.T.);
#12622=ORIENTED_EDGE('',*,*,#9016,.F.);
#12623=ORIENTED_EDGE('',*,*,#9017,.T.);
#12624=ORIENTED_EDGE('',*,*,#9018,.T.);
#12625=ORIENTED_EDGE('',*,*,#9019,.T.);
#12626=ORIENTED_EDGE('',*,*,#9020,.F.);
#12627=ORIENTED_EDGE('',*,*,#9021,.T.);
#12628=ORIENTED_EDGE('',*,*,#9022,.T.);
#12629=ORIENTED_EDGE('',*,*,#9023,.T.);
#12630=ORIENTED_EDGE('',*,*,#9024,.F.);
#12631=ORIENTED_EDGE('',*,*,#9025,.T.);
#12632=ORIENTED_EDGE('',*,*,#9026,.T.);
#12633=ORIENTED_EDGE('',*,*,#9027,.T.);
#12634=ORIENTED_EDGE('',*,*,#9028,.F.);
#12635=ORIENTED_EDGE('',*,*,#9029,.T.);
#12636=ORIENTED_EDGE('',*,*,#9030,.T.);
#12637=ORIENTED_EDGE('',*,*,#9031,.T.);
#12638=ORIENTED_EDGE('',*,*,#9032,.F.);
#12639=ORIENTED_EDGE('',*,*,#9033,.T.);
#12640=ORIENTED_EDGE('',*,*,#9034,.T.);
#12641=ORIENTED_EDGE('',*,*,#9035,.T.);
#12642=ORIENTED_EDGE('',*,*,#9036,.F.);
#12643=ORIENTED_EDGE('',*,*,#9037,.T.);
#12644=ORIENTED_EDGE('',*,*,#9038,.T.);
#12645=ORIENTED_EDGE('',*,*,#9039,.T.);
#12646=ORIENTED_EDGE('',*,*,#9040,.F.);
#12647=ORIENTED_EDGE('',*,*,#9041,.T.);
#12648=ORIENTED_EDGE('',*,*,#9042,.T.);
#12649=ORIENTED_EDGE('',*,*,#9043,.T.);
#12650=ORIENTED_EDGE('',*,*,#9044,.F.);
#12651=ORIENTED_EDGE('',*,*,#9045,.T.);
#12652=ORIENTED_EDGE('',*,*,#9046,.T.);
#12653=ORIENTED_EDGE('',*,*,#9047,.T.);
#12654=ORIENTED_EDGE('',*,*,#9048,.F.);
#12655=ORIENTED_EDGE('',*,*,#9049,.T.);
#12656=ORIENTED_EDGE('',*,*,#9050,.T.);
#12657=ORIENTED_EDGE('',*,*,#9051,.T.);
#12658=ORIENTED_EDGE('',*,*,#9052,.F.);
#12659=ORIENTED_EDGE('',*,*,#9053,.T.);
#12660=ORIENTED_EDGE('',*,*,#9054,.T.);
#12661=ORIENTED_EDGE('',*,*,#9055,.T.);
#12662=ORIENTED_EDGE('',*,*,#9056,.F.);
#12663=ORIENTED_EDGE('',*,*,#9057,.T.);
#12664=ORIENTED_EDGE('',*,*,#9058,.T.);
#12665=ORIENTED_EDGE('',*,*,#9059,.T.);
#12666=ORIENTED_EDGE('',*,*,#9060,.F.);
#12667=ORIENTED_EDGE('',*,*,#9061,.T.);
#12668=ORIENTED_EDGE('',*,*,#9062,.T.);
#12669=ORIENTED_EDGE('',*,*,#9063,.T.);
#12670=ORIENTED_EDGE('',*,*,#9064,.F.);
#12671=ORIENTED_EDGE('',*,*,#9065,.T.);
#12672=ORIENTED_EDGE('',*,*,#9066,.T.);
#12673=ORIENTED_EDGE('',*,*,#9067,.T.);
#12674=ORIENTED_EDGE('',*,*,#9068,.F.);
#12675=ORIENTED_EDGE('',*,*,#9069,.T.);
#12676=ORIENTED_EDGE('',*,*,#9070,.T.);
#12677=ORIENTED_EDGE('',*,*,#9071,.T.);
#12678=ORIENTED_EDGE('',*,*,#9072,.F.);
#12679=ORIENTED_EDGE('',*,*,#9073,.T.);
#12680=ORIENTED_EDGE('',*,*,#9074,.T.);
#12681=ORIENTED_EDGE('',*,*,#9075,.T.);
#12682=ORIENTED_EDGE('',*,*,#9076,.F.);
#12683=ORIENTED_EDGE('',*,*,#9077,.T.);
#12684=ORIENTED_EDGE('',*,*,#9002,.F.);
#12685=ORIENTED_EDGE('',*,*,#9078,.T.);
#12686=ORIENTED_EDGE('',*,*,#9079,.F.);
#12687=ORIENTED_EDGE('',*,*,#9080,.F.);
#12688=ORIENTED_EDGE('',*,*,#9081,.F.);
#12689=ORIENTED_EDGE('',*,*,#9079,.T.);
#12690=ORIENTED_EDGE('',*,*,#9082,.T.);
#12691=ORIENTED_EDGE('',*,*,#9000,.F.);
#12692=ORIENTED_EDGE('',*,*,#9001,.F.);
#12693=ORIENTED_EDGE('',*,*,#9082,.F.);
#12694=ORIENTED_EDGE('',*,*,#9078,.F.);
#12695=ORIENTED_EDGE('',*,*,#9083,.T.);
#12696=ORIENTED_EDGE('',*,*,#9076,.T.);
#12697=ORIENTED_EDGE('',*,*,#9084,.T.);
#12698=ORIENTED_EDGE('',*,*,#9085,.T.);
#12699=ORIENTED_EDGE('',*,*,#9072,.T.);
#12700=ORIENTED_EDGE('',*,*,#9086,.T.);
#12701=ORIENTED_EDGE('',*,*,#9087,.T.);
#12702=ORIENTED_EDGE('',*,*,#9068,.T.);
#12703=ORIENTED_EDGE('',*,*,#9088,.T.);
#12704=ORIENTED_EDGE('',*,*,#9089,.T.);
#12705=ORIENTED_EDGE('',*,*,#9064,.T.);
#12706=ORIENTED_EDGE('',*,*,#9090,.T.);
#12707=ORIENTED_EDGE('',*,*,#9091,.T.);
#12708=ORIENTED_EDGE('',*,*,#9060,.T.);
#12709=ORIENTED_EDGE('',*,*,#9092,.T.);
#12710=ORIENTED_EDGE('',*,*,#9093,.T.);
#12711=ORIENTED_EDGE('',*,*,#9056,.T.);
#12712=ORIENTED_EDGE('',*,*,#9094,.T.);
#12713=ORIENTED_EDGE('',*,*,#9095,.T.);
#12714=ORIENTED_EDGE('',*,*,#9052,.T.);
#12715=ORIENTED_EDGE('',*,*,#9096,.T.);
#12716=ORIENTED_EDGE('',*,*,#9097,.T.);
#12717=ORIENTED_EDGE('',*,*,#9048,.T.);
#12718=ORIENTED_EDGE('',*,*,#9098,.T.);
#12719=ORIENTED_EDGE('',*,*,#9099,.T.);
#12720=ORIENTED_EDGE('',*,*,#9044,.T.);
#12721=ORIENTED_EDGE('',*,*,#9100,.T.);
#12722=ORIENTED_EDGE('',*,*,#9101,.T.);
#12723=ORIENTED_EDGE('',*,*,#9040,.T.);
#12724=ORIENTED_EDGE('',*,*,#9102,.T.);
#12725=ORIENTED_EDGE('',*,*,#9103,.T.);
#12726=ORIENTED_EDGE('',*,*,#9036,.T.);
#12727=ORIENTED_EDGE('',*,*,#9104,.T.);
#12728=ORIENTED_EDGE('',*,*,#9105,.T.);
#12729=ORIENTED_EDGE('',*,*,#9032,.T.);
#12730=ORIENTED_EDGE('',*,*,#9106,.T.);
#12731=ORIENTED_EDGE('',*,*,#9107,.T.);
#12732=ORIENTED_EDGE('',*,*,#9028,.T.);
#12733=ORIENTED_EDGE('',*,*,#9108,.T.);
#12734=ORIENTED_EDGE('',*,*,#9109,.T.);
#12735=ORIENTED_EDGE('',*,*,#9024,.T.);
#12736=ORIENTED_EDGE('',*,*,#9110,.T.);
#12737=ORIENTED_EDGE('',*,*,#9111,.T.);
#12738=ORIENTED_EDGE('',*,*,#9020,.T.);
#12739=ORIENTED_EDGE('',*,*,#9112,.T.);
#12740=ORIENTED_EDGE('',*,*,#9113,.T.);
#12741=ORIENTED_EDGE('',*,*,#9016,.T.);
#12742=ORIENTED_EDGE('',*,*,#9114,.T.);
#12743=ORIENTED_EDGE('',*,*,#9115,.T.);
#12744=ORIENTED_EDGE('',*,*,#9012,.T.);
#12745=ORIENTED_EDGE('',*,*,#9116,.T.);
#12746=ORIENTED_EDGE('',*,*,#9117,.T.);
#12747=ORIENTED_EDGE('',*,*,#9008,.T.);
#12748=ORIENTED_EDGE('',*,*,#9118,.T.);
#12749=ORIENTED_EDGE('',*,*,#9119,.T.);
#12750=ORIENTED_EDGE('',*,*,#9004,.T.);
#12751=ORIENTED_EDGE('',*,*,#8931,.T.);
#12752=ORIENTED_EDGE('',*,*,#8933,.T.);
#12753=ORIENTED_EDGE('',*,*,#9003,.T.);
#12754=ORIENTED_EDGE('',*,*,#9080,.T.);
#12755=ORIENTED_EDGE('',*,*,#9081,.T.);
#12756=ORIENTED_EDGE('',*,*,#8999,.T.);
#12757=ORIENTED_EDGE('',*,*,#9120,.T.);
#12758=ORIENTED_EDGE('',*,*,#9121,.T.);
#12759=ORIENTED_EDGE('',*,*,#8995,.T.);
#12760=ORIENTED_EDGE('',*,*,#9122,.T.);
#12761=ORIENTED_EDGE('',*,*,#9123,.T.);
#12762=ORIENTED_EDGE('',*,*,#8991,.T.);
#12763=ORIENTED_EDGE('',*,*,#9124,.T.);
#12764=ORIENTED_EDGE('',*,*,#9125,.T.);
#12765=ORIENTED_EDGE('',*,*,#8987,.T.);
#12766=ORIENTED_EDGE('',*,*,#9126,.T.);
#12767=ORIENTED_EDGE('',*,*,#9127,.T.);
#12768=ORIENTED_EDGE('',*,*,#8983,.T.);
#12769=ORIENTED_EDGE('',*,*,#9128,.T.);
#12770=ORIENTED_EDGE('',*,*,#9129,.T.);
#12771=ORIENTED_EDGE('',*,*,#8979,.T.);
#12772=ORIENTED_EDGE('',*,*,#9130,.T.);
#12773=ORIENTED_EDGE('',*,*,#9131,.T.);
#12774=ORIENTED_EDGE('',*,*,#8975,.T.);
#12775=ORIENTED_EDGE('',*,*,#9132,.T.);
#12776=ORIENTED_EDGE('',*,*,#9133,.T.);
#12777=ORIENTED_EDGE('',*,*,#8971,.T.);
#12778=ORIENTED_EDGE('',*,*,#9134,.T.);
#12779=ORIENTED_EDGE('',*,*,#9135,.T.);
#12780=ORIENTED_EDGE('',*,*,#8967,.T.);
#12781=ORIENTED_EDGE('',*,*,#9136,.T.);
#12782=ORIENTED_EDGE('',*,*,#9137,.T.);
#12783=ORIENTED_EDGE('',*,*,#8963,.T.);
#12784=ORIENTED_EDGE('',*,*,#9138,.T.);
#12785=ORIENTED_EDGE('',*,*,#9139,.T.);
#12786=ORIENTED_EDGE('',*,*,#8959,.T.);
#12787=ORIENTED_EDGE('',*,*,#9140,.T.);
#12788=ORIENTED_EDGE('',*,*,#9141,.T.);
#12789=ORIENTED_EDGE('',*,*,#8955,.T.);
#12790=ORIENTED_EDGE('',*,*,#9142,.T.);
#12791=ORIENTED_EDGE('',*,*,#9143,.T.);
#12792=ORIENTED_EDGE('',*,*,#8951,.T.);
#12793=ORIENTED_EDGE('',*,*,#9144,.T.);
#12794=ORIENTED_EDGE('',*,*,#9145,.T.);
#12795=ORIENTED_EDGE('',*,*,#8947,.T.);
#12796=ORIENTED_EDGE('',*,*,#9146,.T.);
#12797=ORIENTED_EDGE('',*,*,#9147,.T.);
#12798=ORIENTED_EDGE('',*,*,#8943,.T.);
#12799=ORIENTED_EDGE('',*,*,#9148,.T.);
#12800=ORIENTED_EDGE('',*,*,#9149,.T.);
#12801=ORIENTED_EDGE('',*,*,#8939,.T.);
#12802=ORIENTED_EDGE('',*,*,#9150,.T.);
#12803=ORIENTED_EDGE('',*,*,#9151,.T.);
#12804=ORIENTED_EDGE('',*,*,#9152,.T.);
#12805=ORIENTED_EDGE('',*,*,#9151,.F.);
#12806=ORIENTED_EDGE('',*,*,#8997,.F.);
#12807=ORIENTED_EDGE('',*,*,#9153,.F.);
#12808=ORIENTED_EDGE('',*,*,#9154,.F.);
#12809=ORIENTED_EDGE('',*,*,#8998,.F.);
#12810=ORIENTED_EDGE('',*,*,#9154,.T.);
#12811=ORIENTED_EDGE('',*,*,#9155,.F.);
#12812=ORIENTED_EDGE('',*,*,#9120,.F.);
#12813=ORIENTED_EDGE('',*,*,#8996,.F.);
#12814=ORIENTED_EDGE('',*,*,#9121,.F.);
#12815=ORIENTED_EDGE('',*,*,#9155,.T.);
#12816=ORIENTED_EDGE('',*,*,#9153,.T.);
#12817=ORIENTED_EDGE('',*,*,#8994,.F.);
#12818=ORIENTED_EDGE('',*,*,#9156,.T.);
#12819=ORIENTED_EDGE('',*,*,#9157,.F.);
#12820=ORIENTED_EDGE('',*,*,#9122,.F.);
#12821=ORIENTED_EDGE('',*,*,#9123,.F.);
#12822=ORIENTED_EDGE('',*,*,#9157,.T.);
#12823=ORIENTED_EDGE('',*,*,#9158,.T.);
#12824=ORIENTED_EDGE('',*,*,#8992,.F.);
#12825=ORIENTED_EDGE('',*,*,#8993,.F.);
#12826=ORIENTED_EDGE('',*,*,#9158,.F.);
#12827=ORIENTED_EDGE('',*,*,#9156,.F.);
#12828=ORIENTED_EDGE('',*,*,#8989,.F.);
#12829=ORIENTED_EDGE('',*,*,#9159,.F.);
#12830=ORIENTED_EDGE('',*,*,#9160,.F.);
#12831=ORIENTED_EDGE('',*,*,#8990,.F.);
#12832=ORIENTED_EDGE('',*,*,#9160,.T.);
#12833=ORIENTED_EDGE('',*,*,#9161,.F.);
#12834=ORIENTED_EDGE('',*,*,#9124,.F.);
#12835=ORIENTED_EDGE('',*,*,#8988,.F.);
#12836=ORIENTED_EDGE('',*,*,#9125,.F.);
#12837=ORIENTED_EDGE('',*,*,#9161,.T.);
#12838=ORIENTED_EDGE('',*,*,#9159,.T.);
#12839=ORIENTED_EDGE('',*,*,#8986,.F.);
#12840=ORIENTED_EDGE('',*,*,#9162,.T.);
#12841=ORIENTED_EDGE('',*,*,#9163,.F.);
#12842=ORIENTED_EDGE('',*,*,#9126,.F.);
#12843=ORIENTED_EDGE('',*,*,#9127,.F.);
#12844=ORIENTED_EDGE('',*,*,#9163,.T.);
#12845=ORIENTED_EDGE('',*,*,#9164,.T.);
#12846=ORIENTED_EDGE('',*,*,#8984,.F.);
#12847=ORIENTED_EDGE('',*,*,#8985,.F.);
#12848=ORIENTED_EDGE('',*,*,#9164,.F.);
#12849=ORIENTED_EDGE('',*,*,#9162,.F.);
#12850=ORIENTED_EDGE('',*,*,#8981,.F.);
#12851=ORIENTED_EDGE('',*,*,#9165,.F.);
#12852=ORIENTED_EDGE('',*,*,#9166,.F.);
#12853=ORIENTED_EDGE('',*,*,#8982,.F.);
#12854=ORIENTED_EDGE('',*,*,#9166,.T.);
#12855=ORIENTED_EDGE('',*,*,#9167,.F.);
#12856=ORIENTED_EDGE('',*,*,#9128,.F.);
#12857=ORIENTED_EDGE('',*,*,#8980,.F.);
#12858=ORIENTED_EDGE('',*,*,#9129,.F.);
#12859=ORIENTED_EDGE('',*,*,#9167,.T.);
#12860=ORIENTED_EDGE('',*,*,#9165,.T.);
#12861=ORIENTED_EDGE('',*,*,#8978,.F.);
#12862=ORIENTED_EDGE('',*,*,#9168,.T.);
#12863=ORIENTED_EDGE('',*,*,#9169,.F.);
#12864=ORIENTED_EDGE('',*,*,#9130,.F.);
#12865=ORIENTED_EDGE('',*,*,#9131,.F.);
#12866=ORIENTED_EDGE('',*,*,#9169,.T.);
#12867=ORIENTED_EDGE('',*,*,#9170,.T.);
#12868=ORIENTED_EDGE('',*,*,#8976,.F.);
#12869=ORIENTED_EDGE('',*,*,#8977,.F.);
#12870=ORIENTED_EDGE('',*,*,#9170,.F.);
#12871=ORIENTED_EDGE('',*,*,#9168,.F.);
#12872=ORIENTED_EDGE('',*,*,#8973,.F.);
#12873=ORIENTED_EDGE('',*,*,#9171,.F.);
#12874=ORIENTED_EDGE('',*,*,#9172,.F.);
#12875=ORIENTED_EDGE('',*,*,#8974,.F.);
#12876=ORIENTED_EDGE('',*,*,#9172,.T.);
#12877=ORIENTED_EDGE('',*,*,#9173,.F.);
#12878=ORIENTED_EDGE('',*,*,#9132,.F.);
#12879=ORIENTED_EDGE('',*,*,#8972,.F.);
#12880=ORIENTED_EDGE('',*,*,#9133,.F.);
#12881=ORIENTED_EDGE('',*,*,#9173,.T.);
#12882=ORIENTED_EDGE('',*,*,#9171,.T.);
#12883=ORIENTED_EDGE('',*,*,#8970,.F.);
#12884=ORIENTED_EDGE('',*,*,#9174,.T.);
#12885=ORIENTED_EDGE('',*,*,#9175,.F.);
#12886=ORIENTED_EDGE('',*,*,#9134,.F.);
#12887=ORIENTED_EDGE('',*,*,#9135,.F.);
#12888=ORIENTED_EDGE('',*,*,#9175,.T.);
#12889=ORIENTED_EDGE('',*,*,#9176,.T.);
#12890=ORIENTED_EDGE('',*,*,#8968,.F.);
#12891=ORIENTED_EDGE('',*,*,#8969,.F.);
#12892=ORIENTED_EDGE('',*,*,#9176,.F.);
#12893=ORIENTED_EDGE('',*,*,#9174,.F.);
#12894=ORIENTED_EDGE('',*,*,#8965,.F.);
#12895=ORIENTED_EDGE('',*,*,#9177,.F.);
#12896=ORIENTED_EDGE('',*,*,#9178,.F.);
#12897=ORIENTED_EDGE('',*,*,#8966,.F.);
#12898=ORIENTED_EDGE('',*,*,#9178,.T.);
#12899=ORIENTED_EDGE('',*,*,#9179,.F.);
#12900=ORIENTED_EDGE('',*,*,#9136,.F.);
#12901=ORIENTED_EDGE('',*,*,#8964,.F.);
#12902=ORIENTED_EDGE('',*,*,#9137,.F.);
#12903=ORIENTED_EDGE('',*,*,#9179,.T.);
#12904=ORIENTED_EDGE('',*,*,#9177,.T.);
#12905=ORIENTED_EDGE('',*,*,#8962,.F.);
#12906=ORIENTED_EDGE('',*,*,#9180,.T.);
#12907=ORIENTED_EDGE('',*,*,#9181,.F.);
#12908=ORIENTED_EDGE('',*,*,#9138,.F.);
#12909=ORIENTED_EDGE('',*,*,#9139,.F.);
#12910=ORIENTED_EDGE('',*,*,#9181,.T.);
#12911=ORIENTED_EDGE('',*,*,#9182,.T.);
#12912=ORIENTED_EDGE('',*,*,#8960,.F.);
#12913=ORIENTED_EDGE('',*,*,#8961,.F.);
#12914=ORIENTED_EDGE('',*,*,#9182,.F.);
#12915=ORIENTED_EDGE('',*,*,#9180,.F.);
#12916=ORIENTED_EDGE('',*,*,#8957,.F.);
#12917=ORIENTED_EDGE('',*,*,#9183,.F.);
#12918=ORIENTED_EDGE('',*,*,#9184,.F.);
#12919=ORIENTED_EDGE('',*,*,#8958,.F.);
#12920=ORIENTED_EDGE('',*,*,#9184,.T.);
#12921=ORIENTED_EDGE('',*,*,#9185,.F.);
#12922=ORIENTED_EDGE('',*,*,#9140,.F.);
#12923=ORIENTED_EDGE('',*,*,#8956,.F.);
#12924=ORIENTED_EDGE('',*,*,#9141,.F.);
#12925=ORIENTED_EDGE('',*,*,#9185,.T.);
#12926=ORIENTED_EDGE('',*,*,#9183,.T.);
#12927=ORIENTED_EDGE('',*,*,#8954,.F.);
#12928=ORIENTED_EDGE('',*,*,#9186,.T.);
#12929=ORIENTED_EDGE('',*,*,#9187,.F.);
#12930=ORIENTED_EDGE('',*,*,#9142,.F.);
#12931=ORIENTED_EDGE('',*,*,#9143,.F.);
#12932=ORIENTED_EDGE('',*,*,#9187,.T.);
#12933=ORIENTED_EDGE('',*,*,#9188,.T.);
#12934=ORIENTED_EDGE('',*,*,#8952,.F.);
#12935=ORIENTED_EDGE('',*,*,#8953,.F.);
#12936=ORIENTED_EDGE('',*,*,#9188,.F.);
#12937=ORIENTED_EDGE('',*,*,#9186,.F.);
#12938=ORIENTED_EDGE('',*,*,#8949,.F.);
#12939=ORIENTED_EDGE('',*,*,#9189,.F.);
#12940=ORIENTED_EDGE('',*,*,#9190,.F.);
#12941=ORIENTED_EDGE('',*,*,#8950,.F.);
#12942=ORIENTED_EDGE('',*,*,#9190,.T.);
#12943=ORIENTED_EDGE('',*,*,#9191,.F.);
#12944=ORIENTED_EDGE('',*,*,#9144,.F.);
#12945=ORIENTED_EDGE('',*,*,#8948,.F.);
#12946=ORIENTED_EDGE('',*,*,#9145,.F.);
#12947=ORIENTED_EDGE('',*,*,#9191,.T.);
#12948=ORIENTED_EDGE('',*,*,#9189,.T.);
#12949=ORIENTED_EDGE('',*,*,#8946,.F.);
#12950=ORIENTED_EDGE('',*,*,#9192,.T.);
#12951=ORIENTED_EDGE('',*,*,#9193,.F.);
#12952=ORIENTED_EDGE('',*,*,#9146,.F.);
#12953=ORIENTED_EDGE('',*,*,#9147,.F.);
#12954=ORIENTED_EDGE('',*,*,#9193,.T.);
#12955=ORIENTED_EDGE('',*,*,#9194,.T.);
#12956=ORIENTED_EDGE('',*,*,#8944,.F.);
#12957=ORIENTED_EDGE('',*,*,#8945,.F.);
#12958=ORIENTED_EDGE('',*,*,#9194,.F.);
#12959=ORIENTED_EDGE('',*,*,#9192,.F.);
#12960=ORIENTED_EDGE('',*,*,#8941,.F.);
#12961=ORIENTED_EDGE('',*,*,#9195,.F.);
#12962=ORIENTED_EDGE('',*,*,#9196,.F.);
#12963=ORIENTED_EDGE('',*,*,#8942,.F.);
#12964=ORIENTED_EDGE('',*,*,#9196,.T.);
#12965=ORIENTED_EDGE('',*,*,#9197,.F.);
#12966=ORIENTED_EDGE('',*,*,#9148,.F.);
#12967=ORIENTED_EDGE('',*,*,#8940,.F.);
#12968=ORIENTED_EDGE('',*,*,#9149,.F.);
#12969=ORIENTED_EDGE('',*,*,#9197,.T.);
#12970=ORIENTED_EDGE('',*,*,#9195,.T.);
#12971=ORIENTED_EDGE('',*,*,#8938,.F.);
#12972=ORIENTED_EDGE('',*,*,#9198,.T.);
#12973=ORIENTED_EDGE('',*,*,#9199,.F.);
#12974=ORIENTED_EDGE('',*,*,#9150,.F.);
#12975=ORIENTED_EDGE('',*,*,#9083,.F.);
#12976=ORIENTED_EDGE('',*,*,#9199,.T.);
#12977=ORIENTED_EDGE('',*,*,#9200,.T.);
#12978=ORIENTED_EDGE('',*,*,#9077,.F.);
#12979=ORIENTED_EDGE('',*,*,#8934,.F.);
#12980=ORIENTED_EDGE('',*,*,#9200,.F.);
#12981=ORIENTED_EDGE('',*,*,#9198,.F.);
#12982=ORIENTED_EDGE('',*,*,#8937,.F.);
#12983=ORIENTED_EDGE('',*,*,#9074,.F.);
#12984=ORIENTED_EDGE('',*,*,#9201,.F.);
#12985=ORIENTED_EDGE('',*,*,#9202,.F.);
#12986=ORIENTED_EDGE('',*,*,#9075,.F.);
#12987=ORIENTED_EDGE('',*,*,#9202,.T.);
#12988=ORIENTED_EDGE('',*,*,#9203,.F.);
#12989=ORIENTED_EDGE('',*,*,#9084,.F.);
#12990=ORIENTED_EDGE('',*,*,#9073,.F.);
#12991=ORIENTED_EDGE('',*,*,#9085,.F.);
#12992=ORIENTED_EDGE('',*,*,#9203,.T.);
#12993=ORIENTED_EDGE('',*,*,#9201,.T.);
#12994=ORIENTED_EDGE('',*,*,#9071,.F.);
#12995=ORIENTED_EDGE('',*,*,#9204,.T.);
#12996=ORIENTED_EDGE('',*,*,#9205,.F.);
#12997=ORIENTED_EDGE('',*,*,#9086,.F.);
#12998=ORIENTED_EDGE('',*,*,#9087,.F.);
#12999=ORIENTED_EDGE('',*,*,#9205,.T.);
#13000=ORIENTED_EDGE('',*,*,#9206,.T.);
#13001=ORIENTED_EDGE('',*,*,#9069,.F.);
#13002=ORIENTED_EDGE('',*,*,#9070,.F.);
#13003=ORIENTED_EDGE('',*,*,#9206,.F.);
#13004=ORIENTED_EDGE('',*,*,#9204,.F.);
#13005=ORIENTED_EDGE('',*,*,#9066,.F.);
#13006=ORIENTED_EDGE('',*,*,#9207,.F.);
#13007=ORIENTED_EDGE('',*,*,#9208,.F.);
#13008=ORIENTED_EDGE('',*,*,#9067,.F.);
#13009=ORIENTED_EDGE('',*,*,#9208,.T.);
#13010=ORIENTED_EDGE('',*,*,#9209,.F.);
#13011=ORIENTED_EDGE('',*,*,#9088,.F.);
#13012=ORIENTED_EDGE('',*,*,#9065,.F.);
#13013=ORIENTED_EDGE('',*,*,#9089,.F.);
#13014=ORIENTED_EDGE('',*,*,#9209,.T.);
#13015=ORIENTED_EDGE('',*,*,#9207,.T.);
#13016=ORIENTED_EDGE('',*,*,#9063,.F.);
#13017=ORIENTED_EDGE('',*,*,#9210,.T.);
#13018=ORIENTED_EDGE('',*,*,#9211,.F.);
#13019=ORIENTED_EDGE('',*,*,#9090,.F.);
#13020=ORIENTED_EDGE('',*,*,#9091,.F.);
#13021=ORIENTED_EDGE('',*,*,#9211,.T.);
#13022=ORIENTED_EDGE('',*,*,#9212,.T.);
#13023=ORIENTED_EDGE('',*,*,#9061,.F.);
#13024=ORIENTED_EDGE('',*,*,#9062,.F.);
#13025=ORIENTED_EDGE('',*,*,#9212,.F.);
#13026=ORIENTED_EDGE('',*,*,#9210,.F.);
#13027=ORIENTED_EDGE('',*,*,#9058,.F.);
#13028=ORIENTED_EDGE('',*,*,#9213,.F.);
#13029=ORIENTED_EDGE('',*,*,#9214,.F.);
#13030=ORIENTED_EDGE('',*,*,#9059,.F.);
#13031=ORIENTED_EDGE('',*,*,#9214,.T.);
#13032=ORIENTED_EDGE('',*,*,#9215,.F.);
#13033=ORIENTED_EDGE('',*,*,#9092,.F.);
#13034=ORIENTED_EDGE('',*,*,#9057,.F.);
#13035=ORIENTED_EDGE('',*,*,#9093,.F.);
#13036=ORIENTED_EDGE('',*,*,#9215,.T.);
#13037=ORIENTED_EDGE('',*,*,#9213,.T.);
#13038=ORIENTED_EDGE('',*,*,#9055,.F.);
#13039=ORIENTED_EDGE('',*,*,#9216,.T.);
#13040=ORIENTED_EDGE('',*,*,#9217,.F.);
#13041=ORIENTED_EDGE('',*,*,#9094,.F.);
#13042=ORIENTED_EDGE('',*,*,#9095,.F.);
#13043=ORIENTED_EDGE('',*,*,#9217,.T.);
#13044=ORIENTED_EDGE('',*,*,#9218,.T.);
#13045=ORIENTED_EDGE('',*,*,#9053,.F.);
#13046=ORIENTED_EDGE('',*,*,#9054,.F.);
#13047=ORIENTED_EDGE('',*,*,#9218,.F.);
#13048=ORIENTED_EDGE('',*,*,#9216,.F.);
#13049=ORIENTED_EDGE('',*,*,#9050,.F.);
#13050=ORIENTED_EDGE('',*,*,#9219,.F.);
#13051=ORIENTED_EDGE('',*,*,#9220,.F.);
#13052=ORIENTED_EDGE('',*,*,#9051,.F.);
#13053=ORIENTED_EDGE('',*,*,#9220,.T.);
#13054=ORIENTED_EDGE('',*,*,#9221,.F.);
#13055=ORIENTED_EDGE('',*,*,#9096,.F.);
#13056=ORIENTED_EDGE('',*,*,#9049,.F.);
#13057=ORIENTED_EDGE('',*,*,#9097,.F.);
#13058=ORIENTED_EDGE('',*,*,#9221,.T.);
#13059=ORIENTED_EDGE('',*,*,#9219,.T.);
#13060=ORIENTED_EDGE('',*,*,#9047,.F.);
#13061=ORIENTED_EDGE('',*,*,#9222,.T.);
#13062=ORIENTED_EDGE('',*,*,#9223,.F.);
#13063=ORIENTED_EDGE('',*,*,#9098,.F.);
#13064=ORIENTED_EDGE('',*,*,#9099,.F.);
#13065=ORIENTED_EDGE('',*,*,#9223,.T.);
#13066=ORIENTED_EDGE('',*,*,#9224,.T.);
#13067=ORIENTED_EDGE('',*,*,#9045,.F.);
#13068=ORIENTED_EDGE('',*,*,#9046,.F.);
#13069=ORIENTED_EDGE('',*,*,#9224,.F.);
#13070=ORIENTED_EDGE('',*,*,#9222,.F.);
#13071=ORIENTED_EDGE('',*,*,#9042,.F.);
#13072=ORIENTED_EDGE('',*,*,#9225,.F.);
#13073=ORIENTED_EDGE('',*,*,#9226,.F.);
#13074=ORIENTED_EDGE('',*,*,#9043,.F.);
#13075=ORIENTED_EDGE('',*,*,#9226,.T.);
#13076=ORIENTED_EDGE('',*,*,#9227,.F.);
#13077=ORIENTED_EDGE('',*,*,#9100,.F.);
#13078=ORIENTED_EDGE('',*,*,#9041,.F.);
#13079=ORIENTED_EDGE('',*,*,#9101,.F.);
#13080=ORIENTED_EDGE('',*,*,#9227,.T.);
#13081=ORIENTED_EDGE('',*,*,#9225,.T.);
#13082=ORIENTED_EDGE('',*,*,#9039,.F.);
#13083=ORIENTED_EDGE('',*,*,#9228,.T.);
#13084=ORIENTED_EDGE('',*,*,#9229,.F.);
#13085=ORIENTED_EDGE('',*,*,#9102,.F.);
#13086=ORIENTED_EDGE('',*,*,#9103,.F.);
#13087=ORIENTED_EDGE('',*,*,#9229,.T.);
#13088=ORIENTED_EDGE('',*,*,#9230,.T.);
#13089=ORIENTED_EDGE('',*,*,#9037,.F.);
#13090=ORIENTED_EDGE('',*,*,#9038,.F.);
#13091=ORIENTED_EDGE('',*,*,#9230,.F.);
#13092=ORIENTED_EDGE('',*,*,#9228,.F.);
#13093=ORIENTED_EDGE('',*,*,#9034,.F.);
#13094=ORIENTED_EDGE('',*,*,#9231,.F.);
#13095=ORIENTED_EDGE('',*,*,#9232,.F.);
#13096=ORIENTED_EDGE('',*,*,#9035,.F.);
#13097=ORIENTED_EDGE('',*,*,#9232,.T.);
#13098=ORIENTED_EDGE('',*,*,#9233,.F.);
#13099=ORIENTED_EDGE('',*,*,#9104,.F.);
#13100=ORIENTED_EDGE('',*,*,#9033,.F.);
#13101=ORIENTED_EDGE('',*,*,#9105,.F.);
#13102=ORIENTED_EDGE('',*,*,#9233,.T.);
#13103=ORIENTED_EDGE('',*,*,#9231,.T.);
#13104=ORIENTED_EDGE('',*,*,#9031,.F.);
#13105=ORIENTED_EDGE('',*,*,#9234,.T.);
#13106=ORIENTED_EDGE('',*,*,#9235,.F.);
#13107=ORIENTED_EDGE('',*,*,#9106,.F.);
#13108=ORIENTED_EDGE('',*,*,#9107,.F.);
#13109=ORIENTED_EDGE('',*,*,#9235,.T.);
#13110=ORIENTED_EDGE('',*,*,#9236,.T.);
#13111=ORIENTED_EDGE('',*,*,#9029,.F.);
#13112=ORIENTED_EDGE('',*,*,#9030,.F.);
#13113=ORIENTED_EDGE('',*,*,#9236,.F.);
#13114=ORIENTED_EDGE('',*,*,#9234,.F.);
#13115=ORIENTED_EDGE('',*,*,#9026,.F.);
#13116=ORIENTED_EDGE('',*,*,#9237,.F.);
#13117=ORIENTED_EDGE('',*,*,#9238,.F.);
#13118=ORIENTED_EDGE('',*,*,#9027,.F.);
#13119=ORIENTED_EDGE('',*,*,#9238,.T.);
#13120=ORIENTED_EDGE('',*,*,#9239,.F.);
#13121=ORIENTED_EDGE('',*,*,#9108,.F.);
#13122=ORIENTED_EDGE('',*,*,#9025,.F.);
#13123=ORIENTED_EDGE('',*,*,#9109,.F.);
#13124=ORIENTED_EDGE('',*,*,#9239,.T.);
#13125=ORIENTED_EDGE('',*,*,#9237,.T.);
#13126=ORIENTED_EDGE('',*,*,#9023,.F.);
#13127=ORIENTED_EDGE('',*,*,#9240,.T.);
#13128=ORIENTED_EDGE('',*,*,#9241,.F.);
#13129=ORIENTED_EDGE('',*,*,#9110,.F.);
#13130=ORIENTED_EDGE('',*,*,#9111,.F.);
#13131=ORIENTED_EDGE('',*,*,#9241,.T.);
#13132=ORIENTED_EDGE('',*,*,#9242,.T.);
#13133=ORIENTED_EDGE('',*,*,#9021,.F.);
#13134=ORIENTED_EDGE('',*,*,#9022,.F.);
#13135=ORIENTED_EDGE('',*,*,#9242,.F.);
#13136=ORIENTED_EDGE('',*,*,#9240,.F.);
#13137=ORIENTED_EDGE('',*,*,#9018,.F.);
#13138=ORIENTED_EDGE('',*,*,#9243,.F.);
#13139=ORIENTED_EDGE('',*,*,#9244,.F.);
#13140=ORIENTED_EDGE('',*,*,#9019,.F.);
#13141=ORIENTED_EDGE('',*,*,#9244,.T.);
#13142=ORIENTED_EDGE('',*,*,#9245,.F.);
#13143=ORIENTED_EDGE('',*,*,#9112,.F.);
#13144=ORIENTED_EDGE('',*,*,#9017,.F.);
#13145=ORIENTED_EDGE('',*,*,#9113,.F.);
#13146=ORIENTED_EDGE('',*,*,#9245,.T.);
#13147=ORIENTED_EDGE('',*,*,#9243,.T.);
#13148=ORIENTED_EDGE('',*,*,#9015,.F.);
#13149=ORIENTED_EDGE('',*,*,#9246,.T.);
#13150=ORIENTED_EDGE('',*,*,#9247,.F.);
#13151=ORIENTED_EDGE('',*,*,#9114,.F.);
#13152=ORIENTED_EDGE('',*,*,#9115,.F.);
#13153=ORIENTED_EDGE('',*,*,#9247,.T.);
#13154=ORIENTED_EDGE('',*,*,#9248,.T.);
#13155=ORIENTED_EDGE('',*,*,#9013,.F.);
#13156=ORIENTED_EDGE('',*,*,#9014,.F.);
#13157=ORIENTED_EDGE('',*,*,#9248,.F.);
#13158=ORIENTED_EDGE('',*,*,#9246,.F.);
#13159=ORIENTED_EDGE('',*,*,#9010,.F.);
#13160=ORIENTED_EDGE('',*,*,#9249,.F.);
#13161=ORIENTED_EDGE('',*,*,#9250,.F.);
#13162=ORIENTED_EDGE('',*,*,#9011,.F.);
#13163=ORIENTED_EDGE('',*,*,#9250,.T.);
#13164=ORIENTED_EDGE('',*,*,#9251,.F.);
#13165=ORIENTED_EDGE('',*,*,#9116,.F.);
#13166=ORIENTED_EDGE('',*,*,#9009,.F.);
#13167=ORIENTED_EDGE('',*,*,#9117,.F.);
#13168=ORIENTED_EDGE('',*,*,#9251,.T.);
#13169=ORIENTED_EDGE('',*,*,#9249,.T.);
#13170=ORIENTED_EDGE('',*,*,#9007,.F.);
#13171=ORIENTED_EDGE('',*,*,#9252,.T.);
#13172=ORIENTED_EDGE('',*,*,#9253,.F.);
#13173=ORIENTED_EDGE('',*,*,#9118,.F.);
#13174=ORIENTED_EDGE('',*,*,#9119,.F.);
#13175=ORIENTED_EDGE('',*,*,#9253,.T.);
#13176=ORIENTED_EDGE('',*,*,#9254,.T.);
#13177=ORIENTED_EDGE('',*,*,#9005,.F.);
#13178=ORIENTED_EDGE('',*,*,#9006,.F.);
#13179=ORIENTED_EDGE('',*,*,#9254,.F.);
#13180=ORIENTED_EDGE('',*,*,#9252,.F.);
#13181=ORIENTED_EDGE('',*,*,#8923,.T.);
#13182=ORIENTED_EDGE('',*,*,#9255,.T.);
#13183=ORIENTED_EDGE('',*,*,#8936,.T.);
#13184=ORIENTED_EDGE('',*,*,#9255,.F.);
#13185=ORIENTED_EDGE('',*,*,#9152,.F.);
#13186=ORIENTED_EDGE('',*,*,#9256,.T.);
#13187=ORIENTED_EDGE('',*,*,#9257,.F.);
#13188=ORIENTED_EDGE('',*,*,#9258,.T.);
#13189=ORIENTED_EDGE('',*,*,#9259,.F.);
#13190=ORIENTED_EDGE('',*,*,#9260,.F.);
#13191=ORIENTED_EDGE('',*,*,#9261,.T.);
#13192=ORIENTED_EDGE('',*,*,#9262,.F.);
#13193=ORIENTED_EDGE('',*,*,#9263,.F.);
#13194=ORIENTED_EDGE('',*,*,#9264,.T.);
#13195=ORIENTED_EDGE('',*,*,#9265,.F.);
#13196=ORIENTED_EDGE('',*,*,#9266,.F.);
#13197=ORIENTED_EDGE('',*,*,#9267,.T.);
#13198=ORIENTED_EDGE('',*,*,#9268,.F.);
#13199=ORIENTED_EDGE('',*,*,#9269,.F.);
#13200=ORIENTED_EDGE('',*,*,#9270,.T.);
#13201=ORIENTED_EDGE('',*,*,#9271,.F.);
#13202=ORIENTED_EDGE('',*,*,#9272,.F.);
#13203=ORIENTED_EDGE('',*,*,#9273,.T.);
#13204=ORIENTED_EDGE('',*,*,#9274,.F.);
#13205=ORIENTED_EDGE('',*,*,#9275,.T.);
#13206=ORIENTED_EDGE('',*,*,#9256,.F.);
#13207=ORIENTED_EDGE('',*,*,#9275,.F.);
#13208=ORIENTED_EDGE('',*,*,#9276,.F.);
#13209=ORIENTED_EDGE('',*,*,#9264,.F.);
#13210=ORIENTED_EDGE('',*,*,#9277,.F.);
#13211=ORIENTED_EDGE('',*,*,#9278,.F.);
#13212=ORIENTED_EDGE('',*,*,#9279,.F.);
#13213=ORIENTED_EDGE('',*,*,#9267,.F.);
#13214=ORIENTED_EDGE('',*,*,#9280,.F.);
#13215=ORIENTED_EDGE('',*,*,#9281,.F.);
#13216=ORIENTED_EDGE('',*,*,#9282,.F.);
#13217=ORIENTED_EDGE('',*,*,#9283,.F.);
#13218=ORIENTED_EDGE('',*,*,#9284,.F.);
#13219=ORIENTED_EDGE('',*,*,#9261,.F.);
#13220=ORIENTED_EDGE('',*,*,#9285,.F.);
#13221=ORIENTED_EDGE('',*,*,#9270,.F.);
#13222=ORIENTED_EDGE('',*,*,#9286,.F.);
#13223=ORIENTED_EDGE('',*,*,#9287,.F.);
#13224=ORIENTED_EDGE('',*,*,#9288,.F.);
#13225=ORIENTED_EDGE('',*,*,#9289,.F.);
#13226=ORIENTED_EDGE('',*,*,#9290,.F.);
#13227=ORIENTED_EDGE('',*,*,#9258,.F.);
#13228=ORIENTED_EDGE('',*,*,#9291,.F.);
#13229=ORIENTED_EDGE('',*,*,#9292,.F.);
#13230=ORIENTED_EDGE('',*,*,#9293,.F.);
#13231=ORIENTED_EDGE('',*,*,#9273,.F.);
#13232=ORIENTED_EDGE('',*,*,#9271,.T.);
#13233=ORIENTED_EDGE('',*,*,#9285,.T.);
#13234=ORIENTED_EDGE('',*,*,#9294,.F.);
#13235=ORIENTED_EDGE('',*,*,#9286,.T.);
#13236=ORIENTED_EDGE('',*,*,#9269,.T.);
#13237=ORIENTED_EDGE('',*,*,#9295,.T.);
#13238=ORIENTED_EDGE('',*,*,#9296,.T.);
#13239=ORIENTED_EDGE('',*,*,#9297,.F.);
#13240=ORIENTED_EDGE('',*,*,#9268,.T.);
#13241=ORIENTED_EDGE('',*,*,#9279,.T.);
#13242=ORIENTED_EDGE('',*,*,#9298,.F.);
#13243=ORIENTED_EDGE('',*,*,#9280,.T.);
#13244=ORIENTED_EDGE('',*,*,#9266,.T.);
#13245=ORIENTED_EDGE('',*,*,#9299,.T.);
#13246=ORIENTED_EDGE('',*,*,#9300,.T.);
#13247=ORIENTED_EDGE('',*,*,#9295,.F.);
#13248=ORIENTED_EDGE('',*,*,#9265,.T.);
#13249=ORIENTED_EDGE('',*,*,#9276,.T.);
#13250=ORIENTED_EDGE('',*,*,#9301,.F.);
#13251=ORIENTED_EDGE('',*,*,#9277,.T.);
#13252=ORIENTED_EDGE('',*,*,#9263,.T.);
#13253=ORIENTED_EDGE('',*,*,#9302,.T.);
#13254=ORIENTED_EDGE('',*,*,#9303,.T.);
#13255=ORIENTED_EDGE('',*,*,#9299,.F.);
#13256=ORIENTED_EDGE('',*,*,#9278,.T.);
#13257=ORIENTED_EDGE('',*,*,#9301,.T.);
#13258=ORIENTED_EDGE('',*,*,#9281,.T.);
#13259=ORIENTED_EDGE('',*,*,#9298,.T.);
#13260=ORIENTED_EDGE('',*,*,#9283,.T.);
#13261=ORIENTED_EDGE('',*,*,#9304,.T.);
#13262=ORIENTED_EDGE('',*,*,#9287,.T.);
#13263=ORIENTED_EDGE('',*,*,#9294,.T.);
#13264=ORIENTED_EDGE('',*,*,#9289,.T.);
#13265=ORIENTED_EDGE('',*,*,#9305,.T.);
#13266=ORIENTED_EDGE('',*,*,#9292,.T.);
#13267=ORIENTED_EDGE('',*,*,#9306,.T.);
#13268=ORIENTED_EDGE('',*,*,#9307,.F.);
#13269=ORIENTED_EDGE('',*,*,#9308,.T.);
#13270=ORIENTED_EDGE('',*,*,#9303,.F.);
#13271=ORIENTED_EDGE('',*,*,#9309,.T.);
#13272=ORIENTED_EDGE('',*,*,#9300,.F.);
#13273=ORIENTED_EDGE('',*,*,#9310,.T.);
#13274=ORIENTED_EDGE('',*,*,#9296,.F.);
#13275=ORIENTED_EDGE('',*,*,#9311,.T.);
#13276=ORIENTED_EDGE('',*,*,#9312,.F.);
#13277=ORIENTED_EDGE('',*,*,#9313,.T.);
#13278=ORIENTED_EDGE('',*,*,#9314,.F.);
#13279=ORIENTED_EDGE('',*,*,#9315,.T.);
#13280=ORIENTED_EDGE('',*,*,#9316,.T.);
#13281=ORIENTED_EDGE('',*,*,#9313,.F.);
#13282=ORIENTED_EDGE('',*,*,#9311,.F.);
#13283=ORIENTED_EDGE('',*,*,#9310,.F.);
#13284=ORIENTED_EDGE('',*,*,#9309,.F.);
#13285=ORIENTED_EDGE('',*,*,#9308,.F.);
#13286=ORIENTED_EDGE('',*,*,#9315,.F.);
#13287=ORIENTED_EDGE('',*,*,#9316,.F.);
#13288=ORIENTED_EDGE('',*,*,#9260,.T.);
#13289=ORIENTED_EDGE('',*,*,#9317,.T.);
#13290=ORIENTED_EDGE('',*,*,#9307,.T.);
#13291=ORIENTED_EDGE('',*,*,#9302,.F.);
#13292=ORIENTED_EDGE('',*,*,#9262,.T.);
#13293=ORIENTED_EDGE('',*,*,#9284,.T.);
#13294=ORIENTED_EDGE('',*,*,#9304,.F.);
#13295=ORIENTED_EDGE('',*,*,#9282,.T.);
#13296=ORIENTED_EDGE('',*,*,#9257,.T.);
#13297=ORIENTED_EDGE('',*,*,#9318,.T.);
#13298=ORIENTED_EDGE('',*,*,#9314,.T.);
#13299=ORIENTED_EDGE('',*,*,#9317,.F.);
#13300=ORIENTED_EDGE('',*,*,#9259,.T.);
#13301=ORIENTED_EDGE('',*,*,#9290,.T.);
#13302=ORIENTED_EDGE('',*,*,#9305,.F.);
#13303=ORIENTED_EDGE('',*,*,#9288,.T.);
#13304=ORIENTED_EDGE('',*,*,#9272,.T.);
#13305=ORIENTED_EDGE('',*,*,#9297,.T.);
#13306=ORIENTED_EDGE('',*,*,#9312,.T.);
#13307=ORIENTED_EDGE('',*,*,#9318,.F.);
#13308=ORIENTED_EDGE('',*,*,#9274,.T.);
#13309=ORIENTED_EDGE('',*,*,#9293,.T.);
#13310=ORIENTED_EDGE('',*,*,#9306,.F.);
#13311=ORIENTED_EDGE('',*,*,#9291,.T.);
#13312=ORIENTED_EDGE('',*,*,#9319,.F.);
#13313=ORIENTED_EDGE('',*,*,#9320,.F.);
#13314=ORIENTED_EDGE('',*,*,#9321,.F.);
#13315=ORIENTED_EDGE('',*,*,#9322,.T.);
#13316=ORIENTED_EDGE('',*,*,#9323,.F.);
#13317=ORIENTED_EDGE('',*,*,#9324,.F.);
#13318=ORIENTED_EDGE('',*,*,#9319,.T.);
#13319=ORIENTED_EDGE('',*,*,#9325,.T.);
#13320=ORIENTED_EDGE('',*,*,#9326,.T.);
#13321=ORIENTED_EDGE('',*,*,#9327,.F.);
#13322=ORIENTED_EDGE('',*,*,#9328,.F.);
#13323=ORIENTED_EDGE('',*,*,#9323,.T.);
#13324=ORIENTED_EDGE('',*,*,#9329,.T.);
#13325=ORIENTED_EDGE('',*,*,#9330,.F.);
#13326=ORIENTED_EDGE('',*,*,#9331,.F.);
#13327=ORIENTED_EDGE('',*,*,#9327,.T.);
#13328=ORIENTED_EDGE('',*,*,#9332,.T.);
#13329=ORIENTED_EDGE('',*,*,#9333,.T.);
#13330=ORIENTED_EDGE('',*,*,#9334,.F.);
#13331=ORIENTED_EDGE('',*,*,#9335,.F.);
#13332=ORIENTED_EDGE('',*,*,#9336,.F.);
#13333=ORIENTED_EDGE('',*,*,#9330,.T.);
#13334=ORIENTED_EDGE('',*,*,#9337,.T.);
#13335=ORIENTED_EDGE('',*,*,#9338,.T.);
#13336=ORIENTED_EDGE('',*,*,#9339,.F.);
#13337=ORIENTED_EDGE('',*,*,#9340,.F.);
#13338=ORIENTED_EDGE('',*,*,#9334,.T.);
#13339=ORIENTED_EDGE('',*,*,#9341,.T.);
#13340=ORIENTED_EDGE('',*,*,#9342,.F.);
#13341=ORIENTED_EDGE('',*,*,#9343,.F.);
#13342=ORIENTED_EDGE('',*,*,#9344,.F.);
#13343=ORIENTED_EDGE('',*,*,#9339,.T.);
#13344=ORIENTED_EDGE('',*,*,#9345,.T.);
#13345=ORIENTED_EDGE('',*,*,#9346,.T.);
#13346=ORIENTED_EDGE('',*,*,#9347,.F.);
#13347=ORIENTED_EDGE('',*,*,#9348,.F.);
#13348=ORIENTED_EDGE('',*,*,#9342,.T.);
#13349=ORIENTED_EDGE('',*,*,#9349,.T.);
#13350=ORIENTED_EDGE('',*,*,#9350,.F.);
#13351=ORIENTED_EDGE('',*,*,#9351,.F.);
#13352=ORIENTED_EDGE('',*,*,#9352,.F.);
#13353=ORIENTED_EDGE('',*,*,#9347,.T.);
#13354=ORIENTED_EDGE('',*,*,#9353,.T.);
#13355=ORIENTED_EDGE('',*,*,#9354,.T.);
#13356=ORIENTED_EDGE('',*,*,#9355,.F.);
#13357=ORIENTED_EDGE('',*,*,#9356,.F.);
#13358=ORIENTED_EDGE('',*,*,#9350,.T.);
#13359=ORIENTED_EDGE('',*,*,#9357,.T.);
#13360=ORIENTED_EDGE('',*,*,#9358,.F.);
#13361=ORIENTED_EDGE('',*,*,#9359,.F.);
#13362=ORIENTED_EDGE('',*,*,#9360,.F.);
#13363=ORIENTED_EDGE('',*,*,#9355,.T.);
#13364=ORIENTED_EDGE('',*,*,#9361,.T.);
#13365=ORIENTED_EDGE('',*,*,#9362,.T.);
#13366=ORIENTED_EDGE('',*,*,#9363,.F.);
#13367=ORIENTED_EDGE('',*,*,#9364,.F.);
#13368=ORIENTED_EDGE('',*,*,#9365,.F.);
#13369=ORIENTED_EDGE('',*,*,#9358,.T.);
#13370=ORIENTED_EDGE('',*,*,#9366,.T.);
#13371=ORIENTED_EDGE('',*,*,#9367,.F.);
#13372=ORIENTED_EDGE('',*,*,#9368,.F.);
#13373=ORIENTED_EDGE('',*,*,#9363,.T.);
#13374=ORIENTED_EDGE('',*,*,#9369,.T.);
#13375=ORIENTED_EDGE('',*,*,#9370,.T.);
#13376=ORIENTED_EDGE('',*,*,#9371,.F.);
#13377=ORIENTED_EDGE('',*,*,#9372,.F.);
#13378=ORIENTED_EDGE('',*,*,#9373,.F.);
#13379=ORIENTED_EDGE('',*,*,#9367,.T.);
#13380=ORIENTED_EDGE('',*,*,#9374,.T.);
#13381=ORIENTED_EDGE('',*,*,#9375,.F.);
#13382=ORIENTED_EDGE('',*,*,#9376,.F.);
#13383=ORIENTED_EDGE('',*,*,#9371,.T.);
#13384=ORIENTED_EDGE('',*,*,#9377,.T.);
#13385=ORIENTED_EDGE('',*,*,#9378,.T.);
#13386=ORIENTED_EDGE('',*,*,#9379,.F.);
#13387=ORIENTED_EDGE('',*,*,#9380,.F.);
#13388=ORIENTED_EDGE('',*,*,#9381,.F.);
#13389=ORIENTED_EDGE('',*,*,#9375,.T.);
#13390=ORIENTED_EDGE('',*,*,#9382,.T.);
#13391=ORIENTED_EDGE('',*,*,#9383,.F.);
#13392=ORIENTED_EDGE('',*,*,#9384,.F.);
#13393=ORIENTED_EDGE('',*,*,#9379,.T.);
#13394=ORIENTED_EDGE('',*,*,#9385,.T.);
#13395=ORIENTED_EDGE('',*,*,#9386,.T.);
#13396=ORIENTED_EDGE('',*,*,#9387,.F.);
#13397=ORIENTED_EDGE('',*,*,#9388,.F.);
#13398=ORIENTED_EDGE('',*,*,#9389,.F.);
#13399=ORIENTED_EDGE('',*,*,#9383,.T.);
#13400=ORIENTED_EDGE('',*,*,#9390,.T.);
#13401=ORIENTED_EDGE('',*,*,#9391,.F.);
#13402=ORIENTED_EDGE('',*,*,#9392,.F.);
#13403=ORIENTED_EDGE('',*,*,#9387,.T.);
#13404=ORIENTED_EDGE('',*,*,#9393,.T.);
#13405=ORIENTED_EDGE('',*,*,#9394,.T.);
#13406=ORIENTED_EDGE('',*,*,#9395,.F.);
#13407=ORIENTED_EDGE('',*,*,#9396,.F.);
#13408=ORIENTED_EDGE('',*,*,#9397,.F.);
#13409=ORIENTED_EDGE('',*,*,#9391,.T.);
#13410=ORIENTED_EDGE('',*,*,#9398,.T.);
#13411=ORIENTED_EDGE('',*,*,#9399,.F.);
#13412=ORIENTED_EDGE('',*,*,#9400,.F.);
#13413=ORIENTED_EDGE('',*,*,#9395,.T.);
#13414=ORIENTED_EDGE('',*,*,#9401,.T.);
#13415=ORIENTED_EDGE('',*,*,#9402,.T.);
#13416=ORIENTED_EDGE('',*,*,#9403,.F.);
#13417=ORIENTED_EDGE('',*,*,#9404,.F.);
#13418=ORIENTED_EDGE('',*,*,#9405,.F.);
#13419=ORIENTED_EDGE('',*,*,#9399,.T.);
#13420=ORIENTED_EDGE('',*,*,#9406,.T.);
#13421=ORIENTED_EDGE('',*,*,#9407,.F.);
#13422=ORIENTED_EDGE('',*,*,#9408,.F.);
#13423=ORIENTED_EDGE('',*,*,#9403,.T.);
#13424=ORIENTED_EDGE('',*,*,#9409,.T.);
#13425=ORIENTED_EDGE('',*,*,#9410,.T.);
#13426=ORIENTED_EDGE('',*,*,#9411,.T.);
#13427=ORIENTED_EDGE('',*,*,#9412,.T.);
#13428=ORIENTED_EDGE('',*,*,#9413,.T.);
#13429=ORIENTED_EDGE('',*,*,#9414,.T.);
#13430=ORIENTED_EDGE('',*,*,#9415,.T.);
#13431=ORIENTED_EDGE('',*,*,#9416,.T.);
#13432=ORIENTED_EDGE('',*,*,#9417,.T.);
#13433=ORIENTED_EDGE('',*,*,#9418,.T.);
#13434=ORIENTED_EDGE('',*,*,#9419,.T.);
#13435=ORIENTED_EDGE('',*,*,#9420,.T.);
#13436=ORIENTED_EDGE('',*,*,#9421,.T.);
#13437=ORIENTED_EDGE('',*,*,#9422,.T.);
#13438=ORIENTED_EDGE('',*,*,#9423,.T.);
#13439=ORIENTED_EDGE('',*,*,#9424,.T.);
#13440=ORIENTED_EDGE('',*,*,#9425,.T.);
#13441=ORIENTED_EDGE('',*,*,#9426,.T.);
#13442=ORIENTED_EDGE('',*,*,#9427,.T.);
#13443=ORIENTED_EDGE('',*,*,#9428,.T.);
#13444=ORIENTED_EDGE('',*,*,#9429,.T.);
#13445=ORIENTED_EDGE('',*,*,#9430,.T.);
#13446=ORIENTED_EDGE('',*,*,#9431,.T.);
#13447=ORIENTED_EDGE('',*,*,#9432,.T.);
#13448=ORIENTED_EDGE('',*,*,#9433,.T.);
#13449=ORIENTED_EDGE('',*,*,#9434,.T.);
#13450=ORIENTED_EDGE('',*,*,#9435,.T.);
#13451=ORIENTED_EDGE('',*,*,#9436,.T.);
#13452=ORIENTED_EDGE('',*,*,#9437,.F.);
#13453=ORIENTED_EDGE('',*,*,#9438,.T.);
#13454=ORIENTED_EDGE('',*,*,#9439,.T.);
#13455=ORIENTED_EDGE('',*,*,#9440,.T.);
#13456=ORIENTED_EDGE('',*,*,#9441,.T.);
#13457=ORIENTED_EDGE('',*,*,#9442,.T.);
#13458=ORIENTED_EDGE('',*,*,#9443,.T.);
#13459=ORIENTED_EDGE('',*,*,#9444,.T.);
#13460=ORIENTED_EDGE('',*,*,#9445,.T.);
#13461=ORIENTED_EDGE('',*,*,#9446,.T.);
#13462=ORIENTED_EDGE('',*,*,#9447,.T.);
#13463=ORIENTED_EDGE('',*,*,#9448,.T.);
#13464=ORIENTED_EDGE('',*,*,#9449,.T.);
#13465=ORIENTED_EDGE('',*,*,#9450,.T.);
#13466=ORIENTED_EDGE('',*,*,#9451,.T.);
#13467=ORIENTED_EDGE('',*,*,#9452,.T.);
#13468=ORIENTED_EDGE('',*,*,#9453,.T.);
#13469=ORIENTED_EDGE('',*,*,#9454,.T.);
#13470=ORIENTED_EDGE('',*,*,#9455,.T.);
#13471=ORIENTED_EDGE('',*,*,#9456,.T.);
#13472=ORIENTED_EDGE('',*,*,#9457,.T.);
#13473=ORIENTED_EDGE('',*,*,#9458,.T.);
#13474=ORIENTED_EDGE('',*,*,#9459,.T.);
#13475=ORIENTED_EDGE('',*,*,#9460,.T.);
#13476=ORIENTED_EDGE('',*,*,#9461,.T.);
#13477=ORIENTED_EDGE('',*,*,#9407,.T.);
#13478=ORIENTED_EDGE('',*,*,#9462,.T.);
#13479=ORIENTED_EDGE('',*,*,#9463,.F.);
#13480=ORIENTED_EDGE('',*,*,#9464,.F.);
#13481=ORIENTED_EDGE('',*,*,#9465,.F.);
#13482=ORIENTED_EDGE('',*,*,#9466,.F.);
#13483=ORIENTED_EDGE('',*,*,#9467,.T.);
#13484=ORIENTED_EDGE('',*,*,#9463,.T.);
#13485=ORIENTED_EDGE('',*,*,#9468,.T.);
#13486=ORIENTED_EDGE('',*,*,#9469,.T.);
#13487=ORIENTED_EDGE('',*,*,#9470,.F.);
#13488=ORIENTED_EDGE('',*,*,#9467,.F.);
#13489=ORIENTED_EDGE('',*,*,#9471,.F.);
#13490=ORIENTED_EDGE('',*,*,#9436,.F.);
#13491=ORIENTED_EDGE('',*,*,#9435,.F.);
#13492=ORIENTED_EDGE('',*,*,#9434,.F.);
#13493=ORIENTED_EDGE('',*,*,#9433,.F.);
#13494=ORIENTED_EDGE('',*,*,#9432,.F.);
#13495=ORIENTED_EDGE('',*,*,#9431,.F.);
#13496=ORIENTED_EDGE('',*,*,#9430,.F.);
#13497=ORIENTED_EDGE('',*,*,#9429,.F.);
#13498=ORIENTED_EDGE('',*,*,#9428,.F.);
#13499=ORIENTED_EDGE('',*,*,#9427,.F.);
#13500=ORIENTED_EDGE('',*,*,#9426,.F.);
#13501=ORIENTED_EDGE('',*,*,#9425,.F.);
#13502=ORIENTED_EDGE('',*,*,#9424,.F.);
#13503=ORIENTED_EDGE('',*,*,#9423,.F.);
#13504=ORIENTED_EDGE('',*,*,#9422,.F.);
#13505=ORIENTED_EDGE('',*,*,#9421,.F.);
#13506=ORIENTED_EDGE('',*,*,#9420,.F.);
#13507=ORIENTED_EDGE('',*,*,#9419,.F.);
#13508=ORIENTED_EDGE('',*,*,#9418,.F.);
#13509=ORIENTED_EDGE('',*,*,#9417,.F.);
#13510=ORIENTED_EDGE('',*,*,#9416,.F.);
#13511=ORIENTED_EDGE('',*,*,#9415,.F.);
#13512=ORIENTED_EDGE('',*,*,#9414,.F.);
#13513=ORIENTED_EDGE('',*,*,#9413,.F.);
#13514=ORIENTED_EDGE('',*,*,#9412,.F.);
#13515=ORIENTED_EDGE('',*,*,#9472,.F.);
#13516=ORIENTED_EDGE('',*,*,#9473,.T.);
#13517=ORIENTED_EDGE('',*,*,#9320,.T.);
#13518=ORIENTED_EDGE('',*,*,#9324,.T.);
#13519=ORIENTED_EDGE('',*,*,#9328,.T.);
#13520=ORIENTED_EDGE('',*,*,#9331,.T.);
#13521=ORIENTED_EDGE('',*,*,#9336,.T.);
#13522=ORIENTED_EDGE('',*,*,#9335,.T.);
#13523=ORIENTED_EDGE('',*,*,#9340,.T.);
#13524=ORIENTED_EDGE('',*,*,#9344,.T.);
#13525=ORIENTED_EDGE('',*,*,#9343,.T.);
#13526=ORIENTED_EDGE('',*,*,#9348,.T.);
#13527=ORIENTED_EDGE('',*,*,#9352,.T.);
#13528=ORIENTED_EDGE('',*,*,#9351,.T.);
#13529=ORIENTED_EDGE('',*,*,#9356,.T.);
#13530=ORIENTED_EDGE('',*,*,#9360,.T.);
#13531=ORIENTED_EDGE('',*,*,#9359,.T.);
#13532=ORIENTED_EDGE('',*,*,#9365,.T.);
#13533=ORIENTED_EDGE('',*,*,#9364,.T.);
#13534=ORIENTED_EDGE('',*,*,#9368,.T.);
#13535=ORIENTED_EDGE('',*,*,#9373,.T.);
#13536=ORIENTED_EDGE('',*,*,#9372,.T.);
#13537=ORIENTED_EDGE('',*,*,#9376,.T.);
#13538=ORIENTED_EDGE('',*,*,#9381,.T.);
#13539=ORIENTED_EDGE('',*,*,#9380,.T.);
#13540=ORIENTED_EDGE('',*,*,#9384,.T.);
#13541=ORIENTED_EDGE('',*,*,#9389,.T.);
#13542=ORIENTED_EDGE('',*,*,#9388,.T.);
#13543=ORIENTED_EDGE('',*,*,#9392,.T.);
#13544=ORIENTED_EDGE('',*,*,#9397,.T.);
#13545=ORIENTED_EDGE('',*,*,#9396,.T.);
#13546=ORIENTED_EDGE('',*,*,#9400,.T.);
#13547=ORIENTED_EDGE('',*,*,#9405,.T.);
#13548=ORIENTED_EDGE('',*,*,#9404,.T.);
#13549=ORIENTED_EDGE('',*,*,#9408,.T.);
#13550=ORIENTED_EDGE('',*,*,#9465,.T.);
#13551=ORIENTED_EDGE('',*,*,#9464,.T.);
#13552=ORIENTED_EDGE('',*,*,#9474,.T.);
#13553=ORIENTED_EDGE('',*,*,#9475,.T.);
#13554=ORIENTED_EDGE('',*,*,#9476,.T.);
#13555=ORIENTED_EDGE('',*,*,#9321,.T.);
#13556=ORIENTED_EDGE('',*,*,#9473,.F.);
#13557=ORIENTED_EDGE('',*,*,#9472,.T.);
#13558=ORIENTED_EDGE('',*,*,#9469,.F.);
#13559=ORIENTED_EDGE('',*,*,#9468,.F.);
#13560=ORIENTED_EDGE('',*,*,#9462,.F.);
#13561=ORIENTED_EDGE('',*,*,#9409,.F.);
#13562=ORIENTED_EDGE('',*,*,#9406,.F.);
#13563=ORIENTED_EDGE('',*,*,#9402,.F.);
#13564=ORIENTED_EDGE('',*,*,#9401,.F.);
#13565=ORIENTED_EDGE('',*,*,#9398,.F.);
#13566=ORIENTED_EDGE('',*,*,#9394,.F.);
#13567=ORIENTED_EDGE('',*,*,#9393,.F.);
#13568=ORIENTED_EDGE('',*,*,#9390,.F.);
#13569=ORIENTED_EDGE('',*,*,#9386,.F.);
#13570=ORIENTED_EDGE('',*,*,#9385,.F.);
#13571=ORIENTED_EDGE('',*,*,#9382,.F.);
#13572=ORIENTED_EDGE('',*,*,#9378,.F.);
#13573=ORIENTED_EDGE('',*,*,#9377,.F.);
#13574=ORIENTED_EDGE('',*,*,#9374,.F.);
#13575=ORIENTED_EDGE('',*,*,#9370,.F.);
#13576=ORIENTED_EDGE('',*,*,#9369,.F.);
#13577=ORIENTED_EDGE('',*,*,#9366,.F.);
#13578=ORIENTED_EDGE('',*,*,#9362,.F.);
#13579=ORIENTED_EDGE('',*,*,#9361,.F.);
#13580=ORIENTED_EDGE('',*,*,#9357,.F.);
#13581=ORIENTED_EDGE('',*,*,#9354,.F.);
#13582=ORIENTED_EDGE('',*,*,#9353,.F.);
#13583=ORIENTED_EDGE('',*,*,#9349,.F.);
#13584=ORIENTED_EDGE('',*,*,#9346,.F.);
#13585=ORIENTED_EDGE('',*,*,#9345,.F.);
#13586=ORIENTED_EDGE('',*,*,#9341,.F.);
#13587=ORIENTED_EDGE('',*,*,#9338,.F.);
#13588=ORIENTED_EDGE('',*,*,#9337,.F.);
#13589=ORIENTED_EDGE('',*,*,#9333,.F.);
#13590=ORIENTED_EDGE('',*,*,#9332,.F.);
#13591=ORIENTED_EDGE('',*,*,#9329,.F.);
#13592=ORIENTED_EDGE('',*,*,#9326,.F.);
#13593=ORIENTED_EDGE('',*,*,#9325,.F.);
#13594=ORIENTED_EDGE('',*,*,#9322,.F.);
#13595=ORIENTED_EDGE('',*,*,#9476,.F.);
#13596=ORIENTED_EDGE('',*,*,#9477,.T.);
#13597=ORIENTED_EDGE('',*,*,#9410,.F.);
#13598=ORIENTED_EDGE('',*,*,#9461,.F.);
#13599=ORIENTED_EDGE('',*,*,#9460,.F.);
#13600=ORIENTED_EDGE('',*,*,#9459,.F.);
#13601=ORIENTED_EDGE('',*,*,#9458,.F.);
#13602=ORIENTED_EDGE('',*,*,#9457,.F.);
#13603=ORIENTED_EDGE('',*,*,#9456,.F.);
#13604=ORIENTED_EDGE('',*,*,#9455,.F.);
#13605=ORIENTED_EDGE('',*,*,#9454,.F.);
#13606=ORIENTED_EDGE('',*,*,#9453,.F.);
#13607=ORIENTED_EDGE('',*,*,#9452,.F.);
#13608=ORIENTED_EDGE('',*,*,#9451,.F.);
#13609=ORIENTED_EDGE('',*,*,#9450,.F.);
#13610=ORIENTED_EDGE('',*,*,#9449,.F.);
#13611=ORIENTED_EDGE('',*,*,#9448,.F.);
#13612=ORIENTED_EDGE('',*,*,#9447,.F.);
#13613=ORIENTED_EDGE('',*,*,#9446,.F.);
#13614=ORIENTED_EDGE('',*,*,#9445,.F.);
#13615=ORIENTED_EDGE('',*,*,#9444,.F.);
#13616=ORIENTED_EDGE('',*,*,#9443,.F.);
#13617=ORIENTED_EDGE('',*,*,#9442,.F.);
#13618=ORIENTED_EDGE('',*,*,#9441,.F.);
#13619=ORIENTED_EDGE('',*,*,#9440,.F.);
#13620=ORIENTED_EDGE('',*,*,#9439,.F.);
#13621=ORIENTED_EDGE('',*,*,#9438,.F.);
#13622=ORIENTED_EDGE('',*,*,#9478,.F.);
#13623=ORIENTED_EDGE('',*,*,#9479,.T.);
#13624=ORIENTED_EDGE('',*,*,#9480,.F.);
#13625=ORIENTED_EDGE('',*,*,#9481,.F.);
#13626=ORIENTED_EDGE('',*,*,#9482,.T.);
#13627=ORIENTED_EDGE('',*,*,#9483,.F.);
#13628=ORIENTED_EDGE('',*,*,#9484,.F.);
#13629=ORIENTED_EDGE('',*,*,#9485,.T.);
#13630=ORIENTED_EDGE('',*,*,#9486,.F.);
#13631=ORIENTED_EDGE('',*,*,#9487,.F.);
#13632=ORIENTED_EDGE('',*,*,#9488,.T.);
#13633=ORIENTED_EDGE('',*,*,#9489,.F.);
#13634=ORIENTED_EDGE('',*,*,#9490,.F.);
#13635=ORIENTED_EDGE('',*,*,#9491,.T.);
#13636=ORIENTED_EDGE('',*,*,#9492,.F.);
#13637=ORIENTED_EDGE('',*,*,#9493,.F.);
#13638=ORIENTED_EDGE('',*,*,#9494,.T.);
#13639=ORIENTED_EDGE('',*,*,#9495,.F.);
#13640=ORIENTED_EDGE('',*,*,#9496,.T.);
#13641=ORIENTED_EDGE('',*,*,#9497,.F.);
#13642=ORIENTED_EDGE('',*,*,#9496,.F.);
#13643=ORIENTED_EDGE('',*,*,#9498,.F.);
#13644=ORIENTED_EDGE('',*,*,#9485,.F.);
#13645=ORIENTED_EDGE('',*,*,#9499,.F.);
#13646=ORIENTED_EDGE('',*,*,#9500,.F.);
#13647=ORIENTED_EDGE('',*,*,#9501,.F.);
#13648=ORIENTED_EDGE('',*,*,#9488,.F.);
#13649=ORIENTED_EDGE('',*,*,#9502,.F.);
#13650=ORIENTED_EDGE('',*,*,#9503,.F.);
#13651=ORIENTED_EDGE('',*,*,#9504,.F.);
#13652=ORIENTED_EDGE('',*,*,#9505,.F.);
#13653=ORIENTED_EDGE('',*,*,#9506,.F.);
#13654=ORIENTED_EDGE('',*,*,#9482,.F.);
#13655=ORIENTED_EDGE('',*,*,#9507,.F.);
#13656=ORIENTED_EDGE('',*,*,#9491,.F.);
#13657=ORIENTED_EDGE('',*,*,#9508,.F.);
#13658=ORIENTED_EDGE('',*,*,#9509,.F.);
#13659=ORIENTED_EDGE('',*,*,#9510,.F.);
#13660=ORIENTED_EDGE('',*,*,#9511,.F.);
#13661=ORIENTED_EDGE('',*,*,#9512,.F.);
#13662=ORIENTED_EDGE('',*,*,#9479,.F.);
#13663=ORIENTED_EDGE('',*,*,#9513,.F.);
#13664=ORIENTED_EDGE('',*,*,#9514,.F.);
#13665=ORIENTED_EDGE('',*,*,#9515,.F.);
#13666=ORIENTED_EDGE('',*,*,#9494,.F.);
#13667=ORIENTED_EDGE('',*,*,#9492,.T.);
#13668=ORIENTED_EDGE('',*,*,#9507,.T.);
#13669=ORIENTED_EDGE('',*,*,#9516,.F.);
#13670=ORIENTED_EDGE('',*,*,#9508,.T.);
#13671=ORIENTED_EDGE('',*,*,#9490,.T.);
#13672=ORIENTED_EDGE('',*,*,#9517,.T.);
#13673=ORIENTED_EDGE('',*,*,#9518,.T.);
#13674=ORIENTED_EDGE('',*,*,#9519,.F.);
#13675=ORIENTED_EDGE('',*,*,#9489,.T.);
#13676=ORIENTED_EDGE('',*,*,#9501,.T.);
#13677=ORIENTED_EDGE('',*,*,#9520,.F.);
#13678=ORIENTED_EDGE('',*,*,#9502,.T.);
#13679=ORIENTED_EDGE('',*,*,#9487,.T.);
#13680=ORIENTED_EDGE('',*,*,#9521,.T.);
#13681=ORIENTED_EDGE('',*,*,#9522,.T.);
#13682=ORIENTED_EDGE('',*,*,#9517,.F.);
#13683=ORIENTED_EDGE('',*,*,#9486,.T.);
#13684=ORIENTED_EDGE('',*,*,#9498,.T.);
#13685=ORIENTED_EDGE('',*,*,#9523,.F.);
#13686=ORIENTED_EDGE('',*,*,#9499,.T.);
#13687=ORIENTED_EDGE('',*,*,#9484,.T.);
#13688=ORIENTED_EDGE('',*,*,#9524,.T.);
#13689=ORIENTED_EDGE('',*,*,#9525,.T.);
#13690=ORIENTED_EDGE('',*,*,#9521,.F.);
#13691=ORIENTED_EDGE('',*,*,#9500,.T.);
#13692=ORIENTED_EDGE('',*,*,#9523,.T.);
#13693=ORIENTED_EDGE('',*,*,#9503,.T.);
#13694=ORIENTED_EDGE('',*,*,#9520,.T.);
#13695=ORIENTED_EDGE('',*,*,#9505,.T.);
#13696=ORIENTED_EDGE('',*,*,#9526,.T.);
#13697=ORIENTED_EDGE('',*,*,#9509,.T.);
#13698=ORIENTED_EDGE('',*,*,#9516,.T.);
#13699=ORIENTED_EDGE('',*,*,#9511,.T.);
#13700=ORIENTED_EDGE('',*,*,#9527,.T.);
#13701=ORIENTED_EDGE('',*,*,#9514,.T.);
#13702=ORIENTED_EDGE('',*,*,#9528,.T.);
#13703=ORIENTED_EDGE('',*,*,#9529,.F.);
#13704=ORIENTED_EDGE('',*,*,#9530,.T.);
#13705=ORIENTED_EDGE('',*,*,#9525,.F.);
#13706=ORIENTED_EDGE('',*,*,#9531,.T.);
#13707=ORIENTED_EDGE('',*,*,#9522,.F.);
#13708=ORIENTED_EDGE('',*,*,#9532,.T.);
#13709=ORIENTED_EDGE('',*,*,#9518,.F.);
#13710=ORIENTED_EDGE('',*,*,#9533,.T.);
#13711=ORIENTED_EDGE('',*,*,#9534,.F.);
#13712=ORIENTED_EDGE('',*,*,#9535,.T.);
#13713=ORIENTED_EDGE('',*,*,#9536,.F.);
#13714=ORIENTED_EDGE('',*,*,#9537,.T.);
#13715=ORIENTED_EDGE('',*,*,#9538,.T.);
#13716=ORIENTED_EDGE('',*,*,#9535,.F.);
#13717=ORIENTED_EDGE('',*,*,#9533,.F.);
#13718=ORIENTED_EDGE('',*,*,#9532,.F.);
#13719=ORIENTED_EDGE('',*,*,#9531,.F.);
#13720=ORIENTED_EDGE('',*,*,#9530,.F.);
#13721=ORIENTED_EDGE('',*,*,#9537,.F.);
#13722=ORIENTED_EDGE('',*,*,#9538,.F.);
#13723=ORIENTED_EDGE('',*,*,#9481,.T.);
#13724=ORIENTED_EDGE('',*,*,#9539,.T.);
#13725=ORIENTED_EDGE('',*,*,#9529,.T.);
#13726=ORIENTED_EDGE('',*,*,#9524,.F.);
#13727=ORIENTED_EDGE('',*,*,#9483,.T.);
#13728=ORIENTED_EDGE('',*,*,#9506,.T.);
#13729=ORIENTED_EDGE('',*,*,#9526,.F.);
#13730=ORIENTED_EDGE('',*,*,#9504,.T.);
#13731=ORIENTED_EDGE('',*,*,#9478,.T.);
#13732=ORIENTED_EDGE('',*,*,#9540,.T.);
#13733=ORIENTED_EDGE('',*,*,#9536,.T.);
#13734=ORIENTED_EDGE('',*,*,#9539,.F.);
#13735=ORIENTED_EDGE('',*,*,#9480,.T.);
#13736=ORIENTED_EDGE('',*,*,#9512,.T.);
#13737=ORIENTED_EDGE('',*,*,#9527,.F.);
#13738=ORIENTED_EDGE('',*,*,#9510,.T.);
#13739=ORIENTED_EDGE('',*,*,#9493,.T.);
#13740=ORIENTED_EDGE('',*,*,#9519,.T.);
#13741=ORIENTED_EDGE('',*,*,#9534,.T.);
#13742=ORIENTED_EDGE('',*,*,#9540,.F.);
#13743=ORIENTED_EDGE('',*,*,#9495,.T.);
#13744=ORIENTED_EDGE('',*,*,#9515,.T.);
#13745=ORIENTED_EDGE('',*,*,#9528,.F.);
#13746=ORIENTED_EDGE('',*,*,#9513,.T.);
#13747=ORIENTED_EDGE('',*,*,#9541,.F.);
#13748=ORIENTED_EDGE('',*,*,#9497,.T.);
#13749=ORIENTED_EDGE('',*,*,#9477,.F.);
#13750=ORIENTED_EDGE('',*,*,#9475,.F.);
#13751=ORIENTED_EDGE('',*,*,#9542,.T.);
#13752=ORIENTED_EDGE('',*,*,#9541,.T.);
#13753=ORIENTED_EDGE('',*,*,#9542,.F.);
#13754=ORIENTED_EDGE('',*,*,#9474,.F.);
#13755=ORIENTED_EDGE('',*,*,#9411,.F.);
#13756=ORIENTED_EDGE('',*,*,#9466,.T.);
#13757=ORIENTED_EDGE('',*,*,#9543,.T.);
#13758=ORIENTED_EDGE('',*,*,#9544,.F.);
#13759=ORIENTED_EDGE('',*,*,#9543,.F.);
#13760=ORIENTED_EDGE('',*,*,#9470,.T.);
#13761=ORIENTED_EDGE('',*,*,#9437,.T.);
#13762=ORIENTED_EDGE('',*,*,#9471,.T.);
#13763=ORIENTED_EDGE('',*,*,#9544,.T.);
#13764=ORIENTED_EDGE('',*,*,#9545,.F.);
#13765=ORIENTED_EDGE('',*,*,#9546,.F.);
#13766=ORIENTED_EDGE('',*,*,#9547,.F.);
#13767=ORIENTED_EDGE('',*,*,#9548,.F.);
#13768=ORIENTED_EDGE('',*,*,#9549,.F.);
#13769=ORIENTED_EDGE('',*,*,#9550,.F.);
#13770=ORIENTED_EDGE('',*,*,#9545,.T.);
#13771=ORIENTED_EDGE('',*,*,#9551,.F.);
#13772=ORIENTED_EDGE('',*,*,#9552,.T.);
#13773=ORIENTED_EDGE('',*,*,#9553,.T.);
#13774=ORIENTED_EDGE('',*,*,#9554,.F.);
#13775=ORIENTED_EDGE('',*,*,#9555,.F.);
#13776=ORIENTED_EDGE('',*,*,#9548,.T.);
#13777=ORIENTED_EDGE('',*,*,#9556,.T.);
#13778=ORIENTED_EDGE('',*,*,#9557,.T.);
#13779=ORIENTED_EDGE('',*,*,#9558,.F.);
#13780=ORIENTED_EDGE('',*,*,#9559,.F.);
#13781=ORIENTED_EDGE('',*,*,#9560,.F.);
#13782=ORIENTED_EDGE('',*,*,#9554,.T.);
#13783=ORIENTED_EDGE('',*,*,#9561,.T.);
#13784=ORIENTED_EDGE('',*,*,#9562,.T.);
#13785=ORIENTED_EDGE('',*,*,#9563,.F.);
#13786=ORIENTED_EDGE('',*,*,#9564,.F.);
#13787=ORIENTED_EDGE('',*,*,#9558,.T.);
#13788=ORIENTED_EDGE('',*,*,#9565,.T.);
#13789=ORIENTED_EDGE('',*,*,#9566,.T.);
#13790=ORIENTED_EDGE('',*,*,#9567,.F.);
#13791=ORIENTED_EDGE('',*,*,#9568,.F.);
#13792=ORIENTED_EDGE('',*,*,#9569,.F.);
#13793=ORIENTED_EDGE('',*,*,#9563,.T.);
#13794=ORIENTED_EDGE('',*,*,#9570,.T.);
#13795=ORIENTED_EDGE('',*,*,#9571,.T.);
#13796=ORIENTED_EDGE('',*,*,#9572,.F.);
#13797=ORIENTED_EDGE('',*,*,#9573,.F.);
#13798=ORIENTED_EDGE('',*,*,#9567,.T.);
#13799=ORIENTED_EDGE('',*,*,#9574,.T.);
#13800=ORIENTED_EDGE('',*,*,#9575,.T.);
#13801=ORIENTED_EDGE('',*,*,#9576,.F.);
#13802=ORIENTED_EDGE('',*,*,#9577,.F.);
#13803=ORIENTED_EDGE('',*,*,#9578,.F.);
#13804=ORIENTED_EDGE('',*,*,#9572,.T.);
#13805=ORIENTED_EDGE('',*,*,#9579,.T.);
#13806=ORIENTED_EDGE('',*,*,#9580,.T.);
#13807=ORIENTED_EDGE('',*,*,#9581,.F.);
#13808=ORIENTED_EDGE('',*,*,#9582,.F.);
#13809=ORIENTED_EDGE('',*,*,#9576,.T.);
#13810=ORIENTED_EDGE('',*,*,#9583,.T.);
#13811=ORIENTED_EDGE('',*,*,#9584,.T.);
#13812=ORIENTED_EDGE('',*,*,#9585,.F.);
#13813=ORIENTED_EDGE('',*,*,#9586,.F.);
#13814=ORIENTED_EDGE('',*,*,#9587,.F.);
#13815=ORIENTED_EDGE('',*,*,#9581,.T.);
#13816=ORIENTED_EDGE('',*,*,#9588,.T.);
#13817=ORIENTED_EDGE('',*,*,#9589,.T.);
#13818=ORIENTED_EDGE('',*,*,#9590,.F.);
#13819=ORIENTED_EDGE('',*,*,#9591,.T.);
#13820=ORIENTED_EDGE('',*,*,#9592,.T.);
#13821=ORIENTED_EDGE('',*,*,#9590,.T.);
#13822=ORIENTED_EDGE('',*,*,#9593,.T.);
#13823=ORIENTED_EDGE('',*,*,#9594,.F.);
#13824=ORIENTED_EDGE('',*,*,#9595,.T.);
#13825=ORIENTED_EDGE('',*,*,#9596,.T.);
#13826=ORIENTED_EDGE('',*,*,#9597,.T.);
#13827=ORIENTED_EDGE('',*,*,#9594,.T.);
#13828=ORIENTED_EDGE('',*,*,#9598,.T.);
#13829=ORIENTED_EDGE('',*,*,#9599,.T.);
#13830=ORIENTED_EDGE('',*,*,#9600,.T.);
#13831=ORIENTED_EDGE('',*,*,#9601,.T.);
#13832=ORIENTED_EDGE('',*,*,#9602,.T.);
#13833=ORIENTED_EDGE('',*,*,#9603,.T.);
#13834=ORIENTED_EDGE('',*,*,#9604,.T.);
#13835=ORIENTED_EDGE('',*,*,#9605,.T.);
#13836=ORIENTED_EDGE('',*,*,#9606,.T.);
#13837=ORIENTED_EDGE('',*,*,#9607,.T.);
#13838=ORIENTED_EDGE('',*,*,#9608,.T.);
#13839=ORIENTED_EDGE('',*,*,#9609,.T.);
#13840=ORIENTED_EDGE('',*,*,#9610,.F.);
#13841=ORIENTED_EDGE('',*,*,#9611,.F.);
#13842=ORIENTED_EDGE('',*,*,#9612,.T.);
#13843=ORIENTED_EDGE('',*,*,#9613,.T.);
#13844=ORIENTED_EDGE('',*,*,#9614,.T.);
#13845=ORIENTED_EDGE('',*,*,#9615,.T.);
#13846=ORIENTED_EDGE('',*,*,#9616,.T.);
#13847=ORIENTED_EDGE('',*,*,#9617,.T.);
#13848=ORIENTED_EDGE('',*,*,#9618,.T.);
#13849=ORIENTED_EDGE('',*,*,#9619,.T.);
#13850=ORIENTED_EDGE('',*,*,#9620,.T.);
#13851=ORIENTED_EDGE('',*,*,#9621,.T.);
#13852=ORIENTED_EDGE('',*,*,#9585,.T.);
#13853=ORIENTED_EDGE('',*,*,#9622,.T.);
#13854=ORIENTED_EDGE('',*,*,#9623,.T.);
#13855=ORIENTED_EDGE('',*,*,#9624,.F.);
#13856=ORIENTED_EDGE('',*,*,#9625,.F.);
#13857=ORIENTED_EDGE('',*,*,#9595,.F.);
#13858=ORIENTED_EDGE('',*,*,#9597,.F.);
#13859=ORIENTED_EDGE('',*,*,#9621,.F.);
#13860=ORIENTED_EDGE('',*,*,#9620,.F.);
#13861=ORIENTED_EDGE('',*,*,#9619,.F.);
#13862=ORIENTED_EDGE('',*,*,#9618,.F.);
#13863=ORIENTED_EDGE('',*,*,#9617,.F.);
#13864=ORIENTED_EDGE('',*,*,#9616,.F.);
#13865=ORIENTED_EDGE('',*,*,#9615,.F.);
#13866=ORIENTED_EDGE('',*,*,#9614,.F.);
#13867=ORIENTED_EDGE('',*,*,#9613,.F.);
#13868=ORIENTED_EDGE('',*,*,#9612,.F.);
#13869=ORIENTED_EDGE('',*,*,#9626,.F.);
#13870=ORIENTED_EDGE('',*,*,#9623,.F.);
#13871=ORIENTED_EDGE('',*,*,#9622,.F.);
#13872=ORIENTED_EDGE('',*,*,#9589,.F.);
#13873=ORIENTED_EDGE('',*,*,#9588,.F.);
#13874=ORIENTED_EDGE('',*,*,#9584,.F.);
#13875=ORIENTED_EDGE('',*,*,#9583,.F.);
#13876=ORIENTED_EDGE('',*,*,#9580,.F.);
#13877=ORIENTED_EDGE('',*,*,#9579,.F.);
#13878=ORIENTED_EDGE('',*,*,#9575,.F.);
#13879=ORIENTED_EDGE('',*,*,#9574,.F.);
#13880=ORIENTED_EDGE('',*,*,#9571,.F.);
#13881=ORIENTED_EDGE('',*,*,#9570,.F.);
#13882=ORIENTED_EDGE('',*,*,#9566,.F.);
#13883=ORIENTED_EDGE('',*,*,#9565,.F.);
#13884=ORIENTED_EDGE('',*,*,#9562,.F.);
#13885=ORIENTED_EDGE('',*,*,#9561,.F.);
#13886=ORIENTED_EDGE('',*,*,#9557,.F.);
#13887=ORIENTED_EDGE('',*,*,#9556,.F.);
#13888=ORIENTED_EDGE('',*,*,#9553,.F.);
#13889=ORIENTED_EDGE('',*,*,#9552,.F.);
#13890=ORIENTED_EDGE('',*,*,#9627,.F.);
#13891=ORIENTED_EDGE('',*,*,#9628,.F.);
#13892=ORIENTED_EDGE('',*,*,#9629,.T.);
#13893=ORIENTED_EDGE('',*,*,#9624,.T.);
#13894=ORIENTED_EDGE('',*,*,#9626,.T.);
#13895=ORIENTED_EDGE('',*,*,#9592,.F.);
#13896=ORIENTED_EDGE('',*,*,#9630,.F.);
#13897=ORIENTED_EDGE('',*,*,#9546,.T.);
#13898=ORIENTED_EDGE('',*,*,#9550,.T.);
#13899=ORIENTED_EDGE('',*,*,#9549,.T.);
#13900=ORIENTED_EDGE('',*,*,#9555,.T.);
#13901=ORIENTED_EDGE('',*,*,#9560,.T.);
#13902=ORIENTED_EDGE('',*,*,#9559,.T.);
#13903=ORIENTED_EDGE('',*,*,#9564,.T.);
#13904=ORIENTED_EDGE('',*,*,#9569,.T.);
#13905=ORIENTED_EDGE('',*,*,#9568,.T.);
#13906=ORIENTED_EDGE('',*,*,#9573,.T.);
#13907=ORIENTED_EDGE('',*,*,#9578,.T.);
#13908=ORIENTED_EDGE('',*,*,#9577,.T.);
#13909=ORIENTED_EDGE('',*,*,#9582,.T.);
#13910=ORIENTED_EDGE('',*,*,#9587,.T.);
#13911=ORIENTED_EDGE('',*,*,#9586,.T.);
#13912=ORIENTED_EDGE('',*,*,#9625,.T.);
#13913=ORIENTED_EDGE('',*,*,#9629,.F.);
#13914=ORIENTED_EDGE('',*,*,#9631,.F.);
#13915=ORIENTED_EDGE('',*,*,#9609,.F.);
#13916=ORIENTED_EDGE('',*,*,#9608,.F.);
#13917=ORIENTED_EDGE('',*,*,#9607,.F.);
#13918=ORIENTED_EDGE('',*,*,#9606,.F.);
#13919=ORIENTED_EDGE('',*,*,#9605,.F.);
#13920=ORIENTED_EDGE('',*,*,#9604,.F.);
#13921=ORIENTED_EDGE('',*,*,#9603,.F.);
#13922=ORIENTED_EDGE('',*,*,#9602,.F.);
#13923=ORIENTED_EDGE('',*,*,#9601,.F.);
#13924=ORIENTED_EDGE('',*,*,#9600,.F.);
#13925=ORIENTED_EDGE('',*,*,#9599,.F.);
#13926=ORIENTED_EDGE('',*,*,#9598,.F.);
#13927=ORIENTED_EDGE('',*,*,#9593,.F.);
#13928=ORIENTED_EDGE('',*,*,#9627,.T.);
#13929=ORIENTED_EDGE('',*,*,#9551,.T.);
#13930=ORIENTED_EDGE('',*,*,#9547,.T.);
#13931=ORIENTED_EDGE('',*,*,#9630,.T.);
#13932=ORIENTED_EDGE('',*,*,#9591,.F.);
#13933=ORIENTED_EDGE('',*,*,#9596,.F.);
#13934=ORIENTED_EDGE('',*,*,#9632,.T.);
#13935=ORIENTED_EDGE('',*,*,#9633,.T.);
#13936=ORIENTED_EDGE('',*,*,#9610,.T.);
#13937=ORIENTED_EDGE('',*,*,#9631,.T.);
#13938=ORIENTED_EDGE('',*,*,#9628,.T.);
#13939=ORIENTED_EDGE('',*,*,#9611,.T.);
#13940=ORIENTED_EDGE('',*,*,#9633,.F.);
#13941=ORIENTED_EDGE('',*,*,#9634,.F.);
#13942=ORIENTED_EDGE('',*,*,#9632,.F.);
#13943=ORIENTED_EDGE('',*,*,#9635,.F.);
#13944=ORIENTED_EDGE('',*,*,#9636,.F.);
#13945=ORIENTED_EDGE('',*,*,#9637,.F.);
#13946=ORIENTED_EDGE('',*,*,#9638,.F.);
#13947=ORIENTED_EDGE('',*,*,#9639,.F.);
#13948=ORIENTED_EDGE('',*,*,#9640,.F.);
#13949=ORIENTED_EDGE('',*,*,#9641,.F.);
#13950=ORIENTED_EDGE('',*,*,#9642,.F.);
#13951=ORIENTED_EDGE('',*,*,#9643,.F.);
#13952=ORIENTED_EDGE('',*,*,#9644,.F.);
#13953=ORIENTED_EDGE('',*,*,#9645,.F.);
#13954=ORIENTED_EDGE('',*,*,#9646,.F.);
#13955=ORIENTED_EDGE('',*,*,#9647,.T.);
#13956=ORIENTED_EDGE('',*,*,#9636,.T.);
#13957=ORIENTED_EDGE('',*,*,#9646,.T.);
#13958=ORIENTED_EDGE('',*,*,#9644,.T.);
#13959=ORIENTED_EDGE('',*,*,#9642,.T.);
#13960=ORIENTED_EDGE('',*,*,#9640,.T.);
#13961=ORIENTED_EDGE('',*,*,#9638,.T.);
#13962=ORIENTED_EDGE('',*,*,#9647,.F.);
#13963=ORIENTED_EDGE('',*,*,#9648,.F.);
#13964=ORIENTED_EDGE('',*,*,#9649,.T.);
#13965=ORIENTED_EDGE('',*,*,#9635,.T.);
#13966=ORIENTED_EDGE('',*,*,#9650,.F.);
#13967=ORIENTED_EDGE('',*,*,#9651,.F.);
#13968=ORIENTED_EDGE('',*,*,#9650,.T.);
#13969=ORIENTED_EDGE('',*,*,#9637,.T.);
#13970=ORIENTED_EDGE('',*,*,#9652,.F.);
#13971=ORIENTED_EDGE('',*,*,#9653,.F.);
#13972=ORIENTED_EDGE('',*,*,#9652,.T.);
#13973=ORIENTED_EDGE('',*,*,#9639,.T.);
#13974=ORIENTED_EDGE('',*,*,#9654,.F.);
#13975=ORIENTED_EDGE('',*,*,#9655,.F.);
#13976=ORIENTED_EDGE('',*,*,#9654,.T.);
#13977=ORIENTED_EDGE('',*,*,#9641,.T.);
#13978=ORIENTED_EDGE('',*,*,#9656,.F.);
#13979=ORIENTED_EDGE('',*,*,#9657,.F.);
#13980=ORIENTED_EDGE('',*,*,#9658,.T.);
#13981=ORIENTED_EDGE('',*,*,#9645,.T.);
#13982=ORIENTED_EDGE('',*,*,#9649,.F.);
#13983=ORIENTED_EDGE('',*,*,#9659,.F.);
#13984=ORIENTED_EDGE('',*,*,#9656,.T.);
#13985=ORIENTED_EDGE('',*,*,#9643,.T.);
#13986=ORIENTED_EDGE('',*,*,#9658,.F.);
#13987=ORIENTED_EDGE('',*,*,#9660,.F.);
#13988=ORIENTED_EDGE('',*,*,#9661,.T.);
#13989=ORIENTED_EDGE('',*,*,#9634,.T.);
#13990=ORIENTED_EDGE('',*,*,#9661,.F.);
#13991=ORIENTED_EDGE('',*,*,#9651,.T.);
#13992=ORIENTED_EDGE('',*,*,#9653,.T.);
#13993=ORIENTED_EDGE('',*,*,#9655,.T.);
#13994=ORIENTED_EDGE('',*,*,#9659,.T.);
#13995=ORIENTED_EDGE('',*,*,#9657,.T.);
#13996=ORIENTED_EDGE('',*,*,#9648,.T.);
#13997=ORIENTED_EDGE('',*,*,#9662,.T.);
#13998=ORIENTED_EDGE('',*,*,#9660,.T.);
#13999=ORIENTED_EDGE('',*,*,#9662,.F.);
#14000=ORIENTED_EDGE('',*,*,#9663,.F.);
#14001=ORIENTED_EDGE('',*,*,#9664,.F.);
#14002=ORIENTED_EDGE('',*,*,#9665,.F.);
#14003=ORIENTED_EDGE('',*,*,#9666,.F.);
#14004=ORIENTED_EDGE('',*,*,#9667,.F.);
#14005=ORIENTED_EDGE('',*,*,#9663,.T.);
#14006=ORIENTED_EDGE('',*,*,#9668,.F.);
#14007=ORIENTED_EDGE('',*,*,#9669,.T.);
#14008=ORIENTED_EDGE('',*,*,#9670,.T.);
#14009=ORIENTED_EDGE('',*,*,#9671,.F.);
#14010=ORIENTED_EDGE('',*,*,#9672,.F.);
#14011=ORIENTED_EDGE('',*,*,#9666,.T.);
#14012=ORIENTED_EDGE('',*,*,#9673,.T.);
#14013=ORIENTED_EDGE('',*,*,#9674,.T.);
#14014=ORIENTED_EDGE('',*,*,#9675,.F.);
#14015=ORIENTED_EDGE('',*,*,#9676,.F.);
#14016=ORIENTED_EDGE('',*,*,#9671,.T.);
#14017=ORIENTED_EDGE('',*,*,#9677,.T.);
#14018=ORIENTED_EDGE('',*,*,#9678,.T.);
#14019=ORIENTED_EDGE('',*,*,#9679,.F.);
#14020=ORIENTED_EDGE('',*,*,#9680,.F.);
#14021=ORIENTED_EDGE('',*,*,#9675,.T.);
#14022=ORIENTED_EDGE('',*,*,#9681,.T.);
#14023=ORIENTED_EDGE('',*,*,#9682,.T.);
#14024=ORIENTED_EDGE('',*,*,#9683,.F.);
#14025=ORIENTED_EDGE('',*,*,#9684,.F.);
#14026=ORIENTED_EDGE('',*,*,#9685,.F.);
#14027=ORIENTED_EDGE('',*,*,#9679,.T.);
#14028=ORIENTED_EDGE('',*,*,#9686,.T.);
#14029=ORIENTED_EDGE('',*,*,#9687,.T.);
#14030=ORIENTED_EDGE('',*,*,#9688,.F.);
#14031=ORIENTED_EDGE('',*,*,#9689,.F.);
#14032=ORIENTED_EDGE('',*,*,#9683,.T.);
#14033=ORIENTED_EDGE('',*,*,#9690,.T.);
#14034=ORIENTED_EDGE('',*,*,#9691,.T.);
#14035=ORIENTED_EDGE('',*,*,#9692,.F.);
#14036=ORIENTED_EDGE('',*,*,#9693,.F.);
#14037=ORIENTED_EDGE('',*,*,#9694,.F.);
#14038=ORIENTED_EDGE('',*,*,#9688,.T.);
#14039=ORIENTED_EDGE('',*,*,#9695,.T.);
#14040=ORIENTED_EDGE('',*,*,#9696,.T.);
#14041=ORIENTED_EDGE('',*,*,#9697,.F.);
#14042=ORIENTED_EDGE('',*,*,#9698,.F.);
#14043=ORIENTED_EDGE('',*,*,#9692,.T.);
#14044=ORIENTED_EDGE('',*,*,#9699,.T.);
#14045=ORIENTED_EDGE('',*,*,#9700,.T.);
#14046=ORIENTED_EDGE('',*,*,#9701,.F.);
#14047=ORIENTED_EDGE('',*,*,#9702,.F.);
#14048=ORIENTED_EDGE('',*,*,#9703,.F.);
#14049=ORIENTED_EDGE('',*,*,#9697,.T.);
#14050=ORIENTED_EDGE('',*,*,#9704,.T.);
#14051=ORIENTED_EDGE('',*,*,#9705,.T.);
#14052=ORIENTED_EDGE('',*,*,#9706,.F.);
#14053=ORIENTED_EDGE('',*,*,#9707,.F.);
#14054=ORIENTED_EDGE('',*,*,#9701,.T.);
#14055=ORIENTED_EDGE('',*,*,#9708,.T.);
#14056=ORIENTED_EDGE('',*,*,#9709,.T.);
#14057=ORIENTED_EDGE('',*,*,#9710,.F.);
#14058=ORIENTED_EDGE('',*,*,#9711,.F.);
#14059=ORIENTED_EDGE('',*,*,#9712,.F.);
#14060=ORIENTED_EDGE('',*,*,#9706,.T.);
#14061=ORIENTED_EDGE('',*,*,#9713,.T.);
#14062=ORIENTED_EDGE('',*,*,#9714,.T.);
#14063=ORIENTED_EDGE('',*,*,#9715,.T.);
#14064=ORIENTED_EDGE('',*,*,#9716,.T.);
#14065=ORIENTED_EDGE('',*,*,#9717,.T.);
#14066=ORIENTED_EDGE('',*,*,#9718,.T.);
#14067=ORIENTED_EDGE('',*,*,#9719,.T.);
#14068=ORIENTED_EDGE('',*,*,#9720,.T.);
#14069=ORIENTED_EDGE('',*,*,#9721,.T.);
#14070=ORIENTED_EDGE('',*,*,#9722,.T.);
#14071=ORIENTED_EDGE('',*,*,#9723,.T.);
#14072=ORIENTED_EDGE('',*,*,#9724,.T.);
#14073=ORIENTED_EDGE('',*,*,#9725,.T.);
#14074=ORIENTED_EDGE('',*,*,#9726,.T.);
#14075=ORIENTED_EDGE('',*,*,#9727,.T.);
#14076=ORIENTED_EDGE('',*,*,#9728,.T.);
#14077=ORIENTED_EDGE('',*,*,#9729,.T.);
#14078=ORIENTED_EDGE('',*,*,#9730,.T.);
#14079=ORIENTED_EDGE('',*,*,#9731,.F.);
#14080=ORIENTED_EDGE('',*,*,#9732,.T.);
#14081=ORIENTED_EDGE('',*,*,#9733,.T.);
#14082=ORIENTED_EDGE('',*,*,#9734,.T.);
#14083=ORIENTED_EDGE('',*,*,#9735,.T.);
#14084=ORIENTED_EDGE('',*,*,#9736,.T.);
#14085=ORIENTED_EDGE('',*,*,#9737,.T.);
#14086=ORIENTED_EDGE('',*,*,#9738,.T.);
#14087=ORIENTED_EDGE('',*,*,#9739,.T.);
#14088=ORIENTED_EDGE('',*,*,#9740,.T.);
#14089=ORIENTED_EDGE('',*,*,#9741,.T.);
#14090=ORIENTED_EDGE('',*,*,#9742,.T.);
#14091=ORIENTED_EDGE('',*,*,#9743,.T.);
#14092=ORIENTED_EDGE('',*,*,#9744,.T.);
#14093=ORIENTED_EDGE('',*,*,#9710,.T.);
#14094=ORIENTED_EDGE('',*,*,#9745,.T.);
#14095=ORIENTED_EDGE('',*,*,#9746,.T.);
#14096=ORIENTED_EDGE('',*,*,#9747,.F.);
#14097=ORIENTED_EDGE('',*,*,#9748,.F.);
#14098=ORIENTED_EDGE('',*,*,#9749,.F.);
#14099=ORIENTED_EDGE('',*,*,#9664,.T.);
#14100=ORIENTED_EDGE('',*,*,#9667,.T.);
#14101=ORIENTED_EDGE('',*,*,#9672,.T.);
#14102=ORIENTED_EDGE('',*,*,#9676,.T.);
#14103=ORIENTED_EDGE('',*,*,#9680,.T.);
#14104=ORIENTED_EDGE('',*,*,#9685,.T.);
#14105=ORIENTED_EDGE('',*,*,#9684,.T.);
#14106=ORIENTED_EDGE('',*,*,#9689,.T.);
#14107=ORIENTED_EDGE('',*,*,#9694,.T.);
#14108=ORIENTED_EDGE('',*,*,#9693,.T.);
#14109=ORIENTED_EDGE('',*,*,#9698,.T.);
#14110=ORIENTED_EDGE('',*,*,#9703,.T.);
#14111=ORIENTED_EDGE('',*,*,#9702,.T.);
#14112=ORIENTED_EDGE('',*,*,#9707,.T.);
#14113=ORIENTED_EDGE('',*,*,#9712,.T.);
#14114=ORIENTED_EDGE('',*,*,#9711,.T.);
#14115=ORIENTED_EDGE('',*,*,#9748,.T.);
#14116=ORIENTED_EDGE('',*,*,#9750,.F.);
#14117=ORIENTED_EDGE('',*,*,#9751,.F.);
#14118=ORIENTED_EDGE('',*,*,#9730,.F.);
#14119=ORIENTED_EDGE('',*,*,#9729,.F.);
#14120=ORIENTED_EDGE('',*,*,#9728,.F.);
#14121=ORIENTED_EDGE('',*,*,#9727,.F.);
#14122=ORIENTED_EDGE('',*,*,#9726,.F.);
#14123=ORIENTED_EDGE('',*,*,#9725,.F.);
#14124=ORIENTED_EDGE('',*,*,#9724,.F.);
#14125=ORIENTED_EDGE('',*,*,#9723,.F.);
#14126=ORIENTED_EDGE('',*,*,#9722,.F.);
#14127=ORIENTED_EDGE('',*,*,#9721,.F.);
#14128=ORIENTED_EDGE('',*,*,#9720,.F.);
#14129=ORIENTED_EDGE('',*,*,#9719,.F.);
#14130=ORIENTED_EDGE('',*,*,#9718,.F.);
#14131=ORIENTED_EDGE('',*,*,#9717,.F.);
#14132=ORIENTED_EDGE('',*,*,#9752,.F.);
#14133=ORIENTED_EDGE('',*,*,#9753,.F.);
#14134=ORIENTED_EDGE('',*,*,#9750,.T.);
#14135=ORIENTED_EDGE('',*,*,#9747,.T.);
#14136=ORIENTED_EDGE('',*,*,#9754,.T.);
#14137=ORIENTED_EDGE('',*,*,#9755,.F.);
#14138=ORIENTED_EDGE('',*,*,#9756,.F.);
#14139=ORIENTED_EDGE('',*,*,#9715,.F.);
#14140=ORIENTED_EDGE('',*,*,#9744,.F.);
#14141=ORIENTED_EDGE('',*,*,#9743,.F.);
#14142=ORIENTED_EDGE('',*,*,#9742,.F.);
#14143=ORIENTED_EDGE('',*,*,#9741,.F.);
#14144=ORIENTED_EDGE('',*,*,#9740,.F.);
#14145=ORIENTED_EDGE('',*,*,#9739,.F.);
#14146=ORIENTED_EDGE('',*,*,#9738,.F.);
#14147=ORIENTED_EDGE('',*,*,#9737,.F.);
#14148=ORIENTED_EDGE('',*,*,#9736,.F.);
#14149=ORIENTED_EDGE('',*,*,#9735,.F.);
#14150=ORIENTED_EDGE('',*,*,#9734,.F.);
#14151=ORIENTED_EDGE('',*,*,#9733,.F.);
#14152=ORIENTED_EDGE('',*,*,#9732,.F.);
#14153=ORIENTED_EDGE('',*,*,#9754,.F.);
#14154=ORIENTED_EDGE('',*,*,#9746,.F.);
#14155=ORIENTED_EDGE('',*,*,#9745,.F.);
#14156=ORIENTED_EDGE('',*,*,#9714,.F.);
#14157=ORIENTED_EDGE('',*,*,#9713,.F.);
#14158=ORIENTED_EDGE('',*,*,#9709,.F.);
#14159=ORIENTED_EDGE('',*,*,#9708,.F.);
#14160=ORIENTED_EDGE('',*,*,#9705,.F.);
#14161=ORIENTED_EDGE('',*,*,#9704,.F.);
#14162=ORIENTED_EDGE('',*,*,#9700,.F.);
#14163=ORIENTED_EDGE('',*,*,#9699,.F.);
#14164=ORIENTED_EDGE('',*,*,#9696,.F.);
#14165=ORIENTED_EDGE('',*,*,#9695,.F.);
#14166=ORIENTED_EDGE('',*,*,#9691,.F.);
#14167=ORIENTED_EDGE('',*,*,#9690,.F.);
#14168=ORIENTED_EDGE('',*,*,#9687,.F.);
#14169=ORIENTED_EDGE('',*,*,#9686,.F.);
#14170=ORIENTED_EDGE('',*,*,#9682,.F.);
#14171=ORIENTED_EDGE('',*,*,#9681,.F.);
#14172=ORIENTED_EDGE('',*,*,#9678,.F.);
#14173=ORIENTED_EDGE('',*,*,#9677,.F.);
#14174=ORIENTED_EDGE('',*,*,#9674,.F.);
#14175=ORIENTED_EDGE('',*,*,#9673,.F.);
#14176=ORIENTED_EDGE('',*,*,#9670,.F.);
#14177=ORIENTED_EDGE('',*,*,#9669,.F.);
#14178=ORIENTED_EDGE('',*,*,#9757,.T.);
#14179=ORIENTED_EDGE('',*,*,#9758,.T.);
#14180=ORIENTED_EDGE('',*,*,#9755,.T.);
#14181=ORIENTED_EDGE('',*,*,#9731,.T.);
#14182=ORIENTED_EDGE('',*,*,#9751,.T.);
#14183=ORIENTED_EDGE('',*,*,#9753,.T.);
#14184=ORIENTED_EDGE('',*,*,#9758,.F.);
#14185=ORIENTED_EDGE('',*,*,#9759,.F.);
#14186=ORIENTED_EDGE('',*,*,#9757,.F.);
#14187=ORIENTED_EDGE('',*,*,#9760,.F.);
#14188=ORIENTED_EDGE('',*,*,#9761,.F.);
#14189=ORIENTED_EDGE('',*,*,#9762,.F.);
#14190=ORIENTED_EDGE('',*,*,#9763,.F.);
#14191=ORIENTED_EDGE('',*,*,#9764,.F.);
#14192=ORIENTED_EDGE('',*,*,#9765,.F.);
#14193=ORIENTED_EDGE('',*,*,#9763,.T.);
#14194=ORIENTED_EDGE('',*,*,#9766,.F.);
#14195=ORIENTED_EDGE('',*,*,#9767,.F.);
#14196=ORIENTED_EDGE('',*,*,#9768,.F.);
#14197=ORIENTED_EDGE('',*,*,#9769,.F.);
#14198=ORIENTED_EDGE('',*,*,#9770,.F.);
#14199=ORIENTED_EDGE('',*,*,#9771,.F.);
#14200=ORIENTED_EDGE('',*,*,#9772,.F.);
#14201=ORIENTED_EDGE('',*,*,#9773,.F.);
#14202=ORIENTED_EDGE('',*,*,#9774,.F.);
#14203=ORIENTED_EDGE('',*,*,#9761,.T.);
#14204=ORIENTED_EDGE('',*,*,#9760,.T.);
#14205=ORIENTED_EDGE('',*,*,#9775,.T.);
#14206=ORIENTED_EDGE('',*,*,#9759,.T.);
#14207=ORIENTED_EDGE('',*,*,#9775,.F.);
#14208=ORIENTED_EDGE('',*,*,#9764,.T.);
#14209=ORIENTED_EDGE('',*,*,#9765,.T.);
#14210=ORIENTED_EDGE('',*,*,#9776,.F.);
#14211=ORIENTED_EDGE('',*,*,#9766,.T.);
#14212=ORIENTED_EDGE('',*,*,#9762,.T.);
#14213=ORIENTED_EDGE('',*,*,#9774,.T.);
#14214=ORIENTED_EDGE('',*,*,#9777,.F.);
#14215=ORIENTED_EDGE('',*,*,#9770,.T.);
#14216=ORIENTED_EDGE('',*,*,#9768,.T.);
#14217=ORIENTED_EDGE('',*,*,#9778,.T.);
#14218=ORIENTED_EDGE('',*,*,#9772,.T.);
#14219=ORIENTED_EDGE('',*,*,#9779,.T.);
#14220=ORIENTED_EDGE('',*,*,#9769,.T.);
#14221=ORIENTED_EDGE('',*,*,#9778,.F.);
#14222=ORIENTED_EDGE('',*,*,#9767,.T.);
#14223=ORIENTED_EDGE('',*,*,#9776,.T.);
#14224=ORIENTED_EDGE('',*,*,#9780,.F.);
#14225=ORIENTED_EDGE('',*,*,#9780,.T.);
#14226=ORIENTED_EDGE('',*,*,#9781,.T.);
#14227=ORIENTED_EDGE('',*,*,#9752,.T.);
#14228=ORIENTED_EDGE('',*,*,#9716,.F.);
#14229=ORIENTED_EDGE('',*,*,#9756,.T.);
#14230=ORIENTED_EDGE('',*,*,#9668,.T.);
#14231=ORIENTED_EDGE('',*,*,#9665,.T.);
#14232=ORIENTED_EDGE('',*,*,#9749,.T.);
#14233=ORIENTED_EDGE('',*,*,#9781,.F.);
#14234=ORIENTED_EDGE('',*,*,#9771,.T.);
#14235=ORIENTED_EDGE('',*,*,#9777,.T.);
#14236=ORIENTED_EDGE('',*,*,#9773,.T.);
#14237=ORIENTED_EDGE('',*,*,#9779,.F.);
#14238=CONICAL_SURFACE('',#15207,2.89999999999999,0.785398163397463);
#14239=CONICAL_SURFACE('',#15216,2.9,0.785398163397441);
#14240=CONICAL_SURFACE('',#15220,2.9,0.785398163397434);
#14241=CONICAL_SURFACE('',#15224,2.9,0.785398163397434);
#14242=CONICAL_SURFACE('',#15228,2.89999999999999,0.785398163397463);
#14243=CONICAL_SURFACE('',#15237,2.9,0.785398163397441);
#14244=CONICAL_SURFACE('',#15241,2.9,0.785398163397434);
#14245=CONICAL_SURFACE('',#15245,2.9,0.785398163397434);
#14246=CONICAL_SURFACE('',#15249,3.24999999999999,0.785398163397438);
#14247=CONICAL_SURFACE('',#15262,3.24999999999999,0.785398163397438);
#14248=CONICAL_SURFACE('',#15266,3.25,0.785398163397449);
#14249=CONICAL_SURFACE('',#15270,3.25,0.785398163397449);
#14250=CONICAL_SURFACE('',#15274,3.25,0.785398163397449);
#14251=CONICAL_SURFACE('',#15278,3.25,0.785398163397449);
#14252=CONICAL_SURFACE('',#15282,3.24999999999999,0.785398163397438);
#14253=CONICAL_SURFACE('',#15286,3.24999999999999,0.785398163397438);
#14254=CONICAL_SURFACE('',#15290,1.525,1.02974425867665);
#14255=CONICAL_SURFACE('',#15291,1.525,1.02974425867665);
#14256=CONICAL_SURFACE('',#15292,1.525,1.02974425867666);
#14257=CONICAL_SURFACE('',#15293,1.525,1.02974425867666);
#14258=CONICAL_SURFACE('',#15294,1.525,1.02974425867665);
#14259=CONICAL_SURFACE('',#15295,1.525,1.02974425867665);
#14260=CONICAL_SURFACE('',#15296,1.525,1.02974425867665);
#14261=CONICAL_SURFACE('',#15297,1.525,1.02974425867665);
#14262=CONICAL_SURFACE('',#15328,2.7,0.785398163397448);
#14263=CONICAL_SURFACE('',#15332,5.15000000000001,0.785398163397478);
#14264=CONICAL_SURFACE('',#15338,2.7,0.785398163397448);
#14265=CONICAL_SURFACE('',#15342,5.15,0.785398163397448);
#14266=CONICAL_SURFACE('',#15348,2.7,0.785398163397463);
#14267=CONICAL_SURFACE('',#15352,5.15,0.785398163397463);
#14268=CONICAL_SURFACE('',#15377,2.7,0.785398163397438);
#14269=CONICAL_SURFACE('',#15381,5.15000000000001,0.785398163397467);
#14270=CONICAL_SURFACE('',#15387,2.7,0.785398163397438);
#14271=CONICAL_SURFACE('',#15391,5.15,0.785398163397438);
#14272=CONICAL_SURFACE('',#15397,2.7,0.785398163397452);
#14273=CONICAL_SURFACE('',#15401,5.15,0.785398163397452);
#14274=CONICAL_SURFACE('',#15426,2.2,0.785398163397419);
#14275=CONICAL_SURFACE('',#15436,2.2,0.78539816339743);
#14276=CONICAL_SURFACE('',#15441,2.2,0.785398163397434);
#14277=CONICAL_SURFACE('',#15446,2.2,0.785398163397429);
#14278=CONICAL_SURFACE('',#15451,1.025,1.02974425867666);
#14279=CONICAL_SURFACE('',#15452,1.025,1.02974425867666);
#14280=CONICAL_SURFACE('',#15453,1.025,1.02974425867666);
#14281=CONICAL_SURFACE('',#15454,1.025,1.02974425867666);
#14282=CONICAL_SURFACE('',#15455,2.2,0.785398163397438);
#14283=CONICAL_SURFACE('',#15465,2.2,0.785398163397449);
#14284=CONICAL_SURFACE('',#15470,2.2,0.785398163397452);
#14285=CONICAL_SURFACE('',#15475,2.2,0.785398163397448);
#14286=CONICAL_SURFACE('',#15480,2.05,1.02974425867665);
#14287=CONICAL_SURFACE('',#15481,2.05,1.02974425867665);
#14288=CONICAL_SURFACE('',#15482,2.05,1.02974425867665);
#14289=CONICAL_SURFACE('',#15483,2.05,1.02974425867665);
#14290=CONICAL_SURFACE('',#15484,3.24999999999999,0.785398163397437);
#14291=CONICAL_SURFACE('',#15503,3.24999999999999,0.785398163397437);
#14292=CONICAL_SURFACE('',#15507,3.24999999999999,0.785398163397437);
#14293=CONICAL_SURFACE('',#15511,3.25,0.785398163397448);
#14294=CONICAL_SURFACE('',#15515,3.25,0.785398163397448);
#14295=CONICAL_SURFACE('',#15519,3.24999999999999,0.785398163397437);
#14296=CONICAL_SURFACE('',#15523,3.05000000000001,1.02974425867666);
#14297=CONICAL_SURFACE('',#15524,3.05000000000001,1.02974425867666);
#14298=CONICAL_SURFACE('',#15525,3.05,1.02974425867665);
#14299=CONICAL_SURFACE('',#15526,3.05,1.02974425867665);
#14300=CONICAL_SURFACE('',#15527,3.05,1.02974425867665);
#14301=CONICAL_SURFACE('',#15528,3.05,1.02974425867665);
#14302=CONICAL_SURFACE('',#15529,5.65000000000001,0.785398163397463);
#14303=CONICAL_SURFACE('',#15533,5.65,0.785398163397434);
#14304=CONICAL_SURFACE('',#15537,5.65,0.785398163397441);
#14305=CONICAL_SURFACE('',#15541,5.65,0.785398163397434);
#14306=CONICAL_SURFACE('',#15545,5.65,0.785398163397441);
#14307=CONICAL_SURFACE('',#15549,5.65,0.785398163397434);
#14308=CONICAL_SURFACE('',#15553,5.65,0.785398163397434);
#14309=CONICAL_SURFACE('',#15557,5.65000000000001,0.785398163397463);
#14310=CONICAL_SURFACE('',#15615,1.65,0.785398163397459);
#14311=CONICAL_SURFACE('',#15622,0.775000000000001,1.02974425867665);
#14312=CONICAL_SURFACE('',#15623,1.65,0.785398163397448);
#14313=CONICAL_SURFACE('',#15630,1.55,1.02974425867665);
#14314=CONICAL_SURFACE('',#15631,2.7,0.785398163397441);
#14315=CONICAL_SURFACE('',#15647,2.7,0.785398163397441);
#14316=CONICAL_SURFACE('',#15659,2.7,0.785398163397456);
#14317=CONICAL_SURFACE('',#15706,1.65,0.785398163397459);
#14318=CONICAL_SURFACE('',#15714,0.775000000000001,1.02974425867665);
#14319=CONICAL_SURFACE('',#15715,1.65,0.785398163397448);
#14320=CONICAL_SURFACE('',#15723,1.55,1.02974425867665);
#14321=CONICAL_SURFACE('',#15724,2.7,0.785398163397471);
#14322=CONICAL_SURFACE('',#15741,2.7,0.785398163397448);
#14323=CONICAL_SURFACE('',#15753,2.7,0.785398163397441);
#14324=CONICAL_SURFACE('',#15765,2.7,0.785398163397441);
#14325=CONICAL_SURFACE('',#16078,2.85,0.785398163397441);
#14326=CONICAL_SURFACE('',#16082,2.85,0.785398163397434);
#14327=CONICAL_SURFACE('',#16127,2.2005,0.785398163397448);
#14328=CONICAL_SURFACE('',#16211,4.05,0.785398163397448);
#14329=CONICAL_SURFACE('',#16319,2.40940107675851,0.785398163397453);
#14330=CONICAL_SURFACE('',#16359,2.30940107675851,1.02974425867666);
#14331=CONICAL_SURFACE('',#16399,1.49337567297406,0.785398163397437);
#14332=CONICAL_SURFACE('',#16440,1.44337567297407,1.02974425867665);
#14333=CONICAL_SURFACE('',#16446,2.26,0.785398163397448);
#14334=CONICAL_SURFACE('',#16447,2.125,0.785398163397448);
#14335=CONICAL_SURFACE('',#16463,2.25,0.785398163397448);
#14336=CONICAL_SURFACE('',#16465,2.25,0.785398163397448);
#14337=CONICAL_SURFACE('',#16495,0.866025403784438,1.02974425867665);
#14338=CONICAL_SURFACE('',#16553,2.55,0.785398163397459);
#14339=CONICAL_SURFACE('',#16556,1.325,0.785398163397496);
#14340=CONICAL_SURFACE('',#16557,2.55,0.785398163397459);
#14341=ADVANCED_FACE('',(#1606),#14238,.F.);
#14342=ADVANCED_FACE('',(#1607,#1083,#1084,#1085,#1086),#1211,.T.);
#14343=ADVANCED_FACE('',(#1608),#851,.F.);
#14344=ADVANCED_FACE('',(#1609),#14239,.F.);
#14345=ADVANCED_FACE('',(#1610),#852,.F.);
#14346=ADVANCED_FACE('',(#1611),#14240,.F.);
#14347=ADVANCED_FACE('',(#1612),#853,.F.);
#14348=ADVANCED_FACE('',(#1613),#14241,.F.);
#14349=ADVANCED_FACE('',(#1614),#854,.F.);
#14350=ADVANCED_FACE('',(#1615),#14242,.F.);
#14351=ADVANCED_FACE('',(#1616,#1087,#1088,#1089,#1090),#1212,.T.);
#14352=ADVANCED_FACE('',(#1617),#855,.F.);
#14353=ADVANCED_FACE('',(#1618),#14243,.F.);
#14354=ADVANCED_FACE('',(#1619),#856,.F.);
#14355=ADVANCED_FACE('',(#1620),#14244,.F.);
#14356=ADVANCED_FACE('',(#1621),#857,.F.);
#14357=ADVANCED_FACE('',(#1622),#14245,.F.);
#14358=ADVANCED_FACE('',(#1623),#858,.F.);
#14359=ADVANCED_FACE('',(#1624),#14246,.F.);
#14360=ADVANCED_FACE('',(#1625,#1091,#1092,#1093,#1094,#1095,#1096,#1097,
#1098),#1213,.T.);
#14361=ADVANCED_FACE('',(#1626),#859,.F.);
#14362=ADVANCED_FACE('',(#1627),#14247,.F.);
#14363=ADVANCED_FACE('',(#1628),#860,.F.);
#14364=ADVANCED_FACE('',(#1629),#14248,.F.);
#14365=ADVANCED_FACE('',(#1630),#861,.F.);
#14366=ADVANCED_FACE('',(#1631),#14249,.F.);
#14367=ADVANCED_FACE('',(#1632),#862,.F.);
#14368=ADVANCED_FACE('',(#1633),#14250,.F.);
#14369=ADVANCED_FACE('',(#1634),#863,.F.);
#14370=ADVANCED_FACE('',(#1635),#14251,.F.);
#14371=ADVANCED_FACE('',(#1636),#864,.F.);
#14372=ADVANCED_FACE('',(#1637),#14252,.F.);
#14373=ADVANCED_FACE('',(#1638),#865,.F.);
#14374=ADVANCED_FACE('',(#1639),#14253,.F.);
#14375=ADVANCED_FACE('',(#1640),#866,.F.);
#14376=ADVANCED_FACE('',(#1641),#14254,.F.);
#14377=ADVANCED_FACE('',(#1642),#14255,.F.);
#14378=ADVANCED_FACE('',(#1643),#14256,.F.);
#14379=ADVANCED_FACE('',(#1644),#14257,.F.);
#14380=ADVANCED_FACE('',(#1645),#14258,.F.);
#14381=ADVANCED_FACE('',(#1646),#14259,.F.);
#14382=ADVANCED_FACE('',(#1647),#14260,.F.);
#14383=ADVANCED_FACE('',(#1648),#14261,.F.);
#14384=ADVANCED_FACE('',(#1649),#1214,.T.);
#14385=ADVANCED_FACE('',(#1650),#1215,.T.);
#14386=ADVANCED_FACE('',(#1651),#1216,.T.);
#14387=ADVANCED_FACE('',(#1652),#1217,.T.);
#14388=ADVANCED_FACE('',(#1653),#1218,.T.);
#14389=ADVANCED_FACE('',(#1654),#1219,.T.);
#14390=ADVANCED_FACE('',(#1655),#1220,.T.);
#14391=ADVANCED_FACE('',(#1656),#1221,.T.);
#14392=ADVANCED_FACE('',(#1657),#1222,.T.);
#14393=ADVANCED_FACE('',(#1658),#1223,.T.);
#14394=ADVANCED_FACE('',(#1659),#1224,.T.);
#14395=ADVANCED_FACE('',(#1660),#1225,.F.);
#14396=ADVANCED_FACE('',(#1661),#1226,.T.);
#14397=ADVANCED_FACE('',(#1662),#1227,.T.);
#14398=ADVANCED_FACE('',(#1663),#1228,.T.);
#14399=ADVANCED_FACE('',(#1664),#1229,.T.);
#14400=ADVANCED_FACE('',(#1665),#1230,.T.);
#14401=ADVANCED_FACE('',(#1666),#1231,.T.);
#14402=ADVANCED_FACE('',(#1667,#1099,#1100,#1101,#1102),#1232,.T.);
#14403=ADVANCED_FACE('',(#1668),#1233,.T.);
#14404=ADVANCED_FACE('',(#1669),#1234,.T.);
#14405=ADVANCED_FACE('',(#1670),#1235,.T.);
#14406=ADVANCED_FACE('',(#1671),#1236,.T.);
#14407=ADVANCED_FACE('',(#1672),#1237,.T.);
#14408=ADVANCED_FACE('',(#1673),#1238,.T.);
#14409=ADVANCED_FACE('',(#1674),#1239,.T.);
#14410=ADVANCED_FACE('',(#1675,#1103,#1104,#1105,#1106),#1240,.T.);
#14411=ADVANCED_FACE('',(#1676),#1241,.T.);
#14412=ADVANCED_FACE('',(#1677),#1242,.T.);
#14413=ADVANCED_FACE('',(#1678),#14262,.F.);
#14414=ADVANCED_FACE('',(#1679),#14263,.F.);
#14415=ADVANCED_FACE('',(#1680),#867,.F.);
#14416=ADVANCED_FACE('',(#1681),#14264,.F.);
#14417=ADVANCED_FACE('',(#1682),#14265,.F.);
#14418=ADVANCED_FACE('',(#1683),#868,.F.);
#14419=ADVANCED_FACE('',(#1684),#14266,.F.);
#14420=ADVANCED_FACE('',(#1685),#14267,.F.);
#14421=ADVANCED_FACE('',(#1686),#869,.F.);
#14422=ADVANCED_FACE('',(#1687,#1107,#1108,#1109),#1243,.T.);
#14423=ADVANCED_FACE('',(#1688),#870,.F.);
#14424=ADVANCED_FACE('',(#1689),#871,.F.);
#14425=ADVANCED_FACE('',(#1690),#872,.F.);
#14426=ADVANCED_FACE('',(#1691,#1110),#1244,.T.);
#14427=ADVANCED_FACE('',(#1692,#1111),#1245,.T.);
#14428=ADVANCED_FACE('',(#1693,#1112),#1246,.T.);
#14429=ADVANCED_FACE('',(#1694),#873,.F.);
#14430=ADVANCED_FACE('',(#1695),#874,.F.);
#14431=ADVANCED_FACE('',(#1696),#875,.F.);
#14432=ADVANCED_FACE('',(#1697),#14268,.F.);
#14433=ADVANCED_FACE('',(#1698),#14269,.F.);
#14434=ADVANCED_FACE('',(#1699),#876,.F.);
#14435=ADVANCED_FACE('',(#1700),#14270,.F.);
#14436=ADVANCED_FACE('',(#1701),#14271,.F.);
#14437=ADVANCED_FACE('',(#1702),#877,.F.);
#14438=ADVANCED_FACE('',(#1703),#14272,.F.);
#14439=ADVANCED_FACE('',(#1704),#14273,.F.);
#14440=ADVANCED_FACE('',(#1705),#878,.F.);
#14441=ADVANCED_FACE('',(#1706,#1113,#1114,#1115),#1247,.T.);
#14442=ADVANCED_FACE('',(#1707),#879,.F.);
#14443=ADVANCED_FACE('',(#1708),#880,.F.);
#14444=ADVANCED_FACE('',(#1709),#881,.F.);
#14445=ADVANCED_FACE('',(#1710,#1116),#1248,.F.);
#14446=ADVANCED_FACE('',(#1711,#1117),#1249,.F.);
#14447=ADVANCED_FACE('',(#1712,#1118),#1250,.F.);
#14448=ADVANCED_FACE('',(#1713),#882,.F.);
#14449=ADVANCED_FACE('',(#1714),#883,.F.);
#14450=ADVANCED_FACE('',(#1715),#884,.F.);
#14451=ADVANCED_FACE('',(#1716),#14274,.F.);
#14452=ADVANCED_FACE('',(#1717,#1119,#1120,#1121,#1122),#1251,.T.);
#14453=ADVANCED_FACE('',(#1718),#885,.F.);
#14454=ADVANCED_FACE('',(#1719),#14275,.F.);
#14455=ADVANCED_FACE('',(#1720),#886,.F.);
#14456=ADVANCED_FACE('',(#1721),#14276,.F.);
#14457=ADVANCED_FACE('',(#1722),#887,.F.);
#14458=ADVANCED_FACE('',(#1723),#14277,.F.);
#14459=ADVANCED_FACE('',(#1724),#888,.F.);
#14460=ADVANCED_FACE('',(#1725),#14278,.F.);
#14461=ADVANCED_FACE('',(#1726),#14279,.F.);
#14462=ADVANCED_FACE('',(#1727),#14280,.F.);
#14463=ADVANCED_FACE('',(#1728),#14281,.F.);
#14464=ADVANCED_FACE('',(#1729),#14282,.F.);
#14465=ADVANCED_FACE('',(#1730,#1123,#1124,#1125,#1126),#1252,.F.);
#14466=ADVANCED_FACE('',(#1731),#889,.F.);
#14467=ADVANCED_FACE('',(#1732),#14283,.F.);
#14468=ADVANCED_FACE('',(#1733),#890,.F.);
#14469=ADVANCED_FACE('',(#1734),#14284,.F.);
#14470=ADVANCED_FACE('',(#1735),#891,.F.);
#14471=ADVANCED_FACE('',(#1736),#14285,.F.);
#14472=ADVANCED_FACE('',(#1737),#892,.F.);
#14473=ADVANCED_FACE('',(#1738),#14286,.F.);
#14474=ADVANCED_FACE('',(#1739),#14287,.F.);
#14475=ADVANCED_FACE('',(#1740),#14288,.F.);
#14476=ADVANCED_FACE('',(#1741),#14289,.F.);
#14477=ADVANCED_FACE('',(#1742),#14290,.F.);
#14478=ADVANCED_FACE('',(#1743,#1127,#1128,#1129,#1130,#1131,#1132,#1133,
#1134,#1135,#1136,#1137,#1138,#1139,#1140),#1253,.T.);
#14479=ADVANCED_FACE('',(#1744),#893,.F.);
#14480=ADVANCED_FACE('',(#1745),#14291,.F.);
#14481=ADVANCED_FACE('',(#1746),#894,.F.);
#14482=ADVANCED_FACE('',(#1747),#14292,.F.);
#14483=ADVANCED_FACE('',(#1748),#895,.F.);
#14484=ADVANCED_FACE('',(#1749),#14293,.F.);
#14485=ADVANCED_FACE('',(#1750),#896,.F.);
#14486=ADVANCED_FACE('',(#1751),#14294,.F.);
#14487=ADVANCED_FACE('',(#1752),#897,.F.);
#14488=ADVANCED_FACE('',(#1753),#14295,.F.);
#14489=ADVANCED_FACE('',(#1754),#898,.F.);
#14490=ADVANCED_FACE('',(#1755),#14296,.F.);
#14491=ADVANCED_FACE('',(#1756),#14297,.F.);
#14492=ADVANCED_FACE('',(#1757),#14298,.F.);
#14493=ADVANCED_FACE('',(#1758),#14299,.F.);
#14494=ADVANCED_FACE('',(#1759),#14300,.F.);
#14495=ADVANCED_FACE('',(#1760),#14301,.F.);
#14496=ADVANCED_FACE('',(#1761),#14302,.F.);
#14497=ADVANCED_FACE('',(#1762),#899,.F.);
#14498=ADVANCED_FACE('',(#1763),#14303,.F.);
#14499=ADVANCED_FACE('',(#1764),#900,.F.);
#14500=ADVANCED_FACE('',(#1765),#14304,.F.);
#14501=ADVANCED_FACE('',(#1766),#901,.F.);
#14502=ADVANCED_FACE('',(#1767),#14305,.F.);
#14503=ADVANCED_FACE('',(#1768),#902,.F.);
#14504=ADVANCED_FACE('',(#1769),#14306,.F.);
#14505=ADVANCED_FACE('',(#1770),#903,.F.);
#14506=ADVANCED_FACE('',(#1771),#14307,.F.);
#14507=ADVANCED_FACE('',(#1772),#904,.F.);
#14508=ADVANCED_FACE('',(#1773),#14308,.F.);
#14509=ADVANCED_FACE('',(#1774),#905,.F.);
#14510=ADVANCED_FACE('',(#1775),#14309,.F.);
#14511=ADVANCED_FACE('',(#1776),#906,.F.);
#14512=ADVANCED_FACE('',(#1777,#1141),#1254,.T.);
#14513=ADVANCED_FACE('',(#1778,#1142),#1255,.T.);
#14514=ADVANCED_FACE('',(#1779,#1143),#1256,.T.);
#14515=ADVANCED_FACE('',(#1780,#1144),#1257,.T.);
#14516=ADVANCED_FACE('',(#1781,#1145),#1258,.T.);
#14517=ADVANCED_FACE('',(#1782,#1146),#1259,.T.);
#14518=ADVANCED_FACE('',(#1783,#1147),#1260,.T.);
#14519=ADVANCED_FACE('',(#1784,#1148),#1261,.T.);
#14520=ADVANCED_FACE('',(#1785),#907,.F.);
#14521=ADVANCED_FACE('',(#1786),#908,.F.);
#14522=ADVANCED_FACE('',(#1787),#909,.F.);
#14523=ADVANCED_FACE('',(#1788),#910,.F.);
#14524=ADVANCED_FACE('',(#1789),#911,.F.);
#14525=ADVANCED_FACE('',(#1790),#912,.F.);
#14526=ADVANCED_FACE('',(#1791),#913,.F.);
#14527=ADVANCED_FACE('',(#1792),#914,.F.);
#14528=ADVANCED_FACE('',(#1793),#1262,.T.);
#14529=ADVANCED_FACE('',(#1794),#1263,.T.);
#14530=ADVANCED_FACE('',(#1795),#1264,.T.);
#14531=ADVANCED_FACE('',(#1796),#1265,.T.);
#14532=ADVANCED_FACE('',(#1797),#1266,.T.);
#14533=ADVANCED_FACE('',(#1798),#1267,.T.);
#14534=ADVANCED_FACE('',(#1799),#1268,.T.);
#14535=ADVANCED_FACE('',(#1800),#1269,.T.);
#14536=ADVANCED_FACE('',(#1801),#1270,.T.);
#14537=ADVANCED_FACE('',(#1802),#1271,.T.);
#14538=ADVANCED_FACE('',(#1803,#1149,#1150,#1151,#1152),#1272,.T.);
#14539=ADVANCED_FACE('',(#1804),#1273,.T.);
#14540=ADVANCED_FACE('',(#1805,#1153,#1154,#1155,#1156,#1157,#1158),#1274,
 .T.);
#14541=ADVANCED_FACE('',(#1806),#1275,.T.);
#14542=ADVANCED_FACE('',(#1807,#1159,#1160,#1161,#1162),#1276,.T.);
#14543=ADVANCED_FACE('',(#1808,#1163,#1164,#1165,#1166,#1167,#1168),#1277,
 .T.);
#14544=ADVANCED_FACE('',(#1809),#1278,.T.);
#14545=ADVANCED_FACE('',(#1810),#1279,.T.);
#14546=ADVANCED_FACE('',(#1811),#1280,.T.);
#14547=ADVANCED_FACE('',(#1812),#1281,.T.);
#14548=ADVANCED_FACE('',(#1813),#1282,.T.);
#14549=ADVANCED_FACE('',(#1814),#14310,.F.);
#14550=ADVANCED_FACE('',(#1815),#1283,.T.);
#14551=ADVANCED_FACE('',(#1816),#915,.F.);
#14552=ADVANCED_FACE('',(#1817),#14311,.F.);
#14553=ADVANCED_FACE('',(#1818),#14312,.F.);
#14554=ADVANCED_FACE('',(#1819),#1284,.F.);
#14555=ADVANCED_FACE('',(#1820),#916,.F.);
#14556=ADVANCED_FACE('',(#1821),#14313,.F.);
#14557=ADVANCED_FACE('',(#1822),#14314,.F.);
#14558=ADVANCED_FACE('',(#1823,#1169,#1170,#1171),#1285,.T.);
#14559=ADVANCED_FACE('',(#1824),#917,.F.);
#14560=ADVANCED_FACE('',(#1825),#14315,.F.);
#14561=ADVANCED_FACE('',(#1826),#918,.F.);
#14562=ADVANCED_FACE('',(#1827),#14316,.F.);
#14563=ADVANCED_FACE('',(#1828),#919,.F.);
#14564=ADVANCED_FACE('',(#1829),#1286,.F.);
#14565=ADVANCED_FACE('',(#1830),#1287,.F.);
#14566=ADVANCED_FACE('',(#1831),#1288,.F.);
#14567=ADVANCED_FACE('',(#1832),#1289,.F.);
#14568=ADVANCED_FACE('',(#1833),#1290,.F.);
#14569=ADVANCED_FACE('',(#1834),#1291,.F.);
#14570=ADVANCED_FACE('',(#1835),#1292,.T.);
#14571=ADVANCED_FACE('',(#1836),#1293,.T.);
#14572=ADVANCED_FACE('',(#1837),#1294,.T.);
#14573=ADVANCED_FACE('',(#1838),#1295,.T.);
#14574=ADVANCED_FACE('',(#1839),#1296,.T.);
#14575=ADVANCED_FACE('',(#1840),#1297,.T.);
#14576=ADVANCED_FACE('',(#1841),#1298,.T.);
#14577=ADVANCED_FACE('',(#1842),#1299,.T.);
#14578=ADVANCED_FACE('',(#1843),#1300,.T.);
#14579=ADVANCED_FACE('',(#1844),#1301,.T.);
#14580=ADVANCED_FACE('',(#1845),#1302,.T.);
#14581=ADVANCED_FACE('',(#1846),#1303,.T.);
#14582=ADVANCED_FACE('',(#1847),#1304,.T.);
#14583=ADVANCED_FACE('',(#1848),#1305,.T.);
#14584=ADVANCED_FACE('',(#1849),#1306,.T.);
#14585=ADVANCED_FACE('',(#1850),#1307,.T.);
#14586=ADVANCED_FACE('',(#1851),#1308,.T.);
#14587=ADVANCED_FACE('',(#1852),#1309,.T.);
#14588=ADVANCED_FACE('',(#1853),#1310,.T.);
#14589=ADVANCED_FACE('',(#1854),#1311,.T.);
#14590=ADVANCED_FACE('',(#1855),#1312,.T.);
#14591=ADVANCED_FACE('',(#1856),#1313,.T.);
#14592=ADVANCED_FACE('',(#1857),#1314,.T.);
#14593=ADVANCED_FACE('',(#1858),#1315,.T.);
#14594=ADVANCED_FACE('',(#1859),#1316,.T.);
#14595=ADVANCED_FACE('',(#1860),#1317,.T.);
#14596=ADVANCED_FACE('',(#1861),#1318,.T.);
#14597=ADVANCED_FACE('',(#1862),#1319,.T.);
#14598=ADVANCED_FACE('',(#1863),#14317,.F.);
#14599=ADVANCED_FACE('',(#1864),#1320,.T.);
#14600=ADVANCED_FACE('',(#1865),#920,.F.);
#14601=ADVANCED_FACE('',(#1866),#14318,.F.);
#14602=ADVANCED_FACE('',(#1867),#14319,.F.);
#14603=ADVANCED_FACE('',(#1868),#1321,.F.);
#14604=ADVANCED_FACE('',(#1869),#921,.F.);
#14605=ADVANCED_FACE('',(#1870),#14320,.F.);
#14606=ADVANCED_FACE('',(#1871),#14321,.F.);
#14607=ADVANCED_FACE('',(#1872,#1172,#1173,#1174,#1175),#1322,.T.);
#14608=ADVANCED_FACE('',(#1873),#922,.F.);
#14609=ADVANCED_FACE('',(#1874),#14322,.F.);
#14610=ADVANCED_FACE('',(#1875),#923,.F.);
#14611=ADVANCED_FACE('',(#1876),#14323,.F.);
#14612=ADVANCED_FACE('',(#1877),#924,.F.);
#14613=ADVANCED_FACE('',(#1878),#14324,.F.);
#14614=ADVANCED_FACE('',(#1879),#925,.F.);
#14615=ADVANCED_FACE('',(#1880),#1323,.T.);
#14616=ADVANCED_FACE('',(#1881),#1324,.T.);
#14617=ADVANCED_FACE('',(#1882),#1325,.T.);
#14618=ADVANCED_FACE('',(#1883),#1326,.T.);
#14619=ADVANCED_FACE('',(#1884),#1327,.T.);
#14620=ADVANCED_FACE('',(#1885),#1328,.T.);
#14621=ADVANCED_FACE('',(#1886),#1329,.T.);
#14622=ADVANCED_FACE('',(#1887),#1330,.T.);
#14623=ADVANCED_FACE('',(#1888),#1331,.T.);
#14624=ADVANCED_FACE('',(#1889),#1332,.T.);
#14625=ADVANCED_FACE('',(#1890),#1333,.T.);
#14626=ADVANCED_FACE('',(#1891),#1334,.T.);
#14627=ADVANCED_FACE('',(#1892),#1335,.T.);
#14628=ADVANCED_FACE('',(#1893),#1336,.T.);
#14629=ADVANCED_FACE('',(#1894),#1337,.T.);
#14630=ADVANCED_FACE('',(#1895),#1338,.T.);
#14631=ADVANCED_FACE('',(#1896),#1339,.T.);
#14632=ADVANCED_FACE('',(#1897),#1340,.T.);
#14633=ADVANCED_FACE('',(#1898),#1341,.T.);
#14634=ADVANCED_FACE('',(#1899),#1342,.T.);
#14635=ADVANCED_FACE('',(#1900),#1343,.T.);
#14636=ADVANCED_FACE('',(#1901),#1344,.T.);
#14637=ADVANCED_FACE('',(#1902),#1345,.T.);
#14638=ADVANCED_FACE('',(#1903),#1346,.T.);
#14639=ADVANCED_FACE('',(#1904),#1347,.T.);
#14640=ADVANCED_FACE('',(#1905),#1348,.T.);
#14641=ADVANCED_FACE('',(#1906),#1349,.T.);
#14642=ADVANCED_FACE('',(#1907),#1350,.T.);
#14643=ADVANCED_FACE('',(#1908),#1351,.T.);
#14644=ADVANCED_FACE('',(#1909),#1352,.T.);
#14645=ADVANCED_FACE('',(#1910),#1353,.T.);
#14646=ADVANCED_FACE('',(#1911),#1354,.T.);
#14647=ADVANCED_FACE('',(#1912),#1355,.T.);
#14648=ADVANCED_FACE('',(#1913),#1356,.T.);
#14649=ADVANCED_FACE('',(#1914),#1357,.T.);
#14650=ADVANCED_FACE('',(#1915),#1358,.T.);
#14651=ADVANCED_FACE('',(#1916),#1359,.T.);
#14652=ADVANCED_FACE('',(#1917),#1360,.T.);
#14653=ADVANCED_FACE('',(#1918),#1361,.T.);
#14654=ADVANCED_FACE('',(#1919),#1362,.F.);
#14655=ADVANCED_FACE('',(#1920),#926,.F.);
#14656=ADVANCED_FACE('',(#1921),#1363,.F.);
#14657=ADVANCED_FACE('',(#1922),#927,.F.);
#14658=ADVANCED_FACE('',(#1923),#1364,.F.);
#14659=ADVANCED_FACE('',(#1924),#928,.F.);
#14660=ADVANCED_FACE('',(#1925),#1365,.F.);
#14661=ADVANCED_FACE('',(#1926),#929,.F.);
#14662=ADVANCED_FACE('',(#1927),#1366,.F.);
#14663=ADVANCED_FACE('',(#1928),#930,.F.);
#14664=ADVANCED_FACE('',(#1929),#1367,.F.);
#14665=ADVANCED_FACE('',(#1930),#931,.F.);
#14666=ADVANCED_FACE('',(#1931),#1368,.F.);
#14667=ADVANCED_FACE('',(#1932),#932,.F.);
#14668=ADVANCED_FACE('',(#1933),#1369,.F.);
#14669=ADVANCED_FACE('',(#1934),#933,.F.);
#14670=ADVANCED_FACE('',(#1935),#1370,.F.);
#14671=ADVANCED_FACE('',(#1936),#934,.F.);
#14672=ADVANCED_FACE('',(#1937),#1371,.F.);
#14673=ADVANCED_FACE('',(#1938),#935,.F.);
#14674=ADVANCED_FACE('',(#1939),#1372,.F.);
#14675=ADVANCED_FACE('',(#1940),#936,.F.);
#14676=ADVANCED_FACE('',(#1941),#1373,.F.);
#14677=ADVANCED_FACE('',(#1942),#937,.F.);
#14678=ADVANCED_FACE('',(#1943),#1374,.F.);
#14679=ADVANCED_FACE('',(#1944),#938,.F.);
#14680=ADVANCED_FACE('',(#1945),#1375,.F.);
#14681=ADVANCED_FACE('',(#1946),#939,.F.);
#14682=ADVANCED_FACE('',(#1947),#1376,.F.);
#14683=ADVANCED_FACE('',(#1948),#940,.F.);
#14684=ADVANCED_FACE('',(#1949),#1377,.F.);
#14685=ADVANCED_FACE('',(#1950),#941,.F.);
#14686=ADVANCED_FACE('',(#1951),#1378,.F.);
#14687=ADVANCED_FACE('',(#1952),#942,.F.);
#14688=ADVANCED_FACE('',(#1953),#1379,.F.);
#14689=ADVANCED_FACE('',(#1954),#943,.F.);
#14690=ADVANCED_FACE('',(#1955),#1380,.F.);
#14691=ADVANCED_FACE('',(#1956),#944,.F.);
#14692=ADVANCED_FACE('',(#1957),#1381,.F.);
#14693=ADVANCED_FACE('',(#1958),#945,.F.);
#14694=ADVANCED_FACE('',(#1959),#1382,.F.);
#14695=ADVANCED_FACE('',(#1960),#946,.F.);
#14696=ADVANCED_FACE('',(#1961),#1383,.F.);
#14697=ADVANCED_FACE('',(#1962),#947,.F.);
#14698=ADVANCED_FACE('',(#1963),#1384,.F.);
#14699=ADVANCED_FACE('',(#1964),#948,.F.);
#14700=ADVANCED_FACE('',(#1965),#1385,.F.);
#14701=ADVANCED_FACE('',(#1966),#949,.F.);
#14702=ADVANCED_FACE('',(#1967),#1386,.F.);
#14703=ADVANCED_FACE('',(#1968),#950,.F.);
#14704=ADVANCED_FACE('',(#1969),#1387,.F.);
#14705=ADVANCED_FACE('',(#1970),#951,.F.);
#14706=ADVANCED_FACE('',(#1971),#1388,.F.);
#14707=ADVANCED_FACE('',(#1972),#952,.F.);
#14708=ADVANCED_FACE('',(#1973),#1389,.F.);
#14709=ADVANCED_FACE('',(#1974),#953,.F.);
#14710=ADVANCED_FACE('',(#1975),#1390,.F.);
#14711=ADVANCED_FACE('',(#1976),#954,.F.);
#14712=ADVANCED_FACE('',(#1977),#1391,.F.);
#14713=ADVANCED_FACE('',(#1978),#955,.F.);
#14714=ADVANCED_FACE('',(#1979),#1392,.F.);
#14715=ADVANCED_FACE('',(#1980),#956,.F.);
#14716=ADVANCED_FACE('',(#1981),#1393,.F.);
#14717=ADVANCED_FACE('',(#1982),#957,.F.);
#14718=ADVANCED_FACE('',(#1983),#1394,.F.);
#14719=ADVANCED_FACE('',(#1984),#958,.F.);
#14720=ADVANCED_FACE('',(#1985),#1395,.F.);
#14721=ADVANCED_FACE('',(#1986),#959,.F.);
#14722=ADVANCED_FACE('',(#1987),#1396,.F.);
#14723=ADVANCED_FACE('',(#1988),#960,.F.);
#14724=ADVANCED_FACE('',(#1989),#1397,.F.);
#14725=ADVANCED_FACE('',(#1990),#961,.F.);
#14726=ADVANCED_FACE('',(#1991),#1398,.F.);
#14727=ADVANCED_FACE('',(#1992),#962,.F.);
#14728=ADVANCED_FACE('',(#1993),#1399,.F.);
#14729=ADVANCED_FACE('',(#1994),#963,.F.);
#14730=ADVANCED_FACE('',(#1995),#1400,.F.);
#14731=ADVANCED_FACE('',(#1996),#964,.F.);
#14732=ADVANCED_FACE('',(#1997),#1401,.F.);
#14733=ADVANCED_FACE('',(#1998),#965,.F.);
#14734=ADVANCED_FACE('',(#1999),#1402,.F.);
#14735=ADVANCED_FACE('',(#2000),#966,.F.);
#14736=ADVANCED_FACE('',(#2001),#1403,.F.);
#14737=ADVANCED_FACE('',(#2002),#967,.F.);
#14738=ADVANCED_FACE('',(#2003),#1404,.F.);
#14739=ADVANCED_FACE('',(#2004),#968,.F.);
#14740=ADVANCED_FACE('',(#2005),#1405,.F.);
#14741=ADVANCED_FACE('',(#2006),#969,.F.);
#14742=ADVANCED_FACE('',(#2007),#1406,.F.);
#14743=ADVANCED_FACE('',(#2008),#970,.F.);
#14744=ADVANCED_FACE('',(#2009),#1407,.F.);
#14745=ADVANCED_FACE('',(#2010),#971,.F.);
#14746=ADVANCED_FACE('',(#2011),#1408,.F.);
#14747=ADVANCED_FACE('',(#2012),#972,.F.);
#14748=ADVANCED_FACE('',(#2013),#1409,.F.);
#14749=ADVANCED_FACE('',(#2014),#973,.F.);
#14750=ADVANCED_FACE('',(#2015),#1410,.F.);
#14751=ADVANCED_FACE('',(#2016),#974,.F.);
#14752=ADVANCED_FACE('',(#2017),#1411,.F.);
#14753=ADVANCED_FACE('',(#2018),#975,.F.);
#14754=ADVANCED_FACE('',(#2019),#1412,.F.);
#14755=ADVANCED_FACE('',(#2020),#976,.F.);
#14756=ADVANCED_FACE('',(#2021),#1413,.F.);
#14757=ADVANCED_FACE('',(#2022),#977,.F.);
#14758=ADVANCED_FACE('',(#2023),#1414,.F.);
#14759=ADVANCED_FACE('',(#2024),#978,.F.);
#14760=ADVANCED_FACE('',(#2025),#1415,.F.);
#14761=ADVANCED_FACE('',(#2026),#979,.F.);
#14762=ADVANCED_FACE('',(#2027),#1416,.F.);
#14763=ADVANCED_FACE('',(#2028),#980,.F.);
#14764=ADVANCED_FACE('',(#2029),#1417,.F.);
#14765=ADVANCED_FACE('',(#2030),#981,.F.);
#14766=ADVANCED_FACE('',(#2031),#1418,.F.);
#14767=ADVANCED_FACE('',(#2032),#982,.F.);
#14768=ADVANCED_FACE('',(#2033),#1419,.F.);
#14769=ADVANCED_FACE('',(#2034),#983,.F.);
#14770=ADVANCED_FACE('',(#2035),#1420,.F.);
#14771=ADVANCED_FACE('',(#2036),#984,.F.);
#14772=ADVANCED_FACE('',(#2037),#1421,.F.);
#14773=ADVANCED_FACE('',(#2038),#985,.F.);
#14774=ADVANCED_FACE('',(#2039),#1422,.T.);
#14775=ADVANCED_FACE('',(#2040),#986,.T.);
#14776=ADVANCED_FACE('',(#2041),#1423,.T.);
#14777=ADVANCED_FACE('',(#2042),#987,.T.);
#14778=ADVANCED_FACE('',(#2043),#1424,.T.);
#14779=ADVANCED_FACE('',(#2044),#988,.T.);
#14780=ADVANCED_FACE('',(#2045),#1425,.T.);
#14781=ADVANCED_FACE('',(#2046),#989,.T.);
#14782=ADVANCED_FACE('',(#2047,#1176,#1177,#1178,#1179,#1180,#1181,#1182,
#1183,#1184,#1185,#1186,#1187,#1188,#1189,#1190),#1426,.T.);
#14783=ADVANCED_FACE('',(#2048,#1191,#1192,#1193,#1194,#1195,#1196,#1197,
#1198,#1199,#1200,#1201,#1202,#1203,#1204,#1205),#1427,.F.);
#14784=ADVANCED_FACE('',(#2049),#1428,.T.);
#14785=ADVANCED_FACE('',(#2050),#14325,.T.);
#14786=ADVANCED_FACE('',(#2051),#990,.T.);
#14787=ADVANCED_FACE('',(#2052),#14326,.T.);
#14788=ADVANCED_FACE('',(#2053),#1429,.T.);
#14789=ADVANCED_FACE('',(#2054),#991,.T.);
#14790=ADVANCED_FACE('',(#2055),#992,.T.);
#14791=ADVANCED_FACE('',(#2056),#993,.T.);
#14792=ADVANCED_FACE('',(#2057),#994,.T.);
#14793=ADVANCED_FACE('',(#2058),#995,.T.);
#14794=ADVANCED_FACE('',(#2059),#996,.T.);
#14795=ADVANCED_FACE('',(#2060),#997,.T.);
#14796=ADVANCED_FACE('',(#2061),#998,.T.);
#14797=ADVANCED_FACE('',(#2062),#999,.T.);
#14798=ADVANCED_FACE('',(#2063),#1000,.T.);
#14799=ADVANCED_FACE('',(#2064),#1001,.T.);
#14800=ADVANCED_FACE('',(#2065),#1002,.T.);
#14801=ADVANCED_FACE('',(#2066),#1003,.T.);
#14802=ADVANCED_FACE('',(#2067),#1004,.T.);
#14803=ADVANCED_FACE('',(#2068),#1005,.T.);
#14804=ADVANCED_FACE('',(#2069),#1006,.T.);
#14805=ADVANCED_FACE('',(#2070),#1007,.T.);
#14806=ADVANCED_FACE('',(#2071),#1008,.T.);
#14807=ADVANCED_FACE('',(#2072),#1009,.T.);
#14808=ADVANCED_FACE('',(#2073),#1010,.T.);
#14809=ADVANCED_FACE('',(#2074),#1011,.T.);
#14810=ADVANCED_FACE('',(#2075),#1012,.T.);
#14811=ADVANCED_FACE('',(#2076),#1013,.T.);
#14812=ADVANCED_FACE('',(#2077),#1014,.T.);
#14813=ADVANCED_FACE('',(#2078),#1015,.T.);
#14814=ADVANCED_FACE('',(#2079),#1016,.T.);
#14815=ADVANCED_FACE('',(#2080),#1430,.F.);
#14816=ADVANCED_FACE('',(#2081),#364,.F.);
#14817=ADVANCED_FACE('',(#2082),#1431,.T.);
#14818=ADVANCED_FACE('',(#2083),#365,.F.);
#14819=ADVANCED_FACE('',(#2084),#360,.F.);
#14820=ADVANCED_FACE('',(#2085,#1206),#1432,.T.);
#14821=ADVANCED_FACE('',(#2086),#14327,.T.);
#14822=ADVANCED_FACE('',(#2087),#1433,.T.);
#14823=ADVANCED_FACE('',(#2088),#1434,.F.);
#14824=ADVANCED_FACE('',(#2089),#1435,.F.);
#14825=ADVANCED_FACE('',(#2090),#1436,.F.);
#14826=ADVANCED_FACE('',(#2091),#1017,.T.);
#14827=ADVANCED_FACE('',(#2092),#1437,.F.);
#14828=ADVANCED_FACE('',(#2093),#1438,.F.);
#14829=ADVANCED_FACE('',(#2094),#1439,.F.);
#14830=ADVANCED_FACE('',(#2095),#14328,.T.);
#14831=ADVANCED_FACE('',(#2096),#1440,.F.);
#14832=ADVANCED_FACE('',(#2097),#1441,.F.);
#14833=ADVANCED_FACE('',(#2098),#1442,.F.);
#14834=ADVANCED_FACE('',(#2099),#1443,.F.);
#14835=ADVANCED_FACE('',(#2100),#1444,.F.);
#14836=ADVANCED_FACE('',(#2101),#1445,.F.);
#14837=ADVANCED_FACE('',(#2102),#1446,.F.);
#14838=ADVANCED_FACE('',(#2103),#1447,.F.);
#14839=ADVANCED_FACE('',(#2104),#1448,.F.);
#14840=ADVANCED_FACE('',(#2105),#1449,.F.);
#14841=ADVANCED_FACE('',(#2106),#1450,.F.);
#14842=ADVANCED_FACE('',(#2107),#1451,.F.);
#14843=ADVANCED_FACE('',(#2108),#1452,.F.);
#14844=ADVANCED_FACE('',(#2109),#1453,.F.);
#14845=ADVANCED_FACE('',(#2110),#1454,.F.);
#14846=ADVANCED_FACE('',(#2111),#1455,.F.);
#14847=ADVANCED_FACE('',(#2112),#1456,.F.);
#14848=ADVANCED_FACE('',(#2113),#1457,.F.);
#14849=ADVANCED_FACE('',(#2114),#1458,.F.);
#14850=ADVANCED_FACE('',(#2115),#1459,.F.);
#14851=ADVANCED_FACE('',(#2116),#1460,.F.);
#14852=ADVANCED_FACE('',(#2117),#1461,.F.);
#14853=ADVANCED_FACE('',(#2118),#1462,.F.);
#14854=ADVANCED_FACE('',(#2119),#1463,.F.);
#14855=ADVANCED_FACE('',(#2120),#1464,.F.);
#14856=ADVANCED_FACE('',(#2121),#1465,.F.);
#14857=ADVANCED_FACE('',(#2122),#1466,.F.);
#14858=ADVANCED_FACE('',(#2123),#1467,.F.);
#14859=ADVANCED_FACE('',(#2124),#1468,.F.);
#14860=ADVANCED_FACE('',(#2125),#1469,.F.);
#14861=ADVANCED_FACE('',(#2126),#1470,.F.);
#14862=ADVANCED_FACE('',(#2127),#1471,.F.);
#14863=ADVANCED_FACE('',(#2128),#1472,.F.);
#14864=ADVANCED_FACE('',(#2129),#1473,.F.);
#14865=ADVANCED_FACE('',(#2130),#1474,.F.);
#14866=ADVANCED_FACE('',(#2131),#1475,.F.);
#14867=ADVANCED_FACE('',(#2132),#1476,.F.);
#14868=ADVANCED_FACE('',(#2133),#1477,.F.);
#14869=ADVANCED_FACE('',(#2134),#1478,.F.);
#14870=ADVANCED_FACE('',(#2135),#1479,.F.);
#14871=ADVANCED_FACE('',(#2136),#1480,.F.);
#14872=ADVANCED_FACE('',(#2137),#1481,.F.);
#14873=ADVANCED_FACE('',(#2138),#1482,.F.);
#14874=ADVANCED_FACE('',(#2139),#1483,.F.);
#14875=ADVANCED_FACE('',(#2140),#1484,.F.);
#14876=ADVANCED_FACE('',(#2141),#1485,.F.);
#14877=ADVANCED_FACE('',(#2142),#1486,.F.);
#14878=ADVANCED_FACE('',(#2143),#1487,.F.);
#14879=ADVANCED_FACE('',(#2144),#1488,.F.);
#14880=ADVANCED_FACE('',(#2145),#1489,.F.);
#14881=ADVANCED_FACE('',(#2146),#1490,.F.);
#14882=ADVANCED_FACE('',(#2147),#1491,.F.);
#14883=ADVANCED_FACE('',(#2148),#1492,.F.);
#14884=ADVANCED_FACE('',(#2149),#1493,.F.);
#14885=ADVANCED_FACE('',(#2150),#1494,.F.);
#14886=ADVANCED_FACE('',(#2151),#1495,.F.);
#14887=ADVANCED_FACE('',(#2152),#1496,.F.);
#14888=ADVANCED_FACE('',(#2153),#1497,.F.);
#14889=ADVANCED_FACE('',(#2154),#1498,.F.);
#14890=ADVANCED_FACE('',(#2155),#1499,.F.);
#14891=ADVANCED_FACE('',(#2156),#1500,.F.);
#14892=ADVANCED_FACE('',(#2157),#1501,.F.);
#14893=ADVANCED_FACE('',(#2158),#1502,.F.);
#14894=ADVANCED_FACE('',(#2159),#1503,.F.);
#14895=ADVANCED_FACE('',(#2160),#1504,.F.);
#14896=ADVANCED_FACE('',(#2161),#1505,.F.);
#14897=ADVANCED_FACE('',(#2162),#1506,.F.);
#14898=ADVANCED_FACE('',(#2163),#1507,.F.);
#14899=ADVANCED_FACE('',(#2164),#1508,.F.);
#14900=ADVANCED_FACE('',(#2165),#1509,.F.);
#14901=ADVANCED_FACE('',(#2166),#1510,.F.);
#14902=ADVANCED_FACE('',(#2167),#1511,.F.);
#14903=ADVANCED_FACE('',(#2168),#1512,.F.);
#14904=ADVANCED_FACE('',(#2169),#1513,.F.);
#14905=ADVANCED_FACE('',(#2170),#1514,.F.);
#14906=ADVANCED_FACE('',(#2171),#1515,.F.);
#14907=ADVANCED_FACE('',(#2172),#1516,.F.);
#14908=ADVANCED_FACE('',(#2173),#1517,.F.);
#14909=ADVANCED_FACE('',(#2174),#1518,.F.);
#14910=ADVANCED_FACE('',(#2175),#1519,.F.);
#14911=ADVANCED_FACE('',(#2176),#1520,.F.);
#14912=ADVANCED_FACE('',(#2177),#1521,.F.);
#14913=ADVANCED_FACE('',(#2178),#1522,.F.);
#14914=ADVANCED_FACE('',(#2179),#1523,.F.);
#14915=ADVANCED_FACE('',(#2180),#1524,.F.);
#14916=ADVANCED_FACE('',(#2181),#1525,.F.);
#14917=ADVANCED_FACE('',(#2182),#1526,.F.);
#14918=ADVANCED_FACE('',(#2183),#1527,.F.);
#14919=ADVANCED_FACE('',(#2184),#1528,.F.);
#14920=ADVANCED_FACE('',(#2185),#1529,.F.);
#14921=ADVANCED_FACE('',(#2186),#1530,.F.);
#14922=ADVANCED_FACE('',(#2187),#1531,.F.);
#14923=ADVANCED_FACE('',(#2188),#1532,.F.);
#14924=ADVANCED_FACE('',(#2189),#1533,.F.);
#14925=ADVANCED_FACE('',(#2190),#1534,.F.);
#14926=ADVANCED_FACE('',(#2191),#1535,.F.);
#14927=ADVANCED_FACE('',(#2192),#1536,.F.);
#14928=ADVANCED_FACE('',(#2193),#1537,.F.);
#14929=ADVANCED_FACE('',(#2194),#1538,.F.);
#14930=ADVANCED_FACE('',(#2195),#1539,.F.);
#14931=ADVANCED_FACE('',(#2196),#1540,.F.);
#14932=ADVANCED_FACE('',(#2197),#1541,.F.);
#14933=ADVANCED_FACE('',(#2198),#361,.T.);
#14934=ADVANCED_FACE('',(#2199,#1207),#1542,.F.);
#14935=ADVANCED_FACE('',(#2200),#14329,.F.);
#14936=ADVANCED_FACE('',(#2201),#1018,.T.);
#14937=ADVANCED_FACE('',(#2202),#1019,.T.);
#14938=ADVANCED_FACE('',(#2203),#1020,.T.);
#14939=ADVANCED_FACE('',(#2204),#1021,.T.);
#14940=ADVANCED_FACE('',(#2205),#1022,.T.);
#14941=ADVANCED_FACE('',(#2206),#1023,.T.);
#14942=ADVANCED_FACE('',(#2207),#1543,.F.);
#14943=ADVANCED_FACE('',(#2208),#1544,.F.);
#14944=ADVANCED_FACE('',(#2209),#1545,.F.);
#14945=ADVANCED_FACE('',(#2210),#1546,.F.);
#14946=ADVANCED_FACE('',(#2211),#1547,.F.);
#14947=ADVANCED_FACE('',(#2212),#1548,.F.);
#14948=ADVANCED_FACE('',(#2213),#1549,.F.);
#14949=ADVANCED_FACE('',(#2214),#1550,.F.);
#14950=ADVANCED_FACE('',(#2215),#1551,.F.);
#14951=ADVANCED_FACE('',(#2216),#1552,.F.);
#14952=ADVANCED_FACE('',(#2217),#1553,.F.);
#14953=ADVANCED_FACE('',(#2218),#1554,.F.);
#14954=ADVANCED_FACE('',(#2219),#1555,.F.);
#14955=ADVANCED_FACE('',(#2220),#1556,.F.);
#14956=ADVANCED_FACE('',(#2221),#1557,.F.);
#14957=ADVANCED_FACE('',(#2222),#14330,.F.);
#14958=ADVANCED_FACE('',(#2223),#1558,.F.);
#14959=ADVANCED_FACE('',(#2224),#1559,.F.);
#14960=ADVANCED_FACE('',(#2225),#1560,.F.);
#14961=ADVANCED_FACE('',(#2226),#1024,.T.);
#14962=ADVANCED_FACE('',(#2227),#1025,.T.);
#14963=ADVANCED_FACE('',(#2228),#1026,.T.);
#14964=ADVANCED_FACE('',(#2229),#1027,.T.);
#14965=ADVANCED_FACE('',(#2230),#1028,.T.);
#14966=ADVANCED_FACE('',(#2231),#1029,.T.);
#14967=ADVANCED_FACE('',(#2232),#1030,.T.);
#14968=ADVANCED_FACE('',(#2233),#1031,.T.);
#14969=ADVANCED_FACE('',(#2234),#1032,.T.);
#14970=ADVANCED_FACE('',(#2235),#1033,.T.);
#14971=ADVANCED_FACE('',(#2236),#1034,.T.);
#14972=ADVANCED_FACE('',(#2237),#1035,.T.);
#14973=ADVANCED_FACE('',(#2238),#1036,.T.);
#14974=ADVANCED_FACE('',(#2239),#1037,.T.);
#14975=ADVANCED_FACE('',(#2240),#1038,.T.);
#14976=ADVANCED_FACE('',(#2241),#1039,.T.);
#14977=ADVANCED_FACE('',(#2242),#1040,.T.);
#14978=ADVANCED_FACE('',(#2243),#1041,.T.);
#14979=ADVANCED_FACE('',(#2244),#1042,.T.);
#14980=ADVANCED_FACE('',(#2245),#1043,.T.);
#14981=ADVANCED_FACE('',(#2246),#1044,.T.);
#14982=ADVANCED_FACE('',(#2247),#1045,.T.);
#14983=ADVANCED_FACE('',(#2248),#1046,.T.);
#14984=ADVANCED_FACE('',(#2249),#1047,.T.);
#14985=ADVANCED_FACE('',(#2250),#1048,.T.);
#14986=ADVANCED_FACE('',(#2251),#1561,.F.);
#14987=ADVANCED_FACE('',(#2252),#366,.F.);
#14988=ADVANCED_FACE('',(#2253),#1562,.T.);
#14989=ADVANCED_FACE('',(#2254),#367,.F.);
#14990=ADVANCED_FACE('',(#2255),#14331,.F.);
#14991=ADVANCED_FACE('',(#2256),#1049,.T.);
#14992=ADVANCED_FACE('',(#2257),#1050,.T.);
#14993=ADVANCED_FACE('',(#2258),#1051,.T.);
#14994=ADVANCED_FACE('',(#2259),#1052,.T.);
#14995=ADVANCED_FACE('',(#2260),#1053,.T.);
#14996=ADVANCED_FACE('',(#2261),#1054,.T.);
#14997=ADVANCED_FACE('',(#2262),#1563,.F.);
#14998=ADVANCED_FACE('',(#2263),#1564,.F.);
#14999=ADVANCED_FACE('',(#2264),#1565,.F.);
#15000=ADVANCED_FACE('',(#2265),#1566,.T.);
#15001=ADVANCED_FACE('',(#2266),#1567,.T.);
#15002=ADVANCED_FACE('',(#2267),#1568,.T.);
#15003=ADVANCED_FACE('',(#2268),#1569,.T.);
#15004=ADVANCED_FACE('',(#2269),#1570,.T.);
#15005=ADVANCED_FACE('',(#2270),#1571,.T.);
#15006=ADVANCED_FACE('',(#2271),#1572,.F.);
#15007=ADVANCED_FACE('',(#2272),#1573,.F.);
#15008=ADVANCED_FACE('',(#2273),#1574,.F.);
#15009=ADVANCED_FACE('',(#2274),#1575,.F.);
#15010=ADVANCED_FACE('',(#2275),#1576,.F.);
#15011=ADVANCED_FACE('',(#2276),#1577,.F.);
#15012=ADVANCED_FACE('',(#2277),#14332,.F.);
#15013=ADVANCED_FACE('',(#2278),#1578,.F.);
#15014=ADVANCED_FACE('',(#2279),#1579,.F.);
#15015=ADVANCED_FACE('',(#2280),#1580,.F.);
#15016=ADVANCED_FACE('',(#2281,#1208),#1581,.T.);
#15017=ADVANCED_FACE('',(#2282),#14333,.T.);
#15018=ADVANCED_FACE('',(#2283),#14334,.T.);
#15019=ADVANCED_FACE('',(#2284),#1582,.T.);
#15020=ADVANCED_FACE('',(#2285),#1055,.T.);
#15021=ADVANCED_FACE('',(#2286),#1056,.T.);
#15022=ADVANCED_FACE('',(#2287),#1057,.T.);
#15023=ADVANCED_FACE('',(#2288),#1058,.T.);
#15024=ADVANCED_FACE('',(#2289),#1059,.T.);
#15025=ADVANCED_FACE('',(#2290),#1060,.T.);
#15026=ADVANCED_FACE('',(#2291),#1061,.T.);
#15027=ADVANCED_FACE('',(#2292),#1062,.T.);
#15028=ADVANCED_FACE('',(#2293),#1063,.T.);
#15029=ADVANCED_FACE('',(#2294),#1064,.T.);
#15030=ADVANCED_FACE('',(#2295),#14335,.F.);
#15031=ADVANCED_FACE('',(#2296),#14336,.F.);
#15032=ADVANCED_FACE('',(#2297),#1065,.T.);
#15033=ADVANCED_FACE('',(#2298),#1066,.T.);
#15034=ADVANCED_FACE('',(#2299),#368,.F.);
#15035=ADVANCED_FACE('',(#2300),#1583,.F.);
#15036=ADVANCED_FACE('',(#2301),#369,.F.);
#15037=ADVANCED_FACE('',(#2302),#1584,.T.);
#15038=ADVANCED_FACE('',(#2303),#362,.F.);
#15039=ADVANCED_FACE('',(#2304,#1209),#1585,.T.);
#15040=ADVANCED_FACE('',(#2305),#1586,.F.);
#15041=ADVANCED_FACE('',(#2306),#1587,.F.);
#15042=ADVANCED_FACE('',(#2307),#1588,.F.);
#15043=ADVANCED_FACE('',(#2308),#1589,.F.);
#15044=ADVANCED_FACE('',(#2309),#1590,.F.);
#15045=ADVANCED_FACE('',(#2310),#1591,.F.);
#15046=ADVANCED_FACE('',(#2311),#14337,.F.);
#15047=ADVANCED_FACE('',(#2312),#1592,.F.);
#15048=ADVANCED_FACE('',(#2313),#1593,.F.);
#15049=ADVANCED_FACE('',(#2314),#1594,.F.);
#15050=ADVANCED_FACE('',(#2315),#1595,.F.);
#15051=ADVANCED_FACE('',(#2316),#1596,.F.);
#15052=ADVANCED_FACE('',(#2317),#1597,.F.);
#15053=ADVANCED_FACE('',(#2318),#1067,.T.);
#15054=ADVANCED_FACE('',(#2319),#259,.T.);
#15055=ADVANCED_FACE('',(#2320),#1068,.T.);
#15056=ADVANCED_FACE('',(#2321),#1069,.T.);
#15057=ADVANCED_FACE('',(#2322),#1070,.T.);
#15058=ADVANCED_FACE('',(#2323),#1071,.T.);
#15059=ADVANCED_FACE('',(#2324),#1072,.T.);
#15060=ADVANCED_FACE('',(#2325),#1073,.T.);
#15061=ADVANCED_FACE('',(#2326),#1074,.T.);
#15062=ADVANCED_FACE('',(#2327),#1075,.T.);
#15063=ADVANCED_FACE('',(#2328),#1076,.T.);
#15064=ADVANCED_FACE('',(#2329),#1077,.T.);
#15065=ADVANCED_FACE('',(#2330),#1078,.T.);
#15066=ADVANCED_FACE('',(#2331),#1079,.T.);
#15067=ADVANCED_FACE('',(#2332),#1080,.T.);
#15068=ADVANCED_FACE('',(#2333),#1081,.T.);
#15069=ADVANCED_FACE('',(#2334),#370,.F.);
#15070=ADVANCED_FACE('',(#2335),#1598,.F.);
#15071=ADVANCED_FACE('',(#2336),#371,.F.);
#15072=ADVANCED_FACE('',(#2337),#363,.F.);
#15073=ADVANCED_FACE('',(#2338,#1210),#1599,.T.);
#15074=ADVANCED_FACE('',(#2339),#1600,.F.);
#15075=ADVANCED_FACE('',(#2340),#1601,.F.);
#15076=ADVANCED_FACE('',(#2341),#1602,.F.);
#15077=ADVANCED_FACE('',(#2342),#1082,.T.);
#15078=ADVANCED_FACE('',(#2343),#1603,.T.);
#15079=ADVANCED_FACE('',(#2344),#1604,.T.);
#15080=ADVANCED_FACE('',(#2345),#14338,.T.);
#15081=ADVANCED_FACE('',(#2346),#1605,.T.);
#15082=ADVANCED_FACE('',(#2347),#14339,.F.);
#15083=ADVANCED_FACE('',(#2348),#14340,.T.);
#15084=CLOSED_SHELL('',(#14341,#14342,#14343,#14344,#14345,#14346,#14347,
#14348,#14349,#14350,#14351,#14352,#14353,#14354,#14355,#14356,#14357,#14358,
#14359,#14360,#14361,#14362,#14363,#14364,#14365,#14366,#14367,#14368,#14369,
#14370,#14371,#14372,#14373,#14374,#14375,#14376,#14377,#14378,#14379,#14380,
#14381,#14382,#14383,#14384,#14385,#14386,#14387,#14388,#14389,#14390,#14391,
#14392,#14393,#14394,#14395,#14396,#14397,#14398,#14399,#14400,#14401,#14402,
#14403,#14404,#14405,#14406,#14407,#14408,#14409,#14410,#14411,#14412));
#15085=CLOSED_SHELL('',(#14413,#14414,#14415,#14416,#14417,#14418,#14419,
#14420,#14421,#14422,#14423,#14424,#14425,#14426,#14427,#14428,#14429,#14430,
#14431,#14432,#14433,#14434,#14435,#14436,#14437,#14438,#14439,#14440,#14441,
#14442,#14443,#14444,#14445,#14446,#14447,#14448,#14449,#14450,#14451,#14452,
#14453,#14454,#14455,#14456,#14457,#14458,#14459,#14460,#14461,#14462,#14463,
#14464,#14465,#14466,#14467,#14468,#14469,#14470,#14471,#14472,#14473,#14474,
#14475,#14476,#14477,#14478,#14479,#14480,#14481,#14482,#14483,#14484,#14485,
#14486,#14487,#14488,#14489,#14490,#14491,#14492,#14493,#14494,#14495,#14496,
#14497,#14498,#14499,#14500,#14501,#14502,#14503,#14504,#14505,#14506,#14507,
#14508,#14509,#14510,#14511,#14512,#14513,#14514,#14515,#14516,#14517,#14518,
#14519,#14520,#14521,#14522,#14523,#14524,#14525,#14526,#14527,#14528,#14529,
#14530,#14531,#14532,#14533,#14534,#14535,#14536,#14537,#14538,#14539,#14540,
#14541,#14542,#14543,#14544,#14545,#14546,#14547,#14548));
#15086=CLOSED_SHELL('',(#14549,#14550,#14551,#14552,#14553,#14554,#14555,
#14556,#14557,#14558,#14559,#14560,#14561,#14562,#14563,#14564,#14565,#14566,
#14567,#14568,#14569,#14570,#14571,#14572,#14573,#14574,#14575,#14576,#14577,
#14578,#14579,#14580,#14581,#14582,#14583,#14584,#14585,#14586,#14587,#14588,
#14589,#14590,#14591,#14592,#14593,#14594,#14595,#14596,#14597));
#15087=CLOSED_SHELL('',(#14598,#14599,#14600,#14601,#14602,#14603,#14604,
#14605,#14606,#14607,#14608,#14609,#14610,#14611,#14612,#14613,#14614,#14615,
#14616,#14617,#14618,#14619,#14620,#14621,#14622,#14623,#14624,#14625,#14626,
#14627,#14628,#14629,#14630,#14631,#14632,#14633,#14634,#14635,#14636,#14637,
#14638,#14639,#14640,#14641,#14642,#14643,#14644,#14645,#14646,#14647,#14648,
#14649,#14650,#14651,#14652,#14653));
#15088=CLOSED_SHELL('',(#14654,#14655,#14656,#14657,#14658,#14659,#14660,
#14661,#14662,#14663,#14664,#14665,#14666,#14667,#14668,#14669,#14670,#14671,
#14672,#14673,#14674,#14675,#14676,#14677,#14678,#14679,#14680,#14681,#14682,
#14683,#14684,#14685,#14686,#14687,#14688,#14689,#14690,#14691,#14692,#14693,
#14694,#14695,#14696,#14697,#14698,#14699,#14700,#14701,#14702,#14703,#14704,
#14705,#14706,#14707,#14708,#14709,#14710,#14711,#14712,#14713,#14714,#14715,
#14716,#14717,#14718,#14719,#14720,#14721,#14722,#14723,#14724,#14725,#14726,
#14727,#14728,#14729,#14730,#14731,#14732,#14733,#14734,#14735,#14736,#14737,
#14738,#14739,#14740,#14741,#14742,#14743,#14744,#14745,#14746,#14747,#14748,
#14749,#14750,#14751,#14752,#14753,#14754,#14755,#14756,#14757,#14758,#14759,
#14760,#14761,#14762,#14763,#14764,#14765,#14766,#14767,#14768,#14769,#14770,
#14771,#14772,#14773,#14774,#14775,#14776,#14777,#14778,#14779,#14780,#14781,
#14782,#14783));
#15089=CLOSED_SHELL('',(#14784,#14785,#14786,#14787,#14788));
#15090=CLOSED_SHELL('',(#14789,#14790,#14791,#14792,#14793,#14794,#14795,
#14796,#14797,#14798,#14799,#14800,#14801,#14802,#14803,#14804,#14805,#14806,
#14807,#14808,#14809,#14810,#14811,#14812,#14813,#14814,#14815,#14816,#14817,
#14818,#14819,#14820,#14821,#14822,#14823,#14824,#14825,#14826,#14827,#14828,
#14829,#14830,#14831,#14832,#14833,#14834,#14835,#14836,#14837,#14838,#14839,
#14840,#14841,#14842,#14843,#14844,#14845,#14846,#14847,#14848,#14849,#14850,
#14851,#14852,#14853,#14854,#14855,#14856,#14857,#14858,#14859,#14860,#14861,
#14862,#14863,#14864,#14865,#14866,#14867,#14868,#14869,#14870,#14871,#14872,
#14873,#14874,#14875,#14876,#14877,#14878,#14879,#14880,#14881,#14882,#14883,
#14884,#14885,#14886,#14887,#14888,#14889,#14890,#14891,#14892,#14893,#14894,
#14895,#14896,#14897,#14898,#14899,#14900,#14901,#14902,#14903,#14904,#14905,
#14906,#14907,#14908,#14909,#14910,#14911,#14912,#14913,#14914,#14915,#14916,
#14917,#14918,#14919,#14920,#14921,#14922,#14923,#14924,#14925,#14926,#14927,
#14928,#14929,#14930,#14931,#14932,#14933,#14934,#14935,#14936,#14937,#14938,
#14939,#14940,#14941,#14942,#14943,#14944,#14945,#14946,#14947,#14948,#14949,
#14950,#14951,#14952,#14953,#14954,#14955,#14956,#14957,#14958,#14959,#14960));
#15091=CLOSED_SHELL('',(#14961,#14962,#14963,#14964,#14965,#14966,#14967,
#14968,#14969,#14970,#14971,#14972,#14973,#14974,#14975,#14976,#14977,#14978,
#14979,#14980,#14981,#14982,#14983,#14984,#14985,#14986,#14987,#14988,#14989,
#14990,#14991,#14992,#14993,#14994,#14995,#14996,#14997,#14998,#14999,#15000,
#15001,#15002,#15003,#15004,#15005,#15006,#15007,#15008,#15009,#15010,#15011,
#15012,#15013,#15014,#15015,#15016,#15017,#15018,#15019));
#15092=CLOSED_SHELL('',(#15020,#15021,#15022,#15023,#15024,#15025,#15026,
#15027,#15028,#15029,#15030,#15031,#15032,#15033,#15034,#15035,#15036,#15037,
#15038,#15039,#15040,#15041,#15042,#15043,#15044,#15045,#15046,#15047,#15048,
#15049,#15050,#15051,#15052,#15053,#15054));
#15093=CLOSED_SHELL('',(#15055,#15056,#15057,#15058,#15059,#15060,#15061,
#15062,#15063,#15064,#15065,#15066,#15067,#15068,#15069,#15070,#15071,#15072,
#15073,#15074,#15075,#15076,#15077,#15078,#15079,#15080,#15081,#15082,#15083));
#15094=DERIVED_UNIT_ELEMENT(#15114,1.);
#15095=DERIVED_UNIT_ELEMENT(#81042,-3.);
#15096=DERIVED_UNIT_ELEMENT(#15114,1.);
#15097=DERIVED_UNIT_ELEMENT(#81042,-3.);
#15098=DERIVED_UNIT_ELEMENT(#15114,1.);
#15099=DERIVED_UNIT_ELEMENT(#81042,-3.);
#15100=DERIVED_UNIT_ELEMENT(#15114,1.);
#15101=DERIVED_UNIT_ELEMENT(#81042,-3.);
#15102=DERIVED_UNIT_ELEMENT(#15114,1.);
#15103=DERIVED_UNIT_ELEMENT(#81042,-3.);
#15104=DERIVED_UNIT_ELEMENT(#15114,1.);
#15105=DERIVED_UNIT_ELEMENT(#81042,-3.);
#15106=DERIVED_UNIT_ELEMENT(#15114,1.);
#15107=DERIVED_UNIT_ELEMENT(#81042,-3.);
#15108=DERIVED_UNIT_ELEMENT(#15114,1.);
#15109=DERIVED_UNIT_ELEMENT(#81042,-3.);
#15110=DERIVED_UNIT_ELEMENT(#15114,1.);
#15111=DERIVED_UNIT_ELEMENT(#81042,-3.);
#15112=DERIVED_UNIT_ELEMENT(#15114,1.);
#15113=DERIVED_UNIT_ELEMENT(#81042,-3.);
#15114=(
MASS_UNIT()
NAMED_UNIT(*)
SI_UNIT(.KILO.,.GRAM.)
);
#15115=DERIVED_UNIT((#15094,#15095));
#15116=DERIVED_UNIT((#15096,#15097));
#15117=DERIVED_UNIT((#15098,#15099));
#15118=DERIVED_UNIT((#15100,#15101));
#15119=DERIVED_UNIT((#15102,#15103));
#15120=DERIVED_UNIT((#15104,#15105));
#15121=DERIVED_UNIT((#15106,#15107));
#15122=DERIVED_UNIT((#15108,#15109));
#15123=DERIVED_UNIT((#15110,#15111));
#15124=DERIVED_UNIT((#15112,#15113));
#15125=MEASURE_REPRESENTATION_ITEM('density measure',
POSITIVE_RATIO_MEASURE(7850.),#15115);
#15126=MEASURE_REPRESENTATION_ITEM('density measure',
POSITIVE_RATIO_MEASURE(7850.),#15116);
#15127=MEASURE_REPRESENTATION_ITEM('density measure',
POSITIVE_RATIO_MEASURE(7850.),#15117);
#15128=MEASURE_REPRESENTATION_ITEM('density measure',
POSITIVE_RATIO_MEASURE(7850.),#15118);
#15129=MEASURE_REPRESENTATION_ITEM('density measure',
POSITIVE_RATIO_MEASURE(7850.),#15119);
#15130=MEASURE_REPRESENTATION_ITEM('density measure',
POSITIVE_RATIO_MEASURE(7850.),#15120);
#15131=MEASURE_REPRESENTATION_ITEM('density measure',
POSITIVE_RATIO_MEASURE(7850.),#15121);
#15132=MEASURE_REPRESENTATION_ITEM('density measure',
POSITIVE_RATIO_MEASURE(7850.),#15122);
#15133=MEASURE_REPRESENTATION_ITEM('density measure',
POSITIVE_RATIO_MEASURE(7850.),#15123);
#15134=MEASURE_REPRESENTATION_ITEM('density measure',
POSITIVE_RATIO_MEASURE(7850.),#15124);
#15135=PROPERTY_DEFINITION_REPRESENTATION(#15185,#15155);
#15136=PROPERTY_DEFINITION_REPRESENTATION(#15186,#15156);
#15137=PROPERTY_DEFINITION_REPRESENTATION(#15187,#15157);
#15138=PROPERTY_DEFINITION_REPRESENTATION(#15188,#15158);
#15139=PROPERTY_DEFINITION_REPRESENTATION(#15189,#15159);
#15140=PROPERTY_DEFINITION_REPRESENTATION(#15190,#15160);
#15141=PROPERTY_DEFINITION_REPRESENTATION(#15191,#15161);
#15142=PROPERTY_DEFINITION_REPRESENTATION(#15192,#15162);
#15143=PROPERTY_DEFINITION_REPRESENTATION(#15193,#15163);
#15144=PROPERTY_DEFINITION_REPRESENTATION(#15194,#15164);
#15145=PROPERTY_DEFINITION_REPRESENTATION(#15195,#15165);
#15146=PROPERTY_DEFINITION_REPRESENTATION(#15196,#15166);
#15147=PROPERTY_DEFINITION_REPRESENTATION(#15197,#15167);
#15148=PROPERTY_DEFINITION_REPRESENTATION(#15198,#15168);
#15149=PROPERTY_DEFINITION_REPRESENTATION(#15199,#15169);
#15150=PROPERTY_DEFINITION_REPRESENTATION(#15200,#15170);
#15151=PROPERTY_DEFINITION_REPRESENTATION(#15201,#15171);
#15152=PROPERTY_DEFINITION_REPRESENTATION(#15202,#15172);
#15153=PROPERTY_DEFINITION_REPRESENTATION(#15203,#15173);
#15154=PROPERTY_DEFINITION_REPRESENTATION(#15204,#15174);
#15155=REPRESENTATION('material name',(#15175),#81030);
#15156=REPRESENTATION('density',(#15125),#81030);
#15157=REPRESENTATION('material name',(#15176),#81031);
#15158=REPRESENTATION('density',(#15126),#81031);
#15159=REPRESENTATION('material name',(#15177),#81032);
#15160=REPRESENTATION('density',(#15127),#81032);
#15161=REPRESENTATION('material name',(#15178),#81033);
#15162=REPRESENTATION('density',(#15128),#81033);
#15163=REPRESENTATION('material name',(#15179),#81034);
#15164=REPRESENTATION('density',(#15129),#81034);
#15165=REPRESENTATION('material name',(#15180),#81035);
#15166=REPRESENTATION('density',(#15130),#81035);
#15167=REPRESENTATION('material name',(#15181),#81036);
#15168=REPRESENTATION('density',(#15131),#81036);
#15169=REPRESENTATION('material name',(#15182),#81037);
#15170=REPRESENTATION('density',(#15132),#81037);
#15171=REPRESENTATION('material name',(#15183),#81038);
#15172=REPRESENTATION('density',(#15133),#81038);
#15173=REPRESENTATION('material name',(#15184),#81039);
#15174=REPRESENTATION('density',(#15134),#81039);
#15175=DESCRIPTIVE_REPRESENTATION_ITEM('Steel','Steel');
#15176=DESCRIPTIVE_REPRESENTATION_ITEM('Steel','Steel');
#15177=DESCRIPTIVE_REPRESENTATION_ITEM('Steel','Steel');
#15178=DESCRIPTIVE_REPRESENTATION_ITEM('Steel','Steel');
#15179=DESCRIPTIVE_REPRESENTATION_ITEM('Steel','Steel');
#15180=DESCRIPTIVE_REPRESENTATION_ITEM('Steel','Steel');
#15181=DESCRIPTIVE_REPRESENTATION_ITEM('Steel','Steel');
#15182=DESCRIPTIVE_REPRESENTATION_ITEM('Steel','Steel');
#15183=DESCRIPTIVE_REPRESENTATION_ITEM('Steel','Steel');
#15184=DESCRIPTIVE_REPRESENTATION_ITEM('Steel','Steel');
#15185=PROPERTY_DEFINITION('material property','material name',#81142);
#15186=PROPERTY_DEFINITION('material property','density of part',#81142);
#15187=PROPERTY_DEFINITION('material property','material name',#81143);
#15188=PROPERTY_DEFINITION('material property','density of part',#81143);
#15189=PROPERTY_DEFINITION('material property','material name',#81144);
#15190=PROPERTY_DEFINITION('material property','density of part',#81144);
#15191=PROPERTY_DEFINITION('material property','material name',#81145);
#15192=PROPERTY_DEFINITION('material property','density of part',#81145);
#15193=PROPERTY_DEFINITION('material property','material name',#81146);
#15194=PROPERTY_DEFINITION('material property','density of part',#81146);
#15195=PROPERTY_DEFINITION('material property','material name',#81147);
#15196=PROPERTY_DEFINITION('material property','density of part',#81147);
#15197=PROPERTY_DEFINITION('material property','material name',#81148);
#15198=PROPERTY_DEFINITION('material property','density of part',#81148);
#15199=PROPERTY_DEFINITION('material property','material name',#81149);
#15200=PROPERTY_DEFINITION('material property','density of part',#81149);
#15201=PROPERTY_DEFINITION('material property','material name',#81150);
#15202=PROPERTY_DEFINITION('material property','density of part',#81150);
#15203=PROPERTY_DEFINITION('material property','material name',#81151);
#15204=PROPERTY_DEFINITION('material property','density of part',#81151);
#15205=AXIS2_PLACEMENT_3D('',#20562,#16620,#16621);
#15206=AXIS2_PLACEMENT_3D('',#20563,#16622,#16623);
#15207=AXIS2_PLACEMENT_3D('',#20564,#16624,#16625);
#15208=AXIS2_PLACEMENT_3D('',#20566,#16626,#16627);
#15209=AXIS2_PLACEMENT_3D('',#20569,#16629,#16630);
#15210=AXIS2_PLACEMENT_3D('',#20570,#16631,#16632);
#15211=AXIS2_PLACEMENT_3D('',#20580,#16637,#16638);
#15212=AXIS2_PLACEMENT_3D('',#20582,#16639,#16640);
#15213=AXIS2_PLACEMENT_3D('',#20584,#16641,#16642);
#15214=AXIS2_PLACEMENT_3D('',#20585,#16643,#16644);
#15215=AXIS2_PLACEMENT_3D('',#20588,#16646,#16647);
#15216=AXIS2_PLACEMENT_3D('',#20589,#16648,#16649);
#15217=AXIS2_PLACEMENT_3D('',#20591,#16650,#16651);
#15218=AXIS2_PLACEMENT_3D('',#20593,#16653,#16654);
#15219=AXIS2_PLACEMENT_3D('',#20596,#16656,#16657);
#15220=AXIS2_PLACEMENT_3D('',#20597,#16658,#16659);
#15221=AXIS2_PLACEMENT_3D('',#20599,#16660,#16661);
#15222=AXIS2_PLACEMENT_3D('',#20601,#16663,#16664);
#15223=AXIS2_PLACEMENT_3D('',#20604,#16666,#16667);
#15224=AXIS2_PLACEMENT_3D('',#20605,#16668,#16669);
#15225=AXIS2_PLACEMENT_3D('',#20607,#16670,#16671);
#15226=AXIS2_PLACEMENT_3D('',#20609,#16673,#16674);
#15227=AXIS2_PLACEMENT_3D('',#20612,#16676,#16677);
#15228=AXIS2_PLACEMENT_3D('',#20613,#16678,#16679);
#15229=AXIS2_PLACEMENT_3D('',#20615,#16680,#16681);
#15230=AXIS2_PLACEMENT_3D('',#20618,#16683,#16684);
#15231=AXIS2_PLACEMENT_3D('',#20619,#16685,#16686);
#15232=AXIS2_PLACEMENT_3D('',#20629,#16691,#16692);
#15233=AXIS2_PLACEMENT_3D('',#20631,#16693,#16694);
#15234=AXIS2_PLACEMENT_3D('',#20633,#16695,#16696);
#15235=AXIS2_PLACEMENT_3D('',#20634,#16697,#16698);
#15236=AXIS2_PLACEMENT_3D('',#20637,#16700,#16701);
#15237=AXIS2_PLACEMENT_3D('',#20638,#16702,#16703);
#15238=AXIS2_PLACEMENT_3D('',#20640,#16704,#16705);
#15239=AXIS2_PLACEMENT_3D('',#20642,#16707,#16708);
#15240=AXIS2_PLACEMENT_3D('',#20645,#16710,#16711);
#15241=AXIS2_PLACEMENT_3D('',#20646,#16712,#16713);
#15242=AXIS2_PLACEMENT_3D('',#20648,#16714,#16715);
#15243=AXIS2_PLACEMENT_3D('',#20650,#16717,#16718);
#15244=AXIS2_PLACEMENT_3D('',#20653,#16720,#16721);
#15245=AXIS2_PLACEMENT_3D('',#20654,#16722,#16723);
#15246=AXIS2_PLACEMENT_3D('',#20656,#16724,#16725);
#15247=AXIS2_PLACEMENT_3D('',#20658,#16727,#16728);
#15248=AXIS2_PLACEMENT_3D('',#20661,#16730,#16731);
#15249=AXIS2_PLACEMENT_3D('',#20662,#16732,#16733);
#15250=AXIS2_PLACEMENT_3D('',#20664,#16734,#16735);
#15251=AXIS2_PLACEMENT_3D('',#20667,#16737,#16738);
#15252=AXIS2_PLACEMENT_3D('',#20668,#16739,#16740);
#15253=AXIS2_PLACEMENT_3D('',#20678,#16745,#16746);
#15254=AXIS2_PLACEMENT_3D('',#20680,#16747,#16748);
#15255=AXIS2_PLACEMENT_3D('',#20682,#16749,#16750);
#15256=AXIS2_PLACEMENT_3D('',#20684,#16751,#16752);
#15257=AXIS2_PLACEMENT_3D('',#20686,#16753,#16754);
#15258=AXIS2_PLACEMENT_3D('',#20688,#16755,#16756);
#15259=AXIS2_PLACEMENT_3D('',#20690,#16757,#16758);
#15260=AXIS2_PLACEMENT_3D('',#20691,#16759,#16760);
#15261=AXIS2_PLACEMENT_3D('',#20694,#16762,#16763);
#15262=AXIS2_PLACEMENT_3D('',#20695,#16764,#16765);
#15263=AXIS2_PLACEMENT_3D('',#20697,#16766,#16767);
#15264=AXIS2_PLACEMENT_3D('',#20699,#16769,#16770);
#15265=AXIS2_PLACEMENT_3D('',#20702,#16772,#16773);
#15266=AXIS2_PLACEMENT_3D('',#20703,#16774,#16775);
#15267=AXIS2_PLACEMENT_3D('',#20705,#16776,#16777);
#15268=AXIS2_PLACEMENT_3D('',#20707,#16779,#16780);
#15269=AXIS2_PLACEMENT_3D('',#20710,#16782,#16783);
#15270=AXIS2_PLACEMENT_3D('',#20711,#16784,#16785);
#15271=AXIS2_PLACEMENT_3D('',#20713,#16786,#16787);
#15272=AXIS2_PLACEMENT_3D('',#20715,#16789,#16790);
#15273=AXIS2_PLACEMENT_3D('',#20718,#16792,#16793);
#15274=AXIS2_PLACEMENT_3D('',#20719,#16794,#16795);
#15275=AXIS2_PLACEMENT_3D('',#20721,#16796,#16797);
#15276=AXIS2_PLACEMENT_3D('',#20723,#16799,#16800);
#15277=AXIS2_PLACEMENT_3D('',#20726,#16802,#16803);
#15278=AXIS2_PLACEMENT_3D('',#20727,#16804,#16805);
#15279=AXIS2_PLACEMENT_3D('',#20729,#16806,#16807);
#15280=AXIS2_PLACEMENT_3D('',#20731,#16809,#16810);
#15281=AXIS2_PLACEMENT_3D('',#20734,#16812,#16813);
#15282=AXIS2_PLACEMENT_3D('',#20735,#16814,#16815);
#15283=AXIS2_PLACEMENT_3D('',#20737,#16816,#16817);
#15284=AXIS2_PLACEMENT_3D('',#20739,#16819,#16820);
#15285=AXIS2_PLACEMENT_3D('',#20742,#16822,#16823);
#15286=AXIS2_PLACEMENT_3D('',#20743,#16824,#16825);
#15287=AXIS2_PLACEMENT_3D('',#20745,#16826,#16827);
#15288=AXIS2_PLACEMENT_3D('',#20747,#16829,#16830);
#15289=AXIS2_PLACEMENT_3D('',#20750,#16832,#16833);
#15290=AXIS2_PLACEMENT_3D('',#20751,#16834,#16835);
#15291=AXIS2_PLACEMENT_3D('',#20754,#16837,#16838);
#15292=AXIS2_PLACEMENT_3D('',#20757,#16840,#16841);
#15293=AXIS2_PLACEMENT_3D('',#20760,#16843,#16844);
#15294=AXIS2_PLACEMENT_3D('',#20763,#16846,#16847);
#15295=AXIS2_PLACEMENT_3D('',#20766,#16849,#16850);
#15296=AXIS2_PLACEMENT_3D('',#20769,#16852,#16853);
#15297=AXIS2_PLACEMENT_3D('',#20772,#16855,#16856);
#15298=AXIS2_PLACEMENT_3D('',#20775,#16858,#16859);
#15299=AXIS2_PLACEMENT_3D('',#20786,#16865,#16866);
#15300=AXIS2_PLACEMENT_3D('',#20793,#16871,#16872);
#15301=AXIS2_PLACEMENT_3D('',#20823,#16889,#16890);
#15302=AXIS2_PLACEMENT_3D('',#20829,#16894,#16895);
#15303=AXIS2_PLACEMENT_3D('',#20837,#16900,#16901);
#15304=AXIS2_PLACEMENT_3D('',#20841,#16904,#16905);
#15305=AXIS2_PLACEMENT_3D('',#20845,#16908,#16909);
#15306=AXIS2_PLACEMENT_3D('',#20851,#16913,#16914);
#15307=AXIS2_PLACEMENT_3D('',#20857,#16918,#16919);
#15308=AXIS2_PLACEMENT_3D('',#20861,#16922,#16923);
#15309=AXIS2_PLACEMENT_3D('',#20864,#16926,#16927);
#15310=AXIS2_PLACEMENT_3D('',#20892,#16943,#16944);
#15311=AXIS2_PLACEMENT_3D('',#20895,#16947,#16948);
#15312=AXIS2_PLACEMENT_3D('',#20897,#16950,#16951);
#15313=AXIS2_PLACEMENT_3D('',#20898,#16952,#16953);
#15314=AXIS2_PLACEMENT_3D('',#20900,#16955,#16956);
#15315=AXIS2_PLACEMENT_3D('',#20902,#16958,#16959);
#15316=AXIS2_PLACEMENT_3D('',#20904,#16961,#16962);
#15317=AXIS2_PLACEMENT_3D('',#20906,#16964,#16965);
#15318=AXIS2_PLACEMENT_3D('',#20908,#16967,#16968);
#15319=AXIS2_PLACEMENT_3D('',#20910,#16970,#16971);
#15320=AXIS2_PLACEMENT_3D('',#20911,#16972,#16973);
#15321=AXIS2_PLACEMENT_3D('',#20913,#16975,#16976);
#15322=AXIS2_PLACEMENT_3D('',#20915,#16978,#16979);
#15323=AXIS2_PLACEMENT_3D('',#20916,#16980,#16981);
#15324=AXIS2_PLACEMENT_3D('',#20917,#16982,#16983);
#15325=AXIS2_PLACEMENT_3D('',#20919,#16985,#16986);
#15326=AXIS2_PLACEMENT_3D('',#20921,#16988,#16989);
#15327=AXIS2_PLACEMENT_3D('',#20922,#16990,#16991);
#15328=AXIS2_PLACEMENT_3D('',#20923,#16992,#16993);
#15329=AXIS2_PLACEMENT_3D('',#20925,#16994,#16995);
#15330=AXIS2_PLACEMENT_3D('',#20929,#16997,#16998);
#15331=AXIS2_PLACEMENT_3D('',#20937,#16999,#17000);
#15332=AXIS2_PLACEMENT_3D('',#20938,#17001,#17002);
#15333=AXIS2_PLACEMENT_3D('',#20940,#17003,#17004);
#15334=AXIS2_PLACEMENT_3D('',#20943,#17006,#17007);
#15335=AXIS2_PLACEMENT_3D('',#20944,#17008,#17009);
#15336=AXIS2_PLACEMENT_3D('',#20945,#17010,#17011);
#15337=AXIS2_PLACEMENT_3D('',#20948,#17013,#17014);
#15338=AXIS2_PLACEMENT_3D('',#20949,#17015,#17016);
#15339=AXIS2_PLACEMENT_3D('',#20951,#17017,#17018);
#15340=AXIS2_PLACEMENT_3D('',#20955,#17020,#17021);
#15341=AXIS2_PLACEMENT_3D('',#20963,#17022,#17023);
#15342=AXIS2_PLACEMENT_3D('',#20964,#17024,#17025);
#15343=AXIS2_PLACEMENT_3D('',#20966,#17026,#17027);
#15344=AXIS2_PLACEMENT_3D('',#20969,#17029,#17030);
#15345=AXIS2_PLACEMENT_3D('',#20970,#17031,#17032);
#15346=AXIS2_PLACEMENT_3D('',#20971,#17033,#17034);
#15347=AXIS2_PLACEMENT_3D('',#20974,#17036,#17037);
#15348=AXIS2_PLACEMENT_3D('',#20975,#17038,#17039);
#15349=AXIS2_PLACEMENT_3D('',#20977,#17040,#17041);
#15350=AXIS2_PLACEMENT_3D('',#20981,#17043,#17044);
#15351=AXIS2_PLACEMENT_3D('',#20989,#17045,#17046);
#15352=AXIS2_PLACEMENT_3D('',#20990,#17047,#17048);
#15353=AXIS2_PLACEMENT_3D('',#20992,#17049,#17050);
#15354=AXIS2_PLACEMENT_3D('',#20995,#17052,#17053);
#15355=AXIS2_PLACEMENT_3D('',#20996,#17054,#17055);
#15356=AXIS2_PLACEMENT_3D('',#20997,#17056,#17057);
#15357=AXIS2_PLACEMENT_3D('',#21000,#17059,#17060);
#15358=AXIS2_PLACEMENT_3D('',#21001,#17061,#17062);
#15359=AXIS2_PLACEMENT_3D('',#21010,#17067,#17068);
#15360=AXIS2_PLACEMENT_3D('',#21013,#17070,#17071);
#15361=AXIS2_PLACEMENT_3D('',#21014,#17072,#17073);
#15362=AXIS2_PLACEMENT_3D('',#21017,#17075,#17076);
#15363=AXIS2_PLACEMENT_3D('',#21018,#17077,#17078);
#15364=AXIS2_PLACEMENT_3D('',#21021,#17080,#17081);
#15365=AXIS2_PLACEMENT_3D('',#21022,#17082,#17083);
#15366=AXIS2_PLACEMENT_3D('',#21024,#17084,#17085);
#15367=AXIS2_PLACEMENT_3D('',#21025,#17086,#17087);
#15368=AXIS2_PLACEMENT_3D('',#21027,#17088,#17089);
#15369=AXIS2_PLACEMENT_3D('',#21028,#17090,#17091);
#15370=AXIS2_PLACEMENT_3D('',#21030,#17092,#17093);
#15371=AXIS2_PLACEMENT_3D('',#21031,#17094,#17095);
#15372=AXIS2_PLACEMENT_3D('',#21034,#17097,#17098);
#15373=AXIS2_PLACEMENT_3D('',#21035,#17099,#17100);
#15374=AXIS2_PLACEMENT_3D('',#21038,#17102,#17103);
#15375=AXIS2_PLACEMENT_3D('',#21039,#17104,#17105);
#15376=AXIS2_PLACEMENT_3D('',#21042,#17107,#17108);
#15377=AXIS2_PLACEMENT_3D('',#21043,#17109,#17110);
#15378=AXIS2_PLACEMENT_3D('',#21045,#17111,#17112);
#15379=AXIS2_PLACEMENT_3D('',#21049,#17114,#17115);
#15380=AXIS2_PLACEMENT_3D('',#21057,#17116,#17117);
#15381=AXIS2_PLACEMENT_3D('',#21058,#17118,#17119);
#15382=AXIS2_PLACEMENT_3D('',#21060,#17120,#17121);
#15383=AXIS2_PLACEMENT_3D('',#21063,#17123,#17124);
#15384=AXIS2_PLACEMENT_3D('',#21064,#17125,#17126);
#15385=AXIS2_PLACEMENT_3D('',#21065,#17127,#17128);
#15386=AXIS2_PLACEMENT_3D('',#21068,#17130,#17131);
#15387=AXIS2_PLACEMENT_3D('',#21069,#17132,#17133);
#15388=AXIS2_PLACEMENT_3D('',#21071,#17134,#17135);
#15389=AXIS2_PLACEMENT_3D('',#21075,#17137,#17138);
#15390=AXIS2_PLACEMENT_3D('',#21083,#17139,#17140);
#15391=AXIS2_PLACEMENT_3D('',#21084,#17141,#17142);
#15392=AXIS2_PLACEMENT_3D('',#21086,#17143,#17144);
#15393=AXIS2_PLACEMENT_3D('',#21089,#17146,#17147);
#15394=AXIS2_PLACEMENT_3D('',#21090,#17148,#17149);
#15395=AXIS2_PLACEMENT_3D('',#21091,#17150,#17151);
#15396=AXIS2_PLACEMENT_3D('',#21094,#17153,#17154);
#15397=AXIS2_PLACEMENT_3D('',#21095,#17155,#17156);
#15398=AXIS2_PLACEMENT_3D('',#21097,#17157,#17158);
#15399=AXIS2_PLACEMENT_3D('',#21101,#17160,#17161);
#15400=AXIS2_PLACEMENT_3D('',#21109,#17162,#17163);
#15401=AXIS2_PLACEMENT_3D('',#21110,#17164,#17165);
#15402=AXIS2_PLACEMENT_3D('',#21112,#17166,#17167);
#15403=AXIS2_PLACEMENT_3D('',#21115,#17169,#17170);
#15404=AXIS2_PLACEMENT_3D('',#21116,#17171,#17172);
#15405=AXIS2_PLACEMENT_3D('',#21117,#17173,#17174);
#15406=AXIS2_PLACEMENT_3D('',#21120,#17176,#17177);
#15407=AXIS2_PLACEMENT_3D('',#21121,#17178,#17179);
#15408=AXIS2_PLACEMENT_3D('',#21130,#17184,#17185);
#15409=AXIS2_PLACEMENT_3D('',#21133,#17187,#17188);
#15410=AXIS2_PLACEMENT_3D('',#21134,#17189,#17190);
#15411=AXIS2_PLACEMENT_3D('',#21137,#17192,#17193);
#15412=AXIS2_PLACEMENT_3D('',#21138,#17194,#17195);
#15413=AXIS2_PLACEMENT_3D('',#21141,#17197,#17198);
#15414=AXIS2_PLACEMENT_3D('',#21142,#17199,#17200);
#15415=AXIS2_PLACEMENT_3D('',#21144,#17201,#17202);
#15416=AXIS2_PLACEMENT_3D('',#21145,#17203,#17204);
#15417=AXIS2_PLACEMENT_3D('',#21147,#17205,#17206);
#15418=AXIS2_PLACEMENT_3D('',#21148,#17207,#17208);
#15419=AXIS2_PLACEMENT_3D('',#21150,#17209,#17210);
#15420=AXIS2_PLACEMENT_3D('',#21151,#17211,#17212);
#15421=AXIS2_PLACEMENT_3D('',#21154,#17214,#17215);
#15422=AXIS2_PLACEMENT_3D('',#21155,#17216,#17217);
#15423=AXIS2_PLACEMENT_3D('',#21158,#17219,#17220);
#15424=AXIS2_PLACEMENT_3D('',#21159,#17221,#17222);
#15425=AXIS2_PLACEMENT_3D('',#21162,#17224,#17225);
#15426=AXIS2_PLACEMENT_3D('',#21163,#17226,#17227);
#15427=AXIS2_PLACEMENT_3D('',#21165,#17228,#17229);
#15428=AXIS2_PLACEMENT_3D('',#21168,#17231,#17232);
#15429=AXIS2_PLACEMENT_3D('',#21169,#17233,#17234);
#15430=AXIS2_PLACEMENT_3D('',#21199,#17249,#17250);
#15431=AXIS2_PLACEMENT_3D('',#21201,#17251,#17252);
#15432=AXIS2_PLACEMENT_3D('',#21203,#17253,#17254);
#15433=AXIS2_PLACEMENT_3D('',#21204,#17255,#17256);
#15434=AXIS2_PLACEMENT_3D('',#21208,#17258,#17259);
#15435=AXIS2_PLACEMENT_3D('',#21209,#17260,#17261);
#15436=AXIS2_PLACEMENT_3D('',#21210,#17262,#17263);
#15437=AXIS2_PLACEMENT_3D('',#21212,#17264,#17265);
#15438=AXIS2_PLACEMENT_3D('',#21214,#17267,#17268);
#15439=AXIS2_PLACEMENT_3D('',#21218,#17270,#17271);
#15440=AXIS2_PLACEMENT_3D('',#21219,#17272,#17273);
#15441=AXIS2_PLACEMENT_3D('',#21220,#17274,#17275);
#15442=AXIS2_PLACEMENT_3D('',#21222,#17276,#17277);
#15443=AXIS2_PLACEMENT_3D('',#21224,#17279,#17280);
#15444=AXIS2_PLACEMENT_3D('',#21228,#17282,#17283);
#15445=AXIS2_PLACEMENT_3D('',#21229,#17284,#17285);
#15446=AXIS2_PLACEMENT_3D('',#21230,#17286,#17287);
#15447=AXIS2_PLACEMENT_3D('',#21232,#17288,#17289);
#15448=AXIS2_PLACEMENT_3D('',#21234,#17291,#17292);
#15449=AXIS2_PLACEMENT_3D('',#21238,#17294,#17295);
#15450=AXIS2_PLACEMENT_3D('',#21239,#17296,#17297);
#15451=AXIS2_PLACEMENT_3D('',#21240,#17298,#17299);
#15452=AXIS2_PLACEMENT_3D('',#21243,#17301,#17302);
#15453=AXIS2_PLACEMENT_3D('',#21246,#17304,#17305);
#15454=AXIS2_PLACEMENT_3D('',#21249,#17307,#17308);
#15455=AXIS2_PLACEMENT_3D('',#21252,#17310,#17311);
#15456=AXIS2_PLACEMENT_3D('',#21254,#17312,#17313);
#15457=AXIS2_PLACEMENT_3D('',#21257,#17315,#17316);
#15458=AXIS2_PLACEMENT_3D('',#21258,#17317,#17318);
#15459=AXIS2_PLACEMENT_3D('',#21288,#17333,#17334);
#15460=AXIS2_PLACEMENT_3D('',#21290,#17335,#17336);
#15461=AXIS2_PLACEMENT_3D('',#21292,#17337,#17338);
#15462=AXIS2_PLACEMENT_3D('',#21293,#17339,#17340);
#15463=AXIS2_PLACEMENT_3D('',#21297,#17342,#17343);
#15464=AXIS2_PLACEMENT_3D('',#21298,#17344,#17345);
#15465=AXIS2_PLACEMENT_3D('',#21299,#17346,#17347);
#15466=AXIS2_PLACEMENT_3D('',#21301,#17348,#17349);
#15467=AXIS2_PLACEMENT_3D('',#21303,#17351,#17352);
#15468=AXIS2_PLACEMENT_3D('',#21307,#17354,#17355);
#15469=AXIS2_PLACEMENT_3D('',#21308,#17356,#17357);
#15470=AXIS2_PLACEMENT_3D('',#21309,#17358,#17359);
#15471=AXIS2_PLACEMENT_3D('',#21311,#17360,#17361);
#15472=AXIS2_PLACEMENT_3D('',#21313,#17363,#17364);
#15473=AXIS2_PLACEMENT_3D('',#21317,#17366,#17367);
#15474=AXIS2_PLACEMENT_3D('',#21318,#17368,#17369);
#15475=AXIS2_PLACEMENT_3D('',#21319,#17370,#17371);
#15476=AXIS2_PLACEMENT_3D('',#21321,#17372,#17373);
#15477=AXIS2_PLACEMENT_3D('',#21323,#17375,#17376);
#15478=AXIS2_PLACEMENT_3D('',#21327,#17378,#17379);
#15479=AXIS2_PLACEMENT_3D('',#21328,#17380,#17381);
#15480=AXIS2_PLACEMENT_3D('',#21329,#17382,#17383);
#15481=AXIS2_PLACEMENT_3D('',#21332,#17385,#17386);
#15482=AXIS2_PLACEMENT_3D('',#21335,#17388,#17389);
#15483=AXIS2_PLACEMENT_3D('',#21338,#17391,#17392);
#15484=AXIS2_PLACEMENT_3D('',#21341,#17394,#17395);
#15485=AXIS2_PLACEMENT_3D('',#21343,#17396,#17397);
#15486=AXIS2_PLACEMENT_3D('',#21346,#17399,#17400);
#15487=AXIS2_PLACEMENT_3D('',#21347,#17401,#17402);
#15488=AXIS2_PLACEMENT_3D('',#21357,#17407,#17408);
#15489=AXIS2_PLACEMENT_3D('',#21359,#17409,#17410);
#15490=AXIS2_PLACEMENT_3D('',#21361,#17411,#17412);
#15491=AXIS2_PLACEMENT_3D('',#21363,#17413,#17414);
#15492=AXIS2_PLACEMENT_3D('',#21365,#17415,#17416);
#15493=AXIS2_PLACEMENT_3D('',#21367,#17417,#17418);
#15494=AXIS2_PLACEMENT_3D('',#21369,#17419,#17420);
#15495=AXIS2_PLACEMENT_3D('',#21371,#17421,#17422);
#15496=AXIS2_PLACEMENT_3D('',#21373,#17423,#17424);
#15497=AXIS2_PLACEMENT_3D('',#21375,#17425,#17426);
#15498=AXIS2_PLACEMENT_3D('',#21377,#17427,#17428);
#15499=AXIS2_PLACEMENT_3D('',#21379,#17429,#17430);
#15500=AXIS2_PLACEMENT_3D('',#21381,#17431,#17432);
#15501=AXIS2_PLACEMENT_3D('',#21382,#17433,#17434);
#15502=AXIS2_PLACEMENT_3D('',#21385,#17436,#17437);
#15503=AXIS2_PLACEMENT_3D('',#21386,#17438,#17439);
#15504=AXIS2_PLACEMENT_3D('',#21388,#17440,#17441);
#15505=AXIS2_PLACEMENT_3D('',#21390,#17443,#17444);
#15506=AXIS2_PLACEMENT_3D('',#21393,#17446,#17447);
#15507=AXIS2_PLACEMENT_3D('',#21394,#17448,#17449);
#15508=AXIS2_PLACEMENT_3D('',#21396,#17450,#17451);
#15509=AXIS2_PLACEMENT_3D('',#21398,#17453,#17454);
#15510=AXIS2_PLACEMENT_3D('',#21401,#17456,#17457);
#15511=AXIS2_PLACEMENT_3D('',#21402,#17458,#17459);
#15512=AXIS2_PLACEMENT_3D('',#21404,#17460,#17461);
#15513=AXIS2_PLACEMENT_3D('',#21406,#17463,#17464);
#15514=AXIS2_PLACEMENT_3D('',#21409,#17466,#17467);
#15515=AXIS2_PLACEMENT_3D('',#21410,#17468,#17469);
#15516=AXIS2_PLACEMENT_3D('',#21412,#17470,#17471);
#15517=AXIS2_PLACEMENT_3D('',#21414,#17473,#17474);
#15518=AXIS2_PLACEMENT_3D('',#21417,#17476,#17477);
#15519=AXIS2_PLACEMENT_3D('',#21418,#17478,#17479);
#15520=AXIS2_PLACEMENT_3D('',#21420,#17480,#17481);
#15521=AXIS2_PLACEMENT_3D('',#21422,#17483,#17484);
#15522=AXIS2_PLACEMENT_3D('',#21425,#17486,#17487);
#15523=AXIS2_PLACEMENT_3D('',#21426,#17488,#17489);
#15524=AXIS2_PLACEMENT_3D('',#21429,#17491,#17492);
#15525=AXIS2_PLACEMENT_3D('',#21432,#17494,#17495);
#15526=AXIS2_PLACEMENT_3D('',#21435,#17497,#17498);
#15527=AXIS2_PLACEMENT_3D('',#21438,#17500,#17501);
#15528=AXIS2_PLACEMENT_3D('',#21441,#17503,#17504);
#15529=AXIS2_PLACEMENT_3D('',#21444,#17506,#17507);
#15530=AXIS2_PLACEMENT_3D('',#21446,#17508,#17509);
#15531=AXIS2_PLACEMENT_3D('',#21448,#17511,#17512);
#15532=AXIS2_PLACEMENT_3D('',#21451,#17514,#17515);
#15533=AXIS2_PLACEMENT_3D('',#21452,#17516,#17517);
#15534=AXIS2_PLACEMENT_3D('',#21454,#17518,#17519);
#15535=AXIS2_PLACEMENT_3D('',#21456,#17521,#17522);
#15536=AXIS2_PLACEMENT_3D('',#21459,#17524,#17525);
#15537=AXIS2_PLACEMENT_3D('',#21460,#17526,#17527);
#15538=AXIS2_PLACEMENT_3D('',#21462,#17528,#17529);
#15539=AXIS2_PLACEMENT_3D('',#21464,#17531,#17532);
#15540=AXIS2_PLACEMENT_3D('',#21467,#17534,#17535);
#15541=AXIS2_PLACEMENT_3D('',#21468,#17536,#17537);
#15542=AXIS2_PLACEMENT_3D('',#21470,#17538,#17539);
#15543=AXIS2_PLACEMENT_3D('',#21472,#17541,#17542);
#15544=AXIS2_PLACEMENT_3D('',#21475,#17544,#17545);
#15545=AXIS2_PLACEMENT_3D('',#21476,#17546,#17547);
#15546=AXIS2_PLACEMENT_3D('',#21478,#17548,#17549);
#15547=AXIS2_PLACEMENT_3D('',#21480,#17551,#17552);
#15548=AXIS2_PLACEMENT_3D('',#21483,#17554,#17555);
#15549=AXIS2_PLACEMENT_3D('',#21484,#17556,#17557);
#15550=AXIS2_PLACEMENT_3D('',#21486,#17558,#17559);
#15551=AXIS2_PLACEMENT_3D('',#21488,#17561,#17562);
#15552=AXIS2_PLACEMENT_3D('',#21491,#17564,#17565);
#15553=AXIS2_PLACEMENT_3D('',#21492,#17566,#17567);
#15554=AXIS2_PLACEMENT_3D('',#21494,#17568,#17569);
#15555=AXIS2_PLACEMENT_3D('',#21496,#17571,#17572);
#15556=AXIS2_PLACEMENT_3D('',#21499,#17574,#17575);
#15557=AXIS2_PLACEMENT_3D('',#21500,#17576,#17577);
#15558=AXIS2_PLACEMENT_3D('',#21502,#17578,#17579);
#15559=AXIS2_PLACEMENT_3D('',#21504,#17581,#17582);
#15560=AXIS2_PLACEMENT_3D('',#21507,#17584,#17585);
#15561=AXIS2_PLACEMENT_3D('',#21508,#17586,#17587);
#15562=AXIS2_PLACEMENT_3D('',#21510,#17588,#17589);
#15563=AXIS2_PLACEMENT_3D('',#21511,#17590,#17591);
#15564=AXIS2_PLACEMENT_3D('',#21513,#17592,#17593);
#15565=AXIS2_PLACEMENT_3D('',#21514,#17594,#17595);
#15566=AXIS2_PLACEMENT_3D('',#21516,#17596,#17597);
#15567=AXIS2_PLACEMENT_3D('',#21517,#17598,#17599);
#15568=AXIS2_PLACEMENT_3D('',#21519,#17600,#17601);
#15569=AXIS2_PLACEMENT_3D('',#21520,#17602,#17603);
#15570=AXIS2_PLACEMENT_3D('',#21522,#17604,#17605);
#15571=AXIS2_PLACEMENT_3D('',#21523,#17606,#17607);
#15572=AXIS2_PLACEMENT_3D('',#21525,#17608,#17609);
#15573=AXIS2_PLACEMENT_3D('',#21526,#17610,#17611);
#15574=AXIS2_PLACEMENT_3D('',#21528,#17612,#17613);
#15575=AXIS2_PLACEMENT_3D('',#21529,#17614,#17615);
#15576=AXIS2_PLACEMENT_3D('',#21531,#17616,#17617);
#15577=AXIS2_PLACEMENT_3D('',#21532,#17618,#17619);
#15578=AXIS2_PLACEMENT_3D('',#21535,#17621,#17622);
#15579=AXIS2_PLACEMENT_3D('',#21536,#17623,#17624);
#15580=AXIS2_PLACEMENT_3D('',#21539,#17626,#17627);
#15581=AXIS2_PLACEMENT_3D('',#21540,#17628,#17629);
#15582=AXIS2_PLACEMENT_3D('',#21543,#17631,#17632);
#15583=AXIS2_PLACEMENT_3D('',#21544,#17633,#17634);
#15584=AXIS2_PLACEMENT_3D('',#21547,#17636,#17637);
#15585=AXIS2_PLACEMENT_3D('',#21548,#17638,#17639);
#15586=AXIS2_PLACEMENT_3D('',#21551,#17641,#17642);
#15587=AXIS2_PLACEMENT_3D('',#21552,#17643,#17644);
#15588=AXIS2_PLACEMENT_3D('',#21555,#17646,#17647);
#15589=AXIS2_PLACEMENT_3D('',#21556,#17648,#17649);
#15590=AXIS2_PLACEMENT_3D('',#21559,#17651,#17652);
#15591=AXIS2_PLACEMENT_3D('',#21560,#17653,#17654);
#15592=AXIS2_PLACEMENT_3D('',#21563,#17656,#17657);
#15593=AXIS2_PLACEMENT_3D('',#21564,#17658,#17659);
#15594=AXIS2_PLACEMENT_3D('',#21569,#17663,#17664);
#15595=AXIS2_PLACEMENT_3D('',#21574,#17668,#17669);
#15596=AXIS2_PLACEMENT_3D('',#21577,#17672,#17673);
#15597=AXIS2_PLACEMENT_3D('',#21582,#17677,#17678);
#15598=AXIS2_PLACEMENT_3D('',#21584,#17680,#17681);
#15599=AXIS2_PLACEMENT_3D('',#21587,#17684,#17685);
#15600=AXIS2_PLACEMENT_3D('',#21591,#17688,#17689);
#15601=AXIS2_PLACEMENT_3D('',#21593,#17691,#17692);
#15602=AXIS2_PLACEMENT_3D('',#21594,#17693,#17694);
#15603=AXIS2_PLACEMENT_3D('',#21597,#17697,#17698);
#15604=AXIS2_PLACEMENT_3D('',#21599,#17700,#17701);
#15605=AXIS2_PLACEMENT_3D('',#21602,#17704,#17705);
#15606=AXIS2_PLACEMENT_3D('',#21604,#17707,#17708);
#15607=AXIS2_PLACEMENT_3D('',#21605,#17709,#17710);
#15608=AXIS2_PLACEMENT_3D('',#21606,#17711,#17712);
#15609=AXIS2_PLACEMENT_3D('',#21608,#17714,#17715);
#15610=AXIS2_PLACEMENT_3D('',#21610,#17717,#17718);
#15611=AXIS2_PLACEMENT_3D('',#21612,#17720,#17721);
#15612=AXIS2_PLACEMENT_3D('',#21614,#17723,#17724);
#15613=AXIS2_PLACEMENT_3D('',#21616,#17726,#17727);
#15614=AXIS2_PLACEMENT_3D('',#21617,#17728,#17729);
#15615=AXIS2_PLACEMENT_3D('',#21618,#17730,#17731);
#15616=AXIS2_PLACEMENT_3D('',#21620,#17732,#17733);
#15617=AXIS2_PLACEMENT_3D('',#21623,#17735,#17736);
#15618=AXIS2_PLACEMENT_3D('',#21624,#17737,#17738);
#15619=AXIS2_PLACEMENT_3D('',#21658,#17756,#17757);
#15620=AXIS2_PLACEMENT_3D('',#21662,#17759,#17760);
#15621=AXIS2_PLACEMENT_3D('',#21663,#17761,#17762);
#15622=AXIS2_PLACEMENT_3D('',#21664,#17763,#17764);
#15623=AXIS2_PLACEMENT_3D('',#21667,#17766,#17767);
#15624=AXIS2_PLACEMENT_3D('',#21669,#17768,#17769);
#15625=AXIS2_PLACEMENT_3D('',#21672,#17771,#17772);
#15626=AXIS2_PLACEMENT_3D('',#21673,#17773,#17774);
#15627=AXIS2_PLACEMENT_3D('',#21707,#17792,#17793);
#15628=AXIS2_PLACEMENT_3D('',#21711,#17795,#17796);
#15629=AXIS2_PLACEMENT_3D('',#21712,#17797,#17798);
#15630=AXIS2_PLACEMENT_3D('',#21713,#17799,#17800);
#15631=AXIS2_PLACEMENT_3D('',#21716,#17802,#17803);
#15632=AXIS2_PLACEMENT_3D('',#21718,#17804,#17805);
#15633=AXIS2_PLACEMENT_3D('',#21721,#17807,#17808);
#15634=AXIS2_PLACEMENT_3D('',#21722,#17809,#17810);
#15635=AXIS2_PLACEMENT_3D('',#21726,#17813,#17814);
#15636=AXIS2_PLACEMENT_3D('',#21728,#17815,#17816);
#15637=AXIS2_PLACEMENT_3D('',#21729,#17817,#17818);
#15638=AXIS2_PLACEMENT_3D('',#21733,#17820,#17821);
#15639=AXIS2_PLACEMENT_3D('',#21737,#17823,#17824);
#15640=AXIS2_PLACEMENT_3D('',#21739,#17825,#17826);
#15641=AXIS2_PLACEMENT_3D('',#21741,#17827,#17828);
#15642=AXIS2_PLACEMENT_3D('',#21745,#17830,#17831);
#15643=AXIS2_PLACEMENT_3D('',#21749,#17833,#17834);
#15644=AXIS2_PLACEMENT_3D('',#21751,#17835,#17836);
#15645=AXIS2_PLACEMENT_3D('',#21753,#17837,#17838);
#15646=AXIS2_PLACEMENT_3D('',#21756,#17840,#17841);
#15647=AXIS2_PLACEMENT_3D('',#21757,#17842,#17843);
#15648=AXIS2_PLACEMENT_3D('',#21759,#17844,#17845);
#15649=AXIS2_PLACEMENT_3D('',#21761,#17847,#17848);
#15650=AXIS2_PLACEMENT_3D('',#21765,#17850,#17851);
#15651=AXIS2_PLACEMENT_3D('',#21769,#17853,#17854);
#15652=AXIS2_PLACEMENT_3D('',#21771,#17855,#17856);
#15653=AXIS2_PLACEMENT_3D('',#21773,#17857,#17858);
#15654=AXIS2_PLACEMENT_3D('',#21777,#17860,#17861);
#15655=AXIS2_PLACEMENT_3D('',#21781,#17863,#17864);
#15656=AXIS2_PLACEMENT_3D('',#21783,#17865,#17866);
#15657=AXIS2_PLACEMENT_3D('',#21785,#17867,#17868);
#15658=AXIS2_PLACEMENT_3D('',#21788,#17870,#17871);
#15659=AXIS2_PLACEMENT_3D('',#21789,#17872,#17873);
#15660=AXIS2_PLACEMENT_3D('',#21791,#17874,#17875);
#15661=AXIS2_PLACEMENT_3D('',#21793,#17877,#17878);
#15662=AXIS2_PLACEMENT_3D('',#21797,#17880,#17881);
#15663=AXIS2_PLACEMENT_3D('',#21801,#17883,#17884);
#15664=AXIS2_PLACEMENT_3D('',#21803,#17885,#17886);
#15665=AXIS2_PLACEMENT_3D('',#21805,#17887,#17888);
#15666=AXIS2_PLACEMENT_3D('',#21809,#17890,#17891);
#15667=AXIS2_PLACEMENT_3D('',#21813,#17893,#17894);
#15668=AXIS2_PLACEMENT_3D('',#21815,#17895,#17896);
#15669=AXIS2_PLACEMENT_3D('',#21817,#17897,#17898);
#15670=AXIS2_PLACEMENT_3D('',#21820,#17900,#17901);
#15671=AXIS2_PLACEMENT_3D('',#21821,#17902,#17903);
#15672=AXIS2_PLACEMENT_3D('',#21823,#17905,#17906);
#15673=AXIS2_PLACEMENT_3D('',#21825,#17908,#17909);
#15674=AXIS2_PLACEMENT_3D('',#21827,#17911,#17912);
#15675=AXIS2_PLACEMENT_3D('',#21829,#17914,#17915);
#15676=AXIS2_PLACEMENT_3D('',#21831,#17917,#17918);
#15677=AXIS2_PLACEMENT_3D('',#21833,#17920,#17921);
#15678=AXIS2_PLACEMENT_3D('',#21839,#17927,#17928);
#15679=AXIS2_PLACEMENT_3D('',#21841,#17930,#17931);
#15680=AXIS2_PLACEMENT_3D('',#21843,#17933,#17934);
#15681=AXIS2_PLACEMENT_3D('',#21845,#17936,#17937);
#15682=AXIS2_PLACEMENT_3D('',#21847,#17939,#17940);
#15683=AXIS2_PLACEMENT_3D('',#21849,#17942,#17943);
#15684=AXIS2_PLACEMENT_3D('',#21851,#17945,#17946);
#15685=AXIS2_PLACEMENT_3D('',#21853,#17948,#17949);
#15686=AXIS2_PLACEMENT_3D('',#21855,#17951,#17952);
#15687=AXIS2_PLACEMENT_3D('',#21857,#17954,#17955);
#15688=AXIS2_PLACEMENT_3D('',#21863,#17959,#17960);
#15689=AXIS2_PLACEMENT_3D('',#21869,#17964,#17965);
#15690=AXIS2_PLACEMENT_3D('',#21872,#17968,#17969);
#15691=AXIS2_PLACEMENT_3D('',#21878,#17973,#17974);
#15692=AXIS2_PLACEMENT_3D('',#21883,#17978,#17979);
#15693=AXIS2_PLACEMENT_3D('',#21887,#17982,#17983);
#15694=AXIS2_PLACEMENT_3D('',#21889,#17985,#17986);
#15695=AXIS2_PLACEMENT_3D('',#21891,#17988,#17989);
#15696=AXIS2_PLACEMENT_3D('',#21893,#17991,#17992);
#15697=AXIS2_PLACEMENT_3D('',#21894,#17993,#17994);
#15698=AXIS2_PLACEMENT_3D('',#21897,#17997,#17998);
#15699=AXIS2_PLACEMENT_3D('',#21899,#18000,#18001);
#15700=AXIS2_PLACEMENT_3D('',#21900,#18002,#18003);
#15701=AXIS2_PLACEMENT_3D('',#21901,#18004,#18005);
#15702=AXIS2_PLACEMENT_3D('',#21902,#18006,#18007);
#15703=AXIS2_PLACEMENT_3D('',#21904,#18009,#18010);
#15704=AXIS2_PLACEMENT_3D('',#21906,#18012,#18013);
#15705=AXIS2_PLACEMENT_3D('',#21907,#18014,#18015);
#15706=AXIS2_PLACEMENT_3D('',#21908,#18016,#18017);
#15707=AXIS2_PLACEMENT_3D('',#21910,#18018,#18019);
#15708=AXIS2_PLACEMENT_3D('',#21914,#18021,#18022);
#15709=AXIS2_PLACEMENT_3D('',#21915,#18023,#18024);
#15710=AXIS2_PLACEMENT_3D('',#21916,#18025,#18026);
#15711=AXIS2_PLACEMENT_3D('',#21950,#18044,#18045);
#15712=AXIS2_PLACEMENT_3D('',#21954,#18047,#18048);
#15713=AXIS2_PLACEMENT_3D('',#21955,#18049,#18050);
#15714=AXIS2_PLACEMENT_3D('',#21956,#18051,#18052);
#15715=AXIS2_PLACEMENT_3D('',#21959,#18054,#18055);
#15716=AXIS2_PLACEMENT_3D('',#21961,#18056,#18057);
#15717=AXIS2_PLACEMENT_3D('',#21965,#18059,#18060);
#15718=AXIS2_PLACEMENT_3D('',#21966,#18061,#18062);
#15719=AXIS2_PLACEMENT_3D('',#21967,#18063,#18064);
#15720=AXIS2_PLACEMENT_3D('',#22001,#18082,#18083);
#15721=AXIS2_PLACEMENT_3D('',#22005,#18085,#18086);
#15722=AXIS2_PLACEMENT_3D('',#22006,#18087,#18088);
#15723=AXIS2_PLACEMENT_3D('',#22007,#18089,#18090);
#15724=AXIS2_PLACEMENT_3D('',#22010,#18092,#18093);
#15725=AXIS2_PLACEMENT_3D('',#22012,#18094,#18095);
#15726=AXIS2_PLACEMENT_3D('',#22015,#18097,#18098);
#15727=AXIS2_PLACEMENT_3D('',#22016,#18099,#18100);
#15728=AXIS2_PLACEMENT_3D('',#22020,#18103,#18104);
#15729=AXIS2_PLACEMENT_3D('',#22022,#18105,#18106);
#15730=AXIS2_PLACEMENT_3D('',#22024,#18107,#18108);
#15731=AXIS2_PLACEMENT_3D('',#22025,#18109,#18110);
#15732=AXIS2_PLACEMENT_3D('',#22029,#18112,#18113);
#15733=AXIS2_PLACEMENT_3D('',#22033,#18115,#18116);
#15734=AXIS2_PLACEMENT_3D('',#22035,#18117,#18118);
#15735=AXIS2_PLACEMENT_3D('',#22037,#18119,#18120);
#15736=AXIS2_PLACEMENT_3D('',#22041,#18122,#18123);
#15737=AXIS2_PLACEMENT_3D('',#22045,#18125,#18126);
#15738=AXIS2_PLACEMENT_3D('',#22047,#18127,#18128);
#15739=AXIS2_PLACEMENT_3D('',#22049,#18129,#18130);
#15740=AXIS2_PLACEMENT_3D('',#22052,#18132,#18133);
#15741=AXIS2_PLACEMENT_3D('',#22053,#18134,#18135);
#15742=AXIS2_PLACEMENT_3D('',#22055,#18136,#18137);
#15743=AXIS2_PLACEMENT_3D('',#22057,#18139,#18140);
#15744=AXIS2_PLACEMENT_3D('',#22061,#18142,#18143);
#15745=AXIS2_PLACEMENT_3D('',#22065,#18145,#18146);
#15746=AXIS2_PLACEMENT_3D('',#22067,#18147,#18148);
#15747=AXIS2_PLACEMENT_3D('',#22069,#18149,#18150);
#15748=AXIS2_PLACEMENT_3D('',#22073,#18152,#18153);
#15749=AXIS2_PLACEMENT_3D('',#22077,#18155,#18156);
#15750=AXIS2_PLACEMENT_3D('',#22079,#18157,#18158);
#15751=AXIS2_PLACEMENT_3D('',#22081,#18159,#18160);
#15752=AXIS2_PLACEMENT_3D('',#22084,#18162,#18163);
#15753=AXIS2_PLACEMENT_3D('',#22085,#18164,#18165);
#15754=AXIS2_PLACEMENT_3D('',#22087,#18166,#18167);
#15755=AXIS2_PLACEMENT_3D('',#22089,#18169,#18170);
#15756=AXIS2_PLACEMENT_3D('',#22093,#18172,#18173);
#15757=AXIS2_PLACEMENT_3D('',#22097,#18175,#18176);
#15758=AXIS2_PLACEMENT_3D('',#22099,#18177,#18178);
#15759=AXIS2_PLACEMENT_3D('',#22101,#18179,#18180);
#15760=AXIS2_PLACEMENT_3D('',#22105,#18182,#18183);
#15761=AXIS2_PLACEMENT_3D('',#22109,#18185,#18186);
#15762=AXIS2_PLACEMENT_3D('',#22111,#18187,#18188);
#15763=AXIS2_PLACEMENT_3D('',#22113,#18189,#18190);
#15764=AXIS2_PLACEMENT_3D('',#22116,#18192,#18193);
#15765=AXIS2_PLACEMENT_3D('',#22117,#18194,#18195);
#15766=AXIS2_PLACEMENT_3D('',#22119,#18196,#18197);
#15767=AXIS2_PLACEMENT_3D('',#22121,#18199,#18200);
#15768=AXIS2_PLACEMENT_3D('',#22125,#18202,#18203);
#15769=AXIS2_PLACEMENT_3D('',#22129,#18205,#18206);
#15770=AXIS2_PLACEMENT_3D('',#22131,#18207,#18208);
#15771=AXIS2_PLACEMENT_3D('',#22133,#18209,#18210);
#15772=AXIS2_PLACEMENT_3D('',#22137,#18212,#18213);
#15773=AXIS2_PLACEMENT_3D('',#22141,#18215,#18216);
#15774=AXIS2_PLACEMENT_3D('',#22143,#18217,#18218);
#15775=AXIS2_PLACEMENT_3D('',#22145,#18219,#18220);
#15776=AXIS2_PLACEMENT_3D('',#22148,#18222,#18223);
#15777=AXIS2_PLACEMENT_3D('',#22149,#18224,#18225);
#15778=AXIS2_PLACEMENT_3D('',#22151,#18227,#18228);
#15779=AXIS2_PLACEMENT_3D('',#22153,#18230,#18231);
#15780=AXIS2_PLACEMENT_3D('',#22155,#18233,#18234);
#15781=AXIS2_PLACEMENT_3D('',#22157,#18236,#18237);
#15782=AXIS2_PLACEMENT_3D('',#22159,#18239,#18240);
#15783=AXIS2_PLACEMENT_3D('',#22161,#18242,#18243);
#15784=AXIS2_PLACEMENT_3D('',#22163,#18245,#18246);
#15785=AXIS2_PLACEMENT_3D('',#22165,#18248,#18249);
#15786=AXIS2_PLACEMENT_3D('',#22172,#18256,#18257);
#15787=AXIS2_PLACEMENT_3D('',#22174,#18259,#18260);
#15788=AXIS2_PLACEMENT_3D('',#22176,#18262,#18263);
#15789=AXIS2_PLACEMENT_3D('',#22178,#18265,#18266);
#15790=AXIS2_PLACEMENT_3D('',#22180,#18268,#18269);
#15791=AXIS2_PLACEMENT_3D('',#22182,#18271,#18272);
#15792=AXIS2_PLACEMENT_3D('',#22184,#18274,#18275);
#15793=AXIS2_PLACEMENT_3D('',#22186,#18277,#18278);
#15794=AXIS2_PLACEMENT_3D('',#22188,#18280,#18281);
#15795=AXIS2_PLACEMENT_3D('',#22190,#18283,#18284);
#15796=AXIS2_PLACEMENT_3D('',#22192,#18286,#18287);
#15797=AXIS2_PLACEMENT_3D('',#22194,#18289,#18290);
#15798=AXIS2_PLACEMENT_3D('',#22196,#18292,#18293);
#15799=AXIS2_PLACEMENT_3D('',#22202,#18297,#18298);
#15800=AXIS2_PLACEMENT_3D('',#22206,#18301,#18302);
#15801=AXIS2_PLACEMENT_3D('',#22212,#18306,#18307);
#15802=AXIS2_PLACEMENT_3D('',#22216,#18310,#18311);
#15803=AXIS2_PLACEMENT_3D('',#22220,#18314,#18315);
#15804=AXIS2_PLACEMENT_3D('',#22224,#18318,#18319);
#15805=AXIS2_PLACEMENT_3D('',#22226,#18321,#18322);
#15806=AXIS2_PLACEMENT_3D('',#22228,#18324,#18325);
#15807=AXIS2_PLACEMENT_3D('',#22231,#18328,#18329);
#15808=AXIS2_PLACEMENT_3D('',#22233,#18331,#18332);
#15809=AXIS2_PLACEMENT_3D('',#22235,#18334,#18335);
#15810=AXIS2_PLACEMENT_3D('',#22236,#18336,#18337);
#15811=AXIS2_PLACEMENT_3D('',#22239,#18340,#18341);
#15812=AXIS2_PLACEMENT_3D('',#22240,#18342,#18343);
#15813=AXIS2_PLACEMENT_3D('',#22241,#18344,#18345);
#15814=AXIS2_PLACEMENT_3D('',#22243,#18347,#18348);
#15815=AXIS2_PLACEMENT_3D('',#22245,#18350,#18351);
#15816=AXIS2_PLACEMENT_3D('',#22246,#18352,#18353);
#15817=AXIS2_PLACEMENT_3D('',#22247,#18354,#18355);
#15818=AXIS2_PLACEMENT_3D('',#22256,#18360,#18361);
#15819=AXIS2_PLACEMENT_3D('',#22258,#18362,#18363);
#15820=AXIS2_PLACEMENT_3D('',#22261,#18365,#18366);
#15821=AXIS2_PLACEMENT_3D('',#22262,#18367,#18368);
#15822=AXIS2_PLACEMENT_3D('',#22268,#18372,#18373);
#15823=AXIS2_PLACEMENT_3D('',#22270,#18374,#18375);
#15824=AXIS2_PLACEMENT_3D('',#22273,#18377,#18378);
#15825=AXIS2_PLACEMENT_3D('',#22274,#18379,#18380);
#15826=AXIS2_PLACEMENT_3D('',#22280,#18384,#18385);
#15827=AXIS2_PLACEMENT_3D('',#22282,#18386,#18387);
#15828=AXIS2_PLACEMENT_3D('',#22285,#18389,#18390);
#15829=AXIS2_PLACEMENT_3D('',#22286,#18391,#18392);
#15830=AXIS2_PLACEMENT_3D('',#22292,#18396,#18397);
#15831=AXIS2_PLACEMENT_3D('',#22293,#18398,#18399);
#15832=AXIS2_PLACEMENT_3D('',#22294,#18400,#18401);
#15833=AXIS2_PLACEMENT_3D('',#22295,#18402,#18403);
#15834=AXIS2_PLACEMENT_3D('',#22304,#18408,#18409);
#15835=AXIS2_PLACEMENT_3D('',#22306,#18410,#18411);
#15836=AXIS2_PLACEMENT_3D('',#22309,#18413,#18414);
#15837=AXIS2_PLACEMENT_3D('',#22310,#18415,#18416);
#15838=AXIS2_PLACEMENT_3D('',#22316,#18420,#18421);
#15839=AXIS2_PLACEMENT_3D('',#22318,#18422,#18423);
#15840=AXIS2_PLACEMENT_3D('',#22321,#18425,#18426);
#15841=AXIS2_PLACEMENT_3D('',#22322,#18427,#18428);
#15842=AXIS2_PLACEMENT_3D('',#22328,#18432,#18433);
#15843=AXIS2_PLACEMENT_3D('',#22330,#18434,#18435);
#15844=AXIS2_PLACEMENT_3D('',#22333,#18437,#18438);
#15845=AXIS2_PLACEMENT_3D('',#22334,#18439,#18440);
#15846=AXIS2_PLACEMENT_3D('',#22340,#18444,#18445);
#15847=AXIS2_PLACEMENT_3D('',#22341,#18446,#18447);
#15848=AXIS2_PLACEMENT_3D('',#22342,#18448,#18449);
#15849=AXIS2_PLACEMENT_3D('',#22343,#18450,#18451);
#15850=AXIS2_PLACEMENT_3D('',#22352,#18456,#18457);
#15851=AXIS2_PLACEMENT_3D('',#22354,#18458,#18459);
#15852=AXIS2_PLACEMENT_3D('',#22357,#18461,#18462);
#15853=AXIS2_PLACEMENT_3D('',#22358,#18463,#18464);
#15854=AXIS2_PLACEMENT_3D('',#22364,#18468,#18469);
#15855=AXIS2_PLACEMENT_3D('',#22366,#18470,#18471);
#15856=AXIS2_PLACEMENT_3D('',#22369,#18473,#18474);
#15857=AXIS2_PLACEMENT_3D('',#22370,#18475,#18476);
#15858=AXIS2_PLACEMENT_3D('',#22376,#18480,#18481);
#15859=AXIS2_PLACEMENT_3D('',#22378,#18482,#18483);
#15860=AXIS2_PLACEMENT_3D('',#22381,#18485,#18486);
#15861=AXIS2_PLACEMENT_3D('',#22382,#18487,#18488);
#15862=AXIS2_PLACEMENT_3D('',#22388,#18492,#18493);
#15863=AXIS2_PLACEMENT_3D('',#22389,#18494,#18495);
#15864=AXIS2_PLACEMENT_3D('',#22390,#18496,#18497);
#15865=AXIS2_PLACEMENT_3D('',#22391,#18498,#18499);
#15866=AXIS2_PLACEMENT_3D('',#22400,#18504,#18505);
#15867=AXIS2_PLACEMENT_3D('',#22402,#18506,#18507);
#15868=AXIS2_PLACEMENT_3D('',#22405,#18509,#18510);
#15869=AXIS2_PLACEMENT_3D('',#22406,#18511,#18512);
#15870=AXIS2_PLACEMENT_3D('',#22412,#18516,#18517);
#15871=AXIS2_PLACEMENT_3D('',#22414,#18518,#18519);
#15872=AXIS2_PLACEMENT_3D('',#22417,#18521,#18522);
#15873=AXIS2_PLACEMENT_3D('',#22418,#18523,#18524);
#15874=AXIS2_PLACEMENT_3D('',#22424,#18528,#18529);
#15875=AXIS2_PLACEMENT_3D('',#22426,#18530,#18531);
#15876=AXIS2_PLACEMENT_3D('',#22429,#18533,#18534);
#15877=AXIS2_PLACEMENT_3D('',#22430,#18535,#18536);
#15878=AXIS2_PLACEMENT_3D('',#22436,#18540,#18541);
#15879=AXIS2_PLACEMENT_3D('',#22437,#18542,#18543);
#15880=AXIS2_PLACEMENT_3D('',#22438,#18544,#18545);
#15881=AXIS2_PLACEMENT_3D('',#22439,#18546,#18547);
#15882=AXIS2_PLACEMENT_3D('',#22448,#18552,#18553);
#15883=AXIS2_PLACEMENT_3D('',#22450,#18554,#18555);
#15884=AXIS2_PLACEMENT_3D('',#22453,#18557,#18558);
#15885=AXIS2_PLACEMENT_3D('',#22454,#18559,#18560);
#15886=AXIS2_PLACEMENT_3D('',#22460,#18564,#18565);
#15887=AXIS2_PLACEMENT_3D('',#22462,#18566,#18567);
#15888=AXIS2_PLACEMENT_3D('',#22465,#18569,#18570);
#15889=AXIS2_PLACEMENT_3D('',#22466,#18571,#18572);
#15890=AXIS2_PLACEMENT_3D('',#22472,#18576,#18577);
#15891=AXIS2_PLACEMENT_3D('',#22474,#18578,#18579);
#15892=AXIS2_PLACEMENT_3D('',#22477,#18581,#18582);
#15893=AXIS2_PLACEMENT_3D('',#22478,#18583,#18584);
#15894=AXIS2_PLACEMENT_3D('',#22484,#18588,#18589);
#15895=AXIS2_PLACEMENT_3D('',#22485,#18590,#18591);
#15896=AXIS2_PLACEMENT_3D('',#22486,#18592,#18593);
#15897=AXIS2_PLACEMENT_3D('',#22487,#18594,#18595);
#15898=AXIS2_PLACEMENT_3D('',#22496,#18600,#18601);
#15899=AXIS2_PLACEMENT_3D('',#22498,#18602,#18603);
#15900=AXIS2_PLACEMENT_3D('',#22501,#18605,#18606);
#15901=AXIS2_PLACEMENT_3D('',#22502,#18607,#18608);
#15902=AXIS2_PLACEMENT_3D('',#22508,#18612,#18613);
#15903=AXIS2_PLACEMENT_3D('',#22510,#18614,#18615);
#15904=AXIS2_PLACEMENT_3D('',#22513,#18617,#18618);
#15905=AXIS2_PLACEMENT_3D('',#22514,#18619,#18620);
#15906=AXIS2_PLACEMENT_3D('',#22520,#18624,#18625);
#15907=AXIS2_PLACEMENT_3D('',#22522,#18626,#18627);
#15908=AXIS2_PLACEMENT_3D('',#22525,#18629,#18630);
#15909=AXIS2_PLACEMENT_3D('',#22526,#18631,#18632);
#15910=AXIS2_PLACEMENT_3D('',#22532,#18636,#18637);
#15911=AXIS2_PLACEMENT_3D('',#22533,#18638,#18639);
#15912=AXIS2_PLACEMENT_3D('',#22534,#18640,#18641);
#15913=AXIS2_PLACEMENT_3D('',#22535,#18642,#18643);
#15914=AXIS2_PLACEMENT_3D('',#22544,#18648,#18649);
#15915=AXIS2_PLACEMENT_3D('',#22546,#18650,#18651);
#15916=AXIS2_PLACEMENT_3D('',#22549,#18653,#18654);
#15917=AXIS2_PLACEMENT_3D('',#22550,#18655,#18656);
#15918=AXIS2_PLACEMENT_3D('',#22556,#18660,#18661);
#15919=AXIS2_PLACEMENT_3D('',#22558,#18662,#18663);
#15920=AXIS2_PLACEMENT_3D('',#22561,#18665,#18666);
#15921=AXIS2_PLACEMENT_3D('',#22562,#18667,#18668);
#15922=AXIS2_PLACEMENT_3D('',#22568,#18672,#18673);
#15923=AXIS2_PLACEMENT_3D('',#22570,#18674,#18675);
#15924=AXIS2_PLACEMENT_3D('',#22573,#18677,#18678);
#15925=AXIS2_PLACEMENT_3D('',#22574,#18679,#18680);
#15926=AXIS2_PLACEMENT_3D('',#22580,#18684,#18685);
#15927=AXIS2_PLACEMENT_3D('',#22581,#18686,#18687);
#15928=AXIS2_PLACEMENT_3D('',#22582,#18688,#18689);
#15929=AXIS2_PLACEMENT_3D('',#22583,#18690,#18691);
#15930=AXIS2_PLACEMENT_3D('',#22592,#18696,#18697);
#15931=AXIS2_PLACEMENT_3D('',#22594,#18698,#18699);
#15932=AXIS2_PLACEMENT_3D('',#22597,#18701,#18702);
#15933=AXIS2_PLACEMENT_3D('',#22598,#18703,#18704);
#15934=AXIS2_PLACEMENT_3D('',#22604,#18708,#18709);
#15935=AXIS2_PLACEMENT_3D('',#22606,#18710,#18711);
#15936=AXIS2_PLACEMENT_3D('',#22609,#18713,#18714);
#15937=AXIS2_PLACEMENT_3D('',#22610,#18715,#18716);
#15938=AXIS2_PLACEMENT_3D('',#22616,#18720,#18721);
#15939=AXIS2_PLACEMENT_3D('',#22618,#18722,#18723);
#15940=AXIS2_PLACEMENT_3D('',#22621,#18725,#18726);
#15941=AXIS2_PLACEMENT_3D('',#22622,#18727,#18728);
#15942=AXIS2_PLACEMENT_3D('',#22628,#18732,#18733);
#15943=AXIS2_PLACEMENT_3D('',#22629,#18734,#18735);
#15944=AXIS2_PLACEMENT_3D('',#22630,#18736,#18737);
#15945=AXIS2_PLACEMENT_3D('',#22631,#18738,#18739);
#15946=AXIS2_PLACEMENT_3D('',#22640,#18744,#18745);
#15947=AXIS2_PLACEMENT_3D('',#22642,#18746,#18747);
#15948=AXIS2_PLACEMENT_3D('',#22645,#18749,#18750);
#15949=AXIS2_PLACEMENT_3D('',#22646,#18751,#18752);
#15950=AXIS2_PLACEMENT_3D('',#22652,#18756,#18757);
#15951=AXIS2_PLACEMENT_3D('',#22654,#18758,#18759);
#15952=AXIS2_PLACEMENT_3D('',#22657,#18761,#18762);
#15953=AXIS2_PLACEMENT_3D('',#22658,#18763,#18764);
#15954=AXIS2_PLACEMENT_3D('',#22664,#18768,#18769);
#15955=AXIS2_PLACEMENT_3D('',#22666,#18770,#18771);
#15956=AXIS2_PLACEMENT_3D('',#22669,#18773,#18774);
#15957=AXIS2_PLACEMENT_3D('',#22670,#18775,#18776);
#15958=AXIS2_PLACEMENT_3D('',#22676,#18780,#18781);
#15959=AXIS2_PLACEMENT_3D('',#22677,#18782,#18783);
#15960=AXIS2_PLACEMENT_3D('',#22678,#18784,#18785);
#15961=AXIS2_PLACEMENT_3D('',#22679,#18786,#18787);
#15962=AXIS2_PLACEMENT_3D('',#22688,#18792,#18793);
#15963=AXIS2_PLACEMENT_3D('',#22690,#18794,#18795);
#15964=AXIS2_PLACEMENT_3D('',#22693,#18797,#18798);
#15965=AXIS2_PLACEMENT_3D('',#22694,#18799,#18800);
#15966=AXIS2_PLACEMENT_3D('',#22700,#18804,#18805);
#15967=AXIS2_PLACEMENT_3D('',#22702,#18806,#18807);
#15968=AXIS2_PLACEMENT_3D('',#22705,#18809,#18810);
#15969=AXIS2_PLACEMENT_3D('',#22706,#18811,#18812);
#15970=AXIS2_PLACEMENT_3D('',#22712,#18816,#18817);
#15971=AXIS2_PLACEMENT_3D('',#22714,#18818,#18819);
#15972=AXIS2_PLACEMENT_3D('',#22717,#18821,#18822);
#15973=AXIS2_PLACEMENT_3D('',#22718,#18823,#18824);
#15974=AXIS2_PLACEMENT_3D('',#22724,#18828,#18829);
#15975=AXIS2_PLACEMENT_3D('',#22725,#18830,#18831);
#15976=AXIS2_PLACEMENT_3D('',#22726,#18832,#18833);
#15977=AXIS2_PLACEMENT_3D('',#22727,#18834,#18835);
#15978=AXIS2_PLACEMENT_3D('',#22736,#18840,#18841);
#15979=AXIS2_PLACEMENT_3D('',#22738,#18842,#18843);
#15980=AXIS2_PLACEMENT_3D('',#22741,#18845,#18846);
#15981=AXIS2_PLACEMENT_3D('',#22742,#18847,#18848);
#15982=AXIS2_PLACEMENT_3D('',#22748,#18852,#18853);
#15983=AXIS2_PLACEMENT_3D('',#22750,#18854,#18855);
#15984=AXIS2_PLACEMENT_3D('',#22753,#18857,#18858);
#15985=AXIS2_PLACEMENT_3D('',#22754,#18859,#18860);
#15986=AXIS2_PLACEMENT_3D('',#22760,#18864,#18865);
#15987=AXIS2_PLACEMENT_3D('',#22762,#18866,#18867);
#15988=AXIS2_PLACEMENT_3D('',#22765,#18869,#18870);
#15989=AXIS2_PLACEMENT_3D('',#22766,#18871,#18872);
#15990=AXIS2_PLACEMENT_3D('',#22772,#18876,#18877);
#15991=AXIS2_PLACEMENT_3D('',#22773,#18878,#18879);
#15992=AXIS2_PLACEMENT_3D('',#22774,#18880,#18881);
#15993=AXIS2_PLACEMENT_3D('',#22775,#18882,#18883);
#15994=AXIS2_PLACEMENT_3D('',#22784,#18888,#18889);
#15995=AXIS2_PLACEMENT_3D('',#22786,#18890,#18891);
#15996=AXIS2_PLACEMENT_3D('',#22789,#18893,#18894);
#15997=AXIS2_PLACEMENT_3D('',#22790,#18895,#18896);
#15998=AXIS2_PLACEMENT_3D('',#22796,#18900,#18901);
#15999=AXIS2_PLACEMENT_3D('',#22798,#18902,#18903);
#16000=AXIS2_PLACEMENT_3D('',#22801,#18905,#18906);
#16001=AXIS2_PLACEMENT_3D('',#22802,#18907,#18908);
#16002=AXIS2_PLACEMENT_3D('',#22808,#18912,#18913);
#16003=AXIS2_PLACEMENT_3D('',#22810,#18914,#18915);
#16004=AXIS2_PLACEMENT_3D('',#22813,#18917,#18918);
#16005=AXIS2_PLACEMENT_3D('',#22814,#18919,#18920);
#16006=AXIS2_PLACEMENT_3D('',#22820,#18924,#18925);
#16007=AXIS2_PLACEMENT_3D('',#22821,#18926,#18927);
#16008=AXIS2_PLACEMENT_3D('',#22822,#18928,#18929);
#16009=AXIS2_PLACEMENT_3D('',#22823,#18930,#18931);
#16010=AXIS2_PLACEMENT_3D('',#22832,#18936,#18937);
#16011=AXIS2_PLACEMENT_3D('',#22834,#18938,#18939);
#16012=AXIS2_PLACEMENT_3D('',#22837,#18941,#18942);
#16013=AXIS2_PLACEMENT_3D('',#22838,#18943,#18944);
#16014=AXIS2_PLACEMENT_3D('',#22844,#18948,#18949);
#16015=AXIS2_PLACEMENT_3D('',#22846,#18950,#18951);
#16016=AXIS2_PLACEMENT_3D('',#22849,#18953,#18954);
#16017=AXIS2_PLACEMENT_3D('',#22850,#18955,#18956);
#16018=AXIS2_PLACEMENT_3D('',#22856,#18960,#18961);
#16019=AXIS2_PLACEMENT_3D('',#22858,#18962,#18963);
#16020=AXIS2_PLACEMENT_3D('',#22861,#18965,#18966);
#16021=AXIS2_PLACEMENT_3D('',#22862,#18967,#18968);
#16022=AXIS2_PLACEMENT_3D('',#22868,#18972,#18973);
#16023=AXIS2_PLACEMENT_3D('',#22869,#18974,#18975);
#16024=AXIS2_PLACEMENT_3D('',#22870,#18976,#18977);
#16025=AXIS2_PLACEMENT_3D('',#22871,#18978,#18979);
#16026=AXIS2_PLACEMENT_3D('',#22880,#18984,#18985);
#16027=AXIS2_PLACEMENT_3D('',#22882,#18986,#18987);
#16028=AXIS2_PLACEMENT_3D('',#22885,#18989,#18990);
#16029=AXIS2_PLACEMENT_3D('',#22886,#18991,#18992);
#16030=AXIS2_PLACEMENT_3D('',#22892,#18996,#18997);
#16031=AXIS2_PLACEMENT_3D('',#22894,#18998,#18999);
#16032=AXIS2_PLACEMENT_3D('',#22897,#19001,#19002);
#16033=AXIS2_PLACEMENT_3D('',#22898,#19003,#19004);
#16034=AXIS2_PLACEMENT_3D('',#22904,#19008,#19009);
#16035=AXIS2_PLACEMENT_3D('',#22906,#19010,#19011);
#16036=AXIS2_PLACEMENT_3D('',#22909,#19013,#19014);
#16037=AXIS2_PLACEMENT_3D('',#22910,#19015,#19016);
#16038=AXIS2_PLACEMENT_3D('',#22916,#19020,#19021);
#16039=AXIS2_PLACEMENT_3D('',#22917,#19022,#19023);
#16040=AXIS2_PLACEMENT_3D('',#22918,#19024,#19025);
#16041=AXIS2_PLACEMENT_3D('',#22919,#19026,#19027);
#16042=AXIS2_PLACEMENT_3D('',#22928,#19032,#19033);
#16043=AXIS2_PLACEMENT_3D('',#22930,#19034,#19035);
#16044=AXIS2_PLACEMENT_3D('',#22933,#19037,#19038);
#16045=AXIS2_PLACEMENT_3D('',#22934,#19039,#19040);
#16046=AXIS2_PLACEMENT_3D('',#22940,#19044,#19045);
#16047=AXIS2_PLACEMENT_3D('',#22942,#19046,#19047);
#16048=AXIS2_PLACEMENT_3D('',#22945,#19049,#19050);
#16049=AXIS2_PLACEMENT_3D('',#22946,#19051,#19052);
#16050=AXIS2_PLACEMENT_3D('',#22952,#19056,#19057);
#16051=AXIS2_PLACEMENT_3D('',#22954,#19058,#19059);
#16052=AXIS2_PLACEMENT_3D('',#22957,#19061,#19062);
#16053=AXIS2_PLACEMENT_3D('',#22958,#19063,#19064);
#16054=AXIS2_PLACEMENT_3D('',#22964,#19068,#19069);
#16055=AXIS2_PLACEMENT_3D('',#22965,#19070,#19071);
#16056=AXIS2_PLACEMENT_3D('',#22966,#19072,#19073);
#16057=AXIS2_PLACEMENT_3D('',#22967,#19074,#19075);
#16058=AXIS2_PLACEMENT_3D('',#22976,#19080,#19081);
#16059=AXIS2_PLACEMENT_3D('',#22978,#19082,#19083);
#16060=AXIS2_PLACEMENT_3D('',#22980,#19084,#19085);
#16061=AXIS2_PLACEMENT_3D('',#22982,#19087,#19088);
#16062=AXIS2_PLACEMENT_3D('',#22988,#19092,#19093);
#16063=AXIS2_PLACEMENT_3D('',#22990,#19094,#19095);
#16064=AXIS2_PLACEMENT_3D('',#22992,#19096,#19097);
#16065=AXIS2_PLACEMENT_3D('',#22994,#19099,#19100);
#16066=AXIS2_PLACEMENT_3D('',#23000,#19104,#19105);
#16067=AXIS2_PLACEMENT_3D('',#23002,#19106,#19107);
#16068=AXIS2_PLACEMENT_3D('',#23004,#19108,#19109);
#16069=AXIS2_PLACEMENT_3D('',#23006,#19111,#19112);
#16070=AXIS2_PLACEMENT_3D('',#23012,#19116,#19117);
#16071=AXIS2_PLACEMENT_3D('',#23013,#19118,#19119);
#16072=AXIS2_PLACEMENT_3D('',#23014,#19120,#19121);
#16073=AXIS2_PLACEMENT_3D('',#23015,#19122,#19123);
#16074=AXIS2_PLACEMENT_3D('',#23016,#19124,#19125);
#16075=AXIS2_PLACEMENT_3D('',#23017,#19126,#19127);
#16076=AXIS2_PLACEMENT_3D('',#23018,#19128,#19129);
#16077=AXIS2_PLACEMENT_3D('',#23020,#19130,#19131);
#16078=AXIS2_PLACEMENT_3D('',#23021,#19132,#19133);
#16079=AXIS2_PLACEMENT_3D('',#23023,#19134,#19135);
#16080=AXIS2_PLACEMENT_3D('',#23025,#19137,#19138);
#16081=AXIS2_PLACEMENT_3D('',#23027,#19139,#19140);
#16082=AXIS2_PLACEMENT_3D('',#23029,#19142,#19143);
#16083=AXIS2_PLACEMENT_3D('',#23032,#19145,#19146);
#16084=AXIS2_PLACEMENT_3D('',#23033,#19147,#19148);
#16085=AXIS2_PLACEMENT_3D('',#23034,#19149,#19150);
#16086=AXIS2_PLACEMENT_3D('',#23035,#19151,#19152);
#16087=AXIS2_PLACEMENT_3D('',#23199,#19154,#19155);
#16088=AXIS2_PLACEMENT_3D('',#23276,#19156,#19157);
#16089=AXIS2_PLACEMENT_3D('',#23715,#19159,#19160);
#16090=AXIS2_PLACEMENT_3D('',#24152,#19162,#19163);
#16091=AXIS2_PLACEMENT_3D('',#24593,#19165,#19166);
#16092=AXIS2_PLACEMENT_3D('',#25076,#19168,#19169);
#16093=AXIS2_PLACEMENT_3D('',#25507,#19171,#19172);
#16094=AXIS2_PLACEMENT_3D('',#25795,#19174,#19175);
#16095=AXIS2_PLACEMENT_3D('',#26263,#19177,#19178);
#16096=AXIS2_PLACEMENT_3D('',#26697,#19180,#19181);
#16097=AXIS2_PLACEMENT_3D('',#26869,#19183,#19184);
#16098=AXIS2_PLACEMENT_3D('',#27191,#19186,#19187);
#16099=AXIS2_PLACEMENT_3D('',#27644,#19189,#19190);
#16100=AXIS2_PLACEMENT_3D('',#28093,#19192,#19193);
#16101=AXIS2_PLACEMENT_3D('',#28528,#19195,#19196);
#16102=AXIS2_PLACEMENT_3D('',#28987,#19198,#19199);
#16103=AXIS2_PLACEMENT_3D('',#29432,#19201,#19202);
#16104=AXIS2_PLACEMENT_3D('',#29911,#19204,#19205);
#16105=AXIS2_PLACEMENT_3D('',#30396,#19207,#19208);
#16106=AXIS2_PLACEMENT_3D('',#30843,#19210,#19211);
#16107=AXIS2_PLACEMENT_3D('',#31290,#19213,#19214);
#16108=AXIS2_PLACEMENT_3D('',#31723,#19216,#19217);
#16109=AXIS2_PLACEMENT_3D('',#32240,#19219,#19220);
#16110=AXIS2_PLACEMENT_3D('',#32691,#19222,#19223);
#16111=AXIS2_PLACEMENT_3D('',#32975,#19225,#19226);
#16112=AXIS2_PLACEMENT_3D('',#32985,#19227,#19228);
#16113=AXIS2_PLACEMENT_3D('',#36520,#19229,#19230);
#16114=AXIS2_PLACEMENT_3D('',#40407,#19231,#19232);
#16115=AXIS2_PLACEMENT_3D('',#40507,#19233,#19234);
#16116=AXIS2_PLACEMENT_3D('',#40613,#19235,#19236);
#16117=AXIS2_PLACEMENT_3D('',#40616,#19237,#19238);
#16118=AXIS2_PLACEMENT_3D('',#40790,#19239,#19240);
#16119=AXIS2_PLACEMENT_3D('',#41513,#19241,#19242);
#16120=AXIS2_PLACEMENT_3D('',#41516,#19243,#19244);
#16121=AXIS2_PLACEMENT_3D('',#41605,#19245,#19246);
#16122=AXIS2_PLACEMENT_3D('',#42238,#19247,#19248);
#16123=AXIS2_PLACEMENT_3D('',#42240,#19249,#19250);
#16124=AXIS2_PLACEMENT_3D('',#42241,#19251,#19252);
#16125=AXIS2_PLACEMENT_3D('',#42242,#19253,#19254);
#16126=AXIS2_PLACEMENT_3D('',#42244,#19255,#19256);
#16127=AXIS2_PLACEMENT_3D('',#42245,#19257,#19258);
#16128=AXIS2_PLACEMENT_3D('',#42248,#19260,#19261);
#16129=AXIS2_PLACEMENT_3D('',#42249,#19262,#19263);
#16130=AXIS2_PLACEMENT_3D('',#42250,#19264,#19265);
#16131=AXIS2_PLACEMENT_3D('',#42253,#19266,#19267);
#16132=AXIS2_PLACEMENT_3D('',#42257,#19270,#19271);
#16133=AXIS2_PLACEMENT_3D('',#42265,#19274,#19275);
#16134=AXIS2_PLACEMENT_3D('',#42271,#19277,#19278);
#16135=AXIS2_PLACEMENT_3D('',#42274,#19279,#19280);
#16136=AXIS2_PLACEMENT_3D('',#42277,#19282,#19283);
#16137=AXIS2_PLACEMENT_3D('',#42279,#19284,#19285);
#16138=AXIS2_PLACEMENT_3D('',#42283,#19287,#19288);
#16139=AXIS2_PLACEMENT_3D('',#42287,#19290,#19291);
#16140=AXIS2_PLACEMENT_3D('',#42291,#19293,#19294);
#16141=AXIS2_PLACEMENT_3D('',#42295,#19296,#19297);
#16142=AXIS2_PLACEMENT_3D('',#42299,#19299,#19300);
#16143=AXIS2_PLACEMENT_3D('',#42303,#19302,#19303);
#16144=AXIS2_PLACEMENT_3D('',#42307,#19305,#19306);
#16145=AXIS2_PLACEMENT_3D('',#42311,#19308,#19309);
#16146=AXIS2_PLACEMENT_3D('',#42315,#19311,#19312);
#16147=AXIS2_PLACEMENT_3D('',#42319,#19314,#19315);
#16148=AXIS2_PLACEMENT_3D('',#42323,#19317,#19318);
#16149=AXIS2_PLACEMENT_3D('',#42327,#19320,#19321);
#16150=AXIS2_PLACEMENT_3D('',#42331,#19323,#19324);
#16151=AXIS2_PLACEMENT_3D('',#42335,#19326,#19327);
#16152=AXIS2_PLACEMENT_3D('',#42339,#19329,#19330);
#16153=AXIS2_PLACEMENT_3D('',#42343,#19332,#19333);
#16154=AXIS2_PLACEMENT_3D('',#42347,#19335,#19336);
#16155=AXIS2_PLACEMENT_3D('',#42351,#19338,#19339);
#16156=AXIS2_PLACEMENT_3D('',#42355,#19341,#19342);
#16157=AXIS2_PLACEMENT_3D('',#42359,#19344,#19345);
#16158=AXIS2_PLACEMENT_3D('',#42363,#19347,#19348);
#16159=AXIS2_PLACEMENT_3D('',#42367,#19350,#19351);
#16160=AXIS2_PLACEMENT_3D('',#42371,#19353,#19354);
#16161=AXIS2_PLACEMENT_3D('',#42375,#19356,#19357);
#16162=AXIS2_PLACEMENT_3D('',#42379,#19359,#19360);
#16163=AXIS2_PLACEMENT_3D('',#42383,#19362,#19363);
#16164=AXIS2_PLACEMENT_3D('',#42387,#19365,#19366);
#16165=AXIS2_PLACEMENT_3D('',#42391,#19368,#19369);
#16166=AXIS2_PLACEMENT_3D('',#42395,#19371,#19372);
#16167=AXIS2_PLACEMENT_3D('',#42399,#19374,#19375);
#16168=AXIS2_PLACEMENT_3D('',#42403,#19377,#19378);
#16169=AXIS2_PLACEMENT_3D('',#42407,#19380,#19381);
#16170=AXIS2_PLACEMENT_3D('',#42410,#19383,#19384);
#16171=AXIS2_PLACEMENT_3D('',#42412,#19385,#19386);
#16172=AXIS2_PLACEMENT_3D('',#42416,#19388,#19389);
#16173=AXIS2_PLACEMENT_3D('',#42420,#19391,#19392);
#16174=AXIS2_PLACEMENT_3D('',#42424,#19394,#19395);
#16175=AXIS2_PLACEMENT_3D('',#42428,#19397,#19398);
#16176=AXIS2_PLACEMENT_3D('',#42432,#19400,#19401);
#16177=AXIS2_PLACEMENT_3D('',#42436,#19403,#19404);
#16178=AXIS2_PLACEMENT_3D('',#42440,#19406,#19407);
#16179=AXIS2_PLACEMENT_3D('',#42444,#19409,#19410);
#16180=AXIS2_PLACEMENT_3D('',#42448,#19412,#19413);
#16181=AXIS2_PLACEMENT_3D('',#42452,#19415,#19416);
#16182=AXIS2_PLACEMENT_3D('',#42456,#19418,#19419);
#16183=AXIS2_PLACEMENT_3D('',#42460,#19421,#19422);
#16184=AXIS2_PLACEMENT_3D('',#42464,#19424,#19425);
#16185=AXIS2_PLACEMENT_3D('',#42468,#19427,#19428);
#16186=AXIS2_PLACEMENT_3D('',#42472,#19430,#19431);
#16187=AXIS2_PLACEMENT_3D('',#42476,#19433,#19434);
#16188=AXIS2_PLACEMENT_3D('',#42480,#19436,#19437);
#16189=AXIS2_PLACEMENT_3D('',#42484,#19439,#19440);
#16190=AXIS2_PLACEMENT_3D('',#42488,#19442,#19443);
#16191=AXIS2_PLACEMENT_3D('',#42492,#19445,#19446);
#16192=AXIS2_PLACEMENT_3D('',#42496,#19448,#19449);
#16193=AXIS2_PLACEMENT_3D('',#42500,#19451,#19452);
#16194=AXIS2_PLACEMENT_3D('',#42504,#19454,#19455);
#16195=AXIS2_PLACEMENT_3D('',#42508,#19457,#19458);
#16196=AXIS2_PLACEMENT_3D('',#42512,#19460,#19461);
#16197=AXIS2_PLACEMENT_3D('',#42516,#19463,#19464);
#16198=AXIS2_PLACEMENT_3D('',#42520,#19466,#19467);
#16199=AXIS2_PLACEMENT_3D('',#42524,#19469,#19470);
#16200=AXIS2_PLACEMENT_3D('',#42528,#19472,#19473);
#16201=AXIS2_PLACEMENT_3D('',#42532,#19475,#19476);
#16202=AXIS2_PLACEMENT_3D('',#42536,#19478,#19479);
#16203=AXIS2_PLACEMENT_3D('',#42540,#19481,#19482);
#16204=AXIS2_PLACEMENT_3D('',#42544,#19484,#19485);
#16205=AXIS2_PLACEMENT_3D('',#42548,#19487,#19488);
#16206=AXIS2_PLACEMENT_3D('',#42552,#19490,#19491);
#16207=AXIS2_PLACEMENT_3D('',#42556,#19493,#19494);
#16208=AXIS2_PLACEMENT_3D('',#42558,#19496,#19497);
#16209=AXIS2_PLACEMENT_3D('',#42566,#19500,#19501);
#16210=AXIS2_PLACEMENT_3D('',#42571,#19503,#19504);
#16211=AXIS2_PLACEMENT_3D('',#42572,#19505,#19506);
#16212=AXIS2_PLACEMENT_3D('',#42813,#19508,#19509);
#16213=AXIS2_PLACEMENT_3D('',#42814,#19510,#19511);
#16214=AXIS2_PLACEMENT_3D('',#42818,#19514,#19515);
#16215=AXIS2_PLACEMENT_3D('',#42820,#19517,#19518);
#16216=AXIS2_PLACEMENT_3D('',#42821,#19519,#19520);
#16217=AXIS2_PLACEMENT_3D('',#42825,#19523,#19524);
#16218=AXIS2_PLACEMENT_3D('',#42827,#19526,#19527);
#16219=AXIS2_PLACEMENT_3D('',#42828,#19528,#19529);
#16220=AXIS2_PLACEMENT_3D('',#42832,#19532,#19533);
#16221=AXIS2_PLACEMENT_3D('',#42834,#19535,#19536);
#16222=AXIS2_PLACEMENT_3D('',#42835,#19537,#19538);
#16223=AXIS2_PLACEMENT_3D('',#42839,#19541,#19542);
#16224=AXIS2_PLACEMENT_3D('',#42841,#19544,#19545);
#16225=AXIS2_PLACEMENT_3D('',#42842,#19546,#19547);
#16226=AXIS2_PLACEMENT_3D('',#42846,#19550,#19551);
#16227=AXIS2_PLACEMENT_3D('',#42848,#19553,#19554);
#16228=AXIS2_PLACEMENT_3D('',#42849,#19555,#19556);
#16229=AXIS2_PLACEMENT_3D('',#42853,#19559,#19560);
#16230=AXIS2_PLACEMENT_3D('',#42855,#19562,#19563);
#16231=AXIS2_PLACEMENT_3D('',#42856,#19564,#19565);
#16232=AXIS2_PLACEMENT_3D('',#42860,#19568,#19569);
#16233=AXIS2_PLACEMENT_3D('',#42862,#19571,#19572);
#16234=AXIS2_PLACEMENT_3D('',#42863,#19573,#19574);
#16235=AXIS2_PLACEMENT_3D('',#42867,#19577,#19578);
#16236=AXIS2_PLACEMENT_3D('',#42869,#19580,#19581);
#16237=AXIS2_PLACEMENT_3D('',#42870,#19582,#19583);
#16238=AXIS2_PLACEMENT_3D('',#42874,#19586,#19587);
#16239=AXIS2_PLACEMENT_3D('',#42876,#19589,#19590);
#16240=AXIS2_PLACEMENT_3D('',#42877,#19591,#19592);
#16241=AXIS2_PLACEMENT_3D('',#42881,#19595,#19596);
#16242=AXIS2_PLACEMENT_3D('',#42883,#19598,#19599);
#16243=AXIS2_PLACEMENT_3D('',#42884,#19600,#19601);
#16244=AXIS2_PLACEMENT_3D('',#42888,#19604,#19605);
#16245=AXIS2_PLACEMENT_3D('',#42890,#19607,#19608);
#16246=AXIS2_PLACEMENT_3D('',#42891,#19609,#19610);
#16247=AXIS2_PLACEMENT_3D('',#42895,#19613,#19614);
#16248=AXIS2_PLACEMENT_3D('',#42897,#19616,#19617);
#16249=AXIS2_PLACEMENT_3D('',#42898,#19618,#19619);
#16250=AXIS2_PLACEMENT_3D('',#42902,#19622,#19623);
#16251=AXIS2_PLACEMENT_3D('',#42904,#19625,#19626);
#16252=AXIS2_PLACEMENT_3D('',#42905,#19627,#19628);
#16253=AXIS2_PLACEMENT_3D('',#42909,#19631,#19632);
#16254=AXIS2_PLACEMENT_3D('',#42911,#19634,#19635);
#16255=AXIS2_PLACEMENT_3D('',#42912,#19636,#19637);
#16256=AXIS2_PLACEMENT_3D('',#42916,#19640,#19641);
#16257=AXIS2_PLACEMENT_3D('',#42918,#19643,#19644);
#16258=AXIS2_PLACEMENT_3D('',#42919,#19645,#19646);
#16259=AXIS2_PLACEMENT_3D('',#42923,#19649,#19650);
#16260=AXIS2_PLACEMENT_3D('',#42925,#19652,#19653);
#16261=AXIS2_PLACEMENT_3D('',#42926,#19654,#19655);
#16262=AXIS2_PLACEMENT_3D('',#42930,#19658,#19659);
#16263=AXIS2_PLACEMENT_3D('',#42932,#19661,#19662);
#16264=AXIS2_PLACEMENT_3D('',#42933,#19663,#19664);
#16265=AXIS2_PLACEMENT_3D('',#42937,#19667,#19668);
#16266=AXIS2_PLACEMENT_3D('',#42939,#19670,#19671);
#16267=AXIS2_PLACEMENT_3D('',#42940,#19672,#19673);
#16268=AXIS2_PLACEMENT_3D('',#42944,#19676,#19677);
#16269=AXIS2_PLACEMENT_3D('',#42946,#19679,#19680);
#16270=AXIS2_PLACEMENT_3D('',#42947,#19681,#19682);
#16271=AXIS2_PLACEMENT_3D('',#42951,#19685,#19686);
#16272=AXIS2_PLACEMENT_3D('',#42953,#19688,#19689);
#16273=AXIS2_PLACEMENT_3D('',#42954,#19690,#19691);
#16274=AXIS2_PLACEMENT_3D('',#42958,#19694,#19695);
#16275=AXIS2_PLACEMENT_3D('',#42960,#19697,#19698);
#16276=AXIS2_PLACEMENT_3D('',#42961,#19699,#19700);
#16277=AXIS2_PLACEMENT_3D('',#42965,#19703,#19704);
#16278=AXIS2_PLACEMENT_3D('',#42967,#19706,#19707);
#16279=AXIS2_PLACEMENT_3D('',#42968,#19708,#19709);
#16280=AXIS2_PLACEMENT_3D('',#42972,#19712,#19713);
#16281=AXIS2_PLACEMENT_3D('',#42974,#19715,#19716);
#16282=AXIS2_PLACEMENT_3D('',#42975,#19717,#19718);
#16283=AXIS2_PLACEMENT_3D('',#42979,#19721,#19722);
#16284=AXIS2_PLACEMENT_3D('',#42981,#19724,#19725);
#16285=AXIS2_PLACEMENT_3D('',#42982,#19726,#19727);
#16286=AXIS2_PLACEMENT_3D('',#42986,#19730,#19731);
#16287=AXIS2_PLACEMENT_3D('',#42988,#19733,#19734);
#16288=AXIS2_PLACEMENT_3D('',#42989,#19735,#19736);
#16289=AXIS2_PLACEMENT_3D('',#42993,#19739,#19740);
#16290=AXIS2_PLACEMENT_3D('',#42995,#19742,#19743);
#16291=AXIS2_PLACEMENT_3D('',#42996,#19744,#19745);
#16292=AXIS2_PLACEMENT_3D('',#43000,#19748,#19749);
#16293=AXIS2_PLACEMENT_3D('',#43002,#19751,#19752);
#16294=AXIS2_PLACEMENT_3D('',#43003,#19753,#19754);
#16295=AXIS2_PLACEMENT_3D('',#43007,#19757,#19758);
#16296=AXIS2_PLACEMENT_3D('',#43009,#19760,#19761);
#16297=AXIS2_PLACEMENT_3D('',#43010,#19762,#19763);
#16298=AXIS2_PLACEMENT_3D('',#43014,#19766,#19767);
#16299=AXIS2_PLACEMENT_3D('',#43016,#19769,#19770);
#16300=AXIS2_PLACEMENT_3D('',#43017,#19771,#19772);
#16301=AXIS2_PLACEMENT_3D('',#43021,#19775,#19776);
#16302=AXIS2_PLACEMENT_3D('',#43023,#19778,#19779);
#16303=AXIS2_PLACEMENT_3D('',#43024,#19780,#19781);
#16304=AXIS2_PLACEMENT_3D('',#43028,#19784,#19785);
#16305=AXIS2_PLACEMENT_3D('',#43030,#19787,#19788);
#16306=AXIS2_PLACEMENT_3D('',#43031,#19789,#19790);
#16307=AXIS2_PLACEMENT_3D('',#43035,#19793,#19794);
#16308=AXIS2_PLACEMENT_3D('',#43037,#19796,#19797);
#16309=AXIS2_PLACEMENT_3D('',#43038,#19798,#19799);
#16310=AXIS2_PLACEMENT_3D('',#43042,#19802,#19803);
#16311=AXIS2_PLACEMENT_3D('',#43044,#19805,#19806);
#16312=AXIS2_PLACEMENT_3D('',#43045,#19807,#19808);
#16313=AXIS2_PLACEMENT_3D('',#43049,#19811,#19812);
#16314=AXIS2_PLACEMENT_3D('',#43051,#19814,#19815);
#16315=AXIS2_PLACEMENT_3D('',#43052,#19816,#19817);
#16316=AXIS2_PLACEMENT_3D('',#43053,#19818,#19819);
#16317=AXIS2_PLACEMENT_3D('',#43054,#19820,#19821);
#16318=AXIS2_PLACEMENT_3D('',#43056,#19822,#19823);
#16319=AXIS2_PLACEMENT_3D('',#43057,#19824,#19825);
#16320=AXIS2_PLACEMENT_3D('',#43064,#19826,#19827);
#16321=AXIS2_PLACEMENT_3D('',#43074,#19828,#19829);
#16322=AXIS2_PLACEMENT_3D('',#43084,#19830,#19831);
#16323=AXIS2_PLACEMENT_3D('',#43094,#19832,#19833);
#16324=AXIS2_PLACEMENT_3D('',#43104,#19834,#19835);
#16325=AXIS2_PLACEMENT_3D('',#43114,#19836,#19837);
#16326=AXIS2_PLACEMENT_3D('',#43119,#19839,#19840);
#16327=AXIS2_PLACEMENT_3D('',#43124,#19843,#19844);
#16328=AXIS2_PLACEMENT_3D('',#43125,#19845,#19846);
#16329=AXIS2_PLACEMENT_3D('',#43130,#19849,#19850);
#16330=AXIS2_PLACEMENT_3D('',#43131,#19851,#19852);
#16331=AXIS2_PLACEMENT_3D('',#43135,#19854,#19855);
#16332=AXIS2_PLACEMENT_3D('',#43137,#19857,#19858);
#16333=AXIS2_PLACEMENT_3D('',#43142,#19861,#19862);
#16334=AXIS2_PLACEMENT_3D('',#43143,#19863,#19864);
#16335=AXIS2_PLACEMENT_3D('',#43147,#19866,#19867);
#16336=AXIS2_PLACEMENT_3D('',#43149,#19869,#19870);
#16337=AXIS2_PLACEMENT_3D('',#43153,#19872,#19873);
#16338=AXIS2_PLACEMENT_3D('',#43155,#19875,#19876);
#16339=AXIS2_PLACEMENT_3D('',#43162,#19881,#19882);
#16340=AXIS2_PLACEMENT_3D('',#43167,#19886,#19887);
#16341=AXIS2_PLACEMENT_3D('',#43172,#19891,#19892);
#16342=AXIS2_PLACEMENT_3D('',#43173,#19893,#19894);
#16343=AXIS2_PLACEMENT_3D('',#43174,#19895,#19896);
#16344=AXIS2_PLACEMENT_3D('',#43176,#19898,#19899);
#16345=AXIS2_PLACEMENT_3D('',#43177,#19900,#19901);
#16346=AXIS2_PLACEMENT_3D('',#43179,#19903,#19904);
#16347=AXIS2_PLACEMENT_3D('',#43181,#19906,#19907);
#16348=AXIS2_PLACEMENT_3D('',#43184,#19909,#19910);
#16349=AXIS2_PLACEMENT_3D('',#43185,#19911,#19912);
#16350=AXIS2_PLACEMENT_3D('',#43186,#19913,#19914);
#16351=AXIS2_PLACEMENT_3D('',#43187,#19915,#19916);
#16352=AXIS2_PLACEMENT_3D('',#43188,#19917,#19918);
#16353=AXIS2_PLACEMENT_3D('',#43189,#19919,#19920);
#16354=AXIS2_PLACEMENT_3D('',#43190,#19921,#19922);
#16355=AXIS2_PLACEMENT_3D('',#43191,#19923,#19924);
#16356=AXIS2_PLACEMENT_3D('',#43194,#19926,#19927);
#16357=AXIS2_PLACEMENT_3D('',#43195,#19928,#19929);
#16358=AXIS2_PLACEMENT_3D('',#43197,#19931,#19932);
#16359=AXIS2_PLACEMENT_3D('',#43198,#19933,#19934);
#16360=AXIS2_PLACEMENT_3D('',#43201,#19936,#19937);
#16361=AXIS2_PLACEMENT_3D('',#43203,#19939,#19940);
#16362=AXIS2_PLACEMENT_3D('',#43205,#19942,#19943);
#16363=AXIS2_PLACEMENT_3D('',#43206,#19944,#19945);
#16364=AXIS2_PLACEMENT_3D('',#43207,#19946,#19947);
#16365=AXIS2_PLACEMENT_3D('',#43387,#19949,#19950);
#16366=AXIS2_PLACEMENT_3D('',#43506,#19951,#19952);
#16367=AXIS2_PLACEMENT_3D('',#43950,#19954,#19955);
#16368=AXIS2_PLACEMENT_3D('',#44382,#19957,#19958);
#16369=AXIS2_PLACEMENT_3D('',#44802,#19960,#19961);
#16370=AXIS2_PLACEMENT_3D('',#45304,#19963,#19964);
#16371=AXIS2_PLACEMENT_3D('',#45734,#19966,#19967);
#16372=AXIS2_PLACEMENT_3D('',#46188,#19969,#19970);
#16373=AXIS2_PLACEMENT_3D('',#46632,#19972,#19973);
#16374=AXIS2_PLACEMENT_3D('',#47114,#19975,#19976);
#16375=AXIS2_PLACEMENT_3D('',#47580,#19978,#19979);
#16376=AXIS2_PLACEMENT_3D('',#48004,#19981,#19982);
#16377=AXIS2_PLACEMENT_3D('',#48468,#19984,#19985);
#16378=AXIS2_PLACEMENT_3D('',#48907,#19987,#19988);
#16379=AXIS2_PLACEMENT_3D('',#49346,#19990,#19991);
#16380=AXIS2_PLACEMENT_3D('',#49795,#19993,#19994);
#16381=AXIS2_PLACEMENT_3D('',#50298,#19996,#19997);
#16382=AXIS2_PLACEMENT_3D('',#50801,#19999,#20000);
#16383=AXIS2_PLACEMENT_3D('',#51280,#20002,#20003);
#16384=AXIS2_PLACEMENT_3D('',#51713,#20005,#20006);
#16385=AXIS2_PLACEMENT_3D('',#52158,#20008,#20009);
#16386=AXIS2_PLACEMENT_3D('',#52607,#20011,#20012);
#16387=AXIS2_PLACEMENT_3D('',#53050,#20014,#20015);
#16388=AXIS2_PLACEMENT_3D('',#53516,#20017,#20018);
#16389=AXIS2_PLACEMENT_3D('',#53526,#20019,#20020);
#16390=AXIS2_PLACEMENT_3D('',#57867,#20021,#20022);
#16391=AXIS2_PLACEMENT_3D('',#61218,#20023,#20024);
#16392=AXIS2_PLACEMENT_3D('',#61429,#20025,#20026);
#16393=AXIS2_PLACEMENT_3D('',#61577,#20027,#20028);
#16394=AXIS2_PLACEMENT_3D('',#61580,#20029,#20030);
#16395=AXIS2_PLACEMENT_3D('',#61759,#20031,#20032);
#16396=AXIS2_PLACEMENT_3D('',#62470,#20033,#20034);
#16397=AXIS2_PLACEMENT_3D('',#62472,#20035,#20036);
#16398=AXIS2_PLACEMENT_3D('',#62474,#20037,#20038);
#16399=AXIS2_PLACEMENT_3D('',#63183,#20039,#20040);
#16400=AXIS2_PLACEMENT_3D('',#63190,#20041,#20042);
#16401=AXIS2_PLACEMENT_3D('',#63200,#20043,#20044);
#16402=AXIS2_PLACEMENT_3D('',#63210,#20045,#20046);
#16403=AXIS2_PLACEMENT_3D('',#63220,#20047,#20048);
#16404=AXIS2_PLACEMENT_3D('',#63230,#20049,#20050);
#16405=AXIS2_PLACEMENT_3D('',#63240,#20051,#20052);
#16406=AXIS2_PLACEMENT_3D('',#63246,#20054,#20055);
#16407=AXIS2_PLACEMENT_3D('',#63247,#20056,#20057);
#16408=AXIS2_PLACEMENT_3D('',#63252,#20060,#20061);
#16409=AXIS2_PLACEMENT_3D('',#63253,#20062,#20063);
#16410=AXIS2_PLACEMENT_3D('',#63258,#20066,#20067);
#16411=AXIS2_PLACEMENT_3D('',#63259,#20068,#20069);
#16412=AXIS2_PLACEMENT_3D('',#63263,#20071,#20072);
#16413=AXIS2_PLACEMENT_3D('',#63265,#20074,#20075);
#16414=AXIS2_PLACEMENT_3D('',#63270,#20078,#20079);
#16415=AXIS2_PLACEMENT_3D('',#63271,#20080,#20081);
#16416=AXIS2_PLACEMENT_3D('',#63275,#20083,#20084);
#16417=AXIS2_PLACEMENT_3D('',#63277,#20086,#20087);
#16418=AXIS2_PLACEMENT_3D('',#63281,#20089,#20090);
#16419=AXIS2_PLACEMENT_3D('',#63283,#20092,#20093);
#16420=AXIS2_PLACEMENT_3D('',#63290,#20098,#20099);
#16421=AXIS2_PLACEMENT_3D('',#63295,#20103,#20104);
#16422=AXIS2_PLACEMENT_3D('',#63300,#20108,#20109);
#16423=AXIS2_PLACEMENT_3D('',#63301,#20110,#20111);
#16424=AXIS2_PLACEMENT_3D('',#63302,#20112,#20113);
#16425=AXIS2_PLACEMENT_3D('',#63304,#20115,#20116);
#16426=AXIS2_PLACEMENT_3D('',#63305,#20117,#20118);
#16427=AXIS2_PLACEMENT_3D('',#63307,#20120,#20121);
#16428=AXIS2_PLACEMENT_3D('',#63309,#20123,#20124);
#16429=AXIS2_PLACEMENT_3D('',#63312,#20126,#20127);
#16430=AXIS2_PLACEMENT_3D('',#63313,#20128,#20129);
#16431=AXIS2_PLACEMENT_3D('',#63314,#20130,#20131);
#16432=AXIS2_PLACEMENT_3D('',#63315,#20132,#20133);
#16433=AXIS2_PLACEMENT_3D('',#63316,#20134,#20135);
#16434=AXIS2_PLACEMENT_3D('',#63317,#20136,#20137);
#16435=AXIS2_PLACEMENT_3D('',#63318,#20138,#20139);
#16436=AXIS2_PLACEMENT_3D('',#63319,#20140,#20141);
#16437=AXIS2_PLACEMENT_3D('',#63322,#20143,#20144);
#16438=AXIS2_PLACEMENT_3D('',#63323,#20145,#20146);
#16439=AXIS2_PLACEMENT_3D('',#63325,#20148,#20149);
#16440=AXIS2_PLACEMENT_3D('',#63326,#20150,#20151);
#16441=AXIS2_PLACEMENT_3D('',#63329,#20153,#20154);
#16442=AXIS2_PLACEMENT_3D('',#63331,#20156,#20157);
#16443=AXIS2_PLACEMENT_3D('',#63333,#20159,#20160);
#16444=AXIS2_PLACEMENT_3D('',#63334,#20161,#20162);
#16445=AXIS2_PLACEMENT_3D('',#63336,#20163,#20164);
#16446=AXIS2_PLACEMENT_3D('',#63337,#20165,#20166);
#16447=AXIS2_PLACEMENT_3D('',#63339,#20168,#20169);
#16448=AXIS2_PLACEMENT_3D('',#63342,#20171,#20172);
#16449=AXIS2_PLACEMENT_3D('',#63343,#20173,#20174);
#16450=AXIS2_PLACEMENT_3D('',#63344,#20175,#20176);
#16451=AXIS2_PLACEMENT_3D('',#63345,#20177,#20178);
#16452=AXIS2_PLACEMENT_3D('',#63375,#20180,#20181);
#16453=AXIS2_PLACEMENT_3D('',#63376,#20182,#20183);
#16454=AXIS2_PLACEMENT_3D('',#63570,#20185,#20186);
#16455=AXIS2_PLACEMENT_3D('',#63751,#20187,#20188);
#16456=AXIS2_PLACEMENT_3D('',#64123,#20190,#20191);
#16457=AXIS2_PLACEMENT_3D('',#64507,#20193,#20194);
#16458=AXIS2_PLACEMENT_3D('',#64890,#20196,#20197);
#16459=AXIS2_PLACEMENT_3D('',#65267,#20199,#20200);
#16460=AXIS2_PLACEMENT_3D('',#65646,#20202,#20203);
#16461=AXIS2_PLACEMENT_3D('',#65874,#20205,#20206);
#16462=AXIS2_PLACEMENT_3D('',#66226,#20208,#20209);
#16463=AXIS2_PLACEMENT_3D('',#66608,#20211,#20212);
#16464=AXIS2_PLACEMENT_3D('',#66613,#20214,#20215);
#16465=AXIS2_PLACEMENT_3D('',#66642,#20216,#20217);
#16466=AXIS2_PLACEMENT_3D('',#66655,#20218,#20219);
#16467=AXIS2_PLACEMENT_3D('',#66671,#20220,#20221);
#16468=AXIS2_PLACEMENT_3D('',#66672,#20222,#20223);
#16469=AXIS2_PLACEMENT_3D('',#68635,#20224,#20225);
#16470=AXIS2_PLACEMENT_3D('',#68637,#20226,#20227);
#16471=AXIS2_PLACEMENT_3D('',#70382,#20228,#20229);
#16472=AXIS2_PLACEMENT_3D('',#70544,#20230,#20231);
#16473=AXIS2_PLACEMENT_3D('',#71016,#20232,#20233);
#16474=AXIS2_PLACEMENT_3D('',#71017,#20234,#20235);
#16475=AXIS2_PLACEMENT_3D('',#71019,#20236,#20237);
#16476=AXIS2_PLACEMENT_3D('',#71388,#20238,#20239);
#16477=AXIS2_PLACEMENT_3D('',#71393,#20240,#20241);
#16478=AXIS2_PLACEMENT_3D('',#71394,#20242,#20243);
#16479=AXIS2_PLACEMENT_3D('',#71396,#20244,#20245);
#16480=AXIS2_PLACEMENT_3D('',#71397,#20246,#20247);
#16481=AXIS2_PLACEMENT_3D('',#71398,#20248,#20249);
#16482=AXIS2_PLACEMENT_3D('',#71400,#20250,#20251);
#16483=AXIS2_PLACEMENT_3D('',#71401,#20252,#20253);
#16484=AXIS2_PLACEMENT_3D('',#71405,#20255,#20256);
#16485=AXIS2_PLACEMENT_3D('',#71406,#20257,#20258);
#16486=AXIS2_PLACEMENT_3D('',#71409,#20260,#20261);
#16487=AXIS2_PLACEMENT_3D('',#71410,#20262,#20263);
#16488=AXIS2_PLACEMENT_3D('',#71413,#20265,#20266);
#16489=AXIS2_PLACEMENT_3D('',#71414,#20267,#20268);
#16490=AXIS2_PLACEMENT_3D('',#71417,#20270,#20271);
#16491=AXIS2_PLACEMENT_3D('',#71418,#20272,#20273);
#16492=AXIS2_PLACEMENT_3D('',#71421,#20275,#20276);
#16493=AXIS2_PLACEMENT_3D('',#71422,#20277,#20278);
#16494=AXIS2_PLACEMENT_3D('',#71424,#20280,#20281);
#16495=AXIS2_PLACEMENT_3D('',#71425,#20282,#20283);
#16496=AXIS2_PLACEMENT_3D('',#71428,#20285,#20286);
#16497=AXIS2_PLACEMENT_3D('',#71431,#20287,#20288);
#16498=AXIS2_PLACEMENT_3D('',#71434,#20291,#20292);
#16499=AXIS2_PLACEMENT_3D('',#71436,#20293,#20294);
#16500=AXIS2_PLACEMENT_3D('',#71438,#20296,#20297);
#16501=AXIS2_PLACEMENT_3D('',#71440,#20298,#20299);
#16502=AXIS2_PLACEMENT_3D('',#71442,#20301,#20302);
#16503=AXIS2_PLACEMENT_3D('',#71444,#20303,#20304);
#16504=AXIS2_PLACEMENT_3D('',#71446,#20306,#20307);
#16505=AXIS2_PLACEMENT_3D('',#71448,#20308,#20309);
#16506=AXIS2_PLACEMENT_3D('',#71450,#20311,#20312);
#16507=AXIS2_PLACEMENT_3D('',#71451,#20313,#20314);
#16508=AXIS2_PLACEMENT_3D('',#71452,#20315,#20316);
#16509=AXIS2_PLACEMENT_3D('',#71454,#20317,#20318);
#16510=AXIS2_PLACEMENT_3D('',#71456,#20320,#20321);
#16511=AXIS2_PLACEMENT_3D('',#71457,#20322,#20323);
#16512=AXIS2_PLACEMENT_3D('',#71458,#20324,#20325);
#16513=AXIS2_PLACEMENT_3D('',#71459,#20326,#20327);
#16514=AXIS2_PLACEMENT_3D('',#71514,#20329,#20330);
#16515=AXIS2_PLACEMENT_3D('',#71515,#20331,#20332);
#16516=AXIS2_PLACEMENT_3D('',#71714,#20334,#20335);
#16517=AXIS2_PLACEMENT_3D('',#71883,#20336,#20337);
#16518=AXIS2_PLACEMENT_3D('',#72249,#20339,#20340);
#16519=AXIS2_PLACEMENT_3D('',#72615,#20342,#20343);
#16520=AXIS2_PLACEMENT_3D('',#72989,#20345,#20346);
#16521=AXIS2_PLACEMENT_3D('',#73364,#20348,#20349);
#16522=AXIS2_PLACEMENT_3D('',#73715,#20351,#20352);
#16523=AXIS2_PLACEMENT_3D('',#73943,#20354,#20355);
#16524=AXIS2_PLACEMENT_3D('',#74315,#20357,#20358);
#16525=AXIS2_PLACEMENT_3D('',#74690,#20360,#20361);
#16526=AXIS2_PLACEMENT_3D('',#75064,#20363,#20364);
#16527=AXIS2_PLACEMENT_3D('',#75443,#20366,#20367);
#16528=AXIS2_PLACEMENT_3D('',#75454,#20368,#20369);
#16529=AXIS2_PLACEMENT_3D('',#77597,#20370,#20371);
#16530=AXIS2_PLACEMENT_3D('',#79711,#20372,#20373);
#16531=AXIS2_PLACEMENT_3D('',#79870,#20374,#20375);
#16532=AXIS2_PLACEMENT_3D('',#80463,#20376,#20377);
#16533=AXIS2_PLACEMENT_3D('',#80465,#20378,#20379);
#16534=AXIS2_PLACEMENT_3D('',#80551,#20380,#20381);
#16535=AXIS2_PLACEMENT_3D('',#80894,#20382,#20383);
#16536=AXIS2_PLACEMENT_3D('',#80896,#20384,#20385);
#16537=AXIS2_PLACEMENT_3D('',#80897,#20386,#20387);
#16538=AXIS2_PLACEMENT_3D('',#80898,#20388,#20389);
#16539=AXIS2_PLACEMENT_3D('',#80900,#20390,#20391);
#16540=AXIS2_PLACEMENT_3D('',#80901,#20392,#20393);
#16541=AXIS2_PLACEMENT_3D('',#80904,#20394,#20395);
#16542=AXIS2_PLACEMENT_3D('',#80908,#20397,#20398);
#16543=AXIS2_PLACEMENT_3D('',#80911,#20400,#20401);
#16544=AXIS2_PLACEMENT_3D('',#80912,#20402,#20403);
#16545=AXIS2_PLACEMENT_3D('',#80926,#20407,#20408);
#16546=AXIS2_PLACEMENT_3D('',#80940,#20412,#20413);
#16547=AXIS2_PLACEMENT_3D('',#80942,#20415,#20416);
#16548=AXIS2_PLACEMENT_3D('',#80943,#20417,#20418);
#16549=AXIS2_PLACEMENT_3D('',#80944,#20419,#20420);
#16550=AXIS2_PLACEMENT_3D('',#80945,#20421,#20422);
#16551=AXIS2_PLACEMENT_3D('',#80946,#20423,#20424);
#16552=AXIS2_PLACEMENT_3D('',#80947,#20425,#20426);
#16553=AXIS2_PLACEMENT_3D('',#80948,#20427,#20428);
#16554=AXIS2_PLACEMENT_3D('',#80949,#20429,#20430);
#16555=AXIS2_PLACEMENT_3D('',#80951,#20431,#20432);
#16556=AXIS2_PLACEMENT_3D('',#80952,#20433,#20434);
#16557=AXIS2_PLACEMENT_3D('',#80954,#20436,#20437);
#16558=AXIS2_PLACEMENT_3D('',#80955,#20438,#20439);
#16559=AXIS2_PLACEMENT_3D('',#80956,#20440,#20441);
#16560=AXIS2_PLACEMENT_3D('',#80957,#20442,#20443);
#16561=AXIS2_PLACEMENT_3D('',#80958,#20444,#20445);
#16562=AXIS2_PLACEMENT_3D('',#80959,#20446,#20447);
#16563=AXIS2_PLACEMENT_3D('',#80960,#20448,#20449);
#16564=AXIS2_PLACEMENT_3D('',#80961,#20450,#20451);
#16565=AXIS2_PLACEMENT_3D('',#80962,#20452,#20453);
#16566=AXIS2_PLACEMENT_3D('',#80963,#20454,#20455);
#16567=AXIS2_PLACEMENT_3D('',#80964,#20456,#20457);
#16568=AXIS2_PLACEMENT_3D('',#80965,#20458,#20459);
#16569=AXIS2_PLACEMENT_3D('',#80966,#20460,#20461);
#16570=AXIS2_PLACEMENT_3D('',#80967,#20462,#20463);
#16571=AXIS2_PLACEMENT_3D('',#80968,#20464,#20465);
#16572=AXIS2_PLACEMENT_3D('',#80969,#20466,#20467);
#16573=AXIS2_PLACEMENT_3D('',#80970,#20468,#20469);
#16574=AXIS2_PLACEMENT_3D('',#80971,#20470,#20471);
#16575=AXIS2_PLACEMENT_3D('',#80972,#20472,#20473);
#16576=AXIS2_PLACEMENT_3D('',#80973,#20474,#20475);
#16577=AXIS2_PLACEMENT_3D('',#80974,#20476,#20477);
#16578=AXIS2_PLACEMENT_3D('',#80975,#20478,#20479);
#16579=AXIS2_PLACEMENT_3D('',#80976,#20480,#20481);
#16580=AXIS2_PLACEMENT_3D('',#80977,#20482,#20483);
#16581=AXIS2_PLACEMENT_3D('',#80978,#20484,#20485);
#16582=AXIS2_PLACEMENT_3D('',#80979,#20486,#20487);
#16583=AXIS2_PLACEMENT_3D('',#80980,#20488,#20489);
#16584=AXIS2_PLACEMENT_3D('',#80981,#20490,#20491);
#16585=AXIS2_PLACEMENT_3D('',#80982,#20492,#20493);
#16586=AXIS2_PLACEMENT_3D('',#80983,#20494,#20495);
#16587=AXIS2_PLACEMENT_3D('',#80984,#20496,#20497);
#16588=AXIS2_PLACEMENT_3D('',#80985,#20498,#20499);
#16589=AXIS2_PLACEMENT_3D('',#80986,#20500,#20501);
#16590=AXIS2_PLACEMENT_3D('',#80987,#20502,#20503);
#16591=AXIS2_PLACEMENT_3D('',#80988,#20504,#20505);
#16592=AXIS2_PLACEMENT_3D('',#80989,#20506,#20507);
#16593=AXIS2_PLACEMENT_3D('',#80990,#20508,#20509);
#16594=AXIS2_PLACEMENT_3D('',#80991,#20510,#20511);
#16595=AXIS2_PLACEMENT_3D('',#80992,#20512,#20513);
#16596=AXIS2_PLACEMENT_3D('',#80993,#20514,#20515);
#16597=AXIS2_PLACEMENT_3D('',#80994,#20516,#20517);
#16598=AXIS2_PLACEMENT_3D('',#80995,#20518,#20519);
#16599=AXIS2_PLACEMENT_3D('',#80996,#20520,#20521);
#16600=AXIS2_PLACEMENT_3D('',#80997,#20522,#20523);
#16601=AXIS2_PLACEMENT_3D('',#80998,#20524,#20525);
#16602=AXIS2_PLACEMENT_3D('',#80999,#20526,#20527);
#16603=AXIS2_PLACEMENT_3D('',#81000,#20528,#20529);
#16604=AXIS2_PLACEMENT_3D('',#81001,#20530,#20531);
#16605=AXIS2_PLACEMENT_3D('',#81002,#20532,#20533);
#16606=AXIS2_PLACEMENT_3D('',#81003,#20534,#20535);
#16607=AXIS2_PLACEMENT_3D('',#81004,#20536,#20537);
#16608=AXIS2_PLACEMENT_3D('',#81005,#20538,#20539);
#16609=AXIS2_PLACEMENT_3D('',#81006,#20540,#20541);
#16610=AXIS2_PLACEMENT_3D('',#81007,#20542,#20543);
#16611=AXIS2_PLACEMENT_3D('',#81008,#20544,#20545);
#16612=AXIS2_PLACEMENT_3D('',#81009,#20546,#20547);
#16613=AXIS2_PLACEMENT_3D('',#81010,#20548,#20549);
#16614=AXIS2_PLACEMENT_3D('',#81011,#20550,#20551);
#16615=AXIS2_PLACEMENT_3D('',#81012,#20552,#20553);
#16616=AXIS2_PLACEMENT_3D('',#81013,#20554,#20555);
#16617=AXIS2_PLACEMENT_3D('',#81014,#20556,#20557);
#16618=AXIS2_PLACEMENT_3D('',#81015,#20558,#20559);
#16619=AXIS2_PLACEMENT_3D('',#81016,#20560,#20561);
#16620=DIRECTION('axis',(0.,0.,1.));
#16621=DIRECTION('refdir',(1.,0.,0.));
#16622=DIRECTION('axis',(0.,0.,1.));
#16623=DIRECTION('refdir',(1.,0.,0.));
#16624=DIRECTION('center_axis',(0.,0.,-1.));
#16625=DIRECTION('ref_axis',(1.,0.,0.));
#16626=DIRECTION('center_axis',(0.,0.,1.));
#16627=DIRECTION('ref_axis',(1.,0.,0.));
#16628=DIRECTION('',(-0.707106781186558,8.65956056235506E-17,-0.707106781186537));
#16629=DIRECTION('center_axis',(0.,0.,-1.));
#16630=DIRECTION('ref_axis',(1.,0.,0.));
#16631=DIRECTION('center_axis',(0.,0.,-1.));
#16632=DIRECTION('ref_axis',(0.,1.,0.));
#16633=DIRECTION('',(-1.,0.,0.));
#16634=DIRECTION('',(0.,1.,0.));
#16635=DIRECTION('',(1.,0.,0.));
#16636=DIRECTION('',(0.,-1.,0.));
#16637=DIRECTION('center_axis',(0.,0.,-1.));
#16638=DIRECTION('ref_axis',(1.,0.,0.));
#16639=DIRECTION('center_axis',(0.,0.,-1.));
#16640=DIRECTION('ref_axis',(1.,0.,0.));
#16641=DIRECTION('center_axis',(0.,0.,-1.));
#16642=DIRECTION('ref_axis',(1.,0.,0.));
#16643=DIRECTION('center_axis',(0.,0.,1.));
#16644=DIRECTION('ref_axis',(1.,0.,0.));
#16645=DIRECTION('',(0.,0.,1.));
#16646=DIRECTION('center_axis',(0.,0.,-1.));
#16647=DIRECTION('ref_axis',(1.,0.,0.));
#16648=DIRECTION('center_axis',(0.,0.,-1.));
#16649=DIRECTION('ref_axis',(1.,0.,0.));
#16650=DIRECTION('center_axis',(0.,0.,1.));
#16651=DIRECTION('ref_axis',(1.,0.,0.));
#16652=DIRECTION('',(-0.707106781186542,8.65956056235487E-17,-0.707106781186553));
#16653=DIRECTION('center_axis',(0.,0.,1.));
#16654=DIRECTION('ref_axis',(1.,0.,0.));
#16655=DIRECTION('',(0.,0.,1.));
#16656=DIRECTION('center_axis',(0.,0.,-1.));
#16657=DIRECTION('ref_axis',(1.,0.,0.));
#16658=DIRECTION('center_axis',(0.,0.,-1.));
#16659=DIRECTION('ref_axis',(1.,0.,0.));
#16660=DIRECTION('center_axis',(0.,0.,1.));
#16661=DIRECTION('ref_axis',(1.,0.,0.));
#16662=DIRECTION('',(-0.707106781186537,8.65956056235481E-17,-0.707106781186558));
#16663=DIRECTION('center_axis',(0.,0.,1.));
#16664=DIRECTION('ref_axis',(1.,0.,0.));
#16665=DIRECTION('',(0.,0.,1.));
#16666=DIRECTION('center_axis',(0.,0.,-1.));
#16667=DIRECTION('ref_axis',(1.,0.,0.));
#16668=DIRECTION('center_axis',(0.,0.,-1.));
#16669=DIRECTION('ref_axis',(1.,0.,0.));
#16670=DIRECTION('center_axis',(0.,0.,1.));
#16671=DIRECTION('ref_axis',(1.,0.,0.));
#16672=DIRECTION('',(-0.707106781186537,8.65956056235481E-17,-0.707106781186558));
#16673=DIRECTION('center_axis',(0.,0.,1.));
#16674=DIRECTION('ref_axis',(1.,0.,0.));
#16675=DIRECTION('',(0.,0.,1.));
#16676=DIRECTION('center_axis',(0.,0.,-1.));
#16677=DIRECTION('ref_axis',(1.,0.,0.));
#16678=DIRECTION('center_axis',(0.,0.,1.));
#16679=DIRECTION('ref_axis',(1.,0.,0.));
#16680=DIRECTION('center_axis',(0.,0.,-1.));
#16681=DIRECTION('ref_axis',(1.,0.,0.));
#16682=DIRECTION('',(-0.707106781186558,-8.65956056235506E-17,0.707106781186537));
#16683=DIRECTION('center_axis',(0.,0.,1.));
#16684=DIRECTION('ref_axis',(1.,0.,0.));
#16685=DIRECTION('center_axis',(0.,0.,1.));
#16686=DIRECTION('ref_axis',(0.,-1.,0.));
#16687=DIRECTION('',(1.,0.,0.));
#16688=DIRECTION('',(0.,1.,0.));
#16689=DIRECTION('',(1.,0.,0.));
#16690=DIRECTION('',(0.,-1.,0.));
#16691=DIRECTION('center_axis',(0.,0.,1.));
#16692=DIRECTION('ref_axis',(1.,0.,0.));
#16693=DIRECTION('center_axis',(0.,0.,1.));
#16694=DIRECTION('ref_axis',(1.,0.,0.));
#16695=DIRECTION('center_axis',(0.,0.,1.));
#16696=DIRECTION('ref_axis',(1.,0.,0.));
#16697=DIRECTION('center_axis',(0.,0.,-1.));
#16698=DIRECTION('ref_axis',(1.,0.,0.));
#16699=DIRECTION('',(0.,0.,-1.));
#16700=DIRECTION('center_axis',(0.,0.,1.));
#16701=DIRECTION('ref_axis',(1.,0.,0.));
#16702=DIRECTION('center_axis',(0.,0.,1.));
#16703=DIRECTION('ref_axis',(1.,0.,0.));
#16704=DIRECTION('center_axis',(0.,0.,-1.));
#16705=DIRECTION('ref_axis',(1.,0.,0.));
#16706=DIRECTION('',(-0.707106781186542,-8.65956056235487E-17,0.707106781186553));
#16707=DIRECTION('center_axis',(0.,0.,-1.));
#16708=DIRECTION('ref_axis',(1.,0.,0.));
#16709=DIRECTION('',(0.,0.,-1.));
#16710=DIRECTION('center_axis',(0.,0.,1.));
#16711=DIRECTION('ref_axis',(1.,0.,0.));
#16712=DIRECTION('center_axis',(0.,0.,1.));
#16713=DIRECTION('ref_axis',(1.,0.,0.));
#16714=DIRECTION('center_axis',(0.,0.,-1.));
#16715=DIRECTION('ref_axis',(1.,0.,0.));
#16716=DIRECTION('',(-0.707106781186537,-8.65956056235481E-17,0.707106781186558));
#16717=DIRECTION('center_axis',(0.,0.,-1.));
#16718=DIRECTION('ref_axis',(1.,0.,0.));
#16719=DIRECTION('',(0.,0.,-1.));
#16720=DIRECTION('center_axis',(0.,0.,1.));
#16721=DIRECTION('ref_axis',(1.,0.,0.));
#16722=DIRECTION('center_axis',(0.,0.,1.));
#16723=DIRECTION('ref_axis',(1.,0.,0.));
#16724=DIRECTION('center_axis',(0.,0.,-1.));
#16725=DIRECTION('ref_axis',(1.,0.,0.));
#16726=DIRECTION('',(-0.707106781186537,-8.65956056235481E-17,0.707106781186558));
#16727=DIRECTION('center_axis',(0.,0.,-1.));
#16728=DIRECTION('ref_axis',(1.,0.,0.));
#16729=DIRECTION('',(0.,0.,-1.));
#16730=DIRECTION('center_axis',(0.,0.,1.));
#16731=DIRECTION('ref_axis',(1.,0.,0.));
#16732=DIRECTION('center_axis',(0.,-1.,0.));
#16733=DIRECTION('ref_axis',(1.,0.,0.));
#16734=DIRECTION('center_axis',(0.,1.,0.));
#16735=DIRECTION('ref_axis',(1.,0.,0.));
#16736=DIRECTION('',(-0.70710678118654,-0.707106781186555,-8.65956056235484E-17));
#16737=DIRECTION('center_axis',(0.,-1.,0.));
#16738=DIRECTION('ref_axis',(1.,0.,0.));
#16739=DIRECTION('center_axis',(0.,-1.,0.));
#16740=DIRECTION('ref_axis',(0.,0.,-1.));
#16741=DIRECTION('',(0.,0.,-1.));
#16742=DIRECTION('',(1.,0.,0.));
#16743=DIRECTION('',(0.,0.,1.));
#16744=DIRECTION('',(-1.,0.,0.));
#16745=DIRECTION('center_axis',(0.,-1.,0.));
#16746=DIRECTION('ref_axis',(1.,0.,0.));
#16747=DIRECTION('center_axis',(0.,-1.,0.));
#16748=DIRECTION('ref_axis',(1.,0.,0.));
#16749=DIRECTION('center_axis',(0.,-1.,0.));
#16750=DIRECTION('ref_axis',(1.,0.,0.));
#16751=DIRECTION('center_axis',(0.,-1.,0.));
#16752=DIRECTION('ref_axis',(1.,0.,0.));
#16753=DIRECTION('center_axis',(0.,-1.,0.));
#16754=DIRECTION('ref_axis',(1.,0.,0.));
#16755=DIRECTION('center_axis',(0.,-1.,0.));
#16756=DIRECTION('ref_axis',(1.,0.,0.));
#16757=DIRECTION('center_axis',(0.,-1.,0.));
#16758=DIRECTION('ref_axis',(1.,0.,0.));
#16759=DIRECTION('center_axis',(0.,1.,0.));
#16760=DIRECTION('ref_axis',(1.,0.,0.));
#16761=DIRECTION('',(0.,1.,0.));
#16762=DIRECTION('center_axis',(0.,1.,0.));
#16763=DIRECTION('ref_axis',(1.,0.,0.));
#16764=DIRECTION('center_axis',(0.,-1.,0.));
#16765=DIRECTION('ref_axis',(1.,0.,0.));
#16766=DIRECTION('center_axis',(0.,1.,0.));
#16767=DIRECTION('ref_axis',(1.,0.,0.));
#16768=DIRECTION('',(-0.70710678118654,-0.707106781186555,-8.65956056235484E-17));
#16769=DIRECTION('center_axis',(0.,1.,0.));
#16770=DIRECTION('ref_axis',(1.,0.,0.));
#16771=DIRECTION('',(0.,1.,0.));
#16772=DIRECTION('center_axis',(0.,1.,0.));
#16773=DIRECTION('ref_axis',(1.,0.,0.));
#16774=DIRECTION('center_axis',(0.,-1.,0.));
#16775=DIRECTION('ref_axis',(1.,0.,0.));
#16776=DIRECTION('center_axis',(0.,1.,0.));
#16777=DIRECTION('ref_axis',(1.,0.,0.));
#16778=DIRECTION('',(-0.707106781186548,-0.707106781186547,-8.65956056235494E-17));
#16779=DIRECTION('center_axis',(0.,1.,0.));
#16780=DIRECTION('ref_axis',(1.,0.,0.));
#16781=DIRECTION('',(0.,1.,0.));
#16782=DIRECTION('center_axis',(0.,1.,0.));
#16783=DIRECTION('ref_axis',(1.,0.,0.));
#16784=DIRECTION('center_axis',(0.,-1.,0.));
#16785=DIRECTION('ref_axis',(1.,0.,0.));
#16786=DIRECTION('center_axis',(0.,1.,0.));
#16787=DIRECTION('ref_axis',(1.,0.,0.));
#16788=DIRECTION('',(-0.707106781186548,-0.707106781186547,-8.65956056235494E-17));
#16789=DIRECTION('center_axis',(0.,1.,0.));
#16790=DIRECTION('ref_axis',(1.,0.,0.));
#16791=DIRECTION('',(0.,1.,0.));
#16792=DIRECTION('center_axis',(0.,1.,0.));
#16793=DIRECTION('ref_axis',(1.,0.,0.));
#16794=DIRECTION('center_axis',(0.,-1.,0.));
#16795=DIRECTION('ref_axis',(1.,0.,0.));
#16796=DIRECTION('center_axis',(0.,1.,0.));
#16797=DIRECTION('ref_axis',(1.,0.,0.));
#16798=DIRECTION('',(-0.707106781186548,-0.707106781186547,-8.65956056235494E-17));
#16799=DIRECTION('center_axis',(0.,1.,0.));
#16800=DIRECTION('ref_axis',(1.,0.,0.));
#16801=DIRECTION('',(0.,1.,0.));
#16802=DIRECTION('center_axis',(0.,1.,0.));
#16803=DIRECTION('ref_axis',(1.,0.,0.));
#16804=DIRECTION('center_axis',(0.,-1.,0.));
#16805=DIRECTION('ref_axis',(1.,0.,0.));
#16806=DIRECTION('center_axis',(0.,1.,0.));
#16807=DIRECTION('ref_axis',(1.,0.,0.));
#16808=DIRECTION('',(-0.707106781186548,-0.707106781186547,-8.65956056235494E-17));
#16809=DIRECTION('center_axis',(0.,1.,0.));
#16810=DIRECTION('ref_axis',(1.,0.,0.));
#16811=DIRECTION('',(0.,1.,0.));
#16812=DIRECTION('center_axis',(0.,1.,0.));
#16813=DIRECTION('ref_axis',(1.,0.,0.));
#16814=DIRECTION('center_axis',(0.,-1.,0.));
#16815=DIRECTION('ref_axis',(1.,0.,0.));
#16816=DIRECTION('center_axis',(0.,1.,0.));
#16817=DIRECTION('ref_axis',(1.,0.,0.));
#16818=DIRECTION('',(-0.70710678118654,-0.707106781186555,-8.65956056235484E-17));
#16819=DIRECTION('center_axis',(0.,1.,0.));
#16820=DIRECTION('ref_axis',(1.,0.,0.));
#16821=DIRECTION('',(0.,1.,0.));
#16822=DIRECTION('center_axis',(0.,1.,0.));
#16823=DIRECTION('ref_axis',(1.,0.,0.));
#16824=DIRECTION('center_axis',(0.,-1.,0.));
#16825=DIRECTION('ref_axis',(1.,0.,0.));
#16826=DIRECTION('center_axis',(0.,1.,0.));
#16827=DIRECTION('ref_axis',(1.,0.,0.));
#16828=DIRECTION('',(-0.70710678118654,-0.707106781186555,-8.65956056235484E-17));
#16829=DIRECTION('center_axis',(0.,1.,0.));
#16830=DIRECTION('ref_axis',(1.,0.,0.));
#16831=DIRECTION('',(0.,1.,0.));
#16832=DIRECTION('center_axis',(0.,1.,0.));
#16833=DIRECTION('ref_axis',(1.,0.,0.));
#16834=DIRECTION('center_axis',(0.,-1.,0.));
#16835=DIRECTION('ref_axis',(1.,0.,0.));
#16836=DIRECTION('',(-0.85716730070211,-0.515038074910058,-1.04972719113862E-16));
#16837=DIRECTION('center_axis',(0.,-1.,0.));
#16838=DIRECTION('ref_axis',(1.,0.,0.));
#16839=DIRECTION('',(-0.85716730070211,-0.515038074910058,-1.04972719113862E-16));
#16840=DIRECTION('center_axis',(0.,-1.,0.));
#16841=DIRECTION('ref_axis',(1.,0.,0.));
#16842=DIRECTION('',(-0.857167300702115,-0.515038074910049,-1.04972719113862E-16));
#16843=DIRECTION('center_axis',(0.,-1.,0.));
#16844=DIRECTION('ref_axis',(1.,0.,0.));
#16845=DIRECTION('',(-0.857167300702115,-0.515038074910049,-1.04972719113862E-16));
#16846=DIRECTION('center_axis',(0.,-1.,0.));
#16847=DIRECTION('ref_axis',(1.,0.,0.));
#16848=DIRECTION('',(-0.85716730070211,-0.515038074910058,-1.04972719113862E-16));
#16849=DIRECTION('center_axis',(0.,-1.,0.));
#16850=DIRECTION('ref_axis',(1.,0.,0.));
#16851=DIRECTION('',(-0.85716730070211,-0.515038074910058,-1.04972719113862E-16));
#16852=DIRECTION('center_axis',(0.,-1.,0.));
#16853=DIRECTION('ref_axis',(1.,0.,0.));
#16854=DIRECTION('',(-0.85716730070211,-0.515038074910058,-1.04972719113862E-16));
#16855=DIRECTION('center_axis',(0.,-1.,0.));
#16856=DIRECTION('ref_axis',(1.,0.,0.));
#16857=DIRECTION('',(-0.85716730070211,-0.515038074910058,-1.04972719113862E-16));
#16858=DIRECTION('center_axis',(0.707106781186541,0.,-0.707106781186554));
#16859=DIRECTION('ref_axis',(-0.707106781186554,0.,-0.707106781186541));
#16860=DIRECTION('',(0.577350269189632,0.577350269189623,0.577350269189622));
#16861=DIRECTION('',(0.,-1.,0.));
#16862=DIRECTION('',(-0.577350269189632,-0.577350269189624,-0.577350269189622));
#16863=DIRECTION('',(-0.577350269189632,0.577350269189624,-0.577350269189622));
#16864=DIRECTION('',(0.,1.,0.));
#16865=DIRECTION('center_axis',(0.707106781186543,-0.707106781186552,0.));
#16866=DIRECTION('ref_axis',(0.,0.,-1.));
#16867=DIRECTION('',(0.,0.,1.));
#16868=DIRECTION('',(-0.577350269189628,-0.577350269189621,0.577350269189628));
#16869=DIRECTION('',(-0.577350269189628,-0.577350269189621,-0.577350269189628));
#16870=DIRECTION('',(0.577350269189632,0.577350269189624,-0.577350269189622));
#16871=DIRECTION('center_axis',(1.,0.,0.));
#16872=DIRECTION('ref_axis',(0.,0.,-1.));
#16873=DIRECTION('',(0.,0.,1.));
#16874=DIRECTION('',(0.,-1.,0.));
#16875=DIRECTION('',(0.,0.,1.));
#16876=DIRECTION('',(0.,1.,0.));
#16877=DIRECTION('',(0.,-0.707106781186553,-0.707106781186542));
#16878=DIRECTION('',(0.,0.,1.));
#16879=DIRECTION('',(0.,0.707106781186542,-0.707106781186553));
#16880=DIRECTION('',(0.,0.,1.));
#16881=DIRECTION('',(0.,-0.707106781186542,-0.707106781186553));
#16882=DIRECTION('',(0.,0.,1.));
#16883=DIRECTION('',(0.,0.707106781186542,-0.707106781186553));
#16884=DIRECTION('',(0.,-1.,0.));
#16885=DIRECTION('',(0.,0.,1.));
#16886=DIRECTION('',(0.,1.,0.));
#16887=DIRECTION('',(0.,0.,1.));
#16888=DIRECTION('',(0.,1.,0.));
#16889=DIRECTION('center_axis',(0.,0.707106781186547,-0.707106781186548));
#16890=DIRECTION('ref_axis',(-1.,0.,0.));
#16891=DIRECTION('',(-1.,0.,0.));
#16892=DIRECTION('',(0.577350269189627,-0.577350269189626,-0.577350269189625));
#16893=DIRECTION('',(1.,0.,0.));
#16894=DIRECTION('center_axis',(0.,-0.707106781186552,0.707106781186543));
#16895=DIRECTION('ref_axis',(1.,0.,0.));
#16896=DIRECTION('',(0.577350269189628,-0.577350269189621,-0.577350269189628));
#16897=DIRECTION('',(-1.,0.,0.));
#16898=DIRECTION('',(0.577350269189623,0.577350269189623,0.577350269189631));
#16899=DIRECTION('',(-0.577350269189623,0.577350269189624,0.577350269189631));
#16900=DIRECTION('center_axis',(0.707106781186548,0.,0.707106781186548));
#16901=DIRECTION('ref_axis',(0.707106781186548,0.,-0.707106781186548));
#16902=DIRECTION('',(-0.577350269189628,-0.577350269189621,0.577350269189628));
#16903=DIRECTION('',(0.,-1.,0.));
#16904=DIRECTION('center_axis',(0.,0.,1.));
#16905=DIRECTION('ref_axis',(0.,-1.,0.));
#16906=DIRECTION('',(1.,0.,0.));
#16907=DIRECTION('',(0.,1.,0.));
#16908=DIRECTION('center_axis',(-0.707106781186553,0.,0.707106781186543));
#16909=DIRECTION('ref_axis',(0.707106781186543,0.,0.707106781186553));
#16910=DIRECTION('',(-0.577350269189623,0.577350269189623,-0.577350269189631));
#16911=DIRECTION('',(0.,-1.,0.));
#16912=DIRECTION('',(0.577350269189623,-0.577350269189623,0.577350269189631));
#16913=DIRECTION('center_axis',(-0.707106781186548,-0.707106781186547,0.));
#16914=DIRECTION('ref_axis',(0.,0.,1.));
#16915=DIRECTION('',(0.,0.,-1.));
#16916=DIRECTION('',(0.577350269189626,-0.577350269189627,-0.577350269189624));
#16917=DIRECTION('',(0.577350269189626,-0.577350269189627,0.577350269189625));
#16918=DIRECTION('center_axis',(0.,-0.707106781186546,-0.707106781186549));
#16919=DIRECTION('ref_axis',(-1.,0.,0.));
#16920=DIRECTION('',(-0.577350269189627,-0.577350269189627,0.577350269189624));
#16921=DIRECTION('',(1.,0.,0.));
#16922=DIRECTION('center_axis',(-0.707106781186546,0.,-0.707106781186549));
#16923=DIRECTION('ref_axis',(-0.707106781186549,0.,0.707106781186546));
#16924=DIRECTION('',(0.,1.,0.));
#16925=DIRECTION('',(0.,-1.,0.));
#16926=DIRECTION('center_axis',(1.,0.,0.));
#16927=DIRECTION('ref_axis',(0.,0.,-1.));
#16928=DIRECTION('',(0.,0.,-1.));
#16929=DIRECTION('',(0.,-1.,0.));
#16930=DIRECTION('',(0.,0.,-1.));
#16931=DIRECTION('',(0.,1.,0.));
#16932=DIRECTION('',(0.,-0.707106781186542,0.707106781186553));
#16933=DIRECTION('',(0.,0.,-1.));
#16934=DIRECTION('',(0.,0.707106781186542,0.707106781186553));
#16935=DIRECTION('',(0.,0.,-1.));
#16936=DIRECTION('',(0.,-0.707106781186542,0.707106781186553));
#16937=DIRECTION('',(0.,0.,-1.));
#16938=DIRECTION('',(0.,0.707106781186553,0.707106781186542));
#16939=DIRECTION('',(0.,-1.,0.));
#16940=DIRECTION('',(0.,0.,-1.));
#16941=DIRECTION('',(0.,1.,0.));
#16942=DIRECTION('',(0.,0.,-1.));
#16943=DIRECTION('center_axis',(0.,0.707106781186542,-0.707106781186553));
#16944=DIRECTION('ref_axis',(-1.,0.,0.));
#16945=DIRECTION('',(-1.,0.,0.));
#16946=DIRECTION('',(1.,0.,0.));
#16947=DIRECTION('center_axis',(0.,1.,0.));
#16948=DIRECTION('ref_axis',(0.,0.,1.));
#16949=DIRECTION('',(-1.,0.,0.));
#16950=DIRECTION('center_axis',(0.,0.707106781186553,0.707106781186542));
#16951=DIRECTION('ref_axis',(1.,0.,0.));
#16952=DIRECTION('center_axis',(0.,0.707106781186553,-0.707106781186542));
#16953=DIRECTION('ref_axis',(-1.,0.,0.));
#16954=DIRECTION('',(1.,0.,0.));
#16955=DIRECTION('center_axis',(0.,1.,0.));
#16956=DIRECTION('ref_axis',(0.,0.,1.));
#16957=DIRECTION('',(-1.,0.,0.));
#16958=DIRECTION('center_axis',(0.,0.707106781186553,0.707106781186542));
#16959=DIRECTION('ref_axis',(1.,0.,0.));
#16960=DIRECTION('',(1.,0.,0.));
#16961=DIRECTION('center_axis',(0.,0.,1.));
#16962=DIRECTION('ref_axis',(0.,-1.,0.));
#16963=DIRECTION('',(1.,0.,0.));
#16964=DIRECTION('center_axis',(0.,0.707106781186552,0.707106781186543));
#16965=DIRECTION('ref_axis',(1.,0.,0.));
#16966=DIRECTION('',(-1.,0.,0.));
#16967=DIRECTION('center_axis',(0.,1.,0.));
#16968=DIRECTION('ref_axis',(0.,0.,1.));
#16969=DIRECTION('',(1.,0.,0.));
#16970=DIRECTION('center_axis',(0.,0.,-1.));
#16971=DIRECTION('ref_axis',(0.,1.,0.));
#16972=DIRECTION('center_axis',(0.,1.,0.));
#16973=DIRECTION('ref_axis',(0.,0.,1.));
#16974=DIRECTION('',(1.,0.,0.));
#16975=DIRECTION('center_axis',(0.,0.,-1.));
#16976=DIRECTION('ref_axis',(0.,1.,0.));
#16977=DIRECTION('',(1.,0.,0.));
#16978=DIRECTION('center_axis',(0.,1.,0.));
#16979=DIRECTION('ref_axis',(0.,0.,1.));
#16980=DIRECTION('center_axis',(0.,1.,0.));
#16981=DIRECTION('ref_axis',(0.,0.,1.));
#16982=DIRECTION('center_axis',(0.,0.,-1.));
#16983=DIRECTION('ref_axis',(0.,1.,0.));
#16984=DIRECTION('',(1.,0.,0.));
#16985=DIRECTION('center_axis',(0.,1.,0.));
#16986=DIRECTION('ref_axis',(0.,0.,1.));
#16987=DIRECTION('',(1.,0.,0.));
#16988=DIRECTION('center_axis',(0.,0.,1.));
#16989=DIRECTION('ref_axis',(0.,-1.,0.));
#16990=DIRECTION('axis',(0.,0.,1.));
#16991=DIRECTION('refdir',(1.,0.,0.));
#16992=DIRECTION('center_axis',(0.,0.,1.));
#16993=DIRECTION('ref_axis',(1.,0.,0.));
#16994=DIRECTION('center_axis',(0.,0.,-1.));
#16995=DIRECTION('ref_axis',(1.,0.,0.));
#16996=DIRECTION('',(-0.707106781186547,-8.65956056235493E-17,0.707106781186548));
#16997=DIRECTION('center_axis',(0.,0.,1.));
#16998=DIRECTION('ref_axis',(1.,0.,0.));
#16999=DIRECTION('center_axis',(0.,0.,1.));
#17000=DIRECTION('ref_axis',(1.,0.,0.));
#17001=DIRECTION('center_axis',(0.,0.,1.));
#17002=DIRECTION('ref_axis',(1.,0.,0.));
#17003=DIRECTION('center_axis',(0.,0.,-1.));
#17004=DIRECTION('ref_axis',(1.,0.,0.));
#17005=DIRECTION('',(-0.707106781186569,-8.65956056235519E-17,0.707106781186526));
#17006=DIRECTION('center_axis',(0.,0.,1.));
#17007=DIRECTION('ref_axis',(1.,0.,0.));
#17008=DIRECTION('center_axis',(0.,0.,1.));
#17009=DIRECTION('ref_axis',(1.,0.,0.));
#17010=DIRECTION('center_axis',(0.,0.,-1.));
#17011=DIRECTION('ref_axis',(1.,0.,0.));
#17012=DIRECTION('',(0.,0.,-1.));
#17013=DIRECTION('center_axis',(0.,0.,1.));
#17014=DIRECTION('ref_axis',(1.,0.,0.));
#17015=DIRECTION('center_axis',(0.,0.,1.));
#17016=DIRECTION('ref_axis',(1.,0.,0.));
#17017=DIRECTION('center_axis',(0.,0.,-1.));
#17018=DIRECTION('ref_axis',(1.,0.,0.));
#17019=DIRECTION('',(-0.707106781186547,-8.65956056235493E-17,0.707106781186548));
#17020=DIRECTION('center_axis',(0.,0.,1.));
#17021=DIRECTION('ref_axis',(1.,0.,0.));
#17022=DIRECTION('center_axis',(0.,0.,1.));
#17023=DIRECTION('ref_axis',(1.,0.,0.));
#17024=DIRECTION('center_axis',(0.,0.,1.));
#17025=DIRECTION('ref_axis',(1.,0.,0.));
#17026=DIRECTION('center_axis',(0.,0.,-1.));
#17027=DIRECTION('ref_axis',(1.,0.,0.));
#17028=DIRECTION('',(-0.707106781186547,-8.65956056235493E-17,0.707106781186548));
#17029=DIRECTION('center_axis',(0.,0.,1.));
#17030=DIRECTION('ref_axis',(1.,0.,0.));
#17031=DIRECTION('center_axis',(0.,0.,1.));
#17032=DIRECTION('ref_axis',(1.,0.,0.));
#17033=DIRECTION('center_axis',(0.,0.,-1.));
#17034=DIRECTION('ref_axis',(1.,0.,0.));
#17035=DIRECTION('',(0.,0.,-1.));
#17036=DIRECTION('center_axis',(0.,0.,1.));
#17037=DIRECTION('ref_axis',(1.,0.,0.));
#17038=DIRECTION('center_axis',(0.,0.,1.));
#17039=DIRECTION('ref_axis',(1.,0.,0.));
#17040=DIRECTION('center_axis',(0.,0.,-1.));
#17041=DIRECTION('ref_axis',(1.,0.,0.));
#17042=DIRECTION('',(-0.707106781186558,-8.65956056235506E-17,0.707106781186537));
#17043=DIRECTION('center_axis',(0.,0.,1.));
#17044=DIRECTION('ref_axis',(1.,0.,0.));
#17045=DIRECTION('center_axis',(0.,0.,1.));
#17046=DIRECTION('ref_axis',(1.,0.,0.));
#17047=DIRECTION('center_axis',(0.,0.,1.));
#17048=DIRECTION('ref_axis',(1.,0.,0.));
#17049=DIRECTION('center_axis',(0.,0.,-1.));
#17050=DIRECTION('ref_axis',(1.,0.,0.));
#17051=DIRECTION('',(-0.707106781186558,-8.65956056235506E-17,0.707106781186537));
#17052=DIRECTION('center_axis',(0.,0.,1.));
#17053=DIRECTION('ref_axis',(1.,0.,0.));
#17054=DIRECTION('center_axis',(0.,0.,1.));
#17055=DIRECTION('ref_axis',(1.,0.,0.));
#17056=DIRECTION('center_axis',(0.,0.,-1.));
#17057=DIRECTION('ref_axis',(1.,0.,0.));
#17058=DIRECTION('',(0.,0.,-1.));
#17059=DIRECTION('center_axis',(0.,0.,1.));
#17060=DIRECTION('ref_axis',(1.,0.,0.));
#17061=DIRECTION('center_axis',(0.,0.,1.));
#17062=DIRECTION('ref_axis',(0.,-1.,0.));
#17063=DIRECTION('',(0.,-1.,0.));
#17064=DIRECTION('',(1.,0.,0.));
#17065=DIRECTION('',(0.,1.,0.));
#17066=DIRECTION('',(-1.,0.,0.));
#17067=DIRECTION('center_axis',(0.,0.,-1.));
#17068=DIRECTION('ref_axis',(1.,0.,0.));
#17069=DIRECTION('',(0.,0.,-1.));
#17070=DIRECTION('center_axis',(0.,0.,-1.));
#17071=DIRECTION('ref_axis',(1.,0.,0.));
#17072=DIRECTION('center_axis',(0.,0.,-1.));
#17073=DIRECTION('ref_axis',(1.,0.,0.));
#17074=DIRECTION('',(0.,0.,-1.));
#17075=DIRECTION('center_axis',(0.,0.,-1.));
#17076=DIRECTION('ref_axis',(1.,0.,0.));
#17077=DIRECTION('center_axis',(0.,0.,-1.));
#17078=DIRECTION('ref_axis',(1.,0.,0.));
#17079=DIRECTION('',(0.,0.,-1.));
#17080=DIRECTION('center_axis',(0.,0.,-1.));
#17081=DIRECTION('ref_axis',(1.,0.,0.));
#17082=DIRECTION('center_axis',(0.,0.,1.));
#17083=DIRECTION('ref_axis',(1.,0.,0.));
#17084=DIRECTION('center_axis',(0.,0.,1.));
#17085=DIRECTION('ref_axis',(1.,0.,0.));
#17086=DIRECTION('center_axis',(0.,0.,1.));
#17087=DIRECTION('ref_axis',(1.,0.,0.));
#17088=DIRECTION('center_axis',(0.,0.,1.));
#17089=DIRECTION('ref_axis',(1.,0.,0.));
#17090=DIRECTION('center_axis',(0.,0.,1.));
#17091=DIRECTION('ref_axis',(1.,0.,0.));
#17092=DIRECTION('center_axis',(0.,0.,1.));
#17093=DIRECTION('ref_axis',(1.,0.,0.));
#17094=DIRECTION('center_axis',(0.,0.,-1.));
#17095=DIRECTION('ref_axis',(1.,0.,0.));
#17096=DIRECTION('',(0.,0.,-1.));
#17097=DIRECTION('center_axis',(0.,0.,1.));
#17098=DIRECTION('ref_axis',(1.,0.,0.));
#17099=DIRECTION('center_axis',(0.,0.,-1.));
#17100=DIRECTION('ref_axis',(1.,0.,0.));
#17101=DIRECTION('',(0.,0.,-1.));
#17102=DIRECTION('center_axis',(0.,0.,1.));
#17103=DIRECTION('ref_axis',(1.,0.,0.));
#17104=DIRECTION('center_axis',(0.,0.,-1.));
#17105=DIRECTION('ref_axis',(1.,0.,0.));
#17106=DIRECTION('',(0.,0.,-1.));
#17107=DIRECTION('center_axis',(0.,0.,1.));
#17108=DIRECTION('ref_axis',(1.,0.,0.));
#17109=DIRECTION('center_axis',(0.,0.,-1.));
#17110=DIRECTION('ref_axis',(1.,0.,0.));
#17111=DIRECTION('center_axis',(0.,0.,1.));
#17112=DIRECTION('ref_axis',(1.,0.,0.));
#17113=DIRECTION('',(-0.70710678118654,8.65956056235484E-17,-0.707106781186555));
#17114=DIRECTION('center_axis',(0.,0.,-1.));
#17115=DIRECTION('ref_axis',(1.,0.,0.));
#17116=DIRECTION('center_axis',(0.,0.,-1.));
#17117=DIRECTION('ref_axis',(1.,0.,0.));
#17118=DIRECTION('center_axis',(0.,0.,-1.));
#17119=DIRECTION('ref_axis',(1.,0.,0.));
#17120=DIRECTION('center_axis',(0.,0.,1.));
#17121=DIRECTION('ref_axis',(1.,0.,0.));
#17122=DIRECTION('',(-0.707106781186561,8.6595605623551E-17,-0.707106781186534));
#17123=DIRECTION('center_axis',(0.,0.,-1.));
#17124=DIRECTION('ref_axis',(1.,0.,0.));
#17125=DIRECTION('center_axis',(0.,0.,-1.));
#17126=DIRECTION('ref_axis',(1.,0.,0.));
#17127=DIRECTION('center_axis',(0.,0.,1.));
#17128=DIRECTION('ref_axis',(1.,0.,0.));
#17129=DIRECTION('',(0.,0.,1.));
#17130=DIRECTION('center_axis',(0.,0.,-1.));
#17131=DIRECTION('ref_axis',(1.,0.,0.));
#17132=DIRECTION('center_axis',(0.,0.,-1.));
#17133=DIRECTION('ref_axis',(1.,0.,0.));
#17134=DIRECTION('center_axis',(0.,0.,1.));
#17135=DIRECTION('ref_axis',(1.,0.,0.));
#17136=DIRECTION('',(-0.70710678118654,8.65956056235484E-17,-0.707106781186555));
#17137=DIRECTION('center_axis',(0.,0.,-1.));
#17138=DIRECTION('ref_axis',(1.,0.,0.));
#17139=DIRECTION('center_axis',(0.,0.,-1.));
#17140=DIRECTION('ref_axis',(1.,0.,0.));
#17141=DIRECTION('center_axis',(0.,0.,-1.));
#17142=DIRECTION('ref_axis',(1.,0.,0.));
#17143=DIRECTION('center_axis',(0.,0.,1.));
#17144=DIRECTION('ref_axis',(1.,0.,0.));
#17145=DIRECTION('',(-0.70710678118654,8.65956056235484E-17,-0.707106781186555));
#17146=DIRECTION('center_axis',(0.,0.,-1.));
#17147=DIRECTION('ref_axis',(1.,0.,0.));
#17148=DIRECTION('center_axis',(0.,0.,-1.));
#17149=DIRECTION('ref_axis',(1.,0.,0.));
#17150=DIRECTION('center_axis',(0.,0.,1.));
#17151=DIRECTION('ref_axis',(1.,0.,0.));
#17152=DIRECTION('',(0.,0.,1.));
#17153=DIRECTION('center_axis',(0.,0.,-1.));
#17154=DIRECTION('ref_axis',(1.,0.,0.));
#17155=DIRECTION('center_axis',(0.,0.,-1.));
#17156=DIRECTION('ref_axis',(1.,0.,0.));
#17157=DIRECTION('center_axis',(0.,0.,1.));
#17158=DIRECTION('ref_axis',(1.,0.,0.));
#17159=DIRECTION('',(-0.70710678118655,8.65956056235497E-17,-0.707106781186545));
#17160=DIRECTION('center_axis',(0.,0.,-1.));
#17161=DIRECTION('ref_axis',(1.,0.,0.));
#17162=DIRECTION('center_axis',(0.,0.,-1.));
#17163=DIRECTION('ref_axis',(1.,0.,0.));
#17164=DIRECTION('center_axis',(0.,0.,-1.));
#17165=DIRECTION('ref_axis',(1.,0.,0.));
#17166=DIRECTION('center_axis',(0.,0.,1.));
#17167=DIRECTION('ref_axis',(1.,0.,0.));
#17168=DIRECTION('',(-0.70710678118655,8.65956056235496E-17,-0.707106781186545));
#17169=DIRECTION('center_axis',(0.,0.,-1.));
#17170=DIRECTION('ref_axis',(1.,0.,0.));
#17171=DIRECTION('center_axis',(0.,0.,-1.));
#17172=DIRECTION('ref_axis',(1.,0.,0.));
#17173=DIRECTION('center_axis',(0.,0.,1.));
#17174=DIRECTION('ref_axis',(1.,0.,0.));
#17175=DIRECTION('',(0.,0.,1.));
#17176=DIRECTION('center_axis',(0.,0.,-1.));
#17177=DIRECTION('ref_axis',(1.,0.,0.));
#17178=DIRECTION('center_axis',(0.,0.,-1.));
#17179=DIRECTION('ref_axis',(0.,1.,0.));
#17180=DIRECTION('',(0.,1.,0.));
#17181=DIRECTION('',(1.,0.,0.));
#17182=DIRECTION('',(0.,-1.,0.));
#17183=DIRECTION('',(-1.,0.,0.));
#17184=DIRECTION('center_axis',(0.,0.,1.));
#17185=DIRECTION('ref_axis',(1.,0.,0.));
#17186=DIRECTION('',(0.,0.,1.));
#17187=DIRECTION('center_axis',(0.,0.,1.));
#17188=DIRECTION('ref_axis',(1.,0.,0.));
#17189=DIRECTION('center_axis',(0.,0.,1.));
#17190=DIRECTION('ref_axis',(1.,0.,0.));
#17191=DIRECTION('',(0.,0.,1.));
#17192=DIRECTION('center_axis',(0.,0.,1.));
#17193=DIRECTION('ref_axis',(1.,0.,0.));
#17194=DIRECTION('center_axis',(0.,0.,1.));
#17195=DIRECTION('ref_axis',(1.,0.,0.));
#17196=DIRECTION('',(0.,0.,1.));
#17197=DIRECTION('center_axis',(0.,0.,1.));
#17198=DIRECTION('ref_axis',(1.,0.,0.));
#17199=DIRECTION('center_axis',(0.,0.,1.));
#17200=DIRECTION('ref_axis',(1.,0.,0.));
#17201=DIRECTION('center_axis',(0.,0.,-1.));
#17202=DIRECTION('ref_axis',(1.,0.,0.));
#17203=DIRECTION('center_axis',(0.,0.,1.));
#17204=DIRECTION('ref_axis',(1.,0.,0.));
#17205=DIRECTION('center_axis',(0.,0.,-1.));
#17206=DIRECTION('ref_axis',(1.,0.,0.));
#17207=DIRECTION('center_axis',(0.,0.,1.));
#17208=DIRECTION('ref_axis',(1.,0.,0.));
#17209=DIRECTION('center_axis',(0.,0.,-1.));
#17210=DIRECTION('ref_axis',(1.,0.,0.));
#17211=DIRECTION('center_axis',(0.,0.,1.));
#17212=DIRECTION('ref_axis',(1.,0.,0.));
#17213=DIRECTION('',(0.,0.,1.));
#17214=DIRECTION('center_axis',(0.,0.,-1.));
#17215=DIRECTION('ref_axis',(1.,0.,0.));
#17216=DIRECTION('center_axis',(0.,0.,1.));
#17217=DIRECTION('ref_axis',(1.,0.,0.));
#17218=DIRECTION('',(0.,0.,1.));
#17219=DIRECTION('center_axis',(0.,0.,-1.));
#17220=DIRECTION('ref_axis',(1.,0.,0.));
#17221=DIRECTION('center_axis',(0.,0.,1.));
#17222=DIRECTION('ref_axis',(1.,0.,0.));
#17223=DIRECTION('',(0.,0.,1.));
#17224=DIRECTION('center_axis',(0.,0.,-1.));
#17225=DIRECTION('ref_axis',(1.,0.,0.));
#17226=DIRECTION('center_axis',(1.,0.,0.));
#17227=DIRECTION('ref_axis',(0.,0.,-1.));
#17228=DIRECTION('center_axis',(-1.,0.,0.));
#17229=DIRECTION('ref_axis',(0.,0.,-1.));
#17230=DIRECTION('',(0.707106781186568,-8.65956056235468E-17,0.707106781186527));
#17231=DIRECTION('center_axis',(1.,0.,0.));
#17232=DIRECTION('ref_axis',(0.,0.,-1.));
#17233=DIRECTION('center_axis',(1.,0.,0.));
#17234=DIRECTION('ref_axis',(0.,0.,-1.));
#17235=DIRECTION('',(0.,1.,0.));
#17236=DIRECTION('',(0.,0.,-1.));
#17237=DIRECTION('',(0.,-0.707106781186547,0.707106781186547));
#17238=DIRECTION('',(0.,1.,0.));
#17239=DIRECTION('',(0.,0.,-1.));
#17240=DIRECTION('',(0.,-1.,0.));
#17241=DIRECTION('',(0.,0.,-1.));
#17242=DIRECTION('',(0.,1.,0.));
#17243=DIRECTION('',(0.,0.,-1.));
#17244=DIRECTION('',(0.,-1.,0.));
#17245=DIRECTION('',(0.,0.707106781186555,0.70710678118654));
#17246=DIRECTION('',(0.,0.,-1.));
#17247=DIRECTION('',(0.,-1.,0.));
#17248=DIRECTION('',(0.,0.,-1.));
#17249=DIRECTION('center_axis',(1.,0.,0.));
#17250=DIRECTION('ref_axis',(0.,0.,-1.));
#17251=DIRECTION('center_axis',(1.,0.,0.));
#17252=DIRECTION('ref_axis',(0.,0.,-1.));
#17253=DIRECTION('center_axis',(1.,0.,0.));
#17254=DIRECTION('ref_axis',(0.,0.,-1.));
#17255=DIRECTION('center_axis',(-1.,0.,0.));
#17256=DIRECTION('ref_axis',(0.,0.,-1.));
#17257=DIRECTION('',(-1.,0.,0.));
#17258=DIRECTION('center_axis',(-1.,0.,0.));
#17259=DIRECTION('ref_axis',(0.,0.,-1.));
#17260=DIRECTION('center_axis',(-1.,0.,0.));
#17261=DIRECTION('ref_axis',(0.,0.,-1.));
#17262=DIRECTION('center_axis',(1.,0.,0.));
#17263=DIRECTION('ref_axis',(0.,0.,-1.));
#17264=DIRECTION('center_axis',(-1.,0.,0.));
#17265=DIRECTION('ref_axis',(0.,0.,-1.));
#17266=DIRECTION('',(0.70710678118656,-8.65956056235478E-17,0.707106781186535));
#17267=DIRECTION('center_axis',(-1.,0.,0.));
#17268=DIRECTION('ref_axis',(0.,0.,-1.));
#17269=DIRECTION('',(-1.,0.,0.));
#17270=DIRECTION('center_axis',(-1.,0.,0.));
#17271=DIRECTION('ref_axis',(0.,0.,-1.));
#17272=DIRECTION('center_axis',(-1.,0.,0.));
#17273=DIRECTION('ref_axis',(0.,0.,-1.));
#17274=DIRECTION('center_axis',(1.,0.,0.));
#17275=DIRECTION('ref_axis',(0.,0.,-1.));
#17276=DIRECTION('center_axis',(-1.,0.,0.));
#17277=DIRECTION('ref_axis',(0.,0.,-1.));
#17278=DIRECTION('',(0.707106781186558,-8.65956056235481E-17,0.707106781186537));
#17279=DIRECTION('center_axis',(-1.,0.,0.));
#17280=DIRECTION('ref_axis',(0.,0.,-1.));
#17281=DIRECTION('',(-1.,0.,0.));
#17282=DIRECTION('center_axis',(-1.,0.,0.));
#17283=DIRECTION('ref_axis',(0.,0.,-1.));
#17284=DIRECTION('center_axis',(-1.,0.,0.));
#17285=DIRECTION('ref_axis',(0.,0.,-1.));
#17286=DIRECTION('center_axis',(1.,0.,0.));
#17287=DIRECTION('ref_axis',(0.,0.,-1.));
#17288=DIRECTION('center_axis',(-1.,0.,0.));
#17289=DIRECTION('ref_axis',(0.,0.,-1.));
#17290=DIRECTION('',(0.707106781186561,-8.65956056235477E-17,0.707106781186534));
#17291=DIRECTION('center_axis',(-1.,0.,0.));
#17292=DIRECTION('ref_axis',(0.,0.,-1.));
#17293=DIRECTION('',(-1.,0.,0.));
#17294=DIRECTION('center_axis',(-1.,0.,0.));
#17295=DIRECTION('ref_axis',(0.,0.,-1.));
#17296=DIRECTION('center_axis',(-1.,0.,0.));
#17297=DIRECTION('ref_axis',(0.,0.,-1.));
#17298=DIRECTION('center_axis',(1.,0.,0.));
#17299=DIRECTION('ref_axis',(0.,1.,0.));
#17300=DIRECTION('',(0.515038074910049,-0.857167300702115,-1.04972719113862E-16));
#17301=DIRECTION('center_axis',(1.,0.,0.));
#17302=DIRECTION('ref_axis',(0.,1.,0.));
#17303=DIRECTION('',(0.515038074910049,-0.857167300702115,-1.04972719113862E-16));
#17304=DIRECTION('center_axis',(1.,0.,0.));
#17305=DIRECTION('ref_axis',(0.,1.,0.));
#17306=DIRECTION('',(0.515038074910049,-0.857167300702115,-1.04972719113862E-16));
#17307=DIRECTION('center_axis',(1.,0.,0.));
#17308=DIRECTION('ref_axis',(0.,1.,0.));
#17309=DIRECTION('',(0.515038074910049,-0.857167300702115,-1.04972719113862E-16));
#17310=DIRECTION('center_axis',(-1.,0.,0.));
#17311=DIRECTION('ref_axis',(0.,0.,-1.));
#17312=DIRECTION('center_axis',(1.,0.,0.));
#17313=DIRECTION('ref_axis',(0.,0.,-1.));
#17314=DIRECTION('',(-0.707106781186555,8.65956056235485E-17,0.70710678118654));
#17315=DIRECTION('center_axis',(-1.,0.,0.));
#17316=DIRECTION('ref_axis',(0.,0.,-1.));
#17317=DIRECTION('center_axis',(1.,0.,0.));
#17318=DIRECTION('ref_axis',(0.,0.,-1.));
#17319=DIRECTION('',(0.,1.,0.));
#17320=DIRECTION('',(0.,0.,-1.));
#17321=DIRECTION('',(0.,-0.707106781186555,-0.70710678118654));
#17322=DIRECTION('',(0.,-1.,0.));
#17323=DIRECTION('',(0.,0.,-1.));
#17324=DIRECTION('',(0.,1.,0.));
#17325=DIRECTION('',(0.,0.,-1.));
#17326=DIRECTION('',(0.,-1.,0.));
#17327=DIRECTION('',(0.,0.,-1.));
#17328=DIRECTION('',(0.,1.,0.));
#17329=DIRECTION('',(0.,0.707106781186547,-0.707106781186547));
#17330=DIRECTION('',(0.,0.,-1.));
#17331=DIRECTION('',(0.,-1.,0.));
#17332=DIRECTION('',(0.,0.,1.));
#17333=DIRECTION('center_axis',(-1.,0.,0.));
#17334=DIRECTION('ref_axis',(0.,0.,-1.));
#17335=DIRECTION('center_axis',(-1.,0.,0.));
#17336=DIRECTION('ref_axis',(0.,0.,-1.));
#17337=DIRECTION('center_axis',(-1.,0.,0.));
#17338=DIRECTION('ref_axis',(0.,0.,-1.));
#17339=DIRECTION('center_axis',(1.,0.,0.));
#17340=DIRECTION('ref_axis',(0.,0.,-1.));
#17341=DIRECTION('',(1.,0.,0.));
#17342=DIRECTION('center_axis',(1.,0.,0.));
#17343=DIRECTION('ref_axis',(0.,0.,-1.));
#17344=DIRECTION('center_axis',(1.,0.,0.));
#17345=DIRECTION('ref_axis',(0.,0.,-1.));
#17346=DIRECTION('center_axis',(-1.,0.,0.));
#17347=DIRECTION('ref_axis',(0.,0.,-1.));
#17348=DIRECTION('center_axis',(1.,0.,0.));
#17349=DIRECTION('ref_axis',(0.,0.,-1.));
#17350=DIRECTION('',(-0.707106781186547,8.65956056235494E-17,0.707106781186548));
#17351=DIRECTION('center_axis',(1.,0.,0.));
#17352=DIRECTION('ref_axis',(0.,0.,-1.));
#17353=DIRECTION('',(1.,0.,0.));
#17354=DIRECTION('center_axis',(1.,0.,0.));
#17355=DIRECTION('ref_axis',(0.,0.,-1.));
#17356=DIRECTION('center_axis',(1.,0.,0.));
#17357=DIRECTION('ref_axis',(0.,0.,-1.));
#17358=DIRECTION('center_axis',(-1.,0.,0.));
#17359=DIRECTION('ref_axis',(0.,0.,-1.));
#17360=DIRECTION('center_axis',(1.,0.,0.));
#17361=DIRECTION('ref_axis',(0.,0.,-1.));
#17362=DIRECTION('',(-0.707106781186545,8.65956056235496E-17,0.70710678118655));
#17363=DIRECTION('center_axis',(1.,0.,0.));
#17364=DIRECTION('ref_axis',(0.,0.,-1.));
#17365=DIRECTION('',(1.,0.,0.));
#17366=DIRECTION('center_axis',(1.,0.,0.));
#17367=DIRECTION('ref_axis',(0.,0.,-1.));
#17368=DIRECTION('center_axis',(1.,0.,0.));
#17369=DIRECTION('ref_axis',(0.,0.,-1.));
#17370=DIRECTION('center_axis',(-1.,0.,0.));
#17371=DIRECTION('ref_axis',(0.,0.,-1.));
#17372=DIRECTION('center_axis',(1.,0.,0.));
#17373=DIRECTION('ref_axis',(0.,0.,-1.));
#17374=DIRECTION('',(-0.707106781186548,8.65956056235493E-17,0.707106781186547));
#17375=DIRECTION('center_axis',(1.,0.,0.));
#17376=DIRECTION('ref_axis',(0.,0.,-1.));
#17377=DIRECTION('',(1.,0.,0.));
#17378=DIRECTION('center_axis',(1.,0.,0.));
#17379=DIRECTION('ref_axis',(0.,0.,-1.));
#17380=DIRECTION('center_axis',(1.,0.,0.));
#17381=DIRECTION('ref_axis',(0.,0.,-1.));
#17382=DIRECTION('center_axis',(-1.,0.,0.));
#17383=DIRECTION('ref_axis',(0.,1.,0.));
#17384=DIRECTION('',(-0.515038074910058,-0.85716730070211,1.04972719113862E-16));
#17385=DIRECTION('center_axis',(-1.,0.,0.));
#17386=DIRECTION('ref_axis',(0.,1.,0.));
#17387=DIRECTION('',(-0.515038074910058,-0.85716730070211,1.04972719113862E-16));
#17388=DIRECTION('center_axis',(-1.,0.,0.));
#17389=DIRECTION('ref_axis',(0.,1.,0.));
#17390=DIRECTION('',(-0.515038074910058,-0.85716730070211,1.04972719113862E-16));
#17391=DIRECTION('center_axis',(-1.,0.,0.));
#17392=DIRECTION('ref_axis',(0.,1.,0.));
#17393=DIRECTION('',(-0.515038074910058,-0.85716730070211,1.04972719113862E-16));
#17394=DIRECTION('center_axis',(0.,1.,0.));
#17395=DIRECTION('ref_axis',(1.,0.,0.));
#17396=DIRECTION('center_axis',(0.,-1.,0.));
#17397=DIRECTION('ref_axis',(1.,0.,0.));
#17398=DIRECTION('',(-0.707106781186539,0.707106781186555,8.65956056235483E-17));
#17399=DIRECTION('center_axis',(0.,1.,0.));
#17400=DIRECTION('ref_axis',(1.,0.,0.));
#17401=DIRECTION('center_axis',(0.,1.,0.));
#17402=DIRECTION('ref_axis',(0.,0.,1.));
#17403=DIRECTION('',(0.,0.,1.));
#17404=DIRECTION('',(1.,0.,0.));
#17405=DIRECTION('',(0.,0.,-1.));
#17406=DIRECTION('',(-1.,0.,0.));
#17407=DIRECTION('center_axis',(0.,1.,0.));
#17408=DIRECTION('ref_axis',(1.,0.,0.));
#17409=DIRECTION('center_axis',(0.,1.,0.));
#17410=DIRECTION('ref_axis',(1.,0.,0.));
#17411=DIRECTION('center_axis',(0.,1.,0.));
#17412=DIRECTION('ref_axis',(1.,0.,0.));
#17413=DIRECTION('center_axis',(0.,1.,0.));
#17414=DIRECTION('ref_axis',(1.,0.,0.));
#17415=DIRECTION('center_axis',(0.,1.,0.));
#17416=DIRECTION('ref_axis',(1.,0.,0.));
#17417=DIRECTION('center_axis',(0.,1.,0.));
#17418=DIRECTION('ref_axis',(1.,0.,0.));
#17419=DIRECTION('center_axis',(0.,1.,0.));
#17420=DIRECTION('ref_axis',(1.,0.,0.));
#17421=DIRECTION('center_axis',(0.,1.,0.));
#17422=DIRECTION('ref_axis',(1.,0.,0.));
#17423=DIRECTION('center_axis',(0.,1.,0.));
#17424=DIRECTION('ref_axis',(1.,0.,0.));
#17425=DIRECTION('center_axis',(0.,1.,0.));
#17426=DIRECTION('ref_axis',(1.,0.,0.));
#17427=DIRECTION('center_axis',(0.,1.,0.));
#17428=DIRECTION('ref_axis',(1.,0.,0.));
#17429=DIRECTION('center_axis',(0.,1.,0.));
#17430=DIRECTION('ref_axis',(1.,0.,0.));
#17431=DIRECTION('center_axis',(0.,1.,0.));
#17432=DIRECTION('ref_axis',(1.,0.,0.));
#17433=DIRECTION('center_axis',(0.,-1.,0.));
#17434=DIRECTION('ref_axis',(1.,0.,0.));
#17435=DIRECTION('',(0.,-1.,0.));
#17436=DIRECTION('center_axis',(0.,-1.,0.));
#17437=DIRECTION('ref_axis',(1.,0.,0.));
#17438=DIRECTION('center_axis',(0.,1.,0.));
#17439=DIRECTION('ref_axis',(1.,0.,0.));
#17440=DIRECTION('center_axis',(0.,-1.,0.));
#17441=DIRECTION('ref_axis',(1.,0.,0.));
#17442=DIRECTION('',(-0.707106781186539,0.707106781186555,8.65956056235483E-17));
#17443=DIRECTION('center_axis',(0.,-1.,0.));
#17444=DIRECTION('ref_axis',(1.,0.,0.));
#17445=DIRECTION('',(0.,-1.,0.));
#17446=DIRECTION('center_axis',(0.,-1.,0.));
#17447=DIRECTION('ref_axis',(1.,0.,0.));
#17448=DIRECTION('center_axis',(0.,1.,0.));
#17449=DIRECTION('ref_axis',(1.,0.,0.));
#17450=DIRECTION('center_axis',(0.,-1.,0.));
#17451=DIRECTION('ref_axis',(1.,0.,0.));
#17452=DIRECTION('',(-0.707106781186539,0.707106781186555,8.65956056235483E-17));
#17453=DIRECTION('center_axis',(0.,-1.,0.));
#17454=DIRECTION('ref_axis',(1.,0.,0.));
#17455=DIRECTION('',(0.,-1.,0.));
#17456=DIRECTION('center_axis',(0.,-1.,0.));
#17457=DIRECTION('ref_axis',(1.,0.,0.));
#17458=DIRECTION('center_axis',(0.,1.,0.));
#17459=DIRECTION('ref_axis',(1.,0.,0.));
#17460=DIRECTION('center_axis',(0.,-1.,0.));
#17461=DIRECTION('ref_axis',(1.,0.,0.));
#17462=DIRECTION('',(-0.707106781186547,0.707106781186548,8.65956056235493E-17));
#17463=DIRECTION('center_axis',(0.,-1.,0.));
#17464=DIRECTION('ref_axis',(1.,0.,0.));
#17465=DIRECTION('',(0.,-1.,0.));
#17466=DIRECTION('center_axis',(0.,-1.,0.));
#17467=DIRECTION('ref_axis',(1.,0.,0.));
#17468=DIRECTION('center_axis',(0.,1.,0.));
#17469=DIRECTION('ref_axis',(1.,0.,0.));
#17470=DIRECTION('center_axis',(0.,-1.,0.));
#17471=DIRECTION('ref_axis',(1.,0.,0.));
#17472=DIRECTION('',(-0.707106781186547,0.707106781186548,8.65956056235493E-17));
#17473=DIRECTION('center_axis',(0.,-1.,0.));
#17474=DIRECTION('ref_axis',(1.,0.,0.));
#17475=DIRECTION('',(0.,-1.,0.));
#17476=DIRECTION('center_axis',(0.,-1.,0.));
#17477=DIRECTION('ref_axis',(1.,0.,0.));
#17478=DIRECTION('center_axis',(0.,1.,0.));
#17479=DIRECTION('ref_axis',(1.,0.,0.));
#17480=DIRECTION('center_axis',(0.,-1.,0.));
#17481=DIRECTION('ref_axis',(1.,0.,0.));
#17482=DIRECTION('',(-0.707106781186539,0.707106781186555,8.65956056235483E-17));
#17483=DIRECTION('center_axis',(0.,-1.,0.));
#17484=DIRECTION('ref_axis',(1.,0.,0.));
#17485=DIRECTION('',(0.,-1.,0.));
#17486=DIRECTION('center_axis',(0.,-1.,0.));
#17487=DIRECTION('ref_axis',(1.,0.,0.));
#17488=DIRECTION('center_axis',(0.,1.,0.));
#17489=DIRECTION('ref_axis',(1.,0.,0.));
#17490=DIRECTION('',(-0.857167300702115,0.515038074910049,1.04972719113862E-16));
#17491=DIRECTION('center_axis',(0.,1.,0.));
#17492=DIRECTION('ref_axis',(1.,0.,0.));
#17493=DIRECTION('',(-0.857167300702115,0.515038074910049,1.04972719113862E-16));
#17494=DIRECTION('center_axis',(0.,1.,0.));
#17495=DIRECTION('ref_axis',(1.,0.,0.));
#17496=DIRECTION('',(-0.85716730070211,0.515038074910058,1.04972719113862E-16));
#17497=DIRECTION('center_axis',(0.,1.,0.));
#17498=DIRECTION('ref_axis',(1.,0.,0.));
#17499=DIRECTION('',(-0.85716730070211,0.515038074910058,1.04972719113862E-16));
#17500=DIRECTION('center_axis',(0.,1.,0.));
#17501=DIRECTION('ref_axis',(1.,0.,0.));
#17502=DIRECTION('',(-0.85716730070211,0.515038074910058,1.04972719113862E-16));
#17503=DIRECTION('center_axis',(0.,1.,0.));
#17504=DIRECTION('ref_axis',(1.,0.,0.));
#17505=DIRECTION('',(-0.85716730070211,0.515038074910058,1.04972719113862E-16));
#17506=DIRECTION('center_axis',(0.,1.,0.));
#17507=DIRECTION('ref_axis',(1.,0.,0.));
#17508=DIRECTION('center_axis',(0.,-1.,0.));
#17509=DIRECTION('ref_axis',(1.,0.,0.));
#17510=DIRECTION('',(-0.707106781186558,0.707106781186537,8.65956056235506E-17));
#17511=DIRECTION('center_axis',(0.,-1.,0.));
#17512=DIRECTION('ref_axis',(1.,0.,0.));
#17513=DIRECTION('',(0.,-1.,0.));
#17514=DIRECTION('center_axis',(0.,-1.,0.));
#17515=DIRECTION('ref_axis',(1.,0.,0.));
#17516=DIRECTION('center_axis',(0.,1.,0.));
#17517=DIRECTION('ref_axis',(1.,0.,0.));
#17518=DIRECTION('center_axis',(0.,-1.,0.));
#17519=DIRECTION('ref_axis',(1.,0.,0.));
#17520=DIRECTION('',(-0.707106781186537,0.707106781186558,8.65956056235481E-17));
#17521=DIRECTION('center_axis',(0.,-1.,0.));
#17522=DIRECTION('ref_axis',(1.,0.,0.));
#17523=DIRECTION('',(0.,-1.,0.));
#17524=DIRECTION('center_axis',(0.,-1.,0.));
#17525=DIRECTION('ref_axis',(1.,0.,0.));
#17526=DIRECTION('center_axis',(0.,1.,0.));
#17527=DIRECTION('ref_axis',(1.,0.,0.));
#17528=DIRECTION('center_axis',(0.,-1.,0.));
#17529=DIRECTION('ref_axis',(1.,0.,0.));
#17530=DIRECTION('',(-0.707106781186542,0.707106781186553,8.65956056235487E-17));
#17531=DIRECTION('center_axis',(0.,-1.,0.));
#17532=DIRECTION('ref_axis',(1.,0.,0.));
#17533=DIRECTION('',(0.,-1.,0.));
#17534=DIRECTION('center_axis',(0.,-1.,0.));
#17535=DIRECTION('ref_axis',(1.,0.,0.));
#17536=DIRECTION('center_axis',(0.,1.,0.));
#17537=DIRECTION('ref_axis',(1.,0.,0.));
#17538=DIRECTION('center_axis',(0.,-1.,0.));
#17539=DIRECTION('ref_axis',(1.,0.,0.));
#17540=DIRECTION('',(-0.707106781186537,0.707106781186558,8.65956056235481E-17));
#17541=DIRECTION('center_axis',(0.,-1.,0.));
#17542=DIRECTION('ref_axis',(1.,0.,0.));
#17543=DIRECTION('',(0.,-1.,0.));
#17544=DIRECTION('center_axis',(0.,-1.,0.));
#17545=DIRECTION('ref_axis',(1.,0.,0.));
#17546=DIRECTION('center_axis',(0.,1.,0.));
#17547=DIRECTION('ref_axis',(1.,0.,0.));
#17548=DIRECTION('center_axis',(0.,-1.,0.));
#17549=DIRECTION('ref_axis',(1.,0.,0.));
#17550=DIRECTION('',(-0.707106781186542,0.707106781186553,8.65956056235487E-17));
#17551=DIRECTION('center_axis',(0.,-1.,0.));
#17552=DIRECTION('ref_axis',(1.,0.,0.));
#17553=DIRECTION('',(0.,-1.,0.));
#17554=DIRECTION('center_axis',(0.,-1.,0.));
#17555=DIRECTION('ref_axis',(1.,0.,0.));
#17556=DIRECTION('center_axis',(0.,1.,0.));
#17557=DIRECTION('ref_axis',(1.,0.,0.));
#17558=DIRECTION('center_axis',(0.,-1.,0.));
#17559=DIRECTION('ref_axis',(1.,0.,0.));
#17560=DIRECTION('',(-0.707106781186537,0.707106781186558,8.65956056235481E-17));
#17561=DIRECTION('center_axis',(0.,-1.,0.));
#17562=DIRECTION('ref_axis',(1.,0.,0.));
#17563=DIRECTION('',(0.,-1.,0.));
#17564=DIRECTION('center_axis',(0.,-1.,0.));
#17565=DIRECTION('ref_axis',(1.,0.,0.));
#17566=DIRECTION('center_axis',(0.,1.,0.));
#17567=DIRECTION('ref_axis',(1.,0.,0.));
#17568=DIRECTION('center_axis',(0.,-1.,0.));
#17569=DIRECTION('ref_axis',(1.,0.,0.));
#17570=DIRECTION('',(-0.707106781186537,0.707106781186558,8.65956056235481E-17));
#17571=DIRECTION('center_axis',(0.,-1.,0.));
#17572=DIRECTION('ref_axis',(1.,0.,0.));
#17573=DIRECTION('',(0.,-1.,0.));
#17574=DIRECTION('center_axis',(0.,-1.,0.));
#17575=DIRECTION('ref_axis',(1.,0.,0.));
#17576=DIRECTION('center_axis',(0.,1.,0.));
#17577=DIRECTION('ref_axis',(1.,0.,0.));
#17578=DIRECTION('center_axis',(0.,-1.,0.));
#17579=DIRECTION('ref_axis',(1.,0.,0.));
#17580=DIRECTION('',(-0.707106781186558,0.707106781186537,8.65956056235506E-17));
#17581=DIRECTION('center_axis',(0.,-1.,0.));
#17582=DIRECTION('ref_axis',(1.,0.,0.));
#17583=DIRECTION('',(0.,-1.,0.));
#17584=DIRECTION('center_axis',(0.,-1.,0.));
#17585=DIRECTION('ref_axis',(1.,0.,0.));
#17586=DIRECTION('center_axis',(0.,1.,0.));
#17587=DIRECTION('ref_axis',(1.,0.,0.));
#17588=DIRECTION('center_axis',(0.,1.,0.));
#17589=DIRECTION('ref_axis',(1.,0.,0.));
#17590=DIRECTION('center_axis',(0.,1.,0.));
#17591=DIRECTION('ref_axis',(1.,0.,0.));
#17592=DIRECTION('center_axis',(0.,1.,0.));
#17593=DIRECTION('ref_axis',(1.,0.,0.));
#17594=DIRECTION('center_axis',(0.,1.,0.));
#17595=DIRECTION('ref_axis',(1.,0.,0.));
#17596=DIRECTION('center_axis',(0.,1.,0.));
#17597=DIRECTION('ref_axis',(1.,0.,0.));
#17598=DIRECTION('center_axis',(0.,1.,0.));
#17599=DIRECTION('ref_axis',(1.,0.,0.));
#17600=DIRECTION('center_axis',(0.,1.,0.));
#17601=DIRECTION('ref_axis',(1.,0.,0.));
#17602=DIRECTION('center_axis',(0.,1.,0.));
#17603=DIRECTION('ref_axis',(1.,0.,0.));
#17604=DIRECTION('center_axis',(0.,1.,0.));
#17605=DIRECTION('ref_axis',(1.,0.,0.));
#17606=DIRECTION('center_axis',(0.,1.,0.));
#17607=DIRECTION('ref_axis',(1.,0.,0.));
#17608=DIRECTION('center_axis',(0.,1.,0.));
#17609=DIRECTION('ref_axis',(1.,0.,0.));
#17610=DIRECTION('center_axis',(0.,1.,0.));
#17611=DIRECTION('ref_axis',(1.,0.,0.));
#17612=DIRECTION('center_axis',(0.,1.,0.));
#17613=DIRECTION('ref_axis',(1.,0.,0.));
#17614=DIRECTION('center_axis',(0.,1.,0.));
#17615=DIRECTION('ref_axis',(1.,0.,0.));
#17616=DIRECTION('center_axis',(0.,1.,0.));
#17617=DIRECTION('ref_axis',(1.,0.,0.));
#17618=DIRECTION('center_axis',(0.,-1.,0.));
#17619=DIRECTION('ref_axis',(1.,0.,0.));
#17620=DIRECTION('',(0.,-1.,0.));
#17621=DIRECTION('center_axis',(0.,1.,0.));
#17622=DIRECTION('ref_axis',(1.,0.,0.));
#17623=DIRECTION('center_axis',(0.,-1.,0.));
#17624=DIRECTION('ref_axis',(1.,0.,0.));
#17625=DIRECTION('',(0.,-1.,0.));
#17626=DIRECTION('center_axis',(0.,1.,0.));
#17627=DIRECTION('ref_axis',(1.,0.,0.));
#17628=DIRECTION('center_axis',(0.,-1.,0.));
#17629=DIRECTION('ref_axis',(1.,0.,0.));
#17630=DIRECTION('',(0.,-1.,0.));
#17631=DIRECTION('center_axis',(0.,1.,0.));
#17632=DIRECTION('ref_axis',(1.,0.,0.));
#17633=DIRECTION('center_axis',(0.,-1.,0.));
#17634=DIRECTION('ref_axis',(1.,0.,0.));
#17635=DIRECTION('',(0.,-1.,0.));
#17636=DIRECTION('center_axis',(0.,1.,0.));
#17637=DIRECTION('ref_axis',(1.,0.,0.));
#17638=DIRECTION('center_axis',(0.,-1.,0.));
#17639=DIRECTION('ref_axis',(1.,0.,0.));
#17640=DIRECTION('',(0.,-1.,0.));
#17641=DIRECTION('center_axis',(0.,1.,0.));
#17642=DIRECTION('ref_axis',(1.,0.,0.));
#17643=DIRECTION('center_axis',(0.,-1.,0.));
#17644=DIRECTION('ref_axis',(1.,0.,0.));
#17645=DIRECTION('',(0.,-1.,0.));
#17646=DIRECTION('center_axis',(0.,1.,0.));
#17647=DIRECTION('ref_axis',(1.,0.,0.));
#17648=DIRECTION('center_axis',(0.,-1.,0.));
#17649=DIRECTION('ref_axis',(1.,0.,0.));
#17650=DIRECTION('',(0.,-1.,0.));
#17651=DIRECTION('center_axis',(0.,1.,0.));
#17652=DIRECTION('ref_axis',(1.,0.,0.));
#17653=DIRECTION('center_axis',(0.,-1.,0.));
#17654=DIRECTION('ref_axis',(1.,0.,0.));
#17655=DIRECTION('',(0.,-1.,0.));
#17656=DIRECTION('center_axis',(0.,1.,0.));
#17657=DIRECTION('ref_axis',(1.,0.,0.));
#17658=DIRECTION('center_axis',(0.707106781186548,0.,0.707106781186548));
#17659=DIRECTION('ref_axis',(0.707106781186548,0.,-0.707106781186548));
#17660=DIRECTION('',(0.577350269189628,-0.577350269189621,-0.577350269189628));
#17661=DIRECTION('',(-0.577350269189629,0.577350269189619,0.577350269189629));
#17662=DIRECTION('',(-0.577350269189626,-0.577350269189626,0.577350269189626));
#17663=DIRECTION('center_axis',(0.707106781186541,0.707106781186554,0.));
#17664=DIRECTION('ref_axis',(0.,0.,-1.));
#17665=DIRECTION('',(-0.577350269189633,0.577350269189622,-0.577350269189622));
#17666=DIRECTION('',(-0.577350269189632,0.577350269189622,0.577350269189624));
#17667=DIRECTION('',(0.577350269189633,-0.577350269189622,0.577350269189622));
#17668=DIRECTION('center_axis',(0.,-0.707106781186552,0.707106781186543));
#17669=DIRECTION('ref_axis',(1.,0.,0.));
#17670=DIRECTION('',(0.577350269189623,0.577350269189623,0.577350269189631));
#17671=DIRECTION('',(1.,0.,0.));
#17672=DIRECTION('center_axis',(0.,0.707106781186549,-0.707106781186546));
#17673=DIRECTION('ref_axis',(-1.,0.,0.));
#17674=DIRECTION('',(0.577350269189633,0.577350269189621,0.577350269189623));
#17675=DIRECTION('',(0.577350269189628,-0.577350269189624,-0.577350269189626));
#17676=DIRECTION('',(-0.577350269189627,-0.577350269189624,-0.577350269189627));
#17677=DIRECTION('center_axis',(0.707106781186541,0.,-0.707106781186554));
#17678=DIRECTION('ref_axis',(-0.707106781186554,0.,-0.707106781186541));
#17679=DIRECTION('',(-0.577350269189634,0.577350269189621,-0.577350269189623));
#17680=DIRECTION('center_axis',(-0.707106781186546,0.,-0.707106781186549));
#17681=DIRECTION('ref_axis',(-0.707106781186549,0.,0.707106781186546));
#17682=DIRECTION('',(-0.577350269189628,-0.577350269189623,0.577350269189626));
#17683=DIRECTION('',(0.577350269189627,0.577350269189625,-0.577350269189625));
#17684=DIRECTION('center_axis',(-0.707106781186546,0.707106781186549,0.));
#17685=DIRECTION('ref_axis',(0.,0.,1.));
#17686=DIRECTION('',(0.577350269189624,0.577350269189622,0.577350269189632));
#17687=DIRECTION('',(0.577350269189627,0.577350269189625,-0.577350269189625));
#17688=DIRECTION('center_axis',(0.,0.707106781186548,0.707106781186548));
#17689=DIRECTION('ref_axis',(1.,0.,0.));
#17690=DIRECTION('',(-0.57735026918962,0.577350269189629,-0.577350269189629));
#17691=DIRECTION('center_axis',(-0.707106781186553,0.,0.707106781186543));
#17692=DIRECTION('ref_axis',(0.707106781186543,0.,0.707106781186553));
#17693=DIRECTION('center_axis',(0.,-0.70710678118654,0.707106781186555));
#17694=DIRECTION('ref_axis',(1.,0.,0.));
#17695=DIRECTION('',(-1.,0.,0.));
#17696=DIRECTION('',(1.,0.,0.));
#17697=DIRECTION('center_axis',(0.,-1.,0.));
#17698=DIRECTION('ref_axis',(0.,0.,-1.));
#17699=DIRECTION('',(-1.,0.,0.));
#17700=DIRECTION('center_axis',(0.,-0.707106781186548,-0.707106781186548));
#17701=DIRECTION('ref_axis',(-1.,0.,0.));
#17702=DIRECTION('',(-1.,0.,0.));
#17703=DIRECTION('',(1.,0.,0.));
#17704=DIRECTION('center_axis',(0.,0.,-1.));
#17705=DIRECTION('ref_axis',(0.,1.,0.));
#17706=DIRECTION('',(1.,0.,0.));
#17707=DIRECTION('center_axis',(0.,-0.707106781186549,-0.707106781186546));
#17708=DIRECTION('ref_axis',(-1.,0.,0.));
#17709=DIRECTION('center_axis',(0.,-1.,0.));
#17710=DIRECTION('ref_axis',(0.,0.,-1.));
#17711=DIRECTION('center_axis',(0.,0.,1.));
#17712=DIRECTION('ref_axis',(0.,-1.,0.));
#17713=DIRECTION('',(1.,0.,0.));
#17714=DIRECTION('center_axis',(0.,-1.,0.));
#17715=DIRECTION('ref_axis',(0.,0.,-1.));
#17716=DIRECTION('',(1.,0.,0.));
#17717=DIRECTION('center_axis',(0.,0.,-1.));
#17718=DIRECTION('ref_axis',(0.,1.,0.));
#17719=DIRECTION('',(1.,0.,0.));
#17720=DIRECTION('center_axis',(0.,-1.,0.));
#17721=DIRECTION('ref_axis',(0.,0.,-1.));
#17722=DIRECTION('',(1.,0.,0.));
#17723=DIRECTION('center_axis',(0.,0.,1.));
#17724=DIRECTION('ref_axis',(0.,-1.,0.));
#17725=DIRECTION('',(1.,0.,0.));
#17726=DIRECTION('center_axis',(0.,-1.,0.));
#17727=DIRECTION('ref_axis',(0.,0.,-1.));
#17728=DIRECTION('axis',(0.,0.,1.));
#17729=DIRECTION('refdir',(1.,0.,0.));
#17730=DIRECTION('center_axis',(1.,0.,0.));
#17731=DIRECTION('ref_axis',(0.,0.,-1.));
#17732=DIRECTION('center_axis',(-1.,0.,0.));
#17733=DIRECTION('ref_axis',(0.,0.,-1.));
#17734=DIRECTION('',(0.70710678118654,-8.65956056235502E-17,0.707106781186555));
#17735=DIRECTION('center_axis',(1.,0.,0.));
#17736=DIRECTION('ref_axis',(0.,0.,-1.));
#17737=DIRECTION('center_axis',(1.,0.,0.));
#17738=DIRECTION('ref_axis',(0.,0.,-1.));
#17739=DIRECTION('',(0.,0.,1.));
#17740=DIRECTION('',(0.,-0.70710678118655,0.707106781186545));
#17741=DIRECTION('',(0.,1.,0.));
#17742=DIRECTION('',(0.,-0.707106781186547,-0.707106781186547));
#17743=DIRECTION('',(0.,0.,-1.));
#17744=DIRECTION('',(0.,0.707106781186547,-0.707106781186547));
#17745=DIRECTION('',(0.,-1.,0.));
#17746=DIRECTION('',(0.,0.923879532511291,0.38268343236508));
#17747=DIRECTION('',(0.,-0.707106781186547,-0.707106781186547));
#17748=DIRECTION('',(0.,0.,-1.));
#17749=DIRECTION('',(0.,-1.,0.));
#17750=DIRECTION('',(0.,0.,1.));
#17751=DIRECTION('',(0.,-0.707106781186548,0.707106781186547));
#17752=DIRECTION('',(0.,0.923879532511287,-0.38268343236509));
#17753=DIRECTION('',(0.,-1.,0.));
#17754=DIRECTION('',(0.,-1.,0.));
#17755=DIRECTION('',(0.,0.707106781186549,0.707106781186546));
#17756=DIRECTION('center_axis',(-1.,0.,0.));
#17757=DIRECTION('ref_axis',(0.,0.,-1.));
#17758=DIRECTION('',(-1.,0.,0.));
#17759=DIRECTION('center_axis',(-1.,0.,0.));
#17760=DIRECTION('ref_axis',(0.,0.,-1.));
#17761=DIRECTION('center_axis',(-1.,0.,0.));
#17762=DIRECTION('ref_axis',(0.,0.,-1.));
#17763=DIRECTION('center_axis',(1.,0.,0.));
#17764=DIRECTION('ref_axis',(0.,1.,0.));
#17765=DIRECTION('',(0.515038074910058,-0.85716730070211,-1.04972719113862E-16));
#17766=DIRECTION('center_axis',(-1.,0.,0.));
#17767=DIRECTION('ref_axis',(0.,0.,-1.));
#17768=DIRECTION('center_axis',(1.,0.,0.));
#17769=DIRECTION('ref_axis',(0.,0.,-1.));
#17770=DIRECTION('',(-0.707106781186548,8.65956056235493E-17,0.707106781186547));
#17771=DIRECTION('center_axis',(-1.,0.,0.));
#17772=DIRECTION('ref_axis',(0.,0.,-1.));
#17773=DIRECTION('center_axis',(1.,0.,0.));
#17774=DIRECTION('ref_axis',(0.,0.,-1.));
#17775=DIRECTION('',(0.,0.,-1.));
#17776=DIRECTION('',(0.,-0.707106781186549,-0.707106781186546));
#17777=DIRECTION('',(0.,1.,0.));
#17778=DIRECTION('',(0.,1.,0.));
#17779=DIRECTION('',(0.,-0.923879532511287,0.38268343236509));
#17780=DIRECTION('',(0.,0.707106781186548,-0.707106781186547));
#17781=DIRECTION('',(0.,0.,-1.));
#17782=DIRECTION('',(0.,1.,0.));
#17783=DIRECTION('',(0.,0.,1.));
#17784=DIRECTION('',(0.,0.707106781186547,0.707106781186547));
#17785=DIRECTION('',(0.,-0.923879532511291,-0.38268343236508));
#17786=DIRECTION('',(0.,1.,0.));
#17787=DIRECTION('',(0.,-0.707106781186547,0.707106781186547));
#17788=DIRECTION('',(0.,0.,1.));
#17789=DIRECTION('',(0.,0.707106781186547,0.707106781186547));
#17790=DIRECTION('',(0.,-1.,0.));
#17791=DIRECTION('',(0.,0.70710678118655,-0.707106781186545));
#17792=DIRECTION('center_axis',(1.,0.,0.));
#17793=DIRECTION('ref_axis',(0.,0.,-1.));
#17794=DIRECTION('',(1.,0.,0.));
#17795=DIRECTION('center_axis',(1.,0.,0.));
#17796=DIRECTION('ref_axis',(0.,0.,-1.));
#17797=DIRECTION('center_axis',(1.,0.,0.));
#17798=DIRECTION('ref_axis',(0.,0.,-1.));
#17799=DIRECTION('center_axis',(-1.,0.,0.));
#17800=DIRECTION('ref_axis',(0.,1.,0.));
#17801=DIRECTION('',(-0.515038074910058,-0.85716730070211,1.04972719113862E-16));
#17802=DIRECTION('center_axis',(0.,0.,-1.));
#17803=DIRECTION('ref_axis',(1.,0.,0.));
#17804=DIRECTION('center_axis',(0.,0.,1.));
#17805=DIRECTION('ref_axis',(1.,0.,0.));
#17806=DIRECTION('',(-0.707106781186542,8.65956056235487E-17,-0.707106781186553));
#17807=DIRECTION('center_axis',(0.,0.,-1.));
#17808=DIRECTION('ref_axis',(1.,0.,0.));
#17809=DIRECTION('center_axis',(0.,0.,-1.));
#17810=DIRECTION('ref_axis',(0.,1.,0.));
#17811=DIRECTION('',(1.,0.,0.));
#17812=DIRECTION('',(-1.,0.,0.));
#17813=DIRECTION('center_axis',(0.,0.,-1.));
#17814=DIRECTION('ref_axis',(1.,0.,0.));
#17815=DIRECTION('center_axis',(0.,0.,-1.));
#17816=DIRECTION('ref_axis',(1.,0.,0.));
#17817=DIRECTION('center_axis',(0.,0.,1.));
#17818=DIRECTION('ref_axis',(1.,0.,0.));
#17819=DIRECTION('',(0.,0.,1.));
#17820=DIRECTION('center_axis',(0.,0.,-1.));
#17821=DIRECTION('ref_axis',(1.,0.,0.));
#17822=DIRECTION('',(0.,0.,-1.));
#17823=DIRECTION('center_axis',(0.,-0.707106781186547,-0.707106781186548));
#17824=DIRECTION('ref_axis',(0.,0.707106781186548,-0.707106781186547));
#17825=DIRECTION('center_axis',(0.,0.,1.));
#17826=DIRECTION('ref_axis',(1.,0.,0.));
#17827=DIRECTION('center_axis',(0.,-0.707106781186547,-0.707106781186548));
#17828=DIRECTION('ref_axis',(0.,0.707106781186548,-0.707106781186547));
#17829=DIRECTION('',(0.,0.,1.));
#17830=DIRECTION('center_axis',(0.,0.,-1.));
#17831=DIRECTION('ref_axis',(1.,0.,0.));
#17832=DIRECTION('',(0.,0.,-1.));
#17833=DIRECTION('center_axis',(0.,0.707106781186548,-0.707106781186548));
#17834=DIRECTION('ref_axis',(0.,0.707106781186547,0.707106781186547));
#17835=DIRECTION('center_axis',(0.,0.,1.));
#17836=DIRECTION('ref_axis',(1.,0.,0.));
#17837=DIRECTION('center_axis',(0.,0.707106781186548,-0.707106781186548));
#17838=DIRECTION('ref_axis',(0.,0.707106781186547,0.707106781186547));
#17839=DIRECTION('',(0.,0.,1.));
#17840=DIRECTION('center_axis',(0.,0.,-1.));
#17841=DIRECTION('ref_axis',(1.,0.,0.));
#17842=DIRECTION('center_axis',(0.,0.,-1.));
#17843=DIRECTION('ref_axis',(1.,0.,0.));
#17844=DIRECTION('center_axis',(0.,0.,1.));
#17845=DIRECTION('ref_axis',(1.,0.,0.));
#17846=DIRECTION('',(-0.707106781186542,8.65956056235487E-17,-0.707106781186553));
#17847=DIRECTION('center_axis',(0.,0.,1.));
#17848=DIRECTION('ref_axis',(1.,0.,0.));
#17849=DIRECTION('',(0.,0.,1.));
#17850=DIRECTION('center_axis',(0.,0.,-1.));
#17851=DIRECTION('ref_axis',(1.,0.,0.));
#17852=DIRECTION('',(0.,0.,-1.));
#17853=DIRECTION('center_axis',(0.,-0.707106781186547,-0.707106781186548));
#17854=DIRECTION('ref_axis',(0.,0.707106781186548,-0.707106781186547));
#17855=DIRECTION('center_axis',(0.,0.,1.));
#17856=DIRECTION('ref_axis',(1.,0.,0.));
#17857=DIRECTION('center_axis',(0.,-0.707106781186547,-0.707106781186548));
#17858=DIRECTION('ref_axis',(0.,0.707106781186548,-0.707106781186547));
#17859=DIRECTION('',(0.,0.,1.));
#17860=DIRECTION('center_axis',(0.,0.,-1.));
#17861=DIRECTION('ref_axis',(1.,0.,0.));
#17862=DIRECTION('',(0.,0.,-1.));
#17863=DIRECTION('center_axis',(0.,0.707106781186548,-0.707106781186548));
#17864=DIRECTION('ref_axis',(0.,0.707106781186547,0.707106781186547));
#17865=DIRECTION('center_axis',(0.,0.,1.));
#17866=DIRECTION('ref_axis',(1.,0.,0.));
#17867=DIRECTION('center_axis',(0.,0.707106781186548,-0.707106781186548));
#17868=DIRECTION('ref_axis',(0.,0.707106781186547,0.707106781186547));
#17869=DIRECTION('',(0.,0.,1.));
#17870=DIRECTION('center_axis',(0.,0.,-1.));
#17871=DIRECTION('ref_axis',(1.,0.,0.));
#17872=DIRECTION('center_axis',(0.,0.,-1.));
#17873=DIRECTION('ref_axis',(1.,0.,0.));
#17874=DIRECTION('center_axis',(0.,0.,1.));
#17875=DIRECTION('ref_axis',(1.,0.,0.));
#17876=DIRECTION('',(-0.707106781186553,8.659560562355E-17,-0.707106781186542));
#17877=DIRECTION('center_axis',(0.,0.,1.));
#17878=DIRECTION('ref_axis',(1.,0.,0.));
#17879=DIRECTION('',(0.,0.,1.));
#17880=DIRECTION('center_axis',(0.,0.,-1.));
#17881=DIRECTION('ref_axis',(1.,0.,0.));
#17882=DIRECTION('',(0.,0.,-1.));
#17883=DIRECTION('center_axis',(0.,-0.707106781186547,-0.707106781186548));
#17884=DIRECTION('ref_axis',(0.,0.707106781186548,-0.707106781186547));
#17885=DIRECTION('center_axis',(0.,0.,1.));
#17886=DIRECTION('ref_axis',(1.,0.,0.));
#17887=DIRECTION('center_axis',(0.,-0.707106781186547,-0.707106781186548));
#17888=DIRECTION('ref_axis',(0.,0.707106781186548,-0.707106781186547));
#17889=DIRECTION('',(0.,0.,1.));
#17890=DIRECTION('center_axis',(0.,0.,-1.));
#17891=DIRECTION('ref_axis',(1.,0.,0.));
#17892=DIRECTION('',(0.,0.,-1.));
#17893=DIRECTION('center_axis',(0.,0.707106781186548,-0.707106781186548));
#17894=DIRECTION('ref_axis',(0.,0.707106781186548,0.707106781186548));
#17895=DIRECTION('center_axis',(0.,0.,1.));
#17896=DIRECTION('ref_axis',(1.,0.,0.));
#17897=DIRECTION('center_axis',(0.,0.707106781186548,-0.707106781186548));
#17898=DIRECTION('ref_axis',(0.,0.707106781186548,0.707106781186548));
#17899=DIRECTION('',(0.,0.,1.));
#17900=DIRECTION('center_axis',(0.,0.,-1.));
#17901=DIRECTION('ref_axis',(1.,0.,0.));
#17902=DIRECTION('center_axis',(0.,0.,1.));
#17903=DIRECTION('ref_axis',(1.,0.,0.));
#17904=DIRECTION('',(-1.,0.,0.));
#17905=DIRECTION('center_axis',(0.,0.,1.));
#17906=DIRECTION('ref_axis',(1.,0.,0.));
#17907=DIRECTION('',(1.,0.,0.));
#17908=DIRECTION('center_axis',(0.,0.,1.));
#17909=DIRECTION('ref_axis',(1.,0.,0.));
#17910=DIRECTION('',(-1.,0.,0.));
#17911=DIRECTION('center_axis',(0.,0.,1.));
#17912=DIRECTION('ref_axis',(1.,0.,0.));
#17913=DIRECTION('',(1.,0.,0.));
#17914=DIRECTION('center_axis',(0.,0.,1.));
#17915=DIRECTION('ref_axis',(1.,0.,0.));
#17916=DIRECTION('',(-1.,0.,0.));
#17917=DIRECTION('center_axis',(0.,0.,1.));
#17918=DIRECTION('ref_axis',(1.,0.,0.));
#17919=DIRECTION('',(1.,0.,0.));
#17920=DIRECTION('center_axis',(0.,-0.707106781186548,0.707106781186548));
#17921=DIRECTION('ref_axis',(0.,-0.707106781186548,-0.707106781186548));
#17922=DIRECTION('',(1.,0.,0.));
#17923=DIRECTION('',(1.,0.,0.));
#17924=DIRECTION('',(1.,0.,0.));
#17925=DIRECTION('',(1.,0.,0.));
#17926=DIRECTION('',(1.,0.,0.));
#17927=DIRECTION('center_axis',(0.,-1.,0.));
#17928=DIRECTION('ref_axis',(0.,0.,-1.));
#17929=DIRECTION('',(1.,0.,0.));
#17930=DIRECTION('center_axis',(0.,-1.,0.));
#17931=DIRECTION('ref_axis',(0.,0.,-1.));
#17932=DIRECTION('',(1.,0.,0.));
#17933=DIRECTION('center_axis',(0.,-1.,0.));
#17934=DIRECTION('ref_axis',(0.,0.,-1.));
#17935=DIRECTION('',(1.,0.,0.));
#17936=DIRECTION('center_axis',(0.,0.,1.));
#17937=DIRECTION('ref_axis',(0.,-1.,0.));
#17938=DIRECTION('',(1.,0.,0.));
#17939=DIRECTION('center_axis',(0.,0.,1.));
#17940=DIRECTION('ref_axis',(0.,-1.,0.));
#17941=DIRECTION('',(1.,0.,0.));
#17942=DIRECTION('center_axis',(0.,0.,1.));
#17943=DIRECTION('ref_axis',(0.,-1.,0.));
#17944=DIRECTION('',(1.,0.,0.));
#17945=DIRECTION('center_axis',(0.,1.,0.));
#17946=DIRECTION('ref_axis',(0.,0.,1.));
#17947=DIRECTION('',(1.,0.,0.));
#17948=DIRECTION('center_axis',(0.,1.,0.));
#17949=DIRECTION('ref_axis',(0.,0.,1.));
#17950=DIRECTION('',(1.,0.,0.));
#17951=DIRECTION('center_axis',(0.,1.,0.));
#17952=DIRECTION('ref_axis',(0.,0.,1.));
#17953=DIRECTION('',(1.,0.,0.));
#17954=DIRECTION('center_axis',(0.707106781186534,-0.707106781186561,0.));
#17955=DIRECTION('ref_axis',(0.,0.,-1.));
#17956=DIRECTION('',(0.577350269189641,0.57735026918962,-0.577350269189616));
#17957=DIRECTION('',(-0.577350269189641,-0.57735026918962,-0.577350269189617));
#17958=DIRECTION('',(0.,0.,-1.));
#17959=DIRECTION('center_axis',(0.,-1.,0.));
#17960=DIRECTION('ref_axis',(0.,0.,-1.));
#17961=DIRECTION('',(1.,0.,0.));
#17962=DIRECTION('',(0.,0.,1.));
#17963=DIRECTION('',(-1.,0.,0.));
#17964=DIRECTION('center_axis',(0.,-0.707106781186546,0.707106781186549));
#17965=DIRECTION('ref_axis',(1.,0.,0.));
#17966=DIRECTION('',(-1.,0.,0.));
#17967=DIRECTION('',(-0.577350269189627,0.577350269189627,0.577350269189624));
#17968=DIRECTION('center_axis',(0.707106781186532,0.707106781186563,0.));
#17969=DIRECTION('ref_axis',(0.,0.,-1.));
#17970=DIRECTION('',(0.577350269189643,-0.577350269189617,0.577350269189617));
#17971=DIRECTION('',(-0.577350269189643,0.577350269189617,0.577350269189617));
#17972=DIRECTION('',(0.,0.,1.));
#17973=DIRECTION('center_axis',(0.,0.707106781186548,0.707106781186548));
#17974=DIRECTION('ref_axis',(1.,0.,0.));
#17975=DIRECTION('',(-1.,0.,0.));
#17976=DIRECTION('',(0.577350269189629,0.577350269189624,-0.577350269189624));
#17977=DIRECTION('',(1.,0.,0.));
#17978=DIRECTION('center_axis',(0.,1.,0.));
#17979=DIRECTION('ref_axis',(0.,0.,1.));
#17980=DIRECTION('',(1.,0.,0.));
#17981=DIRECTION('',(0.,0.,-1.));
#17982=DIRECTION('center_axis',(-0.707106781186548,-0.707106781186548,0.));
#17983=DIRECTION('ref_axis',(0.,0.,1.));
#17984=DIRECTION('',(0.577350269189627,-0.577350269189627,0.577350269189623));
#17985=DIRECTION('center_axis',(-0.707106781186545,0.70710678118655,0.));
#17986=DIRECTION('ref_axis',(0.,0.,1.));
#17987=DIRECTION('',(-0.577350269189629,-0.577350269189624,-0.577350269189624));
#17988=DIRECTION('center_axis',(0.,-0.38268343236508,0.923879532511291));
#17989=DIRECTION('ref_axis',(1.,0.,0.));
#17990=DIRECTION('',(-1.,0.,0.));
#17991=DIRECTION('center_axis',(0.,0.,1.));
#17992=DIRECTION('ref_axis',(0.,-1.,0.));
#17993=DIRECTION('center_axis',(0.,0.38268343236509,0.923879532511287));
#17994=DIRECTION('ref_axis',(1.,0.,0.));
#17995=DIRECTION('',(-1.,0.,0.));
#17996=DIRECTION('',(1.,0.,0.));
#17997=DIRECTION('center_axis',(0.,0.707106781186547,0.707106781186548));
#17998=DIRECTION('ref_axis',(0.,-0.707106781186548,0.707106781186547));
#17999=DIRECTION('',(1.,0.,0.));
#18000=DIRECTION('center_axis',(0.,-0.707106781186545,-0.70710678118655));
#18001=DIRECTION('ref_axis',(-1.,0.,0.));
#18002=DIRECTION('center_axis',(0.,0.707106781186548,-0.707106781186548));
#18003=DIRECTION('ref_axis',(-1.,0.,0.));
#18004=DIRECTION('center_axis',(0.,0.,1.));
#18005=DIRECTION('ref_axis',(0.,-1.,0.));
#18006=DIRECTION('center_axis',(0.,1.,0.));
#18007=DIRECTION('ref_axis',(0.,0.,1.));
#18008=DIRECTION('',(1.,0.,0.));
#18009=DIRECTION('center_axis',(0.,0.,1.));
#18010=DIRECTION('ref_axis',(0.,-1.,0.));
#18011=DIRECTION('',(1.,0.,0.));
#18012=DIRECTION('center_axis',(0.,-1.,0.));
#18013=DIRECTION('ref_axis',(0.,0.,-1.));
#18014=DIRECTION('axis',(0.,0.,1.));
#18015=DIRECTION('refdir',(1.,0.,0.));
#18016=DIRECTION('center_axis',(1.,0.,0.));
#18017=DIRECTION('ref_axis',(0.,0.,-1.));
#18018=DIRECTION('center_axis',(-1.,0.,0.));
#18019=DIRECTION('ref_axis',(0.,0.,-1.));
#18020=DIRECTION('',(0.70710678118654,-8.65956056235502E-17,0.707106781186555));
#18021=DIRECTION('center_axis',(1.,0.,0.));
#18022=DIRECTION('ref_axis',(0.,0.,-1.));
#18023=DIRECTION('center_axis',(1.,0.,0.));
#18024=DIRECTION('ref_axis',(0.,0.,-1.));
#18025=DIRECTION('center_axis',(1.,0.,0.));
#18026=DIRECTION('ref_axis',(0.,0.,-1.));
#18027=DIRECTION('',(0.,0.,1.));
#18028=DIRECTION('',(0.,-0.707106781186549,0.707106781186546));
#18029=DIRECTION('',(0.,1.,0.));
#18030=DIRECTION('',(0.,-0.923879532511287,-0.38268343236509));
#18031=DIRECTION('',(0.,0.707106781186547,0.707106781186548));
#18032=DIRECTION('',(0.,0.,1.));
#18033=DIRECTION('',(0.,1.,0.));
#18034=DIRECTION('',(0.,0.,-1.));
#18035=DIRECTION('',(0.,0.707106781186547,-0.707106781186548));
#18036=DIRECTION('',(0.,-0.923879532511287,0.38268343236509));
#18037=DIRECTION('',(0.,1.,0.));
#18038=DIRECTION('',(0.,1.,0.));
#18039=DIRECTION('',(0.,-0.707106781186547,-0.707106781186547));
#18040=DIRECTION('',(0.,0.,-1.));
#18041=DIRECTION('',(0.,0.707106781186547,-0.707106781186547));
#18042=DIRECTION('',(0.,-1.,0.));
#18043=DIRECTION('',(0.,0.70710678118655,0.707106781186545));
#18044=DIRECTION('center_axis',(-1.,0.,0.));
#18045=DIRECTION('ref_axis',(0.,0.,-1.));
#18046=DIRECTION('',(-1.,0.,0.));
#18047=DIRECTION('center_axis',(-1.,0.,0.));
#18048=DIRECTION('ref_axis',(0.,0.,-1.));
#18049=DIRECTION('center_axis',(-1.,0.,0.));
#18050=DIRECTION('ref_axis',(0.,0.,-1.));
#18051=DIRECTION('center_axis',(1.,0.,0.));
#18052=DIRECTION('ref_axis',(0.,1.,0.));
#18053=DIRECTION('',(0.515038074910058,-0.85716730070211,-1.04972719113862E-16));
#18054=DIRECTION('center_axis',(-1.,0.,0.));
#18055=DIRECTION('ref_axis',(0.,0.,-1.));
#18056=DIRECTION('center_axis',(1.,0.,0.));
#18057=DIRECTION('ref_axis',(0.,0.,-1.));
#18058=DIRECTION('',(-0.707106781186548,8.65956056235493E-17,0.707106781186547));
#18059=DIRECTION('center_axis',(-1.,0.,0.));
#18060=DIRECTION('ref_axis',(0.,0.,-1.));
#18061=DIRECTION('center_axis',(-1.,0.,0.));
#18062=DIRECTION('ref_axis',(0.,0.,-1.));
#18063=DIRECTION('center_axis',(1.,0.,0.));
#18064=DIRECTION('ref_axis',(0.,0.,-1.));
#18065=DIRECTION('',(0.,0.,1.));
#18066=DIRECTION('',(0.,0.707106781186547,0.707106781186547));
#18067=DIRECTION('',(0.,1.,0.));
#18068=DIRECTION('',(0.,1.,0.));
#18069=DIRECTION('',(0.,0.923879532511287,-0.38268343236509));
#18070=DIRECTION('',(0.,0.707106781186547,-0.707106781186548));
#18071=DIRECTION('',(0.,0.,-1.));
#18072=DIRECTION('',(0.,1.,0.));
#18073=DIRECTION('',(0.,0.,1.));
#18074=DIRECTION('',(0.,0.707106781186547,0.707106781186548));
#18075=DIRECTION('',(0.,0.923879532511287,0.38268343236509));
#18076=DIRECTION('',(0.,1.,0.));
#18077=DIRECTION('',(0.,0.707106781186549,-0.707106781186546));
#18078=DIRECTION('',(0.,0.,-1.));
#18079=DIRECTION('',(0.,-0.70710678118655,-0.707106781186545));
#18080=DIRECTION('',(0.,-1.,0.));
#18081=DIRECTION('',(0.,-0.707106781186547,0.707106781186547));
#18082=DIRECTION('center_axis',(1.,0.,0.));
#18083=DIRECTION('ref_axis',(0.,0.,-1.));
#18084=DIRECTION('',(1.,0.,0.));
#18085=DIRECTION('center_axis',(1.,0.,0.));
#18086=DIRECTION('ref_axis',(0.,0.,-1.));
#18087=DIRECTION('center_axis',(1.,0.,0.));
#18088=DIRECTION('ref_axis',(0.,0.,-1.));
#18089=DIRECTION('center_axis',(-1.,0.,0.));
#18090=DIRECTION('ref_axis',(0.,1.,0.));
#18091=DIRECTION('',(-0.515038074910058,-0.85716730070211,1.04972719113862E-16));
#18092=DIRECTION('center_axis',(0.,0.,1.));
#18093=DIRECTION('ref_axis',(1.,0.,0.));
#18094=DIRECTION('center_axis',(0.,0.,-1.));
#18095=DIRECTION('ref_axis',(1.,0.,0.));
#18096=DIRECTION('',(-0.707106781186564,-8.65956056235513E-17,0.707106781186531));
#18097=DIRECTION('center_axis',(0.,0.,1.));
#18098=DIRECTION('ref_axis',(1.,0.,0.));
#18099=DIRECTION('center_axis',(0.,0.,1.));
#18100=DIRECTION('ref_axis',(0.,-1.,0.));
#18101=DIRECTION('',(-1.,0.,0.));
#18102=DIRECTION('',(1.,0.,0.));
#18103=DIRECTION('center_axis',(0.,0.,1.));
#18104=DIRECTION('ref_axis',(1.,0.,0.));
#18105=DIRECTION('center_axis',(0.,0.,1.));
#18106=DIRECTION('ref_axis',(1.,0.,0.));
#18107=DIRECTION('center_axis',(0.,0.,1.));
#18108=DIRECTION('ref_axis',(1.,0.,0.));
#18109=DIRECTION('center_axis',(0.,0.,-1.));
#18110=DIRECTION('ref_axis',(1.,0.,0.));
#18111=DIRECTION('',(0.,0.,-1.));
#18112=DIRECTION('center_axis',(0.,0.,1.));
#18113=DIRECTION('ref_axis',(1.,0.,0.));
#18114=DIRECTION('',(0.,0.,1.));
#18115=DIRECTION('center_axis',(0.,0.707106781186548,0.707106781186547));
#18116=DIRECTION('ref_axis',(0.,-0.707106781186547,0.707106781186548));
#18117=DIRECTION('center_axis',(0.,0.,-1.));
#18118=DIRECTION('ref_axis',(1.,0.,0.));
#18119=DIRECTION('center_axis',(0.,0.707106781186548,0.707106781186547));
#18120=DIRECTION('ref_axis',(0.,-0.707106781186547,0.707106781186548));
#18121=DIRECTION('',(0.,0.,-1.));
#18122=DIRECTION('center_axis',(0.,0.,1.));
#18123=DIRECTION('ref_axis',(1.,0.,0.));
#18124=DIRECTION('',(0.,0.,1.));
#18125=DIRECTION('center_axis',(0.,-0.707106781186548,0.707106781186547));
#18126=DIRECTION('ref_axis',(0.,-0.707106781186547,-0.707106781186548));
#18127=DIRECTION('center_axis',(0.,0.,-1.));
#18128=DIRECTION('ref_axis',(1.,0.,0.));
#18129=DIRECTION('center_axis',(0.,-0.707106781186548,0.707106781186547));
#18130=DIRECTION('ref_axis',(0.,-0.707106781186547,-0.707106781186548));
#18131=DIRECTION('',(0.,0.,-1.));
#18132=DIRECTION('center_axis',(0.,0.,1.));
#18133=DIRECTION('ref_axis',(1.,0.,0.));
#18134=DIRECTION('center_axis',(0.,0.,1.));
#18135=DIRECTION('ref_axis',(1.,0.,0.));
#18136=DIRECTION('center_axis',(0.,0.,-1.));
#18137=DIRECTION('ref_axis',(1.,0.,0.));
#18138=DIRECTION('',(-0.707106781186547,-8.65956056235493E-17,0.707106781186548));
#18139=DIRECTION('center_axis',(0.,0.,-1.));
#18140=DIRECTION('ref_axis',(1.,0.,0.));
#18141=DIRECTION('',(0.,0.,-1.));
#18142=DIRECTION('center_axis',(0.,0.,1.));
#18143=DIRECTION('ref_axis',(1.,0.,0.));
#18144=DIRECTION('',(0.,0.,1.));
#18145=DIRECTION('center_axis',(0.,0.707106781186548,0.707106781186547));
#18146=DIRECTION('ref_axis',(0.,-0.707106781186547,0.707106781186548));
#18147=DIRECTION('center_axis',(0.,0.,-1.));
#18148=DIRECTION('ref_axis',(1.,0.,0.));
#18149=DIRECTION('center_axis',(0.,0.707106781186548,0.707106781186547));
#18150=DIRECTION('ref_axis',(0.,-0.707106781186547,0.707106781186548));
#18151=DIRECTION('',(0.,0.,-1.));
#18152=DIRECTION('center_axis',(0.,0.,1.));
#18153=DIRECTION('ref_axis',(1.,0.,0.));
#18154=DIRECTION('',(0.,0.,1.));
#18155=DIRECTION('center_axis',(0.,-0.707106781186548,0.707106781186547));
#18156=DIRECTION('ref_axis',(0.,-0.707106781186547,-0.707106781186548));
#18157=DIRECTION('center_axis',(0.,0.,-1.));
#18158=DIRECTION('ref_axis',(1.,0.,0.));
#18159=DIRECTION('center_axis',(0.,-0.707106781186548,0.707106781186547));
#18160=DIRECTION('ref_axis',(0.,-0.707106781186547,-0.707106781186548));
#18161=DIRECTION('',(0.,0.,-1.));
#18162=DIRECTION('center_axis',(0.,0.,1.));
#18163=DIRECTION('ref_axis',(1.,0.,0.));
#18164=DIRECTION('center_axis',(0.,0.,1.));
#18165=DIRECTION('ref_axis',(1.,0.,0.));
#18166=DIRECTION('center_axis',(0.,0.,-1.));
#18167=DIRECTION('ref_axis',(1.,0.,0.));
#18168=DIRECTION('',(-0.707106781186542,-8.65956056235487E-17,0.707106781186553));
#18169=DIRECTION('center_axis',(0.,0.,-1.));
#18170=DIRECTION('ref_axis',(1.,0.,0.));
#18171=DIRECTION('',(0.,0.,-1.));
#18172=DIRECTION('center_axis',(0.,0.,1.));
#18173=DIRECTION('ref_axis',(1.,0.,0.));
#18174=DIRECTION('',(0.,0.,1.));
#18175=DIRECTION('center_axis',(0.,0.707106781186548,0.707106781186547));
#18176=DIRECTION('ref_axis',(0.,-0.707106781186547,0.707106781186548));
#18177=DIRECTION('center_axis',(0.,0.,-1.));
#18178=DIRECTION('ref_axis',(1.,0.,0.));
#18179=DIRECTION('center_axis',(0.,0.707106781186548,0.707106781186547));
#18180=DIRECTION('ref_axis',(0.,-0.707106781186547,0.707106781186548));
#18181=DIRECTION('',(0.,0.,-1.));
#18182=DIRECTION('center_axis',(0.,0.,1.));
#18183=DIRECTION('ref_axis',(1.,0.,0.));
#18184=DIRECTION('',(0.,0.,1.));
#18185=DIRECTION('center_axis',(0.,-0.707106781186548,0.707106781186547));
#18186=DIRECTION('ref_axis',(0.,-0.707106781186547,-0.707106781186548));
#18187=DIRECTION('center_axis',(0.,0.,-1.));
#18188=DIRECTION('ref_axis',(1.,0.,0.));
#18189=DIRECTION('center_axis',(0.,-0.707106781186548,0.707106781186547));
#18190=DIRECTION('ref_axis',(0.,-0.707106781186547,-0.707106781186548));
#18191=DIRECTION('',(0.,0.,-1.));
#18192=DIRECTION('center_axis',(0.,0.,1.));
#18193=DIRECTION('ref_axis',(1.,0.,0.));
#18194=DIRECTION('center_axis',(0.,0.,1.));
#18195=DIRECTION('ref_axis',(1.,0.,0.));
#18196=DIRECTION('center_axis',(0.,0.,-1.));
#18197=DIRECTION('ref_axis',(1.,0.,0.));
#18198=DIRECTION('',(-0.707106781186542,-8.65956056235487E-17,0.707106781186553));
#18199=DIRECTION('center_axis',(0.,0.,-1.));
#18200=DIRECTION('ref_axis',(1.,0.,0.));
#18201=DIRECTION('',(0.,0.,-1.));
#18202=DIRECTION('center_axis',(0.,0.,1.));
#18203=DIRECTION('ref_axis',(1.,0.,0.));
#18204=DIRECTION('',(0.,0.,1.));
#18205=DIRECTION('center_axis',(0.,0.707106781186548,0.707106781186547));
#18206=DIRECTION('ref_axis',(0.,-0.707106781186547,0.707106781186548));
#18207=DIRECTION('center_axis',(0.,0.,-1.));
#18208=DIRECTION('ref_axis',(1.,0.,0.));
#18209=DIRECTION('center_axis',(0.,0.707106781186548,0.707106781186547));
#18210=DIRECTION('ref_axis',(0.,-0.707106781186547,0.707106781186548));
#18211=DIRECTION('',(0.,0.,-1.));
#18212=DIRECTION('center_axis',(0.,0.,1.));
#18213=DIRECTION('ref_axis',(1.,0.,0.));
#18214=DIRECTION('',(0.,0.,1.));
#18215=DIRECTION('center_axis',(0.,-0.707106781186548,0.707106781186547));
#18216=DIRECTION('ref_axis',(0.,-0.707106781186547,-0.707106781186548));
#18217=DIRECTION('center_axis',(0.,0.,-1.));
#18218=DIRECTION('ref_axis',(1.,0.,0.));
#18219=DIRECTION('center_axis',(0.,-0.707106781186548,0.707106781186547));
#18220=DIRECTION('ref_axis',(0.,-0.707106781186547,-0.707106781186548));
#18221=DIRECTION('',(0.,0.,-1.));
#18222=DIRECTION('center_axis',(0.,0.,1.));
#18223=DIRECTION('ref_axis',(1.,0.,0.));
#18224=DIRECTION('center_axis',(0.,0.,1.));
#18225=DIRECTION('ref_axis',(1.,0.,0.));
#18226=DIRECTION('',(-1.,0.,0.));
#18227=DIRECTION('center_axis',(0.,0.,1.));
#18228=DIRECTION('ref_axis',(1.,0.,0.));
#18229=DIRECTION('',(1.,0.,0.));
#18230=DIRECTION('center_axis',(0.,0.,1.));
#18231=DIRECTION('ref_axis',(1.,0.,0.));
#18232=DIRECTION('',(-1.,0.,0.));
#18233=DIRECTION('center_axis',(0.,0.,1.));
#18234=DIRECTION('ref_axis',(1.,0.,0.));
#18235=DIRECTION('',(1.,0.,0.));
#18236=DIRECTION('center_axis',(0.,0.,1.));
#18237=DIRECTION('ref_axis',(1.,0.,0.));
#18238=DIRECTION('',(-1.,0.,0.));
#18239=DIRECTION('center_axis',(0.,0.,1.));
#18240=DIRECTION('ref_axis',(1.,0.,0.));
#18241=DIRECTION('',(1.,0.,0.));
#18242=DIRECTION('center_axis',(0.,0.,1.));
#18243=DIRECTION('ref_axis',(1.,0.,0.));
#18244=DIRECTION('',(-1.,0.,0.));
#18245=DIRECTION('center_axis',(0.,0.,1.));
#18246=DIRECTION('ref_axis',(1.,0.,0.));
#18247=DIRECTION('',(1.,0.,0.));
#18248=DIRECTION('center_axis',(0.,0.707106781186548,-0.707106781186547));
#18249=DIRECTION('ref_axis',(0.,0.707106781186547,0.707106781186548));
#18250=DIRECTION('',(1.,0.,0.));
#18251=DIRECTION('',(1.,0.,0.));
#18252=DIRECTION('',(1.,0.,0.));
#18253=DIRECTION('',(1.,0.,0.));
#18254=DIRECTION('',(1.,0.,0.));
#18255=DIRECTION('',(1.,0.,0.));
#18256=DIRECTION('center_axis',(0.,1.,0.));
#18257=DIRECTION('ref_axis',(0.,0.,1.));
#18258=DIRECTION('',(1.,0.,0.));
#18259=DIRECTION('center_axis',(0.,1.,0.));
#18260=DIRECTION('ref_axis',(0.,0.,1.));
#18261=DIRECTION('',(1.,0.,0.));
#18262=DIRECTION('center_axis',(0.,1.,0.));
#18263=DIRECTION('ref_axis',(0.,0.,1.));
#18264=DIRECTION('',(1.,0.,0.));
#18265=DIRECTION('center_axis',(0.,1.,0.));
#18266=DIRECTION('ref_axis',(0.,0.,1.));
#18267=DIRECTION('',(1.,0.,0.));
#18268=DIRECTION('center_axis',(0.,0.,-1.));
#18269=DIRECTION('ref_axis',(0.,1.,0.));
#18270=DIRECTION('',(1.,0.,0.));
#18271=DIRECTION('center_axis',(0.,0.,-1.));
#18272=DIRECTION('ref_axis',(0.,1.,0.));
#18273=DIRECTION('',(1.,0.,0.));
#18274=DIRECTION('center_axis',(0.,0.,-1.));
#18275=DIRECTION('ref_axis',(0.,1.,0.));
#18276=DIRECTION('',(1.,0.,0.));
#18277=DIRECTION('center_axis',(0.,0.,-1.));
#18278=DIRECTION('ref_axis',(0.,1.,0.));
#18279=DIRECTION('',(1.,0.,0.));
#18280=DIRECTION('center_axis',(0.,-1.,0.));
#18281=DIRECTION('ref_axis',(0.,0.,-1.));
#18282=DIRECTION('',(1.,0.,0.));
#18283=DIRECTION('center_axis',(0.,-1.,0.));
#18284=DIRECTION('ref_axis',(0.,0.,-1.));
#18285=DIRECTION('',(1.,0.,0.));
#18286=DIRECTION('center_axis',(0.,-1.,0.));
#18287=DIRECTION('ref_axis',(0.,0.,-1.));
#18288=DIRECTION('',(1.,0.,0.));
#18289=DIRECTION('center_axis',(0.,-1.,0.));
#18290=DIRECTION('ref_axis',(0.,0.,-1.));
#18291=DIRECTION('',(1.,0.,0.));
#18292=DIRECTION('center_axis',(0.707106781186534,-0.707106781186561,0.));
#18293=DIRECTION('ref_axis',(0.,0.,-1.));
#18294=DIRECTION('',(0.577350269189641,0.57735026918962,-0.577350269189617));
#18295=DIRECTION('',(-0.577350269189641,-0.57735026918962,-0.577350269189616));
#18296=DIRECTION('',(0.,0.,-1.));
#18297=DIRECTION('center_axis',(0.,-0.707106781186545,0.70710678118655));
#18298=DIRECTION('ref_axis',(1.,0.,0.));
#18299=DIRECTION('',(-0.577350269189628,0.577350269189626,0.577350269189623));
#18300=DIRECTION('',(1.,0.,0.));
#18301=DIRECTION('center_axis',(0.707106781186532,0.707106781186563,0.));
#18302=DIRECTION('ref_axis',(0.,0.,-1.));
#18303=DIRECTION('',(0.577350269189643,-0.577350269189617,0.577350269189617));
#18304=DIRECTION('',(-0.577350269189643,0.577350269189617,0.577350269189617));
#18305=DIRECTION('',(0.,0.,1.));
#18306=DIRECTION('center_axis',(0.,0.707106781186548,0.707106781186548));
#18307=DIRECTION('ref_axis',(1.,0.,0.));
#18308=DIRECTION('',(-1.,0.,0.));
#18309=DIRECTION('',(0.577350269189629,0.577350269189624,-0.577350269189624));
#18310=DIRECTION('center_axis',(-0.707106781186545,0.70710678118655,0.));
#18311=DIRECTION('ref_axis',(0.,0.,1.));
#18312=DIRECTION('',(0.,0.,-1.));
#18313=DIRECTION('',(-0.577350269189629,-0.577350269189624,-0.577350269189624));
#18314=DIRECTION('center_axis',(-0.707106781186546,-0.707106781186549,0.));
#18315=DIRECTION('ref_axis',(0.,0.,1.));
#18316=DIRECTION('',(0.577350269189628,-0.577350269189626,0.577350269189623));
#18317=DIRECTION('',(0.,0.,1.));
#18318=DIRECTION('center_axis',(0.,0.38268343236509,-0.923879532511287));
#18319=DIRECTION('ref_axis',(-1.,0.,0.));
#18320=DIRECTION('',(-1.,0.,0.));
#18321=DIRECTION('center_axis',(0.,0.,-1.));
#18322=DIRECTION('ref_axis',(0.,1.,0.));
#18323=DIRECTION('',(1.,0.,0.));
#18324=DIRECTION('center_axis',(0.,-0.38268343236509,-0.923879532511287));
#18325=DIRECTION('ref_axis',(-1.,0.,0.));
#18326=DIRECTION('',(-1.,0.,0.));
#18327=DIRECTION('',(1.,0.,0.));
#18328=DIRECTION('center_axis',(0.,-0.707106781186548,-0.707106781186547));
#18329=DIRECTION('ref_axis',(0.,0.707106781186547,-0.707106781186548));
#18330=DIRECTION('',(1.,0.,0.));
#18331=DIRECTION('center_axis',(0.,-1.,0.));
#18332=DIRECTION('ref_axis',(0.,0.,-1.));
#18333=DIRECTION('',(-1.,0.,0.));
#18334=DIRECTION('center_axis',(0.,-0.707106781186546,-0.707106781186549));
#18335=DIRECTION('ref_axis',(-1.,0.,0.));
#18336=DIRECTION('center_axis',(0.,0.707106781186548,-0.707106781186548));
#18337=DIRECTION('ref_axis',(-1.,0.,0.));
#18338=DIRECTION('',(-1.,0.,0.));
#18339=DIRECTION('',(1.,0.,0.));
#18340=DIRECTION('center_axis',(0.,0.,-1.));
#18341=DIRECTION('ref_axis',(0.,1.,0.));
#18342=DIRECTION('center_axis',(0.,1.,0.));
#18343=DIRECTION('ref_axis',(0.,0.,1.));
#18344=DIRECTION('center_axis',(0.,-1.,0.));
#18345=DIRECTION('ref_axis',(0.,0.,-1.));
#18346=DIRECTION('',(1.,0.,0.));
#18347=DIRECTION('center_axis',(0.,0.,-1.));
#18348=DIRECTION('ref_axis',(0.,1.,0.));
#18349=DIRECTION('',(1.,0.,0.));
#18350=DIRECTION('center_axis',(0.,1.,0.));
#18351=DIRECTION('ref_axis',(0.,0.,1.));
#18352=DIRECTION('axis',(0.,0.,1.));
#18353=DIRECTION('refdir',(1.,0.,0.));
#18354=DIRECTION('center_axis',(-1.,0.,0.));
#18355=DIRECTION('ref_axis',(0.,-1.,0.));
#18356=DIRECTION('',(0.,-1.,0.));
#18357=DIRECTION('',(0.,0.,1.));
#18358=DIRECTION('',(0.,1.,0.));
#18359=DIRECTION('',(0.,0.,1.));
#18360=DIRECTION('center_axis',(0.,0.,1.));
#18361=DIRECTION('ref_axis',(-8.88178419700065E-14,1.,0.));
#18362=DIRECTION('center_axis',(0.,0.,1.));
#18363=DIRECTION('ref_axis',(-8.88178419700065E-14,1.,0.));
#18364=DIRECTION('',(0.,0.,1.));
#18365=DIRECTION('center_axis',(0.,0.,-1.));
#18366=DIRECTION('ref_axis',(-8.88178419700065E-14,1.,0.));
#18367=DIRECTION('center_axis',(0.,1.,0.));
#18368=DIRECTION('ref_axis',(-1.,0.,0.));
#18369=DIRECTION('',(-1.,0.,0.));
#18370=DIRECTION('',(0.,0.,1.));
#18371=DIRECTION('',(1.,0.,0.));
#18372=DIRECTION('center_axis',(0.,0.,1.));
#18373=DIRECTION('ref_axis',(1.,-1.33226762955033E-13,0.));
#18374=DIRECTION('center_axis',(0.,0.,1.));
#18375=DIRECTION('ref_axis',(1.,-1.33226762955033E-13,0.));
#18376=DIRECTION('',(0.,0.,1.));
#18377=DIRECTION('center_axis',(0.,0.,-1.));
#18378=DIRECTION('ref_axis',(1.,-1.33226762955033E-13,0.));
#18379=DIRECTION('center_axis',(1.,0.,0.));
#18380=DIRECTION('ref_axis',(0.,1.,0.));
#18381=DIRECTION('',(0.,1.,0.));
#18382=DIRECTION('',(0.,0.,1.));
#18383=DIRECTION('',(0.,-1.,0.));
#18384=DIRECTION('center_axis',(0.,0.,1.));
#18385=DIRECTION('ref_axis',(-8.88178419700248E-14,-1.,0.));
#18386=DIRECTION('center_axis',(0.,0.,1.));
#18387=DIRECTION('ref_axis',(-8.88178419700248E-14,-1.,0.));
#18388=DIRECTION('',(0.,0.,1.));
#18389=DIRECTION('center_axis',(0.,0.,-1.));
#18390=DIRECTION('ref_axis',(-8.88178419700248E-14,-1.,0.));
#18391=DIRECTION('center_axis',(0.,-1.,0.));
#18392=DIRECTION('ref_axis',(1.,0.,0.));
#18393=DIRECTION('',(1.,0.,0.));
#18394=DIRECTION('',(0.,0.,1.));
#18395=DIRECTION('',(-1.,0.,0.));
#18396=DIRECTION('center_axis',(0.,0.,1.));
#18397=DIRECTION('ref_axis',(-1.,-6.66133814775049E-14,0.));
#18398=DIRECTION('center_axis',(0.,0.,1.));
#18399=DIRECTION('ref_axis',(-1.,-6.66133814775049E-14,0.));
#18400=DIRECTION('center_axis',(0.,0.,-1.));
#18401=DIRECTION('ref_axis',(-1.,-6.66133814775049E-14,0.));
#18402=DIRECTION('center_axis',(-1.,0.,0.));
#18403=DIRECTION('ref_axis',(0.,-1.,0.));
#18404=DIRECTION('',(0.,-1.,0.));
#18405=DIRECTION('',(0.,0.,1.));
#18406=DIRECTION('',(0.,1.,0.));
#18407=DIRECTION('',(0.,0.,1.));
#18408=DIRECTION('center_axis',(0.,0.,1.));
#18409=DIRECTION('ref_axis',(1.11022302462517E-14,1.,0.));
#18410=DIRECTION('center_axis',(0.,0.,1.));
#18411=DIRECTION('ref_axis',(1.11022302462517E-14,1.,0.));
#18412=DIRECTION('',(0.,0.,1.));
#18413=DIRECTION('center_axis',(0.,0.,-1.));
#18414=DIRECTION('ref_axis',(1.11022302462517E-14,1.,0.));
#18415=DIRECTION('center_axis',(0.,1.,0.));
#18416=DIRECTION('ref_axis',(-1.,0.,0.));
#18417=DIRECTION('',(-1.,0.,0.));
#18418=DIRECTION('',(0.,0.,1.));
#18419=DIRECTION('',(1.,0.,0.));
#18420=DIRECTION('center_axis',(0.,0.,1.));
#18421=DIRECTION('ref_axis',(1.,-1.11022302462516E-14,0.));
#18422=DIRECTION('center_axis',(0.,0.,1.));
#18423=DIRECTION('ref_axis',(1.,-1.11022302462516E-14,0.));
#18424=DIRECTION('',(0.,0.,1.));
#18425=DIRECTION('center_axis',(0.,0.,-1.));
#18426=DIRECTION('ref_axis',(1.,-1.11022302462516E-14,0.));
#18427=DIRECTION('center_axis',(1.,0.,0.));
#18428=DIRECTION('ref_axis',(0.,1.,0.));
#18429=DIRECTION('',(0.,1.,0.));
#18430=DIRECTION('',(0.,0.,1.));
#18431=DIRECTION('',(0.,-1.,0.));
#18432=DIRECTION('center_axis',(0.,0.,1.));
#18433=DIRECTION('ref_axis',(2.22044604925034E-14,-1.,0.));
#18434=DIRECTION('center_axis',(0.,0.,1.));
#18435=DIRECTION('ref_axis',(2.22044604925034E-14,-1.,0.));
#18436=DIRECTION('',(0.,0.,1.));
#18437=DIRECTION('center_axis',(0.,0.,-1.));
#18438=DIRECTION('ref_axis',(2.22044604925034E-14,-1.,0.));
#18439=DIRECTION('center_axis',(0.,-1.,0.));
#18440=DIRECTION('ref_axis',(1.,0.,0.));
#18441=DIRECTION('',(1.,0.,0.));
#18442=DIRECTION('',(0.,0.,1.));
#18443=DIRECTION('',(-1.,0.,0.));
#18444=DIRECTION('center_axis',(0.,0.,1.));
#18445=DIRECTION('ref_axis',(-1.,5.55111512312584E-15,0.));
#18446=DIRECTION('center_axis',(0.,0.,1.));
#18447=DIRECTION('ref_axis',(-1.,5.55111512312584E-15,0.));
#18448=DIRECTION('center_axis',(0.,0.,-1.));
#18449=DIRECTION('ref_axis',(-1.,5.55111512312584E-15,0.));
#18450=DIRECTION('center_axis',(-1.,0.,0.));
#18451=DIRECTION('ref_axis',(0.,-1.,0.));
#18452=DIRECTION('',(0.,-1.,0.));
#18453=DIRECTION('',(0.,0.,1.));
#18454=DIRECTION('',(0.,1.,0.));
#18455=DIRECTION('',(0.,0.,1.));
#18456=DIRECTION('center_axis',(0.,0.,1.));
#18457=DIRECTION('ref_axis',(-2.96059473233373E-14,1.,0.));
#18458=DIRECTION('center_axis',(0.,0.,1.));
#18459=DIRECTION('ref_axis',(-2.96059473233373E-14,1.,0.));
#18460=DIRECTION('',(0.,0.,1.));
#18461=DIRECTION('center_axis',(0.,0.,-1.));
#18462=DIRECTION('ref_axis',(-2.96059473233373E-14,1.,0.));
#18463=DIRECTION('center_axis',(0.,1.,0.));
#18464=DIRECTION('ref_axis',(-1.,0.,0.));
#18465=DIRECTION('',(-1.,0.,0.));
#18466=DIRECTION('',(0.,0.,1.));
#18467=DIRECTION('',(1.,0.,0.));
#18468=DIRECTION('center_axis',(0.,0.,1.));
#18469=DIRECTION('ref_axis',(1.,0.,0.));
#18470=DIRECTION('center_axis',(0.,0.,1.));
#18471=DIRECTION('ref_axis',(1.,0.,0.));
#18472=DIRECTION('',(0.,0.,1.));
#18473=DIRECTION('center_axis',(0.,0.,-1.));
#18474=DIRECTION('ref_axis',(1.,0.,0.));
#18475=DIRECTION('center_axis',(1.,0.,0.));
#18476=DIRECTION('ref_axis',(0.,1.,0.));
#18477=DIRECTION('',(0.,1.,0.));
#18478=DIRECTION('',(0.,0.,1.));
#18479=DIRECTION('',(0.,-1.,0.));
#18480=DIRECTION('center_axis',(0.,0.,1.));
#18481=DIRECTION('ref_axis',(2.96059473233373E-14,-1.,0.));
#18482=DIRECTION('center_axis',(0.,0.,1.));
#18483=DIRECTION('ref_axis',(2.96059473233373E-14,-1.,0.));
#18484=DIRECTION('',(0.,0.,1.));
#18485=DIRECTION('center_axis',(0.,0.,-1.));
#18486=DIRECTION('ref_axis',(2.96059473233373E-14,-1.,0.));
#18487=DIRECTION('center_axis',(0.,-1.,0.));
#18488=DIRECTION('ref_axis',(1.,0.,0.));
#18489=DIRECTION('',(1.,0.,0.));
#18490=DIRECTION('',(0.,0.,1.));
#18491=DIRECTION('',(-1.,0.,0.));
#18492=DIRECTION('center_axis',(0.,0.,1.));
#18493=DIRECTION('ref_axis',(-1.,-7.40148683083432E-15,0.));
#18494=DIRECTION('center_axis',(0.,0.,1.));
#18495=DIRECTION('ref_axis',(-1.,-7.40148683083432E-15,0.));
#18496=DIRECTION('center_axis',(0.,0.,-1.));
#18497=DIRECTION('ref_axis',(-1.,-7.40148683083432E-15,0.));
#18498=DIRECTION('center_axis',(-1.,0.,0.));
#18499=DIRECTION('ref_axis',(0.,-1.,0.));
#18500=DIRECTION('',(0.,-1.,0.));
#18501=DIRECTION('',(0.,0.,1.));
#18502=DIRECTION('',(0.,1.,0.));
#18503=DIRECTION('',(0.,0.,1.));
#18504=DIRECTION('center_axis',(0.,0.,1.));
#18505=DIRECTION('ref_axis',(-2.96059473233373E-14,1.,0.));
#18506=DIRECTION('center_axis',(0.,0.,1.));
#18507=DIRECTION('ref_axis',(-2.96059473233373E-14,1.,0.));
#18508=DIRECTION('',(0.,0.,1.));
#18509=DIRECTION('center_axis',(0.,0.,-1.));
#18510=DIRECTION('ref_axis',(-2.96059473233373E-14,1.,0.));
#18511=DIRECTION('center_axis',(0.,1.,0.));
#18512=DIRECTION('ref_axis',(-1.,0.,0.));
#18513=DIRECTION('',(-1.,0.,0.));
#18514=DIRECTION('',(0.,0.,1.));
#18515=DIRECTION('',(1.,0.,0.));
#18516=DIRECTION('center_axis',(0.,0.,1.));
#18517=DIRECTION('ref_axis',(1.,0.,0.));
#18518=DIRECTION('center_axis',(0.,0.,1.));
#18519=DIRECTION('ref_axis',(1.,0.,0.));
#18520=DIRECTION('',(0.,0.,1.));
#18521=DIRECTION('center_axis',(0.,0.,-1.));
#18522=DIRECTION('ref_axis',(1.,0.,0.));
#18523=DIRECTION('center_axis',(1.,0.,0.));
#18524=DIRECTION('ref_axis',(0.,1.,0.));
#18525=DIRECTION('',(0.,1.,0.));
#18526=DIRECTION('',(0.,0.,1.));
#18527=DIRECTION('',(0.,-1.,0.));
#18528=DIRECTION('center_axis',(0.,0.,1.));
#18529=DIRECTION('ref_axis',(2.96059473233373E-14,-1.,0.));
#18530=DIRECTION('center_axis',(0.,0.,1.));
#18531=DIRECTION('ref_axis',(2.96059473233373E-14,-1.,0.));
#18532=DIRECTION('',(0.,0.,1.));
#18533=DIRECTION('center_axis',(0.,0.,-1.));
#18534=DIRECTION('ref_axis',(2.96059473233373E-14,-1.,0.));
#18535=DIRECTION('center_axis',(0.,-1.,0.));
#18536=DIRECTION('ref_axis',(1.,0.,0.));
#18537=DIRECTION('',(1.,0.,0.));
#18538=DIRECTION('',(0.,0.,1.));
#18539=DIRECTION('',(-1.,0.,0.));
#18540=DIRECTION('center_axis',(0.,0.,1.));
#18541=DIRECTION('ref_axis',(-1.,-7.40148683083432E-15,0.));
#18542=DIRECTION('center_axis',(0.,0.,1.));
#18543=DIRECTION('ref_axis',(-1.,-7.40148683083432E-15,0.));
#18544=DIRECTION('center_axis',(0.,0.,-1.));
#18545=DIRECTION('ref_axis',(-1.,-7.40148683083432E-15,0.));
#18546=DIRECTION('center_axis',(-1.,0.,0.));
#18547=DIRECTION('ref_axis',(0.,-1.,0.));
#18548=DIRECTION('',(0.,-1.,0.));
#18549=DIRECTION('',(0.,0.,1.));
#18550=DIRECTION('',(0.,1.,0.));
#18551=DIRECTION('',(0.,0.,1.));
#18552=DIRECTION('center_axis',(0.,0.,1.));
#18553=DIRECTION('ref_axis',(0.,1.,0.));
#18554=DIRECTION('center_axis',(0.,0.,1.));
#18555=DIRECTION('ref_axis',(0.,1.,0.));
#18556=DIRECTION('',(0.,0.,1.));
#18557=DIRECTION('center_axis',(0.,0.,-1.));
#18558=DIRECTION('ref_axis',(0.,1.,0.));
#18559=DIRECTION('center_axis',(0.,1.,0.));
#18560=DIRECTION('ref_axis',(-1.,0.,0.));
#18561=DIRECTION('',(-1.,0.,0.));
#18562=DIRECTION('',(0.,0.,1.));
#18563=DIRECTION('',(1.,0.,0.));
#18564=DIRECTION('center_axis',(0.,0.,1.));
#18565=DIRECTION('ref_axis',(1.,-2.96059473233381E-14,0.));
#18566=DIRECTION('center_axis',(0.,0.,1.));
#18567=DIRECTION('ref_axis',(1.,-2.96059473233381E-14,0.));
#18568=DIRECTION('',(0.,0.,1.));
#18569=DIRECTION('center_axis',(0.,0.,-1.));
#18570=DIRECTION('ref_axis',(1.,-2.96059473233381E-14,0.));
#18571=DIRECTION('center_axis',(1.,0.,0.));
#18572=DIRECTION('ref_axis',(0.,1.,0.));
#18573=DIRECTION('',(0.,1.,0.));
#18574=DIRECTION('',(0.,0.,1.));
#18575=DIRECTION('',(0.,-1.,0.));
#18576=DIRECTION('center_axis',(0.,0.,1.));
#18577=DIRECTION('ref_axis',(0.,-1.,0.));
#18578=DIRECTION('center_axis',(0.,0.,1.));
#18579=DIRECTION('ref_axis',(0.,-1.,0.));
#18580=DIRECTION('',(0.,0.,1.));
#18581=DIRECTION('center_axis',(0.,0.,-1.));
#18582=DIRECTION('ref_axis',(0.,-1.,0.));
#18583=DIRECTION('center_axis',(0.,-1.,0.));
#18584=DIRECTION('ref_axis',(1.,0.,0.));
#18585=DIRECTION('',(1.,0.,0.));
#18586=DIRECTION('',(0.,0.,1.));
#18587=DIRECTION('',(-1.,0.,0.));
#18588=DIRECTION('center_axis',(0.,0.,1.));
#18589=DIRECTION('ref_axis',(-1.,2.22044604925036E-14,0.));
#18590=DIRECTION('center_axis',(0.,0.,1.));
#18591=DIRECTION('ref_axis',(-1.,2.22044604925036E-14,0.));
#18592=DIRECTION('center_axis',(0.,0.,-1.));
#18593=DIRECTION('ref_axis',(-1.,2.22044604925036E-14,0.));
#18594=DIRECTION('center_axis',(-1.,0.,0.));
#18595=DIRECTION('ref_axis',(0.,-1.,0.));
#18596=DIRECTION('',(0.,-1.,0.));
#18597=DIRECTION('',(0.,0.,1.));
#18598=DIRECTION('',(0.,1.,0.));
#18599=DIRECTION('',(0.,0.,1.));
#18600=DIRECTION('center_axis',(0.,0.,1.));
#18601=DIRECTION('ref_axis',(0.,1.,0.));
#18602=DIRECTION('center_axis',(0.,0.,1.));
#18603=DIRECTION('ref_axis',(0.,1.,0.));
#18604=DIRECTION('',(0.,0.,1.));
#18605=DIRECTION('center_axis',(0.,0.,-1.));
#18606=DIRECTION('ref_axis',(0.,1.,0.));
#18607=DIRECTION('center_axis',(0.,1.,0.));
#18608=DIRECTION('ref_axis',(-1.,0.,0.));
#18609=DIRECTION('',(-1.,0.,0.));
#18610=DIRECTION('',(0.,0.,1.));
#18611=DIRECTION('',(1.,0.,0.));
#18612=DIRECTION('center_axis',(0.,0.,1.));
#18613=DIRECTION('ref_axis',(1.,-2.96059473233381E-14,0.));
#18614=DIRECTION('center_axis',(0.,0.,1.));
#18615=DIRECTION('ref_axis',(1.,-2.96059473233381E-14,0.));
#18616=DIRECTION('',(0.,0.,1.));
#18617=DIRECTION('center_axis',(0.,0.,-1.));
#18618=DIRECTION('ref_axis',(1.,-2.96059473233381E-14,0.));
#18619=DIRECTION('center_axis',(1.,0.,0.));
#18620=DIRECTION('ref_axis',(0.,1.,0.));
#18621=DIRECTION('',(0.,1.,0.));
#18622=DIRECTION('',(0.,0.,1.));
#18623=DIRECTION('',(0.,-1.,0.));
#18624=DIRECTION('center_axis',(0.,0.,1.));
#18625=DIRECTION('ref_axis',(0.,-1.,0.));
#18626=DIRECTION('center_axis',(0.,0.,1.));
#18627=DIRECTION('ref_axis',(0.,-1.,0.));
#18628=DIRECTION('',(0.,0.,1.));
#18629=DIRECTION('center_axis',(0.,0.,-1.));
#18630=DIRECTION('ref_axis',(0.,-1.,0.));
#18631=DIRECTION('center_axis',(0.,-1.,0.));
#18632=DIRECTION('ref_axis',(1.,0.,0.));
#18633=DIRECTION('',(1.,0.,0.));
#18634=DIRECTION('',(0.,0.,1.));
#18635=DIRECTION('',(-1.,0.,0.));
#18636=DIRECTION('center_axis',(0.,0.,1.));
#18637=DIRECTION('ref_axis',(-1.,2.22044604925036E-14,0.));
#18638=DIRECTION('center_axis',(0.,0.,1.));
#18639=DIRECTION('ref_axis',(-1.,2.22044604925036E-14,0.));
#18640=DIRECTION('center_axis',(0.,0.,-1.));
#18641=DIRECTION('ref_axis',(-1.,2.22044604925036E-14,0.));
#18642=DIRECTION('center_axis',(-1.,0.,0.));
#18643=DIRECTION('ref_axis',(0.,-1.,0.));
#18644=DIRECTION('',(0.,-1.,0.));
#18645=DIRECTION('',(0.,0.,1.));
#18646=DIRECTION('',(0.,1.,0.));
#18647=DIRECTION('',(0.,0.,1.));
#18648=DIRECTION('center_axis',(0.,0.,1.));
#18649=DIRECTION('ref_axis',(0.,1.,0.));
#18650=DIRECTION('center_axis',(0.,0.,1.));
#18651=DIRECTION('ref_axis',(0.,1.,0.));
#18652=DIRECTION('',(0.,0.,1.));
#18653=DIRECTION('center_axis',(0.,0.,-1.));
#18654=DIRECTION('ref_axis',(0.,1.,0.));
#18655=DIRECTION('center_axis',(0.,1.,0.));
#18656=DIRECTION('ref_axis',(-1.,0.,0.));
#18657=DIRECTION('',(-1.,0.,0.));
#18658=DIRECTION('',(0.,0.,1.));
#18659=DIRECTION('',(1.,0.,0.));
#18660=DIRECTION('center_axis',(0.,0.,1.));
#18661=DIRECTION('ref_axis',(1.,-2.96059473233381E-14,0.));
#18662=DIRECTION('center_axis',(0.,0.,1.));
#18663=DIRECTION('ref_axis',(1.,-2.96059473233381E-14,0.));
#18664=DIRECTION('',(0.,0.,1.));
#18665=DIRECTION('center_axis',(0.,0.,-1.));
#18666=DIRECTION('ref_axis',(1.,-2.96059473233381E-14,0.));
#18667=DIRECTION('center_axis',(1.,0.,0.));
#18668=DIRECTION('ref_axis',(0.,1.,0.));
#18669=DIRECTION('',(0.,1.,0.));
#18670=DIRECTION('',(0.,0.,1.));
#18671=DIRECTION('',(0.,-1.,0.));
#18672=DIRECTION('center_axis',(0.,0.,1.));
#18673=DIRECTION('ref_axis',(0.,-1.,0.));
#18674=DIRECTION('center_axis',(0.,0.,1.));
#18675=DIRECTION('ref_axis',(0.,-1.,0.));
#18676=DIRECTION('',(0.,0.,1.));
#18677=DIRECTION('center_axis',(0.,0.,-1.));
#18678=DIRECTION('ref_axis',(0.,-1.,0.));
#18679=DIRECTION('center_axis',(0.,-1.,0.));
#18680=DIRECTION('ref_axis',(1.,0.,0.));
#18681=DIRECTION('',(1.,0.,0.));
#18682=DIRECTION('',(0.,0.,1.));
#18683=DIRECTION('',(-1.,0.,0.));
#18684=DIRECTION('center_axis',(0.,0.,1.));
#18685=DIRECTION('ref_axis',(-1.,2.22044604925036E-14,0.));
#18686=DIRECTION('center_axis',(0.,0.,1.));
#18687=DIRECTION('ref_axis',(-1.,2.22044604925036E-14,0.));
#18688=DIRECTION('center_axis',(0.,0.,-1.));
#18689=DIRECTION('ref_axis',(-1.,2.22044604925036E-14,0.));
#18690=DIRECTION('center_axis',(-1.,0.,0.));
#18691=DIRECTION('ref_axis',(0.,-1.,0.));
#18692=DIRECTION('',(0.,-1.,0.));
#18693=DIRECTION('',(0.,0.,1.));
#18694=DIRECTION('',(0.,1.,0.));
#18695=DIRECTION('',(0.,0.,1.));
#18696=DIRECTION('center_axis',(0.,0.,1.));
#18697=DIRECTION('ref_axis',(0.,1.,0.));
#18698=DIRECTION('center_axis',(0.,0.,1.));
#18699=DIRECTION('ref_axis',(0.,1.,0.));
#18700=DIRECTION('',(0.,0.,1.));
#18701=DIRECTION('center_axis',(0.,0.,-1.));
#18702=DIRECTION('ref_axis',(0.,1.,0.));
#18703=DIRECTION('center_axis',(0.,1.,0.));
#18704=DIRECTION('ref_axis',(-1.,0.,0.));
#18705=DIRECTION('',(-1.,0.,0.));
#18706=DIRECTION('',(0.,0.,1.));
#18707=DIRECTION('',(1.,0.,0.));
#18708=DIRECTION('center_axis',(0.,0.,1.));
#18709=DIRECTION('ref_axis',(1.,-1.48029736616686E-14,0.));
#18710=DIRECTION('center_axis',(0.,0.,1.));
#18711=DIRECTION('ref_axis',(1.,-1.48029736616686E-14,0.));
#18712=DIRECTION('',(0.,0.,1.));
#18713=DIRECTION('center_axis',(0.,0.,-1.));
#18714=DIRECTION('ref_axis',(1.,-1.48029736616686E-14,0.));
#18715=DIRECTION('center_axis',(1.,0.,0.));
#18716=DIRECTION('ref_axis',(0.,1.,0.));
#18717=DIRECTION('',(0.,1.,0.));
#18718=DIRECTION('',(0.,0.,1.));
#18719=DIRECTION('',(0.,-1.,0.));
#18720=DIRECTION('center_axis',(0.,0.,1.));
#18721=DIRECTION('ref_axis',(1.48029736616688E-14,-1.,0.));
#18722=DIRECTION('center_axis',(0.,0.,1.));
#18723=DIRECTION('ref_axis',(1.48029736616688E-14,-1.,0.));
#18724=DIRECTION('',(0.,0.,1.));
#18725=DIRECTION('center_axis',(0.,0.,-1.));
#18726=DIRECTION('ref_axis',(1.48029736616688E-14,-1.,0.));
#18727=DIRECTION('center_axis',(0.,-1.,0.));
#18728=DIRECTION('ref_axis',(1.,0.,0.));
#18729=DIRECTION('',(1.,0.,0.));
#18730=DIRECTION('',(0.,0.,1.));
#18731=DIRECTION('',(-1.,0.,0.));
#18732=DIRECTION('center_axis',(0.,0.,1.));
#18733=DIRECTION('ref_axis',(-1.,-3.70074341541716E-15,0.));
#18734=DIRECTION('center_axis',(0.,0.,1.));
#18735=DIRECTION('ref_axis',(-1.,-3.70074341541716E-15,0.));
#18736=DIRECTION('center_axis',(0.,0.,-1.));
#18737=DIRECTION('ref_axis',(-1.,-3.70074341541716E-15,0.));
#18738=DIRECTION('center_axis',(-1.,0.,0.));
#18739=DIRECTION('ref_axis',(0.,-1.,0.));
#18740=DIRECTION('',(0.,-1.,0.));
#18741=DIRECTION('',(0.,0.,1.));
#18742=DIRECTION('',(0.,1.,0.));
#18743=DIRECTION('',(0.,0.,1.));
#18744=DIRECTION('center_axis',(0.,0.,1.));
#18745=DIRECTION('ref_axis',(0.,1.,0.));
#18746=DIRECTION('center_axis',(0.,0.,1.));
#18747=DIRECTION('ref_axis',(0.,1.,0.));
#18748=DIRECTION('',(0.,0.,1.));
#18749=DIRECTION('center_axis',(0.,0.,-1.));
#18750=DIRECTION('ref_axis',(0.,1.,0.));
#18751=DIRECTION('center_axis',(0.,1.,0.));
#18752=DIRECTION('ref_axis',(-1.,0.,0.));
#18753=DIRECTION('',(-1.,0.,0.));
#18754=DIRECTION('',(0.,0.,1.));
#18755=DIRECTION('',(1.,0.,0.));
#18756=DIRECTION('center_axis',(0.,0.,1.));
#18757=DIRECTION('ref_axis',(1.,-7.40148683083432E-15,0.));
#18758=DIRECTION('center_axis',(0.,0.,1.));
#18759=DIRECTION('ref_axis',(1.,-7.40148683083432E-15,0.));
#18760=DIRECTION('',(0.,0.,1.));
#18761=DIRECTION('center_axis',(0.,0.,-1.));
#18762=DIRECTION('ref_axis',(1.,-7.40148683083432E-15,0.));
#18763=DIRECTION('center_axis',(1.,0.,0.));
#18764=DIRECTION('ref_axis',(0.,1.,0.));
#18765=DIRECTION('',(0.,1.,0.));
#18766=DIRECTION('',(0.,0.,1.));
#18767=DIRECTION('',(0.,-1.,0.));
#18768=DIRECTION('center_axis',(0.,0.,1.));
#18769=DIRECTION('ref_axis',(0.,-1.,0.));
#18770=DIRECTION('center_axis',(0.,0.,1.));
#18771=DIRECTION('ref_axis',(0.,-1.,0.));
#18772=DIRECTION('',(0.,0.,1.));
#18773=DIRECTION('center_axis',(0.,0.,-1.));
#18774=DIRECTION('ref_axis',(0.,-1.,0.));
#18775=DIRECTION('center_axis',(0.,-1.,0.));
#18776=DIRECTION('ref_axis',(1.,0.,0.));
#18777=DIRECTION('',(1.,0.,0.));
#18778=DIRECTION('',(0.,0.,1.));
#18779=DIRECTION('',(-1.,0.,0.));
#18780=DIRECTION('center_axis',(0.,0.,1.));
#18781=DIRECTION('ref_axis',(-1.,-3.70074341541716E-15,0.));
#18782=DIRECTION('center_axis',(0.,0.,1.));
#18783=DIRECTION('ref_axis',(-1.,-3.70074341541716E-15,0.));
#18784=DIRECTION('center_axis',(0.,0.,-1.));
#18785=DIRECTION('ref_axis',(-1.,-3.70074341541716E-15,0.));
#18786=DIRECTION('center_axis',(-1.,0.,0.));
#18787=DIRECTION('ref_axis',(0.,-1.,0.));
#18788=DIRECTION('',(0.,-1.,0.));
#18789=DIRECTION('',(0.,0.,1.));
#18790=DIRECTION('',(0.,1.,0.));
#18791=DIRECTION('',(0.,0.,1.));
#18792=DIRECTION('center_axis',(0.,0.,1.));
#18793=DIRECTION('ref_axis',(-1.48029736616688E-14,1.,0.));
#18794=DIRECTION('center_axis',(0.,0.,1.));
#18795=DIRECTION('ref_axis',(-1.48029736616688E-14,1.,0.));
#18796=DIRECTION('',(0.,0.,1.));
#18797=DIRECTION('center_axis',(0.,0.,-1.));
#18798=DIRECTION('ref_axis',(-1.48029736616688E-14,1.,0.));
#18799=DIRECTION('center_axis',(0.,1.,0.));
#18800=DIRECTION('ref_axis',(-1.,0.,0.));
#18801=DIRECTION('',(-1.,0.,0.));
#18802=DIRECTION('',(0.,0.,1.));
#18803=DIRECTION('',(1.,0.,0.));
#18804=DIRECTION('center_axis',(0.,0.,1.));
#18805=DIRECTION('ref_axis',(1.,-1.48029736616686E-14,0.));
#18806=DIRECTION('center_axis',(0.,0.,1.));
#18807=DIRECTION('ref_axis',(1.,-1.48029736616686E-14,0.));
#18808=DIRECTION('',(0.,0.,1.));
#18809=DIRECTION('center_axis',(0.,0.,-1.));
#18810=DIRECTION('ref_axis',(1.,-1.48029736616686E-14,0.));
#18811=DIRECTION('center_axis',(1.,0.,0.));
#18812=DIRECTION('ref_axis',(0.,1.,0.));
#18813=DIRECTION('',(0.,1.,0.));
#18814=DIRECTION('',(0.,0.,1.));
#18815=DIRECTION('',(0.,-1.,0.));
#18816=DIRECTION('center_axis',(0.,0.,1.));
#18817=DIRECTION('ref_axis',(1.48029736616688E-14,-1.,0.));
#18818=DIRECTION('center_axis',(0.,0.,1.));
#18819=DIRECTION('ref_axis',(1.48029736616688E-14,-1.,0.));
#18820=DIRECTION('',(0.,0.,1.));
#18821=DIRECTION('center_axis',(0.,0.,-1.));
#18822=DIRECTION('ref_axis',(1.48029736616688E-14,-1.,0.));
#18823=DIRECTION('center_axis',(0.,-1.,0.));
#18824=DIRECTION('ref_axis',(1.,0.,0.));
#18825=DIRECTION('',(1.,0.,0.));
#18826=DIRECTION('',(0.,0.,1.));
#18827=DIRECTION('',(-1.,0.,0.));
#18828=DIRECTION('center_axis',(0.,0.,1.));
#18829=DIRECTION('ref_axis',(-1.,3.70074341541716E-15,0.));
#18830=DIRECTION('center_axis',(0.,0.,1.));
#18831=DIRECTION('ref_axis',(-1.,3.70074341541716E-15,0.));
#18832=DIRECTION('center_axis',(0.,0.,-1.));
#18833=DIRECTION('ref_axis',(-1.,3.70074341541716E-15,0.));
#18834=DIRECTION('center_axis',(-1.,0.,0.));
#18835=DIRECTION('ref_axis',(0.,-1.,0.));
#18836=DIRECTION('',(0.,-1.,0.));
#18837=DIRECTION('',(0.,0.,1.));
#18838=DIRECTION('',(0.,1.,0.));
#18839=DIRECTION('',(0.,0.,1.));
#18840=DIRECTION('center_axis',(0.,0.,1.));
#18841=DIRECTION('ref_axis',(0.,1.,0.));
#18842=DIRECTION('center_axis',(0.,0.,1.));
#18843=DIRECTION('ref_axis',(0.,1.,0.));
#18844=DIRECTION('',(0.,0.,1.));
#18845=DIRECTION('center_axis',(0.,0.,-1.));
#18846=DIRECTION('ref_axis',(0.,1.,0.));
#18847=DIRECTION('center_axis',(0.,1.,0.));
#18848=DIRECTION('ref_axis',(-1.,0.,0.));
#18849=DIRECTION('',(-1.,0.,0.));
#18850=DIRECTION('',(0.,0.,1.));
#18851=DIRECTION('',(1.,0.,0.));
#18852=DIRECTION('center_axis',(0.,0.,1.));
#18853=DIRECTION('ref_axis',(1.,-2.96059473233381E-14,0.));
#18854=DIRECTION('center_axis',(0.,0.,1.));
#18855=DIRECTION('ref_axis',(1.,-2.96059473233381E-14,0.));
#18856=DIRECTION('',(0.,0.,1.));
#18857=DIRECTION('center_axis',(0.,0.,-1.));
#18858=DIRECTION('ref_axis',(1.,-2.96059473233381E-14,0.));
#18859=DIRECTION('center_axis',(1.,0.,0.));
#18860=DIRECTION('ref_axis',(0.,1.,0.));
#18861=DIRECTION('',(0.,1.,0.));
#18862=DIRECTION('',(0.,0.,1.));
#18863=DIRECTION('',(0.,-1.,0.));
#18864=DIRECTION('center_axis',(0.,0.,1.));
#18865=DIRECTION('ref_axis',(0.,-1.,0.));
#18866=DIRECTION('center_axis',(0.,0.,1.));
#18867=DIRECTION('ref_axis',(0.,-1.,0.));
#18868=DIRECTION('',(0.,0.,1.));
#18869=DIRECTION('center_axis',(0.,0.,-1.));
#18870=DIRECTION('ref_axis',(0.,-1.,0.));
#18871=DIRECTION('center_axis',(0.,-1.,0.));
#18872=DIRECTION('ref_axis',(1.,0.,0.));
#18873=DIRECTION('',(1.,0.,0.));
#18874=DIRECTION('',(0.,0.,1.));
#18875=DIRECTION('',(-1.,0.,0.));
#18876=DIRECTION('center_axis',(0.,0.,1.));
#18877=DIRECTION('ref_axis',(-1.,2.22044604925036E-14,0.));
#18878=DIRECTION('center_axis',(0.,0.,1.));
#18879=DIRECTION('ref_axis',(-1.,2.22044604925036E-14,0.));
#18880=DIRECTION('center_axis',(0.,0.,-1.));
#18881=DIRECTION('ref_axis',(-1.,2.22044604925036E-14,0.));
#18882=DIRECTION('center_axis',(-1.,0.,0.));
#18883=DIRECTION('ref_axis',(0.,-1.,0.));
#18884=DIRECTION('',(0.,-1.,0.));
#18885=DIRECTION('',(0.,0.,1.));
#18886=DIRECTION('',(0.,1.,0.));
#18887=DIRECTION('',(0.,0.,1.));
#18888=DIRECTION('center_axis',(0.,0.,1.));
#18889=DIRECTION('ref_axis',(0.,1.,0.));
#18890=DIRECTION('center_axis',(0.,0.,1.));
#18891=DIRECTION('ref_axis',(0.,1.,0.));
#18892=DIRECTION('',(0.,0.,1.));
#18893=DIRECTION('center_axis',(0.,0.,-1.));
#18894=DIRECTION('ref_axis',(0.,1.,0.));
#18895=DIRECTION('center_axis',(0.,1.,0.));
#18896=DIRECTION('ref_axis',(-1.,0.,0.));
#18897=DIRECTION('',(-1.,0.,0.));
#18898=DIRECTION('',(0.,0.,1.));
#18899=DIRECTION('',(1.,0.,0.));
#18900=DIRECTION('center_axis',(0.,0.,1.));
#18901=DIRECTION('ref_axis',(1.,-7.40148683083432E-15,0.));
#18902=DIRECTION('center_axis',(0.,0.,1.));
#18903=DIRECTION('ref_axis',(1.,-7.40148683083432E-15,0.));
#18904=DIRECTION('',(0.,0.,1.));
#18905=DIRECTION('center_axis',(0.,0.,-1.));
#18906=DIRECTION('ref_axis',(1.,-7.40148683083432E-15,0.));
#18907=DIRECTION('center_axis',(1.,0.,0.));
#18908=DIRECTION('ref_axis',(0.,1.,0.));
#18909=DIRECTION('',(0.,1.,0.));
#18910=DIRECTION('',(0.,0.,1.));
#18911=DIRECTION('',(0.,-1.,0.));
#18912=DIRECTION('center_axis',(0.,0.,1.));
#18913=DIRECTION('ref_axis',(0.,-1.,0.));
#18914=DIRECTION('center_axis',(0.,0.,1.));
#18915=DIRECTION('ref_axis',(0.,-1.,0.));
#18916=DIRECTION('',(0.,0.,1.));
#18917=DIRECTION('center_axis',(0.,0.,-1.));
#18918=DIRECTION('ref_axis',(0.,-1.,0.));
#18919=DIRECTION('center_axis',(0.,-1.,0.));
#18920=DIRECTION('ref_axis',(1.,0.,0.));
#18921=DIRECTION('',(1.,0.,0.));
#18922=DIRECTION('',(0.,0.,1.));
#18923=DIRECTION('',(-1.,0.,0.));
#18924=DIRECTION('center_axis',(0.,0.,1.));
#18925=DIRECTION('ref_axis',(-1.,-3.70074341541716E-15,0.));
#18926=DIRECTION('center_axis',(0.,0.,1.));
#18927=DIRECTION('ref_axis',(-1.,-3.70074341541716E-15,0.));
#18928=DIRECTION('center_axis',(0.,0.,-1.));
#18929=DIRECTION('ref_axis',(-1.,-3.70074341541716E-15,0.));
#18930=DIRECTION('center_axis',(-1.,0.,0.));
#18931=DIRECTION('ref_axis',(0.,-1.,0.));
#18932=DIRECTION('',(0.,-1.,0.));
#18933=DIRECTION('',(0.,0.,1.));
#18934=DIRECTION('',(0.,1.,0.));
#18935=DIRECTION('',(0.,0.,1.));
#18936=DIRECTION('center_axis',(0.,0.,1.));
#18937=DIRECTION('ref_axis',(0.,1.,0.));
#18938=DIRECTION('center_axis',(0.,0.,1.));
#18939=DIRECTION('ref_axis',(0.,1.,0.));
#18940=DIRECTION('',(0.,0.,1.));
#18941=DIRECTION('center_axis',(0.,0.,-1.));
#18942=DIRECTION('ref_axis',(0.,1.,0.));
#18943=DIRECTION('center_axis',(0.,1.,0.));
#18944=DIRECTION('ref_axis',(-1.,0.,0.));
#18945=DIRECTION('',(-1.,0.,0.));
#18946=DIRECTION('',(0.,0.,1.));
#18947=DIRECTION('',(1.,0.,0.));
#18948=DIRECTION('center_axis',(0.,0.,1.));
#18949=DIRECTION('ref_axis',(1.,0.,0.));
#18950=DIRECTION('center_axis',(0.,0.,1.));
#18951=DIRECTION('ref_axis',(1.,0.,0.));
#18952=DIRECTION('',(0.,0.,1.));
#18953=DIRECTION('center_axis',(0.,0.,-1.));
#18954=DIRECTION('ref_axis',(1.,0.,0.));
#18955=DIRECTION('center_axis',(1.,0.,0.));
#18956=DIRECTION('ref_axis',(0.,1.,0.));
#18957=DIRECTION('',(0.,1.,0.));
#18958=DIRECTION('',(0.,0.,1.));
#18959=DIRECTION('',(0.,-1.,0.));
#18960=DIRECTION('center_axis',(0.,0.,1.));
#18961=DIRECTION('ref_axis',(2.96059473233373E-14,-1.,0.));
#18962=DIRECTION('center_axis',(0.,0.,1.));
#18963=DIRECTION('ref_axis',(2.96059473233373E-14,-1.,0.));
#18964=DIRECTION('',(0.,0.,1.));
#18965=DIRECTION('center_axis',(0.,0.,-1.));
#18966=DIRECTION('ref_axis',(2.96059473233373E-14,-1.,0.));
#18967=DIRECTION('center_axis',(0.,-1.,0.));
#18968=DIRECTION('ref_axis',(1.,0.,0.));
#18969=DIRECTION('',(1.,0.,0.));
#18970=DIRECTION('',(0.,0.,1.));
#18971=DIRECTION('',(-1.,0.,0.));
#18972=DIRECTION('center_axis',(0.,0.,1.));
#18973=DIRECTION('ref_axis',(-1.,2.22044604925036E-14,0.));
#18974=DIRECTION('center_axis',(0.,0.,1.));
#18975=DIRECTION('ref_axis',(-1.,2.22044604925036E-14,0.));
#18976=DIRECTION('center_axis',(0.,0.,-1.));
#18977=DIRECTION('ref_axis',(-1.,2.22044604925036E-14,0.));
#18978=DIRECTION('center_axis',(-1.,0.,0.));
#18979=DIRECTION('ref_axis',(0.,-1.,0.));
#18980=DIRECTION('',(0.,-1.,0.));
#18981=DIRECTION('',(0.,0.,1.));
#18982=DIRECTION('',(0.,1.,0.));
#18983=DIRECTION('',(0.,0.,1.));
#18984=DIRECTION('center_axis',(0.,0.,1.));
#18985=DIRECTION('ref_axis',(-2.96059473233373E-14,1.,0.));
#18986=DIRECTION('center_axis',(0.,0.,1.));
#18987=DIRECTION('ref_axis',(-2.96059473233373E-14,1.,0.));
#18988=DIRECTION('',(0.,0.,1.));
#18989=DIRECTION('center_axis',(0.,0.,-1.));
#18990=DIRECTION('ref_axis',(-2.96059473233373E-14,1.,0.));
#18991=DIRECTION('center_axis',(0.,1.,0.));
#18992=DIRECTION('ref_axis',(-1.,0.,0.));
#18993=DIRECTION('',(-1.,0.,0.));
#18994=DIRECTION('',(0.,0.,1.));
#18995=DIRECTION('',(1.,0.,0.));
#18996=DIRECTION('center_axis',(0.,0.,1.));
#18997=DIRECTION('ref_axis',(1.,0.,0.));
#18998=DIRECTION('center_axis',(0.,0.,1.));
#18999=DIRECTION('ref_axis',(1.,0.,0.));
#19000=DIRECTION('',(0.,0.,1.));
#19001=DIRECTION('center_axis',(0.,0.,-1.));
#19002=DIRECTION('ref_axis',(1.,0.,0.));
#19003=DIRECTION('center_axis',(1.,0.,0.));
#19004=DIRECTION('ref_axis',(0.,1.,0.));
#19005=DIRECTION('',(0.,1.,0.));
#19006=DIRECTION('',(0.,0.,1.));
#19007=DIRECTION('',(0.,-1.,0.));
#19008=DIRECTION('center_axis',(0.,0.,1.));
#19009=DIRECTION('ref_axis',(2.96059473233373E-14,-1.,0.));
#19010=DIRECTION('center_axis',(0.,0.,1.));
#19011=DIRECTION('ref_axis',(2.96059473233373E-14,-1.,0.));
#19012=DIRECTION('',(0.,0.,1.));
#19013=DIRECTION('center_axis',(0.,0.,-1.));
#19014=DIRECTION('ref_axis',(2.96059473233373E-14,-1.,0.));
#19015=DIRECTION('center_axis',(0.,-1.,0.));
#19016=DIRECTION('ref_axis',(1.,0.,0.));
#19017=DIRECTION('',(1.,0.,0.));
#19018=DIRECTION('',(0.,0.,1.));
#19019=DIRECTION('',(-1.,0.,0.));
#19020=DIRECTION('center_axis',(0.,0.,1.));
#19021=DIRECTION('ref_axis',(-1.,-7.40148683083432E-15,0.));
#19022=DIRECTION('center_axis',(0.,0.,1.));
#19023=DIRECTION('ref_axis',(-1.,-7.40148683083432E-15,0.));
#19024=DIRECTION('center_axis',(0.,0.,-1.));
#19025=DIRECTION('ref_axis',(-1.,-7.40148683083432E-15,0.));
#19026=DIRECTION('center_axis',(-1.,0.,0.));
#19027=DIRECTION('ref_axis',(0.,-1.,0.));
#19028=DIRECTION('',(0.,-1.,0.));
#19029=DIRECTION('',(0.,0.,1.));
#19030=DIRECTION('',(0.,1.,0.));
#19031=DIRECTION('',(0.,0.,1.));
#19032=DIRECTION('center_axis',(0.,0.,1.));
#19033=DIRECTION('ref_axis',(0.,1.,0.));
#19034=DIRECTION('center_axis',(0.,0.,1.));
#19035=DIRECTION('ref_axis',(0.,1.,0.));
#19036=DIRECTION('',(0.,0.,1.));
#19037=DIRECTION('center_axis',(0.,0.,-1.));
#19038=DIRECTION('ref_axis',(0.,1.,0.));
#19039=DIRECTION('center_axis',(0.,1.,0.));
#19040=DIRECTION('ref_axis',(-1.,0.,0.));
#19041=DIRECTION('',(-1.,0.,0.));
#19042=DIRECTION('',(0.,0.,1.));
#19043=DIRECTION('',(1.,0.,0.));
#19044=DIRECTION('center_axis',(0.,0.,1.));
#19045=DIRECTION('ref_axis',(1.,3.70074341541705E-14,0.));
#19046=DIRECTION('center_axis',(0.,0.,1.));
#19047=DIRECTION('ref_axis',(1.,3.70074341541705E-14,0.));
#19048=DIRECTION('',(0.,0.,1.));
#19049=DIRECTION('center_axis',(0.,0.,-1.));
#19050=DIRECTION('ref_axis',(1.,3.70074341541705E-14,0.));
#19051=DIRECTION('center_axis',(1.,0.,0.));
#19052=DIRECTION('ref_axis',(0.,1.,0.));
#19053=DIRECTION('',(0.,1.,0.));
#19054=DIRECTION('',(0.,0.,1.));
#19055=DIRECTION('',(0.,-1.,0.));
#19056=DIRECTION('center_axis',(0.,0.,1.));
#19057=DIRECTION('ref_axis',(0.,-1.,0.));
#19058=DIRECTION('center_axis',(0.,0.,1.));
#19059=DIRECTION('ref_axis',(0.,-1.,0.));
#19060=DIRECTION('',(0.,0.,1.));
#19061=DIRECTION('center_axis',(0.,0.,-1.));
#19062=DIRECTION('ref_axis',(0.,-1.,0.));
#19063=DIRECTION('center_axis',(0.,-1.,0.));
#19064=DIRECTION('ref_axis',(1.,0.,0.));
#19065=DIRECTION('',(1.,0.,0.));
#19066=DIRECTION('',(0.,0.,1.));
#19067=DIRECTION('',(-1.,0.,0.));
#19068=DIRECTION('center_axis',(0.,0.,1.));
#19069=DIRECTION('ref_axis',(-1.,-4.07081775695875E-14,0.));
#19070=DIRECTION('center_axis',(0.,0.,1.));
#19071=DIRECTION('ref_axis',(-1.,-4.07081775695875E-14,0.));
#19072=DIRECTION('center_axis',(0.,0.,-1.));
#19073=DIRECTION('ref_axis',(-1.,-4.07081775695875E-14,0.));
#19074=DIRECTION('center_axis',(-1.,0.,0.));
#19075=DIRECTION('ref_axis',(0.,-1.,0.));
#19076=DIRECTION('',(0.,-1.,0.));
#19077=DIRECTION('',(0.,0.,1.));
#19078=DIRECTION('',(0.,-1.,0.));
#19079=DIRECTION('',(0.,0.,1.));
#19080=DIRECTION('center_axis',(0.,0.,1.));
#19081=DIRECTION('ref_axis',(0.,1.,0.));
#19082=DIRECTION('center_axis',(0.,0.,1.));
#19083=DIRECTION('ref_axis',(0.,1.,0.));
#19084=DIRECTION('center_axis',(0.,0.,1.));
#19085=DIRECTION('ref_axis',(0.,1.,0.));
#19086=DIRECTION('',(0.,0.,1.));
#19087=DIRECTION('center_axis',(0.,1.,0.));
#19088=DIRECTION('ref_axis',(-1.,0.,0.));
#19089=DIRECTION('',(-1.,0.,0.));
#19090=DIRECTION('',(-1.,0.,0.));
#19091=DIRECTION('',(0.,0.,1.));
#19092=DIRECTION('center_axis',(0.,0.,1.));
#19093=DIRECTION('ref_axis',(1.,8.88178419700113E-15,0.));
#19094=DIRECTION('center_axis',(0.,0.,1.));
#19095=DIRECTION('ref_axis',(1.,8.88178419700113E-15,0.));
#19096=DIRECTION('center_axis',(0.,0.,1.));
#19097=DIRECTION('ref_axis',(1.,8.88178419700113E-15,0.));
#19098=DIRECTION('',(0.,0.,1.));
#19099=DIRECTION('center_axis',(1.,0.,0.));
#19100=DIRECTION('ref_axis',(0.,1.,0.));
#19101=DIRECTION('',(0.,1.,0.));
#19102=DIRECTION('',(0.,1.,0.));
#19103=DIRECTION('',(0.,0.,1.));
#19104=DIRECTION('center_axis',(0.,0.,1.));
#19105=DIRECTION('ref_axis',(0.,-1.,0.));
#19106=DIRECTION('center_axis',(0.,0.,1.));
#19107=DIRECTION('ref_axis',(0.,-1.,0.));
#19108=DIRECTION('center_axis',(0.,0.,1.));
#19109=DIRECTION('ref_axis',(0.,-1.,0.));
#19110=DIRECTION('',(0.,0.,1.));
#19111=DIRECTION('center_axis',(0.,-1.,0.));
#19112=DIRECTION('ref_axis',(1.,0.,0.));
#19113=DIRECTION('',(1.,0.,0.));
#19114=DIRECTION('',(1.,0.,0.));
#19115=DIRECTION('',(0.,0.,1.));
#19116=DIRECTION('center_axis',(0.,0.,1.));
#19117=DIRECTION('ref_axis',(-1.,-2.22044604925031E-15,0.));
#19118=DIRECTION('center_axis',(0.,0.,1.));
#19119=DIRECTION('ref_axis',(-1.,-2.22044604925031E-15,0.));
#19120=DIRECTION('center_axis',(0.,0.,1.));
#19121=DIRECTION('ref_axis',(-1.,-2.22044604925031E-15,0.));
#19122=DIRECTION('center_axis',(0.,0.,1.));
#19123=DIRECTION('ref_axis',(1.,0.,0.));
#19124=DIRECTION('center_axis',(0.,0.,1.));
#19125=DIRECTION('ref_axis',(1.,0.,0.));
#19126=DIRECTION('axis',(0.,0.,1.));
#19127=DIRECTION('refdir',(1.,0.,0.));
#19128=DIRECTION('center_axis',(0.,1.,0.));
#19129=DIRECTION('ref_axis',(0.,0.,1.));
#19130=DIRECTION('center_axis',(0.,-1.,0.));
#19131=DIRECTION('ref_axis',(1.,0.,0.));
#19132=DIRECTION('center_axis',(0.,-1.,0.));
#19133=DIRECTION('ref_axis',(1.,0.,0.));
#19134=DIRECTION('center_axis',(0.,-1.,0.));
#19135=DIRECTION('ref_axis',(1.,0.,0.));
#19136=DIRECTION('',(0.707106781186542,0.707106781186553,8.65956056235487E-17));
#19137=DIRECTION('center_axis',(0.,-1.,0.));
#19138=DIRECTION('ref_axis',(1.,0.,0.));
#19139=DIRECTION('center_axis',(0.,-1.,0.));
#19140=DIRECTION('ref_axis',(1.,0.,0.));
#19141=DIRECTION('',(0.,1.,0.));
#19142=DIRECTION('center_axis',(0.,1.,0.));
#19143=DIRECTION('ref_axis',(1.,0.,0.));
#19144=DIRECTION('',(0.707106781186537,-0.707106781186558,-8.65956056235481E-17));
#19145=DIRECTION('center_axis',(0.,-1.,0.));
#19146=DIRECTION('ref_axis',(1.,0.,0.));
#19147=DIRECTION('center_axis',(0.,-1.,0.));
#19148=DIRECTION('ref_axis',(0.,0.,-1.));
#19149=DIRECTION('axis',(0.,0.,1.));
#19150=DIRECTION('refdir',(1.,0.,0.));
#19151=DIRECTION('center_axis',(0.,0.,1.));
#19152=DIRECTION('ref_axis',(-0.0824405823441869,-0.996595981520471,0.));
#19153=DIRECTION('',(0.,0.,-1.));
#19154=DIRECTION('center_axis',(0.,0.,-1.));
#19155=DIRECTION('ref_axis',(1.,-2.89417707885741E-14,0.));
#19156=DIRECTION('center_axis',(0.,0.,1.));
#19157=DIRECTION('ref_axis',(-0.0824405823441869,-0.996595981520471,0.));
#19158=DIRECTION('',(0.,0.,-1.));
#19159=DIRECTION('center_axis',(0.,0.,1.));
#19160=DIRECTION('ref_axis',(-0.0824405823441869,-0.996595981520471,0.));
#19161=DIRECTION('',(0.,0.,-1.));
#19162=DIRECTION('center_axis',(0.,0.,1.));
#19163=DIRECTION('ref_axis',(-0.0824405823441869,-0.996595981520471,0.));
#19164=DIRECTION('',(0.,0.,-1.));
#19165=DIRECTION('center_axis',(0.,0.,1.));
#19166=DIRECTION('ref_axis',(-0.0824405823441869,-0.996595981520471,0.));
#19167=DIRECTION('',(0.,0.,-1.));
#19168=DIRECTION('center_axis',(0.,0.,1.));
#19169=DIRECTION('ref_axis',(-0.0824405823441869,-0.996595981520471,0.));
#19170=DIRECTION('',(0.,0.,-1.));
#19171=DIRECTION('center_axis',(0.,0.,1.));
#19172=DIRECTION('ref_axis',(-0.0824405823441869,-0.996595981520471,0.));
#19173=DIRECTION('',(0.,0.,-1.));
#19174=DIRECTION('center_axis',(0.,0.,1.));
#19175=DIRECTION('ref_axis',(-0.0824405823441869,-0.996595981520471,0.));
#19176=DIRECTION('',(0.,0.,-1.));
#19177=DIRECTION('center_axis',(0.,0.,1.));
#19178=DIRECTION('ref_axis',(-0.0824405823441869,-0.996595981520471,0.));
#19179=DIRECTION('',(0.,0.,-1.));
#19180=DIRECTION('center_axis',(0.,0.,1.));
#19181=DIRECTION('ref_axis',(-0.0824405823441869,-0.996595981520471,0.));
#19182=DIRECTION('',(0.,0.,-1.));
#19183=DIRECTION('center_axis',(0.,0.,1.));
#19184=DIRECTION('ref_axis',(-0.0824405823441869,-0.996595981520471,0.));
#19185=DIRECTION('',(0.,0.,-1.));
#19186=DIRECTION('center_axis',(0.,0.,1.));
#19187=DIRECTION('ref_axis',(-0.0824405823441869,-0.996595981520471,0.));
#19188=DIRECTION('',(0.,0.,-1.));
#19189=DIRECTION('center_axis',(0.,0.,1.));
#19190=DIRECTION('ref_axis',(-0.0824405823441869,-0.996595981520471,0.));
#19191=DIRECTION('',(0.,0.,-1.));
#19192=DIRECTION('center_axis',(0.,0.,1.));
#19193=DIRECTION('ref_axis',(-0.0824405823441869,-0.996595981520471,0.));
#19194=DIRECTION('',(0.,0.,-1.));
#19195=DIRECTION('center_axis',(0.,0.,1.));
#19196=DIRECTION('ref_axis',(-0.0824405823441869,-0.996595981520471,0.));
#19197=DIRECTION('',(0.,0.,-1.));
#19198=DIRECTION('center_axis',(0.,0.,1.));
#19199=DIRECTION('ref_axis',(-0.0824405823441869,-0.996595981520471,0.));
#19200=DIRECTION('',(0.,0.,-1.));
#19201=DIRECTION('center_axis',(0.,0.,1.));
#19202=DIRECTION('ref_axis',(-0.0824405823441869,-0.996595981520471,0.));
#19203=DIRECTION('',(0.,0.,-1.));
#19204=DIRECTION('center_axis',(0.,0.,1.));
#19205=DIRECTION('ref_axis',(-0.0824405823441869,-0.996595981520471,0.));
#19206=DIRECTION('',(0.,0.,-1.));
#19207=DIRECTION('center_axis',(0.,0.,1.));
#19208=DIRECTION('ref_axis',(-0.0824405823441869,-0.996595981520471,0.));
#19209=DIRECTION('',(0.,0.,-1.));
#19210=DIRECTION('center_axis',(0.,0.,1.));
#19211=DIRECTION('ref_axis',(-0.0824405823441869,-0.996595981520471,0.));
#19212=DIRECTION('',(0.,0.,-1.));
#19213=DIRECTION('center_axis',(0.,0.,1.));
#19214=DIRECTION('ref_axis',(-0.0824405823441869,-0.996595981520471,0.));
#19215=DIRECTION('',(0.,0.,-1.));
#19216=DIRECTION('center_axis',(0.,0.,1.));
#19217=DIRECTION('ref_axis',(-0.0824405823441869,-0.996595981520471,0.));
#19218=DIRECTION('',(0.,0.,-1.));
#19219=DIRECTION('center_axis',(0.,0.,1.));
#19220=DIRECTION('ref_axis',(-0.0824405823441869,-0.996595981520471,0.));
#19221=DIRECTION('',(0.,0.,-1.));
#19222=DIRECTION('center_axis',(0.,0.,1.));
#19223=DIRECTION('ref_axis',(-0.0824405823441869,-0.996595981520471,0.));
#19224=DIRECTION('',(0.,0.,-1.));
#19225=DIRECTION('center_axis',(0.,0.,1.));
#19226=DIRECTION('ref_axis',(1.,0.,0.));
#19227=DIRECTION('center_axis',(0.,0.,-1.));
#19228=DIRECTION('ref_axis',(1.,0.,0.));
#19229=DIRECTION('center_axis',(0.,0.,1.));
#19230=DIRECTION('ref_axis',(1.,0.,0.));
#19231=DIRECTION('center_axis',(0.,0.,1.));
#19232=DIRECTION('ref_axis',(-0.0824405823441869,-0.996595981520471,0.));
#19233=DIRECTION('center_axis',(0.,0.,1.));
#19234=DIRECTION('ref_axis',(1.,-2.89417707885741E-14,0.));
#19235=DIRECTION('center_axis',(0.,0.,1.));
#19236=DIRECTION('ref_axis',(1.,0.,0.));
#19237=DIRECTION('center_axis',(0.,0.,1.));
#19238=DIRECTION('ref_axis',(1.,0.,0.));
#19239=DIRECTION('center_axis',(0.,0.,1.));
#19240=DIRECTION('ref_axis',(1.,0.,0.));
#19241=DIRECTION('center_axis',(0.,0.,1.));
#19242=DIRECTION('ref_axis',(1.,0.,0.));
#19243=DIRECTION('center_axis',(0.,0.,-1.));
#19244=DIRECTION('ref_axis',(1.,0.,0.));
#19245=DIRECTION('center_axis',(0.,0.,-1.));
#19246=DIRECTION('ref_axis',(1.,0.,0.));
#19247=DIRECTION('center_axis',(0.,0.,-1.));
#19248=DIRECTION('ref_axis',(-1.,0.,0.));
#19249=DIRECTION('center_axis',(0.,0.,1.));
#19250=DIRECTION('ref_axis',(1.,0.,0.));
#19251=DIRECTION('center_axis',(0.,1.,0.));
#19252=DIRECTION('ref_axis',(1.,0.,0.));
#19253=DIRECTION('center_axis',(0.,0.,1.));
#19254=DIRECTION('ref_axis',(1.,0.,0.));
#19255=DIRECTION('center_axis',(0.,0.,-1.));
#19256=DIRECTION('ref_axis',(1.,0.,0.));
#19257=DIRECTION('center_axis',(0.,0.,-1.));
#19258=DIRECTION('ref_axis',(1.,0.,0.));
#19259=DIRECTION('',(0.707106781186547,-8.65956056235493E-17,0.707106781186548));
#19260=DIRECTION('center_axis',(0.,0.,-1.));
#19261=DIRECTION('ref_axis',(1.,0.,0.));
#19262=DIRECTION('center_axis',(0.,0.,1.));
#19263=DIRECTION('ref_axis',(1.,0.,0.));
#19264=DIRECTION('center_axis',(0.,0.,1.));
#19265=DIRECTION('ref_axis',(0.984807753012208,-0.17364817766693,0.));
#19266=DIRECTION('center_axis',(0.,0.,1.));
#19267=DIRECTION('ref_axis',(1.,0.,0.));
#19268=DIRECTION('',(0.808467844782638,-0.588540350318069,0.));
#19269=DIRECTION('',(-0.961003922853658,-0.276534736081891,0.));
#19270=DIRECTION('center_axis',(-0.276534736081891,0.961003922853658,0.));
#19271=DIRECTION('ref_axis',(-0.961003922853658,-0.276534736081891,0.));
#19272=DIRECTION('',(0.,0.,-1.));
#19273=DIRECTION('',(0.,0.,1.));
#19274=DIRECTION('center_axis',(-0.58854035031807,-0.808467844782638,0.));
#19275=DIRECTION('ref_axis',(0.808467844782638,-0.58854035031807,0.));
#19276=DIRECTION('',(0.,0.,1.));
#19277=DIRECTION('center_axis',(0.,0.,-1.));
#19278=DIRECTION('ref_axis',(1.,0.,0.));
#19279=DIRECTION('center_axis',(0.,0.,1.));
#19280=DIRECTION('ref_axis',(1.,0.,0.));
#19281=DIRECTION('',(0.,0.,1.));
#19282=DIRECTION('center_axis',(0.,0.,1.));
#19283=DIRECTION('ref_axis',(1.,0.,0.));
#19284=DIRECTION('center_axis',(0.,0.,1.));
#19285=DIRECTION('ref_axis',(1.,0.,0.));
#19286=DIRECTION('',(0.,0.,-1.));
#19287=DIRECTION('center_axis',(0.,0.,-1.));
#19288=DIRECTION('ref_axis',(1.,0.,0.));
#19289=DIRECTION('',(0.,0.,1.));
#19290=DIRECTION('center_axis',(0.,0.,1.));
#19291=DIRECTION('ref_axis',(1.,0.,0.));
#19292=DIRECTION('',(0.,0.,-1.));
#19293=DIRECTION('center_axis',(0.,0.,-1.));
#19294=DIRECTION('ref_axis',(1.,0.,0.));
#19295=DIRECTION('',(0.,0.,1.));
#19296=DIRECTION('center_axis',(0.,0.,1.));
#19297=DIRECTION('ref_axis',(1.,0.,0.));
#19298=DIRECTION('',(0.,0.,-1.));
#19299=DIRECTION('center_axis',(0.,0.,-1.));
#19300=DIRECTION('ref_axis',(1.,0.,0.));
#19301=DIRECTION('',(0.,0.,1.));
#19302=DIRECTION('center_axis',(0.,0.,1.));
#19303=DIRECTION('ref_axis',(1.,0.,0.));
#19304=DIRECTION('',(0.,0.,-1.));
#19305=DIRECTION('center_axis',(0.,0.,-1.));
#19306=DIRECTION('ref_axis',(1.,0.,0.));
#19307=DIRECTION('',(0.,0.,1.));
#19308=DIRECTION('center_axis',(0.,0.,1.));
#19309=DIRECTION('ref_axis',(1.,0.,0.));
#19310=DIRECTION('',(0.,0.,-1.));
#19311=DIRECTION('center_axis',(0.,0.,-1.));
#19312=DIRECTION('ref_axis',(1.,0.,0.));
#19313=DIRECTION('',(0.,0.,1.));
#19314=DIRECTION('center_axis',(0.,0.,1.));
#19315=DIRECTION('ref_axis',(1.,0.,0.));
#19316=DIRECTION('',(0.,0.,-1.));
#19317=DIRECTION('center_axis',(0.,0.,-1.));
#19318=DIRECTION('ref_axis',(1.,0.,0.));
#19319=DIRECTION('',(0.,0.,1.));
#19320=DIRECTION('center_axis',(0.,0.,1.));
#19321=DIRECTION('ref_axis',(1.,0.,0.));
#19322=DIRECTION('',(0.,0.,-1.));
#19323=DIRECTION('center_axis',(0.,0.,-1.));
#19324=DIRECTION('ref_axis',(1.,0.,0.));
#19325=DIRECTION('',(0.,0.,1.));
#19326=DIRECTION('center_axis',(0.,0.,1.));
#19327=DIRECTION('ref_axis',(1.,0.,0.));
#19328=DIRECTION('',(0.,0.,-1.));
#19329=DIRECTION('center_axis',(0.,0.,-1.));
#19330=DIRECTION('ref_axis',(1.,0.,0.));
#19331=DIRECTION('',(0.,0.,1.));
#19332=DIRECTION('center_axis',(0.,0.,1.));
#19333=DIRECTION('ref_axis',(1.,0.,0.));
#19334=DIRECTION('',(0.,0.,-1.));
#19335=DIRECTION('center_axis',(0.,0.,-1.));
#19336=DIRECTION('ref_axis',(1.,0.,0.));
#19337=DIRECTION('',(0.,0.,1.));
#19338=DIRECTION('center_axis',(0.,0.,1.));
#19339=DIRECTION('ref_axis',(1.,0.,0.));
#19340=DIRECTION('',(0.,0.,-1.));
#19341=DIRECTION('center_axis',(0.,0.,-1.));
#19342=DIRECTION('ref_axis',(1.,0.,0.));
#19343=DIRECTION('',(0.,0.,1.));
#19344=DIRECTION('center_axis',(0.,0.,1.));
#19345=DIRECTION('ref_axis',(1.,0.,0.));
#19346=DIRECTION('',(0.,0.,-1.));
#19347=DIRECTION('center_axis',(0.,0.,-1.));
#19348=DIRECTION('ref_axis',(1.,0.,0.));
#19349=DIRECTION('',(0.,0.,1.));
#19350=DIRECTION('center_axis',(0.,0.,1.));
#19351=DIRECTION('ref_axis',(1.,0.,0.));
#19352=DIRECTION('',(0.,0.,-1.));
#19353=DIRECTION('center_axis',(0.,0.,-1.));
#19354=DIRECTION('ref_axis',(1.,0.,0.));
#19355=DIRECTION('',(0.,0.,1.));
#19356=DIRECTION('center_axis',(0.,0.,1.));
#19357=DIRECTION('ref_axis',(1.,0.,0.));
#19358=DIRECTION('',(0.,0.,-1.));
#19359=DIRECTION('center_axis',(0.,0.,-1.));
#19360=DIRECTION('ref_axis',(1.,0.,0.));
#19361=DIRECTION('',(0.,0.,1.));
#19362=DIRECTION('center_axis',(0.,0.,1.));
#19363=DIRECTION('ref_axis',(1.,0.,0.));
#19364=DIRECTION('',(0.,0.,-1.));
#19365=DIRECTION('center_axis',(0.,0.,-1.));
#19366=DIRECTION('ref_axis',(1.,0.,0.));
#19367=DIRECTION('',(0.,0.,1.));
#19368=DIRECTION('center_axis',(0.,0.,1.));
#19369=DIRECTION('ref_axis',(1.,0.,0.));
#19370=DIRECTION('',(0.,0.,-1.));
#19371=DIRECTION('center_axis',(0.,0.,-1.));
#19372=DIRECTION('ref_axis',(1.,0.,0.));
#19373=DIRECTION('',(0.,0.,1.));
#19374=DIRECTION('center_axis',(0.,0.,1.));
#19375=DIRECTION('ref_axis',(1.,0.,0.));
#19376=DIRECTION('',(0.,0.,-1.));
#19377=DIRECTION('center_axis',(0.,0.,-1.));
#19378=DIRECTION('ref_axis',(1.,0.,0.));
#19379=DIRECTION('',(0.,0.,1.));
#19380=DIRECTION('center_axis',(0.,0.,1.));
#19381=DIRECTION('ref_axis',(1.,0.,0.));
#19382=DIRECTION('',(0.,0.,-1.));
#19383=DIRECTION('center_axis',(0.,0.,-1.));
#19384=DIRECTION('ref_axis',(1.,0.,0.));
#19385=DIRECTION('center_axis',(0.,0.,-1.));
#19386=DIRECTION('ref_axis',(1.,0.,0.));
#19387=DIRECTION('',(0.,0.,1.));
#19388=DIRECTION('center_axis',(0.,0.,1.));
#19389=DIRECTION('ref_axis',(1.,0.,0.));
#19390=DIRECTION('',(0.,0.,-1.));
#19391=DIRECTION('center_axis',(0.,0.,-1.));
#19392=DIRECTION('ref_axis',(1.,0.,0.));
#19393=DIRECTION('',(0.,0.,1.));
#19394=DIRECTION('center_axis',(0.,0.,1.));
#19395=DIRECTION('ref_axis',(1.,0.,0.));
#19396=DIRECTION('',(0.,0.,-1.));
#19397=DIRECTION('center_axis',(0.,0.,-1.));
#19398=DIRECTION('ref_axis',(1.,0.,0.));
#19399=DIRECTION('',(0.,0.,1.));
#19400=DIRECTION('center_axis',(0.,0.,1.));
#19401=DIRECTION('ref_axis',(1.,0.,0.));
#19402=DIRECTION('',(0.,0.,-1.));
#19403=DIRECTION('center_axis',(0.,0.,-1.));
#19404=DIRECTION('ref_axis',(1.,0.,0.));
#19405=DIRECTION('',(0.,0.,1.));
#19406=DIRECTION('center_axis',(0.,0.,1.));
#19407=DIRECTION('ref_axis',(1.,0.,0.));
#19408=DIRECTION('',(0.,0.,-1.));
#19409=DIRECTION('center_axis',(0.,0.,-1.));
#19410=DIRECTION('ref_axis',(1.,0.,0.));
#19411=DIRECTION('',(0.,0.,1.));
#19412=DIRECTION('center_axis',(0.,0.,1.));
#19413=DIRECTION('ref_axis',(1.,0.,0.));
#19414=DIRECTION('',(0.,0.,-1.));
#19415=DIRECTION('center_axis',(0.,0.,-1.));
#19416=DIRECTION('ref_axis',(1.,0.,0.));
#19417=DIRECTION('',(0.,0.,1.));
#19418=DIRECTION('center_axis',(0.,0.,1.));
#19419=DIRECTION('ref_axis',(1.,0.,0.));
#19420=DIRECTION('',(0.,0.,-1.));
#19421=DIRECTION('center_axis',(0.,0.,-1.));
#19422=DIRECTION('ref_axis',(1.,0.,0.));
#19423=DIRECTION('',(0.,0.,1.));
#19424=DIRECTION('center_axis',(0.,0.,1.));
#19425=DIRECTION('ref_axis',(1.,0.,0.));
#19426=DIRECTION('',(0.,0.,-1.));
#19427=DIRECTION('center_axis',(0.,0.,-1.));
#19428=DIRECTION('ref_axis',(1.,0.,0.));
#19429=DIRECTION('',(0.,0.,1.));
#19430=DIRECTION('center_axis',(0.,0.,1.));
#19431=DIRECTION('ref_axis',(1.,0.,0.));
#19432=DIRECTION('',(0.,0.,-1.));
#19433=DIRECTION('center_axis',(0.,0.,-1.));
#19434=DIRECTION('ref_axis',(1.,0.,0.));
#19435=DIRECTION('',(0.,0.,1.));
#19436=DIRECTION('center_axis',(0.,0.,1.));
#19437=DIRECTION('ref_axis',(1.,0.,0.));
#19438=DIRECTION('',(0.,0.,-1.));
#19439=DIRECTION('center_axis',(0.,0.,-1.));
#19440=DIRECTION('ref_axis',(1.,0.,0.));
#19441=DIRECTION('',(0.,0.,1.));
#19442=DIRECTION('center_axis',(0.,0.,1.));
#19443=DIRECTION('ref_axis',(1.,0.,0.));
#19444=DIRECTION('',(0.,0.,-1.));
#19445=DIRECTION('center_axis',(0.,0.,-1.));
#19446=DIRECTION('ref_axis',(1.,0.,0.));
#19447=DIRECTION('',(0.,0.,1.));
#19448=DIRECTION('center_axis',(0.,0.,1.));
#19449=DIRECTION('ref_axis',(1.,0.,0.));
#19450=DIRECTION('',(0.,0.,-1.));
#19451=DIRECTION('center_axis',(0.,0.,-1.));
#19452=DIRECTION('ref_axis',(1.,0.,0.));
#19453=DIRECTION('',(0.,0.,1.));
#19454=DIRECTION('center_axis',(0.,0.,1.));
#19455=DIRECTION('ref_axis',(1.,0.,0.));
#19456=DIRECTION('',(0.,0.,-1.));
#19457=DIRECTION('center_axis',(0.,0.,-1.));
#19458=DIRECTION('ref_axis',(1.,0.,0.));
#19459=DIRECTION('',(0.,0.,1.));
#19460=DIRECTION('center_axis',(0.,0.,1.));
#19461=DIRECTION('ref_axis',(1.,0.,0.));
#19462=DIRECTION('',(0.,0.,-1.));
#19463=DIRECTION('center_axis',(0.,0.,-1.));
#19464=DIRECTION('ref_axis',(1.,0.,0.));
#19465=DIRECTION('',(0.,0.,1.));
#19466=DIRECTION('center_axis',(0.,0.,1.));
#19467=DIRECTION('ref_axis',(1.,0.,0.));
#19468=DIRECTION('',(0.,0.,-1.));
#19469=DIRECTION('center_axis',(0.,0.,-1.));
#19470=DIRECTION('ref_axis',(1.,0.,0.));
#19471=DIRECTION('',(0.,0.,1.));
#19472=DIRECTION('center_axis',(0.,0.,1.));
#19473=DIRECTION('ref_axis',(1.,0.,0.));
#19474=DIRECTION('',(0.,0.,-1.));
#19475=DIRECTION('center_axis',(0.,0.,-1.));
#19476=DIRECTION('ref_axis',(1.,0.,0.));
#19477=DIRECTION('',(0.,0.,1.));
#19478=DIRECTION('center_axis',(0.,0.,1.));
#19479=DIRECTION('ref_axis',(1.,0.,0.));
#19480=DIRECTION('',(0.,0.,-1.));
#19481=DIRECTION('center_axis',(0.,0.,-1.));
#19482=DIRECTION('ref_axis',(1.,0.,0.));
#19483=DIRECTION('',(0.,0.,1.));
#19484=DIRECTION('center_axis',(0.,0.,1.));
#19485=DIRECTION('ref_axis',(1.,0.,0.));
#19486=DIRECTION('',(0.,0.,-1.));
#19487=DIRECTION('center_axis',(0.,0.,-1.));
#19488=DIRECTION('ref_axis',(1.,0.,0.));
#19489=DIRECTION('',(0.,0.,1.));
#19490=DIRECTION('center_axis',(0.,0.,1.));
#19491=DIRECTION('ref_axis',(1.,0.,0.));
#19492=DIRECTION('',(0.,0.,-1.));
#19493=DIRECTION('center_axis',(0.,0.,-1.));
#19494=DIRECTION('ref_axis',(1.,0.,0.));
#19495=DIRECTION('',(0.,0.,1.));
#19496=DIRECTION('center_axis',(-0.105456972136321,0.994423866883654,0.));
#19497=DIRECTION('ref_axis',(-0.994423866883654,-0.105456972136321,0.));
#19498=DIRECTION('',(-0.994423866883654,-0.105456972136321,0.));
#19499=DIRECTION('',(0.,0.,1.));
#19500=DIRECTION('center_axis',(-0.719988067902572,-0.693986442286822,0.));
#19501=DIRECTION('ref_axis',(0.693986442286822,-0.719988067902572,0.));
#19502=DIRECTION('',(0.693986442286822,-0.719988067902572,0.));
#19503=DIRECTION('center_axis',(0.,0.,1.));
#19504=DIRECTION('ref_axis',(0.939692620785908,-0.342020143325669,0.));
#19505=DIRECTION('center_axis',(0.,0.,1.));
#19506=DIRECTION('ref_axis',(1.,0.,0.));
#19507=DIRECTION('',(0.707106781186547,8.65956056235493E-17,-0.707106781186548));
#19508=DIRECTION('center_axis',(0.,0.,1.));
#19509=DIRECTION('ref_axis',(1.,0.,0.));
#19510=DIRECTION('center_axis',(0.,0.,1.));
#19511=DIRECTION('ref_axis',(0.866025403784438,-0.5,0.));
#19512=DIRECTION('',(0.558418612916207,-0.829559312375396,0.));
#19513=DIRECTION('',(-0.997628744921147,0.0688250485438069,0.));
#19514=DIRECTION('center_axis',(0.0688250485438069,0.997628744921147,0.));
#19515=DIRECTION('ref_axis',(-0.997628744921147,0.0688250485438069,0.));
#19516=DIRECTION('',(0.,0.,1.));
#19517=DIRECTION('center_axis',(-0.829559312375396,-0.558418612916207,0.));
#19518=DIRECTION('ref_axis',(0.558418612916207,-0.829559312375396,0.));
#19519=DIRECTION('center_axis',(0.241015854951086,0.970521178368714,0.));
#19520=DIRECTION('ref_axis',(-0.970521178368714,0.241015854951086,0.));
#19521=DIRECTION('',(-0.970521178368714,0.241015854951086,0.));
#19522=DIRECTION('',(0.,0.,1.));
#19523=DIRECTION('center_axis',(-0.91392481691896,-0.405883516565584,0.));
#19524=DIRECTION('ref_axis',(0.405883516565584,-0.91392481691896,0.));
#19525=DIRECTION('',(0.405883516565584,-0.91392481691896,0.));
#19526=DIRECTION('center_axis',(0.,0.,1.));
#19527=DIRECTION('ref_axis',(0.766044443118978,-0.64278760968654,0.));
#19528=DIRECTION('center_axis',(0.,0.,1.));
#19529=DIRECTION('ref_axis',(0.642787609686539,-0.766044443118978,0.));
#19530=DIRECTION('',(0.241015854951086,-0.970521178368714,0.));
#19531=DIRECTION('',(-0.91392481691896,0.405883516565585,0.));
#19532=DIRECTION('center_axis',(0.405883516565585,0.91392481691896,0.));
#19533=DIRECTION('ref_axis',(-0.91392481691896,0.405883516565585,0.));
#19534=DIRECTION('',(0.,0.,1.));
#19535=DIRECTION('center_axis',(-0.970521178368714,-0.241015854951086,0.));
#19536=DIRECTION('ref_axis',(0.241015854951086,-0.970521178368714,0.));
#19537=DIRECTION('center_axis',(0.558418612916207,0.829559312375396,0.));
#19538=DIRECTION('ref_axis',(-0.829559312375396,0.558418612916207,0.));
#19539=DIRECTION('',(-0.829559312375396,0.558418612916207,0.));
#19540=DIRECTION('',(0.,0.,1.));
#19541=DIRECTION('center_axis',(-0.997628744921147,-0.0688250485438065,
0.));
#19542=DIRECTION('ref_axis',(0.0688250485438065,-0.997628744921147,0.));
#19543=DIRECTION('',(0.0688250485438065,-0.997628744921147,0.));
#19544=DIRECTION('center_axis',(0.,0.,1.));
#19545=DIRECTION('ref_axis',(0.5,-0.866025403784439,0.));
#19546=DIRECTION('center_axis',(0.,0.,1.));
#19547=DIRECTION('ref_axis',(0.342020143325668,-0.939692620785909,0.));
#19548=DIRECTION('',(-0.105456972136323,-0.994423866883654,0.));
#19549=DIRECTION('',(-0.719988067902571,0.693986442286823,0.));
#19550=DIRECTION('center_axis',(0.693986442286823,0.719988067902571,0.));
#19551=DIRECTION('ref_axis',(-0.719988067902571,0.693986442286823,0.));
#19552=DIRECTION('',(0.,0.,1.));
#19553=DIRECTION('center_axis',(-0.994423866883654,0.105456972136322,0.));
#19554=DIRECTION('ref_axis',(-0.105456972136322,-0.994423866883654,0.));
#19555=DIRECTION('center_axis',(0.808467844782639,0.588540350318069,0.));
#19556=DIRECTION('ref_axis',(-0.588540350318069,0.808467844782639,0.));
#19557=DIRECTION('',(-0.588540350318069,0.808467844782638,0.));
#19558=DIRECTION('',(0.,0.,1.));
#19559=DIRECTION('center_axis',(-0.961003922853658,0.276534736081891,0.));
#19560=DIRECTION('ref_axis',(-0.276534736081891,-0.961003922853658,0.));
#19561=DIRECTION('',(-0.276534736081891,-0.961003922853658,0.));
#19562=DIRECTION('center_axis',(0.,0.,1.));
#19563=DIRECTION('ref_axis',(0.17364817766693,-0.984807753012208,0.));
#19564=DIRECTION('center_axis',(0.,0.,1.));
#19565=DIRECTION('ref_axis',(-1.83697019872103E-16,-1.,0.));
#19566=DIRECTION('',(-0.43921013200494,-0.898384360919202,0.));
#19567=DIRECTION('',(-0.43921013200494,0.898384360919202,0.));
#19568=DIRECTION('center_axis',(0.898384360919202,0.43921013200494,0.));
#19569=DIRECTION('ref_axis',(-0.43921013200494,0.898384360919202,0.));
#19570=DIRECTION('',(0.,0.,1.));
#19571=DIRECTION('center_axis',(-0.898384360919202,0.43921013200494,0.));
#19572=DIRECTION('ref_axis',(-0.43921013200494,-0.898384360919202,0.));
#19573=DIRECTION('center_axis',(0.961003922853658,0.276534736081891,0.));
#19574=DIRECTION('ref_axis',(-0.276534736081891,0.961003922853658,0.));
#19575=DIRECTION('',(-0.276534736081891,0.961003922853658,0.));
#19576=DIRECTION('',(0.,0.,1.));
#19577=DIRECTION('center_axis',(-0.808467844782638,0.58854035031807,0.));
#19578=DIRECTION('ref_axis',(-0.58854035031807,-0.808467844782638,0.));
#19579=DIRECTION('',(-0.588540350318069,-0.808467844782638,0.));
#19580=DIRECTION('center_axis',(0.,0.,1.));
#19581=DIRECTION('ref_axis',(-0.17364817766693,-0.984807753012208,0.));
#19582=DIRECTION('center_axis',(0.,0.,1.));
#19583=DIRECTION('ref_axis',(-0.342020143325669,-0.939692620785908,0.));
#19584=DIRECTION('',(-0.719988067902572,-0.693986442286823,0.));
#19585=DIRECTION('',(-0.105456972136321,0.994423866883654,0.));
#19586=DIRECTION('center_axis',(0.994423866883654,0.105456972136321,0.));
#19587=DIRECTION('ref_axis',(-0.105456972136321,0.994423866883654,0.));
#19588=DIRECTION('',(0.,0.,1.));
#19589=DIRECTION('center_axis',(-0.693986442286823,0.719988067902572,0.));
#19590=DIRECTION('ref_axis',(-0.719988067902572,-0.693986442286823,0.));
#19591=DIRECTION('center_axis',(0.997628744921147,-0.0688250485438069,0.));
#19592=DIRECTION('ref_axis',(0.0688250485438069,0.997628744921147,0.));
#19593=DIRECTION('',(0.0688250485438069,0.997628744921147,0.));
#19594=DIRECTION('',(0.,0.,1.));
#19595=DIRECTION('center_axis',(-0.558418612916207,0.829559312375396,0.));
#19596=DIRECTION('ref_axis',(-0.829559312375396,-0.558418612916207,0.));
#19597=DIRECTION('',(-0.829559312375396,-0.558418612916207,0.));
#19598=DIRECTION('center_axis',(0.,0.,1.));
#19599=DIRECTION('ref_axis',(-0.5,-0.866025403784438,0.));
#19600=DIRECTION('center_axis',(0.,0.,1.));
#19601=DIRECTION('ref_axis',(-0.642787609686539,-0.766044443118978,0.));
#19602=DIRECTION('',(-0.91392481691896,-0.405883516565584,0.));
#19603=DIRECTION('',(0.241015854951086,0.970521178368714,0.));
#19604=DIRECTION('center_axis',(0.970521178368714,-0.241015854951086,0.));
#19605=DIRECTION('ref_axis',(0.241015854951086,0.970521178368714,0.));
#19606=DIRECTION('',(0.,0.,1.));
#19607=DIRECTION('center_axis',(-0.405883516565584,0.91392481691896,0.));
#19608=DIRECTION('ref_axis',(-0.91392481691896,-0.405883516565584,0.));
#19609=DIRECTION('center_axis',(0.91392481691896,-0.405883516565585,0.));
#19610=DIRECTION('ref_axis',(0.405883516565585,0.91392481691896,0.));
#19611=DIRECTION('',(0.405883516565584,0.91392481691896,0.));
#19612=DIRECTION('',(0.,0.,1.));
#19613=DIRECTION('center_axis',(-0.241015854951086,0.970521178368714,0.));
#19614=DIRECTION('ref_axis',(-0.970521178368714,-0.241015854951086,0.));
#19615=DIRECTION('',(-0.970521178368714,-0.241015854951086,0.));
#19616=DIRECTION('center_axis',(0.,0.,1.));
#19617=DIRECTION('ref_axis',(-0.766044443118978,-0.642787609686539,0.));
#19618=DIRECTION('center_axis',(0.,0.,1.));
#19619=DIRECTION('ref_axis',(-0.866025403784439,-0.5,0.));
#19620=DIRECTION('',(-0.997628744921147,-0.0688250485438061,0.));
#19621=DIRECTION('',(0.558418612916207,0.829559312375396,0.));
#19622=DIRECTION('center_axis',(0.829559312375396,-0.558418612916207,0.));
#19623=DIRECTION('ref_axis',(0.558418612916207,0.829559312375396,0.));
#19624=DIRECTION('',(0.,0.,1.));
#19625=DIRECTION('center_axis',(-0.0688250485438061,0.997628744921147,0.));
#19626=DIRECTION('ref_axis',(-0.997628744921147,-0.0688250485438061,0.));
#19627=DIRECTION('center_axis',(0.719988067902572,-0.693986442286823,0.));
#19628=DIRECTION('ref_axis',(0.693986442286823,0.719988067902572,0.));
#19629=DIRECTION('',(0.693986442286823,0.719988067902572,0.));
#19630=DIRECTION('',(0.,0.,1.));
#19631=DIRECTION('center_axis',(0.105456972136322,0.994423866883654,0.));
#19632=DIRECTION('ref_axis',(-0.994423866883654,0.105456972136322,0.));
#19633=DIRECTION('',(-0.994423866883654,0.105456972136322,0.));
#19634=DIRECTION('center_axis',(0.,0.,1.));
#19635=DIRECTION('ref_axis',(-0.939692620785908,-0.342020143325669,0.));
#19636=DIRECTION('center_axis',(0.,0.,1.));
#19637=DIRECTION('ref_axis',(-0.984807753012208,-0.17364817766693,0.));
#19638=DIRECTION('',(-0.961003922853658,0.276534736081891,0.));
#19639=DIRECTION('',(0.808467844782638,0.588540350318069,0.));
#19640=DIRECTION('center_axis',(0.588540350318069,-0.808467844782638,0.));
#19641=DIRECTION('ref_axis',(0.808467844782639,0.588540350318069,0.));
#19642=DIRECTION('',(0.,0.,1.));
#19643=DIRECTION('center_axis',(0.276534736081891,0.961003922853658,0.));
#19644=DIRECTION('ref_axis',(-0.961003922853658,0.276534736081891,0.));
#19645=DIRECTION('center_axis',(0.43921013200494,-0.898384360919202,0.));
#19646=DIRECTION('ref_axis',(0.898384360919202,0.43921013200494,0.));
#19647=DIRECTION('',(0.898384360919202,0.43921013200494,0.));
#19648=DIRECTION('',(0.,0.,1.));
#19649=DIRECTION('center_axis',(0.43921013200494,0.898384360919202,0.));
#19650=DIRECTION('ref_axis',(-0.898384360919202,0.43921013200494,0.));
#19651=DIRECTION('',(-0.898384360919202,0.43921013200494,0.));
#19652=DIRECTION('center_axis',(0.,0.,1.));
#19653=DIRECTION('ref_axis',(-1.,1.22464679914735E-16,0.));
#19654=DIRECTION('center_axis',(0.,0.,1.));
#19655=DIRECTION('ref_axis',(-0.984807753012208,0.173648177666931,0.));
#19656=DIRECTION('',(-0.808467844782638,0.58854035031807,0.));
#19657=DIRECTION('',(0.961003922853658,0.276534736081891,0.));
#19658=DIRECTION('center_axis',(0.276534736081891,-0.961003922853658,0.));
#19659=DIRECTION('ref_axis',(0.961003922853658,0.276534736081891,0.));
#19660=DIRECTION('',(0.,0.,1.));
#19661=DIRECTION('center_axis',(0.58854035031807,0.808467844782638,0.));
#19662=DIRECTION('ref_axis',(-0.808467844782638,0.58854035031807,0.));
#19663=DIRECTION('center_axis',(0.105456972136322,-0.994423866883654,0.));
#19664=DIRECTION('ref_axis',(0.994423866883654,0.105456972136322,0.));
#19665=DIRECTION('',(0.994423866883654,0.105456972136322,0.));
#19666=DIRECTION('',(0.,0.,1.));
#19667=DIRECTION('center_axis',(0.719988067902572,0.693986442286823,0.));
#19668=DIRECTION('ref_axis',(-0.693986442286823,0.719988067902572,0.));
#19669=DIRECTION('',(-0.693986442286823,0.719988067902572,0.));
#19670=DIRECTION('center_axis',(0.,0.,1.));
#19671=DIRECTION('ref_axis',(-0.939692620785908,0.342020143325669,0.));
#19672=DIRECTION('center_axis',(0.,0.,1.));
#19673=DIRECTION('ref_axis',(-0.866025403784439,0.5,0.));
#19674=DIRECTION('',(-0.558418612916207,0.829559312375396,0.));
#19675=DIRECTION('',(0.997628744921147,-0.0688250485438063,0.));
#19676=DIRECTION('center_axis',(-0.0688250485438063,-0.997628744921147,
0.));
#19677=DIRECTION('ref_axis',(0.997628744921147,-0.0688250485438063,0.));
#19678=DIRECTION('',(0.,0.,1.));
#19679=DIRECTION('center_axis',(0.829559312375396,0.558418612916207,0.));
#19680=DIRECTION('ref_axis',(-0.558418612916207,0.829559312375396,0.));
#19681=DIRECTION('center_axis',(-0.241015854951086,-0.970521178368714,0.));
#19682=DIRECTION('ref_axis',(0.970521178368714,-0.241015854951086,0.));
#19683=DIRECTION('',(0.970521178368714,-0.241015854951086,0.));
#19684=DIRECTION('',(0.,0.,1.));
#19685=DIRECTION('center_axis',(0.91392481691896,0.405883516565584,0.));
#19686=DIRECTION('ref_axis',(-0.405883516565584,0.91392481691896,0.));
#19687=DIRECTION('',(-0.405883516565584,0.91392481691896,0.));
#19688=DIRECTION('center_axis',(0.,0.,1.));
#19689=DIRECTION('ref_axis',(-0.766044443118978,0.642787609686539,0.));
#19690=DIRECTION('center_axis',(0.,0.,1.));
#19691=DIRECTION('ref_axis',(-0.642787609686539,0.766044443118978,0.));
#19692=DIRECTION('',(-0.241015854951086,0.970521178368714,0.));
#19693=DIRECTION('',(0.91392481691896,-0.405883516565584,0.));
#19694=DIRECTION('center_axis',(-0.405883516565584,-0.91392481691896,0.));
#19695=DIRECTION('ref_axis',(0.91392481691896,-0.405883516565584,0.));
#19696=DIRECTION('',(0.,0.,1.));
#19697=DIRECTION('center_axis',(0.970521178368714,0.241015854951086,0.));
#19698=DIRECTION('ref_axis',(-0.241015854951086,0.970521178368714,0.));
#19699=DIRECTION('center_axis',(-0.558418612916207,-0.829559312375396,0.));
#19700=DIRECTION('ref_axis',(0.829559312375396,-0.558418612916207,0.));
#19701=DIRECTION('',(0.829559312375396,-0.558418612916207,0.));
#19702=DIRECTION('',(0.,0.,1.));
#19703=DIRECTION('center_axis',(0.997628744921147,0.0688250485438062,0.));
#19704=DIRECTION('ref_axis',(-0.0688250485438062,0.997628744921147,0.));
#19705=DIRECTION('',(-0.0688250485438062,0.997628744921147,0.));
#19706=DIRECTION('center_axis',(0.,0.,1.));
#19707=DIRECTION('ref_axis',(-0.5,0.866025403784439,0.));
#19708=DIRECTION('center_axis',(0.,0.,1.));
#19709=DIRECTION('ref_axis',(-0.342020143325669,0.939692620785908,0.));
#19710=DIRECTION('',(0.105456972136322,0.994423866883654,0.));
#19711=DIRECTION('',(0.719988067902572,-0.693986442286823,0.));
#19712=DIRECTION('center_axis',(-0.693986442286823,-0.719988067902572,0.));
#19713=DIRECTION('ref_axis',(0.719988067902572,-0.693986442286823,0.));
#19714=DIRECTION('',(0.,0.,1.));
#19715=DIRECTION('center_axis',(0.994423866883654,-0.105456972136322,0.));
#19716=DIRECTION('ref_axis',(0.105456972136322,0.994423866883654,0.));
#19717=DIRECTION('center_axis',(-0.808467844782638,-0.58854035031807,0.));
#19718=DIRECTION('ref_axis',(0.58854035031807,-0.808467844782638,0.));
#19719=DIRECTION('',(0.588540350318069,-0.808467844782638,0.));
#19720=DIRECTION('',(0.,0.,1.));
#19721=DIRECTION('center_axis',(0.961003922853658,-0.276534736081891,0.));
#19722=DIRECTION('ref_axis',(0.276534736081891,0.961003922853658,0.));
#19723=DIRECTION('',(0.276534736081891,0.961003922853658,0.));
#19724=DIRECTION('center_axis',(0.,0.,1.));
#19725=DIRECTION('ref_axis',(-0.17364817766693,0.984807753012208,0.));
#19726=DIRECTION('center_axis',(0.,0.,1.));
#19727=DIRECTION('ref_axis',(6.12323399573677E-17,1.,0.));
#19728=DIRECTION('',(0.43921013200494,0.898384360919202,0.));
#19729=DIRECTION('',(0.43921013200494,-0.898384360919202,0.));
#19730=DIRECTION('center_axis',(-0.898384360919202,-0.43921013200494,0.));
#19731=DIRECTION('ref_axis',(0.43921013200494,-0.898384360919202,0.));
#19732=DIRECTION('',(0.,0.,1.));
#19733=DIRECTION('center_axis',(0.898384360919202,-0.43921013200494,0.));
#19734=DIRECTION('ref_axis',(0.43921013200494,0.898384360919202,0.));
#19735=DIRECTION('center_axis',(-0.961003922853658,-0.276534736081891,0.));
#19736=DIRECTION('ref_axis',(0.276534736081891,-0.961003922853658,0.));
#19737=DIRECTION('',(0.276534736081891,-0.961003922853658,0.));
#19738=DIRECTION('',(0.,0.,1.));
#19739=DIRECTION('center_axis',(0.808467844782638,-0.58854035031807,0.));
#19740=DIRECTION('ref_axis',(0.58854035031807,0.808467844782638,0.));
#19741=DIRECTION('',(0.588540350318069,0.808467844782638,0.));
#19742=DIRECTION('center_axis',(0.,0.,1.));
#19743=DIRECTION('ref_axis',(0.17364817766693,0.984807753012208,0.));
#19744=DIRECTION('center_axis',(0.,0.,1.));
#19745=DIRECTION('ref_axis',(0.342020143325669,0.939692620785908,0.));
#19746=DIRECTION('',(0.719988067902572,0.693986442286823,0.));
#19747=DIRECTION('',(0.105456972136322,-0.994423866883654,0.));
#19748=DIRECTION('center_axis',(-0.994423866883654,-0.105456972136322,0.));
#19749=DIRECTION('ref_axis',(0.105456972136322,-0.994423866883654,0.));
#19750=DIRECTION('',(0.,0.,1.));
#19751=DIRECTION('center_axis',(0.693986442286823,-0.719988067902572,0.));
#19752=DIRECTION('ref_axis',(0.719988067902572,0.693986442286823,0.));
#19753=DIRECTION('center_axis',(-0.997628744921147,0.0688250485438065,0.));
#19754=DIRECTION('ref_axis',(-0.0688250485438065,-0.997628744921147,0.));
#19755=DIRECTION('',(-0.0688250485438065,-0.997628744921147,0.));
#19756=DIRECTION('',(0.,0.,1.));
#19757=DIRECTION('center_axis',(0.558418612916207,-0.829559312375396,0.));
#19758=DIRECTION('ref_axis',(0.829559312375396,0.558418612916207,0.));
#19759=DIRECTION('',(0.829559312375396,0.558418612916207,0.));
#19760=DIRECTION('center_axis',(0.,0.,1.));
#19761=DIRECTION('ref_axis',(0.5,0.866025403784439,0.));
#19762=DIRECTION('center_axis',(0.,0.,1.));
#19763=DIRECTION('ref_axis',(0.642787609686539,0.766044443118978,0.));
#19764=DIRECTION('',(0.91392481691896,0.405883516565584,0.));
#19765=DIRECTION('',(-0.241015854951086,-0.970521178368714,0.));
#19766=DIRECTION('center_axis',(-0.970521178368714,0.241015854951086,0.));
#19767=DIRECTION('ref_axis',(-0.241015854951086,-0.970521178368714,0.));
#19768=DIRECTION('',(0.,0.,1.));
#19769=DIRECTION('center_axis',(0.405883516565584,-0.91392481691896,0.));
#19770=DIRECTION('ref_axis',(0.91392481691896,0.405883516565584,0.));
#19771=DIRECTION('center_axis',(-0.91392481691896,0.405883516565585,0.));
#19772=DIRECTION('ref_axis',(-0.405883516565585,-0.91392481691896,0.));
#19773=DIRECTION('',(-0.405883516565584,-0.91392481691896,0.));
#19774=DIRECTION('',(0.,0.,1.));
#19775=DIRECTION('center_axis',(0.241015854951086,-0.970521178368714,0.));
#19776=DIRECTION('ref_axis',(0.970521178368714,0.241015854951086,0.));
#19777=DIRECTION('',(0.970521178368714,0.241015854951086,0.));
#19778=DIRECTION('center_axis',(0.,0.,1.));
#19779=DIRECTION('ref_axis',(0.766044443118978,0.642787609686539,0.));
#19780=DIRECTION('center_axis',(0.,0.,1.));
#19781=DIRECTION('ref_axis',(0.866025403784439,0.5,0.));
#19782=DIRECTION('',(0.997628744921147,0.0688250485438063,0.));
#19783=DIRECTION('',(-0.558418612916207,-0.829559312375396,0.));
#19784=DIRECTION('center_axis',(-0.829559312375396,0.558418612916207,0.));
#19785=DIRECTION('ref_axis',(-0.558418612916207,-0.829559312375396,0.));
#19786=DIRECTION('',(0.,0.,1.));
#19787=DIRECTION('center_axis',(0.0688250485438063,-0.997628744921147,0.));
#19788=DIRECTION('ref_axis',(0.997628744921147,0.0688250485438063,0.));
#19789=DIRECTION('center_axis',(-0.719988067902572,0.693986442286823,0.));
#19790=DIRECTION('ref_axis',(-0.693986442286823,-0.719988067902572,0.));
#19791=DIRECTION('',(-0.693986442286823,-0.719988067902572,0.));
#19792=DIRECTION('',(0.,0.,1.));
#19793=DIRECTION('center_axis',(-0.105456972136322,-0.994423866883654,0.));
#19794=DIRECTION('ref_axis',(0.994423866883654,-0.105456972136322,0.));
#19795=DIRECTION('',(0.994423866883654,-0.105456972136322,0.));
#19796=DIRECTION('center_axis',(0.,0.,1.));
#19797=DIRECTION('ref_axis',(0.939692620785908,0.342020143325669,0.));
#19798=DIRECTION('center_axis',(0.,0.,1.));
#19799=DIRECTION('ref_axis',(0.984807753012208,0.17364817766693,0.));
#19800=DIRECTION('',(0.961003922853658,-0.276534736081891,0.));
#19801=DIRECTION('',(-0.808467844782638,-0.588540350318069,0.));
#19802=DIRECTION('center_axis',(-0.58854035031807,0.808467844782638,0.));
#19803=DIRECTION('ref_axis',(-0.808467844782638,-0.58854035031807,0.));
#19804=DIRECTION('',(0.,0.,1.));
#19805=DIRECTION('center_axis',(-0.276534736081891,-0.961003922853658,0.));
#19806=DIRECTION('ref_axis',(0.961003922853658,-0.276534736081891,0.));
#19807=DIRECTION('center_axis',(-0.43921013200494,0.898384360919202,0.));
#19808=DIRECTION('ref_axis',(-0.898384360919202,-0.43921013200494,0.));
#19809=DIRECTION('',(-0.898384360919202,-0.43921013200494,0.));
#19810=DIRECTION('',(0.,0.,1.));
#19811=DIRECTION('center_axis',(-0.43921013200494,-0.898384360919202,0.));
#19812=DIRECTION('ref_axis',(0.898384360919202,-0.43921013200494,0.));
#19813=DIRECTION('',(0.898384360919202,-0.43921013200494,0.));
#19814=DIRECTION('center_axis',(0.,0.,1.));
#19815=DIRECTION('ref_axis',(1.,0.,0.));
#19816=DIRECTION('center_axis',(0.,0.,1.));
#19817=DIRECTION('ref_axis',(1.,0.,0.));
#19818=DIRECTION('center_axis',(0.,-1.,0.));
#19819=DIRECTION('ref_axis',(-1.,0.,0.));
#19820=DIRECTION('center_axis',(0.,0.,1.));
#19821=DIRECTION('ref_axis',(1.,0.,0.));
#19822=DIRECTION('center_axis',(0.,0.,1.));
#19823=DIRECTION('ref_axis',(1.,0.,0.));
#19824=DIRECTION('center_axis',(0.,0.,-1.));
#19825=DIRECTION('ref_axis',(1.,0.,0.));
#19826=DIRECTION('center_axis',(0.,0.,1.));
#19827=DIRECTION('ref_axis',(1.,0.,0.));
#19828=DIRECTION('center_axis',(0.,0.,1.));
#19829=DIRECTION('ref_axis',(1.,0.,0.));
#19830=DIRECTION('center_axis',(0.,0.,1.));
#19831=DIRECTION('ref_axis',(1.,0.,0.));
#19832=DIRECTION('center_axis',(0.,0.,1.));
#19833=DIRECTION('ref_axis',(1.,0.,0.));
#19834=DIRECTION('center_axis',(0.,0.,1.));
#19835=DIRECTION('ref_axis',(1.,0.,0.));
#19836=DIRECTION('center_axis',(0.,0.,1.));
#19837=DIRECTION('ref_axis',(1.,0.,0.));
#19838=DIRECTION('',(-0.707106781186551,8.65956056235498E-17,-0.707106781186544));
#19839=DIRECTION('center_axis',(0.,0.,1.));
#19840=DIRECTION('ref_axis',(1.,0.,0.));
#19841=DIRECTION('',(0.,0.,-1.));
#19842=DIRECTION('',(0.,0.,1.));
#19843=DIRECTION('center_axis',(0.,0.,-1.));
#19844=DIRECTION('ref_axis',(1.,0.,0.));
#19845=DIRECTION('center_axis',(0.,0.,1.));
#19846=DIRECTION('ref_axis',(1.,0.,0.));
#19847=DIRECTION('',(0.,0.,-1.));
#19848=DIRECTION('',(0.,0.,1.));
#19849=DIRECTION('center_axis',(0.,0.,-1.));
#19850=DIRECTION('ref_axis',(1.,0.,0.));
#19851=DIRECTION('center_axis',(0.,0.,1.));
#19852=DIRECTION('ref_axis',(1.,0.,0.));
#19853=DIRECTION('',(0.,0.,1.));
#19854=DIRECTION('center_axis',(0.,0.,-1.));
#19855=DIRECTION('ref_axis',(1.,0.,0.));
#19856=DIRECTION('',(0.,0.,-1.));
#19857=DIRECTION('center_axis',(0.,0.,1.));
#19858=DIRECTION('ref_axis',(1.,0.,0.));
#19859=DIRECTION('',(0.,0.,-1.));
#19860=DIRECTION('',(0.,0.,1.));
#19861=DIRECTION('center_axis',(0.,0.,-1.));
#19862=DIRECTION('ref_axis',(1.,0.,0.));
#19863=DIRECTION('center_axis',(0.,0.,1.));
#19864=DIRECTION('ref_axis',(1.,0.,0.));
#19865=DIRECTION('',(0.,0.,1.));
#19866=DIRECTION('center_axis',(0.,0.,-1.));
#19867=DIRECTION('ref_axis',(1.,0.,0.));
#19868=DIRECTION('',(0.,0.,-1.));
#19869=DIRECTION('center_axis',(0.,0.,1.));
#19870=DIRECTION('ref_axis',(1.,0.,0.));
#19871=DIRECTION('',(0.,0.,1.));
#19872=DIRECTION('center_axis',(0.,0.,-1.));
#19873=DIRECTION('ref_axis',(1.,0.,0.));
#19874=DIRECTION('',(0.,0.,-1.));
#19875=DIRECTION('center_axis',(0.,1.,0.));
#19876=DIRECTION('ref_axis',(-1.,0.,0.));
#19877=DIRECTION('',(-1.,0.,0.));
#19878=DIRECTION('',(0.,0.,1.));
#19879=DIRECTION('',(-1.,0.,0.));
#19880=DIRECTION('',(0.,0.,1.));
#19881=DIRECTION('center_axis',(0.866025403784438,0.500000000000001,0.));
#19882=DIRECTION('ref_axis',(-0.500000000000001,0.866025403784438,0.));
#19883=DIRECTION('',(-0.500000000000001,0.866025403784438,0.));
#19884=DIRECTION('',(0.,0.,1.));
#19885=DIRECTION('',(-0.500000000000001,0.866025403784438,0.));
#19886=DIRECTION('center_axis',(0.866025403784438,-0.500000000000001,0.));
#19887=DIRECTION('ref_axis',(0.500000000000001,0.866025403784438,0.));
#19888=DIRECTION('',(0.500000000000001,0.866025403784438,0.));
#19889=DIRECTION('',(0.,0.,1.));
#19890=DIRECTION('',(0.500000000000001,0.866025403784438,0.));
#19891=DIRECTION('center_axis',(0.,0.,1.));
#19892=DIRECTION('ref_axis',(1.,0.,0.));
#19893=DIRECTION('center_axis',(0.,0.,1.));
#19894=DIRECTION('ref_axis',(1.,0.,0.));
#19895=DIRECTION('center_axis',(0.,0.,1.));
#19896=DIRECTION('ref_axis',(1.,0.,0.));
#19897=DIRECTION('',(1.,0.,0.));
#19898=DIRECTION('center_axis',(0.,0.,1.));
#19899=DIRECTION('ref_axis',(1.,0.,0.));
#19900=DIRECTION('center_axis',(0.,0.,1.));
#19901=DIRECTION('ref_axis',(1.,0.,0.));
#19902=DIRECTION('',(0.500000000000001,-0.866025403784438,0.));
#19903=DIRECTION('center_axis',(0.,0.,1.));
#19904=DIRECTION('ref_axis',(1.,0.,0.));
#19905=DIRECTION('',(-0.500000000000001,-0.866025403784438,0.));
#19906=DIRECTION('center_axis',(0.,0.,-1.));
#19907=DIRECTION('ref_axis',(-1.,0.,0.));
#19908=DIRECTION('',(1.,0.,0.));
#19909=DIRECTION('center_axis',(0.,0.,1.));
#19910=DIRECTION('ref_axis',(1.,0.,0.));
#19911=DIRECTION('center_axis',(0.,0.,-1.));
#19912=DIRECTION('ref_axis',(-1.,0.,0.));
#19913=DIRECTION('center_axis',(0.,0.,1.));
#19914=DIRECTION('ref_axis',(1.,0.,0.));
#19915=DIRECTION('center_axis',(0.,0.,-1.));
#19916=DIRECTION('ref_axis',(-1.,0.,0.));
#19917=DIRECTION('center_axis',(0.,0.,1.));
#19918=DIRECTION('ref_axis',(1.,0.,0.));
#19919=DIRECTION('center_axis',(0.,0.,-1.));
#19920=DIRECTION('ref_axis',(-1.,0.,0.));
#19921=DIRECTION('center_axis',(0.,0.,1.));
#19922=DIRECTION('ref_axis',(1.,0.,0.));
#19923=DIRECTION('center_axis',(0.,0.,-1.));
#19924=DIRECTION('ref_axis',(-1.,0.,0.));
#19925=DIRECTION('',(-0.500000000000001,-0.866025403784438,0.));
#19926=DIRECTION('center_axis',(0.,0.,1.));
#19927=DIRECTION('ref_axis',(1.,0.,0.));
#19928=DIRECTION('center_axis',(0.,0.,-1.));
#19929=DIRECTION('ref_axis',(-1.,0.,0.));
#19930=DIRECTION('',(0.500000000000001,-0.866025403784438,0.));
#19931=DIRECTION('center_axis',(0.,0.,1.));
#19932=DIRECTION('ref_axis',(1.,0.,0.));
#19933=DIRECTION('center_axis',(0.,0.,-1.));
#19934=DIRECTION('ref_axis',(1.,0.,0.));
#19935=DIRECTION('',(-0.857167300702115,1.04972719113862E-16,-0.515038074910049));
#19936=DIRECTION('center_axis',(0.,-1.,0.));
#19937=DIRECTION('ref_axis',(1.,0.,0.));
#19938=DIRECTION('',(0.,0.,1.));
#19939=DIRECTION('center_axis',(-0.866025403784438,-0.500000000000001,0.));
#19940=DIRECTION('ref_axis',(0.500000000000001,-0.866025403784438,0.));
#19941=DIRECTION('',(0.,0.,1.));
#19942=DIRECTION('center_axis',(-0.866025403784438,0.500000000000001,0.));
#19943=DIRECTION('ref_axis',(-0.500000000000001,-0.866025403784438,0.));
#19944=DIRECTION('axis',(0.,0.,1.));
#19945=DIRECTION('refdir',(1.,0.,0.));
#19946=DIRECTION('center_axis',(0.,0.,1.));
#19947=DIRECTION('ref_axis',(0.979226971796874,-0.202767200763645,0.));
#19948=DIRECTION('',(0.,0.,-1.));
#19949=DIRECTION('center_axis',(0.,0.,-1.));
#19950=DIRECTION('ref_axis',(1.,6.67887018197865E-15,0.));
#19951=DIRECTION('center_axis',(0.,0.,1.));
#19952=DIRECTION('ref_axis',(0.979226971796874,-0.202767200763645,0.));
#19953=DIRECTION('',(0.,0.,-1.));
#19954=DIRECTION('center_axis',(0.,0.,1.));
#19955=DIRECTION('ref_axis',(0.979226971796874,-0.202767200763645,0.));
#19956=DIRECTION('',(0.,0.,-1.));
#19957=DIRECTION('center_axis',(0.,0.,1.));
#19958=DIRECTION('ref_axis',(0.979226971796874,-0.202767200763645,0.));
#19959=DIRECTION('',(0.,0.,-1.));
#19960=DIRECTION('center_axis',(0.,0.,1.));
#19961=DIRECTION('ref_axis',(0.979226971796874,-0.202767200763645,0.));
#19962=DIRECTION('',(0.,0.,-1.));
#19963=DIRECTION('center_axis',(0.,0.,1.));
#19964=DIRECTION('ref_axis',(0.979226971796874,-0.202767200763645,0.));
#19965=DIRECTION('',(0.,0.,-1.));
#19966=DIRECTION('center_axis',(0.,0.,1.));
#19967=DIRECTION('ref_axis',(0.979226971796874,-0.202767200763645,0.));
#19968=DIRECTION('',(0.,0.,-1.));
#19969=DIRECTION('center_axis',(0.,0.,1.));
#19970=DIRECTION('ref_axis',(0.979226971796874,-0.202767200763645,0.));
#19971=DIRECTION('',(0.,0.,-1.));
#19972=DIRECTION('center_axis',(0.,0.,1.));
#19973=DIRECTION('ref_axis',(0.979226971796874,-0.202767200763645,0.));
#19974=DIRECTION('',(0.,0.,-1.));
#19975=DIRECTION('center_axis',(0.,0.,1.));
#19976=DIRECTION('ref_axis',(0.979226971796874,-0.202767200763645,0.));
#19977=DIRECTION('',(0.,0.,-1.));
#19978=DIRECTION('center_axis',(0.,0.,1.));
#19979=DIRECTION('ref_axis',(0.979226971796874,-0.202767200763645,0.));
#19980=DIRECTION('',(0.,0.,-1.));
#19981=DIRECTION('center_axis',(0.,0.,1.));
#19982=DIRECTION('ref_axis',(0.979226971796874,-0.202767200763645,0.));
#19983=DIRECTION('',(0.,0.,-1.));
#19984=DIRECTION('center_axis',(0.,0.,1.));
#19985=DIRECTION('ref_axis',(0.979226971796874,-0.202767200763645,0.));
#19986=DIRECTION('',(0.,0.,-1.));
#19987=DIRECTION('center_axis',(0.,0.,1.));
#19988=DIRECTION('ref_axis',(0.979226971796874,-0.202767200763645,0.));
#19989=DIRECTION('',(0.,0.,-1.));
#19990=DIRECTION('center_axis',(0.,0.,1.));
#19991=DIRECTION('ref_axis',(0.979226971796874,-0.202767200763645,0.));
#19992=DIRECTION('',(0.,0.,-1.));
#19993=DIRECTION('center_axis',(0.,0.,1.));
#19994=DIRECTION('ref_axis',(0.979226971796874,-0.202767200763645,0.));
#19995=DIRECTION('',(0.,0.,-1.));
#19996=DIRECTION('center_axis',(0.,0.,1.));
#19997=DIRECTION('ref_axis',(0.979226971796874,-0.202767200763645,0.));
#19998=DIRECTION('',(0.,0.,-1.));
#19999=DIRECTION('center_axis',(0.,0.,1.));
#20000=DIRECTION('ref_axis',(0.979226971796874,-0.202767200763645,0.));
#20001=DIRECTION('',(0.,0.,-1.));
#20002=DIRECTION('center_axis',(0.,0.,1.));
#20003=DIRECTION('ref_axis',(0.979226971796874,-0.202767200763645,0.));
#20004=DIRECTION('',(0.,0.,-1.));
#20005=DIRECTION('center_axis',(0.,0.,1.));
#20006=DIRECTION('ref_axis',(0.979226971796874,-0.202767200763645,0.));
#20007=DIRECTION('',(0.,0.,-1.));
#20008=DIRECTION('center_axis',(0.,0.,1.));
#20009=DIRECTION('ref_axis',(0.979226971796874,-0.202767200763645,0.));
#20010=DIRECTION('',(0.,0.,-1.));
#20011=DIRECTION('center_axis',(0.,0.,1.));
#20012=DIRECTION('ref_axis',(0.979226971796874,-0.202767200763645,0.));
#20013=DIRECTION('',(0.,0.,-1.));
#20014=DIRECTION('center_axis',(0.,0.,1.));
#20015=DIRECTION('ref_axis',(0.979226971796874,-0.202767200763645,0.));
#20016=DIRECTION('',(0.,0.,-1.));
#20017=DIRECTION('center_axis',(0.,0.,1.));
#20018=DIRECTION('ref_axis',(1.,0.,0.));
#20019=DIRECTION('center_axis',(0.,0.,1.));
#20020=DIRECTION('ref_axis',(1.,0.,0.));
#20021=DIRECTION('center_axis',(0.,0.,-1.));
#20022=DIRECTION('ref_axis',(1.,0.,0.));
#20023=DIRECTION('center_axis',(0.,0.,1.));
#20024=DIRECTION('ref_axis',(0.979226971796874,-0.202767200763645,0.));
#20025=DIRECTION('center_axis',(0.,0.,1.));
#20026=DIRECTION('ref_axis',(1.,6.67887018197865E-15,0.));
#20027=DIRECTION('center_axis',(0.,0.,1.));
#20028=DIRECTION('ref_axis',(1.,0.,0.));
#20029=DIRECTION('center_axis',(0.,0.,-1.));
#20030=DIRECTION('ref_axis',(1.,0.,0.));
#20031=DIRECTION('center_axis',(0.,0.,-1.));
#20032=DIRECTION('ref_axis',(1.,0.,0.));
#20033=DIRECTION('center_axis',(0.,0.,1.));
#20034=DIRECTION('ref_axis',(1.,0.,0.));
#20035=DIRECTION('center_axis',(0.,0.,1.));
#20036=DIRECTION('ref_axis',(1.,0.,0.));
#20037=DIRECTION('center_axis',(0.,0.,1.));
#20038=DIRECTION('ref_axis',(1.,0.,0.));
#20039=DIRECTION('center_axis',(0.,0.,-1.));
#20040=DIRECTION('ref_axis',(1.,0.,0.));
#20041=DIRECTION('center_axis',(0.,0.,1.));
#20042=DIRECTION('ref_axis',(1.,0.,0.));
#20043=DIRECTION('center_axis',(0.,0.,1.));
#20044=DIRECTION('ref_axis',(1.,0.,0.));
#20045=DIRECTION('center_axis',(0.,0.,1.));
#20046=DIRECTION('ref_axis',(1.,0.,0.));
#20047=DIRECTION('center_axis',(0.,0.,1.));
#20048=DIRECTION('ref_axis',(1.,0.,0.));
#20049=DIRECTION('center_axis',(0.,0.,1.));
#20050=DIRECTION('ref_axis',(1.,0.,0.));
#20051=DIRECTION('center_axis',(0.,0.,1.));
#20052=DIRECTION('ref_axis',(1.,0.,0.));
#20053=DIRECTION('',(-0.707106781186539,8.65956056235484E-17,-0.707106781186556));
#20054=DIRECTION('center_axis',(0.,0.,1.));
#20055=DIRECTION('ref_axis',(1.,0.,0.));
#20056=DIRECTION('center_axis',(0.,0.,1.));
#20057=DIRECTION('ref_axis',(1.,0.,0.));
#20058=DIRECTION('',(0.,0.,-1.));
#20059=DIRECTION('',(0.,0.,1.));
#20060=DIRECTION('center_axis',(0.,0.,-1.));
#20061=DIRECTION('ref_axis',(1.,0.,0.));
#20062=DIRECTION('center_axis',(0.,0.,1.));
#20063=DIRECTION('ref_axis',(1.,0.,0.));
#20064=DIRECTION('',(0.,0.,-1.));
#20065=DIRECTION('',(0.,0.,1.));
#20066=DIRECTION('center_axis',(0.,0.,-1.));
#20067=DIRECTION('ref_axis',(1.,0.,0.));
#20068=DIRECTION('center_axis',(0.,0.,1.));
#20069=DIRECTION('ref_axis',(1.,0.,0.));
#20070=DIRECTION('',(0.,0.,1.));
#20071=DIRECTION('center_axis',(0.,0.,-1.));
#20072=DIRECTION('ref_axis',(1.,0.,0.));
#20073=DIRECTION('',(0.,0.,-1.));
#20074=DIRECTION('center_axis',(0.,0.,1.));
#20075=DIRECTION('ref_axis',(1.,0.,0.));
#20076=DIRECTION('',(0.,0.,-1.));
#20077=DIRECTION('',(0.,0.,1.));
#20078=DIRECTION('center_axis',(0.,0.,-1.));
#20079=DIRECTION('ref_axis',(1.,0.,0.));
#20080=DIRECTION('center_axis',(0.,0.,1.));
#20081=DIRECTION('ref_axis',(1.,0.,0.));
#20082=DIRECTION('',(0.,0.,1.));
#20083=DIRECTION('center_axis',(0.,0.,-1.));
#20084=DIRECTION('ref_axis',(1.,0.,0.));
#20085=DIRECTION('',(0.,0.,-1.));
#20086=DIRECTION('center_axis',(0.,0.,1.));
#20087=DIRECTION('ref_axis',(1.,0.,0.));
#20088=DIRECTION('',(0.,0.,1.));
#20089=DIRECTION('center_axis',(0.,0.,-1.));
#20090=DIRECTION('ref_axis',(1.,0.,0.));
#20091=DIRECTION('',(0.,0.,-1.));
#20092=DIRECTION('center_axis',(0.,1.,0.));
#20093=DIRECTION('ref_axis',(-1.,0.,0.));
#20094=DIRECTION('',(-1.,0.,0.));
#20095=DIRECTION('',(0.,0.,1.));
#20096=DIRECTION('',(-1.,0.,0.));
#20097=DIRECTION('',(0.,0.,1.));
#20098=DIRECTION('center_axis',(0.86602540378444,0.499999999999998,0.));
#20099=DIRECTION('ref_axis',(-0.499999999999998,0.86602540378444,0.));
#20100=DIRECTION('',(-0.499999999999998,0.86602540378444,0.));
#20101=DIRECTION('',(0.,0.,1.));
#20102=DIRECTION('',(-0.499999999999998,0.86602540378444,0.));
#20103=DIRECTION('center_axis',(0.86602540378444,-0.499999999999998,0.));
#20104=DIRECTION('ref_axis',(0.499999999999998,0.86602540378444,0.));
#20105=DIRECTION('',(0.499999999999998,0.86602540378444,0.));
#20106=DIRECTION('',(0.,0.,1.));
#20107=DIRECTION('',(0.499999999999998,0.86602540378444,0.));
#20108=DIRECTION('center_axis',(0.,0.,-1.));
#20109=DIRECTION('ref_axis',(-1.,0.,0.));
#20110=DIRECTION('center_axis',(0.,0.,-1.));
#20111=DIRECTION('ref_axis',(-1.,0.,0.));
#20112=DIRECTION('center_axis',(0.,0.,-1.));
#20113=DIRECTION('ref_axis',(-1.,0.,0.));
#20114=DIRECTION('',(1.,0.,0.));
#20115=DIRECTION('center_axis',(0.,0.,-1.));
#20116=DIRECTION('ref_axis',(-1.,0.,0.));
#20117=DIRECTION('center_axis',(0.,0.,-1.));
#20118=DIRECTION('ref_axis',(-1.,0.,0.));
#20119=DIRECTION('',(0.499999999999998,-0.86602540378444,0.));
#20120=DIRECTION('center_axis',(0.,0.,-1.));
#20121=DIRECTION('ref_axis',(-1.,0.,0.));
#20122=DIRECTION('',(-0.499999999999998,-0.86602540378444,0.));
#20123=DIRECTION('center_axis',(0.,0.,-1.));
#20124=DIRECTION('ref_axis',(-1.,0.,0.));
#20125=DIRECTION('',(1.,0.,0.));
#20126=DIRECTION('center_axis',(0.,0.,1.));
#20127=DIRECTION('ref_axis',(1.,0.,0.));
#20128=DIRECTION('center_axis',(0.,0.,-1.));
#20129=DIRECTION('ref_axis',(-1.,0.,0.));
#20130=DIRECTION('center_axis',(0.,0.,1.));
#20131=DIRECTION('ref_axis',(1.,0.,0.));
#20132=DIRECTION('center_axis',(0.,0.,-1.));
#20133=DIRECTION('ref_axis',(-1.,0.,0.));
#20134=DIRECTION('center_axis',(0.,0.,1.));
#20135=DIRECTION('ref_axis',(1.,0.,0.));
#20136=DIRECTION('center_axis',(0.,0.,-1.));
#20137=DIRECTION('ref_axis',(-1.,0.,0.));
#20138=DIRECTION('center_axis',(0.,0.,1.));
#20139=DIRECTION('ref_axis',(1.,0.,0.));
#20140=DIRECTION('center_axis',(0.,0.,-1.));
#20141=DIRECTION('ref_axis',(-1.,0.,0.));
#20142=DIRECTION('',(-0.499999999999998,-0.86602540378444,0.));
#20143=DIRECTION('center_axis',(0.,0.,1.));
#20144=DIRECTION('ref_axis',(1.,0.,0.));
#20145=DIRECTION('center_axis',(0.,0.,-1.));
#20146=DIRECTION('ref_axis',(-1.,0.,0.));
#20147=DIRECTION('',(0.499999999999998,-0.86602540378444,0.));
#20148=DIRECTION('center_axis',(0.,0.,1.));
#20149=DIRECTION('ref_axis',(1.,0.,0.));
#20150=DIRECTION('center_axis',(0.,0.,-1.));
#20151=DIRECTION('ref_axis',(1.,0.,0.));
#20152=DIRECTION('',(-0.85716730070211,1.04972719113862E-16,-0.515038074910058));
#20153=DIRECTION('center_axis',(0.,-1.,0.));
#20154=DIRECTION('ref_axis',(1.,0.,0.));
#20155=DIRECTION('',(0.,0.,1.));
#20156=DIRECTION('center_axis',(-0.86602540378444,-0.499999999999998,0.));
#20157=DIRECTION('ref_axis',(0.499999999999998,-0.86602540378444,0.));
#20158=DIRECTION('',(0.,0.,1.));
#20159=DIRECTION('center_axis',(-0.86602540378444,0.499999999999998,0.));
#20160=DIRECTION('ref_axis',(-0.499999999999998,-0.86602540378444,0.));
#20161=DIRECTION('center_axis',(0.,0.,-1.));
#20162=DIRECTION('ref_axis',(-1.,0.,0.));
#20163=DIRECTION('center_axis',(0.,0.,1.));
#20164=DIRECTION('ref_axis',(1.,0.,0.));
#20165=DIRECTION('center_axis',(0.,0.,1.));
#20166=DIRECTION('ref_axis',(1.,0.,0.));
#20167=DIRECTION('',(0.707106781186547,8.65956056235493E-17,-0.707106781186548));
#20168=DIRECTION('center_axis',(0.,0.,-1.));
#20169=DIRECTION('ref_axis',(1.,0.,0.));
#20170=DIRECTION('',(0.707106781186547,-8.65956056235493E-17,0.707106781186548));
#20171=DIRECTION('center_axis',(0.,0.,1.));
#20172=DIRECTION('ref_axis',(1.,0.,0.));
#20173=DIRECTION('center_axis',(0.,0.,1.));
#20174=DIRECTION('ref_axis',(1.,0.,0.));
#20175=DIRECTION('axis',(0.,0.,1.));
#20176=DIRECTION('refdir',(1.,0.,0.));
#20177=DIRECTION('center_axis',(0.,0.,1.));
#20178=DIRECTION('ref_axis',(0.487024915847047,-0.873388076025873,0.));
#20179=DIRECTION('',(0.,0.,-1.));
#20180=DIRECTION('center_axis',(0.,0.,-1.));
#20181=DIRECTION('ref_axis',(1.,6.23361216984672E-14,0.));
#20182=DIRECTION('center_axis',(0.,0.,1.));
#20183=DIRECTION('ref_axis',(0.487024915847047,-0.873388076025873,0.));
#20184=DIRECTION('',(0.,0.,-1.));
#20185=DIRECTION('center_axis',(0.,0.,-1.));
#20186=DIRECTION('ref_axis',(1.,6.23361216984672E-14,0.));
#20187=DIRECTION('center_axis',(0.,0.,1.));
#20188=DIRECTION('ref_axis',(0.487024915847047,-0.873388076025873,0.));
#20189=DIRECTION('',(0.,0.,-1.));
#20190=DIRECTION('center_axis',(0.,0.,1.));
#20191=DIRECTION('ref_axis',(0.487024915847047,-0.873388076025873,0.));
#20192=DIRECTION('',(0.,0.,-1.));
#20193=DIRECTION('center_axis',(0.,0.,1.));
#20194=DIRECTION('ref_axis',(0.487024915847047,-0.873388076025873,0.));
#20195=DIRECTION('',(0.,0.,-1.));
#20196=DIRECTION('center_axis',(0.,0.,1.));
#20197=DIRECTION('ref_axis',(0.487024915847047,-0.873388076025873,0.));
#20198=DIRECTION('',(0.,0.,-1.));
#20199=DIRECTION('center_axis',(0.,0.,1.));
#20200=DIRECTION('ref_axis',(0.487024915847047,-0.873388076025873,0.));
#20201=DIRECTION('',(0.,0.,-1.));
#20202=DIRECTION('center_axis',(0.,0.,1.));
#20203=DIRECTION('ref_axis',(0.487024915847047,-0.873388076025873,0.));
#20204=DIRECTION('',(0.,0.,-1.));
#20205=DIRECTION('center_axis',(0.,0.,1.));
#20206=DIRECTION('ref_axis',(0.487024915847047,-0.873388076025873,0.));
#20207=DIRECTION('',(0.,0.,-1.));
#20208=DIRECTION('center_axis',(0.,0.,1.));
#20209=DIRECTION('ref_axis',(0.487024915847047,-0.873388076025873,0.));
#20210=DIRECTION('',(0.,0.,-1.));
#20211=DIRECTION('center_axis',(0.,0.,-1.));
#20212=DIRECTION('ref_axis',(1.,0.,0.));
#20213=DIRECTION('',(-0.707106781186547,8.65956056235493E-17,-0.707106781186548));
#20214=DIRECTION('center_axis',(0.,0.,1.));
#20215=DIRECTION('ref_axis',(1.,0.,0.));
#20216=DIRECTION('center_axis',(0.,0.,-1.));
#20217=DIRECTION('ref_axis',(1.,0.,0.));
#20218=DIRECTION('center_axis',(0.,0.,1.));
#20219=DIRECTION('ref_axis',(1.,0.,0.));
#20220=DIRECTION('center_axis',(0.,0.,1.));
#20221=DIRECTION('ref_axis',(1.,0.,0.));
#20222=DIRECTION('center_axis',(0.,0.,1.));
#20223=DIRECTION('ref_axis',(1.,0.,0.));
#20224=DIRECTION('center_axis',(0.,0.,1.));
#20225=DIRECTION('ref_axis',(1.,0.,0.));
#20226=DIRECTION('center_axis',(0.,0.,1.));
#20227=DIRECTION('ref_axis',(1.,0.,0.));
#20228=DIRECTION('center_axis',(0.,0.,1.));
#20229=DIRECTION('ref_axis',(0.487024915847047,-0.873388076025873,0.));
#20230=DIRECTION('center_axis',(0.,0.,1.));
#20231=DIRECTION('ref_axis',(1.,6.23361216984672E-14,0.));
#20232=DIRECTION('center_axis',(-4.0203604687501E-11,3.07178135510889E-11,
-1.));
#20233=DIRECTION('ref_axis',(0.523940213008024,0.85175504295138,5.09976739692055E-12));
#20234=DIRECTION('center_axis',(0.,0.,1.));
#20235=DIRECTION('ref_axis',(1.,0.,0.));
#20236=DIRECTION('center_axis',(0.,0.,1.));
#20237=DIRECTION('ref_axis',(1.,0.,0.));
#20238=DIRECTION('center_axis',(6.22475379338965E-12,5.06217749195052E-11,
-1.));
#20239=DIRECTION('ref_axis',(0.946205103506986,-0.323567461431668,-1.04896653964898E-11));
#20240=DIRECTION('center_axis',(0.,0.,-1.));
#20241=DIRECTION('ref_axis',(-1.,0.,0.));
#20242=DIRECTION('center_axis',(0.,0.,1.));
#20243=DIRECTION('ref_axis',(1.,0.,0.));
#20244=DIRECTION('center_axis',(0.,0.,-1.));
#20245=DIRECTION('ref_axis',(1.,0.,0.));
#20246=DIRECTION('center_axis',(0.,1.,0.));
#20247=DIRECTION('ref_axis',(-1.,0.,0.));
#20248=DIRECTION('center_axis',(0.,0.,-1.));
#20249=DIRECTION('ref_axis',(-1.,0.,0.));
#20250=DIRECTION('center_axis',(0.,0.,1.));
#20251=DIRECTION('ref_axis',(1.,0.,0.));
#20252=DIRECTION('center_axis',(0.,0.,1.));
#20253=DIRECTION('ref_axis',(1.,0.,0.));
#20254=DIRECTION('',(-0.499999999999998,0.86602540378444,0.));
#20255=DIRECTION('center_axis',(0.,0.,1.));
#20256=DIRECTION('ref_axis',(1.,0.,0.));
#20257=DIRECTION('center_axis',(0.,0.,1.));
#20258=DIRECTION('ref_axis',(1.,0.,0.));
#20259=DIRECTION('',(0.5,0.866025403784439,0.));
#20260=DIRECTION('center_axis',(0.,0.,1.));
#20261=DIRECTION('ref_axis',(1.,0.,0.));
#20262=DIRECTION('center_axis',(0.,0.,1.));
#20263=DIRECTION('ref_axis',(1.,0.,0.));
#20264=DIRECTION('',(1.,0.,0.));
#20265=DIRECTION('center_axis',(0.,0.,1.));
#20266=DIRECTION('ref_axis',(1.,0.,0.));
#20267=DIRECTION('center_axis',(0.,0.,1.));
#20268=DIRECTION('ref_axis',(1.,0.,0.));
#20269=DIRECTION('',(0.5,-0.866025403784439,0.));
#20270=DIRECTION('center_axis',(0.,0.,1.));
#20271=DIRECTION('ref_axis',(1.,0.,0.));
#20272=DIRECTION('center_axis',(0.,0.,1.));
#20273=DIRECTION('ref_axis',(1.,0.,0.));
#20274=DIRECTION('',(-0.499999999999999,-0.866025403784439,0.));
#20275=DIRECTION('center_axis',(0.,0.,1.));
#20276=DIRECTION('ref_axis',(1.,0.,0.));
#20277=DIRECTION('center_axis',(0.,0.,1.));
#20278=DIRECTION('ref_axis',(1.,0.,0.));
#20279=DIRECTION('',(-1.,0.,0.));
#20280=DIRECTION('center_axis',(0.,0.,1.));
#20281=DIRECTION('ref_axis',(1.,0.,0.));
#20282=DIRECTION('center_axis',(0.,0.,1.));
#20283=DIRECTION('ref_axis',(1.,0.,0.));
#20284=DIRECTION('',(-0.85716730070211,-1.04972719113862E-16,0.515038074910058));
#20285=DIRECTION('center_axis',(-0.86602540378444,-0.499999999999998,0.));
#20286=DIRECTION('ref_axis',(-0.499999999999998,0.86602540378444,0.));
#20287=DIRECTION('center_axis',(-0.86602540378444,-0.499999999999998,0.));
#20288=DIRECTION('ref_axis',(0.,0.,-1.));
#20289=DIRECTION('',(0.,0.,-1.));
#20290=DIRECTION('',(0.,0.,-1.));
#20291=DIRECTION('center_axis',(-0.866025403784439,0.5,0.));
#20292=DIRECTION('ref_axis',(0.5,0.866025403784439,0.));
#20293=DIRECTION('center_axis',(-0.866025403784439,0.5,0.));
#20294=DIRECTION('ref_axis',(0.,0.,-1.));
#20295=DIRECTION('',(0.,0.,-1.));
#20296=DIRECTION('center_axis',(0.,1.,0.));
#20297=DIRECTION('ref_axis',(1.,0.,0.));
#20298=DIRECTION('center_axis',(0.,1.,0.));
#20299=DIRECTION('ref_axis',(0.,0.,-1.));
#20300=DIRECTION('',(0.,0.,-1.));
#20301=DIRECTION('center_axis',(0.866025403784439,0.5,0.));
#20302=DIRECTION('ref_axis',(0.5,-0.866025403784439,0.));
#20303=DIRECTION('center_axis',(0.866025403784439,0.5,0.));
#20304=DIRECTION('ref_axis',(0.,0.,-1.));
#20305=DIRECTION('',(0.,0.,-1.));
#20306=DIRECTION('center_axis',(0.,-1.,0.));
#20307=DIRECTION('ref_axis',(-1.,0.,0.));
#20308=DIRECTION('center_axis',(0.,-1.,0.));
#20309=DIRECTION('ref_axis',(0.,0.,1.));
#20310=DIRECTION('',(0.,0.,-1.));
#20311=DIRECTION('center_axis',(0.866025403784439,-0.5,0.));
#20312=DIRECTION('ref_axis',(-0.5,-0.866025403784439,0.));
#20313=DIRECTION('center_axis',(0.866025403784439,-0.5,0.));
#20314=DIRECTION('ref_axis',(0.,0.,1.));
#20315=DIRECTION('center_axis',(0.,0.,1.));
#20316=DIRECTION('ref_axis',(1.,0.,0.));
#20317=DIRECTION('center_axis',(0.,0.,1.));
#20318=DIRECTION('ref_axis',(1.,0.,0.));
#20319=DIRECTION('',(0.,0.,-1.));
#20320=DIRECTION('center_axis',(0.,0.,1.));
#20321=DIRECTION('ref_axis',(1.,0.,0.));
#20322=DIRECTION('center_axis',(0.,-1.,0.));
#20323=DIRECTION('ref_axis',(-1.,0.,0.));
#20324=DIRECTION('axis',(0.,0.,1.));
#20325=DIRECTION('refdir',(1.,0.,0.));
#20326=DIRECTION('center_axis',(1.,0.,0.));
#20327=DIRECTION('ref_axis',(0.,0.761817798782983,-0.64779135642385));
#20328=DIRECTION('',(-1.,0.,0.));
#20329=DIRECTION('center_axis',(-1.,0.,0.));
#20330=DIRECTION('ref_axis',(0.,1.,6.78718384827097E-14));
#20331=DIRECTION('center_axis',(1.,0.,0.));
#20332=DIRECTION('ref_axis',(0.,0.761817798782983,-0.64779135642385));
#20333=DIRECTION('',(-1.,0.,0.));
#20334=DIRECTION('center_axis',(-1.,0.,0.));
#20335=DIRECTION('ref_axis',(0.,1.,6.78718384827097E-14));
#20336=DIRECTION('center_axis',(1.,0.,0.));
#20337=DIRECTION('ref_axis',(0.,0.761817798782983,-0.64779135642385));
#20338=DIRECTION('',(-1.,0.,0.));
#20339=DIRECTION('center_axis',(1.,0.,0.));
#20340=DIRECTION('ref_axis',(0.,0.761817798782983,-0.64779135642385));
#20341=DIRECTION('',(-1.,0.,0.));
#20342=DIRECTION('center_axis',(1.,0.,0.));
#20343=DIRECTION('ref_axis',(0.,0.761817798782983,-0.64779135642385));
#20344=DIRECTION('',(-1.,0.,0.));
#20345=DIRECTION('center_axis',(1.,0.,0.));
#20346=DIRECTION('ref_axis',(0.,0.761817798782983,-0.64779135642385));
#20347=DIRECTION('',(-1.,0.,0.));
#20348=DIRECTION('center_axis',(1.,0.,0.));
#20349=DIRECTION('ref_axis',(0.,0.761817798782983,-0.64779135642385));
#20350=DIRECTION('',(-1.,0.,0.));
#20351=DIRECTION('center_axis',(1.,0.,0.));
#20352=DIRECTION('ref_axis',(0.,0.761817798782983,-0.64779135642385));
#20353=DIRECTION('',(-1.,0.,0.));
#20354=DIRECTION('center_axis',(1.,0.,0.));
#20355=DIRECTION('ref_axis',(0.,0.761817798782983,-0.64779135642385));
#20356=DIRECTION('',(-1.,0.,0.));
#20357=DIRECTION('center_axis',(1.,0.,0.));
#20358=DIRECTION('ref_axis',(0.,0.761817798782983,-0.64779135642385));
#20359=DIRECTION('',(-1.,0.,0.));
#20360=DIRECTION('center_axis',(1.,0.,0.));
#20361=DIRECTION('ref_axis',(0.,0.761817798782983,-0.64779135642385));
#20362=DIRECTION('',(-1.,0.,0.));
#20363=DIRECTION('center_axis',(1.,0.,0.));
#20364=DIRECTION('ref_axis',(0.,0.761817798782983,-0.64779135642385));
#20365=DIRECTION('',(-1.,0.,0.));
#20366=DIRECTION('center_axis',(1.,0.,0.));
#20367=DIRECTION('ref_axis',(0.,1.,0.));
#20368=DIRECTION('center_axis',(1.,0.,0.));
#20369=DIRECTION('ref_axis',(0.,1.,0.));
#20370=DIRECTION('center_axis',(1.,0.,0.));
#20371=DIRECTION('ref_axis',(0.,1.,0.));
#20372=DIRECTION('center_axis',(1.,0.,0.));
#20373=DIRECTION('ref_axis',(0.,0.761817798782983,-0.64779135642385));
#20374=DIRECTION('center_axis',(1.,0.,0.));
#20375=DIRECTION('ref_axis',(0.,1.,6.78718384827097E-14));
#20376=DIRECTION('center_axis',(1.,0.,0.));
#20377=DIRECTION('ref_axis',(0.,0.,-1.));
#20378=DIRECTION('center_axis',(1.,0.,0.));
#20379=DIRECTION('ref_axis',(0.,1.,0.));
#20380=DIRECTION('center_axis',(1.,0.,0.));
#20381=DIRECTION('ref_axis',(0.,1.,0.));
#20382=DIRECTION('center_axis',(1.,0.,0.));
#20383=DIRECTION('ref_axis',(0.,0.,-1.));
#20384=DIRECTION('center_axis',(-1.,0.,0.));
#20385=DIRECTION('ref_axis',(0.,1.,0.));
#20386=DIRECTION('center_axis',(0.,1.,0.));
#20387=DIRECTION('ref_axis',(0.,0.,1.));
#20388=DIRECTION('center_axis',(-1.,0.,0.));
#20389=DIRECTION('ref_axis',(0.,0.,1.));
#20390=DIRECTION('center_axis',(1.,0.,0.));
#20391=DIRECTION('ref_axis',(0.,0.,-1.));
#20392=DIRECTION('center_axis',(-1.,0.,0.));
#20393=DIRECTION('ref_axis',(0.,0.,1.));
#20394=DIRECTION('center_axis',(-1.,0.,0.));
#20395=DIRECTION('ref_axis',(0.,1.,0.));
#20396=DIRECTION('',(0.,-1.,0.));
#20397=DIRECTION('center_axis',(-1.,0.,0.));
#20398=DIRECTION('ref_axis',(0.,1.,0.));
#20399=DIRECTION('',(0.,1.,0.));
#20400=DIRECTION('center_axis',(-1.,0.,0.));
#20401=DIRECTION('ref_axis',(0.,1.,0.));
#20402=DIRECTION('center_axis',(0.,0.,1.));
#20403=DIRECTION('ref_axis',(0.,1.,0.));
#20404=DIRECTION('',(1.,0.,0.));
#20405=DIRECTION('',(-1.,0.,0.));
#20406=DIRECTION('',(0.,1.,0.));
#20407=DIRECTION('center_axis',(0.,0.,-1.));
#20408=DIRECTION('ref_axis',(0.,-1.,0.));
#20409=DIRECTION('',(-1.,0.,0.));
#20410=DIRECTION('',(0.,-1.,0.));
#20411=DIRECTION('',(1.,0.,0.));
#20412=DIRECTION('center_axis',(1.,0.,0.));
#20413=DIRECTION('ref_axis',(0.,1.,0.));
#20414=DIRECTION('',(-1.,0.,0.));
#20415=DIRECTION('center_axis',(1.,0.,0.));
#20416=DIRECTION('ref_axis',(0.,0.,-1.));
#20417=DIRECTION('center_axis',(1.,0.,0.));
#20418=DIRECTION('ref_axis',(0.,0.,-1.));
#20419=DIRECTION('center_axis',(1.,0.,0.));
#20420=DIRECTION('ref_axis',(0.,0.,-1.));
#20421=DIRECTION('center_axis',(1.,0.,0.));
#20422=DIRECTION('ref_axis',(0.,0.,-1.));
#20423=DIRECTION('center_axis',(1.,0.,0.));
#20424=DIRECTION('ref_axis',(0.,0.,-1.));
#20425=DIRECTION('center_axis',(1.,0.,0.));
#20426=DIRECTION('ref_axis',(0.,0.,-1.));
#20427=DIRECTION('center_axis',(-1.,0.,0.));
#20428=DIRECTION('ref_axis',(0.,1.,0.));
#20429=DIRECTION('center_axis',(-1.,0.,0.));
#20430=DIRECTION('ref_axis',(0.,0.,1.));
#20431=DIRECTION('center_axis',(1.,0.,0.));
#20432=DIRECTION('ref_axis',(0.,0.,-1.));
#20433=DIRECTION('center_axis',(-1.,0.,0.));
#20434=DIRECTION('ref_axis',(0.,1.,0.));
#20435=DIRECTION('',(-0.707106781186514,-0.707106781186581,8.65956056235535E-17));
#20436=DIRECTION('center_axis',(-1.,0.,0.));
#20437=DIRECTION('ref_axis',(0.,1.,0.));
#20438=DIRECTION('',(0.,0.,1.));
#20439=DIRECTION('',(1.,0.,0.));
#20440=DIRECTION('',(0.,0.,1.));
#20441=DIRECTION('',(1.,0.,0.));
#20442=DIRECTION('',(0.,0.,1.));
#20443=DIRECTION('',(1.,0.,0.));
#20444=DIRECTION('',(0.,0.,1.));
#20445=DIRECTION('',(1.,0.,0.));
#20446=DIRECTION('',(0.,0.,1.));
#20447=DIRECTION('',(1.,0.,0.));
#20448=DIRECTION('',(0.,0.,1.));
#20449=DIRECTION('',(1.,0.,0.));
#20450=DIRECTION('',(0.,0.,1.));
#20451=DIRECTION('',(1.,0.,0.));
#20452=DIRECTION('',(0.,0.,1.));
#20453=DIRECTION('',(1.,0.,0.));
#20454=DIRECTION('',(0.,0.,1.));
#20455=DIRECTION('',(1.,0.,0.));
#20456=DIRECTION('',(0.,-0.707106781186548,0.707106781186547));
#20457=DIRECTION('',(1.,0.,0.));
#20458=DIRECTION('',(1.22464679914735E-16,0.,-1.));
#20459=DIRECTION('',(-1.,0.,-1.22464679914735E-16));
#20460=DIRECTION('',(1.22464679914735E-16,0.,-1.));
#20461=DIRECTION('',(-1.,0.,-1.22464679914735E-16));
#20462=DIRECTION('',(1.22464679914735E-16,0.,-1.));
#20463=DIRECTION('',(-1.,0.,-1.22464679914735E-16));
#20464=DIRECTION('',(0.,0.707106781186548,0.707106781186547));
#20465=DIRECTION('',(1.,0.,0.));
#20466=DIRECTION('',(0.,-0.707106781186548,0.707106781186547));
#20467=DIRECTION('',(1.,0.,0.));
#20468=DIRECTION('',(0.,0.707106781186548,0.707106781186547));
#20469=DIRECTION('',(1.,0.,0.));
#20470=DIRECTION('',(0.,-0.707106781186548,0.707106781186547));
#20471=DIRECTION('',(1.,0.,0.));
#20472=DIRECTION('',(0.,0.707106781186548,0.707106781186547));
#20473=DIRECTION('',(1.,0.,0.));
#20474=DIRECTION('',(0.,-0.707106781186548,0.707106781186547));
#20475=DIRECTION('',(1.,0.,0.));
#20476=DIRECTION('',(0.,0.707106781186548,0.707106781186547));
#20477=DIRECTION('',(1.,0.,0.));
#20478=DIRECTION('',(0.,-0.707106781186548,0.707106781186547));
#20479=DIRECTION('',(1.,0.,0.));
#20480=DIRECTION('',(0.,0.707106781186548,0.707106781186547));
#20481=DIRECTION('',(1.,0.,0.));
#20482=DIRECTION('',(0.,-0.707106781186548,0.707106781186547));
#20483=DIRECTION('',(1.,0.,0.));
#20484=DIRECTION('',(0.,0.707106781186548,0.707106781186547));
#20485=DIRECTION('',(1.,0.,0.));
#20486=DIRECTION('',(0.,-0.707106781186548,0.707106781186547));
#20487=DIRECTION('',(1.,0.,0.));
#20488=DIRECTION('',(8.65956056235493E-17,-0.707106781186548,-0.707106781186547));
#20489=DIRECTION('',(-1.,-1.84470294816695E-31,-1.22464679914735E-16));
#20490=DIRECTION('',(8.65956056235493E-17,0.707106781186548,-0.707106781186547));
#20491=DIRECTION('',(-1.,1.84470294816695E-31,-1.22464679914735E-16));
#20492=DIRECTION('',(8.65956056235493E-17,-0.707106781186548,-0.707106781186547));
#20493=DIRECTION('',(-1.,-1.84470294816695E-31,-1.22464679914735E-16));
#20494=DIRECTION('',(8.65956056235493E-17,0.707106781186548,-0.707106781186547));
#20495=DIRECTION('',(-1.,1.84470294816695E-31,-1.22464679914735E-16));
#20496=DIRECTION('',(8.65956056235493E-17,-0.707106781186548,-0.707106781186547));
#20497=DIRECTION('',(-1.,-1.84470294816695E-31,-1.22464679914735E-16));
#20498=DIRECTION('',(8.65956056235493E-17,0.707106781186548,-0.707106781186547));
#20499=DIRECTION('',(-1.,1.84470294816695E-31,-1.22464679914735E-16));
#20500=DIRECTION('',(8.65956056235493E-17,-0.707106781186548,-0.707106781186547));
#20501=DIRECTION('',(-1.,-1.84470294816695E-31,-1.22464679914735E-16));
#20502=DIRECTION('',(8.65956056235493E-17,0.707106781186548,-0.707106781186547));
#20503=DIRECTION('',(-1.,1.84470294816695E-31,-1.22464679914735E-16));
#20504=DIRECTION('',(8.65956056235493E-17,-0.707106781186548,-0.707106781186547));
#20505=DIRECTION('',(-1.,-1.84470294816695E-31,-1.22464679914735E-16));
#20506=DIRECTION('',(8.65956056235493E-17,0.707106781186548,-0.707106781186547));
#20507=DIRECTION('',(-1.,1.84470294816695E-31,-1.22464679914735E-16));
#20508=DIRECTION('',(8.65956056235493E-17,-0.707106781186548,-0.707106781186547));
#20509=DIRECTION('',(-1.,-1.84470294816695E-31,-1.22464679914735E-16));
#20510=DIRECTION('',(8.65956056235493E-17,0.707106781186548,-0.707106781186547));
#20511=DIRECTION('',(-1.,1.84470294816695E-31,-1.22464679914735E-16));
#20512=DIRECTION('',(8.65956056235493E-17,-0.707106781186548,-0.707106781186547));
#20513=DIRECTION('',(-1.,-1.84470294816695E-31,-1.22464679914735E-16));
#20514=DIRECTION('',(1.22464679914735E-16,0.,-1.));
#20515=DIRECTION('',(-1.,0.,-1.22464679914735E-16));
#20516=DIRECTION('',(0.,0.,1.));
#20517=DIRECTION('',(1.,0.,0.));
#20518=DIRECTION('',(1.22464679914735E-16,0.,-1.));
#20519=DIRECTION('',(-1.,0.,-1.22464679914735E-16));
#20520=DIRECTION('',(0.,0.,1.));
#20521=DIRECTION('',(1.,0.,0.));
#20522=DIRECTION('',(1.22464679914735E-16,0.,-1.));
#20523=DIRECTION('',(-1.,0.,-1.22464679914735E-16));
#20524=DIRECTION('',(1.22464679914735E-16,0.,-1.));
#20525=DIRECTION('',(-1.,0.,-1.22464679914735E-16));
#20526=DIRECTION('',(0.,0.,1.));
#20527=DIRECTION('',(1.,0.,0.));
#20528=DIRECTION('',(1.22464679914735E-16,0.,-1.));
#20529=DIRECTION('',(-1.,0.,-1.22464679914735E-16));
#20530=DIRECTION('',(0.,0.,1.));
#20531=DIRECTION('',(1.,0.,0.));
#20532=DIRECTION('',(1.22464679914735E-16,0.,-1.));
#20533=DIRECTION('',(-1.,0.,-1.22464679914735E-16));
#20534=DIRECTION('',(1.22464679914735E-16,0.,-1.));
#20535=DIRECTION('',(-1.,0.,-1.22464679914735E-16));
#20536=DIRECTION('',(0.,0.,1.));
#20537=DIRECTION('',(1.,0.,0.));
#20538=DIRECTION('',(1.22464679914735E-16,0.,-1.));
#20539=DIRECTION('',(-1.,0.,-1.22464679914735E-16));
#20540=DIRECTION('',(0.,0.,1.));
#20541=DIRECTION('',(1.,0.,0.));
#20542=DIRECTION('',(1.22464679914735E-16,0.,-1.));
#20543=DIRECTION('',(-1.,0.,-1.22464679914735E-16));
#20544=DIRECTION('',(0.,0.,1.));
#20545=DIRECTION('',(1.,0.,0.));
#20546=DIRECTION('',(1.22464679914735E-16,0.,-1.));
#20547=DIRECTION('',(-1.,0.,-1.22464679914735E-16));
#20548=DIRECTION('',(1.22464679914735E-16,0.,-1.));
#20549=DIRECTION('',(-1.,0.,-1.22464679914735E-16));
#20550=DIRECTION('',(0.,0.,1.));
#20551=DIRECTION('',(-1.,1.22464679914735E-16,0.));
#20552=DIRECTION('',(1.22464679914735E-16,-1.258548236767E-48,-1.));
#20553=DIRECTION('',(1.,1.22464679914735E-16,1.22464679914735E-16));
#20554=DIRECTION('',(0.,0.,1.));
#20555=DIRECTION('',(1.,0.,0.));
#20556=DIRECTION('',(1.22464679914735E-16,0.,-1.));
#20557=DIRECTION('',(-1.,0.,-1.22464679914735E-16));
#20558=DIRECTION('',(0.,0.,1.));
#20559=DIRECTION('',(-1.,1.22464679914735E-16,0.));
#20560=DIRECTION('',(1.22464679914735E-16,-1.258548236767E-48,-1.));
#20561=DIRECTION('',(1.,1.22464679914735E-16,1.22464679914735E-16));
#20562=CARTESIAN_POINT('',(0.,0.,0.));
#20563=CARTESIAN_POINT('',(0.,0.,0.));
#20564=CARTESIAN_POINT('Origin',(180.,21.,55.65));
#20565=CARTESIAN_POINT('',(177.25,21.,55.8));
#20566=CARTESIAN_POINT('Origin',(180.,21.,55.8));
#20567=CARTESIAN_POINT('',(176.95,21.,55.5));
#20568=CARTESIAN_POINT('',(177.1,21.,55.65));
#20569=CARTESIAN_POINT('Origin',(180.,21.,55.5));
#20570=CARTESIAN_POINT('Origin',(0.,13.,55.5));
#20571=CARTESIAN_POINT('',(210.,31.2,55.5));
#20572=CARTESIAN_POINT('',(0.,31.2,55.5));
#20573=CARTESIAN_POINT('',(0.,31.2,55.5));
#20574=CARTESIAN_POINT('',(210.,13.,55.5));
#20575=CARTESIAN_POINT('',(210.,31.5,55.5));
#20576=CARTESIAN_POINT('',(0.,13.,55.5));
#20577=CARTESIAN_POINT('',(0.,13.,55.5));
#20578=CARTESIAN_POINT('',(0.,31.5,55.5));
#20579=CARTESIAN_POINT('',(26.95,21.,55.5));
#20580=CARTESIAN_POINT('Origin',(30.,21.,55.5));
#20581=CARTESIAN_POINT('',(126.95,21.,55.5));
#20582=CARTESIAN_POINT('Origin',(130.,21.,55.5));
#20583=CARTESIAN_POINT('',(76.95,21.,55.5));
#20584=CARTESIAN_POINT('Origin',(80.,21.,55.5));
#20585=CARTESIAN_POINT('Origin',(180.,21.,55.5));
#20586=CARTESIAN_POINT('',(177.25,21.,60.5));
#20587=CARTESIAN_POINT('',(177.25,21.,55.5));
#20588=CARTESIAN_POINT('Origin',(180.,21.,60.5));
#20589=CARTESIAN_POINT('Origin',(30.,21.,55.65));
#20590=CARTESIAN_POINT('',(27.25,21.,55.8));
#20591=CARTESIAN_POINT('Origin',(30.,21.,55.8));
#20592=CARTESIAN_POINT('',(27.1,21.,55.65));
#20593=CARTESIAN_POINT('Origin',(30.,21.,55.5));
#20594=CARTESIAN_POINT('',(27.25,21.,60.5));
#20595=CARTESIAN_POINT('',(27.25,21.,55.5));
#20596=CARTESIAN_POINT('Origin',(30.,21.,60.5));
#20597=CARTESIAN_POINT('Origin',(80.,21.,55.65));
#20598=CARTESIAN_POINT('',(77.25,21.,55.8));
#20599=CARTESIAN_POINT('Origin',(80.,21.,55.8));
#20600=CARTESIAN_POINT('',(77.1,21.,55.65));
#20601=CARTESIAN_POINT('Origin',(80.,21.,55.5));
#20602=CARTESIAN_POINT('',(77.25,21.,60.5));
#20603=CARTESIAN_POINT('',(77.25,21.,55.5));
#20604=CARTESIAN_POINT('Origin',(80.,21.,60.5));
#20605=CARTESIAN_POINT('Origin',(130.,21.,55.65));
#20606=CARTESIAN_POINT('',(127.25,21.,55.8));
#20607=CARTESIAN_POINT('Origin',(130.,21.,55.8));
#20608=CARTESIAN_POINT('',(127.1,21.,55.65));
#20609=CARTESIAN_POINT('Origin',(130.,21.,55.5));
#20610=CARTESIAN_POINT('',(127.25,21.,60.5));
#20611=CARTESIAN_POINT('',(127.25,21.,55.5));
#20612=CARTESIAN_POINT('Origin',(130.,21.,60.5));
#20613=CARTESIAN_POINT('Origin',(180.,21.,44.35));
#20614=CARTESIAN_POINT('',(177.25,21.,44.2));
#20615=CARTESIAN_POINT('Origin',(180.,21.,44.2));
#20616=CARTESIAN_POINT('',(176.95,21.,44.5));
#20617=CARTESIAN_POINT('',(177.1,21.,44.35));
#20618=CARTESIAN_POINT('Origin',(180.,21.,44.5));
#20619=CARTESIAN_POINT('Origin',(0.,31.5,44.5));
#20620=CARTESIAN_POINT('',(0.,31.2,44.5));
#20621=CARTESIAN_POINT('',(210.,31.2,44.5));
#20622=CARTESIAN_POINT('',(0.,31.2,44.5));
#20623=CARTESIAN_POINT('',(0.,13.,44.5));
#20624=CARTESIAN_POINT('',(0.,13.,44.5));
#20625=CARTESIAN_POINT('',(210.,13.,44.5));
#20626=CARTESIAN_POINT('',(0.,13.,44.5));
#20627=CARTESIAN_POINT('',(210.,13.,44.5));
#20628=CARTESIAN_POINT('',(26.95,21.,44.5));
#20629=CARTESIAN_POINT('Origin',(30.,21.,44.5));
#20630=CARTESIAN_POINT('',(126.95,21.,44.5));
#20631=CARTESIAN_POINT('Origin',(130.,21.,44.5));
#20632=CARTESIAN_POINT('',(76.95,21.,44.5));
#20633=CARTESIAN_POINT('Origin',(80.,21.,44.5));
#20634=CARTESIAN_POINT('Origin',(180.,21.,44.5));
#20635=CARTESIAN_POINT('',(177.25,21.,39.5));
#20636=CARTESIAN_POINT('',(177.25,21.,44.5));
#20637=CARTESIAN_POINT('Origin',(180.,21.,39.5));
#20638=CARTESIAN_POINT('Origin',(30.,21.,44.35));
#20639=CARTESIAN_POINT('',(27.25,21.,44.2));
#20640=CARTESIAN_POINT('Origin',(30.,21.,44.2));
#20641=CARTESIAN_POINT('',(27.1,21.,44.35));
#20642=CARTESIAN_POINT('Origin',(30.,21.,44.5));
#20643=CARTESIAN_POINT('',(27.25,21.,39.5));
#20644=CARTESIAN_POINT('',(27.25,21.,44.5));
#20645=CARTESIAN_POINT('Origin',(30.,21.,39.5));
#20646=CARTESIAN_POINT('Origin',(80.,21.,44.35));
#20647=CARTESIAN_POINT('',(77.25,21.,44.2));
#20648=CARTESIAN_POINT('Origin',(80.,21.,44.2));
#20649=CARTESIAN_POINT('',(77.1,21.,44.35));
#20650=CARTESIAN_POINT('Origin',(80.,21.,44.5));
#20651=CARTESIAN_POINT('',(77.25,21.,39.5));
#20652=CARTESIAN_POINT('',(77.25,21.,44.5));
#20653=CARTESIAN_POINT('Origin',(80.,21.,39.5));
#20654=CARTESIAN_POINT('Origin',(130.,21.,44.35));
#20655=CARTESIAN_POINT('',(127.25,21.,44.2));
#20656=CARTESIAN_POINT('Origin',(130.,21.,44.2));
#20657=CARTESIAN_POINT('',(127.1,21.,44.35));
#20658=CARTESIAN_POINT('Origin',(130.,21.,44.5));
#20659=CARTESIAN_POINT('',(127.25,21.,39.5));
#20660=CARTESIAN_POINT('',(127.25,21.,44.5));
#20661=CARTESIAN_POINT('Origin',(130.,21.,39.5));
#20662=CARTESIAN_POINT('Origin',(200.,0.2,80.));
#20663=CARTESIAN_POINT('',(196.95,0.4,80.));
#20664=CARTESIAN_POINT('Origin',(200.,0.4,80.));
#20665=CARTESIAN_POINT('',(196.55,0.,80.));
#20666=CARTESIAN_POINT('',(196.75,0.2,80.));
#20667=CARTESIAN_POINT('Origin',(200.,0.,80.));
#20668=CARTESIAN_POINT('Origin',(0.,0.,100.));
#20669=CARTESIAN_POINT('',(209.5,0.,99.5));
#20670=CARTESIAN_POINT('',(209.5,0.,0.499999999999998));
#20671=CARTESIAN_POINT('',(209.5,0.,75.));
#20672=CARTESIAN_POINT('',(0.5,0.,99.5));
#20673=CARTESIAN_POINT('',(0.,0.,99.5));
#20674=CARTESIAN_POINT('',(0.5,0.,0.499999999999998));
#20675=CARTESIAN_POINT('',(0.5,0.,75.));
#20676=CARTESIAN_POINT('',(0.,0.,0.499999999999998));
#20677=CARTESIAN_POINT('',(146.55,0.,80.));
#20678=CARTESIAN_POINT('Origin',(150.,0.,80.));
#20679=CARTESIAN_POINT('',(56.55,0.,20.));
#20680=CARTESIAN_POINT('Origin',(60.,0.,20.));
#20681=CARTESIAN_POINT('',(56.55,0.,80.));
#20682=CARTESIAN_POINT('Origin',(60.,0.,80.));
#20683=CARTESIAN_POINT('',(196.55,0.,20.));
#20684=CARTESIAN_POINT('Origin',(200.,0.,20.));
#20685=CARTESIAN_POINT('',(146.55,0.,20.));
#20686=CARTESIAN_POINT('Origin',(150.,0.,20.));
#20687=CARTESIAN_POINT('',(6.55,0.,80.));
#20688=CARTESIAN_POINT('Origin',(10.,0.,80.));
#20689=CARTESIAN_POINT('',(6.55,0.,20.));
#20690=CARTESIAN_POINT('Origin',(10.,0.,20.));
#20691=CARTESIAN_POINT('Origin',(200.,0.,80.));
#20692=CARTESIAN_POINT('',(196.95,8.,80.));
#20693=CARTESIAN_POINT('',(196.95,0.,80.));
#20694=CARTESIAN_POINT('Origin',(200.,8.,80.));
#20695=CARTESIAN_POINT('Origin',(150.,0.2,80.));
#20696=CARTESIAN_POINT('',(146.95,0.4,80.));
#20697=CARTESIAN_POINT('Origin',(150.,0.4,80.));
#20698=CARTESIAN_POINT('',(146.75,0.2,80.));
#20699=CARTESIAN_POINT('Origin',(150.,0.,80.));
#20700=CARTESIAN_POINT('',(146.95,8.,80.));
#20701=CARTESIAN_POINT('',(146.95,0.,80.));
#20702=CARTESIAN_POINT('Origin',(150.,8.,80.));
#20703=CARTESIAN_POINT('Origin',(10.,0.2,20.));
#20704=CARTESIAN_POINT('',(6.95,0.4,20.));
#20705=CARTESIAN_POINT('Origin',(10.,0.4,20.));
#20706=CARTESIAN_POINT('',(6.75,0.2,20.));
#20707=CARTESIAN_POINT('Origin',(10.,0.,20.));
#20708=CARTESIAN_POINT('',(6.95,8.,20.));
#20709=CARTESIAN_POINT('',(6.95,0.,20.));
#20710=CARTESIAN_POINT('Origin',(10.,8.,20.));
#20711=CARTESIAN_POINT('Origin',(60.,0.2,20.));
#20712=CARTESIAN_POINT('',(56.95,0.4,20.));
#20713=CARTESIAN_POINT('Origin',(60.,0.4,20.));
#20714=CARTESIAN_POINT('',(56.75,0.2,20.));
#20715=CARTESIAN_POINT('Origin',(60.,0.,20.));
#20716=CARTESIAN_POINT('',(56.95,8.,20.));
#20717=CARTESIAN_POINT('',(56.95,0.,20.));
#20718=CARTESIAN_POINT('Origin',(60.,8.,20.));
#20719=CARTESIAN_POINT('Origin',(10.,0.2,80.));
#20720=CARTESIAN_POINT('',(6.95,0.4,80.));
#20721=CARTESIAN_POINT('Origin',(10.,0.4,80.));
#20722=CARTESIAN_POINT('',(6.75,0.2,80.));
#20723=CARTESIAN_POINT('Origin',(10.,0.,80.));
#20724=CARTESIAN_POINT('',(6.95,8.,80.));
#20725=CARTESIAN_POINT('',(6.95,0.,80.));
#20726=CARTESIAN_POINT('Origin',(10.,8.,80.));
#20727=CARTESIAN_POINT('Origin',(60.,0.2,80.));
#20728=CARTESIAN_POINT('',(56.95,0.4,80.));
#20729=CARTESIAN_POINT('Origin',(60.,0.4,80.));
#20730=CARTESIAN_POINT('',(56.75,0.2,80.));
#20731=CARTESIAN_POINT('Origin',(60.,0.,80.));
#20732=CARTESIAN_POINT('',(56.95,8.,80.));
#20733=CARTESIAN_POINT('',(56.95,0.,80.));
#20734=CARTESIAN_POINT('Origin',(60.,8.,80.));
#20735=CARTESIAN_POINT('Origin',(150.,0.2,20.));
#20736=CARTESIAN_POINT('',(146.95,0.4,20.));
#20737=CARTESIAN_POINT('Origin',(150.,0.4,20.));
#20738=CARTESIAN_POINT('',(146.75,0.2,20.));
#20739=CARTESIAN_POINT('Origin',(150.,0.,20.));
#20740=CARTESIAN_POINT('',(146.95,8.,20.));
#20741=CARTESIAN_POINT('',(146.95,0.,20.));
#20742=CARTESIAN_POINT('Origin',(150.,8.,20.));
#20743=CARTESIAN_POINT('Origin',(200.,0.2,20.));
#20744=CARTESIAN_POINT('',(196.95,0.4,20.));
#20745=CARTESIAN_POINT('Origin',(200.,0.4,20.));
#20746=CARTESIAN_POINT('',(196.75,0.2,20.));
#20747=CARTESIAN_POINT('Origin',(200.,0.,20.));
#20748=CARTESIAN_POINT('',(196.95,8.,20.));
#20749=CARTESIAN_POINT('',(196.95,0.,20.));
#20750=CARTESIAN_POINT('Origin',(200.,8.,20.));
#20751=CARTESIAN_POINT('Origin',(200.,8.91631244401703,80.));
#20752=CARTESIAN_POINT('',(200.,9.83262488803406,80.));
#20753=CARTESIAN_POINT('',(198.475,8.91631244401703,80.));
#20754=CARTESIAN_POINT('Origin',(200.,8.91631244401703,20.));
#20755=CARTESIAN_POINT('',(200.,9.83262488803406,20.));
#20756=CARTESIAN_POINT('',(198.475,8.91631244401703,20.));
#20757=CARTESIAN_POINT('Origin',(150.,8.91631244401703,80.));
#20758=CARTESIAN_POINT('',(150.,9.83262488803406,80.));
#20759=CARTESIAN_POINT('',(148.475,8.91631244401703,80.));
#20760=CARTESIAN_POINT('Origin',(150.,8.91631244401703,20.));
#20761=CARTESIAN_POINT('',(150.,9.83262488803406,20.));
#20762=CARTESIAN_POINT('',(148.475,8.91631244401703,20.));
#20763=CARTESIAN_POINT('Origin',(60.,8.91631244401703,80.));
#20764=CARTESIAN_POINT('',(60.,9.83262488803406,80.));
#20765=CARTESIAN_POINT('',(58.475,8.91631244401703,80.));
#20766=CARTESIAN_POINT('Origin',(60.,8.91631244401703,20.));
#20767=CARTESIAN_POINT('',(60.,9.83262488803406,20.));
#20768=CARTESIAN_POINT('',(58.475,8.91631244401703,20.));
#20769=CARTESIAN_POINT('Origin',(10.,8.91631244401703,80.));
#20770=CARTESIAN_POINT('',(10.,9.83262488803406,80.));
#20771=CARTESIAN_POINT('',(8.475,8.91631244401703,80.));
#20772=CARTESIAN_POINT('Origin',(10.,8.91631244401703,20.));
#20773=CARTESIAN_POINT('',(10.,9.83262488803406,20.));
#20774=CARTESIAN_POINT('',(8.475,8.91631244401703,20.));
#20775=CARTESIAN_POINT('Origin',(209.75,7.875,0.249999999999999));
#20776=CARTESIAN_POINT('',(209.5,12.5,0.));
#20777=CARTESIAN_POINT('',(210.,13.,0.499999999999998));
#20778=CARTESIAN_POINT('',(173.979166666666,-23.0208333333335,-35.5208333333335));
#20779=CARTESIAN_POINT('',(210.,0.5,0.499999999999998));
#20780=CARTESIAN_POINT('',(210.,7.875,0.499999999999998));
#20781=CARTESIAN_POINT('',(209.75,0.250000000000012,0.249999999999995));
#20782=CARTESIAN_POINT('',(223.479166666667,13.9791666666665,13.9791666666665));
#20783=CARTESIAN_POINT('',(209.5,0.5,0.));
#20784=CARTESIAN_POINT('',(173.520833333333,36.4791666666669,-35.9791666666668));
#20785=CARTESIAN_POINT('',(209.5,7.875,0.));
#20786=CARTESIAN_POINT('Origin',(209.75,0.25,75.));
#20787=CARTESIAN_POINT('',(210.,0.5,99.5));
#20788=CARTESIAN_POINT('',(210.,0.5,75.));
#20789=CARTESIAN_POINT('',(209.75,0.249999999999986,99.75));
#20790=CARTESIAN_POINT('',(216.229166666667,6.72916666666661,93.2708333333333));
#20791=CARTESIAN_POINT('',(170.666666666666,-38.8333333333332,60.6666666666663));
#20792=CARTESIAN_POINT('',(162.333333333333,-47.1666666666668,47.6666666666666));
#20793=CARTESIAN_POINT('Origin',(210.,15.75,50.));
#20794=CARTESIAN_POINT('',(210.,13.,24.));
#20795=CARTESIAN_POINT('',(210.,13.,24.));
#20796=CARTESIAN_POINT('',(210.,5.5,24.));
#20797=CARTESIAN_POINT('',(210.,5.5,24.));
#20798=CARTESIAN_POINT('',(210.,5.5,39.5));
#20799=CARTESIAN_POINT('',(210.,5.5,39.5));
#20800=CARTESIAN_POINT('',(210.,31.2,39.5));
#20801=CARTESIAN_POINT('',(210.,31.5,39.5));
#20802=CARTESIAN_POINT('',(210.,31.5,39.8));
#20803=CARTESIAN_POINT('',(210.,30.0374999999999,38.3375));
#20804=CARTESIAN_POINT('',(210.,31.5,44.2));
#20805=CARTESIAN_POINT('',(210.,31.5,44.5));
#20806=CARTESIAN_POINT('',(210.,26.0375000000001,49.6625));
#20807=CARTESIAN_POINT('',(210.,13.,55.5));
#20808=CARTESIAN_POINT('',(210.,31.5,55.8));
#20809=CARTESIAN_POINT('',(210.,26.0375000000001,50.3375));
#20810=CARTESIAN_POINT('',(210.,31.5,60.2));
#20811=CARTESIAN_POINT('',(210.,31.5,60.5));
#20812=CARTESIAN_POINT('',(210.,31.2,60.5));
#20813=CARTESIAN_POINT('',(210.,30.0375000000001,61.6625));
#20814=CARTESIAN_POINT('',(210.,5.5,60.5));
#20815=CARTESIAN_POINT('',(210.,5.5,60.5));
#20816=CARTESIAN_POINT('',(210.,5.5,76.));
#20817=CARTESIAN_POINT('',(210.,5.5,76.));
#20818=CARTESIAN_POINT('',(210.,13.,76.));
#20819=CARTESIAN_POINT('',(210.,13.,76.));
#20820=CARTESIAN_POINT('',(210.,13.,99.5));
#20821=CARTESIAN_POINT('',(210.,13.,100.));
#20822=CARTESIAN_POINT('',(210.,14.375,99.5));
#20823=CARTESIAN_POINT('Origin',(0.,12.75,0.25));
#20824=CARTESIAN_POINT('',(0.5,12.5,0.));
#20825=CARTESIAN_POINT('',(0.,12.5,0.));
#20826=CARTESIAN_POINT('',(0.,13.,0.499999999999998));
#20827=CARTESIAN_POINT('',(1.02083333333333,11.9791666666667,-0.520833333333332));
#20828=CARTESIAN_POINT('',(0.,13.,0.5));
#20829=CARTESIAN_POINT('Origin',(0.,0.25,99.75));
#20830=CARTESIAN_POINT('',(209.5,0.5,100.));
#20831=CARTESIAN_POINT('',(172.4375,37.5624999999998,137.0625));
#20832=CARTESIAN_POINT('',(0.5,0.5,100.));
#20833=CARTESIAN_POINT('',(0.,0.5,100.));
#20834=CARTESIAN_POINT('',(0.25,0.250000000000001,99.75));
#20835=CARTESIAN_POINT('',(2.56249999999998,2.56249999999998,102.0625));
#20836=CARTESIAN_POINT('',(4.33333333333335,-3.83333333333335,95.6666666666666));
#20837=CARTESIAN_POINT('Origin',(209.75,14.375,99.75));
#20838=CARTESIAN_POINT('',(209.5,12.5,100.));
#20839=CARTESIAN_POINT('',(175.0625,-21.9374999999999,134.4375));
#20840=CARTESIAN_POINT('',(209.5,14.375,100.));
#20841=CARTESIAN_POINT('Origin',(0.,13.,100.));
#20842=CARTESIAN_POINT('',(0.5,12.5,100.));
#20843=CARTESIAN_POINT('',(0.,12.5,100.));
#20844=CARTESIAN_POINT('',(0.5,14.375,100.));
#20845=CARTESIAN_POINT('Origin',(0.25,14.375,99.75));
#20846=CARTESIAN_POINT('',(0.,13.,99.5));
#20847=CARTESIAN_POINT('',(-0.0624999999999985,13.0625,99.4375));
#20848=CARTESIAN_POINT('',(0.,0.5,99.5));
#20849=CARTESIAN_POINT('',(0.,14.375,99.5));
#20850=CARTESIAN_POINT('',(-6.22916666666666,6.72916666666667,93.2708333333333));
#20851=CARTESIAN_POINT('Origin',(0.25,0.25,75.));
#20852=CARTESIAN_POINT('',(0.,0.5,0.499999999999998));
#20853=CARTESIAN_POINT('',(0.,0.5,75.));
#20854=CARTESIAN_POINT('',(0.25,0.25,0.25));
#20855=CARTESIAN_POINT('',(-13.4791666666666,13.9791666666667,13.9791666666666));
#20856=CARTESIAN_POINT('',(12.6666666666666,-12.1666666666667,12.6666666666666));
#20857=CARTESIAN_POINT('Origin',(0.,0.25,0.249999999999999));
#20858=CARTESIAN_POINT('',(0.5,0.5,0.));
#20859=CARTESIAN_POINT('',(1.47916666666667,1.47916666666667,-0.979166666666666));
#20860=CARTESIAN_POINT('',(0.,0.5,0.));
#20861=CARTESIAN_POINT('Origin',(0.25,7.875,0.249999999999999));
#20862=CARTESIAN_POINT('',(0.,7.875,0.499999999999998));
#20863=CARTESIAN_POINT('',(0.5,7.875,0.));
#20864=CARTESIAN_POINT('Origin',(0.,15.75,50.));
#20865=CARTESIAN_POINT('',(0.,13.,76.));
#20866=CARTESIAN_POINT('',(0.,13.,100.));
#20867=CARTESIAN_POINT('',(0.,5.5,76.));
#20868=CARTESIAN_POINT('',(0.,13.,76.));
#20869=CARTESIAN_POINT('',(0.,5.5,60.5));
#20870=CARTESIAN_POINT('',(0.,5.5,76.));
#20871=CARTESIAN_POINT('',(0.,31.2,60.5));
#20872=CARTESIAN_POINT('',(0.,5.5,60.5));
#20873=CARTESIAN_POINT('',(0.,31.5,60.2));
#20874=CARTESIAN_POINT('',(0.,30.0375000000001,61.6625));
#20875=CARTESIAN_POINT('',(0.,31.5,55.8));
#20876=CARTESIAN_POINT('',(0.,31.5,60.5));
#20877=CARTESIAN_POINT('',(0.,26.0375000000001,50.3375));
#20878=CARTESIAN_POINT('',(0.,13.,55.5));
#20879=CARTESIAN_POINT('',(0.,31.5,44.2));
#20880=CARTESIAN_POINT('',(0.,26.0375000000001,49.6625));
#20881=CARTESIAN_POINT('',(0.,31.5,39.8));
#20882=CARTESIAN_POINT('',(0.,31.5,44.5));
#20883=CARTESIAN_POINT('',(0.,31.2,39.5));
#20884=CARTESIAN_POINT('',(0.,30.0374999999999,38.3375));
#20885=CARTESIAN_POINT('',(0.,5.5,39.5));
#20886=CARTESIAN_POINT('',(0.,31.5,39.5));
#20887=CARTESIAN_POINT('',(0.,5.5,24.));
#20888=CARTESIAN_POINT('',(0.,5.5,39.5));
#20889=CARTESIAN_POINT('',(0.,13.,24.));
#20890=CARTESIAN_POINT('',(0.,5.5,24.));
#20891=CARTESIAN_POINT('',(0.,13.,24.));
#20892=CARTESIAN_POINT('Origin',(0.,31.35,39.65));
#20893=CARTESIAN_POINT('',(0.,31.2,39.5));
#20894=CARTESIAN_POINT('',(0.,31.5,39.8));
#20895=CARTESIAN_POINT('Origin',(0.,31.5,39.5));
#20896=CARTESIAN_POINT('',(0.,31.5,44.2));
#20897=CARTESIAN_POINT('Origin',(0.,31.35,44.35));
#20898=CARTESIAN_POINT('Origin',(0.,31.35,55.65));
#20899=CARTESIAN_POINT('',(0.,31.5,55.8));
#20900=CARTESIAN_POINT('Origin',(0.,31.5,55.5));
#20901=CARTESIAN_POINT('',(0.,31.5,60.2));
#20902=CARTESIAN_POINT('Origin',(0.,31.35,60.35));
#20903=CARTESIAN_POINT('',(0.,31.2,60.5));
#20904=CARTESIAN_POINT('Origin',(0.,31.5,60.5));
#20905=CARTESIAN_POINT('',(0.,5.5,60.5));
#20906=CARTESIAN_POINT('Origin',(0.,12.75,99.75));
#20907=CARTESIAN_POINT('',(0.,13.,99.5));
#20908=CARTESIAN_POINT('Origin',(0.,13.,0.));
#20909=CARTESIAN_POINT('',(0.,13.,24.));
#20910=CARTESIAN_POINT('Origin',(0.,0.,0.));
#20911=CARTESIAN_POINT('Origin',(0.,13.,76.));
#20912=CARTESIAN_POINT('',(0.,13.,76.));
#20913=CARTESIAN_POINT('Origin',(0.,5.5,76.));
#20914=CARTESIAN_POINT('',(0.,5.5,76.));
#20915=CARTESIAN_POINT('Origin',(0.,5.5,60.5));
#20916=CARTESIAN_POINT('Origin',(0.,13.,44.5));
#20917=CARTESIAN_POINT('Origin',(0.,5.5,39.5));
#20918=CARTESIAN_POINT('',(0.,5.5,39.5));
#20919=CARTESIAN_POINT('Origin',(0.,5.5,24.));
#20920=CARTESIAN_POINT('',(0.,5.5,24.));
#20921=CARTESIAN_POINT('Origin',(0.,13.,24.));
#20922=CARTESIAN_POINT('',(0.,0.,0.));
#20923=CARTESIAN_POINT('Origin',(155.,29.,99.85));
#20924=CARTESIAN_POINT('',(152.45,29.,99.7));
#20925=CARTESIAN_POINT('Origin',(155.,29.,99.7));
#20926=CARTESIAN_POINT('',(152.15,29.,100.));
#20927=CARTESIAN_POINT('',(152.3,29.,99.85));
#20928=CARTESIAN_POINT('',(154.259173435261,26.24796875,100.));
#20929=CARTESIAN_POINT('Origin',(155.,29.,100.));
#20930=CARTESIAN_POINT('',(155.740826564739,26.24796875,100.));
#20931=CARTESIAN_POINT('Ctrl Pts',(154.259173435261,26.24796875,99.9999999999999));
#20932=CARTESIAN_POINT('Ctrl Pts',(154.508665267946,26.2326405180042,99.9499486302178));
#20933=CARTESIAN_POINT('Ctrl Pts',(154.758456056481,26.225,99.925));
#20934=CARTESIAN_POINT('Ctrl Pts',(155.241543943519,26.225,99.925));
#20935=CARTESIAN_POINT('Ctrl Pts',(155.491334732054,26.2326405180042,99.9499486302178));
#20936=CARTESIAN_POINT('Ctrl Pts',(155.740826564739,26.24796875,99.9999999999999));
#20937=CARTESIAN_POINT('Origin',(155.,29.,100.));
#20938=CARTESIAN_POINT('Origin',(155.,21.,99.85));
#20939=CARTESIAN_POINT('',(150.,21.,99.7));
#20940=CARTESIAN_POINT('Origin',(155.,21.,99.7));
#20941=CARTESIAN_POINT('',(149.7,21.,100.));
#20942=CARTESIAN_POINT('',(149.85,21.,99.85));
#20943=CARTESIAN_POINT('Origin',(155.,21.,100.));
#20944=CARTESIAN_POINT('Origin',(155.,21.,100.));
#20945=CARTESIAN_POINT('Origin',(155.,29.,100.));
#20946=CARTESIAN_POINT('',(152.45,29.,75.5));
#20947=CARTESIAN_POINT('',(152.45,29.,100.));
#20948=CARTESIAN_POINT('Origin',(155.,29.,75.5));
#20949=CARTESIAN_POINT('Origin',(105.,29.,99.85));
#20950=CARTESIAN_POINT('',(102.45,29.,99.7));
#20951=CARTESIAN_POINT('Origin',(105.,29.,99.7));
#20952=CARTESIAN_POINT('',(102.15,29.,100.));
#20953=CARTESIAN_POINT('',(102.3,29.,99.85));
#20954=CARTESIAN_POINT('',(104.259173435261,26.24796875,100.));
#20955=CARTESIAN_POINT('Origin',(105.,29.,100.));
#20956=CARTESIAN_POINT('',(105.740826564739,26.24796875,100.));
#20957=CARTESIAN_POINT('Ctrl Pts',(104.259173435261,26.24796875,99.9999999999999));
#20958=CARTESIAN_POINT('Ctrl Pts',(104.508665267946,26.2326405180042,99.9499486302178));
#20959=CARTESIAN_POINT('Ctrl Pts',(104.758456056481,26.225,99.925));
#20960=CARTESIAN_POINT('Ctrl Pts',(105.241543943519,26.225,99.925));
#20961=CARTESIAN_POINT('Ctrl Pts',(105.491334732054,26.2326405180042,99.9499486302178));
#20962=CARTESIAN_POINT('Ctrl Pts',(105.740826564739,26.24796875,99.9999999999999));
#20963=CARTESIAN_POINT('Origin',(105.,29.,100.));
#20964=CARTESIAN_POINT('Origin',(105.,21.,99.85));
#20965=CARTESIAN_POINT('',(100.,21.,99.7));
#20966=CARTESIAN_POINT('Origin',(105.,21.,99.7));
#20967=CARTESIAN_POINT('',(99.7,21.,100.));
#20968=CARTESIAN_POINT('',(99.85,21.,99.85));
#20969=CARTESIAN_POINT('Origin',(105.,21.,100.));
#20970=CARTESIAN_POINT('Origin',(105.,21.,100.));
#20971=CARTESIAN_POINT('Origin',(105.,29.,100.));
#20972=CARTESIAN_POINT('',(102.45,29.,75.5));
#20973=CARTESIAN_POINT('',(102.45,29.,100.));
#20974=CARTESIAN_POINT('Origin',(105.,29.,75.5));
#20975=CARTESIAN_POINT('Origin',(55.,29.,99.85));
#20976=CARTESIAN_POINT('',(52.45,29.,99.7));
#20977=CARTESIAN_POINT('Origin',(55.,29.,99.7));
#20978=CARTESIAN_POINT('',(52.15,29.,100.));
#20979=CARTESIAN_POINT('',(52.3,29.,99.85));
#20980=CARTESIAN_POINT('',(54.2591734352607,26.24796875,100.));
#20981=CARTESIAN_POINT('Origin',(55.,29.,100.));
#20982=CARTESIAN_POINT('',(55.7408265647393,26.24796875,100.));
#20983=CARTESIAN_POINT('Ctrl Pts',(54.2591734352607,26.24796875,100.));
#20984=CARTESIAN_POINT('Ctrl Pts',(54.5086652679461,26.2326405180042,99.9499486302178));
#20985=CARTESIAN_POINT('Ctrl Pts',(54.7584560564804,26.225,99.925));
#20986=CARTESIAN_POINT('Ctrl Pts',(55.2415439435196,26.225,99.925));
#20987=CARTESIAN_POINT('Ctrl Pts',(55.4913347320539,26.2326405180042,99.9499486302178));
#20988=CARTESIAN_POINT('Ctrl Pts',(55.7408265647393,26.24796875,100.));
#20989=CARTESIAN_POINT('Origin',(55.,29.,100.));
#20990=CARTESIAN_POINT('Origin',(55.,21.,99.85));
#20991=CARTESIAN_POINT('',(50.,21.,99.7));
#20992=CARTESIAN_POINT('Origin',(55.,21.,99.7));
#20993=CARTESIAN_POINT('',(49.7,21.,100.));
#20994=CARTESIAN_POINT('',(49.85,21.,99.85));
#20995=CARTESIAN_POINT('Origin',(55.,21.,100.));
#20996=CARTESIAN_POINT('Origin',(55.,21.,100.));
#20997=CARTESIAN_POINT('Origin',(55.,29.,100.));
#20998=CARTESIAN_POINT('',(52.45,29.,75.5));
#20999=CARTESIAN_POINT('',(52.45,29.,100.));
#21000=CARTESIAN_POINT('Origin',(55.,29.,75.5));
#21001=CARTESIAN_POINT('Origin',(0.,45.,100.));
#21002=CARTESIAN_POINT('',(209.5,44.5,100.));
#21003=CARTESIAN_POINT('',(209.5,14.5,100.));
#21004=CARTESIAN_POINT('',(209.5,37.25,100.));
#21005=CARTESIAN_POINT('',(0.5,44.5,100.));
#21006=CARTESIAN_POINT('',(0.,44.5,100.));
#21007=CARTESIAN_POINT('',(0.5,14.5,100.));
#21008=CARTESIAN_POINT('',(0.5,37.25,100.));
#21009=CARTESIAN_POINT('',(0.,14.5,100.));
#21010=CARTESIAN_POINT('Origin',(155.,21.,100.));
#21011=CARTESIAN_POINT('',(150.,21.,92.5));
#21012=CARTESIAN_POINT('',(150.,21.,100.));
#21013=CARTESIAN_POINT('Origin',(155.,21.,92.5));
#21014=CARTESIAN_POINT('Origin',(105.,21.,100.));
#21015=CARTESIAN_POINT('',(100.,21.,92.5));
#21016=CARTESIAN_POINT('',(100.,21.,100.));
#21017=CARTESIAN_POINT('Origin',(105.,21.,92.5));
#21018=CARTESIAN_POINT('Origin',(55.,21.,100.));
#21019=CARTESIAN_POINT('',(50.,21.,92.5));
#21020=CARTESIAN_POINT('',(50.,21.,100.));
#21021=CARTESIAN_POINT('Origin',(55.,21.,92.5));
#21022=CARTESIAN_POINT('Origin',(55.,21.,92.5));
#21023=CARTESIAN_POINT('',(52.,21.,92.5));
#21024=CARTESIAN_POINT('Origin',(55.,21.,92.5));
#21025=CARTESIAN_POINT('Origin',(105.,21.,92.5));
#21026=CARTESIAN_POINT('',(102.,21.,92.5));
#21027=CARTESIAN_POINT('Origin',(105.,21.,92.5));
#21028=CARTESIAN_POINT('Origin',(155.,21.,92.5));
#21029=CARTESIAN_POINT('',(152.,21.,92.5));
#21030=CARTESIAN_POINT('Origin',(155.,21.,92.5));
#21031=CARTESIAN_POINT('Origin',(55.,21.,100.));
#21032=CARTESIAN_POINT('',(52.,21.,75.5));
#21033=CARTESIAN_POINT('',(52.,21.,100.));
#21034=CARTESIAN_POINT('Origin',(55.,21.,75.5));
#21035=CARTESIAN_POINT('Origin',(105.,21.,100.));
#21036=CARTESIAN_POINT('',(102.,21.,75.5));
#21037=CARTESIAN_POINT('',(102.,21.,100.));
#21038=CARTESIAN_POINT('Origin',(105.,21.,75.5));
#21039=CARTESIAN_POINT('Origin',(155.,21.,100.));
#21040=CARTESIAN_POINT('',(152.,21.,75.5));
#21041=CARTESIAN_POINT('',(152.,21.,100.));
#21042=CARTESIAN_POINT('Origin',(155.,21.,75.5));
#21043=CARTESIAN_POINT('Origin',(155.,29.,0.15));
#21044=CARTESIAN_POINT('',(152.45,29.,0.3));
#21045=CARTESIAN_POINT('Origin',(155.,29.,0.3));
#21046=CARTESIAN_POINT('',(152.15,29.,-4.59701721133854E-15));
#21047=CARTESIAN_POINT('',(152.3,29.,0.15));
#21048=CARTESIAN_POINT('',(155.740826564739,26.24796875,0.));
#21049=CARTESIAN_POINT('Origin',(155.,29.,0.));
#21050=CARTESIAN_POINT('',(154.259173435261,26.24796875,0.));
#21051=CARTESIAN_POINT('Ctrl Pts',(155.740826564739,26.24796875,6.73332917200398E-14));
#21052=CARTESIAN_POINT('Ctrl Pts',(155.491334732054,26.2326405180042,0.0500513697821895));
#21053=CARTESIAN_POINT('Ctrl Pts',(155.241543943519,26.225,0.0750000000000045));
#21054=CARTESIAN_POINT('Ctrl Pts',(154.758456056481,26.225,0.0750000000000045));
#21055=CARTESIAN_POINT('Ctrl Pts',(154.508665267946,26.2326405180042,0.0500513697821932));
#21056=CARTESIAN_POINT('Ctrl Pts',(154.259173435261,26.24796875,7.24507259741713E-14));
#21057=CARTESIAN_POINT('Origin',(155.,29.,0.));
#21058=CARTESIAN_POINT('Origin',(155.,21.,0.15));
#21059=CARTESIAN_POINT('',(150.,21.,0.3));
#21060=CARTESIAN_POINT('Origin',(155.,21.,0.3));
#21061=CARTESIAN_POINT('',(149.7,21.,-9.19403442267708E-15));
#21062=CARTESIAN_POINT('',(149.85,21.,0.15));
#21063=CARTESIAN_POINT('Origin',(155.,21.,0.));
#21064=CARTESIAN_POINT('Origin',(155.,21.,0.));
#21065=CARTESIAN_POINT('Origin',(155.,29.,0.));
#21066=CARTESIAN_POINT('',(152.45,29.,24.5));
#21067=CARTESIAN_POINT('',(152.45,29.,0.));
#21068=CARTESIAN_POINT('Origin',(155.,29.,24.5));
#21069=CARTESIAN_POINT('Origin',(105.,29.,0.15));
#21070=CARTESIAN_POINT('',(102.45,29.,0.3));
#21071=CARTESIAN_POINT('Origin',(105.,29.,0.3));
#21072=CARTESIAN_POINT('',(102.15,29.,-4.59701721133854E-15));
#21073=CARTESIAN_POINT('',(102.3,29.,0.15));
#21074=CARTESIAN_POINT('',(105.740826564739,26.24796875,0.));
#21075=CARTESIAN_POINT('Origin',(105.,29.,0.));
#21076=CARTESIAN_POINT('',(104.259173435261,26.24796875,0.));
#21077=CARTESIAN_POINT('Ctrl Pts',(105.740826564739,26.24796875,5.15299608538911E-14));
#21078=CARTESIAN_POINT('Ctrl Pts',(105.491334732054,26.2326405180042,0.0500513697821832));
#21079=CARTESIAN_POINT('Ctrl Pts',(105.241543943519,26.225,0.0749999999999978));
#21080=CARTESIAN_POINT('Ctrl Pts',(104.758456056481,26.225,0.0749999999999978));
#21081=CARTESIAN_POINT('Ctrl Pts',(104.508665267946,26.2326405180042,0.0500513697821799));
#21082=CARTESIAN_POINT('Ctrl Pts',(104.259173435261,26.24796875,5.67341312818215E-14));
#21083=CARTESIAN_POINT('Origin',(105.,29.,0.));
#21084=CARTESIAN_POINT('Origin',(105.,21.,0.15));
#21085=CARTESIAN_POINT('',(100.,21.,0.3));
#21086=CARTESIAN_POINT('Origin',(105.,21.,0.3));
#21087=CARTESIAN_POINT('',(99.7,21.,1.50920942409982E-15));
#21088=CARTESIAN_POINT('',(99.85,21.,0.15));
#21089=CARTESIAN_POINT('Origin',(105.,21.,0.));
#21090=CARTESIAN_POINT('Origin',(105.,21.,0.));
#21091=CARTESIAN_POINT('Origin',(105.,29.,0.));
#21092=CARTESIAN_POINT('',(102.45,29.,24.5));
#21093=CARTESIAN_POINT('',(102.45,29.,0.));
#21094=CARTESIAN_POINT('Origin',(105.,29.,24.5));
#21095=CARTESIAN_POINT('Origin',(55.,29.,0.15));
#21096=CARTESIAN_POINT('',(52.45,29.,0.3));
#21097=CARTESIAN_POINT('Origin',(55.,29.,0.3));
#21098=CARTESIAN_POINT('',(52.15,29.,-2.41126563160776E-15));
#21099=CARTESIAN_POINT('',(52.3,29.,0.15));
#21100=CARTESIAN_POINT('',(55.7408265647393,26.24796875,0.));
#21101=CARTESIAN_POINT('Origin',(55.,29.,0.));
#21102=CARTESIAN_POINT('',(54.2591734352607,26.24796875,0.));
#21103=CARTESIAN_POINT('Ctrl Pts',(55.7408265647393,26.24796875,-2.9316826744008E-15));
#21104=CARTESIAN_POINT('Ctrl Pts',(55.4913347320539,26.2326405180042,0.0500513697821647));
#21105=CARTESIAN_POINT('Ctrl Pts',(55.2415439435196,26.225,0.0749999999999999));
#21106=CARTESIAN_POINT('Ctrl Pts',(54.7584560564804,26.225,0.0749999999999999));
#21107=CARTESIAN_POINT('Ctrl Pts',(54.5086652679461,26.2326405180042,0.0500513697821644));
#21108=CARTESIAN_POINT('Ctrl Pts',(54.2591734352607,26.24796875,1.21430643318376E-15));
#21109=CARTESIAN_POINT('Origin',(55.,29.,0.));
#21110=CARTESIAN_POINT('Origin',(55.,21.,0.15));
#21111=CARTESIAN_POINT('',(50.,21.,0.3));
#21112=CARTESIAN_POINT('Origin',(55.,21.,0.3));
#21113=CARTESIAN_POINT('',(49.7,21.,-2.4980018054066E-15));
#21114=CARTESIAN_POINT('',(49.85,21.,0.15));
#21115=CARTESIAN_POINT('Origin',(55.,21.,0.));
#21116=CARTESIAN_POINT('Origin',(55.,21.,0.));
#21117=CARTESIAN_POINT('Origin',(55.,29.,0.));
#21118=CARTESIAN_POINT('',(52.45,29.,24.5));
#21119=CARTESIAN_POINT('',(52.45,29.,0.));
#21120=CARTESIAN_POINT('Origin',(55.,29.,24.5));
#21121=CARTESIAN_POINT('Origin',(0.,14.,0.));
#21122=CARTESIAN_POINT('',(209.5,14.5,0.));
#21123=CARTESIAN_POINT('',(209.5,44.5,0.));
#21124=CARTESIAN_POINT('',(209.5,21.75,0.));
#21125=CARTESIAN_POINT('',(0.5,14.5,0.));
#21126=CARTESIAN_POINT('',(0.,14.5,0.));
#21127=CARTESIAN_POINT('',(0.5,44.5,0.));
#21128=CARTESIAN_POINT('',(0.5,21.75,0.));
#21129=CARTESIAN_POINT('',(0.,44.5,0.));
#21130=CARTESIAN_POINT('Origin',(155.,21.,0.));
#21131=CARTESIAN_POINT('',(150.,21.,7.5));
#21132=CARTESIAN_POINT('',(150.,21.,0.));
#21133=CARTESIAN_POINT('Origin',(155.,21.,7.5));
#21134=CARTESIAN_POINT('Origin',(105.,21.,0.));
#21135=CARTESIAN_POINT('',(100.,21.,7.5));
#21136=CARTESIAN_POINT('',(100.,21.,0.));
#21137=CARTESIAN_POINT('Origin',(105.,21.,7.5));
#21138=CARTESIAN_POINT('Origin',(55.,21.,0.));
#21139=CARTESIAN_POINT('',(50.,21.,7.5));
#21140=CARTESIAN_POINT('',(50.,21.,0.));
#21141=CARTESIAN_POINT('Origin',(55.,21.,7.5));
#21142=CARTESIAN_POINT('Origin',(55.,21.,7.5));
#21143=CARTESIAN_POINT('',(52.,21.,7.5));
#21144=CARTESIAN_POINT('Origin',(55.,21.,7.5));
#21145=CARTESIAN_POINT('Origin',(105.,21.,7.5));
#21146=CARTESIAN_POINT('',(102.,21.,7.5));
#21147=CARTESIAN_POINT('Origin',(105.,21.,7.5));
#21148=CARTESIAN_POINT('Origin',(155.,21.,7.5));
#21149=CARTESIAN_POINT('',(152.,21.,7.5));
#21150=CARTESIAN_POINT('Origin',(155.,21.,7.5));
#21151=CARTESIAN_POINT('Origin',(55.,21.,0.));
#21152=CARTESIAN_POINT('',(52.,21.,24.5));
#21153=CARTESIAN_POINT('',(52.,21.,0.));
#21154=CARTESIAN_POINT('Origin',(55.,21.,24.5));
#21155=CARTESIAN_POINT('Origin',(105.,21.,0.));
#21156=CARTESIAN_POINT('',(102.,21.,24.5));
#21157=CARTESIAN_POINT('',(102.,21.,0.));
#21158=CARTESIAN_POINT('Origin',(105.,21.,24.5));
#21159=CARTESIAN_POINT('Origin',(155.,21.,0.));
#21160=CARTESIAN_POINT('',(152.,21.,24.5));
#21161=CARTESIAN_POINT('',(152.,21.,0.));
#21162=CARTESIAN_POINT('Origin',(155.,21.,24.5));
#21163=CARTESIAN_POINT('Origin',(209.85,30.,96.));
#21164=CARTESIAN_POINT('',(209.7,30.,98.05));
#21165=CARTESIAN_POINT('Origin',(209.7,30.,96.));
#21166=CARTESIAN_POINT('',(210.,30.,98.35));
#21167=CARTESIAN_POINT('',(209.85,30.,98.2));
#21168=CARTESIAN_POINT('Origin',(210.,30.,96.));
#21169=CARTESIAN_POINT('Origin',(210.,29.5,50.));
#21170=CARTESIAN_POINT('',(210.,14.,99.5));
#21171=CARTESIAN_POINT('',(210.,44.5,99.5));
#21172=CARTESIAN_POINT('',(210.,37.25,99.5));
#21173=CARTESIAN_POINT('',(210.,14.,75.8));
#21174=CARTESIAN_POINT('',(210.,14.,100.));
#21175=CARTESIAN_POINT('',(210.,14.3,75.5));
#21176=CARTESIAN_POINT('',(210.,24.4,65.4));
#21177=CARTESIAN_POINT('',(210.,36.5,75.5));
#21178=CARTESIAN_POINT('',(210.,14.,75.5));
#21179=CARTESIAN_POINT('',(210.,36.5,60.));
#21180=CARTESIAN_POINT('',(210.,36.5,75.5));
#21181=CARTESIAN_POINT('',(210.,32.,60.));
#21182=CARTESIAN_POINT('',(210.,36.5,60.));
#21183=CARTESIAN_POINT('',(210.,32.,40.));
#21184=CARTESIAN_POINT('',(210.,32.,60.));
#21185=CARTESIAN_POINT('',(210.,36.5,40.));
#21186=CARTESIAN_POINT('',(210.,32.,40.));
#21187=CARTESIAN_POINT('',(210.,36.5,24.5));
#21188=CARTESIAN_POINT('',(210.,36.5,40.));
#21189=CARTESIAN_POINT('',(210.,14.3,24.5));
#21190=CARTESIAN_POINT('',(210.,36.5,24.5));
#21191=CARTESIAN_POINT('',(210.,14.,24.2));
#21192=CARTESIAN_POINT('',(210.,24.4000000000001,34.5999999999999));
#21193=CARTESIAN_POINT('',(210.,14.,0.499999999999998));
#21194=CARTESIAN_POINT('',(210.,14.,24.5));
#21195=CARTESIAN_POINT('',(210.,44.5,0.499999999999998));
#21196=CARTESIAN_POINT('',(210.,21.75,0.499999999999998));
#21197=CARTESIAN_POINT('',(210.,44.5,25.));
#21198=CARTESIAN_POINT('',(210.,37.,22.35));
#21199=CARTESIAN_POINT('Origin',(210.,37.,20.));
#21200=CARTESIAN_POINT('',(210.,30.,6.35));
#21201=CARTESIAN_POINT('Origin',(210.,30.,4.));
#21202=CARTESIAN_POINT('',(210.,37.,82.35));
#21203=CARTESIAN_POINT('Origin',(210.,37.,80.));
#21204=CARTESIAN_POINT('Origin',(210.,30.,96.));
#21205=CARTESIAN_POINT('',(202.,30.,98.05));
#21206=CARTESIAN_POINT('',(210.,30.,98.05));
#21207=CARTESIAN_POINT('',(202.,27.95,96.));
#21208=CARTESIAN_POINT('Origin',(202.,30.,96.));
#21209=CARTESIAN_POINT('Origin',(202.,30.,96.));
#21210=CARTESIAN_POINT('Origin',(209.85,37.,20.));
#21211=CARTESIAN_POINT('',(209.7,37.,22.05));
#21212=CARTESIAN_POINT('Origin',(209.7,37.,20.));
#21213=CARTESIAN_POINT('',(209.85,37.,22.2));
#21214=CARTESIAN_POINT('Origin',(210.,37.,20.));
#21215=CARTESIAN_POINT('',(202.,37.,22.05));
#21216=CARTESIAN_POINT('',(210.,37.,22.05));
#21217=CARTESIAN_POINT('',(202.,34.95,20.));
#21218=CARTESIAN_POINT('Origin',(202.,37.,20.));
#21219=CARTESIAN_POINT('Origin',(202.,37.,20.));
#21220=CARTESIAN_POINT('Origin',(209.85,37.,80.));
#21221=CARTESIAN_POINT('',(209.7,37.,82.05));
#21222=CARTESIAN_POINT('Origin',(209.7,37.,80.));
#21223=CARTESIAN_POINT('',(209.85,37.,82.2));
#21224=CARTESIAN_POINT('Origin',(210.,37.,80.));
#21225=CARTESIAN_POINT('',(202.,37.,82.05));
#21226=CARTESIAN_POINT('',(210.,37.,82.05));
#21227=CARTESIAN_POINT('',(202.,34.95,80.));
#21228=CARTESIAN_POINT('Origin',(202.,37.,80.));
#21229=CARTESIAN_POINT('Origin',(202.,37.,80.));
#21230=CARTESIAN_POINT('Origin',(209.85,30.,4.));
#21231=CARTESIAN_POINT('',(209.7,30.,6.05));
#21232=CARTESIAN_POINT('Origin',(209.7,30.,4.));
#21233=CARTESIAN_POINT('',(209.85,30.,6.2));
#21234=CARTESIAN_POINT('Origin',(210.,30.,4.));
#21235=CARTESIAN_POINT('',(202.,30.,6.05));
#21236=CARTESIAN_POINT('',(210.,30.,6.05));
#21237=CARTESIAN_POINT('',(202.,27.95,4.));
#21238=CARTESIAN_POINT('Origin',(202.,30.,4.));
#21239=CARTESIAN_POINT('Origin',(202.,30.,4.));
#21240=CARTESIAN_POINT('Origin',(201.384117865497,30.,96.));
#21241=CARTESIAN_POINT('',(200.768235730993,30.,96.));
#21242=CARTESIAN_POINT('',(201.384117865497,28.975,96.));
#21243=CARTESIAN_POINT('Origin',(201.384117865497,30.,4.));
#21244=CARTESIAN_POINT('',(200.768235730993,30.,4.));
#21245=CARTESIAN_POINT('',(201.384117865497,28.975,4.));
#21246=CARTESIAN_POINT('Origin',(201.384117865497,37.,80.));
#21247=CARTESIAN_POINT('',(200.768235730993,37.,80.));
#21248=CARTESIAN_POINT('',(201.384117865497,35.975,80.));
#21249=CARTESIAN_POINT('Origin',(201.384117865497,37.,20.));
#21250=CARTESIAN_POINT('',(200.768235730993,37.,20.));
#21251=CARTESIAN_POINT('',(201.384117865497,35.975,20.));
#21252=CARTESIAN_POINT('Origin',(0.15,30.,96.));
#21253=CARTESIAN_POINT('',(0.3,30.,98.05));
#21254=CARTESIAN_POINT('Origin',(0.3,30.,96.));
#21255=CARTESIAN_POINT('',(0.,30.,98.35));
#21256=CARTESIAN_POINT('',(0.15,30.,98.2));
#21257=CARTESIAN_POINT('Origin',(0.,30.,96.));
#21258=CARTESIAN_POINT('Origin',(0.,29.5,50.));
#21259=CARTESIAN_POINT('',(0.,14.,0.499999999999998));
#21260=CARTESIAN_POINT('',(0.,44.5,0.499999999999998));
#21261=CARTESIAN_POINT('',(0.,21.75,0.499999999999998));
#21262=CARTESIAN_POINT('',(0.,14.,24.2));
#21263=CARTESIAN_POINT('',(0.,14.,24.5));
#21264=CARTESIAN_POINT('',(0.,14.3,24.5));
#21265=CARTESIAN_POINT('',(0.,24.4000000000001,34.5999999999999));
#21266=CARTESIAN_POINT('',(0.,36.5,24.5));
#21267=CARTESIAN_POINT('',(0.,36.5,24.5));
#21268=CARTESIAN_POINT('',(0.,36.5,40.));
#21269=CARTESIAN_POINT('',(0.,36.5,40.));
#21270=CARTESIAN_POINT('',(0.,32.,40.));
#21271=CARTESIAN_POINT('',(0.,32.,40.));
#21272=CARTESIAN_POINT('',(0.,32.,60.));
#21273=CARTESIAN_POINT('',(0.,32.,60.));
#21274=CARTESIAN_POINT('',(0.,36.5,60.));
#21275=CARTESIAN_POINT('',(0.,36.5,60.));
#21276=CARTESIAN_POINT('',(0.,36.5,75.5));
#21277=CARTESIAN_POINT('',(0.,36.5,75.5));
#21278=CARTESIAN_POINT('',(0.,14.3,75.5));
#21279=CARTESIAN_POINT('',(0.,14.,75.5));
#21280=CARTESIAN_POINT('',(0.,14.,75.8));
#21281=CARTESIAN_POINT('',(0.,24.4,65.4));
#21282=CARTESIAN_POINT('',(0.,14.,99.5));
#21283=CARTESIAN_POINT('',(0.,14.,100.));
#21284=CARTESIAN_POINT('',(0.,44.5,99.5));
#21285=CARTESIAN_POINT('',(0.,37.25,99.5));
#21286=CARTESIAN_POINT('',(0.,44.5,25.));
#21287=CARTESIAN_POINT('',(0.,37.,22.35));
#21288=CARTESIAN_POINT('Origin',(0.,37.,20.));
#21289=CARTESIAN_POINT('',(0.,30.,6.35));
#21290=CARTESIAN_POINT('Origin',(0.,30.,4.));
#21291=CARTESIAN_POINT('',(0.,37.,82.35));
#21292=CARTESIAN_POINT('Origin',(0.,37.,80.));
#21293=CARTESIAN_POINT('Origin',(0.,30.,96.));
#21294=CARTESIAN_POINT('',(8.,30.,98.05));
#21295=CARTESIAN_POINT('',(0.,30.,98.05));
#21296=CARTESIAN_POINT('',(7.99999999999999,27.95,96.));
#21297=CARTESIAN_POINT('Origin',(8.,30.,96.));
#21298=CARTESIAN_POINT('Origin',(8.,30.,96.));
#21299=CARTESIAN_POINT('Origin',(0.15,37.,20.));
#21300=CARTESIAN_POINT('',(0.3,37.,22.05));
#21301=CARTESIAN_POINT('Origin',(0.3,37.,20.));
#21302=CARTESIAN_POINT('',(0.15,37.,22.2));
#21303=CARTESIAN_POINT('Origin',(0.,37.,20.));
#21304=CARTESIAN_POINT('',(8.,37.,22.05));
#21305=CARTESIAN_POINT('',(0.,37.,22.05));
#21306=CARTESIAN_POINT('',(8.,34.95,20.));
#21307=CARTESIAN_POINT('Origin',(8.,37.,20.));
#21308=CARTESIAN_POINT('Origin',(8.,37.,20.));
#21309=CARTESIAN_POINT('Origin',(0.15,37.,80.));
#21310=CARTESIAN_POINT('',(0.3,37.,82.05));
#21311=CARTESIAN_POINT('Origin',(0.3,37.,80.));
#21312=CARTESIAN_POINT('',(0.15,37.,82.2));
#21313=CARTESIAN_POINT('Origin',(0.,37.,80.));
#21314=CARTESIAN_POINT('',(8.,37.,82.05));
#21315=CARTESIAN_POINT('',(0.,37.,82.05));
#21316=CARTESIAN_POINT('',(8.,34.95,80.));
#21317=CARTESIAN_POINT('Origin',(8.,37.,80.));
#21318=CARTESIAN_POINT('Origin',(8.,37.,80.));
#21319=CARTESIAN_POINT('Origin',(0.15,30.,4.));
#21320=CARTESIAN_POINT('',(0.3,30.,6.05));
#21321=CARTESIAN_POINT('Origin',(0.3,30.,4.));
#21322=CARTESIAN_POINT('',(0.15,30.,6.2));
#21323=CARTESIAN_POINT('Origin',(0.,30.,4.));
#21324=CARTESIAN_POINT('',(8.,30.,6.05));
#21325=CARTESIAN_POINT('',(0.,30.,6.05));
#21326=CARTESIAN_POINT('',(8.,27.95,4.));
#21327=CARTESIAN_POINT('Origin',(8.,30.,4.));
#21328=CARTESIAN_POINT('Origin',(8.,30.,4.));
#21329=CARTESIAN_POINT('Origin',(8.,30.,96.));
#21330=CARTESIAN_POINT('',(9.2317642690065,30.,96.));
#21331=CARTESIAN_POINT('',(8.,27.95,96.));
#21332=CARTESIAN_POINT('Origin',(8.,30.,4.));
#21333=CARTESIAN_POINT('',(9.2317642690065,30.,4.));
#21334=CARTESIAN_POINT('',(8.,27.95,4.));
#21335=CARTESIAN_POINT('Origin',(8.,37.,80.));
#21336=CARTESIAN_POINT('',(9.2317642690065,37.,80.));
#21337=CARTESIAN_POINT('',(8.,34.95,80.));
#21338=CARTESIAN_POINT('Origin',(8.,37.,20.));
#21339=CARTESIAN_POINT('',(9.2317642690065,37.,20.));
#21340=CARTESIAN_POINT('',(8.,34.95,20.));
#21341=CARTESIAN_POINT('Origin',(155.,44.8,75.));
#21342=CARTESIAN_POINT('',(151.95,44.6,75.));
#21343=CARTESIAN_POINT('Origin',(155.,44.6,75.));
#21344=CARTESIAN_POINT('',(151.55,45.,75.));
#21345=CARTESIAN_POINT('',(151.75,44.8,75.));
#21346=CARTESIAN_POINT('Origin',(155.,45.,75.));
#21347=CARTESIAN_POINT('Origin',(0.,45.,0.));
#21348=CARTESIAN_POINT('',(209.5,45.,0.5));
#21349=CARTESIAN_POINT('',(209.5,45.,99.5));
#21350=CARTESIAN_POINT('',(209.5,45.,25.));
#21351=CARTESIAN_POINT('',(0.5,45.,0.5));
#21352=CARTESIAN_POINT('',(0.,45.,0.5));
#21353=CARTESIAN_POINT('',(0.5,45.,99.5));
#21354=CARTESIAN_POINT('',(0.5,45.,25.));
#21355=CARTESIAN_POINT('',(0.,45.,99.5));
#21356=CARTESIAN_POINT('',(101.55,45.,75.));
#21357=CARTESIAN_POINT('Origin',(105.,45.,75.));
#21358=CARTESIAN_POINT('',(51.55,45.,75.));
#21359=CARTESIAN_POINT('Origin',(55.,45.,75.));
#21360=CARTESIAN_POINT('',(151.55,45.,25.));
#21361=CARTESIAN_POINT('Origin',(155.,45.,25.));
#21362=CARTESIAN_POINT('',(174.2,45.,81.5));
#21363=CARTESIAN_POINT('Origin',(180.,45.,81.5));
#21364=CARTESIAN_POINT('',(24.2,45.,18.5));
#21365=CARTESIAN_POINT('Origin',(30.,45.,18.5));
#21366=CARTESIAN_POINT('',(24.2,45.,81.5));
#21367=CARTESIAN_POINT('Origin',(30.,45.,81.5));
#21368=CARTESIAN_POINT('',(124.2,45.,18.5));
#21369=CARTESIAN_POINT('Origin',(130.,45.,18.5));
#21370=CARTESIAN_POINT('',(174.2,45.,18.5));
#21371=CARTESIAN_POINT('Origin',(180.,45.,18.5));
#21372=CARTESIAN_POINT('',(74.2,45.,81.5));
#21373=CARTESIAN_POINT('Origin',(80.,45.,81.5));
#21374=CARTESIAN_POINT('',(74.2,45.,18.5));
#21375=CARTESIAN_POINT('Origin',(80.,45.,18.5));
#21376=CARTESIAN_POINT('',(124.2,45.,81.5));
#21377=CARTESIAN_POINT('Origin',(130.,45.,81.5));
#21378=CARTESIAN_POINT('',(51.55,45.,25.));
#21379=CARTESIAN_POINT('Origin',(55.,45.,25.));
#21380=CARTESIAN_POINT('',(101.55,45.,25.));
#21381=CARTESIAN_POINT('Origin',(105.,45.,25.));
#21382=CARTESIAN_POINT('Origin',(155.,45.,75.));
#21383=CARTESIAN_POINT('',(151.95,38.5,75.));
#21384=CARTESIAN_POINT('',(151.95,45.,75.));
#21385=CARTESIAN_POINT('Origin',(155.,38.5,75.));
#21386=CARTESIAN_POINT('Origin',(105.,44.8,75.));
#21387=CARTESIAN_POINT('',(101.95,44.6,75.));
#21388=CARTESIAN_POINT('Origin',(105.,44.6,75.));
#21389=CARTESIAN_POINT('',(101.75,44.8,75.));
#21390=CARTESIAN_POINT('Origin',(105.,45.,75.));
#21391=CARTESIAN_POINT('',(101.95,38.5,75.));
#21392=CARTESIAN_POINT('',(101.95,45.,75.));
#21393=CARTESIAN_POINT('Origin',(105.,38.5,75.));
#21394=CARTESIAN_POINT('Origin',(105.,44.8,25.));
#21395=CARTESIAN_POINT('',(101.95,44.6,25.));
#21396=CARTESIAN_POINT('Origin',(105.,44.6,25.));
#21397=CARTESIAN_POINT('',(101.75,44.8,25.));
#21398=CARTESIAN_POINT('Origin',(105.,45.,25.));
#21399=CARTESIAN_POINT('',(101.95,38.5,25.));
#21400=CARTESIAN_POINT('',(101.95,45.,25.));
#21401=CARTESIAN_POINT('Origin',(105.,38.5,25.));
#21402=CARTESIAN_POINT('Origin',(55.,44.8,75.));
#21403=CARTESIAN_POINT('',(51.95,44.6,75.));
#21404=CARTESIAN_POINT('Origin',(55.,44.6,75.));
#21405=CARTESIAN_POINT('',(51.75,44.8,75.));
#21406=CARTESIAN_POINT('Origin',(55.,45.,75.));
#21407=CARTESIAN_POINT('',(51.95,38.5,75.));
#21408=CARTESIAN_POINT('',(51.95,45.,75.));
#21409=CARTESIAN_POINT('Origin',(55.,38.5,75.));
#21410=CARTESIAN_POINT('Origin',(55.,44.8,25.));
#21411=CARTESIAN_POINT('',(51.95,44.6,25.));
#21412=CARTESIAN_POINT('Origin',(55.,44.6,25.));
#21413=CARTESIAN_POINT('',(51.75,44.8,25.));
#21414=CARTESIAN_POINT('Origin',(55.,45.,25.));
#21415=CARTESIAN_POINT('',(51.95,38.5,25.));
#21416=CARTESIAN_POINT('',(51.95,45.,25.));
#21417=CARTESIAN_POINT('Origin',(55.,38.5,25.));
#21418=CARTESIAN_POINT('Origin',(155.,44.8,25.));
#21419=CARTESIAN_POINT('',(151.95,44.6,25.));
#21420=CARTESIAN_POINT('Origin',(155.,44.6,25.));
#21421=CARTESIAN_POINT('',(151.75,44.8,25.));
#21422=CARTESIAN_POINT('Origin',(155.,45.,25.));
#21423=CARTESIAN_POINT('',(151.95,38.5,25.));
#21424=CARTESIAN_POINT('',(151.95,45.,25.));
#21425=CARTESIAN_POINT('Origin',(155.,38.5,25.));
#21426=CARTESIAN_POINT('Origin',(155.,38.5,75.));
#21427=CARTESIAN_POINT('',(155.,36.6673751119659,75.));
#21428=CARTESIAN_POINT('',(151.95,38.5,75.));
#21429=CARTESIAN_POINT('Origin',(155.,38.5,25.));
#21430=CARTESIAN_POINT('',(155.,36.6673751119659,25.));
#21431=CARTESIAN_POINT('',(151.95,38.5,25.));
#21432=CARTESIAN_POINT('Origin',(105.,38.5,75.));
#21433=CARTESIAN_POINT('',(105.,36.6673751119659,75.));
#21434=CARTESIAN_POINT('',(101.95,38.5,75.));
#21435=CARTESIAN_POINT('Origin',(105.,38.5,25.));
#21436=CARTESIAN_POINT('',(105.,36.6673751119659,25.));
#21437=CARTESIAN_POINT('',(101.95,38.5,25.));
#21438=CARTESIAN_POINT('Origin',(55.,38.5,75.));
#21439=CARTESIAN_POINT('',(55.,36.6673751119659,75.));
#21440=CARTESIAN_POINT('',(51.95,38.5,75.));
#21441=CARTESIAN_POINT('Origin',(55.,38.5,25.));
#21442=CARTESIAN_POINT('',(55.,36.6673751119659,25.));
#21443=CARTESIAN_POINT('',(51.95,38.5,25.));
#21444=CARTESIAN_POINT('Origin',(180.,44.85,81.5));
#21445=CARTESIAN_POINT('',(174.5,44.7,81.5));
#21446=CARTESIAN_POINT('Origin',(180.,44.7,81.5));
#21447=CARTESIAN_POINT('',(174.35,44.85,81.5));
#21448=CARTESIAN_POINT('Origin',(180.,45.,81.5));
#21449=CARTESIAN_POINT('',(174.5,38.,81.5));
#21450=CARTESIAN_POINT('',(174.5,45.,81.5));
#21451=CARTESIAN_POINT('Origin',(180.,38.,81.5));
#21452=CARTESIAN_POINT('Origin',(130.,44.85,81.5));
#21453=CARTESIAN_POINT('',(124.5,44.7,81.5));
#21454=CARTESIAN_POINT('Origin',(130.,44.7,81.5));
#21455=CARTESIAN_POINT('',(124.35,44.85,81.5));
#21456=CARTESIAN_POINT('Origin',(130.,45.,81.5));
#21457=CARTESIAN_POINT('',(124.5,38.,81.5));
#21458=CARTESIAN_POINT('',(124.5,45.,81.5));
#21459=CARTESIAN_POINT('Origin',(130.,38.,81.5));
#21460=CARTESIAN_POINT('Origin',(30.,44.85,18.5));
#21461=CARTESIAN_POINT('',(24.5,44.7,18.5));
#21462=CARTESIAN_POINT('Origin',(30.,44.7,18.5));
#21463=CARTESIAN_POINT('',(24.35,44.85,18.5));
#21464=CARTESIAN_POINT('Origin',(30.,45.,18.5));
#21465=CARTESIAN_POINT('',(24.5,38.,18.5));
#21466=CARTESIAN_POINT('',(24.5,45.,18.5));
#21467=CARTESIAN_POINT('Origin',(30.,38.,18.5));
#21468=CARTESIAN_POINT('Origin',(80.,44.85,18.5));
#21469=CARTESIAN_POINT('',(74.5,44.7,18.5));
#21470=CARTESIAN_POINT('Origin',(80.,44.7,18.5));
#21471=CARTESIAN_POINT('',(74.35,44.85,18.5));
#21472=CARTESIAN_POINT('Origin',(80.,45.,18.5));
#21473=CARTESIAN_POINT('',(74.5,38.,18.5));
#21474=CARTESIAN_POINT('',(74.5,45.,18.5));
#21475=CARTESIAN_POINT('Origin',(80.,38.,18.5));
#21476=CARTESIAN_POINT('Origin',(30.,44.85,81.5));
#21477=CARTESIAN_POINT('',(24.5,44.7,81.5));
#21478=CARTESIAN_POINT('Origin',(30.,44.7,81.5));
#21479=CARTESIAN_POINT('',(24.35,44.85,81.5));
#21480=CARTESIAN_POINT('Origin',(30.,45.,81.5));
#21481=CARTESIAN_POINT('',(24.5,38.,81.5));
#21482=CARTESIAN_POINT('',(24.5,45.,81.5));
#21483=CARTESIAN_POINT('Origin',(30.,38.,81.5));
#21484=CARTESIAN_POINT('Origin',(80.,44.85,81.5));
#21485=CARTESIAN_POINT('',(74.5,44.7,81.5));
#21486=CARTESIAN_POINT('Origin',(80.,44.7,81.5));
#21487=CARTESIAN_POINT('',(74.35,44.85,81.5));
#21488=CARTESIAN_POINT('Origin',(80.,45.,81.5));
#21489=CARTESIAN_POINT('',(74.5,38.,81.5));
#21490=CARTESIAN_POINT('',(74.5,45.,81.5));
#21491=CARTESIAN_POINT('Origin',(80.,38.,81.5));
#21492=CARTESIAN_POINT('Origin',(130.,44.85,18.5));
#21493=CARTESIAN_POINT('',(124.5,44.7,18.5));
#21494=CARTESIAN_POINT('Origin',(130.,44.7,18.5));
#21495=CARTESIAN_POINT('',(124.35,44.85,18.5));
#21496=CARTESIAN_POINT('Origin',(130.,45.,18.5));
#21497=CARTESIAN_POINT('',(124.5,38.,18.5));
#21498=CARTESIAN_POINT('',(124.5,45.,18.5));
#21499=CARTESIAN_POINT('Origin',(130.,38.,18.5));
#21500=CARTESIAN_POINT('Origin',(180.,44.85,18.5));
#21501=CARTESIAN_POINT('',(174.5,44.7,18.5));
#21502=CARTESIAN_POINT('Origin',(180.,44.7,18.5));
#21503=CARTESIAN_POINT('',(174.35,44.85,18.5));
#21504=CARTESIAN_POINT('Origin',(180.,45.,18.5));
#21505=CARTESIAN_POINT('',(174.5,38.,18.5));
#21506=CARTESIAN_POINT('',(174.5,45.,18.5));
#21507=CARTESIAN_POINT('Origin',(180.,38.,18.5));
#21508=CARTESIAN_POINT('Origin',(180.,38.,18.5));
#21509=CARTESIAN_POINT('',(176.5,38.,18.5));
#21510=CARTESIAN_POINT('Origin',(180.,38.,18.5));
#21511=CARTESIAN_POINT('Origin',(130.,38.,18.5));
#21512=CARTESIAN_POINT('',(126.5,38.,18.5));
#21513=CARTESIAN_POINT('Origin',(130.,38.,18.5));
#21514=CARTESIAN_POINT('Origin',(80.,38.,81.5));
#21515=CARTESIAN_POINT('',(76.5,38.,81.5));
#21516=CARTESIAN_POINT('Origin',(80.,38.,81.5));
#21517=CARTESIAN_POINT('Origin',(30.,38.,81.5));
#21518=CARTESIAN_POINT('',(26.5,38.,81.5));
#21519=CARTESIAN_POINT('Origin',(30.,38.,81.5));
#21520=CARTESIAN_POINT('Origin',(80.,38.,18.5));
#21521=CARTESIAN_POINT('',(76.5,38.,18.5));
#21522=CARTESIAN_POINT('Origin',(80.,38.,18.5));
#21523=CARTESIAN_POINT('Origin',(30.,38.,18.5));
#21524=CARTESIAN_POINT('',(26.5,38.,18.5));
#21525=CARTESIAN_POINT('Origin',(30.,38.,18.5));
#21526=CARTESIAN_POINT('Origin',(130.,38.,81.5));
#21527=CARTESIAN_POINT('',(126.5,38.,81.5));
#21528=CARTESIAN_POINT('Origin',(130.,38.,81.5));
#21529=CARTESIAN_POINT('Origin',(180.,38.,81.5));
#21530=CARTESIAN_POINT('',(176.5,38.,81.5));
#21531=CARTESIAN_POINT('Origin',(180.,38.,81.5));
#21532=CARTESIAN_POINT('Origin',(180.,45.,18.5));
#21533=CARTESIAN_POINT('',(176.5,14.,18.5));
#21534=CARTESIAN_POINT('',(176.5,45.,18.5));
#21535=CARTESIAN_POINT('Origin',(180.,14.,18.5));
#21536=CARTESIAN_POINT('Origin',(130.,45.,18.5));
#21537=CARTESIAN_POINT('',(126.5,14.,18.5));
#21538=CARTESIAN_POINT('',(126.5,45.,18.5));
#21539=CARTESIAN_POINT('Origin',(130.,14.,18.5));
#21540=CARTESIAN_POINT('Origin',(80.,45.,81.5));
#21541=CARTESIAN_POINT('',(76.5,14.,81.5));
#21542=CARTESIAN_POINT('',(76.5,45.,81.5));
#21543=CARTESIAN_POINT('Origin',(80.,14.,81.5));
#21544=CARTESIAN_POINT('Origin',(30.,45.,81.5));
#21545=CARTESIAN_POINT('',(26.5,14.,81.5));
#21546=CARTESIAN_POINT('',(26.5,45.,81.5));
#21547=CARTESIAN_POINT('Origin',(30.,14.,81.5));
#21548=CARTESIAN_POINT('Origin',(80.,45.,18.5));
#21549=CARTESIAN_POINT('',(76.5,14.,18.5));
#21550=CARTESIAN_POINT('',(76.5,45.,18.5));
#21551=CARTESIAN_POINT('Origin',(80.,14.,18.5));
#21552=CARTESIAN_POINT('Origin',(30.,45.,18.5));
#21553=CARTESIAN_POINT('',(26.5,14.,18.5));
#21554=CARTESIAN_POINT('',(26.5,45.,18.5));
#21555=CARTESIAN_POINT('Origin',(30.,14.,18.5));
#21556=CARTESIAN_POINT('Origin',(130.,45.,81.5));
#21557=CARTESIAN_POINT('',(126.5,14.,81.5));
#21558=CARTESIAN_POINT('',(126.5,45.,81.5));
#21559=CARTESIAN_POINT('Origin',(130.,14.,81.5));
#21560=CARTESIAN_POINT('Origin',(180.,45.,81.5));
#21561=CARTESIAN_POINT('',(176.5,14.,81.5));
#21562=CARTESIAN_POINT('',(176.5,45.,81.5));
#21563=CARTESIAN_POINT('Origin',(180.,14.,81.5));
#21564=CARTESIAN_POINT('Origin',(209.75,37.25,99.75));
#21565=CARTESIAN_POINT('',(170.958333333333,53.0416666666664,138.541666666667));
#21566=CARTESIAN_POINT('',(209.75,44.75,99.75));
#21567=CARTESIAN_POINT('',(223.458333333333,31.0416666666668,86.0416666666665));
#21568=CARTESIAN_POINT('',(173.541666666667,8.54166666666666,135.958333333333));
#21569=CARTESIAN_POINT('Origin',(209.75,44.75,25.));
#21570=CARTESIAN_POINT('',(209.75,44.75,0.250000000000017));
#21571=CARTESIAN_POINT('',(217.708333333333,36.7916666666668,8.20833333333323));
#21572=CARTESIAN_POINT('',(170.666666666666,83.8333333333334,39.3333333333336));
#21573=CARTESIAN_POINT('',(162.333333333332,92.1666666666667,52.3333333333333));
#21574=CARTESIAN_POINT('Origin',(0.,14.25,99.75));
#21575=CARTESIAN_POINT('',(4.04166666666663,18.0416666666666,103.541666666667));
#21576=CARTESIAN_POINT('',(0.,14.,99.5));
#21577=CARTESIAN_POINT('Origin',(0.,44.75,0.25));
#21578=CARTESIAN_POINT('',(170.958333333332,5.95833333333323,-38.5416666666669));
#21579=CARTESIAN_POINT('',(0.249999999999999,44.75,0.250000000000001));
#21580=CARTESIAN_POINT('',(4.04166666666667,40.9583333333334,-3.54166666666665));
#21581=CARTESIAN_POINT('',(4.33333333333334,48.8333333333333,4.33333333333334));
#21582=CARTESIAN_POINT('Origin',(209.75,21.75,0.249999999999999));
#21583=CARTESIAN_POINT('',(173.541666666666,50.4583333333335,-35.9583333333336));
#21584=CARTESIAN_POINT('Origin',(0.25,21.75,0.249999999999999));
#21585=CARTESIAN_POINT('',(1.45833333333333,15.4583333333333,-0.958333333333329));
#21586=CARTESIAN_POINT('',(-7.70833333333334,36.7916666666667,8.20833333333331));
#21587=CARTESIAN_POINT('Origin',(0.25,44.75,25.));
#21588=CARTESIAN_POINT('',(0.25,44.75,99.75));
#21589=CARTESIAN_POINT('',(-13.4583333333334,31.0416666666666,86.0416666666664));
#21590=CARTESIAN_POINT('',(12.6666666666667,57.1666666666666,87.3333333333334));
#21591=CARTESIAN_POINT('Origin',(0.,44.75,99.75));
#21592=CARTESIAN_POINT('',(1.45833333333333,43.5416666666667,100.958333333333));
#21593=CARTESIAN_POINT('Origin',(0.25,37.25,99.75));
#21594=CARTESIAN_POINT('Origin',(0.,14.15,24.35));
#21595=CARTESIAN_POINT('',(0.,14.3,24.5));
#21596=CARTESIAN_POINT('',(0.,14.,24.2));
#21597=CARTESIAN_POINT('Origin',(0.,14.,24.5));
#21598=CARTESIAN_POINT('',(0.,14.,0.5));
#21599=CARTESIAN_POINT('Origin',(0.,14.15,75.65));
#21600=CARTESIAN_POINT('',(0.,14.,75.8));
#21601=CARTESIAN_POINT('',(0.,14.3,75.5));
#21602=CARTESIAN_POINT('Origin',(0.,14.,75.5));
#21603=CARTESIAN_POINT('',(0.,36.5,75.5));
#21604=CARTESIAN_POINT('Origin',(0.,14.25,0.25));
#21605=CARTESIAN_POINT('Origin',(0.,14.,100.));
#21606=CARTESIAN_POINT('Origin',(0.,36.5,24.5));
#21607=CARTESIAN_POINT('',(0.,36.5,24.5));
#21608=CARTESIAN_POINT('Origin',(0.,36.5,40.));
#21609=CARTESIAN_POINT('',(0.,36.5,40.));
#21610=CARTESIAN_POINT('Origin',(0.,32.,40.));
#21611=CARTESIAN_POINT('',(0.,32.,40.));
#21612=CARTESIAN_POINT('Origin',(0.,32.,60.));
#21613=CARTESIAN_POINT('',(0.,32.,60.));
#21614=CARTESIAN_POINT('Origin',(0.,36.5,60.));
#21615=CARTESIAN_POINT('',(0.,36.5,60.));
#21616=CARTESIAN_POINT('Origin',(0.,36.5,75.5));
#21617=CARTESIAN_POINT('',(0.,0.,0.));
#21618=CARTESIAN_POINT('Origin',(204.9,11.,29.5));
#21619=CARTESIAN_POINT('',(204.8,11.,31.05));
#21620=CARTESIAN_POINT('Origin',(204.8,11.,29.5));
#21621=CARTESIAN_POINT('',(205.,11.,31.25));
#21622=CARTESIAN_POINT('',(204.9,11.,31.15));
#21623=CARTESIAN_POINT('Origin',(205.,11.,29.5));
#21624=CARTESIAN_POINT('Origin',(205.,21.,27.875));
#21625=CARTESIAN_POINT('',(205.,6.3,24.7));
#21626=CARTESIAN_POINT('',(205.,6.3,31.05));
#21627=CARTESIAN_POINT('',(205.,6.3,29.5625));
#21628=CARTESIAN_POINT('',(205.,6.5,24.5));
#21629=CARTESIAN_POINT('',(205.,9.15625000000002,21.84375));
#21630=CARTESIAN_POINT('',(205.,35.5,24.5));
#21631=CARTESIAN_POINT('',(205.,36.,24.5));
#21632=CARTESIAN_POINT('',(205.,35.7,24.7));
#21633=CARTESIAN_POINT('',(205.,32.84375,21.84375));
#21634=CARTESIAN_POINT('',(205.,35.7,31.05));
#21635=CARTESIAN_POINT('',(205.,35.7,26.1875));
#21636=CARTESIAN_POINT('',(205.,35.5,31.25));
#21637=CARTESIAN_POINT('',(205.,32.84375,33.90625));
#21638=CARTESIAN_POINT('',(205.,24.696,31.25));
#21639=CARTESIAN_POINT('',(205.,24.496,31.25));
#21640=CARTESIAN_POINT('',(205.,24.3545786437627,31.1085786437627));
#21641=CARTESIAN_POINT('',(205.,22.4366566484982,30.3141493417505));
#21642=CARTESIAN_POINT('',(205.,21.6,28.354));
#21643=CARTESIAN_POINT('',(205.,21.6,28.354));
#21644=CARTESIAN_POINT('',(205.,21.6,27.154));
#21645=CARTESIAN_POINT('',(205.,21.6,27.154));
#21646=CARTESIAN_POINT('',(205.,20.4,27.154));
#21647=CARTESIAN_POINT('',(205.,20.4,27.154));
#21648=CARTESIAN_POINT('',(205.,20.4,28.354));
#21649=CARTESIAN_POINT('',(205.,20.4,28.354));
#21650=CARTESIAN_POINT('',(205.,17.6454213562373,31.1085786437627));
#21651=CARTESIAN_POINT('',(205.,17.504,31.25));
#21652=CARTESIAN_POINT('',(205.,17.304,31.25));
#21653=CARTESIAN_POINT('',(205.,19.5633433515018,30.3141493417505));
#21654=CARTESIAN_POINT('',(205.,6.,31.25));
#21655=CARTESIAN_POINT('',(205.,6.5,31.25));
#21656=CARTESIAN_POINT('',(205.,6.,31.25));
#21657=CARTESIAN_POINT('',(205.,9.15625000000002,33.90625));
#21658=CARTESIAN_POINT('Origin',(205.,11.,29.5));
#21659=CARTESIAN_POINT('',(198.,11.,31.05));
#21660=CARTESIAN_POINT('',(205.,11.,31.05));
#21661=CARTESIAN_POINT('',(198.,9.45,29.5));
#21662=CARTESIAN_POINT('Origin',(198.,11.,29.5));
#21663=CARTESIAN_POINT('Origin',(198.,11.,29.5));
#21664=CARTESIAN_POINT('Origin',(197.534333020254,11.,29.5));
#21665=CARTESIAN_POINT('',(197.068666040507,11.,29.5));
#21666=CARTESIAN_POINT('',(197.534333020254,10.225,29.5));
#21667=CARTESIAN_POINT('Origin',(5.1,11.,29.5));
#21668=CARTESIAN_POINT('',(5.2,11.,31.05));
#21669=CARTESIAN_POINT('Origin',(5.2,11.,29.5));
#21670=CARTESIAN_POINT('',(5.,11.,31.25));
#21671=CARTESIAN_POINT('',(5.1,11.,31.15));
#21672=CARTESIAN_POINT('Origin',(5.,11.,29.5));
#21673=CARTESIAN_POINT('Origin',(5.,21.,27.875));
#21674=CARTESIAN_POINT('',(5.,6.3,31.05));
#21675=CARTESIAN_POINT('',(5.,6.3,24.7));
#21676=CARTESIAN_POINT('',(5.,6.3,29.5625));
#21677=CARTESIAN_POINT('',(5.,6.5,31.25));
#21678=CARTESIAN_POINT('',(5.,9.15625000000002,33.90625));
#21679=CARTESIAN_POINT('',(5.,6.,31.25));
#21680=CARTESIAN_POINT('',(5.,17.304,31.25));
#21681=CARTESIAN_POINT('',(5.,6.,31.25));
#21682=CARTESIAN_POINT('',(5.,17.6454213562373,31.1085786437627));
#21683=CARTESIAN_POINT('',(5.,19.5633433515018,30.3141493417505));
#21684=CARTESIAN_POINT('',(5.,20.4,28.354));
#21685=CARTESIAN_POINT('',(5.,17.504,31.25));
#21686=CARTESIAN_POINT('',(5.,20.4,27.154));
#21687=CARTESIAN_POINT('',(5.,20.4,28.354));
#21688=CARTESIAN_POINT('',(5.,21.6,27.154));
#21689=CARTESIAN_POINT('',(5.,20.4,27.154));
#21690=CARTESIAN_POINT('',(5.,21.6,28.354));
#21691=CARTESIAN_POINT('',(5.,21.6,27.154));
#21692=CARTESIAN_POINT('',(5.,24.3545786437627,31.1085786437627));
#21693=CARTESIAN_POINT('',(5.,21.6,28.354));
#21694=CARTESIAN_POINT('',(5.,24.696,31.25));
#21695=CARTESIAN_POINT('',(5.,22.4366566484982,30.3141493417505));
#21696=CARTESIAN_POINT('',(5.,35.5,31.25));
#21697=CARTESIAN_POINT('',(5.,24.496,31.25));
#21698=CARTESIAN_POINT('',(5.,35.7,31.05));
#21699=CARTESIAN_POINT('',(5.,32.84375,33.90625));
#21700=CARTESIAN_POINT('',(5.,35.7,24.7));
#21701=CARTESIAN_POINT('',(5.,35.7,26.1875));
#21702=CARTESIAN_POINT('',(5.,35.5,24.5));
#21703=CARTESIAN_POINT('',(5.,32.84375,21.84375));
#21704=CARTESIAN_POINT('',(5.,6.5,24.5));
#21705=CARTESIAN_POINT('',(5.,36.,24.5));
#21706=CARTESIAN_POINT('',(5.,9.15625000000002,21.84375));
#21707=CARTESIAN_POINT('Origin',(5.,11.,29.5));
#21708=CARTESIAN_POINT('',(12.,11.,31.05));
#21709=CARTESIAN_POINT('',(5.,11.,31.05));
#21710=CARTESIAN_POINT('',(12.,9.45,29.5));
#21711=CARTESIAN_POINT('Origin',(12.,11.,29.5));
#21712=CARTESIAN_POINT('Origin',(12.,11.,29.5));
#21713=CARTESIAN_POINT('Origin',(12.,11.,29.5));
#21714=CARTESIAN_POINT('',(12.9313339594927,11.,29.5));
#21715=CARTESIAN_POINT('',(12.,9.45,29.5));
#21716=CARTESIAN_POINT('Origin',(155.,21.,24.65));
#21717=CARTESIAN_POINT('',(152.45,21.,24.8));
#21718=CARTESIAN_POINT('Origin',(155.,21.,24.8));
#21719=CARTESIAN_POINT('',(152.15,21.,24.5));
#21720=CARTESIAN_POINT('',(152.3,21.,24.65));
#21721=CARTESIAN_POINT('Origin',(155.,21.,24.5));
#21722=CARTESIAN_POINT('Origin',(5.,6.,24.5));
#21723=CARTESIAN_POINT('',(5.,6.5,24.5));
#21724=CARTESIAN_POINT('',(5.,35.5,24.5));
#21725=CARTESIAN_POINT('',(102.15,21.,24.5));
#21726=CARTESIAN_POINT('Origin',(105.,21.,24.5));
#21727=CARTESIAN_POINT('',(52.15,21.,24.5));
#21728=CARTESIAN_POINT('Origin',(55.,21.,24.5));
#21729=CARTESIAN_POINT('Origin',(155.,21.,24.5));
#21730=CARTESIAN_POINT('',(152.45,21.,27.154));
#21731=CARTESIAN_POINT('',(152.45,21.,24.5));
#21732=CARTESIAN_POINT('',(152.521593253721,20.4,27.154));
#21733=CARTESIAN_POINT('Origin',(155.,21.,27.154));
#21734=CARTESIAN_POINT('',(152.521593253721,20.4,28.354));
#21735=CARTESIAN_POINT('',(152.521593253721,20.4,24.5));
#21736=CARTESIAN_POINT('',(152.545690321088,20.308,28.446));
#21737=CARTESIAN_POINT('Origin',(155.,21.,27.754));
#21738=CARTESIAN_POINT('',(157.454309678912,20.308,28.446));
#21739=CARTESIAN_POINT('Origin',(155.,21.,28.446));
#21740=CARTESIAN_POINT('',(157.478406746279,20.4,28.354));
#21741=CARTESIAN_POINT('Origin',(155.,21.,27.754));
#21742=CARTESIAN_POINT('',(157.478406746279,20.4,27.154));
#21743=CARTESIAN_POINT('',(157.478406746279,20.4,24.5));
#21744=CARTESIAN_POINT('',(157.478406746279,21.6,27.154));
#21745=CARTESIAN_POINT('Origin',(155.,21.,27.154));
#21746=CARTESIAN_POINT('',(157.478406746279,21.6,28.354));
#21747=CARTESIAN_POINT('',(157.478406746279,21.6,24.5));
#21748=CARTESIAN_POINT('',(157.454309678912,21.692,28.446));
#21749=CARTESIAN_POINT('Origin',(155.,21.,27.754));
#21750=CARTESIAN_POINT('',(152.545690321088,21.692,28.446));
#21751=CARTESIAN_POINT('Origin',(155.,21.,28.446));
#21752=CARTESIAN_POINT('',(152.521593253721,21.6,28.354));
#21753=CARTESIAN_POINT('Origin',(155.,21.,27.754));
#21754=CARTESIAN_POINT('',(152.521593253721,21.6,27.154));
#21755=CARTESIAN_POINT('',(152.521593253721,21.6,24.5));
#21756=CARTESIAN_POINT('Origin',(155.,21.,27.154));
#21757=CARTESIAN_POINT('Origin',(105.,21.,24.65));
#21758=CARTESIAN_POINT('',(102.45,21.,24.8));
#21759=CARTESIAN_POINT('Origin',(105.,21.,24.8));
#21760=CARTESIAN_POINT('',(102.3,21.,24.65));
#21761=CARTESIAN_POINT('Origin',(105.,21.,24.5));
#21762=CARTESIAN_POINT('',(102.45,21.,27.154));
#21763=CARTESIAN_POINT('',(102.45,21.,24.5));
#21764=CARTESIAN_POINT('',(102.521593253721,20.4,27.154));
#21765=CARTESIAN_POINT('Origin',(105.,21.,27.154));
#21766=CARTESIAN_POINT('',(102.521593253721,20.4,28.354));
#21767=CARTESIAN_POINT('',(102.521593253721,20.4,24.5));
#21768=CARTESIAN_POINT('',(102.545690321088,20.308,28.446));
#21769=CARTESIAN_POINT('Origin',(105.,21.,27.754));
#21770=CARTESIAN_POINT('',(107.454309678912,20.308,28.446));
#21771=CARTESIAN_POINT('Origin',(105.,21.,28.446));
#21772=CARTESIAN_POINT('',(107.478406746279,20.4,28.354));
#21773=CARTESIAN_POINT('Origin',(105.,21.,27.754));
#21774=CARTESIAN_POINT('',(107.478406746279,20.4,27.154));
#21775=CARTESIAN_POINT('',(107.478406746279,20.4,24.5));
#21776=CARTESIAN_POINT('',(107.478406746279,21.6,27.154));
#21777=CARTESIAN_POINT('Origin',(105.,21.,27.154));
#21778=CARTESIAN_POINT('',(107.478406746279,21.6,28.354));
#21779=CARTESIAN_POINT('',(107.478406746279,21.6,24.5));
#21780=CARTESIAN_POINT('',(107.454309678912,21.692,28.446));
#21781=CARTESIAN_POINT('Origin',(105.,21.,27.754));
#21782=CARTESIAN_POINT('',(102.545690321088,21.692,28.446));
#21783=CARTESIAN_POINT('Origin',(105.,21.,28.446));
#21784=CARTESIAN_POINT('',(102.521593253721,21.6,28.354));
#21785=CARTESIAN_POINT('Origin',(105.,21.,27.754));
#21786=CARTESIAN_POINT('',(102.521593253721,21.6,27.154));
#21787=CARTESIAN_POINT('',(102.521593253721,21.6,24.5));
#21788=CARTESIAN_POINT('Origin',(105.,21.,27.154));
#21789=CARTESIAN_POINT('Origin',(55.,21.,24.65));
#21790=CARTESIAN_POINT('',(52.45,21.,24.8));
#21791=CARTESIAN_POINT('Origin',(55.,21.,24.8));
#21792=CARTESIAN_POINT('',(52.3,21.,24.65));
#21793=CARTESIAN_POINT('Origin',(55.,21.,24.5));
#21794=CARTESIAN_POINT('',(52.45,21.,27.154));
#21795=CARTESIAN_POINT('',(52.45,21.,24.5));
#21796=CARTESIAN_POINT('',(52.5215932537213,20.4,27.154));
#21797=CARTESIAN_POINT('Origin',(55.,21.,27.154));
#21798=CARTESIAN_POINT('',(52.5215932537213,20.4,28.354));
#21799=CARTESIAN_POINT('',(52.5215932537213,20.4,24.5));
#21800=CARTESIAN_POINT('',(52.5456903210882,20.308,28.446));
#21801=CARTESIAN_POINT('Origin',(55.,21.,27.754));
#21802=CARTESIAN_POINT('',(57.4543096789118,20.308,28.446));
#21803=CARTESIAN_POINT('Origin',(55.,21.,28.446));
#21804=CARTESIAN_POINT('',(57.4784067462787,20.4,28.354));
#21805=CARTESIAN_POINT('Origin',(55.,21.,27.754));
#21806=CARTESIAN_POINT('',(57.4784067462787,20.4,27.154));
#21807=CARTESIAN_POINT('',(57.4784067462787,20.4,24.5));
#21808=CARTESIAN_POINT('',(57.4784067462787,21.6,27.154));
#21809=CARTESIAN_POINT('Origin',(55.,21.,27.154));
#21810=CARTESIAN_POINT('',(57.4784067462787,21.6,28.354));
#21811=CARTESIAN_POINT('',(57.4784067462787,21.6,24.5));
#21812=CARTESIAN_POINT('',(57.4543096789118,21.692,28.446));
#21813=CARTESIAN_POINT('Origin',(55.,21.,27.754));
#21814=CARTESIAN_POINT('',(52.5456903210882,21.692,28.446));
#21815=CARTESIAN_POINT('Origin',(55.,21.,28.446));
#21816=CARTESIAN_POINT('',(52.5215932537213,21.6,28.354));
#21817=CARTESIAN_POINT('Origin',(55.,21.,27.754));
#21818=CARTESIAN_POINT('',(52.5215932537213,21.6,27.154));
#21819=CARTESIAN_POINT('',(52.5215932537213,21.6,24.5));
#21820=CARTESIAN_POINT('Origin',(55.,21.,27.154));
#21821=CARTESIAN_POINT('Origin',(55.,21.,28.446));
#21822=CARTESIAN_POINT('',(30.,20.308,28.446));
#21823=CARTESIAN_POINT('Origin',(55.,21.,28.446));
#21824=CARTESIAN_POINT('',(30.,21.692,28.446));
#21825=CARTESIAN_POINT('Origin',(105.,21.,28.446));
#21826=CARTESIAN_POINT('',(55.,20.308,28.446));
#21827=CARTESIAN_POINT('Origin',(105.,21.,28.446));
#21828=CARTESIAN_POINT('',(55.,21.692,28.446));
#21829=CARTESIAN_POINT('Origin',(155.,21.,28.446));
#21830=CARTESIAN_POINT('',(80.,20.308,28.446));
#21831=CARTESIAN_POINT('Origin',(155.,21.,28.446));
#21832=CARTESIAN_POINT('',(80.,21.692,28.446));
#21833=CARTESIAN_POINT('Origin',(5.,24.496,31.25));
#21834=CARTESIAN_POINT('',(5.,21.6,28.354));
#21835=CARTESIAN_POINT('',(5.,21.6,28.354));
#21836=CARTESIAN_POINT('',(5.,21.6,28.354));
#21837=CARTESIAN_POINT('',(5.,24.3545786437627,31.1085786437627));
#21838=CARTESIAN_POINT('',(5.,21.6,28.354));
#21839=CARTESIAN_POINT('Origin',(5.,21.6,28.354));
#21840=CARTESIAN_POINT('',(5.,21.6,27.154));
#21841=CARTESIAN_POINT('Origin',(5.,21.6,28.354));
#21842=CARTESIAN_POINT('',(5.,21.6,27.154));
#21843=CARTESIAN_POINT('Origin',(5.,21.6,28.354));
#21844=CARTESIAN_POINT('',(5.,21.6,27.154));
#21845=CARTESIAN_POINT('Origin',(5.,21.6,27.154));
#21846=CARTESIAN_POINT('',(5.,20.4,27.154));
#21847=CARTESIAN_POINT('Origin',(5.,21.6,27.154));
#21848=CARTESIAN_POINT('',(5.,20.4,27.154));
#21849=CARTESIAN_POINT('Origin',(5.,21.6,27.154));
#21850=CARTESIAN_POINT('',(5.,20.4,27.154));
#21851=CARTESIAN_POINT('Origin',(5.,20.4,27.154));
#21852=CARTESIAN_POINT('',(5.,20.4,28.354));
#21853=CARTESIAN_POINT('Origin',(5.,20.4,27.154));
#21854=CARTESIAN_POINT('',(5.,20.4,28.354));
#21855=CARTESIAN_POINT('Origin',(5.,20.4,27.154));
#21856=CARTESIAN_POINT('',(5.,20.4,28.354));
#21857=CARTESIAN_POINT('Origin',(204.85,6.15,29.5625));
#21858=CARTESIAN_POINT('',(204.7,6.,25.));
#21859=CARTESIAN_POINT('',(170.789583333332,-27.9104166666672,58.910416666667));
#21860=CARTESIAN_POINT('',(204.7,6.,30.75));
#21861=CARTESIAN_POINT('',(171.352083333332,-27.3479166666672,-2.59791666666702));
#21862=CARTESIAN_POINT('',(204.7,6.,29.5625));
#21863=CARTESIAN_POINT('Origin',(5.,6.,31.25));
#21864=CARTESIAN_POINT('',(5.3,6.,30.75));
#21865=CARTESIAN_POINT('',(5.,6.,30.75));
#21866=CARTESIAN_POINT('',(5.3,6.,25.));
#21867=CARTESIAN_POINT('',(5.3,6.,29.5625));
#21868=CARTESIAN_POINT('',(5.,6.,25.));
#21869=CARTESIAN_POINT('Origin',(5.,6.25,31.));
#21870=CARTESIAN_POINT('',(5.,6.5,31.25));
#21871=CARTESIAN_POINT('',(5.31458333333333,5.98541666666667,30.7354166666667));
#21872=CARTESIAN_POINT('Origin',(204.85,35.85,26.1875));
#21873=CARTESIAN_POINT('',(204.7,36.,30.75));
#21874=CARTESIAN_POINT('',(170.789583333331,69.9104166666672,-3.16041666666715));
#21875=CARTESIAN_POINT('',(204.7,36.,25.));
#21876=CARTESIAN_POINT('',(171.352083333331,69.3479166666672,58.3479166666672));
#21877=CARTESIAN_POINT('',(204.7,36.,26.1875));
#21878=CARTESIAN_POINT('Origin',(5.,35.75,31.));
#21879=CARTESIAN_POINT('',(5.3,36.,30.75));
#21880=CARTESIAN_POINT('',(5.,36.,30.75));
#21881=CARTESIAN_POINT('',(5.87708333333334,36.5770833333333,30.1729166666667));
#21882=CARTESIAN_POINT('',(5.,35.5,31.25));
#21883=CARTESIAN_POINT('Origin',(5.,36.,24.5));
#21884=CARTESIAN_POINT('',(5.3,36.,25.));
#21885=CARTESIAN_POINT('',(5.,36.,25.));
#21886=CARTESIAN_POINT('',(5.3,36.,26.1875));
#21887=CARTESIAN_POINT('Origin',(5.15,6.15,29.5625));
#21888=CARTESIAN_POINT('',(5.87708333333333,5.42291666666667,25.5770833333333));
#21889=CARTESIAN_POINT('Origin',(5.15,35.85,26.1875));
#21890=CARTESIAN_POINT('',(5.31458333333333,36.0145833333333,25.0145833333333));
#21891=CARTESIAN_POINT('Origin',(5.,24.5252893218813,31.1792893218813));
#21892=CARTESIAN_POINT('',(5.,24.696,31.25));
#21893=CARTESIAN_POINT('Origin',(5.,36.,31.25));
#21894=CARTESIAN_POINT('Origin',(5.,17.4747106781187,31.1792893218813));
#21895=CARTESIAN_POINT('',(5.,17.6454213562373,31.1085786437627));
#21896=CARTESIAN_POINT('',(5.,17.304,31.25));
#21897=CARTESIAN_POINT('Origin',(5.,20.4,28.354));
#21898=CARTESIAN_POINT('',(5.,20.4,28.354));
#21899=CARTESIAN_POINT('Origin',(5.,6.25,24.75));
#21900=CARTESIAN_POINT('Origin',(5.,35.75,24.75));
#21901=CARTESIAN_POINT('Origin',(5.,17.504,31.25));
#21902=CARTESIAN_POINT('Origin',(5.,20.4,27.154));
#21903=CARTESIAN_POINT('',(5.,20.4,27.154));
#21904=CARTESIAN_POINT('Origin',(5.,21.6,27.154));
#21905=CARTESIAN_POINT('',(5.,21.6,27.154));
#21906=CARTESIAN_POINT('Origin',(5.,21.6,28.354));
#21907=CARTESIAN_POINT('',(0.,0.,0.));
#21908=CARTESIAN_POINT('Origin',(204.9,31.,34.5));
#21909=CARTESIAN_POINT('',(204.8,31.,36.05));
#21910=CARTESIAN_POINT('Origin',(204.8,31.,34.5));
#21911=CARTESIAN_POINT('',(205.,31.,36.25));
#21912=CARTESIAN_POINT('',(204.9,31.,36.15));
#21913=CARTESIAN_POINT('',(205.,31.,32.75));
#21914=CARTESIAN_POINT('Origin',(205.,31.,34.5));
#21915=CARTESIAN_POINT('Origin',(205.,31.,34.5));
#21916=CARTESIAN_POINT('Origin',(205.,21.,36.125));
#21917=CARTESIAN_POINT('',(205.,6.3,32.95));
#21918=CARTESIAN_POINT('',(205.,6.3,39.3));
#21919=CARTESIAN_POINT('',(205.,6.3,37.8125));
#21920=CARTESIAN_POINT('',(205.,6.5,32.75));
#21921=CARTESIAN_POINT('',(205.,9.15625000000002,30.09375));
#21922=CARTESIAN_POINT('',(205.,17.304,32.75));
#21923=CARTESIAN_POINT('',(205.,6.,32.75));
#21924=CARTESIAN_POINT('',(205.,17.6454213562373,32.8914213562373));
#21925=CARTESIAN_POINT('',(205.,19.5633433515018,33.6858506582495));
#21926=CARTESIAN_POINT('',(205.,20.4,35.646));
#21927=CARTESIAN_POINT('',(205.,17.504,32.75));
#21928=CARTESIAN_POINT('',(205.,20.4,36.846));
#21929=CARTESIAN_POINT('',(205.,20.4,35.646));
#21930=CARTESIAN_POINT('',(205.,21.6,36.846));
#21931=CARTESIAN_POINT('',(205.,20.4,36.846));
#21932=CARTESIAN_POINT('',(205.,21.6,35.646));
#21933=CARTESIAN_POINT('',(205.,21.6,36.846));
#21934=CARTESIAN_POINT('',(205.,24.3545786437627,32.8914213562373));
#21935=CARTESIAN_POINT('',(205.,21.6,35.646));
#21936=CARTESIAN_POINT('',(205.,24.696,32.75));
#21937=CARTESIAN_POINT('',(205.,22.4366566484982,33.6858506582495));
#21938=CARTESIAN_POINT('',(205.,24.496,32.75));
#21939=CARTESIAN_POINT('',(205.,35.5,32.75));
#21940=CARTESIAN_POINT('',(205.,24.496,32.75));
#21941=CARTESIAN_POINT('',(205.,35.7,32.95));
#21942=CARTESIAN_POINT('',(205.,32.84375,30.09375));
#21943=CARTESIAN_POINT('',(205.,35.7,39.3));
#21944=CARTESIAN_POINT('',(205.,35.7,34.4375));
#21945=CARTESIAN_POINT('',(205.,35.5,39.5));
#21946=CARTESIAN_POINT('',(205.,32.84375,42.15625));
#21947=CARTESIAN_POINT('',(205.,6.5,39.5));
#21948=CARTESIAN_POINT('',(205.,36.,39.5));
#21949=CARTESIAN_POINT('',(205.,9.15625000000002,42.15625));
#21950=CARTESIAN_POINT('Origin',(205.,31.,34.5));
#21951=CARTESIAN_POINT('',(198.,31.,36.05));
#21952=CARTESIAN_POINT('',(205.,31.,36.05));
#21953=CARTESIAN_POINT('',(198.,29.45,34.5));
#21954=CARTESIAN_POINT('Origin',(198.,31.,34.5));
#21955=CARTESIAN_POINT('Origin',(198.,31.,34.5));
#21956=CARTESIAN_POINT('Origin',(197.534333020254,31.,34.5));
#21957=CARTESIAN_POINT('',(197.068666040507,31.,34.5));
#21958=CARTESIAN_POINT('',(197.534333020254,30.225,34.5));
#21959=CARTESIAN_POINT('Origin',(5.1,31.,34.5));
#21960=CARTESIAN_POINT('',(5.2,31.,36.05));
#21961=CARTESIAN_POINT('Origin',(5.2,31.,34.5));
#21962=CARTESIAN_POINT('',(5.,31.,36.25));
#21963=CARTESIAN_POINT('',(5.1,31.,36.15));
#21964=CARTESIAN_POINT('',(5.,31.,32.75));
#21965=CARTESIAN_POINT('Origin',(5.,31.,34.5));
#21966=CARTESIAN_POINT('Origin',(5.,31.,34.5));
#21967=CARTESIAN_POINT('Origin',(5.,21.,36.125));
#21968=CARTESIAN_POINT('',(5.,35.7,32.95));
#21969=CARTESIAN_POINT('',(5.,35.7,39.3));
#21970=CARTESIAN_POINT('',(5.,35.7,34.4375));
#21971=CARTESIAN_POINT('',(5.,35.5,32.75));
#21972=CARTESIAN_POINT('',(5.,32.84375,30.09375));
#21973=CARTESIAN_POINT('',(5.,24.496,32.75));
#21974=CARTESIAN_POINT('',(5.,24.696,32.75));
#21975=CARTESIAN_POINT('',(5.,24.496,32.75));
#21976=CARTESIAN_POINT('',(5.,24.3545786437627,32.8914213562373));
#21977=CARTESIAN_POINT('',(5.,22.4366566484982,33.6858506582495));
#21978=CARTESIAN_POINT('',(5.,21.6,35.646));
#21979=CARTESIAN_POINT('',(5.,21.6,35.646));
#21980=CARTESIAN_POINT('',(5.,21.6,36.846));
#21981=CARTESIAN_POINT('',(5.,21.6,36.846));
#21982=CARTESIAN_POINT('',(5.,20.4,36.846));
#21983=CARTESIAN_POINT('',(5.,20.4,36.846));
#21984=CARTESIAN_POINT('',(5.,20.4,35.646));
#21985=CARTESIAN_POINT('',(5.,20.4,35.646));
#21986=CARTESIAN_POINT('',(5.,17.6454213562373,32.8914213562373));
#21987=CARTESIAN_POINT('',(5.,17.504,32.75));
#21988=CARTESIAN_POINT('',(5.,17.304,32.75));
#21989=CARTESIAN_POINT('',(5.,19.5633433515018,33.6858506582495));
#21990=CARTESIAN_POINT('',(5.,6.5,32.75));
#21991=CARTESIAN_POINT('',(5.,6.,32.75));
#21992=CARTESIAN_POINT('',(5.,6.3,32.95));
#21993=CARTESIAN_POINT('',(5.,9.15625000000002,30.09375));
#21994=CARTESIAN_POINT('',(5.,6.3,39.3));
#21995=CARTESIAN_POINT('',(5.,6.3,37.8125));
#21996=CARTESIAN_POINT('',(5.,6.5,39.5));
#21997=CARTESIAN_POINT('',(5.,9.15625000000002,42.15625));
#21998=CARTESIAN_POINT('',(5.,35.5,39.5));
#21999=CARTESIAN_POINT('',(5.,36.,39.5));
#22000=CARTESIAN_POINT('',(5.,32.84375,42.15625));
#22001=CARTESIAN_POINT('Origin',(5.,31.,34.5));
#22002=CARTESIAN_POINT('',(12.,31.,36.05));
#22003=CARTESIAN_POINT('',(5.,31.,36.05));
#22004=CARTESIAN_POINT('',(12.,29.45,34.5));
#22005=CARTESIAN_POINT('Origin',(12.,31.,34.5));
#22006=CARTESIAN_POINT('Origin',(12.,31.,34.5));
#22007=CARTESIAN_POINT('Origin',(12.,31.,34.5));
#22008=CARTESIAN_POINT('',(12.9313339594927,31.,34.5));
#22009=CARTESIAN_POINT('',(12.,29.45,34.5));
#22010=CARTESIAN_POINT('Origin',(180.,21.,39.35));
#22011=CARTESIAN_POINT('',(177.45,21.,39.2));
#22012=CARTESIAN_POINT('Origin',(180.,21.,39.2));
#22013=CARTESIAN_POINT('',(177.15,21.,39.5));
#22014=CARTESIAN_POINT('',(177.3,21.,39.35));
#22015=CARTESIAN_POINT('Origin',(180.,21.,39.5));
#22016=CARTESIAN_POINT('Origin',(5.,36.,39.5));
#22017=CARTESIAN_POINT('',(5.,6.5,39.5));
#22018=CARTESIAN_POINT('',(5.,35.5,39.5));
#22019=CARTESIAN_POINT('',(27.15,21.,39.5));
#22020=CARTESIAN_POINT('Origin',(30.,21.,39.5));
#22021=CARTESIAN_POINT('',(127.15,21.,39.5));
#22022=CARTESIAN_POINT('Origin',(130.,21.,39.5));
#22023=CARTESIAN_POINT('',(77.15,21.,39.5));
#22024=CARTESIAN_POINT('Origin',(80.,21.,39.5));
#22025=CARTESIAN_POINT('Origin',(180.,21.,39.5));
#22026=CARTESIAN_POINT('',(177.45,21.,36.846));
#22027=CARTESIAN_POINT('',(177.45,21.,39.5));
#22028=CARTESIAN_POINT('',(177.521593253721,21.6,36.846));
#22029=CARTESIAN_POINT('Origin',(180.,21.,36.846));
#22030=CARTESIAN_POINT('',(177.521593253721,21.6,35.646));
#22031=CARTESIAN_POINT('',(177.521593253721,21.6,39.5));
#22032=CARTESIAN_POINT('',(177.545690321088,21.692,35.554));
#22033=CARTESIAN_POINT('Origin',(180.,21.,36.246));
#22034=CARTESIAN_POINT('',(182.454309678912,21.692,35.554));
#22035=CARTESIAN_POINT('Origin',(180.,21.,35.554));
#22036=CARTESIAN_POINT('',(182.478406746279,21.6,35.646));
#22037=CARTESIAN_POINT('Origin',(180.,21.,36.246));
#22038=CARTESIAN_POINT('',(182.478406746279,21.6,36.846));
#22039=CARTESIAN_POINT('',(182.478406746279,21.6,39.5));
#22040=CARTESIAN_POINT('',(182.478406746279,20.4,36.846));
#22041=CARTESIAN_POINT('Origin',(180.,21.,36.846));
#22042=CARTESIAN_POINT('',(182.478406746279,20.4,35.646));
#22043=CARTESIAN_POINT('',(182.478406746279,20.4,39.5));
#22044=CARTESIAN_POINT('',(182.454309678912,20.308,35.554));
#22045=CARTESIAN_POINT('Origin',(180.,21.,36.246));
#22046=CARTESIAN_POINT('',(177.545690321088,20.308,35.554));
#22047=CARTESIAN_POINT('Origin',(180.,21.,35.554));
#22048=CARTESIAN_POINT('',(177.521593253721,20.4,35.646));
#22049=CARTESIAN_POINT('Origin',(180.,21.,36.246));
#22050=CARTESIAN_POINT('',(177.521593253721,20.4,36.846));
#22051=CARTESIAN_POINT('',(177.521593253721,20.4,39.5));
#22052=CARTESIAN_POINT('Origin',(180.,21.,36.846));
#22053=CARTESIAN_POINT('Origin',(30.,21.,39.35));
#22054=CARTESIAN_POINT('',(27.45,21.,39.2));
#22055=CARTESIAN_POINT('Origin',(30.,21.,39.2));
#22056=CARTESIAN_POINT('',(27.3,21.,39.35));
#22057=CARTESIAN_POINT('Origin',(30.,21.,39.5));
#22058=CARTESIAN_POINT('',(27.45,21.,36.846));
#22059=CARTESIAN_POINT('',(27.45,21.,39.5));
#22060=CARTESIAN_POINT('',(27.5215932537213,21.6,36.846));
#22061=CARTESIAN_POINT('Origin',(30.,21.,36.846));
#22062=CARTESIAN_POINT('',(27.5215932537213,21.6,35.646));
#22063=CARTESIAN_POINT('',(27.5215932537213,21.6,39.5));
#22064=CARTESIAN_POINT('',(27.5456903210882,21.692,35.554));
#22065=CARTESIAN_POINT('Origin',(30.,21.,36.246));
#22066=CARTESIAN_POINT('',(32.4543096789118,21.692,35.554));
#22067=CARTESIAN_POINT('Origin',(30.,21.,35.554));
#22068=CARTESIAN_POINT('',(32.4784067462787,21.6,35.646));
#22069=CARTESIAN_POINT('Origin',(30.,21.,36.246));
#22070=CARTESIAN_POINT('',(32.4784067462787,21.6,36.846));
#22071=CARTESIAN_POINT('',(32.4784067462787,21.6,39.5));
#22072=CARTESIAN_POINT('',(32.4784067462787,20.4,36.846));
#22073=CARTESIAN_POINT('Origin',(30.,21.,36.846));
#22074=CARTESIAN_POINT('',(32.4784067462787,20.4,35.646));
#22075=CARTESIAN_POINT('',(32.4784067462787,20.4,39.5));
#22076=CARTESIAN_POINT('',(32.4543096789118,20.308,35.554));
#22077=CARTESIAN_POINT('Origin',(30.,21.,36.246));
#22078=CARTESIAN_POINT('',(27.5456903210882,20.308,35.554));
#22079=CARTESIAN_POINT('Origin',(30.,21.,35.554));
#22080=CARTESIAN_POINT('',(27.5215932537213,20.4,35.646));
#22081=CARTESIAN_POINT('Origin',(30.,21.,36.246));
#22082=CARTESIAN_POINT('',(27.5215932537213,20.4,36.846));
#22083=CARTESIAN_POINT('',(27.5215932537213,20.4,39.5));
#22084=CARTESIAN_POINT('Origin',(30.,21.,36.846));
#22085=CARTESIAN_POINT('Origin',(80.,21.,39.35));
#22086=CARTESIAN_POINT('',(77.45,21.,39.2));
#22087=CARTESIAN_POINT('Origin',(80.,21.,39.2));
#22088=CARTESIAN_POINT('',(77.3,21.,39.35));
#22089=CARTESIAN_POINT('Origin',(80.,21.,39.5));
#22090=CARTESIAN_POINT('',(77.45,21.,36.846));
#22091=CARTESIAN_POINT('',(77.45,21.,39.5));
#22092=CARTESIAN_POINT('',(77.5215932537212,21.6,36.846));
#22093=CARTESIAN_POINT('Origin',(80.,21.,36.846));
#22094=CARTESIAN_POINT('',(77.5215932537212,21.6,35.646));
#22095=CARTESIAN_POINT('',(77.5215932537212,21.6,39.5));
#22096=CARTESIAN_POINT('',(77.5456903210882,21.692,35.554));
#22097=CARTESIAN_POINT('Origin',(80.,21.,36.246));
#22098=CARTESIAN_POINT('',(82.4543096789118,21.692,35.554));
#22099=CARTESIAN_POINT('Origin',(80.,21.,35.554));
#22100=CARTESIAN_POINT('',(82.4784067462788,21.6,35.646));
#22101=CARTESIAN_POINT('Origin',(80.,21.,36.246));
#22102=CARTESIAN_POINT('',(82.4784067462788,21.6,36.846));
#22103=CARTESIAN_POINT('',(82.4784067462788,21.6,39.5));
#22104=CARTESIAN_POINT('',(82.4784067462788,20.4,36.846));
#22105=CARTESIAN_POINT('Origin',(80.,21.,36.846));
#22106=CARTESIAN_POINT('',(82.4784067462788,20.4,35.646));
#22107=CARTESIAN_POINT('',(82.4784067462788,20.4,39.5));
#22108=CARTESIAN_POINT('',(82.4543096789118,20.308,35.554));
#22109=CARTESIAN_POINT('Origin',(80.,21.,36.246));
#22110=CARTESIAN_POINT('',(77.5456903210882,20.308,35.554));
#22111=CARTESIAN_POINT('Origin',(80.,21.,35.554));
#22112=CARTESIAN_POINT('',(77.5215932537212,20.4,35.646));
#22113=CARTESIAN_POINT('Origin',(80.,21.,36.246));
#22114=CARTESIAN_POINT('',(77.5215932537212,20.4,36.846));
#22115=CARTESIAN_POINT('',(77.5215932537212,20.4,39.5));
#22116=CARTESIAN_POINT('Origin',(80.,21.,36.846));
#22117=CARTESIAN_POINT('Origin',(130.,21.,39.35));
#22118=CARTESIAN_POINT('',(127.45,21.,39.2));
#22119=CARTESIAN_POINT('Origin',(130.,21.,39.2));
#22120=CARTESIAN_POINT('',(127.3,21.,39.35));
#22121=CARTESIAN_POINT('Origin',(130.,21.,39.5));
#22122=CARTESIAN_POINT('',(127.45,21.,36.846));
#22123=CARTESIAN_POINT('',(127.45,21.,39.5));
#22124=CARTESIAN_POINT('',(127.521593253721,21.6,36.846));
#22125=CARTESIAN_POINT('Origin',(130.,21.,36.846));
#22126=CARTESIAN_POINT('',(127.521593253721,21.6,35.646));
#22127=CARTESIAN_POINT('',(127.521593253721,21.6,39.5));
#22128=CARTESIAN_POINT('',(127.545690321088,21.692,35.554));
#22129=CARTESIAN_POINT('Origin',(130.,21.,36.246));
#22130=CARTESIAN_POINT('',(132.454309678912,21.692,35.554));
#22131=CARTESIAN_POINT('Origin',(130.,21.,35.554));
#22132=CARTESIAN_POINT('',(132.478406746279,21.6,35.646));
#22133=CARTESIAN_POINT('Origin',(130.,21.,36.246));
#22134=CARTESIAN_POINT('',(132.478406746279,21.6,36.846));
#22135=CARTESIAN_POINT('',(132.478406746279,21.6,39.5));
#22136=CARTESIAN_POINT('',(132.478406746279,20.4,36.846));
#22137=CARTESIAN_POINT('Origin',(130.,21.,36.846));
#22138=CARTESIAN_POINT('',(132.478406746279,20.4,35.646));
#22139=CARTESIAN_POINT('',(132.478406746279,20.4,39.5));
#22140=CARTESIAN_POINT('',(132.454309678912,20.308,35.554));
#22141=CARTESIAN_POINT('Origin',(130.,21.,36.246));
#22142=CARTESIAN_POINT('',(127.545690321088,20.308,35.554));
#22143=CARTESIAN_POINT('Origin',(130.,21.,35.554));
#22144=CARTESIAN_POINT('',(127.521593253721,20.4,35.646));
#22145=CARTESIAN_POINT('Origin',(130.,21.,36.246));
#22146=CARTESIAN_POINT('',(127.521593253721,20.4,36.846));
#22147=CARTESIAN_POINT('',(127.521593253721,20.4,39.5));
#22148=CARTESIAN_POINT('Origin',(130.,21.,36.846));
#22149=CARTESIAN_POINT('Origin',(130.,21.,35.554));
#22150=CARTESIAN_POINT('',(67.5,21.692,35.554));
#22151=CARTESIAN_POINT('Origin',(130.,21.,35.554));
#22152=CARTESIAN_POINT('',(67.5,20.308,35.554));
#22153=CARTESIAN_POINT('Origin',(80.,21.,35.554));
#22154=CARTESIAN_POINT('',(42.5,21.692,35.554));
#22155=CARTESIAN_POINT('Origin',(80.,21.,35.554));
#22156=CARTESIAN_POINT('',(42.5,20.308,35.554));
#22157=CARTESIAN_POINT('Origin',(30.,21.,35.554));
#22158=CARTESIAN_POINT('',(17.5,21.692,35.554));
#22159=CARTESIAN_POINT('Origin',(30.,21.,35.554));
#22160=CARTESIAN_POINT('',(17.5,20.308,35.554));
#22161=CARTESIAN_POINT('Origin',(180.,21.,35.554));
#22162=CARTESIAN_POINT('',(92.5,21.692,35.554));
#22163=CARTESIAN_POINT('Origin',(180.,21.,35.554));
#22164=CARTESIAN_POINT('',(92.5,20.308,35.554));
#22165=CARTESIAN_POINT('Origin',(5.,17.504,32.75));
#22166=CARTESIAN_POINT('',(5.,20.4,35.646));
#22167=CARTESIAN_POINT('',(5.,20.4,35.646));
#22168=CARTESIAN_POINT('',(5.,17.6454213562373,32.8914213562373));
#22169=CARTESIAN_POINT('',(5.,20.4,35.646));
#22170=CARTESIAN_POINT('',(5.,20.4,35.646));
#22171=CARTESIAN_POINT('',(5.,20.4,35.646));
#22172=CARTESIAN_POINT('Origin',(5.,20.4,35.646));
#22173=CARTESIAN_POINT('',(5.,20.4,36.846));
#22174=CARTESIAN_POINT('Origin',(5.,20.4,35.646));
#22175=CARTESIAN_POINT('',(5.,20.4,36.846));
#22176=CARTESIAN_POINT('Origin',(5.,20.4,35.646));
#22177=CARTESIAN_POINT('',(5.,20.4,36.846));
#22178=CARTESIAN_POINT('Origin',(5.,20.4,35.646));
#22179=CARTESIAN_POINT('',(5.,20.4,36.846));
#22180=CARTESIAN_POINT('Origin',(5.,20.4,36.846));
#22181=CARTESIAN_POINT('',(5.,21.6,36.846));
#22182=CARTESIAN_POINT('Origin',(5.,20.4,36.846));
#22183=CARTESIAN_POINT('',(5.,21.6,36.846));
#22184=CARTESIAN_POINT('Origin',(5.,20.4,36.846));
#22185=CARTESIAN_POINT('',(5.,21.6,36.846));
#22186=CARTESIAN_POINT('Origin',(5.,20.4,36.846));
#22187=CARTESIAN_POINT('',(5.,21.6,36.846));
#22188=CARTESIAN_POINT('Origin',(5.,21.6,36.846));
#22189=CARTESIAN_POINT('',(5.,21.6,35.646));
#22190=CARTESIAN_POINT('Origin',(5.,21.6,36.846));
#22191=CARTESIAN_POINT('',(5.,21.6,35.646));
#22192=CARTESIAN_POINT('Origin',(5.,21.6,36.846));
#22193=CARTESIAN_POINT('',(5.,21.6,35.646));
#22194=CARTESIAN_POINT('Origin',(5.,21.6,36.846));
#22195=CARTESIAN_POINT('',(5.,21.6,35.646));
#22196=CARTESIAN_POINT('Origin',(204.85,6.15,37.8125));
#22197=CARTESIAN_POINT('',(204.7,6.,33.25));
#22198=CARTESIAN_POINT('',(170.789583333332,-27.9104166666672,67.160416666667));
#22199=CARTESIAN_POINT('',(204.7,6.,39.));
#22200=CARTESIAN_POINT('',(171.352083333332,-27.3479166666672,5.652083333333));
#22201=CARTESIAN_POINT('',(204.7,6.,37.8125));
#22202=CARTESIAN_POINT('Origin',(5.,6.25,39.25));
#22203=CARTESIAN_POINT('',(5.3,6.,39.));
#22204=CARTESIAN_POINT('',(5.31458333333333,5.98541666666667,38.9854166666667));
#22205=CARTESIAN_POINT('',(5.,6.,39.));
#22206=CARTESIAN_POINT('Origin',(204.85,35.85,34.4375));
#22207=CARTESIAN_POINT('',(204.7,36.,39.));
#22208=CARTESIAN_POINT('',(170.789583333331,69.9104166666672,5.08958333333285));
#22209=CARTESIAN_POINT('',(204.7,36.,33.25));
#22210=CARTESIAN_POINT('',(171.352083333331,69.3479166666672,66.5979166666672));
#22211=CARTESIAN_POINT('',(204.7,36.,34.4375));
#22212=CARTESIAN_POINT('Origin',(5.,35.75,39.25));
#22213=CARTESIAN_POINT('',(5.3,36.,39.));
#22214=CARTESIAN_POINT('',(5.,36.,39.));
#22215=CARTESIAN_POINT('',(5.87708333333334,36.5770833333333,38.4229166666667));
#22216=CARTESIAN_POINT('Origin',(5.15,35.85,34.4375));
#22217=CARTESIAN_POINT('',(5.3,36.,33.25));
#22218=CARTESIAN_POINT('',(5.3,36.,34.4375));
#22219=CARTESIAN_POINT('',(5.31458333333333,36.0145833333333,33.2645833333333));
#22220=CARTESIAN_POINT('Origin',(5.15,6.15,37.8125));
#22221=CARTESIAN_POINT('',(5.3,6.,33.25));
#22222=CARTESIAN_POINT('',(5.87708333333333,5.42291666666667,33.8270833333333));
#22223=CARTESIAN_POINT('',(5.3,6.,37.8125));
#22224=CARTESIAN_POINT('Origin',(5.,17.4747106781187,32.8207106781187));
#22225=CARTESIAN_POINT('',(5.,17.304,32.75));
#22226=CARTESIAN_POINT('Origin',(5.,6.,32.75));
#22227=CARTESIAN_POINT('',(5.,6.5,32.75));
#22228=CARTESIAN_POINT('Origin',(5.,24.5252893218813,32.8207106781187));
#22229=CARTESIAN_POINT('',(5.,24.3545786437627,32.8914213562373));
#22230=CARTESIAN_POINT('',(5.,24.696,32.75));
#22231=CARTESIAN_POINT('Origin',(5.,21.6,35.646));
#22232=CARTESIAN_POINT('',(5.,21.6,35.646));
#22233=CARTESIAN_POINT('Origin',(5.,6.,39.5));
#22234=CARTESIAN_POINT('',(5.,6.,33.25));
#22235=CARTESIAN_POINT('Origin',(5.,6.25,33.));
#22236=CARTESIAN_POINT('Origin',(5.,35.75,33.));
#22237=CARTESIAN_POINT('',(5.,35.5,32.75));
#22238=CARTESIAN_POINT('',(5.,36.,33.25));
#22239=CARTESIAN_POINT('Origin',(5.,24.496,32.75));
#22240=CARTESIAN_POINT('Origin',(5.,36.,32.75));
#22241=CARTESIAN_POINT('Origin',(5.,21.6,36.846));
#22242=CARTESIAN_POINT('',(5.,21.6,36.846));
#22243=CARTESIAN_POINT('Origin',(5.,20.4,36.846));
#22244=CARTESIAN_POINT('',(5.,20.4,36.846));
#22245=CARTESIAN_POINT('Origin',(5.,20.4,35.646));
#22246=CARTESIAN_POINT('',(0.,0.,0.));
#22247=CARTESIAN_POINT('Origin',(169.2,22.1,31.45));
#22248=CARTESIAN_POINT('',(169.2,22.1,31.45));
#22249=CARTESIAN_POINT('',(169.2,19.9,31.45));
#22250=CARTESIAN_POINT('',(169.2,21.55,31.45));
#22251=CARTESIAN_POINT('',(169.2,22.1,32.55));
#22252=CARTESIAN_POINT('',(169.2,22.1,31.45));
#22253=CARTESIAN_POINT('',(169.2,19.9,32.55));
#22254=CARTESIAN_POINT('',(169.2,21.55,32.55));
#22255=CARTESIAN_POINT('',(169.2,19.9,31.45));
#22256=CARTESIAN_POINT('Origin',(169.6,22.1,31.45));
#22257=CARTESIAN_POINT('',(169.6,22.5,31.45));
#22258=CARTESIAN_POINT('Origin',(169.6,22.1,31.45));
#22259=CARTESIAN_POINT('',(169.6,22.5,32.55));
#22260=CARTESIAN_POINT('',(169.6,22.5,31.45));
#22261=CARTESIAN_POINT('Origin',(169.6,22.1,32.55));
#22262=CARTESIAN_POINT('Origin',(170.,22.5,31.45));
#22263=CARTESIAN_POINT('',(170.,22.5,31.45));
#22264=CARTESIAN_POINT('',(137.5,22.5,31.45));
#22265=CARTESIAN_POINT('',(170.,22.5,32.55));
#22266=CARTESIAN_POINT('',(170.,22.5,31.45));
#22267=CARTESIAN_POINT('',(137.5,22.5,32.55));
#22268=CARTESIAN_POINT('Origin',(170.,22.1000000000001,31.45));
#22269=CARTESIAN_POINT('',(170.4,22.1,31.45));
#22270=CARTESIAN_POINT('Origin',(170.,22.1000000000001,31.45));
#22271=CARTESIAN_POINT('',(170.4,22.1,32.55));
#22272=CARTESIAN_POINT('',(170.4,22.1,31.45));
#22273=CARTESIAN_POINT('Origin',(170.,22.1000000000001,32.55));
#22274=CARTESIAN_POINT('Origin',(170.4,19.9,31.45));
#22275=CARTESIAN_POINT('',(170.4,19.9,31.45));
#22276=CARTESIAN_POINT('',(170.4,20.45,31.45));
#22277=CARTESIAN_POINT('',(170.4,19.9,32.55));
#22278=CARTESIAN_POINT('',(170.4,19.9,31.45));
#22279=CARTESIAN_POINT('',(170.4,20.45,32.55));
#22280=CARTESIAN_POINT('Origin',(170.,19.8999999999999,31.45));
#22281=CARTESIAN_POINT('',(170.,19.5,31.45));
#22282=CARTESIAN_POINT('Origin',(170.,19.8999999999999,31.45));
#22283=CARTESIAN_POINT('',(170.,19.5,32.55));
#22284=CARTESIAN_POINT('',(170.,19.5,31.45));
#22285=CARTESIAN_POINT('Origin',(170.,19.8999999999999,32.55));
#22286=CARTESIAN_POINT('Origin',(169.6,19.5,31.45));
#22287=CARTESIAN_POINT('',(169.6,19.5,31.45));
#22288=CARTESIAN_POINT('',(137.3,19.5,31.45));
#22289=CARTESIAN_POINT('',(169.6,19.5,32.55));
#22290=CARTESIAN_POINT('',(169.6,19.5,31.45));
#22291=CARTESIAN_POINT('',(137.3,19.5,32.55));
#22292=CARTESIAN_POINT('Origin',(169.6,19.9,31.45));
#22293=CARTESIAN_POINT('Origin',(169.6,19.9,31.45));
#22294=CARTESIAN_POINT('Origin',(169.6,19.9,32.55));
#22295=CARTESIAN_POINT('Origin',(39.6,22.1,31.45));
#22296=CARTESIAN_POINT('',(39.6,22.1,31.45));
#22297=CARTESIAN_POINT('',(39.6,19.9,31.45));
#22298=CARTESIAN_POINT('',(39.6,21.55,31.45));
#22299=CARTESIAN_POINT('',(39.6,22.1,32.55));
#22300=CARTESIAN_POINT('',(39.6,22.1,31.45));
#22301=CARTESIAN_POINT('',(39.6,19.9,32.55));
#22302=CARTESIAN_POINT('',(39.6,21.55,32.55));
#22303=CARTESIAN_POINT('',(39.6,19.9,31.45));
#22304=CARTESIAN_POINT('Origin',(40.,22.1,31.45));
#22305=CARTESIAN_POINT('',(40.,22.5,31.45));
#22306=CARTESIAN_POINT('Origin',(40.,22.1,31.45));
#22307=CARTESIAN_POINT('',(40.,22.5,32.55));
#22308=CARTESIAN_POINT('',(40.,22.5,31.45));
#22309=CARTESIAN_POINT('Origin',(40.,22.1,32.55));
#22310=CARTESIAN_POINT('Origin',(40.4,22.5,31.45));
#22311=CARTESIAN_POINT('',(40.4,22.5,31.45));
#22312=CARTESIAN_POINT('',(72.7,22.5,31.45));
#22313=CARTESIAN_POINT('',(40.4,22.5,32.55));
#22314=CARTESIAN_POINT('',(40.4,22.5,31.45));
#22315=CARTESIAN_POINT('',(72.7,22.5,32.55));
#22316=CARTESIAN_POINT('Origin',(40.4,22.1,31.45));
#22317=CARTESIAN_POINT('',(40.8,22.1,31.45));
#22318=CARTESIAN_POINT('Origin',(40.4,22.1,31.45));
#22319=CARTESIAN_POINT('',(40.8,22.1,32.55));
#22320=CARTESIAN_POINT('',(40.8,22.1,31.45));
#22321=CARTESIAN_POINT('Origin',(40.4,22.1,32.55));
#22322=CARTESIAN_POINT('Origin',(40.8,19.9,31.45));
#22323=CARTESIAN_POINT('',(40.8,19.9,31.45));
#22324=CARTESIAN_POINT('',(40.8,20.45,31.45));
#22325=CARTESIAN_POINT('',(40.8,19.9,32.55));
#22326=CARTESIAN_POINT('',(40.8,19.9,31.45));
#22327=CARTESIAN_POINT('',(40.8,20.45,32.55));
#22328=CARTESIAN_POINT('Origin',(40.4,19.9,31.45));
#22329=CARTESIAN_POINT('',(40.4,19.5,31.45));
#22330=CARTESIAN_POINT('Origin',(40.4,19.9,31.45));
#22331=CARTESIAN_POINT('',(40.4,19.5,32.55));
#22332=CARTESIAN_POINT('',(40.4,19.5,31.45));
#22333=CARTESIAN_POINT('Origin',(40.4,19.9,32.55));
#22334=CARTESIAN_POINT('Origin',(40.,19.5,31.45));
#22335=CARTESIAN_POINT('',(40.,19.5,31.45));
#22336=CARTESIAN_POINT('',(72.5,19.5,31.45));
#22337=CARTESIAN_POINT('',(40.,19.5,32.55));
#22338=CARTESIAN_POINT('',(40.,19.5,31.45));
#22339=CARTESIAN_POINT('',(72.5,19.5,32.55));
#22340=CARTESIAN_POINT('Origin',(40.,19.9,31.45));
#22341=CARTESIAN_POINT('Origin',(40.,19.9,31.45));
#22342=CARTESIAN_POINT('Origin',(40.,19.9,32.55));
#22343=CARTESIAN_POINT('Origin',(151.8,24.7,31.45));
#22344=CARTESIAN_POINT('',(151.8,24.7,31.45));
#22345=CARTESIAN_POINT('',(151.8,17.3,31.45));
#22346=CARTESIAN_POINT('',(151.8,22.85,31.45));
#22347=CARTESIAN_POINT('',(151.8,24.7,32.55));
#22348=CARTESIAN_POINT('',(151.8,24.7,31.45));
#22349=CARTESIAN_POINT('',(151.8,17.3,32.55));
#22350=CARTESIAN_POINT('',(151.8,22.85,32.55));
#22351=CARTESIAN_POINT('',(151.8,17.3,31.45));
#22352=CARTESIAN_POINT('Origin',(152.4,24.7,31.45));
#22353=CARTESIAN_POINT('',(152.4,25.3,31.45));
#22354=CARTESIAN_POINT('Origin',(152.4,24.7,31.45));
#22355=CARTESIAN_POINT('',(152.4,25.3,32.55));
#22356=CARTESIAN_POINT('',(152.4,25.3,31.45));
#22357=CARTESIAN_POINT('Origin',(152.4,24.7,32.55));
#22358=CARTESIAN_POINT('Origin',(157.6,25.3,31.45));
#22359=CARTESIAN_POINT('',(157.6,25.3,31.45));
#22360=CARTESIAN_POINT('',(131.3,25.3,31.45));
#22361=CARTESIAN_POINT('',(157.6,25.3,32.55));
#22362=CARTESIAN_POINT('',(157.6,25.3,31.45));
#22363=CARTESIAN_POINT('',(131.3,25.3,32.55));
#22364=CARTESIAN_POINT('Origin',(157.6,24.7,31.45));
#22365=CARTESIAN_POINT('',(158.2,24.7,31.45));
#22366=CARTESIAN_POINT('Origin',(157.6,24.7,31.45));
#22367=CARTESIAN_POINT('',(158.2,24.7,32.55));
#22368=CARTESIAN_POINT('',(158.2,24.7,31.45));
#22369=CARTESIAN_POINT('Origin',(157.6,24.7,32.55));
#22370=CARTESIAN_POINT('Origin',(158.2,17.3,31.45));
#22371=CARTESIAN_POINT('',(158.2,17.3,31.45));
#22372=CARTESIAN_POINT('',(158.2,19.15,31.45));
#22373=CARTESIAN_POINT('',(158.2,17.3,32.55));
#22374=CARTESIAN_POINT('',(158.2,17.3,31.45));
#22375=CARTESIAN_POINT('',(158.2,19.15,32.55));
#22376=CARTESIAN_POINT('Origin',(157.6,17.3,31.45));
#22377=CARTESIAN_POINT('',(157.6,16.7,31.45));
#22378=CARTESIAN_POINT('Origin',(157.6,17.3,31.45));
#22379=CARTESIAN_POINT('',(157.6,16.7,32.55));
#22380=CARTESIAN_POINT('',(157.6,16.7,31.45));
#22381=CARTESIAN_POINT('Origin',(157.6,17.3,32.55));
#22382=CARTESIAN_POINT('Origin',(152.4,16.7,31.45));
#22383=CARTESIAN_POINT('',(152.4,16.7,31.45));
#22384=CARTESIAN_POINT('',(128.7,16.7,31.45));
#22385=CARTESIAN_POINT('',(152.4,16.7,32.55));
#22386=CARTESIAN_POINT('',(152.4,16.7,31.45));
#22387=CARTESIAN_POINT('',(128.7,16.7,32.55));
#22388=CARTESIAN_POINT('Origin',(152.4,17.3,31.45));
#22389=CARTESIAN_POINT('Origin',(152.4,17.3,31.45));
#22390=CARTESIAN_POINT('Origin',(152.4,17.3,32.55));
#22391=CARTESIAN_POINT('Origin',(131.8,24.7,31.45));
#22392=CARTESIAN_POINT('',(131.8,24.7,31.45));
#22393=CARTESIAN_POINT('',(131.8,17.3,31.45));
#22394=CARTESIAN_POINT('',(131.8,22.85,31.45));
#22395=CARTESIAN_POINT('',(131.8,24.7,32.55));
#22396=CARTESIAN_POINT('',(131.8,24.7,31.45));
#22397=CARTESIAN_POINT('',(131.8,17.3,32.55));
#22398=CARTESIAN_POINT('',(131.8,22.85,32.55));
#22399=CARTESIAN_POINT('',(131.8,17.3,31.45));
#22400=CARTESIAN_POINT('Origin',(132.4,24.7,31.45));
#22401=CARTESIAN_POINT('',(132.4,25.3,31.45));
#22402=CARTESIAN_POINT('Origin',(132.4,24.7,31.45));
#22403=CARTESIAN_POINT('',(132.4,25.3,32.55));
#22404=CARTESIAN_POINT('',(132.4,25.3,31.45));
#22405=CARTESIAN_POINT('Origin',(132.4,24.7,32.55));
#22406=CARTESIAN_POINT('Origin',(137.6,25.3,31.45));
#22407=CARTESIAN_POINT('',(137.6,25.3,31.45));
#22408=CARTESIAN_POINT('',(121.3,25.3,31.45));
#22409=CARTESIAN_POINT('',(137.6,25.3,32.55));
#22410=CARTESIAN_POINT('',(137.6,25.3,31.45));
#22411=CARTESIAN_POINT('',(121.3,25.3,32.55));
#22412=CARTESIAN_POINT('Origin',(137.6,24.7,31.45));
#22413=CARTESIAN_POINT('',(138.2,24.7,31.45));
#22414=CARTESIAN_POINT('Origin',(137.6,24.7,31.45));
#22415=CARTESIAN_POINT('',(138.2,24.7,32.55));
#22416=CARTESIAN_POINT('',(138.2,24.7,31.45));
#22417=CARTESIAN_POINT('Origin',(137.6,24.7,32.55));
#22418=CARTESIAN_POINT('Origin',(138.2,17.3,31.45));
#22419=CARTESIAN_POINT('',(138.2,17.3,31.45));
#22420=CARTESIAN_POINT('',(138.2,19.15,31.45));
#22421=CARTESIAN_POINT('',(138.2,17.3,32.55));
#22422=CARTESIAN_POINT('',(138.2,17.3,31.45));
#22423=CARTESIAN_POINT('',(138.2,19.15,32.55));
#22424=CARTESIAN_POINT('Origin',(137.6,17.3,31.45));
#22425=CARTESIAN_POINT('',(137.6,16.7,31.45));
#22426=CARTESIAN_POINT('Origin',(137.6,17.3,31.45));
#22427=CARTESIAN_POINT('',(137.6,16.7,32.55));
#22428=CARTESIAN_POINT('',(137.6,16.7,31.45));
#22429=CARTESIAN_POINT('Origin',(137.6,17.3,32.55));
#22430=CARTESIAN_POINT('Origin',(132.4,16.7,31.45));
#22431=CARTESIAN_POINT('',(132.4,16.7,31.45));
#22432=CARTESIAN_POINT('',(118.7,16.7,31.45));
#22433=CARTESIAN_POINT('',(132.4,16.7,32.55));
#22434=CARTESIAN_POINT('',(132.4,16.7,31.45));
#22435=CARTESIAN_POINT('',(118.7,16.7,32.55));
#22436=CARTESIAN_POINT('Origin',(132.4,17.3,31.45));
#22437=CARTESIAN_POINT('Origin',(132.4,17.3,31.45));
#22438=CARTESIAN_POINT('Origin',(132.4,17.3,32.55));
#22439=CARTESIAN_POINT('Origin',(111.8,24.7,31.45));
#22440=CARTESIAN_POINT('',(111.8,24.7,31.45));
#22441=CARTESIAN_POINT('',(111.8,17.3,31.45));
#22442=CARTESIAN_POINT('',(111.8,22.85,31.45));
#22443=CARTESIAN_POINT('',(111.8,24.7,32.55));
#22444=CARTESIAN_POINT('',(111.8,24.7,31.45));
#22445=CARTESIAN_POINT('',(111.8,17.3,32.55));
#22446=CARTESIAN_POINT('',(111.8,22.85,32.55));
#22447=CARTESIAN_POINT('',(111.8,17.3,31.45));
#22448=CARTESIAN_POINT('Origin',(112.4,24.7,31.45));
#22449=CARTESIAN_POINT('',(112.4,25.3,31.45));
#22450=CARTESIAN_POINT('Origin',(112.4,24.7,31.45));
#22451=CARTESIAN_POINT('',(112.4,25.3,32.55));
#22452=CARTESIAN_POINT('',(112.4,25.3,31.45));
#22453=CARTESIAN_POINT('Origin',(112.4,24.7,32.55));
#22454=CARTESIAN_POINT('Origin',(117.6,25.3,31.45));
#22455=CARTESIAN_POINT('',(117.6,25.3,31.45));
#22456=CARTESIAN_POINT('',(111.3,25.3,31.45));
#22457=CARTESIAN_POINT('',(117.6,25.3,32.55));
#22458=CARTESIAN_POINT('',(117.6,25.3,31.45));
#22459=CARTESIAN_POINT('',(111.3,25.3,32.55));
#22460=CARTESIAN_POINT('Origin',(117.6,24.7,31.45));
#22461=CARTESIAN_POINT('',(118.2,24.7,31.45));
#22462=CARTESIAN_POINT('Origin',(117.6,24.7,31.45));
#22463=CARTESIAN_POINT('',(118.2,24.7,32.55));
#22464=CARTESIAN_POINT('',(118.2,24.7,31.45));
#22465=CARTESIAN_POINT('Origin',(117.6,24.7,32.55));
#22466=CARTESIAN_POINT('Origin',(118.2,17.3,31.45));
#22467=CARTESIAN_POINT('',(118.2,17.3,31.45));
#22468=CARTESIAN_POINT('',(118.2,19.15,31.45));
#22469=CARTESIAN_POINT('',(118.2,17.3,32.55));
#22470=CARTESIAN_POINT('',(118.2,17.3,31.45));
#22471=CARTESIAN_POINT('',(118.2,19.15,32.55));
#22472=CARTESIAN_POINT('Origin',(117.6,17.3,31.45));
#22473=CARTESIAN_POINT('',(117.6,16.7,31.45));
#22474=CARTESIAN_POINT('Origin',(117.6,17.3,31.45));
#22475=CARTESIAN_POINT('',(117.6,16.7,32.55));
#22476=CARTESIAN_POINT('',(117.6,16.7,31.45));
#22477=CARTESIAN_POINT('Origin',(117.6,17.3,32.55));
#22478=CARTESIAN_POINT('Origin',(112.4,16.7,31.45));
#22479=CARTESIAN_POINT('',(112.4,16.7,31.45));
#22480=CARTESIAN_POINT('',(108.7,16.7,31.45));
#22481=CARTESIAN_POINT('',(112.4,16.7,32.55));
#22482=CARTESIAN_POINT('',(112.4,16.7,31.45));
#22483=CARTESIAN_POINT('',(108.7,16.7,32.55));
#22484=CARTESIAN_POINT('Origin',(112.4,17.3,31.45));
#22485=CARTESIAN_POINT('Origin',(112.4,17.3,31.45));
#22486=CARTESIAN_POINT('Origin',(112.4,17.3,32.55));
#22487=CARTESIAN_POINT('Origin',(101.8,24.7,31.45));
#22488=CARTESIAN_POINT('',(101.8,24.7,31.45));
#22489=CARTESIAN_POINT('',(101.8,17.3,31.45));
#22490=CARTESIAN_POINT('',(101.8,22.85,31.45));
#22491=CARTESIAN_POINT('',(101.8,24.7,32.55));
#22492=CARTESIAN_POINT('',(101.8,24.7,31.45));
#22493=CARTESIAN_POINT('',(101.8,17.3,32.55));
#22494=CARTESIAN_POINT('',(101.8,22.85,32.55));
#22495=CARTESIAN_POINT('',(101.8,17.3,31.45));
#22496=CARTESIAN_POINT('Origin',(102.4,24.7,31.45));
#22497=CARTESIAN_POINT('',(102.4,25.3,31.45));
#22498=CARTESIAN_POINT('Origin',(102.4,24.7,31.45));
#22499=CARTESIAN_POINT('',(102.4,25.3,32.55));
#22500=CARTESIAN_POINT('',(102.4,25.3,31.45));
#22501=CARTESIAN_POINT('Origin',(102.4,24.7,32.55));
#22502=CARTESIAN_POINT('Origin',(107.6,25.3,31.45));
#22503=CARTESIAN_POINT('',(107.6,25.3,31.45));
#22504=CARTESIAN_POINT('',(106.3,25.3,31.45));
#22505=CARTESIAN_POINT('',(107.6,25.3,32.55));
#22506=CARTESIAN_POINT('',(107.6,25.3,31.45));
#22507=CARTESIAN_POINT('',(106.3,25.3,32.55));
#22508=CARTESIAN_POINT('Origin',(107.6,24.7,31.45));
#22509=CARTESIAN_POINT('',(108.2,24.7,31.45));
#22510=CARTESIAN_POINT('Origin',(107.6,24.7,31.45));
#22511=CARTESIAN_POINT('',(108.2,24.7,32.55));
#22512=CARTESIAN_POINT('',(108.2,24.7,31.45));
#22513=CARTESIAN_POINT('Origin',(107.6,24.7,32.55));
#22514=CARTESIAN_POINT('Origin',(108.2,17.3,31.45));
#22515=CARTESIAN_POINT('',(108.2,17.3,31.45));
#22516=CARTESIAN_POINT('',(108.2,19.15,31.45));
#22517=CARTESIAN_POINT('',(108.2,17.3,32.55));
#22518=CARTESIAN_POINT('',(108.2,17.3,31.45));
#22519=CARTESIAN_POINT('',(108.2,19.15,32.55));
#22520=CARTESIAN_POINT('Origin',(107.6,17.3,31.45));
#22521=CARTESIAN_POINT('',(107.6,16.7,31.45));
#22522=CARTESIAN_POINT('Origin',(107.6,17.3,31.45));
#22523=CARTESIAN_POINT('',(107.6,16.7,32.55));
#22524=CARTESIAN_POINT('',(107.6,16.7,31.45));
#22525=CARTESIAN_POINT('Origin',(107.6,17.3,32.55));
#22526=CARTESIAN_POINT('Origin',(102.4,16.7,31.45));
#22527=CARTESIAN_POINT('',(102.4,16.7,31.45));
#22528=CARTESIAN_POINT('',(103.7,16.7,31.45));
#22529=CARTESIAN_POINT('',(102.4,16.7,32.55));
#22530=CARTESIAN_POINT('',(102.4,16.7,31.45));
#22531=CARTESIAN_POINT('',(103.7,16.7,32.55));
#22532=CARTESIAN_POINT('Origin',(102.4,17.3,31.45));
#22533=CARTESIAN_POINT('Origin',(102.4,17.3,31.45));
#22534=CARTESIAN_POINT('Origin',(102.4,17.3,32.55));
#22535=CARTESIAN_POINT('Origin',(81.8,24.7,31.45));
#22536=CARTESIAN_POINT('',(81.8,24.7,31.45));
#22537=CARTESIAN_POINT('',(81.8,17.3,31.45));
#22538=CARTESIAN_POINT('',(81.8,22.85,31.45));
#22539=CARTESIAN_POINT('',(81.8,24.7,32.55));
#22540=CARTESIAN_POINT('',(81.8,24.7,31.45));
#22541=CARTESIAN_POINT('',(81.8,17.3,32.55));
#22542=CARTESIAN_POINT('',(81.8,22.85,32.55));
#22543=CARTESIAN_POINT('',(81.8,17.3,31.45));
#22544=CARTESIAN_POINT('Origin',(82.4,24.7,31.45));
#22545=CARTESIAN_POINT('',(82.4,25.3,31.45));
#22546=CARTESIAN_POINT('Origin',(82.4,24.7,31.45));
#22547=CARTESIAN_POINT('',(82.4,25.3,32.55));
#22548=CARTESIAN_POINT('',(82.4,25.3,31.45));
#22549=CARTESIAN_POINT('Origin',(82.4,24.7,32.55));
#22550=CARTESIAN_POINT('Origin',(87.6,25.3,31.45));
#22551=CARTESIAN_POINT('',(87.6,25.3,31.45));
#22552=CARTESIAN_POINT('',(96.3,25.3,31.45));
#22553=CARTESIAN_POINT('',(87.6,25.3,32.55));
#22554=CARTESIAN_POINT('',(87.6,25.3,31.45));
#22555=CARTESIAN_POINT('',(96.3,25.3,32.55));
#22556=CARTESIAN_POINT('Origin',(87.6,24.7,31.45));
#22557=CARTESIAN_POINT('',(88.2,24.7,31.45));
#22558=CARTESIAN_POINT('Origin',(87.6,24.7,31.45));
#22559=CARTESIAN_POINT('',(88.2,24.7,32.55));
#22560=CARTESIAN_POINT('',(88.2,24.7,31.45));
#22561=CARTESIAN_POINT('Origin',(87.6,24.7,32.55));
#22562=CARTESIAN_POINT('Origin',(88.2,17.3,31.45));
#22563=CARTESIAN_POINT('',(88.2,17.3,31.45));
#22564=CARTESIAN_POINT('',(88.2,19.15,31.45));
#22565=CARTESIAN_POINT('',(88.2,17.3,32.55));
#22566=CARTESIAN_POINT('',(88.2,17.3,31.45));
#22567=CARTESIAN_POINT('',(88.2,19.15,32.55));
#22568=CARTESIAN_POINT('Origin',(87.6,17.3,31.45));
#22569=CARTESIAN_POINT('',(87.6,16.7,31.45));
#22570=CARTESIAN_POINT('Origin',(87.6,17.3,31.45));
#22571=CARTESIAN_POINT('',(87.6,16.7,32.55));
#22572=CARTESIAN_POINT('',(87.6,16.7,31.45));
#22573=CARTESIAN_POINT('Origin',(87.6,17.3,32.55));
#22574=CARTESIAN_POINT('Origin',(82.4,16.7,31.45));
#22575=CARTESIAN_POINT('',(82.4,16.7,31.45));
#22576=CARTESIAN_POINT('',(93.7,16.7,31.45));
#22577=CARTESIAN_POINT('',(82.4,16.7,32.55));
#22578=CARTESIAN_POINT('',(82.4,16.7,31.45));
#22579=CARTESIAN_POINT('',(93.7,16.7,32.55));
#22580=CARTESIAN_POINT('Origin',(82.4,17.3,31.45));
#22581=CARTESIAN_POINT('Origin',(82.4,17.3,31.45));
#22582=CARTESIAN_POINT('Origin',(82.4,17.3,32.55));
#22583=CARTESIAN_POINT('Origin',(61.8,24.7,31.45));
#22584=CARTESIAN_POINT('',(61.8,24.7,31.45));
#22585=CARTESIAN_POINT('',(61.8,17.3,31.45));
#22586=CARTESIAN_POINT('',(61.8,22.85,31.45));
#22587=CARTESIAN_POINT('',(61.8,24.7,32.55));
#22588=CARTESIAN_POINT('',(61.8,24.7,31.45));
#22589=CARTESIAN_POINT('',(61.8,17.3,32.55));
#22590=CARTESIAN_POINT('',(61.8,22.85,32.55));
#22591=CARTESIAN_POINT('',(61.8,17.3,31.45));
#22592=CARTESIAN_POINT('Origin',(62.4,24.7,31.45));
#22593=CARTESIAN_POINT('',(62.4,25.3,31.45));
#22594=CARTESIAN_POINT('Origin',(62.4,24.7,31.45));
#22595=CARTESIAN_POINT('',(62.4,25.3,32.55));
#22596=CARTESIAN_POINT('',(62.4,25.3,31.45));
#22597=CARTESIAN_POINT('Origin',(62.4,24.7,32.55));
#22598=CARTESIAN_POINT('Origin',(67.6,25.3,31.45));
#22599=CARTESIAN_POINT('',(67.6,25.3,31.45));
#22600=CARTESIAN_POINT('',(86.3,25.3,31.45));
#22601=CARTESIAN_POINT('',(67.6,25.3,32.55));
#22602=CARTESIAN_POINT('',(67.6,25.3,31.45));
#22603=CARTESIAN_POINT('',(86.3,25.3,32.55));
#22604=CARTESIAN_POINT('Origin',(67.6,24.7,31.45));
#22605=CARTESIAN_POINT('',(68.2,24.7,31.45));
#22606=CARTESIAN_POINT('Origin',(67.6,24.7,31.45));
#22607=CARTESIAN_POINT('',(68.2,24.7,32.55));
#22608=CARTESIAN_POINT('',(68.2,24.7,31.45));
#22609=CARTESIAN_POINT('Origin',(67.6,24.7,32.55));
#22610=CARTESIAN_POINT('Origin',(68.2,17.3,31.45));
#22611=CARTESIAN_POINT('',(68.2,17.3,31.45));
#22612=CARTESIAN_POINT('',(68.2,19.15,31.45));
#22613=CARTESIAN_POINT('',(68.2,17.3,32.55));
#22614=CARTESIAN_POINT('',(68.2,17.3,31.45));
#22615=CARTESIAN_POINT('',(68.2,19.15,32.55));
#22616=CARTESIAN_POINT('Origin',(67.6,17.3,31.45));
#22617=CARTESIAN_POINT('',(67.6,16.7,31.45));
#22618=CARTESIAN_POINT('Origin',(67.6,17.3,31.45));
#22619=CARTESIAN_POINT('',(67.6,16.7,32.55));
#22620=CARTESIAN_POINT('',(67.6,16.7,31.45));
#22621=CARTESIAN_POINT('Origin',(67.6,17.3,32.55));
#22622=CARTESIAN_POINT('Origin',(62.4,16.7,31.45));
#22623=CARTESIAN_POINT('',(62.4,16.7,31.45));
#22624=CARTESIAN_POINT('',(83.7,16.7,31.45));
#22625=CARTESIAN_POINT('',(62.4,16.7,32.55));
#22626=CARTESIAN_POINT('',(62.4,16.7,31.45));
#22627=CARTESIAN_POINT('',(83.7,16.7,32.55));
#22628=CARTESIAN_POINT('Origin',(62.4,17.3,31.45));
#22629=CARTESIAN_POINT('Origin',(62.4,17.3,31.45));
#22630=CARTESIAN_POINT('Origin',(62.4,17.3,32.55));
#22631=CARTESIAN_POINT('Origin',(51.8,24.7,31.45));
#22632=CARTESIAN_POINT('',(51.8,24.7,31.45));
#22633=CARTESIAN_POINT('',(51.8,17.3,31.45));
#22634=CARTESIAN_POINT('',(51.8,22.85,31.45));
#22635=CARTESIAN_POINT('',(51.8,24.7,32.55));
#22636=CARTESIAN_POINT('',(51.8,24.7,31.45));
#22637=CARTESIAN_POINT('',(51.8,17.3,32.55));
#22638=CARTESIAN_POINT('',(51.8,22.85,32.55));
#22639=CARTESIAN_POINT('',(51.8,17.3,31.45));
#22640=CARTESIAN_POINT('Origin',(52.4,24.7,31.45));
#22641=CARTESIAN_POINT('',(52.4,25.3,31.45));
#22642=CARTESIAN_POINT('Origin',(52.4,24.7,31.45));
#22643=CARTESIAN_POINT('',(52.4,25.3,32.55));
#22644=CARTESIAN_POINT('',(52.4,25.3,31.45));
#22645=CARTESIAN_POINT('Origin',(52.4,24.7,32.55));
#22646=CARTESIAN_POINT('Origin',(57.6,25.3,31.45));
#22647=CARTESIAN_POINT('',(57.6,25.3,31.45));
#22648=CARTESIAN_POINT('',(81.3,25.3,31.45));
#22649=CARTESIAN_POINT('',(57.6,25.3,32.55));
#22650=CARTESIAN_POINT('',(57.6,25.3,31.45));
#22651=CARTESIAN_POINT('',(81.3,25.3,32.55));
#22652=CARTESIAN_POINT('Origin',(57.6,24.7,31.45));
#22653=CARTESIAN_POINT('',(58.2,24.7,31.45));
#22654=CARTESIAN_POINT('Origin',(57.6,24.7,31.45));
#22655=CARTESIAN_POINT('',(58.2,24.7,32.55));
#22656=CARTESIAN_POINT('',(58.2,24.7,31.45));
#22657=CARTESIAN_POINT('Origin',(57.6,24.7,32.55));
#22658=CARTESIAN_POINT('Origin',(58.2,17.3,31.45));
#22659=CARTESIAN_POINT('',(58.2,17.3,31.45));
#22660=CARTESIAN_POINT('',(58.2,19.15,31.45));
#22661=CARTESIAN_POINT('',(58.2,17.3,32.55));
#22662=CARTESIAN_POINT('',(58.2,17.3,31.45));
#22663=CARTESIAN_POINT('',(58.2,19.15,32.55));
#22664=CARTESIAN_POINT('Origin',(57.6,17.3,31.45));
#22665=CARTESIAN_POINT('',(57.6,16.7,31.45));
#22666=CARTESIAN_POINT('Origin',(57.6,17.3,31.45));
#22667=CARTESIAN_POINT('',(57.6,16.7,32.55));
#22668=CARTESIAN_POINT('',(57.6,16.7,31.45));
#22669=CARTESIAN_POINT('Origin',(57.6,17.3,32.55));
#22670=CARTESIAN_POINT('Origin',(52.4,16.7,31.45));
#22671=CARTESIAN_POINT('',(52.4,16.7,31.45));
#22672=CARTESIAN_POINT('',(78.7,16.7,31.45));
#22673=CARTESIAN_POINT('',(52.4,16.7,32.55));
#22674=CARTESIAN_POINT('',(52.4,16.7,31.45));
#22675=CARTESIAN_POINT('',(78.7,16.7,32.55));
#22676=CARTESIAN_POINT('Origin',(52.4,17.3,31.45));
#22677=CARTESIAN_POINT('Origin',(52.4,17.3,31.45));
#22678=CARTESIAN_POINT('Origin',(52.4,17.3,32.55));
#22679=CARTESIAN_POINT('Origin',(71.8,24.7,31.45));
#22680=CARTESIAN_POINT('',(71.8,24.7,31.45));
#22681=CARTESIAN_POINT('',(71.8,17.3,31.45));
#22682=CARTESIAN_POINT('',(71.8,22.85,31.45));
#22683=CARTESIAN_POINT('',(71.8,24.7,32.55));
#22684=CARTESIAN_POINT('',(71.8,24.7,31.45));
#22685=CARTESIAN_POINT('',(71.8,17.3,32.55));
#22686=CARTESIAN_POINT('',(71.8,22.85,32.55));
#22687=CARTESIAN_POINT('',(71.8,17.3,31.45));
#22688=CARTESIAN_POINT('Origin',(72.4,24.7,31.45));
#22689=CARTESIAN_POINT('',(72.4,25.3,31.45));
#22690=CARTESIAN_POINT('Origin',(72.4,24.7,31.45));
#22691=CARTESIAN_POINT('',(72.4,25.3,32.55));
#22692=CARTESIAN_POINT('',(72.4,25.3,31.45));
#22693=CARTESIAN_POINT('Origin',(72.4,24.7,32.55));
#22694=CARTESIAN_POINT('Origin',(77.6,25.3,31.45));
#22695=CARTESIAN_POINT('',(77.6,25.3,31.45));
#22696=CARTESIAN_POINT('',(91.3,25.3,31.45));
#22697=CARTESIAN_POINT('',(77.6,25.3,32.55));
#22698=CARTESIAN_POINT('',(77.6,25.3,31.45));
#22699=CARTESIAN_POINT('',(91.3,25.3,32.55));
#22700=CARTESIAN_POINT('Origin',(77.6,24.7,31.45));
#22701=CARTESIAN_POINT('',(78.2,24.7,31.45));
#22702=CARTESIAN_POINT('Origin',(77.6,24.7,31.45));
#22703=CARTESIAN_POINT('',(78.2,24.7,32.55));
#22704=CARTESIAN_POINT('',(78.2,24.7,31.45));
#22705=CARTESIAN_POINT('Origin',(77.6,24.7,32.55));
#22706=CARTESIAN_POINT('Origin',(78.2,17.3,31.45));
#22707=CARTESIAN_POINT('',(78.2,17.3,31.45));
#22708=CARTESIAN_POINT('',(78.2,19.15,31.45));
#22709=CARTESIAN_POINT('',(78.2,17.3,32.55));
#22710=CARTESIAN_POINT('',(78.2,17.3,31.45));
#22711=CARTESIAN_POINT('',(78.2,19.15,32.55));
#22712=CARTESIAN_POINT('Origin',(77.6,17.3,31.45));
#22713=CARTESIAN_POINT('',(77.6,16.7,31.45));
#22714=CARTESIAN_POINT('Origin',(77.6,17.3,31.45));
#22715=CARTESIAN_POINT('',(77.6,16.7,32.55));
#22716=CARTESIAN_POINT('',(77.6,16.7,31.45));
#22717=CARTESIAN_POINT('Origin',(77.6,17.3,32.55));
#22718=CARTESIAN_POINT('Origin',(72.4,16.7,31.45));
#22719=CARTESIAN_POINT('',(72.4,16.7,31.45));
#22720=CARTESIAN_POINT('',(88.7,16.7,31.45));
#22721=CARTESIAN_POINT('',(72.4,16.7,32.55));
#22722=CARTESIAN_POINT('',(72.4,16.7,31.45));
#22723=CARTESIAN_POINT('',(88.7,16.7,32.55));
#22724=CARTESIAN_POINT('Origin',(72.4,17.3,31.45));
#22725=CARTESIAN_POINT('Origin',(72.4,17.3,31.45));
#22726=CARTESIAN_POINT('Origin',(72.4,17.3,32.55));
#22727=CARTESIAN_POINT('Origin',(91.8,24.7,31.45));
#22728=CARTESIAN_POINT('',(91.8,24.7,31.45));
#22729=CARTESIAN_POINT('',(91.8,17.3,31.45));
#22730=CARTESIAN_POINT('',(91.8,22.85,31.45));
#22731=CARTESIAN_POINT('',(91.8,24.7,32.55));
#22732=CARTESIAN_POINT('',(91.8,24.7,31.45));
#22733=CARTESIAN_POINT('',(91.8,17.3,32.55));
#22734=CARTESIAN_POINT('',(91.8,22.85,32.55));
#22735=CARTESIAN_POINT('',(91.8,17.3,31.45));
#22736=CARTESIAN_POINT('Origin',(92.4,24.7,31.45));
#22737=CARTESIAN_POINT('',(92.4,25.3,31.45));
#22738=CARTESIAN_POINT('Origin',(92.4,24.7,31.45));
#22739=CARTESIAN_POINT('',(92.4,25.3,32.55));
#22740=CARTESIAN_POINT('',(92.4,25.3,31.45));
#22741=CARTESIAN_POINT('Origin',(92.4,24.7,32.55));
#22742=CARTESIAN_POINT('Origin',(97.6,25.3,31.45));
#22743=CARTESIAN_POINT('',(97.6,25.3,31.45));
#22744=CARTESIAN_POINT('',(101.3,25.3,31.45));
#22745=CARTESIAN_POINT('',(97.6,25.3,32.55));
#22746=CARTESIAN_POINT('',(97.6,25.3,31.45));
#22747=CARTESIAN_POINT('',(101.3,25.3,32.55));
#22748=CARTESIAN_POINT('Origin',(97.6,24.7,31.45));
#22749=CARTESIAN_POINT('',(98.2,24.7,31.45));
#22750=CARTESIAN_POINT('Origin',(97.6,24.7,31.45));
#22751=CARTESIAN_POINT('',(98.2,24.7,32.55));
#22752=CARTESIAN_POINT('',(98.2,24.7,31.45));
#22753=CARTESIAN_POINT('Origin',(97.6,24.7,32.55));
#22754=CARTESIAN_POINT('Origin',(98.2,17.3,31.45));
#22755=CARTESIAN_POINT('',(98.2,17.3,31.45));
#22756=CARTESIAN_POINT('',(98.2,19.15,31.45));
#22757=CARTESIAN_POINT('',(98.2,17.3,32.55));
#22758=CARTESIAN_POINT('',(98.2,17.3,31.45));
#22759=CARTESIAN_POINT('',(98.2,19.15,32.55));
#22760=CARTESIAN_POINT('Origin',(97.6,17.3,31.45));
#22761=CARTESIAN_POINT('',(97.6,16.7,31.45));
#22762=CARTESIAN_POINT('Origin',(97.6,17.3,31.45));
#22763=CARTESIAN_POINT('',(97.6,16.7,32.55));
#22764=CARTESIAN_POINT('',(97.6,16.7,31.45));
#22765=CARTESIAN_POINT('Origin',(97.6,17.3,32.55));
#22766=CARTESIAN_POINT('Origin',(92.4,16.7,31.45));
#22767=CARTESIAN_POINT('',(92.4,16.7,31.45));
#22768=CARTESIAN_POINT('',(98.7,16.7,31.45));
#22769=CARTESIAN_POINT('',(92.4,16.7,32.55));
#22770=CARTESIAN_POINT('',(92.4,16.7,31.45));
#22771=CARTESIAN_POINT('',(98.7,16.7,32.55));
#22772=CARTESIAN_POINT('Origin',(92.4,17.3,31.45));
#22773=CARTESIAN_POINT('Origin',(92.4,17.3,31.45));
#22774=CARTESIAN_POINT('Origin',(92.4,17.3,32.55));
#22775=CARTESIAN_POINT('Origin',(41.8,24.7,31.45));
#22776=CARTESIAN_POINT('',(41.8,24.7,31.45));
#22777=CARTESIAN_POINT('',(41.8,17.3,31.45));
#22778=CARTESIAN_POINT('',(41.8,22.85,31.45));
#22779=CARTESIAN_POINT('',(41.8,24.7,32.55));
#22780=CARTESIAN_POINT('',(41.8,24.7,31.45));
#22781=CARTESIAN_POINT('',(41.8,17.3,32.55));
#22782=CARTESIAN_POINT('',(41.8,22.85,32.55));
#22783=CARTESIAN_POINT('',(41.8,17.3,31.45));
#22784=CARTESIAN_POINT('Origin',(42.4,24.7,31.45));
#22785=CARTESIAN_POINT('',(42.4,25.3,31.45));
#22786=CARTESIAN_POINT('Origin',(42.4,24.7,31.45));
#22787=CARTESIAN_POINT('',(42.4,25.3,32.55));
#22788=CARTESIAN_POINT('',(42.4,25.3,31.45));
#22789=CARTESIAN_POINT('Origin',(42.4,24.7,32.55));
#22790=CARTESIAN_POINT('Origin',(47.6,25.3,31.45));
#22791=CARTESIAN_POINT('',(47.6,25.3,31.45));
#22792=CARTESIAN_POINT('',(76.3,25.3,31.45));
#22793=CARTESIAN_POINT('',(47.6,25.3,32.55));
#22794=CARTESIAN_POINT('',(47.6,25.3,31.45));
#22795=CARTESIAN_POINT('',(76.3,25.3,32.55));
#22796=CARTESIAN_POINT('Origin',(47.6,24.7,31.45));
#22797=CARTESIAN_POINT('',(48.2,24.7,31.45));
#22798=CARTESIAN_POINT('Origin',(47.6,24.7,31.45));
#22799=CARTESIAN_POINT('',(48.2,24.7,32.55));
#22800=CARTESIAN_POINT('',(48.2,24.7,31.45));
#22801=CARTESIAN_POINT('Origin',(47.6,24.7,32.55));
#22802=CARTESIAN_POINT('Origin',(48.2,17.3,31.45));
#22803=CARTESIAN_POINT('',(48.2,17.3,31.45));
#22804=CARTESIAN_POINT('',(48.2,19.15,31.45));
#22805=CARTESIAN_POINT('',(48.2,17.3,32.55));
#22806=CARTESIAN_POINT('',(48.2,17.3,31.45));
#22807=CARTESIAN_POINT('',(48.2,19.15,32.55));
#22808=CARTESIAN_POINT('Origin',(47.6,17.3,31.45));
#22809=CARTESIAN_POINT('',(47.6,16.7,31.45));
#22810=CARTESIAN_POINT('Origin',(47.6,17.3,31.45));
#22811=CARTESIAN_POINT('',(47.6,16.7,32.55));
#22812=CARTESIAN_POINT('',(47.6,16.7,31.45));
#22813=CARTESIAN_POINT('Origin',(47.6,17.3,32.55));
#22814=CARTESIAN_POINT('Origin',(42.4,16.7,31.45));
#22815=CARTESIAN_POINT('',(42.4,16.7,31.45));
#22816=CARTESIAN_POINT('',(73.7,16.7,31.45));
#22817=CARTESIAN_POINT('',(42.4,16.7,32.55));
#22818=CARTESIAN_POINT('',(42.4,16.7,31.45));
#22819=CARTESIAN_POINT('',(73.7,16.7,32.55));
#22820=CARTESIAN_POINT('Origin',(42.4,17.3,31.45));
#22821=CARTESIAN_POINT('Origin',(42.4,17.3,31.45));
#22822=CARTESIAN_POINT('Origin',(42.4,17.3,32.55));
#22823=CARTESIAN_POINT('Origin',(121.8,24.7,31.45));
#22824=CARTESIAN_POINT('',(121.8,24.7,31.45));
#22825=CARTESIAN_POINT('',(121.8,17.3,31.45));
#22826=CARTESIAN_POINT('',(121.8,22.85,31.45));
#22827=CARTESIAN_POINT('',(121.8,24.7,32.55));
#22828=CARTESIAN_POINT('',(121.8,24.7,31.45));
#22829=CARTESIAN_POINT('',(121.8,17.3,32.55));
#22830=CARTESIAN_POINT('',(121.8,22.85,32.55));
#22831=CARTESIAN_POINT('',(121.8,17.3,31.45));
#22832=CARTESIAN_POINT('Origin',(122.4,24.7,31.45));
#22833=CARTESIAN_POINT('',(122.4,25.3,31.45));
#22834=CARTESIAN_POINT('Origin',(122.4,24.7,31.45));
#22835=CARTESIAN_POINT('',(122.4,25.3,32.55));
#22836=CARTESIAN_POINT('',(122.4,25.3,31.45));
#22837=CARTESIAN_POINT('Origin',(122.4,24.7,32.55));
#22838=CARTESIAN_POINT('Origin',(127.6,25.3,31.45));
#22839=CARTESIAN_POINT('',(127.6,25.3,31.45));
#22840=CARTESIAN_POINT('',(116.3,25.3,31.45));
#22841=CARTESIAN_POINT('',(127.6,25.3,32.55));
#22842=CARTESIAN_POINT('',(127.6,25.3,31.45));
#22843=CARTESIAN_POINT('',(116.3,25.3,32.55));
#22844=CARTESIAN_POINT('Origin',(127.6,24.7,31.45));
#22845=CARTESIAN_POINT('',(128.2,24.7,31.45));
#22846=CARTESIAN_POINT('Origin',(127.6,24.7,31.45));
#22847=CARTESIAN_POINT('',(128.2,24.7,32.55));
#22848=CARTESIAN_POINT('',(128.2,24.7,31.45));
#22849=CARTESIAN_POINT('Origin',(127.6,24.7,32.55));
#22850=CARTESIAN_POINT('Origin',(128.2,17.3,31.45));
#22851=CARTESIAN_POINT('',(128.2,17.3,31.45));
#22852=CARTESIAN_POINT('',(128.2,19.15,31.45));
#22853=CARTESIAN_POINT('',(128.2,17.3,32.55));
#22854=CARTESIAN_POINT('',(128.2,17.3,31.45));
#22855=CARTESIAN_POINT('',(128.2,19.15,32.55));
#22856=CARTESIAN_POINT('Origin',(127.6,17.3,31.45));
#22857=CARTESIAN_POINT('',(127.6,16.7,31.45));
#22858=CARTESIAN_POINT('Origin',(127.6,17.3,31.45));
#22859=CARTESIAN_POINT('',(127.6,16.7,32.55));
#22860=CARTESIAN_POINT('',(127.6,16.7,31.45));
#22861=CARTESIAN_POINT('Origin',(127.6,17.3,32.55));
#22862=CARTESIAN_POINT('Origin',(122.4,16.7,31.45));
#22863=CARTESIAN_POINT('',(122.4,16.7,31.45));
#22864=CARTESIAN_POINT('',(113.7,16.7,31.45));
#22865=CARTESIAN_POINT('',(122.4,16.7,32.55));
#22866=CARTESIAN_POINT('',(122.4,16.7,31.45));
#22867=CARTESIAN_POINT('',(113.7,16.7,32.55));
#22868=CARTESIAN_POINT('Origin',(122.4,17.3,31.45));
#22869=CARTESIAN_POINT('Origin',(122.4,17.3,31.45));
#22870=CARTESIAN_POINT('Origin',(122.4,17.3,32.55));
#22871=CARTESIAN_POINT('Origin',(141.8,24.7,31.45));
#22872=CARTESIAN_POINT('',(141.8,24.7,31.45));
#22873=CARTESIAN_POINT('',(141.8,17.3,31.45));
#22874=CARTESIAN_POINT('',(141.8,22.85,31.45));
#22875=CARTESIAN_POINT('',(141.8,24.7,32.55));
#22876=CARTESIAN_POINT('',(141.8,24.7,31.45));
#22877=CARTESIAN_POINT('',(141.8,17.3,32.55));
#22878=CARTESIAN_POINT('',(141.8,22.85,32.55));
#22879=CARTESIAN_POINT('',(141.8,17.3,31.45));
#22880=CARTESIAN_POINT('Origin',(142.4,24.7,31.45));
#22881=CARTESIAN_POINT('',(142.4,25.3,31.45));
#22882=CARTESIAN_POINT('Origin',(142.4,24.7,31.45));
#22883=CARTESIAN_POINT('',(142.4,25.3,32.55));
#22884=CARTESIAN_POINT('',(142.4,25.3,31.45));
#22885=CARTESIAN_POINT('Origin',(142.4,24.7,32.55));
#22886=CARTESIAN_POINT('Origin',(147.6,25.3,31.45));
#22887=CARTESIAN_POINT('',(147.6,25.3,31.45));
#22888=CARTESIAN_POINT('',(126.3,25.3,31.45));
#22889=CARTESIAN_POINT('',(147.6,25.3,32.55));
#22890=CARTESIAN_POINT('',(147.6,25.3,31.45));
#22891=CARTESIAN_POINT('',(126.3,25.3,32.55));
#22892=CARTESIAN_POINT('Origin',(147.6,24.7,31.45));
#22893=CARTESIAN_POINT('',(148.2,24.7,31.45));
#22894=CARTESIAN_POINT('Origin',(147.6,24.7,31.45));
#22895=CARTESIAN_POINT('',(148.2,24.7,32.55));
#22896=CARTESIAN_POINT('',(148.2,24.7,31.45));
#22897=CARTESIAN_POINT('Origin',(147.6,24.7,32.55));
#22898=CARTESIAN_POINT('Origin',(148.2,17.3,31.45));
#22899=CARTESIAN_POINT('',(148.2,17.3,31.45));
#22900=CARTESIAN_POINT('',(148.2,19.15,31.45));
#22901=CARTESIAN_POINT('',(148.2,17.3,32.55));
#22902=CARTESIAN_POINT('',(148.2,17.3,31.45));
#22903=CARTESIAN_POINT('',(148.2,19.15,32.55));
#22904=CARTESIAN_POINT('Origin',(147.6,17.3,31.45));
#22905=CARTESIAN_POINT('',(147.6,16.7,31.45));
#22906=CARTESIAN_POINT('Origin',(147.6,17.3,31.45));
#22907=CARTESIAN_POINT('',(147.6,16.7,32.55));
#22908=CARTESIAN_POINT('',(147.6,16.7,31.45));
#22909=CARTESIAN_POINT('Origin',(147.6,17.3,32.55));
#22910=CARTESIAN_POINT('Origin',(142.4,16.7,31.45));
#22911=CARTESIAN_POINT('',(142.4,16.7,31.45));
#22912=CARTESIAN_POINT('',(123.7,16.7,31.45));
#22913=CARTESIAN_POINT('',(142.4,16.7,32.55));
#22914=CARTESIAN_POINT('',(142.4,16.7,31.45));
#22915=CARTESIAN_POINT('',(123.7,16.7,32.55));
#22916=CARTESIAN_POINT('Origin',(142.4,17.3,31.45));
#22917=CARTESIAN_POINT('Origin',(142.4,17.3,31.45));
#22918=CARTESIAN_POINT('Origin',(142.4,17.3,32.55));
#22919=CARTESIAN_POINT('Origin',(161.8,24.7,31.45));
#22920=CARTESIAN_POINT('',(161.8,24.7,31.45));
#22921=CARTESIAN_POINT('',(161.8,17.3,31.45));
#22922=CARTESIAN_POINT('',(161.8,22.85,31.45));
#22923=CARTESIAN_POINT('',(161.8,24.7,32.55));
#22924=CARTESIAN_POINT('',(161.8,24.7,31.45));
#22925=CARTESIAN_POINT('',(161.8,17.3,32.55));
#22926=CARTESIAN_POINT('',(161.8,22.85,32.55));
#22927=CARTESIAN_POINT('',(161.8,17.3,31.45));
#22928=CARTESIAN_POINT('Origin',(162.4,24.7,31.45));
#22929=CARTESIAN_POINT('',(162.4,25.3,31.45));
#22930=CARTESIAN_POINT('Origin',(162.4,24.7,31.45));
#22931=CARTESIAN_POINT('',(162.4,25.3,32.55));
#22932=CARTESIAN_POINT('',(162.4,25.3,31.45));
#22933=CARTESIAN_POINT('Origin',(162.4,24.7,32.55));
#22934=CARTESIAN_POINT('Origin',(167.6,25.3,31.45));
#22935=CARTESIAN_POINT('',(167.6,25.3,31.45));
#22936=CARTESIAN_POINT('',(136.3,25.3,31.45));
#22937=CARTESIAN_POINT('',(167.6,25.3,32.55));
#22938=CARTESIAN_POINT('',(167.6,25.3,31.45));
#22939=CARTESIAN_POINT('',(136.3,25.3,32.55));
#22940=CARTESIAN_POINT('Origin',(167.6,24.7,31.45));
#22941=CARTESIAN_POINT('',(168.2,24.7,31.45));
#22942=CARTESIAN_POINT('Origin',(167.6,24.7,31.45));
#22943=CARTESIAN_POINT('',(168.2,24.7,32.55));
#22944=CARTESIAN_POINT('',(168.2,24.7,31.45));
#22945=CARTESIAN_POINT('Origin',(167.6,24.7,32.55));
#22946=CARTESIAN_POINT('Origin',(168.2,17.3,31.45));
#22947=CARTESIAN_POINT('',(168.2,17.3,31.45));
#22948=CARTESIAN_POINT('',(168.2,19.15,31.45));
#22949=CARTESIAN_POINT('',(168.2,17.3,32.55));
#22950=CARTESIAN_POINT('',(168.2,17.3,31.45));
#22951=CARTESIAN_POINT('',(168.2,19.15,32.55));
#22952=CARTESIAN_POINT('Origin',(167.6,17.3,31.45));
#22953=CARTESIAN_POINT('',(167.6,16.7,31.45));
#22954=CARTESIAN_POINT('Origin',(167.6,17.3,31.45));
#22955=CARTESIAN_POINT('',(167.6,16.7,32.55));
#22956=CARTESIAN_POINT('',(167.6,16.7,31.45));
#22957=CARTESIAN_POINT('Origin',(167.6,17.3,32.55));
#22958=CARTESIAN_POINT('Origin',(162.4,16.7,31.45));
#22959=CARTESIAN_POINT('',(162.4,16.7,31.45));
#22960=CARTESIAN_POINT('',(133.7,16.7,31.45));
#22961=CARTESIAN_POINT('',(162.4,16.7,32.55));
#22962=CARTESIAN_POINT('',(162.4,16.7,31.45));
#22963=CARTESIAN_POINT('',(133.7,16.7,32.55));
#22964=CARTESIAN_POINT('Origin',(162.4,17.3,31.45));
#22965=CARTESIAN_POINT('Origin',(162.4,17.3,31.45));
#22966=CARTESIAN_POINT('Origin',(162.4,17.3,32.55));
#22967=CARTESIAN_POINT('Origin',(39.,32.,31.45));
#22968=CARTESIAN_POINT('',(39.,32.,31.45));
#22969=CARTESIAN_POINT('',(39.,10.,31.45));
#22970=CARTESIAN_POINT('',(39.,32.,31.45));
#22971=CARTESIAN_POINT('',(39.,10.,32.55));
#22972=CARTESIAN_POINT('',(39.,10.,31.45));
#22973=CARTESIAN_POINT('',(39.,32.,32.55));
#22974=CARTESIAN_POINT('',(39.,32.,32.55));
#22975=CARTESIAN_POINT('',(39.,32.,31.45));
#22976=CARTESIAN_POINT('Origin',(40.,32.,31.45));
#22977=CARTESIAN_POINT('',(40.,33.,31.45));
#22978=CARTESIAN_POINT('Origin',(40.,32.,31.45));
#22979=CARTESIAN_POINT('',(40.,33.,32.55));
#22980=CARTESIAN_POINT('Origin',(40.,32.,32.55));
#22981=CARTESIAN_POINT('',(40.,33.,31.45));
#22982=CARTESIAN_POINT('Origin',(170.,33.,31.45));
#22983=CARTESIAN_POINT('',(170.,33.,31.45));
#22984=CARTESIAN_POINT('',(170.,33.,31.45));
#22985=CARTESIAN_POINT('',(170.,33.,32.55));
#22986=CARTESIAN_POINT('',(170.,33.,32.55));
#22987=CARTESIAN_POINT('',(170.,33.,31.45));
#22988=CARTESIAN_POINT('Origin',(170.,32.,31.45));
#22989=CARTESIAN_POINT('',(171.,32.,31.45));
#22990=CARTESIAN_POINT('Origin',(170.,32.,31.45));
#22991=CARTESIAN_POINT('',(171.,32.,32.55));
#22992=CARTESIAN_POINT('Origin',(170.,32.,32.55));
#22993=CARTESIAN_POINT('',(171.,32.,31.45));
#22994=CARTESIAN_POINT('Origin',(171.,10.,31.45));
#22995=CARTESIAN_POINT('',(171.,10.,31.45));
#22996=CARTESIAN_POINT('',(171.,10.,31.45));
#22997=CARTESIAN_POINT('',(171.,10.,32.55));
#22998=CARTESIAN_POINT('',(171.,10.,32.55));
#22999=CARTESIAN_POINT('',(171.,10.,31.45));
#23000=CARTESIAN_POINT('Origin',(170.,10.,31.45));
#23001=CARTESIAN_POINT('',(170.,9.,31.45));
#23002=CARTESIAN_POINT('Origin',(170.,10.,31.45));
#23003=CARTESIAN_POINT('',(170.,9.,32.55));
#23004=CARTESIAN_POINT('Origin',(170.,10.,32.55));
#23005=CARTESIAN_POINT('',(170.,9.,31.45));
#23006=CARTESIAN_POINT('Origin',(40.,9.,31.45));
#23007=CARTESIAN_POINT('',(40.,9.,31.45));
#23008=CARTESIAN_POINT('',(40.,9.,31.45));
#23009=CARTESIAN_POINT('',(40.,9.,32.55));
#23010=CARTESIAN_POINT('',(40.,9.,32.55));
#23011=CARTESIAN_POINT('',(40.,9.,31.45));
#23012=CARTESIAN_POINT('Origin',(40.,10.,31.45));
#23013=CARTESIAN_POINT('Origin',(40.,10.,31.45));
#23014=CARTESIAN_POINT('Origin',(40.,10.,32.55));
#23015=CARTESIAN_POINT('Origin',(105.,21.,32.55));
#23016=CARTESIAN_POINT('Origin',(105.,21.,31.45));
#23017=CARTESIAN_POINT('',(0.,0.,0.));
#23018=CARTESIAN_POINT('Origin',(47.7,23.8,32.));
#23019=CARTESIAN_POINT('',(42.3,23.8,32.));
#23020=CARTESIAN_POINT('Origin',(45.,23.8,32.));
#23021=CARTESIAN_POINT('Origin',(45.,23.65,32.));
#23022=CARTESIAN_POINT('',(42.,23.5,32.));
#23023=CARTESIAN_POINT('Origin',(45.,23.5,32.));
#23024=CARTESIAN_POINT('',(42.15,23.65,32.));
#23025=CARTESIAN_POINT('Origin',(45.,21.,32.));
#23026=CARTESIAN_POINT('',(42.,18.5,32.));
#23027=CARTESIAN_POINT('Origin',(45.,18.5,32.));
#23028=CARTESIAN_POINT('',(42.,21.,32.));
#23029=CARTESIAN_POINT('Origin',(45.,18.35,32.));
#23030=CARTESIAN_POINT('',(42.3,18.2,32.));
#23031=CARTESIAN_POINT('',(42.15,18.35,32.));
#23032=CARTESIAN_POINT('Origin',(45.,18.2,32.));
#23033=CARTESIAN_POINT('Origin',(45.,18.2,32.));
#23034=CARTESIAN_POINT('',(0.,0.,0.));
#23035=CARTESIAN_POINT('Origin',(55.,21.,6.22095488139522));
#23036=CARTESIAN_POINT('',(55.1644483595783,22.9879598334805,8.16850613376992));
#23037=CARTESIAN_POINT('',(55.1644483516311,22.987959834138,8.01046478735112));
#23038=CARTESIAN_POINT('',(55.1644483516311,22.987959834138,6.22095488139522));
#23039=CARTESIAN_POINT('',(53.8619125385576,19.3617739799992,7.7));
#23040=CARTESIAN_POINT('Ctrl Pts',(55.1644483595783,22.9879598334805,8.16850613376992));
#23041=CARTESIAN_POINT('Ctrl Pts',(55.1739112702763,22.9871770409337,8.16795475044047));
#23042=CARTESIAN_POINT('Ctrl Pts',(55.1833696088008,22.9863265975055,8.16740313133717));
#23043=CARTESIAN_POINT('Ctrl Pts',(55.3237705246029,22.9726908763678,8.1592036975142));
#23044=CARTESIAN_POINT('Ctrl Pts',(55.4531201253634,22.9470521773363,8.15147670177632));
#23045=CARTESIAN_POINT('Ctrl Pts',(55.5938213859521,22.9043748946883,8.14234975210098));
#23046=CARTESIAN_POINT('Ctrl Pts',(55.6085936065288,22.8997056032264,8.14138272182667));
#23047=CARTESIAN_POINT('Ctrl Pts',(55.6324693111573,22.8918517677942,8.139804738193));
#23048=CARTESIAN_POINT('Ctrl Pts',(55.6416068997965,22.888772384845,8.13919722286266));
#23049=CARTESIAN_POINT('Ctrl Pts',(55.6578308337942,22.8831735755404,8.1381119927678));
#23050=CARTESIAN_POINT('Ctrl Pts',(55.6649259800132,22.8806800791425,8.13763514035216));
#23051=CARTESIAN_POINT('Ctrl Pts',(55.6798501285734,22.8753401715625,8.13662727724571));
#23052=CARTESIAN_POINT('Ctrl Pts',(55.6876757231185,22.8724847269786,8.13609597461454));
#23053=CARTESIAN_POINT('Ctrl Pts',(55.7083667015217,22.8647876918322,8.13468359012937));
#23054=CARTESIAN_POINT('Ctrl Pts',(55.7212001366586,22.8598620558134,8.13379972514799));
#23055=CARTESIAN_POINT('Ctrl Pts',(55.7820172652065,22.8357955597389,8.12957288800204));
#23056=CARTESIAN_POINT('Ctrl Pts',(55.8292925494817,22.8149295845626,8.12617250592043));
#23057=CARTESIAN_POINT('Ctrl Pts',(56.0330419639254,22.7153769234046,8.11099466761143));
#23058=CARTESIAN_POINT('Ctrl Pts',(56.1795621610039,22.6181191419544,8.09859647551919));
#23059=CARTESIAN_POINT('Ctrl Pts',(56.3221210645677,22.4937279297629,8.08555728451026));
#23060=CARTESIAN_POINT('Ctrl Pts',(56.3326694864003,22.4843245235456,8.08458654169387));
#23061=CARTESIAN_POINT('Ctrl Pts',(56.3804326360051,22.4408263606657,8.08016670917425));
#23062=CARTESIAN_POINT('Ctrl Pts',(56.416448451004,22.4054357351974,8.07676506186341));
#23063=CARTESIAN_POINT('Ctrl Pts',(56.4570253807462,22.362416797938,8.0728883373071));
#23064=CARTESIAN_POINT('Ctrl Pts',(56.462923946461,22.3560811276617,8.0723236423558));
#23065=CARTESIAN_POINT('Ctrl Pts',(56.4724145707644,22.3457532199429,8.07141348893154));
#23066=CARTESIAN_POINT('Ctrl Pts',(56.4760320040888,22.3417846033275,8.07106619941156));
#23067=CARTESIAN_POINT('Ctrl Pts',(56.4824368498612,22.3347007237273,8.07045071087391));
#23068=CARTESIAN_POINT('Ctrl Pts',(56.4852305607753,22.331591235476,8.07018204132472));
#23069=CARTESIAN_POINT('Ctrl Pts',(56.4912384529693,22.3248618314058,8.06960385814169));
#23070=CARTESIAN_POINT('Ctrl Pts',(56.4944492435359,22.3212389850583,8.06929459705603));
#23071=CARTESIAN_POINT('Ctrl Pts',(56.5034042461198,22.3110603373111,8.06843119675549));
#23072=CARTESIAN_POINT('Ctrl Pts',(56.5091188088655,22.3044784255482,8.06787922427727));
#23073=CARTESIAN_POINT('Ctrl Pts',(56.5431075755179,22.2648085964654,8.06458868855021));
#23074=CARTESIAN_POINT('Ctrl Pts',(56.5703381863521,22.2308372769387,8.06192074409987));
#23075=CARTESIAN_POINT('Ctrl Pts',(56.7338394295454,22.0125934054582,8.04550169557243));
#23076=CARTESIAN_POINT('Ctrl Pts',(56.8386154691083,21.8068819901909,8.03292315964913));
#23077=CARTESIAN_POINT('Ctrl Pts',(56.914070568179,21.5622110722724,8.01720752420272));
#23078=CARTESIAN_POINT('Ctrl Pts',(56.9214590319891,21.5364163595988,8.01554525244227));
#23079=CARTESIAN_POINT('Ctrl Pts',(56.9311627754301,21.4997608253042,8.01317197072088));
#23080=CARTESIAN_POINT('Ctrl Pts',(56.9339113127624,21.4890169466225,8.01247502441956));
#23081=CARTESIAN_POINT('Ctrl Pts',(56.9382344688724,21.4715112919375,8.01133706496191));
#23082=CARTESIAN_POINT('Ctrl Pts',(56.9398636507752,21.4647631323103,8.01089782654406));
#23083=CARTESIAN_POINT('Ctrl Pts',(56.9432045045168,21.4506014921009,8.00997478172884));
#23084=CARTESIAN_POINT('Ctrl Pts',(56.9449090490337,21.4431864612008,8.00949075318005));
#23085=CARTESIAN_POINT('Ctrl Pts',(56.948874412525,21.4254729776759,8.00833266945935));
#23086=CARTESIAN_POINT('Ctrl Pts',(56.9510960636413,21.4151660798481,8.00765736543105));
#23087=CARTESIAN_POINT('Ctrl Pts',(56.9583849172293,21.3799996627178,8.0053480608139));
#23088=CARTESIAN_POINT('Ctrl Pts',(56.9630593468725,21.3550621484496,8.00370157877714));
#23089=CARTESIAN_POINT('Ctrl Pts',(56.973140202337,21.2949741626493,7.99971130837033));
#23090=CARTESIAN_POINT('Ctrl Pts',(56.9780845687087,21.2597560258546,7.99735372741819));
#23091=CARTESIAN_POINT('Ctrl Pts',(57.0041004668181,21.0299892098894,7.98184970289821));
#23092=CARTESIAN_POINT('Ctrl Pts',(56.9973847445597,20.833415029745,7.96786928123027));
#23093=CARTESIAN_POINT('Ctrl Pts',(56.954586373688,20.5995026971139,7.95168749153061));
#23094=CARTESIAN_POINT('Ctrl Pts',(56.9456821482064,20.5582675526637,7.94885899209389));
#23095=CARTESIAN_POINT('Ctrl Pts',(56.9334936132035,20.5093910231311,7.94555921473854));
#23096=CARTESIAN_POINT('Ctrl Pts',(56.9314616967622,20.5014516673566,7.94502489923333));
#23097=CARTESIAN_POINT('Ctrl Pts',(56.9280566843323,20.4884805147866,7.9441549701788));
#23098=CARTESIAN_POINT('Ctrl Pts',(56.9267127048315,20.4834412750703,7.94381775601036));
#23099=CARTESIAN_POINT('Ctrl Pts',(56.9242574603283,20.4743782601909,7.94321270415758));
#23100=CARTESIAN_POINT('Ctrl Pts',(56.9231533304931,20.4703527069196,7.94294446972559));
#23101=CARTESIAN_POINT('Ctrl Pts',(56.9207027059227,20.4615266634482,7.94235747818033));
#23102=CARTESIAN_POINT('Ctrl Pts',(56.9193508503805,20.456727754098,7.94203903516486));
#23103=CARTESIAN_POINT('Ctrl Pts',(56.9154386730893,20.4430369206054,7.94113246439344));
#23104=CARTESIAN_POINT('Ctrl Pts',(56.9128344135364,20.43415753392,7.94054680931333));
#23105=CARTESIAN_POINT('Ctrl Pts',(56.8947940804951,20.3741960626433,7.93660563219028));
#23106=CARTESIAN_POINT('Ctrl Pts',(56.8773738696665,20.3237281313764,7.93335567538186));
#23107=CARTESIAN_POINT('Ctrl Pts',(56.7931413458539,20.1081593162929,7.91952579157411));
#23108=CARTESIAN_POINT('Ctrl Pts',(56.7064177778546,19.9517243446332,7.90955307986865));
#23109=CARTESIAN_POINT('Ctrl Pts',(56.564692136171,19.7613405832537,7.89534959861422));
#23110=CARTESIAN_POINT('Ctrl Pts',(56.5272122204425,19.7154142871462,7.89174323958466));
#23111=CARTESIAN_POINT('Ctrl Pts',(56.4778621090287,19.6601599609527,7.88713066327911));
#23112=CARTESIAN_POINT('Ctrl Pts',(56.467854701384,19.6492038271897,7.88620186051999));
#23113=CARTESIAN_POINT('Ctrl Pts',(56.4518053374027,19.6320219079677,7.88472198348949));
#23114=CARTESIAN_POINT('Ctrl Pts',(56.4458432700389,19.6257219958655,7.88417429990159));
#23115=CARTESIAN_POINT('Ctrl Pts',(56.4346491001832,19.6140469757009,7.88314969914366));
#23116=CARTESIAN_POINT('Ctrl Pts',(56.4294273823341,19.608662089085,7.88267323428618));
#23117=CARTESIAN_POINT('Ctrl Pts',(56.4177412857351,19.5967460486405,7.8816101074328));
#23118=CARTESIAN_POINT('Ctrl Pts',(56.4112619283098,19.5902298874123,7.88102279686199));
#23119=CARTESIAN_POINT('Ctrl Pts',(56.3921948510716,19.5713176811365,7.87930054058841));
#23120=CARTESIAN_POINT('Ctrl Pts',(56.3794874573028,19.5590440695089,7.8781603180321));
#23121=CARTESIAN_POINT('Ctrl Pts',(56.3503498330901,19.5316397885375,7.87556210552738));
#23122=CARTESIAN_POINT('Ctrl Pts',(56.3338253477606,19.5166132473141,7.8740999487099));
#23123=CARTESIAN_POINT('Ctrl Pts',(56.2787795574664,19.4682208556013,7.86926488891193));
#23124=CARTESIAN_POINT('Ctrl Pts',(56.2392341076601,19.4360554299076,7.86584641114681));
#23125=CARTESIAN_POINT('Ctrl Pts',(56.0973780387822,19.3294334807549,7.85377940760683));
#23126=CARTESIAN_POINT('Ctrl Pts',(55.989256610758,19.263222041386,7.84489643527489));
#23127=CARTESIAN_POINT('Ctrl Pts',(55.8022674540353,19.171870617062,7.83046817173561));
#23128=CARTESIAN_POINT('Ctrl Pts',(55.7267881096822,19.1405720628331,7.82487654362709));
#23129=CARTESIAN_POINT('Ctrl Pts',(55.6398027104851,19.1106119189392,7.81883720863747));
#23130=CARTESIAN_POINT('Ctrl Pts',(55.6299839383764,19.1073153782186,7.81816119356792));
#23131=CARTESIAN_POINT('Ctrl Pts',(55.6151402886258,19.1024601042568,7.81714824743538));
#23132=CARTESIAN_POINT('Ctrl Pts',(55.6101343707833,19.1008445872599,7.81680817867411));
#23133=CARTESIAN_POINT('Ctrl Pts',(55.6011501264652,19.097984368332,7.81620067919868));
#23134=CARTESIAN_POINT('Ctrl Pts',(55.5971743053158,19.0967323395754,7.81593283807526));
#23135=CARTESIAN_POINT('Ctrl Pts',(55.593161552592,19.0954824925416,7.81566350183841));
#23136=CARTESIAN_POINT('Ctrl Pts',(55.5931286308482,19.095472239384,7.81566129219574));
#23137=CARTESIAN_POINT('Ctrl Pts',(55.5930639609698,19.0954521004174,7.81565695181235));
#23138=CARTESIAN_POINT('Ctrl Pts',(55.5930322125785,19.0954422144629,7.81565482104972));
#23139=CARTESIAN_POINT('Ctrl Pts',(55.5929698361398,19.0954227931225,7.81565063483763));
#23140=CARTESIAN_POINT('Ctrl Pts',(55.5929392083847,19.0954132577672,7.81564857940348));
#23141=CARTESIAN_POINT('Ctrl Pts',(55.5928790246036,19.0953945223109,7.81564454057301));
#23142=CARTESIAN_POINT('Ctrl Pts',(55.5928494683373,19.0953853220795,7.81564255715656));
#23143=CARTESIAN_POINT('Ctrl Pts',(55.5927913806998,19.0953672421275,7.81563865920682));
#23144=CARTESIAN_POINT('Ctrl Pts',(55.592762849287,19.0953583623426,7.81563674466705));
#23145=CARTESIAN_POINT('Ctrl Pts',(55.5927067670439,19.0953409093402,7.81563298148622));
#23146=CARTESIAN_POINT('Ctrl Pts',(55.5926792163658,19.0953323361225,7.81563113285198));
#23147=CARTESIAN_POINT('Ctrl Pts',(55.5926250538063,19.0953154831107,7.81562749866834));
#23148=CARTESIAN_POINT('Ctrl Pts',(55.5925984421096,19.0953072033301,7.81562571312819));
#23149=CARTESIAN_POINT('Ctrl Pts',(55.5925461183382,19.095290924874,7.81562220249494));
#23150=CARTESIAN_POINT('Ctrl Pts',(55.5925204062322,19.0952829261479,7.81562047739684));
#23151=CARTESIAN_POINT('Ctrl Pts',(55.592469844534,19.0952671981364,7.81561708514935));
#23152=CARTESIAN_POINT('Ctrl Pts',(55.5924449948286,19.095259468778,7.81561541798968));
#23153=CARTESIAN_POINT('Ctrl Pts',(55.5923961217554,19.0952442681377,7.81561213918404));
#23154=CARTESIAN_POINT('Ctrl Pts',(55.5923720986674,19.095236796908,7.81561052755435));
#23155=CARTESIAN_POINT('Ctrl Pts',(55.5923248464771,19.0952221023601,7.81560735763085));
#23156=CARTESIAN_POINT('Ctrl Pts',(55.59230161689,19.0952148788587,7.81560579930222));
#23157=CARTESIAN_POINT('Ctrl Pts',(55.5922559190593,19.0952006695211,7.81560273378424));
#23158=CARTESIAN_POINT('Ctrl Pts',(55.5922334509298,19.0951936836903,7.8156012266004));
#23159=CARTESIAN_POINT('Ctrl Pts',(55.5921892456743,19.0951799401713,7.81559826133038));
#23160=CARTESIAN_POINT('Ctrl Pts',(55.5921675087154,19.0951731825071,7.81559680325341));
#23161=CARTESIAN_POINT('Ctrl Pts',(55.5921199766948,19.0951584064735,7.81559361495279));
#23162=CARTESIAN_POINT('Ctrl Pts',(55.592094181714,19.0951503882957,7.81559188474645));
#23163=CARTESIAN_POINT('Ctrl Pts',(55.5920427738835,19.0951344096993,7.815588436632));
#23164=CARTESIAN_POINT('Ctrl Pts',(55.5920171608995,19.0951264492309,7.81558671871432));
#23165=CARTESIAN_POINT('Ctrl Pts',(55.5919661138578,19.095110585033,7.81558329496049));
#23166=CARTESIAN_POINT('Ctrl Pts',(55.5919406797052,19.0951026812661,7.81558158911742));
#23167=CARTESIAN_POINT('Ctrl Pts',(55.5918899863674,19.0950869292176,7.8155781892456));
#23168=CARTESIAN_POINT('Ctrl Pts',(55.5918647275076,19.0950790810294,7.81557649523814));
#23169=CARTESIAN_POINT('Ctrl Pts',(55.59181438236,19.0950634393708,7.81557311887522));
#23170=CARTESIAN_POINT('Ctrl Pts',(55.5917892958867,19.0950556458353,7.81557143650681));
#23171=CARTESIAN_POINT('Ctrl Pts',(55.5917392920433,19.0950401123822,7.81556808318776));
#23172=CARTESIAN_POINT('Ctrl Pts',(55.5917143747504,19.0950323724812,7.81556641224178));
#23173=CARTESIAN_POINT('Ctrl Pts',(55.5868173968984,19.0935113605995,7.8152380299307));
#23174=CARTESIAN_POINT('Ctrl Pts',(55.581939485181,19.0920167646392,7.81491238772519));
#23175=CARTESIAN_POINT('Ctrl Pts',(55.5676795705694,19.087707289372,7.81396453357938));
#23176=CARTESIAN_POINT('Ctrl Pts',(55.5582823467525,19.0849427328924,7.8133450925289));
#23177=CARTESIAN_POINT('Ctrl Pts',(55.4871434054314,19.0645826143466,7.80869225079019));
#23178=CARTESIAN_POINT('Ctrl Pts',(55.4245982557927,19.0499058409691,7.80480788208925));
#23179=CARTESIAN_POINT('Ctrl Pts',(55.2234155882325,19.0128380098621,7.79265332231242));
#23180=CARTESIAN_POINT('Ctrl Pts',(55.0830832774369,19.0020442739689,7.78465341362658));
#23181=CARTESIAN_POINT('Ctrl Pts',(54.8684453297137,19.0082041953005,7.77190082410308));
#23182=CARTESIAN_POINT('Ctrl Pts',(54.7942994120393,19.0144918453275,7.76740648100607));
#23183=CARTESIAN_POINT('Ctrl Pts',(54.7063103746654,19.0269352108482,7.76188072368881));
#23184=CARTESIAN_POINT('Ctrl Pts',(54.6919609369275,19.0291245151652,7.76097351206504));
#23185=CARTESIAN_POINT('Ctrl Pts',(54.6683533421166,19.0329904541369,7.7594703781756));
#23186=CARTESIAN_POINT('Ctrl Pts',(54.6590807275695,19.0345763550609,7.75887727161705));
#23187=CARTESIAN_POINT('Ctrl Pts',(54.6423571214046,19.03755851135,7.7578025333055));
#23188=CARTESIAN_POINT('Ctrl Pts',(54.6349021715328,19.0389317711813,7.75732162766313));
#23189=CARTESIAN_POINT('Ctrl Pts',(54.6189487297594,19.0419646404841,7.75628852211697));
#23190=CARTESIAN_POINT('Ctrl Pts',(54.6104528786401,19.0436371563374,7.75573592648535));
#23191=CARTESIAN_POINT('Ctrl Pts',(54.587330318173,19.0483457140913,7.75422520699252));
#23192=CARTESIAN_POINT('Ctrl Pts',(54.5727266259799,19.0514907847362,7.75326367494978));
#23193=CARTESIAN_POINT('Ctrl Pts',(54.4937166405304,19.0694374055787,7.74802016063897));
#23194=CARTESIAN_POINT('Ctrl Pts',(54.4300474570642,19.0872670825043,7.74364307411907));
#23195=CARTESIAN_POINT('Ctrl Pts',(54.1876332328554,19.1683308247533,7.72637366107652));
#23196=CARTESIAN_POINT('Ctrl Pts',(54.0174481366244,19.2537222754074,7.7128318167165));
#23197=CARTESIAN_POINT('Ctrl Pts',(53.8619125385576,19.3617739799992,7.7));
#23198=CARTESIAN_POINT('',(56.1603489846691,19.3774656255483,7.7));
#23199=CARTESIAN_POINT('Origin',(55.,21.,7.7));
#23200=CARTESIAN_POINT('Ctrl Pts',(56.1603489846691,19.3774656255483,7.7));
#23201=CARTESIAN_POINT('Ctrl Pts',(56.2184119355306,19.4189891132105,7.70455633151969));
#23202=CARTESIAN_POINT('Ctrl Pts',(56.2742878120524,19.4636645528829,7.70911266303938));
#23203=CARTESIAN_POINT('Ctrl Pts',(56.327631526034,19.5112347083638,7.71366899455907));
#23204=CARTESIAN_POINT('Ctrl Pts',(56.3829325283937,19.5605503087251,7.71839250706531));
#23205=CARTESIAN_POINT('Ctrl Pts',(56.4355115089017,19.6129768999016,7.72311601957156));
#23206=CARTESIAN_POINT('Ctrl Pts',(56.4850212649274,19.6681819173726,7.72783953207781));
#23207=CARTESIAN_POINT('Ctrl Pts',(56.5327427796166,19.7213929865362,7.73239243618289));
#23208=CARTESIAN_POINT('Ctrl Pts',(56.5776126865276,19.777184823213,7.73694534028798));
#23209=CARTESIAN_POINT('Ctrl Pts',(56.6193586935831,19.8352232042074,7.74149824439307));
#23210=CARTESIAN_POINT('Ctrl Pts',(56.6611051744409,19.8932622439168,7.746051200172));
#23211=CARTESIAN_POINT('Ctrl Pts',(56.6997274177751,19.9535475074006,7.75060415595094));
#23212=CARTESIAN_POINT('Ctrl Pts',(56.7349954777785,20.0157143429938,7.75515711172987));
#23213=CARTESIAN_POINT('Ctrl Pts',(56.7702734473569,20.0778986461461,7.75971134679258));
#23214=CARTESIAN_POINT('Ctrl Pts',(56.8021951346799,20.141965174434,7.76426558185529));
#23215=CARTESIAN_POINT('Ctrl Pts',(56.8305763917255,20.207524362168,7.768819816918));
#23216=CARTESIAN_POINT('Ctrl Pts',(56.8589732786453,20.2731196540764,7.77337656004866));
#23217=CARTESIAN_POINT('Ctrl Pts',(56.8838256779872,20.3402088200512,7.77793330317931));
#23218=CARTESIAN_POINT('Ctrl Pts',(56.9049979603927,20.4083832884379,7.78249004630996));
#23219=CARTESIAN_POINT('Ctrl Pts',(56.9262029963242,20.4766632227434,7.78705383872332));
#23220=CARTESIAN_POINT('Ctrl Pts',(56.9437164171219,20.5460313730339,7.79161763113668));
#23221=CARTESIAN_POINT('Ctrl Pts',(56.9574528908856,20.6160654450776,7.79618142355004));
#23222=CARTESIAN_POINT('Ctrl Pts',(56.9712016619737,20.6861622138298,7.8007493016142));
#23223=CARTESIAN_POINT('Ctrl Pts',(56.9811666872574,20.7569256394431,7.80531717967836));
#23224=CARTESIAN_POINT('Ctrl Pts',(56.9873144028289,20.8279272630282,7.80988505774252));
#23225=CARTESIAN_POINT('Ctrl Pts',(56.9934735122458,20.8990604772048,7.81446140166627));
#23226=CARTESIAN_POINT('Ctrl Pts',(56.9958011727957,20.9704323143018,7.81903774559003));
#23227=CARTESIAN_POINT('Ctrl Pts',(56.9943158867061,21.041613778149,7.82361408951378));
#23228=CARTESIAN_POINT('Ctrl Pts',(56.9939459773054,21.0593414690047,7.82475382457885));
#23229=CARTESIAN_POINT('Ctrl Pts',(56.9933398192831,21.077057379685,7.82589355964391));
#23230=CARTESIAN_POINT('Ctrl Pts',(56.992498196117,21.0947549522225,7.82703329470898));
#23231=CARTESIAN_POINT('Ctrl Pts',(56.9892396630441,21.1632750782667,7.83144603493929));
#23232=CARTESIAN_POINT('Ctrl Pts',(56.9824346045893,21.2317892992464,7.83585877516959));
#23233=CARTESIAN_POINT('Ctrl Pts',(56.9720776952813,21.2998951921485,7.8402715153999));
#23234=CARTESIAN_POINT('Ctrl Pts',(56.9617380090342,21.3678878281029,7.84467691744743));
#23235=CARTESIAN_POINT('Ctrl Pts',(56.9478582607508,21.4354729937093,7.84908231949497));
#23236=CARTESIAN_POINT('Ctrl Pts',(56.9304850929434,21.5022498067926,7.8534877215425));
#23237=CARTESIAN_POINT('Ctrl Pts',(56.9131356262496,21.5689355204954,7.8578871135788));
#23238=CARTESIAN_POINT('Ctrl Pts',(56.8923023260374,21.6348145900977,7.8622865056151));
#23239=CARTESIAN_POINT('Ctrl Pts',(56.8680831432016,21.6994947695202,7.8666858976514));
#23240=CARTESIAN_POINT('Ctrl Pts',(56.8438819052752,21.7641270249492,7.87108203001159));
#23241=CARTESIAN_POINT('Ctrl Pts',(56.8162999323649,21.8275616842975,7.87547816237179));
#23242=CARTESIAN_POINT('Ctrl Pts',(56.7854849764184,21.8894217005921,7.87987429473198));
#23243=CARTESIAN_POINT('Ctrl Pts',(56.7546818822706,21.9512579047138,7.88426873486075));
#23244=CARTESIAN_POINT('Ctrl Pts',(56.7206484962793,22.0115202208583,7.88866317498952));
#23245=CARTESIAN_POINT('Ctrl Pts',(56.6835798897769,22.0698534092289,7.89305761511829));
#23246=CARTESIAN_POINT('Ctrl Pts',(56.6465123564219,22.128184908836,7.89745192802668));
#23247=CARTESIAN_POINT('Ctrl Pts',(56.6064100470769,22.1845869706907,7.90184624093507));
#23248=CARTESIAN_POINT('Ctrl Pts',(56.5635119754025,22.2387323622449,7.90624055384346));
#23249=CARTESIAN_POINT('Ctrl Pts',(56.5205704205432,22.2929326377131,7.9106393210015));
#23250=CARTESIAN_POINT('Ctrl Pts',(56.4748277577648,22.34487128408,7.91503808815953));
#23251=CARTESIAN_POINT('Ctrl Pts',(56.426563324315,22.3942541533807,7.91943685531758));
#23252=CARTESIAN_POINT('Ctrl Pts',(56.3782727050157,22.4436638153379,7.92383800902502));
#23253=CARTESIAN_POINT('Ctrl Pts',(56.3274579612184,22.4905146028582,7.92823916273246));
#23254=CARTESIAN_POINT('Ctrl Pts',(56.2744331730675,22.5345512861697,7.9326403164399));
#23255=CARTESIAN_POINT('Ctrl Pts',(56.2213135028848,22.5786667682871,7.93704934552828));
#23256=CARTESIAN_POINT('Ctrl Pts',(56.1659762959802,22.6199577967211,7.94145837461667));
#23257=CARTESIAN_POINT('Ctrl Pts',(56.1087656593053,22.6582117703252,7.94586740370505));
#23258=CARTESIAN_POINT('Ctrl Pts',(56.0733020212838,22.6819245823412,7.94860046560936));
#23259=CARTESIAN_POINT('Ctrl Pts',(56.037119055604,22.7044712965235,7.95133352751366));
#23260=CARTESIAN_POINT('Ctrl Pts',(56.0003030488091,22.7258103525716,7.95406658941796));
#23261=CARTESIAN_POINT('Ctrl Pts',(55.9402263670326,22.7606316108018,7.95852642372903));
#23262=CARTESIAN_POINT('Ctrl Pts',(55.878211896727,22.7923802153581,7.9629862580401));
#23263=CARTESIAN_POINT('Ctrl Pts',(55.814606302618,22.8208361085597,7.96744609235117));
#23264=CARTESIAN_POINT('Ctrl Pts',(55.751111477527,22.849242445879,7.9718981598695));
#23265=CARTESIAN_POINT('Ctrl Pts',(55.686031476172,22.874367267309,7.97635022738782));
#23266=CARTESIAN_POINT('Ctrl Pts',(55.6197385506428,22.8960357832454,7.98080229490615));
#23267=CARTESIAN_POINT('Ctrl Pts',(55.5535120650873,22.9176825826018,7.98524990048157));
#23268=CARTESIAN_POINT('Ctrl Pts',(55.4860755284922,22.9358797974142,7.98969750605699));
#23269=CARTESIAN_POINT('Ctrl Pts',(55.417821041808,22.9505007407131,7.99414511163241));
#23270=CARTESIAN_POINT('Ctrl Pts',(55.3496157056091,22.9651111553788,7.99858951445907));
#23271=CARTESIAN_POINT('Ctrl Pts',(55.2805940652508,22.9761503110027,8.00303391728573));
#23272=CARTESIAN_POINT('Ctrl Pts',(55.2111614840226,22.9835418801138,8.00747832011239));
#23273=CARTESIAN_POINT('Ctrl Pts',(55.1956094787083,22.9851974965415,8.00847380919197));
#23274=CARTESIAN_POINT('Ctrl Pts',(55.1800368963047,22.9866703158932,8.00946929827154));
#23275=CARTESIAN_POINT('Ctrl Pts',(55.1644483516311,22.987959834138,8.01046478735112));
#23276=CARTESIAN_POINT('Origin',(55.,21.,6.22095488139522));
#23277=CARTESIAN_POINT('',(55.1644483561882,22.987959833761,8.96685094802471));
#23278=CARTESIAN_POINT('',(55.1644479310503,22.9879598689293,8.81003518437327));
#23279=CARTESIAN_POINT('',(55.1644483516311,22.987959834138,6.22095488139522));
#23280=CARTESIAN_POINT('Ctrl Pts',(55.1644483561882,22.987959833761,8.96685094802472));
#23281=CARTESIAN_POINT('Ctrl Pts',(55.1865084564878,22.9861349743398,8.96536845462905));
#23282=CARTESIAN_POINT('Ctrl Pts',(55.2085395154997,22.9839428077344,8.96390036621413));
#23283=CARTESIAN_POINT('Ctrl Pts',(55.2395823717726,22.9803309980166,8.96185353255058));
#23284=CARTESIAN_POINT('Ctrl Pts',(55.2486253068872,22.9792160162485,8.96125989859017));
#23285=CARTESIAN_POINT('Ctrl Pts',(55.2625679963084,22.9773998336391,8.96034898609838));
#23286=CARTESIAN_POINT('Ctrl Pts',(55.2674731711851,22.9767423096468,8.96002935466431));
#23287=CARTESIAN_POINT('Ctrl Pts',(55.2765201775166,22.9754952936337,8.95944144062812));
#23288=CARTESIAN_POINT('Ctrl Pts',(55.2806625788646,22.9749110311965,8.95917287900392));
#23289=CARTESIAN_POINT('Ctrl Pts',(55.2900266624855,22.9735602219081,8.95856718687728));
#23290=CARTESIAN_POINT('Ctrl Pts',(55.2952471506301,22.9727859833341,8.95823049302025));
#23291=CARTESIAN_POINT('Ctrl Pts',(55.3087211275041,22.9707330060598,8.95736388279193));
#23292=CARTESIAN_POINT('Ctrl Pts',(55.316969866643,22.9694231198871,8.95683566485312));
#23293=CARTESIAN_POINT('Ctrl Pts',(55.3691079277055,22.9608076191609,8.95351023926098));
#23294=CARTESIAN_POINT('Ctrl Pts',(55.4127543858073,22.9520864922565,8.95078604867752));
#23295=CARTESIAN_POINT('Ctrl Pts',(55.4693998110486,22.9387827862763,8.94728607288447));
#23296=CARTESIAN_POINT('Ctrl Pts',(55.4826911878615,22.9355164958973,8.94646743070764));
#23297=CARTESIAN_POINT('Ctrl Pts',(55.6551105323159,22.8912587195686,8.93586958493547));
#23298=CARTESIAN_POINT('Ctrl Pts',(55.8086174884301,22.8308939233631,8.92662221527559));
#23299=CARTESIAN_POINT('Ctrl Pts',(56.0118357841249,22.7203787568067,8.91284248232438));
#23300=CARTESIAN_POINT('Ctrl Pts',(56.0690281228826,22.6854353060446,8.90877935135671));
#23301=CARTESIAN_POINT('Ctrl Pts',(56.1366164073965,22.639314249335,8.903685266579));
#23302=CARTESIAN_POINT('Ctrl Pts',(56.1487880083567,22.6308078239558,8.90275583833901));
#23303=CARTESIAN_POINT('Ctrl Pts',(56.1678252651308,22.6171842828034,8.90128241344744));
#23304=CARTESIAN_POINT('Ctrl Pts',(56.1747550454281,22.6121573849866,8.90074187727456));
#23305=CARTESIAN_POINT('Ctrl Pts',(56.187667139856,22.602663429206,8.89972671264464));
#23306=CARTESIAN_POINT('Ctrl Pts',(56.193657169235,22.5982070774024,8.89925250530754));
#23307=CARTESIAN_POINT('Ctrl Pts',(56.2069932677625,22.5881687366505,8.89818933239269));
#23308=CARTESIAN_POINT('Ctrl Pts',(56.2143258734256,22.5825692253111,8.89759968619538));
#23309=CARTESIAN_POINT('Ctrl Pts',(56.2328096587034,22.5682500710014,8.89610023816652));
#23310=CARTESIAN_POINT('Ctrl Pts',(56.2439072057028,22.5594623388304,8.89518775392164));
#23311=CARTESIAN_POINT('Ctrl Pts',(56.3093213635956,22.506520807602,8.88973489358598));
#23312=CARTESIAN_POINT('Ctrl Pts',(56.3613708453414,22.459655723815,8.88508546416893));
#23313=CARTESIAN_POINT('Ctrl Pts',(56.5282364015195,22.2927087169441,8.86908451838339));
#23314=CARTESIAN_POINT('Ctrl Pts',(56.6304864742761,22.161079785623,8.857293965576));
#23315=CARTESIAN_POINT('Ctrl Pts',(56.7330859240166,21.9882623150716,8.84353657859717));
#23316=CARTESIAN_POINT('Ctrl Pts',(56.7501370813457,21.9577419845985,8.84116824626649));
#23317=CARTESIAN_POINT('Ctrl Pts',(56.7730403932579,21.9140902218614,8.83788145016341));
#23318=CARTESIAN_POINT('Ctrl Pts',(56.7795656026522,21.9013209538791,8.83693181604444));
#23319=CARTESIAN_POINT('Ctrl Pts',(56.7907981239385,21.8787422730067,8.83527478665353));
#23320=CARTESIAN_POINT('Ctrl Pts',(56.7955638712028,21.8689627726656,8.834564277132));
#23321=CARTESIAN_POINT('Ctrl Pts',(56.8025380649138,21.8543490626825,8.833513756575));
#23322=CARTESIAN_POINT('Ctrl Pts',(56.804807490471,21.8495444192596,8.83317015962952));
#23323=CARTESIAN_POINT('Ctrl Pts',(56.8088301525623,21.8409390937834,8.83255803144846));
#23324=CARTESIAN_POINT('Ctrl Pts',(56.810590646736,21.8371419182502,8.83228906146702));
#23325=CARTESIAN_POINT('Ctrl Pts',(56.8143947258009,21.8288688376022,8.83170552282115));
#23326=CARTESIAN_POINT('Ctrl Pts',(56.8164337033289,21.8243909106942,8.83139123632787));
#23327=CARTESIAN_POINT('Ctrl Pts',(56.8220464623999,21.8119424553793,8.83052173699147));
#23328=CARTESIAN_POINT('Ctrl Pts',(56.8255845418527,21.8039558129589,8.82996865266857));
#23329=CARTESIAN_POINT('Ctrl Pts',(56.8442367451569,21.7610933736043,8.82702446763403));
#23330=CARTESIAN_POINT('Ctrl Pts',(56.85840527113,21.7258116710683,8.8246859470485));
#23331=CARTESIAN_POINT('Ctrl Pts',(56.9155278156353,21.5709046628101,8.81469396784404));
#23332=CARTESIAN_POINT('Ctrl Pts',(56.9480057108673,21.4477258939431,8.80743463040236));
#23333=CARTESIAN_POINT('Ctrl Pts',(56.9881871096727,21.2022947470752,8.79295922802081));
#23334=CARTESIAN_POINT('Ctrl Pts',(56.9968175632529,21.0807768319081,8.78578164015386));
#23335=CARTESIAN_POINT('Ctrl Pts',(56.9939888480958,20.9423762883097,8.77718580361414));
#23336=CARTESIAN_POINT('Ctrl Pts',(56.9934303699947,20.9255194584189,8.77613215667945));
#23337=CARTESIAN_POINT('Ctrl Pts',(56.9922465063731,20.899689055796,8.77450650512826));
#23338=CARTESIAN_POINT('Ctrl Pts',(56.9917740579242,20.8907089867084,8.77393928047882));
#23339=CARTESIAN_POINT('Ctrl Pts',(56.9908421045692,20.8750179116583,8.77294443357605));
#23340=CARTESIAN_POINT('Ctrl Pts',(56.9904093403938,20.8683054154788,8.77251765539606));
#23341=CARTESIAN_POINT('Ctrl Pts',(56.9893543670329,20.853137314105,8.77155051840636));
#23342=CARTESIAN_POINT('Ctrl Pts',(56.9887121853851,20.8446832714074,8.77100954128639));
#23343=CARTESIAN_POINT('Ctrl Pts',(56.9868277155012,20.8218070373187,8.76954031167875));
#23344=CARTESIAN_POINT('Ctrl Pts',(56.9854823201596,20.8073940784083,8.76860884724143));
#23345=CARTESIAN_POINT('Ctrl Pts',(56.9784364090486,20.739863793031,8.76421653125217));
#23346=CARTESIAN_POINT('Ctrl Pts',(56.9707608782783,20.6869790146462,8.76069441012519));
#23347=CARTESIAN_POINT('Ctrl Pts',(56.9273992381471,20.454355228825,8.74482515023841));
#23348=CARTESIAN_POINT('Ctrl Pts',(56.869169214372,20.2797331910237,8.73179941161804));
#23349=CARTESIAN_POINT('Ctrl Pts',(56.7641527851455,20.067436638048,8.71557049069498));
#23350=CARTESIAN_POINT('Ctrl Pts',(56.7384150534879,20.0202940697493,8.71194787633662));
#23351=CARTESIAN_POINT('Ctrl Pts',(56.7060472880574,19.9663096292685,8.70782426258264));
#23352=CARTESIAN_POINT('Ctrl Pts',(56.7012352521229,19.9584090262773,8.70722142853358));
#23353=CARTESIAN_POINT('Ctrl Pts',(56.6937491459621,19.9463083101455,8.70629946944603));
#23354=CARTESIAN_POINT('Ctrl Pts',(56.6911140980956,19.942084381791,8.70597790234971));
#23355=CARTESIAN_POINT('Ctrl Pts',(56.6862370694153,19.93433138924,8.70538820431591));
#23356=CARTESIAN_POINT('Ctrl Pts',(56.6839998169274,19.9307995232722,8.70511978089514));
#23357=CARTESIAN_POINT('Ctrl Pts',(56.6789336723095,19.9228571403148,8.70451661803648));
#23358=CARTESIAN_POINT('Ctrl Pts',(56.6760985026165,19.9184507282493,8.70418229946691));
#23359=CARTESIAN_POINT('Ctrl Pts',(56.6687663337754,19.9071531696018,8.70332581431172));
#23360=CARTESIAN_POINT('Ctrl Pts',(56.6642439454849,19.900278504851,8.7028052809941));
#23361=CARTESIAN_POINT('Ctrl Pts',(56.6362263645125,19.8582565167433,8.69962616446429));
#23362=CARTESIAN_POINT('Ctrl Pts',(56.6116593732559,19.8238326866816,8.69703343051772));
#23363=CARTESIAN_POINT('Ctrl Pts',(56.5690774512852,19.7680083447545,8.69280166471653));
#23364=CARTESIAN_POINT('Ctrl Pts',(56.5516750033045,19.7461609829284,8.69113821789112));
#23365=CARTESIAN_POINT('Ctrl Pts',(56.4246422639128,19.5933788839755,8.67939690273966));
#23366=CARTESIAN_POINT('Ctrl Pts',(56.2990602063877,19.4766372599477,8.66977820784346));
#23367=CARTESIAN_POINT('Ctrl Pts',(56.1186217146426,19.347632673179,8.65642364828826));
#23368=CARTESIAN_POINT('Ctrl Pts',(56.0759835428922,19.3195562894424,8.65330278979114));
#23369=CARTESIAN_POINT('Ctrl Pts',(56.0206186201192,19.2860711362976,8.64926811520142));
#23370=CARTESIAN_POINT('Ctrl Pts',(56.0088466723956,19.2791156650106,8.64841127130339));
#23371=CARTESIAN_POINT('Ctrl Pts',(55.9898131525822,19.2681321008778,8.64702707573648));
#23372=CARTESIAN_POINT('Ctrl Pts',(55.9825961793813,19.264027292288,8.64650250149506));
#23373=CARTESIAN_POINT('Ctrl Pts',(55.9688062295423,19.2562975041036,8.64550057955995));
#23374=CARTESIAN_POINT('Ctrl Pts',(55.9622379920794,19.2526643285652,8.64502353642583));
#23375=CARTESIAN_POINT('Ctrl Pts',(55.9471891964025,19.2444507733732,8.64393088639118));
#23376=CARTESIAN_POINT('Ctrl Pts',(55.9386956841478,19.2398946429085,8.64331443081922));
#23377=CARTESIAN_POINT('Ctrl Pts',(55.9164455232961,19.2281659638668,8.64169996408948));
#23378=CARTESIAN_POINT('Ctrl Pts',(55.9026378420401,19.2210921461991,8.64069851363044));
#23379=CARTESIAN_POINT('Ctrl Pts',(55.7885075455003,19.1642928918249,8.63242265650306));
#23380=CARTESIAN_POINT('Ctrl Pts',(55.6842605767762,19.1229425526894,8.6248578133751));
#23381=CARTESIAN_POINT('Ctrl Pts',(55.4948114204314,19.0656832433802,8.61117717891633));
#23382=CARTESIAN_POINT('Ctrl Pts',(55.4109899186735,19.0461560159091,8.60515076391878));
#23383=CARTESIAN_POINT('Ctrl Pts',(55.2489589085595,19.0192998970607,8.59374296508921));
#23384=CARTESIAN_POINT('Ctrl Pts',(55.1710495409836,19.0110560464908,8.58836297019318));
#23385=CARTESIAN_POINT('Ctrl Pts',(55.0776135567572,19.006702141134,8.58217487221943));
#23386=CARTESIAN_POINT('Ctrl Pts',(55.0623688232796,19.0061669121444,8.58117369327942));
#23387=CARTESIAN_POINT('Ctrl Pts',(55.0410293850822,19.0056627027973,8.57978545106758));
#23388=CARTESIAN_POINT('Ctrl Pts',(55.0349391409071,19.0055467104376,8.57939075261287));
#23389=CARTESIAN_POINT('Ctrl Pts',(55.0245533542877,19.0053964939698,8.57872034015849));
#23390=CARTESIAN_POINT('Ctrl Pts',(55.020258085147,19.0053482447256,8.57844385662053));
#23391=CARTESIAN_POINT('Ctrl Pts',(55.0119814393164,19.0052820103319,8.57791263653424));
#23392=CARTESIAN_POINT('Ctrl Pts',(55.0080001448542,19.0052620694554,8.57765778797978));
#23393=CARTESIAN_POINT('Ctrl Pts',(54.9984307094535,19.0052427901047,8.57704681857676));
#23394=CARTESIAN_POINT('Ctrl Pts',(54.9928425409804,19.0052550133715,8.5766913353187));
#23395=CARTESIAN_POINT('Ctrl Pts',(54.9724233002512,19.0053854860776,8.5753968994575));
#23396=CARTESIAN_POINT('Ctrl Pts',(54.9575931835433,19.0056456618568,8.57446545805293));
#23397=CARTESIAN_POINT('Ctrl Pts',(54.8041096731952,19.010051208765,8.56490274726291));
#23398=CARTESIAN_POINT('Ctrl Pts',(54.6662245513131,19.0284841901866,8.55694662923051));
#23399=CARTESIAN_POINT('Ctrl Pts',(54.3985642979242,19.0931791887636,8.54095999199972));
#23400=CARTESIAN_POINT('Ctrl Pts',(54.2694431651416,19.1388255619681,8.53296443385819));
#23401=CARTESIAN_POINT('Ctrl Pts',(54.129862678246,19.2049491047315,8.52338510605496));
#23402=CARTESIAN_POINT('Ctrl Pts',(54.1138227293572,19.2128132476175,8.52227006836565));
#23403=CARTESIAN_POINT('Ctrl Pts',(54.089683946122,19.2250529818988,8.52056934336464));
#23404=CARTESIAN_POINT('Ctrl Pts',(54.0815059385225,19.2292710852675,8.51998915452102));
#23405=CARTESIAN_POINT('Ctrl Pts',(54.0667457556547,19.2370139470255,8.51893458805065));
#23406=CARTESIAN_POINT('Ctrl Pts',(54.0601535936528,19.2405193841449,8.51846089863803));
#23407=CARTESIAN_POINT('Ctrl Pts',(54.0460253017488,19.2481342753807,8.51743978876543));
#23408=CARTESIAN_POINT('Ctrl Pts',(54.0384957294043,19.2522555175807,8.51689195613921));
#23409=CARTESIAN_POINT('Ctrl Pts',(54.0182646751908,19.2634991023865,8.51541001917457));
#23410=CARTESIAN_POINT('Ctrl Pts',(54.0056143958029,19.2707120347098,8.51447268823011));
#23411=CARTESIAN_POINT('Ctrl Pts',(53.944330844241,19.306549465321,8.50987850104922));
#23412=CARTESIAN_POINT('Ctrl Pts',(53.8968524391625,19.3370879490345,8.50615279584404));
#23413=CARTESIAN_POINT('Ctrl Pts',(53.692979707825,19.4807968217045,8.48939029214187));
#23414=CARTESIAN_POINT('Ctrl Pts',(53.5522288976417,19.6142799848005,8.47560681094763));
#23415=CARTESIAN_POINT('Ctrl Pts',(53.4071433362011,19.7985170455179,8.45967015303951));
#23416=CARTESIAN_POINT('Ctrl Pts',(53.3824631539231,19.831955152345,8.45688739156822));
#23417=CARTESIAN_POINT('Ctrl Pts',(53.3539277007352,19.8732576422887,8.45360256297839));
#23418=CARTESIAN_POINT('Ctrl Pts',(53.3490580594482,19.8804049524273,8.45303948186538));
#23419=CARTESIAN_POINT('Ctrl Pts',(53.3415307435403,19.8916089130415,8.4521654074708));
#23420=CARTESIAN_POINT('Ctrl Pts',(53.3388411872525,19.8956438634574,8.45185234616995));
#23421=CARTESIAN_POINT('Ctrl Pts',(53.3338542186678,19.9031848981677,8.45127052445996));
#23422=CARTESIAN_POINT('Ctrl Pts',(53.3315531628786,19.9066883863992,8.45100152943208));
#23423=CARTESIAN_POINT('Ctrl Pts',(53.3263075874079,19.9147302015091,8.45038705914323));
#23424=CARTESIAN_POINT('Ctrl Pts',(53.3233704771758,19.9192732665751,8.45004207716746));
#23425=CARTESIAN_POINT('Ctrl Pts',(53.3157041490186,19.9312378696055,8.4491390119709));
#23426=CARTESIAN_POINT('Ctrl Pts',(53.3110054361819,19.9386789481484,8.44858287802332));
#23427=CARTESIAN_POINT('Ctrl Pts',(53.277938754316,19.9918205165758,8.44464832241344));
#23428=CARTESIAN_POINT('Ctrl Pts',(53.2513775054864,20.0386253051174,8.44137712021863));
#23429=CARTESIAN_POINT('Ctrl Pts',(53.137338675478,20.2599825048624,8.42651664325599));
#23430=CARTESIAN_POINT('Ctrl Pts',(53.073892839478,20.4456956293377,8.41563826537016));
#23431=CARTESIAN_POINT('Ctrl Pts',(53.0306708516761,20.6796940777217,8.40123124119365));
#23432=CARTESIAN_POINT('Ctrl Pts',(53.0242624151752,20.7219464670555,8.39860884713311));
#23433=CARTESIAN_POINT('Ctrl Pts',(53.0176372123726,20.7776400830117,8.39511009818263));
#23434=CARTESIAN_POINT('Ctrl Pts',(53.01619203513,20.7909256133051,8.39427238761282));
#23435=CARTESIAN_POINT('Ctrl Pts',(53.0140727632987,20.8124145428847,8.3929120059279));
#23436=CARTESIAN_POINT('Ctrl Pts',(53.0133157431484,20.8206094944647,8.39239194698179));
#23437=CARTESIAN_POINT('Ctrl Pts',(53.0119644584749,20.8362968097598,8.39139389186064));
#23438=CARTESIAN_POINT('Ctrl Pts',(53.0113617830378,20.8437883219442,8.39091616877902));
#23439=CARTESIAN_POINT('Ctrl Pts',(53.0100739931629,20.8610134498793,8.38981513991193));
#23440=CARTESIAN_POINT('Ctrl Pts',(53.0094179387315,20.8707489823764,8.38919093381222));
#23441=CARTESIAN_POINT('Ctrl Pts',(53.0075917999732,20.9011741345993,8.38723401127514));
#23442=CARTESIAN_POINT('Ctrl Pts',(53.006672703119,20.9218768861661,8.3858934976464));
#23443=CARTESIAN_POINT('Ctrl Pts',(53.0028886157614,21.0533021562294,8.37732417736831));
#23444=CARTESIAN_POINT('Ctrl Pts',(53.0089276765414,21.1640696505946,8.36981793052127));
#23445=CARTESIAN_POINT('Ctrl Pts',(53.0377459093852,21.3720756965672,8.35528135071259));
#23446=CARTESIAN_POINT('Ctrl Pts',(53.0586890283821,21.4692470232919,8.34830564531651));
#23447=CARTESIAN_POINT('Ctrl Pts',(53.0940430860314,21.5890797735252,8.33967779543385));
#23448=CARTESIAN_POINT('Ctrl Pts',(53.1017831588605,21.6135630731477,8.33791422517428));
#23449=CARTESIAN_POINT('Ctrl Pts',(53.1240844565702,21.6796395610817,8.33316336334213));
#23450=CARTESIAN_POINT('Ctrl Pts',(53.1395556393487,21.7209136611738,8.33020517847966));
#23451=CARTESIAN_POINT('Ctrl Pts',(53.1595610012074,21.7693381215845,8.3267727273883));
#23452=CARTESIAN_POINT('Ctrl Pts',(53.1627875511733,21.7770117613453,8.32622996905585));
#23453=CARTESIAN_POINT('Ctrl Pts',(53.1681338931271,21.7895073580286,8.32534833023924));
#23454=CARTESIAN_POINT('Ctrl Pts',(53.1702248750348,21.7943414224981,8.32500779355331));
#23455=CARTESIAN_POINT('Ctrl Pts',(53.1740100218018,21.8029979090291,8.32439902175636));
#23456=CARTESIAN_POINT('Ctrl Pts',(53.1756970715198,21.8068233192643,8.324130367564));
#23457=CARTESIAN_POINT('Ctrl Pts',(53.1794091582221,21.8151693595066,8.3235450472189));
#23458=CARTESIAN_POINT('Ctrl Pts',(53.1814390063079,21.8196877523496,8.32322867879699));
#23459=CARTESIAN_POINT('Ctrl Pts',(53.1872589967608,21.8325148743381,8.32233188233438));
#23460=CARTESIAN_POINT('Ctrl Pts',(53.1910894539519,21.8408053310915,8.32175385719594));
#23461=CARTESIAN_POINT('Ctrl Pts',(53.2166556398915,21.8951560827101,8.31797306098169));
#23462=CARTESIAN_POINT('Ctrl Pts',(53.240093699518,21.9404000821336,8.31486657731594));
#23463=CARTESIAN_POINT('Ctrl Pts',(53.3421338799864,22.1201654740435,8.30249346811853));
#23464=CARTESIAN_POINT('Ctrl Pts',(53.434632553002,22.2461628856551,8.29371005804209));
#23465=CARTESIAN_POINT('Ctrl Pts',(53.5958793195042,22.4191492921025,8.27974011144415));
#23466=CARTESIAN_POINT('Ctrl Pts',(53.6544279274001,22.4747789993472,8.27488223774061));
#23467=CARTESIAN_POINT('Ctrl Pts',(53.7274147296392,22.5361542172549,8.26895633068329));
#23468=CARTESIAN_POINT('Ctrl Pts',(53.7387535513966,22.5454774108227,8.26803930739593));
#23469=CARTESIAN_POINT('Ctrl Pts',(53.7575113832154,22.560556870767,8.26652751982694));
#23470=CARTESIAN_POINT('Ctrl Pts',(53.7648700946963,22.5663875069428,8.26593574284831));
#23471=CARTESIAN_POINT('Ctrl Pts',(53.7781667366115,22.5767710749924,8.26486862037936));
#23472=CARTESIAN_POINT('Ctrl Pts',(53.7840896773369,22.5813429834177,8.26439403905699));
#23473=CARTESIAN_POINT('Ctrl Pts',(53.7967609098303,22.5910106092592,8.26338028831986));
#23474=CARTESIAN_POINT('Ctrl Pts',(53.8035161450404,22.5960969419428,8.26284076339189));
#23475=CARTESIAN_POINT('Ctrl Pts',(53.8218289661225,22.6097039338127,8.26138051155975));
#23476=CARTESIAN_POINT('Ctrl Pts',(53.8334463743195,22.6181428738318,8.26045664456695));
#23477=CARTESIAN_POINT('Ctrl Pts',(53.8937646222515,22.6609711655489,8.25567171050551));
#23478=CARTESIAN_POINT('Ctrl Pts',(53.9438938107748,22.6932868647718,8.25173301769435));
#23479=CARTESIAN_POINT('Ctrl Pts',(54.129584481805,22.8015360597188,8.23726755946039));
#23480=CARTESIAN_POINT('Ctrl Pts',(54.272447558802,22.8638164101038,8.22631508550302));
#23481=CARTESIAN_POINT('Ctrl Pts',(54.4265132078227,22.9105425813831,8.21517514585918));
#23482=CARTESIAN_POINT('Ctrl Pts',(54.4319752533222,22.9121736176193,8.21478112214838));
#23483=CARTESIAN_POINT('Ctrl Pts',(54.465706940801,22.9220890430145,8.21235367404621));
#23484=CARTESIAN_POINT('Ctrl Pts',(54.4941512941139,22.9297700843759,8.2103322016777));
#23485=CARTESIAN_POINT('Ctrl Pts',(54.56213677925,22.9465221141484,8.20557530596302));
#23486=CARTESIAN_POINT('Ctrl Pts',(54.6018073095801,22.955023185108,8.20285874755967));
#23487=CARTESIAN_POINT('Ctrl Pts',(54.6497128623326,22.9637700026662,8.19967006300534));
#23488=CARTESIAN_POINT('Ctrl Pts',(54.657722254699,22.9651818370479,8.19914000347872));
#23489=CARTESIAN_POINT('Ctrl Pts',(54.6708803510907,22.9674183600539,8.19827446874979));
#23490=CARTESIAN_POINT('Ctrl Pts',(54.6760239593531,22.9682719002622,8.19793744118423));
#23491=CARTESIAN_POINT('Ctrl Pts',(54.6853071788527,22.9697749993185,8.19733161783432));
#23492=CARTESIAN_POINT('Ctrl Pts',(54.6894455036847,22.9704316850051,8.19706243185619));
#23493=CARTESIAN_POINT('Ctrl Pts',(54.6985534617127,22.971847564879,8.1964719177826));
#23494=CARTESIAN_POINT('Ctrl Pts',(54.7035238972793,22.972601012982,8.1961509144526));
#23495=CARTESIAN_POINT('Ctrl Pts',(54.7178211360494,22.9747130131255,8.19523102984217));
#23496=CARTESIAN_POINT('Ctrl Pts',(54.7271549402624,22.976024285558,8.19463472956572));
#23497=CARTESIAN_POINT('Ctrl Pts',(54.7935071774651,22.9848667597959,8.19042356482895));
#23498=CARTESIAN_POINT('Ctrl Pts',(54.8508243690611,22.9899958099968,8.18693128718723));
#23499=CARTESIAN_POINT('Ctrl Pts',(54.9936931458039,22.996571355401,8.17841136970841));
#23500=CARTESIAN_POINT('Ctrl Pts',(55.0792561425175,22.9950071188978,8.17347009990951));
#23501=CARTESIAN_POINT('Ctrl Pts',(55.1644483595783,22.9879598334805,8.16850613376992));
#23502=CARTESIAN_POINT('',(53.0052503954397,21.0012560281401,8.22095488139522));
#23503=CARTESIAN_POINT('Ctrl Pts',(55.1644483516311,22.987959834138,8.01046478735112));
#23504=CARTESIAN_POINT('Ctrl Pts',(55.0948703834473,22.99371547466,8.01490805700561));
#23505=CARTESIAN_POINT('Ctrl Pts',(55.0249742386028,22.995815270762,8.01935132666011));
#23506=CARTESIAN_POINT('Ctrl Pts',(54.9551724962436,22.9942462379072,8.02379459631461));
#23507=CARTESIAN_POINT('Ctrl Pts',(54.8853627279582,22.9926770246423,8.02823837686401));
#23508=CARTESIAN_POINT('Ctrl Pts',(54.8156478716461,22.9874381586569,8.03268215741341));
#23509=CARTESIAN_POINT('Ctrl Pts',(54.7464386782799,22.9785687298215,8.03712593796281));
#23510=CARTESIAN_POINT('Ctrl Pts',(54.6771547819335,22.969689727507,8.04157451503756));
#23511=CARTESIAN_POINT('Ctrl Pts',(54.6083781223961,22.9571724063764,8.04602309211231));
#23512=CARTESIAN_POINT('Ctrl Pts',(54.5405115177318,22.9411073893947,8.05047166918706));
#23513=CARTESIAN_POINT('Ctrl Pts',(54.4726014940703,22.925032094502,8.05492309232662));
#23514=CARTESIAN_POINT('Ctrl Pts',(54.4056031520644,22.9054047244854,8.05937451546619));
#23515=CARTESIAN_POINT('Ctrl Pts',(54.3399037173856,22.8823656552803,8.06382593860575));
#23516=CARTESIAN_POINT('Ctrl Pts',(54.2740964660976,22.8592887776171,8.06828466679065));
#23517=CARTESIAN_POINT('Ctrl Pts',(54.2095928253016,22.8327892164037,8.07274339497555));
#23518=CARTESIAN_POINT('Ctrl Pts',(54.1467587511724,22.8030548892918,8.07720212316045));
#23519=CARTESIAN_POINT('Ctrl Pts',(54.1284491801205,22.7943904379972,8.07850137681595));
#23520=CARTESIAN_POINT('Ctrl Pts',(54.1102812013221,22.7854516086545,8.07980063047145));
#23521=CARTESIAN_POINT('Ctrl Pts',(54.0922634203053,22.776243751399,8.08109988412695));
#23522=CARTESIAN_POINT('Ctrl Pts',(54.0303847541435,22.744621104601,8.08556192543676));
#23523=CARTESIAN_POINT('Ctrl Pts',(53.9700429673079,22.709701070478,8.09002396674658));
#23524=CARTESIAN_POINT('Ctrl Pts',(53.9116108382143,22.6716568412828,8.09448600805639));
#23525=CARTESIAN_POINT('Ctrl Pts',(53.8532641469313,22.6336682392861,8.0989415250953));
#23526=CARTESIAN_POINT('Ctrl Pts',(53.7968219760873,22.5925647740467,8.1033970421342));
#23527=CARTESIAN_POINT('Ctrl Pts',(53.742633042301,22.548565754557,8.1078525591731));
#23528=CARTESIAN_POINT('Ctrl Pts',(53.6885053116059,22.5046164292727,8.11230304397763));
#23529=CARTESIAN_POINT('Ctrl Pts',(53.6366261398674,22.4577783514479,8.11675352878216));
#23530=CARTESIAN_POINT('Ctrl Pts',(53.5873142773744,22.4083133925337,8.12120401358668));
#23531=CARTESIAN_POINT('Ctrl Pts',(53.5380320620621,22.3588781728446,8.12565182267951));
#23532=CARTESIAN_POINT('Ctrl Pts',(53.4913144370052,22.306819550072,8.13009963177234));
#23533=CARTESIAN_POINT('Ctrl Pts',(53.4474449834977,22.2524378161145,8.13454744086518));
#23534=CARTESIAN_POINT('Ctrl Pts',(53.4035871544836,22.1980704921862,8.13899407138104));
#23535=CARTESIAN_POINT('Ctrl Pts',(53.3625763044683,22.141381658573,8.14344070189691));
#23536=CARTESIAN_POINT('Ctrl Pts',(53.3246560659812,22.0827050684496,8.14788733241278));
#23537=CARTESIAN_POINT('Ctrl Pts',(53.2867331258202,22.0240242978406,8.15233427973428));
#23538=CARTESIAN_POINT('Ctrl Pts',(53.2519014969672,21.9633559002514,8.15678122705579));
#23539=CARTESIAN_POINT('Ctrl Pts',(53.220360799391,21.9010615285072,8.1612281743773));
#23540=CARTESIAN_POINT('Ctrl Pts',(53.1887861866401,21.8387001726865,8.16567990342548));
#23541=CARTESIAN_POINT('Ctrl Pts',(53.1605097885676,21.7747097889159,8.17013163247367));
#23542=CARTESIAN_POINT('Ctrl Pts',(53.1356842295709,21.7094746441061,8.17458336152186));
#23543=CARTESIAN_POINT('Ctrl Pts',(53.1108438409058,21.644200530765,8.17903774983206));
#23544=CARTESIAN_POINT('Ctrl Pts',(53.0894585437783,21.5776806404973,8.18349213814226));
#23545=CARTESIAN_POINT('Ctrl Pts',(53.0716310834577,21.5103144953981,8.18794652645247));
#23546=CARTESIAN_POINT('Ctrl Pts',(53.0537726691785,21.4428313819352,8.19240864895187));
#23547=CARTESIAN_POINT('Ctrl Pts',(53.039484522774,21.3744995576203,8.19687077145126));
#23548=CARTESIAN_POINT('Ctrl Pts',(53.0288181401238,21.3057280454834,8.20133289395066));
#23549=CARTESIAN_POINT('Ctrl Pts',(53.0233996096131,21.2707920649357,8.20359965557908));
#23550=CARTESIAN_POINT('Ctrl Pts',(53.018914896146,21.2357426891999,8.20586641720751));
#23551=CARTESIAN_POINT('Ctrl Pts',(53.0153656007572,21.2006336558065,8.20813317883593));
#23552=CARTESIAN_POINT('Ctrl Pts',(53.0086735267431,21.1344367845124,8.21240707968903));
#23553=CARTESIAN_POINT('Ctrl Pts',(53.0052923566473,21.0678963361395,8.21668098054213));
#23554=CARTESIAN_POINT('Ctrl Pts',(53.0052503954397,21.0012560281401,8.22095488139522));
#23555=CARTESIAN_POINT('Ctrl Pts',(53.0052504499798,21.0013398486355,8.22235592323264));
#23556=CARTESIAN_POINT('Ctrl Pts',(53.0052354588656,20.979021269004,8.22369119184465));
#23557=CARTESIAN_POINT('Ctrl Pts',(53.0055950411512,20.9567032697669,8.22501509771246));
#23558=CARTESIAN_POINT('Ctrl Pts',(53.0118822235976,20.7656411471647,8.23628596927151));
#23559=CARTESIAN_POINT('Ctrl Pts',(53.038837182935,20.5982800528773,8.24580309326332));
#23560=CARTESIAN_POINT('Ctrl Pts',(53.0958551742049,20.4047321928301,8.25795760527897));
#23561=CARTESIAN_POINT('Ctrl Pts',(53.1059377588708,20.3733906086174,8.25996094695637));
#23562=CARTESIAN_POINT('Ctrl Pts',(53.1246729231539,20.3197445873193,8.26346098531721));
#23563=CARTESIAN_POINT('Ctrl Pts',(53.1329598296126,20.2973194202502,8.26494592515493));
#23564=CARTESIAN_POINT('Ctrl Pts',(53.1453892230824,20.2654576737732,8.26708961418652));
#23565=CARTESIAN_POINT('Ctrl Pts',(53.1492051088484,20.2558952846873,8.2677373991672));
#23566=CARTESIAN_POINT('Ctrl Pts',(53.1559520551253,20.2393608386296,8.26886537102514));
#23567=CARTESIAN_POINT('Ctrl Pts',(53.1588490825913,20.2323750567181,8.26934439606832));
#23568=CARTESIAN_POINT('Ctrl Pts',(53.1645014393616,20.2189612647145,8.27026901623429));
#23569=CARTESIAN_POINT('Ctrl Pts',(53.167250990435,20.2125309288626,8.2707144083219));
#23570=CARTESIAN_POINT('Ctrl Pts',(53.1738297883286,20.1973662910301,8.27176992170854));
#23571=CARTESIAN_POINT('Ctrl Pts',(53.1776879431349,20.1886447911613,8.27238102846664));
#23572=CARTESIAN_POINT('Ctrl Pts',(53.191458640716,20.1581093803898,8.27453512457026));
#23573=CARTESIAN_POINT('Ctrl Pts',(53.2017012092166,20.1364474311519,8.2760894431332));
#23574=CARTESIAN_POINT('Ctrl Pts',(53.2765002348601,19.985360127803,8.28712075167099));
#23575=CARTESIAN_POINT('Ctrl Pts',(53.354563967129,19.8631310456656,8.29708629822046));
#23576=CARTESIAN_POINT('Ctrl Pts',(53.4997175605774,19.6825125944605,8.31325773128512));
#23577=CARTESIAN_POINT('Ctrl Pts',(53.5586970386458,19.6182374923628,8.31935566144467));
#23578=CARTESIAN_POINT('Ctrl Pts',(53.6432006933683,19.5374650746013,8.32732090089623));
#23579=CARTESIAN_POINT('Ctrl Pts',(53.6651667349387,19.5173897631785,8.32932810551325));
#23580=CARTESIAN_POINT('Ctrl Pts',(53.6972128646045,19.4893918312796,8.33215790101528));
#23581=CARTESIAN_POINT('Ctrl Pts',(53.706932007257,19.481064008949,8.33300364016904));
#23582=CARTESIAN_POINT('Ctrl Pts',(53.7221350853931,19.4682889798934,8.33430645185761));
#23583=CARTESIAN_POINT('Ctrl Pts',(53.7275634236692,19.463776529334,8.33476771348039));
#23584=CARTESIAN_POINT('Ctrl Pts',(53.7377414858454,19.4554067067298,8.33562511388652));
#23585=CARTESIAN_POINT('Ctrl Pts',(53.7424852072569,19.4515422038009,8.33602173650106));
#23586=CARTESIAN_POINT('Ctrl Pts',(53.7505402179061,19.4450415673173,8.33669006891283));
#23587=CARTESIAN_POINT('Ctrl Pts',(53.7538422257107,19.4423940558081,8.33696258829237));
#23588=CARTESIAN_POINT('Ctrl Pts',(53.7602180910616,19.4373152142198,8.33748597499489));
#23589=CARTESIAN_POINT('Ctrl Pts',(53.7632906932421,19.4348824284845,8.33773695284236));
#23590=CARTESIAN_POINT('Ctrl Pts',(53.7713886425627,19.4285094740506,8.33839519886141));
#23591=CARTESIAN_POINT('Ctrl Pts',(53.776425825021,19.424584314608,8.33880141044685));
#23592=CARTESIAN_POINT('Ctrl Pts',(53.7941172548509,19.4109345324222,8.34021714740838));
#23593=CARTESIAN_POINT('Ctrl Pts',(53.8068696665272,19.4013373400012,8.34121818052374));
#23594=CARTESIAN_POINT('Ctrl Pts',(53.9035917225248,19.3303485384072,8.34867712024682));
#23595=CARTESIAN_POINT('Ctrl Pts',(53.9921440466086,19.275448154112,8.35476314360415));
#23596=CARTESIAN_POINT('Ctrl Pts',(54.1627020086377,19.1873527996347,8.36591987249285));
#23597=CARTESIAN_POINT('Ctrl Pts',(54.2434001979792,19.152213748393,8.37098979536434));
#23598=CARTESIAN_POINT('Ctrl Pts',(54.3996672731362,19.0961278703635,8.38077956062949));
#23599=CARTESIAN_POINT('Ctrl Pts',(54.4746627248512,19.0740853594523,8.38546620294678));
#23600=CARTESIAN_POINT('Ctrl Pts',(54.570635995411,19.0519007669188,8.39155807552668));
#23601=CARTESIAN_POINT('Ctrl Pts',(54.5905889723066,19.0476100202893,8.39282936918941));
#23602=CARTESIAN_POINT('Ctrl Pts',(54.6201307571847,19.0417300285119,8.39472013085657));
#23603=CARTESIAN_POINT('Ctrl Pts',(54.6296713868745,19.0399034116127,8.39533206023183));
#23604=CARTESIAN_POINT('Ctrl Pts',(54.6466281862664,19.0367851399428,8.39642212331452));
#23605=CARTESIAN_POINT('Ctrl Pts',(54.6540390914874,19.0354656346247,8.39689936416734));
#23606=CARTESIAN_POINT('Ctrl Pts',(54.6696255649875,19.032781406114,8.39790491411394));
#23607=CARTESIAN_POINT('Ctrl Pts',(54.6778025092209,19.0314256333667,8.39843349658196));
#23608=CARTESIAN_POINT('Ctrl Pts',(54.6993826216341,19.0279856133351,8.39983138818227));
#23609=CARTESIAN_POINT('Ctrl Pts',(54.7127988265832,19.0259870769582,8.40070338045249));
#23610=CARTESIAN_POINT('Ctrl Pts',(54.7701384370223,19.0180424274027,8.40444334849047));
#23611=CARTESIAN_POINT('Ctrl Pts',(54.8142301760946,19.0134247520525,8.40735248751739));
#23612=CARTESIAN_POINT('Ctrl Pts',(55.05030806839,18.9966284020374,8.42311611347497));
#23613=CARTESIAN_POINT('Ctrl Pts',(55.243134248663,19.0108065762286,8.43678591134482));
#23614=CARTESIAN_POINT('Ctrl Pts',(55.4839463341905,19.0640825457091,8.45368607612069));
#23615=CARTESIAN_POINT('Ctrl Pts',(55.5365074913047,19.077985088639,8.45735361782112));
#23616=CARTESIAN_POINT('Ctrl Pts',(55.597325338169,19.0967615813014,8.46152337226817));
#23617=CARTESIAN_POINT('Ctrl Pts',(55.6061916527687,19.0995669635042,8.46212937469842));
#23618=CARTESIAN_POINT('Ctrl Pts',(55.6197941343001,19.1039757943543,8.46305583931023));
#23619=CARTESIAN_POINT('Ctrl Pts',(55.624544291256,19.1055351713768,8.46337876016643));
#23620=CARTESIAN_POINT('Ctrl Pts',(55.6332646693485,19.1084342524079,8.46397038935791));
#23621=CARTESIAN_POINT('Ctrl Pts',(55.6372365277963,19.1097686048313,8.4642393956039));
#23622=CARTESIAN_POINT('Ctrl Pts',(55.6461688944084,19.1128008027511,8.46484333739955));
#23623=CARTESIAN_POINT('Ctrl Pts',(55.6511269202628,19.1145056920213,8.46517785503626));
#23624=CARTESIAN_POINT('Ctrl Pts',(55.6656898017097,19.1195776436002,8.46615848566965));
#23625=CARTESIAN_POINT('Ctrl Pts',(55.6752758479297,19.1229987506424,8.46680151697287));
#23626=CARTESIAN_POINT('Ctrl Pts',(55.7505634683038,19.1505191397754,8.47183541923421));
#23627=CARTESIAN_POINT('Ctrl Pts',(55.8149893950069,19.1779902543872,8.47604509441022));
#23628=CARTESIAN_POINT('Ctrl Pts',(56.0302021138878,19.2834629651191,8.4901952796307));
#23629=CARTESIAN_POINT('Ctrl Pts',(56.1724070251791,19.3772615734261,8.49976134008208));
#23630=CARTESIAN_POINT('Ctrl Pts',(56.3391834407498,19.5207606619325,8.5130153521124));
#23631=CARTESIAN_POINT('Ctrl Pts',(56.3760805099183,19.5550214225224,8.51609464217308));
#23632=CARTESIAN_POINT('Ctrl Pts',(56.4212583621677,19.6002723327611,8.52008236633211));
#23633=CARTESIAN_POINT('Ctrl Pts',(56.4307773185375,19.6100039119936,8.52093551795479));
#23634=CARTESIAN_POINT('Ctrl Pts',(56.4459317975964,19.6258175055055,8.52231523675366));
#23635=CARTESIAN_POINT('Ctrl Pts',(56.4516304125659,19.6318386668867,8.52283906160205));
#23636=CARTESIAN_POINT('Ctrl Pts',(56.4624198249165,19.6433820629601,8.52384053792747));
#23637=CARTESIAN_POINT('Ctrl Pts',(56.4675173021618,19.6488978807161,8.52431789137474));
#23638=CARTESIAN_POINT('Ctrl Pts',(56.4791036524311,19.6615780263406,8.52541264935526));
#23639=CARTESIAN_POINT('Ctrl Pts',(56.4855718039228,19.6687609515334,8.52603091313816));
#23640=CARTESIAN_POINT('Ctrl Pts',(56.502344177446,19.6876612464348,8.52765301605488));
#23641=CARTESIAN_POINT('Ctrl Pts',(56.5125634059593,19.6994528260736,8.52866034571494));
#23642=CARTESIAN_POINT('Ctrl Pts',(56.6013026288582,19.8043063555221,8.53757888215547));
#23643=CARTESIAN_POINT('Ctrl Pts',(56.6712729892373,19.904239787237,8.5458368146718));
#23644=CARTESIAN_POINT('Ctrl Pts',(56.790711489939,20.1131403271629,8.56252145612563));
#23645=CARTESIAN_POINT('Ctrl Pts',(56.8403846181662,20.2214417561895,8.5709033252617));
#23646=CARTESIAN_POINT('Ctrl Pts',(56.8952961378108,20.376346002623,8.58210457839388));
#23647=CARTESIAN_POINT('Ctrl Pts',(56.9090100793399,20.4196785325523,8.58515529264944));
#23648=CARTESIAN_POINT('Ctrl Pts',(56.923617085572,20.471981606668,8.58871024712029));
#23649=CARTESIAN_POINT('Ctrl Pts',(56.9259442255193,20.4805339637347,8.5892875159814));
#23650=CARTESIAN_POINT('Ctrl Pts',(56.9294679126777,20.4938329404382,8.59017864027216));
#23651=CARTESIAN_POINT('Ctrl Pts',(56.9307040877944,20.4985688034615,8.59049469500652));
#23652=CARTESIAN_POINT('Ctrl Pts',(56.9329648405286,20.5073622018794,8.5910790993988));
#23653=CARTESIAN_POINT('Ctrl Pts',(56.9339940742078,20.511418383159,8.59134770499359));
#23654=CARTESIAN_POINT('Ctrl Pts',(56.9363078023734,20.5206585981959,8.59195743154538));
#23655=CARTESIAN_POINT('Ctrl Pts',(56.9375842456032,20.5258445636657,8.59229808789103));
#23656=CARTESIAN_POINT('Ctrl Pts',(56.9408548516365,20.5393662344828,8.59318242827497));
#23657=CARTESIAN_POINT('Ctrl Pts',(56.9428161710456,20.5477098798375,8.59372429174151));
#23658=CARTESIAN_POINT('Ctrl Pts',(56.9555329374395,20.603417713735,8.59731825910798));
#23659=CARTESIAN_POINT('Ctrl Pts',(56.9646101457994,20.6511527400874,8.60028312388294));
#23660=CARTESIAN_POINT('Ctrl Pts',(56.9828747253291,20.7708790467991,8.60754180860352));
#23661=CARTESIAN_POINT('Ctrl Pts',(56.989894882159,20.8431300449526,8.6117655217173));
#23662=CARTESIAN_POINT('Ctrl Pts',(56.9976909662492,21.0272357279495,8.62246337546874));
#23663=CARTESIAN_POINT('Ctrl Pts',(56.9930308699611,21.1390575238036,8.6289105777023));
#23664=CARTESIAN_POINT('Ctrl Pts',(56.9718463871838,21.3068253484483,8.6390457916876));
#23665=CARTESIAN_POINT('Ctrl Pts',(56.9622056810899,21.3634114747572,8.64254291432021));
#23666=CARTESIAN_POINT('Ctrl Pts',(56.947158695099,21.4333608157624,8.64700117597994));
#23667=CARTESIAN_POINT('Ctrl Pts',(56.9440293846614,21.4471893510382,8.64788916234444));
#23668=CARTESIAN_POINT('Ctrl Pts',(56.9388100093969,21.4691630821336,8.64931124539091));
#23669=CARTESIAN_POINT('Ctrl Pts',(56.9368153569075,21.4773306190817,8.64984227415833));
#23670=CARTESIAN_POINT('Ctrl Pts',(56.932949860111,21.492735504625,8.65084858882708));
#23671=CARTESIAN_POINT('Ctrl Pts',(56.931089846383,21.499975441319,8.65132351777365));
#23672=CARTESIAN_POINT('Ctrl Pts',(56.9267921078319,21.5163221969054,8.65240041308718));
#23673=CARTESIAN_POINT('Ctrl Pts',(56.9243304417408,21.5254224812113,8.6530031454815));
#23674=CARTESIAN_POINT('Ctrl Pts',(56.9178297183122,21.5487957376671,8.654559671652));
#23675=CARTESIAN_POINT('Ctrl Pts',(56.9136958533978,21.563041518063,8.65551652052281));
#23676=CARTESIAN_POINT('Ctrl Pts',(56.8847508403948,21.6587863625304,8.66200386829715));
#23677=CARTESIAN_POINT('Ctrl Pts',(56.8549028676035,21.7386589775971,8.66769851550477));
#23678=CARTESIAN_POINT('Ctrl Pts',(56.7704463885792,21.9269491828465,8.68180497258093));
#23679=CARTESIAN_POINT('Ctrl Pts',(56.7108744673618,22.0327730985579,8.69032922898264));
#23680=CARTESIAN_POINT('Ctrl Pts',(56.6011321564454,22.191890848665,8.70372904869594));
#23681=CARTESIAN_POINT('Ctrl Pts',(56.5569956646777,22.2489974488875,8.70866978976218));
#23682=CARTESIAN_POINT('Ctrl Pts',(56.5002911599855,22.3146742295513,8.71440522798627));
#23683=CARTESIAN_POINT('Ctrl Pts',(56.4906016446421,22.3256502788447,8.71536558289372));
#23684=CARTESIAN_POINT('Ctrl Pts',(56.4767802436842,22.3409636541807,8.71670681956132));
#23685=CARTESIAN_POINT('Ctrl Pts',(56.4727486056412,22.3453902618937,8.71709469400604));
#23686=CARTESIAN_POINT('Ctrl Pts',(56.4658059340686,22.3529444853584,8.71775680220727));
#23687=CARTESIAN_POINT('Ctrl Pts',(56.4629046892727,22.3560810035931,8.71803176282822));
#23688=CARTESIAN_POINT('Ctrl Pts',(56.4568847852795,22.362547282515,8.71859869650468));
#23689=CARTESIAN_POINT('Ctrl Pts',(56.4537647637878,22.3658756851386,8.71889056223909));
#23690=CARTESIAN_POINT('Ctrl Pts',(56.445585643216,22.3745413015623,8.71965066097602));
#23691=CARTESIAN_POINT('Ctrl Pts',(56.4405083442694,22.3798613537975,8.72011752111943));
#23692=CARTESIAN_POINT('Ctrl Pts',(56.4196502942204,22.4014760582974,8.72201581206585));
#23693=CARTESIAN_POINT('Ctrl Pts',(56.403620870934,22.4175297717299,8.72342922169651));
#23694=CARTESIAN_POINT('Ctrl Pts',(56.287187640355,22.530227292239,8.73340821824288));
#23695=CARTESIAN_POINT('Ctrl Pts',(56.1771614556021,22.6163998289023,8.7413638884873));
#23696=CARTESIAN_POINT('Ctrl Pts',(55.9988968815992,22.728082497975,8.7535937769187));
#23697=CARTESIAN_POINT('Ctrl Pts',(55.9367912107991,22.7625224599454,8.75774512955749));
#23698=CARTESIAN_POINT('Ctrl Pts',(55.818387456376,22.8201529311676,8.76562069101969));
#23699=CARTESIAN_POINT('Ctrl Pts',(55.7626090740419,22.8442182710925,8.76931545442381));
#23700=CARTESIAN_POINT('Ctrl Pts',(55.6923237372138,22.8708083127928,8.77399643514121));
#23701=CARTESIAN_POINT('Ctrl Pts',(55.6787688702862,22.8757688300408,8.77490024145092));
#23702=CARTESIAN_POINT('Ctrl Pts',(55.6571763113675,22.8834061168609,8.77634217499607));
#23703=CARTESIAN_POINT('Ctrl Pts',(55.649173176725,22.8861796012813,8.77687709086558));
#23704=CARTESIAN_POINT('Ctrl Pts',(55.6340730904238,22.8913050452776,8.77788735158136));
#23705=CARTESIAN_POINT('Ctrl Pts',(55.6269800875571,22.8936682459199,8.77836231547541));
#23706=CARTESIAN_POINT('Ctrl Pts',(55.6109803514363,22.8988991877287,8.7794346985187));
#23707=CARTESIAN_POINT('Ctrl Pts',(55.6020664363841,22.9017442299764,8.78003285136743));
#23708=CARTESIAN_POINT('Ctrl Pts',(55.5792097578523,22.9088625609522,8.78156854137682));
#23709=CARTESIAN_POINT('Ctrl Pts',(55.5652397433671,22.9130458002811,8.78250898928305));
#23710=CARTESIAN_POINT('Ctrl Pts',(55.4759728459328,22.9387131177805,8.78853110534031));
#23711=CARTESIAN_POINT('Ctrl Pts',(55.3995210587367,22.9558984917152,8.79375032686555));
#23712=CARTESIAN_POINT('Ctrl Pts',(55.269895633711,22.9771191115937,8.80269640197856));
#23713=CARTESIAN_POINT('Ctrl Pts',(55.2172477843832,22.9835921617255,8.80635502660011));
#23714=CARTESIAN_POINT('Ctrl Pts',(55.1644479310504,22.9879598689293,8.81003518437327));
#23715=CARTESIAN_POINT('Origin',(55.,21.,6.22095488139522));
#23716=CARTESIAN_POINT('',(55.1644488239152,22.9879597950695,9.76988214123148));
#23717=CARTESIAN_POINT('',(55.1644483514339,22.9879598341543,9.61229346745724));
#23718=CARTESIAN_POINT('',(55.1644483516311,22.987959834138,6.22095488139522));
#23719=CARTESIAN_POINT('',(53.0052507447458,20.9982762938427,9.17962824983008));
#23720=CARTESIAN_POINT('Ctrl Pts',(55.1644488239152,22.9879597950695,9.76988214123148));
#23721=CARTESIAN_POINT('Ctrl Pts',(55.2474358169254,22.981094911064,9.76424197462399));
#23722=CARTESIAN_POINT('Ctrl Pts',(55.3299662031272,22.9690359088409,9.75847082587752));
#23723=CARTESIAN_POINT('Ctrl Pts',(55.5350448108733,22.9257940103328,9.74386339208412));
#23724=CARTESIAN_POINT('Ctrl Pts',(55.6557960150322,22.8880923220085,9.73500686785206));
#23725=CARTESIAN_POINT('Ctrl Pts',(55.7865152809458,22.8332110941054,9.72561977685455));
#23726=CARTESIAN_POINT('Ctrl Pts',(55.8007778150162,22.8270260341522,9.72459866881045));
#23727=CARTESIAN_POINT('Ctrl Pts',(55.8207325538242,22.8180939299511,9.72317587753889));
#23728=CARTESIAN_POINT('Ctrl Pts',(55.8264858081968,22.8154857957321,9.72276635504612));
#23729=CARTESIAN_POINT('Ctrl Pts',(55.8357772999726,22.8112203430816,9.72210621116057));
#23730=CARTESIAN_POINT('Ctrl Pts',(55.8393231710697,22.8095799074625,9.7218545756369));
#23731=CARTESIAN_POINT('Ctrl Pts',(55.8468201482237,22.8060847847211,9.72132320228721));
#23732=CARTESIAN_POINT('Ctrl Pts',(55.8507700316668,22.8042275263844,9.72104362977629));
#23733=CARTESIAN_POINT('Ctrl Pts',(55.8605365230152,22.7995960611537,9.72035324505411));
#23734=CARTESIAN_POINT('Ctrl Pts',(55.8663459031227,22.7968065754721,9.7199433668461));
#23735=CARTESIAN_POINT('Ctrl Pts',(55.8879724378284,22.7862929075207,9.71842006386957));
#23736=CARTESIAN_POINT('Ctrl Pts',(55.9037012002137,22.7783873573699,9.71731728546934));
#23737=CARTESIAN_POINT('Ctrl Pts',(55.9431738678502,22.7578887455393,9.71455756444242));
#23738=CARTESIAN_POINT('Ctrl Pts',(55.9667723176467,22.7450218381241,9.71291491478273));
#23739=CARTESIAN_POINT('Ctrl Pts',(56.1435284019199,22.6439599284703,9.70061187828319));
#23740=CARTESIAN_POINT('Ctrl Pts',(56.2846240314052,22.5362337799521,9.69072815261629));
#23741=CARTESIAN_POINT('Ctrl Pts',(56.4306772155898,22.3903490240591,9.67847587761321));
#23742=CARTESIAN_POINT('Ctrl Pts',(56.4511961516365,22.3689183049465,9.676701645126));
#23743=CARTESIAN_POINT('Ctrl Pts',(56.5023842136163,22.3130109556065,9.67212420401288));
#23744=CARTESIAN_POINT('Ctrl Pts',(56.532347538901,22.2779149461626,9.6692977715779));
#23745=CARTESIAN_POINT('Ctrl Pts',(56.5696233429099,22.2310560852789,9.66556445982336));
#23746=CARTESIAN_POINT('Ctrl Pts',(56.5780693846057,22.2202104433644,9.66470310064605));
#23747=CARTESIAN_POINT('Ctrl Pts',(56.5914455021725,22.2026628687031,9.66331336621481));
#23748=CARTESIAN_POINT('Ctrl Pts',(56.5964470156194,22.1960157545216,9.66278780918401));
#23749=CARTESIAN_POINT('Ctrl Pts',(56.6058798704214,22.1833147040329,9.66178516108847));
#23750=CARTESIAN_POINT('Ctrl Pts',(56.6103189311115,22.177266658233,9.66130838217501));
#23751=CARTESIAN_POINT('Ctrl Pts',(56.6203649879426,22.1634161695281,9.66021795587926));
#23752=CARTESIAN_POINT('Ctrl Pts',(56.6259499066247,22.1555980155208,9.65960347210462));
#23753=CARTESIAN_POINT('Ctrl Pts',(56.6429365338391,22.1314520320584,9.65770861135957));
#23754=CARTESIAN_POINT('Ctrl Pts',(56.6541501032143,22.1149939656289,9.65642114057298));
#23755=CARTESIAN_POINT('Ctrl Pts',(56.7457084598481,21.9761928106598,9.64559336508185));
#23756=CARTESIAN_POINT('Ctrl Pts',(56.812594561048,21.845538714214,9.63554515303679));
#23757=CARTESIAN_POINT('Ctrl Pts',(56.9089178011617,21.5921398840548,9.61664882556592));
#23758=CARTESIAN_POINT('Ctrl Pts',(56.942215883163,21.4715927667568,9.60789722510685));
#23759=CARTESIAN_POINT('Ctrl Pts',(56.9667614392938,21.3333476141695,9.59859970133848));
#23760=CARTESIAN_POINT('Ctrl Pts',(56.9693097130607,21.3179472931397,9.59757433448284));
#23761=CARTESIAN_POINT('Ctrl Pts',(56.9726366329678,21.2962639231247,9.5961466534224));
#23762=CARTESIAN_POINT('Ctrl Pts',(56.9735664740676,21.2900051257218,9.59573642979091));
#23763=CARTESIAN_POINT('Ctrl Pts',(56.9750225436277,21.279872816958,9.59507546040254));
#23764=CARTESIAN_POINT('Ctrl Pts',(56.9755671857392,21.2760020593865,9.59482369570737));
#23765=CARTESIAN_POINT('Ctrl Pts',(56.9766955732899,21.26780814571,9.59429234152571));
#23766=CARTESIAN_POINT('Ctrl Pts',(56.9772765219454,21.2634846273082,9.5940129159934));
#23767=CARTESIAN_POINT('Ctrl Pts',(56.9786790485502,21.2527808673986,9.59332339749371));
#23768=CARTESIAN_POINT('Ctrl Pts',(56.979483963707,21.2463984258503,9.59291423334154));
#23769=CARTESIAN_POINT('Ctrl Pts',(56.9823663404423,21.2226169178665,9.59139665701355));
#23770=CARTESIAN_POINT('Ctrl Pts',(56.9842454658417,21.2051940076959,9.59029878776543));
#23771=CARTESIAN_POINT('Ctrl Pts',(56.9884088527083,21.1611559738872,9.58755385706965));
#23772=CARTESIAN_POINT('Ctrl Pts',(56.9903886291186,21.1345149033365,9.5859208942389));
#23773=CARTESIAN_POINT('Ctrl Pts',(57.0012374766212,20.9341354214146,9.57379238754803));
#23774=CARTESIAN_POINT('Ctrl Pts',(56.987880697524,20.759934918808,9.56405313362454));
#23775=CARTESIAN_POINT('Ctrl Pts',(56.9458918179942,20.5601816403046,9.5519569544631));
#23776=CARTESIAN_POINT('Ctrl Pts',(56.9390276996911,20.53084477362,9.55015823917536));
#23777=CARTESIAN_POINT('Ctrl Pts',(56.9194413860788,20.4549283736556,9.54543142879155));
#23778=CARTESIAN_POINT('Ctrl Pts',(56.90568844675,20.4086377740589,9.54247720801513));
#23779=CARTESIAN_POINT('Ctrl Pts',(56.88580878461,20.349655503763,9.5385976273945));
#23780=CARTESIAN_POINT('Ctrl Pts',(56.8812078832709,20.3364643038237,9.53772243070247));
#23781=CARTESIAN_POINT('Ctrl Pts',(56.8736302293252,20.3154509883344,9.53631568562753));
#23782=CARTESIAN_POINT('Ctrl Pts',(56.8707420971984,20.3075972357615,9.53578708162576));
#23783=CARTESIAN_POINT('Ctrl Pts',(56.8654376013774,20.2934481009899,9.53482953734228));
#23784=CARTESIAN_POINT('Ctrl Pts',(56.8630385577829,20.2871463256661,9.53440118123162));
#23785=CARTESIAN_POINT('Ctrl Pts',(56.857308563916,20.2723213620472,9.53338896403459));
#23786=CARTESIAN_POINT('Ctrl Pts',(56.8539508457987,20.2638087487069,9.53280421193344));
#23787=CARTESIAN_POINT('Ctrl Pts',(56.843954889813,20.2389687435305,9.53108737416788));
#23788=CARTESIAN_POINT('Ctrl Pts',(56.8371588224166,20.2227062092671,9.52994999600638));
#23789=CARTESIAN_POINT('Ctrl Pts',(56.8212816287692,20.1860849763646,9.52735761091268));
#23790=CARTESIAN_POINT('Ctrl Pts',(56.8120730583125,20.1657844389894,9.52589841598972));
#23791=CARTESIAN_POINT('Ctrl Pts',(56.7807321222224,20.0996611701481,9.52107126168567));
#23792=CARTESIAN_POINT('Ctrl Pts',(56.7571878830396,20.0545334872926,9.5176574354516));
#23793=CARTESIAN_POINT('Ctrl Pts',(56.6700747495815,19.902079111676,9.50571436899782));
#23794=CARTESIAN_POINT('Ctrl Pts',(56.5981889535416,19.7998469853912,9.49695541440072));
#23795=CARTESIAN_POINT('Ctrl Pts',(56.4622906643107,19.6406259759884,9.48241776307868));
#23796=CARTESIAN_POINT('Ctrl Pts',(56.4032925020193,19.5798009732569,9.47660656345379));
#23797=CARTESIAN_POINT('Ctrl Pts',(56.3328967828005,19.5159103847815,9.47036380594232));
#23798=CARTESIAN_POINT('Ctrl Pts',(56.3251374133022,19.5089779791453,9.46968449539547));
#23799=CARTESIAN_POINT('Ctrl Pts',(56.3133527839832,19.4986139754389,9.46866643641604));
#23800=CARTESIAN_POINT('Ctrl Pts',(56.3093676817323,19.4951372801671,9.4683244905446));
#23801=CARTESIAN_POINT('Ctrl Pts',(56.302205113131,19.4889384821466,9.46771411850456));
#23802=CARTESIAN_POINT('Ctrl Pts',(56.2990328770418,19.4862104991774,9.46744526448588));
#23803=CARTESIAN_POINT('Ctrl Pts',(56.2920963941728,19.4802832916158,9.46686059499662));
#23804=CARTESIAN_POINT('Ctrl Pts',(56.2883288450662,19.4770880676076,9.46654507047809));
#23805=CARTESIAN_POINT('Ctrl Pts',(56.2776108833798,19.4680665008374,9.46565309748884));
#23806=CARTESIAN_POINT('Ctrl Pts',(56.2706324445029,19.4622734269091,9.46507901135552));
#23807=CARTESIAN_POINT('Ctrl Pts',(56.2252697957215,19.4251357884157,9.46138831049852));
#23808=CARTESIAN_POINT('Ctrl Pts',(56.18576485171,19.3951803885339,9.45836278077961));
#23809=CARTESIAN_POINT('Ctrl Pts',(56.026363813878,19.2834152898498,9.44669648244644));
#23810=CARTESIAN_POINT('Ctrl Pts',(55.8988040469977,19.2133151330815,9.43848216740319));
#23811=CARTESIAN_POINT('Ctrl Pts',(55.6799441041773,19.1224652253405,9.42455722871241));
#23812=CARTESIAN_POINT('Ctrl Pts',(55.5928087026705,19.093160864219,9.4190589646045));
#23813=CARTESIAN_POINT('Ctrl Pts',(55.4893983604155,19.0661583114225,9.41242120676643));
#23814=CARTESIAN_POINT('Ctrl Pts',(55.4747825213292,19.0625181369568,9.41148067931672));
#23815=CARTESIAN_POINT('Ctrl Pts',(55.4508811319091,19.0568520228991,9.409938154152));
#23816=CARTESIAN_POINT('Ctrl Pts',(55.4416196845429,19.0547262647087,9.40933936011487));
#23817=CARTESIAN_POINT('Ctrl Pts',(55.4250312350394,19.0510433260266,9.40826475000625));
#23818=CARTESIAN_POINT('Ctrl Pts',(55.4177099370897,19.0494610812033,9.40778974598518));
#23819=CARTESIAN_POINT('Ctrl Pts',(55.4021805079563,19.0461963752178,9.406780587133));
#23820=CARTESIAN_POINT('Ctrl Pts',(55.3939703598776,19.0445243245702,9.40624610997406));
#23821=CARTESIAN_POINT('Ctrl Pts',(55.3719955131262,19.0401930102414,9.40481289532779));
#23822=CARTESIAN_POINT('Ctrl Pts',(55.3582131057903,19.0376270861318,9.4039112105417));
#23823=CARTESIAN_POINT('Ctrl Pts',(55.290034822155,19.0256762374187,9.39943622337279));
#23824=CARTESIAN_POINT('Ctrl Pts',(55.2352973079836,19.0184075322534,9.39579680434988));
#23825=CARTESIAN_POINT('Ctrl Pts',(54.9702166105591,18.9943446939053,9.37793664448879));
#23826=CARTESIAN_POINT('Ctrl Pts',(54.758452837742,19.0087263861018,9.36277444052429));
#23827=CARTESIAN_POINT('Ctrl Pts',(54.526047721561,19.062177553013,9.34675778972842));
#23828=CARTESIAN_POINT('Ctrl Pts',(54.4993272457785,19.068908708993,9.34492908193437));
#23829=CARTESIAN_POINT('Ctrl Pts',(54.4651199828682,19.0782836907694,9.34261183692565));
#23830=CARTESIAN_POINT('Ctrl Pts',(54.4574990705697,19.0804211523044,9.3420971254225));
#23831=CARTESIAN_POINT('Ctrl Pts',(54.4453853740963,19.0838966232884,9.34128165065329));
#23832=CARTESIAN_POINT('Ctrl Pts',(54.4408843317689,19.0852051796202,9.34097923820133));
#23833=CARTESIAN_POINT('Ctrl Pts',(54.432331295327,19.087724473857,9.34040576365606));
#23834=CARTESIAN_POINT('Ctrl Pts',(54.4282785855041,19.0889322171496,9.34013454503861));
#23835=CARTESIAN_POINT('Ctrl Pts',(54.4187732929073,19.0917978212293,9.3394995799105));
#23836=CARTESIAN_POINT('Ctrl Pts',(54.4133239375802,19.0934661713425,9.33913644683079));
#23837=CARTESIAN_POINT('Ctrl Pts',(54.3955362568687,19.0989954541472,9.33795380122264));
#23838=CARTESIAN_POINT('Ctrl Pts',(54.3832280035083,19.1029530777621,9.33713970004766));
#23839=CARTESIAN_POINT('Ctrl Pts',(54.3539766718718,19.1126734099067,9.33521312505988));
#23840=CARTESIAN_POINT('Ctrl Pts',(54.3370706999954,19.1185450872518,9.33410624872874));
#23841=CARTESIAN_POINT('Ctrl Pts',(54.2746681863858,19.1411639326497,9.33003722157717));
#23842=CARTESIAN_POINT('Ctrl Pts',(54.2297050930297,19.1593413760665,9.32713821286093));
#23843=CARTESIAN_POINT('Ctrl Pts',(54.0322479865603,19.2476729732111,9.31437116845775));
#23844=CARTESIAN_POINT('Ctrl Pts',(53.8883145717822,19.3352622335131,9.30490591190842));
#23845=CARTESIAN_POINT('Ctrl Pts',(53.7173519639219,19.4714656912236,9.29175165587053));
#23846=CARTESIAN_POINT('Ctrl Pts',(53.6788829729788,19.5045896020782,9.28865025264508));
#23847=CARTESIAN_POINT('Ctrl Pts',(53.631310531202,19.5488215930287,9.28460274158093));
#23848=CARTESIAN_POINT('Ctrl Pts',(53.6210040864466,19.5586118202514,9.28371244538345));
#23849=CARTESIAN_POINT('Ctrl Pts',(53.604759610295,19.5743763663046,9.28228713331507));
#23850=CARTESIAN_POINT('Ctrl Pts',(53.5987531366276,19.5802797055828,9.28175520201736));
#23851=CARTESIAN_POINT('Ctrl Pts',(53.5880110719228,19.590971900264,9.28079488667754));
#23852=CARTESIAN_POINT('Ctrl Pts',(53.5832619840666,19.595747062939,9.28036711066229));
#23853=CARTESIAN_POINT('Ctrl Pts',(53.5735302105996,19.6056318859842,9.2794838011594));
#23854=CARTESIAN_POINT('Ctrl Pts',(53.5685505895157,19.6107444149851,9.27902814253846));
#23855=CARTESIAN_POINT('Ctrl Pts',(53.5540656858923,19.6257764851855,9.27769180155567));
#23856=CARTESIAN_POINT('Ctrl Pts',(53.5446354701373,19.635767476224,9.27680789832642));
#23857=CARTESIAN_POINT('Ctrl Pts',(53.4970643361312,19.6872220740788,9.27227656298673));
#23858=CARTESIAN_POINT('Ctrl Pts',(53.4605924361625,19.7301871011363,9.26855988781367));
#23859=CARTESIAN_POINT('Ctrl Pts',(53.3686124024927,19.8483375392624,9.25850428449512));
#23860=CARTESIAN_POINT('Ctrl Pts',(53.3164878807583,19.9259722658519,9.25205664760387));
#23861=CARTESIAN_POINT('Ctrl Pts',(53.2045285705031,20.1210205292247,9.23639150700404));
#23862=CARTESIAN_POINT('Ctrl Pts',(53.1504939919096,20.2412801941238,9.2271449203542));
#23863=CARTESIAN_POINT('Ctrl Pts',(53.1038361262805,20.3804653685814,9.21742896424449));
#23864=CARTESIAN_POINT('Ctrl Pts',(53.0991503163124,20.3949949508408,9.21642649266329));
#23865=CARTESIAN_POINT('Ctrl Pts',(53.0927757414616,20.4155665105,9.21502510022441));
#23866=CARTESIAN_POINT('Ctrl Pts',(53.0909480986891,20.4215644230553,9.21461864401671));
#23867=CARTESIAN_POINT('Ctrl Pts',(53.0879187286948,20.4316768998494,9.21393707138117));
#23868=CARTESIAN_POINT('Ctrl Pts',(53.0867019378591,20.4357868657837,9.2136610921622));
#23869=CARTESIAN_POINT('Ctrl Pts',(53.0842448293616,20.4441856246199,9.21309926909644));
#23870=CARTESIAN_POINT('Ctrl Pts',(53.0830056479758,20.4484747068629,9.21281349154791));
#23871=CARTESIAN_POINT('Ctrl Pts',(53.0798854177719,20.4594120879097,9.21208754622422));
#23872=CARTESIAN_POINT('Ctrl Pts',(53.0780244728101,20.4660661315871,9.21164853004105));
#23873=CARTESIAN_POINT('Ctrl Pts',(53.074059906336,20.4805312784615,9.21069959286802));
#23874=CARTESIAN_POINT('Ctrl Pts',(53.0719691400743,20.4883458147624,9.21019037325148));
#23875=CARTESIAN_POINT('Ctrl Pts',(53.0660136007062,20.511160455891,9.20871309087908));
#23876=CARTESIAN_POINT('Ctrl Pts',(53.0622758466901,20.5261934678134,9.20775147361118));
#23877=CARTESIAN_POINT('Ctrl Pts',(53.0233269900749,20.6910196695038,9.19732134383069));
#23878=CARTESIAN_POINT('Ctrl Pts',(53.0053837347156,20.8443743993901,9.188605506415));
#23879=CARTESIAN_POINT('Ctrl Pts',(53.0052507447458,20.9982762938427,9.17962824983008));
#23880=CARTESIAN_POINT('Ctrl Pts',(53.0052507434434,20.9982778017065,9.17962816187482));
#23881=CARTESIAN_POINT('Ctrl Pts',(53.0051828401937,21.0769272565001,9.1750404572398));
#23882=CARTESIAN_POINT('Ctrl Pts',(53.0097664109837,21.1555076732957,9.17040293054525));
#23883=CARTESIAN_POINT('Ctrl Pts',(53.0230355497044,21.2680305353932,9.1635329928163));
#23884=CARTESIAN_POINT('Ctrl Pts',(53.0279907401557,21.3023376729557,9.16140790578901));
#23885=CARTESIAN_POINT('Ctrl Pts',(53.0358351204672,21.3481726671077,9.1585194906103));
#23886=CARTESIAN_POINT('Ctrl Pts',(53.0379372937375,21.3598302479825,9.15778056533338));
#23887=CARTESIAN_POINT('Ctrl Pts',(53.0416739774596,21.3795448960094,9.15652332754926));
#23888=CARTESIAN_POINT('Ctrl Pts',(53.0432547111062,21.3876119319661,9.15600671209537));
#23889=CARTESIAN_POINT('Ctrl Pts',(53.0462742901041,21.4025325483763,9.15504706849639));
#23890=CARTESIAN_POINT('Ctrl Pts',(53.0476994550759,21.4093887910904,9.15460448058297));
#23891=CARTESIAN_POINT('Ctrl Pts',(53.0507238080268,21.4235634612059,9.15368605190557));
#23892=CARTESIAN_POINT('Ctrl Pts',(53.0523281760702,21.4308806586773,9.15321005217137));
#23893=CARTESIAN_POINT('Ctrl Pts',(53.0560626777143,21.4474658436589,9.15212677146438));
#23894=CARTESIAN_POINT('Ctrl Pts',(53.0582179352971,21.4567279302136,9.15151869424538));
#23895=CARTESIAN_POINT('Ctrl Pts',(53.0639635059175,21.4806431701988,9.14994037836016));
#23896=CARTESIAN_POINT('Ctrl Pts',(53.0676539226297,21.4952714205266,9.14896694714848));
#23897=CARTESIAN_POINT('Ctrl Pts',(53.0951880963049,21.5994172485215,9.14197780468443));
#23898=CARTESIAN_POINT('Ctrl Pts',(53.1250729235694,21.6872070146052,9.13576682073755));
#23899=CARTESIAN_POINT('Ctrl Pts',(53.1897511065282,21.8411649675577,9.12431160868321));
#23900=CARTESIAN_POINT('Ctrl Pts',(53.2223698334615,21.9080691297876,9.11912867220464));
#23901=CARTESIAN_POINT('Ctrl Pts',(53.2927277785203,22.0339879852313,9.10906759369945));
#23902=CARTESIAN_POINT('Ctrl Pts',(53.329992224216,22.0931534472244,9.10419720451516));
#23903=CARTESIAN_POINT('Ctrl Pts',(53.3987865316909,22.1906241492388,9.0960440760314));
#23904=CARTESIAN_POINT('Ctrl Pts',(53.4287807407972,22.2299355218696,9.09271710116968));
#23905=CARTESIAN_POINT('Ctrl Pts',(53.4659908337132,22.2751181167062,9.08888366975091));
#23906=CARTESIAN_POINT('Ctrl Pts',(53.4718226129579,22.2821014839455,9.08829090823107));
#23907=CARTESIAN_POINT('Ctrl Pts',(53.4808983220537,22.2928194451876,9.0873810520243));
#23908=CARTESIAN_POINT('Ctrl Pts',(53.4841086146754,22.2965821744037,9.08706161268604));
#23909=CARTESIAN_POINT('Ctrl Pts',(53.4900599664645,22.3035053349849,9.08647389584551));
#23910=CARTESIAN_POINT('Ctrl Pts',(53.492796956745,22.3066690668194,9.08620534050696));
#23911=CARTESIAN_POINT('Ctrl Pts',(53.4990113259303,22.3138068528042,9.08559946513332));
#23912=CARTESIAN_POINT('Ctrl Pts',(53.5024945385296,22.3177757170984,9.08526258312509));
#23913=CARTESIAN_POINT('Ctrl Pts',(53.5128631108908,22.3294957396674,9.08426762781139));
#23914=CARTESIAN_POINT('Ctrl Pts',(53.5197933103367,22.3372072447988,9.083612780022));
#23915=CARTESIAN_POINT('Ctrl Pts',(53.5816659592633,22.4049849305818,9.07785180140453));
#23916=CARTESIAN_POINT('Ctrl Pts',(53.6401844158498,22.4616973084398,9.07299206584844));
#23917=CARTESIAN_POINT('Ctrl Pts',(53.7823129006819,22.5834926657165,9.06200781416631));
#23918=CARTESIAN_POINT('Ctrl Pts',(53.8679585648431,22.6458109754695,9.05595091571441));
#23919=CARTESIAN_POINT('Ctrl Pts',(54.0136298890076,22.7350318370136,9.04593301661193));
#23920=CARTESIAN_POINT('Ctrl Pts',(54.0707435092103,22.7662793769604,9.04207055924135));
#23921=CARTESIAN_POINT('Ctrl Pts',(54.1647973677823,22.8119113274246,9.03572091598468));
#23922=CARTESIAN_POINT('Ctrl Pts',(54.2008177053333,22.8280846341323,9.03329202274851));
#23923=CARTESIAN_POINT('Ctrl Pts',(54.2487939292743,22.8479372118482,9.03004930153753));
#23924=CARTESIAN_POINT('Ctrl Pts',(54.2603395659209,22.85258871062,9.029268383939));
#23925=CARTESIAN_POINT('Ctrl Pts',(54.2784532929095,22.8596900384525,9.02804204657741));
#23926=CARTESIAN_POINT('Ctrl Pts',(54.2849921800722,22.8622138719923,9.0275991141178));
#23927=CARTESIAN_POINT('Ctrl Pts',(54.2985389715068,22.8673606983638,9.0266809252215));
#23928=CARTESIAN_POINT('Ctrl Pts',(54.3055485955028,22.8699788224949,9.02620551483901));
#23929=CARTESIAN_POINT('Ctrl Pts',(54.3214224244978,22.8758062023133,9.02512814548741));
#23930=CARTESIAN_POINT('Ctrl Pts',(54.3302949333851,22.8789921642515,9.02452542386294));
#23931=CARTESIAN_POINT('Ctrl Pts',(54.3531673676187,22.8870226738543,9.02297013373542));
#23932=CARTESIAN_POINT('Ctrl Pts',(54.3671990801259,22.8917742999904,9.02201452577132));
#23933=CARTESIAN_POINT('Ctrl Pts',(54.4615267196234,22.9225500590346,9.01557943611792));
#23934=CARTESIAN_POINT('Ctrl Pts',(54.5433412650726,22.9436078897621,9.00993908507125));
#23935=CARTESIAN_POINT('Ctrl Pts',(54.7756036005714,22.9879126892308,8.9937830938481));
#23936=CARTESIAN_POINT('Ctrl Pts',(54.927726568877,22.9992303610272,8.9830021449236));
#23937=CARTESIAN_POINT('Ctrl Pts',(55.1079515180691,22.9920281687318,8.9706680415368));
#23938=CARTESIAN_POINT('Ctrl Pts',(55.1362237077551,22.990294637996,8.96874771432807));
#23939=CARTESIAN_POINT('Ctrl Pts',(55.1644483561882,22.987959833761,8.96685094802472));
#23940=CARTESIAN_POINT('Ctrl Pts',(55.1644479310504,22.9879598689293,8.81003518437327));
#23941=CARTESIAN_POINT('Ctrl Pts',(55.0602828573514,22.9965766076901,8.81729550578455));
#23942=CARTESIAN_POINT('Ctrl Pts',(54.9555267627957,22.9969994905233,8.82464776415277));
#23943=CARTESIAN_POINT('Ctrl Pts',(54.8001413184913,22.9853714186208,8.83530728819776));
#23944=CARTESIAN_POINT('Ctrl Pts',(54.7493015405694,22.9795945148798,8.83875314450029));
#23945=CARTESIAN_POINT('Ctrl Pts',(54.6896973386332,22.9704881166276,8.84270234442929));
#23946=CARTESIAN_POINT('Ctrl Pts',(54.6806684719506,22.9690450838717,8.84329808716922));
#23947=CARTESIAN_POINT('Ctrl Pts',(54.6667607446777,22.9667241108439,8.84421158266041));
#23948=CARTESIAN_POINT('Ctrl Pts',(54.6618748415839,22.965890004045,8.84453170695718));
#23949=CARTESIAN_POINT('Ctrl Pts',(54.6528715016605,22.96431842232,8.84512007622143));
#23950=CARTESIAN_POINT('Ctrl Pts',(54.6487532950705,22.9635862118844,8.84538860362594));
#23951=CARTESIAN_POINT('Ctrl Pts',(54.6394532587541,22.9619024861104,8.8459936798834));
#23952=CARTESIAN_POINT('Ctrl Pts',(54.6342728862875,22.9609433947621,8.84632979607078));
#23953=CARTESIAN_POINT('Ctrl Pts',(54.620917803691,22.9584160778968,8.84719405592738));
#23954=CARTESIAN_POINT('Ctrl Pts',(54.6127489034824,22.9568171707334,8.84772051613693));
#23955=CARTESIAN_POINT('Ctrl Pts',(54.5614680601946,22.9464462139486,8.85101304504314));
#23956=CARTESIAN_POINT('Ctrl Pts',(54.5186426363149,22.9363003043483,8.85370774557413));
#23957=CARTESIAN_POINT('Ctrl Pts',(54.2892830923984,22.8738805644487,8.86801215552247));
#23958=CARTESIAN_POINT('Ctrl Pts',(54.1107798452838,22.7960643456084,8.8787848129137));
#23959=CARTESIAN_POINT('Ctrl Pts',(53.9006595602953,22.6653424175838,8.89365530736729));
#23960=CARTESIAN_POINT('Ctrl Pts',(53.8562045081614,22.6351286997452,8.89693644209995));
#23961=CARTESIAN_POINT('Ctrl Pts',(53.8018559420355,22.5948891945372,8.90115189208636));
#23962=CARTESIAN_POINT('Ctrl Pts',(53.7907729594592,22.5865026553504,8.9020226404251));
#23963=CARTESIAN_POINT('Ctrl Pts',(53.7731726779511,22.5728928821754,8.90342382966811));
#23964=CARTESIAN_POINT('Ctrl Pts',(53.7665988445046,22.5677432452763,8.90395136661294));
#23965=CARTESIAN_POINT('Ctrl Pts',(53.7541879416509,22.5578947416397,8.90495539464881));
#23966=CARTESIAN_POINT('Ctrl Pts',(53.7483446221371,22.5532039541899,8.90543155783345));
#23967=CARTESIAN_POINT('Ctrl Pts',(53.7351190720194,22.5424639023697,8.90651723595808));
#23968=CARTESIAN_POINT('Ctrl Pts',(53.7277535925301,22.5363943912707,8.90712756176496));
#23969=CARTESIAN_POINT('Ctrl Pts',(53.7087675593357,22.5205188384391,8.90871582505917));
#23970=CARTESIAN_POINT('Ctrl Pts',(53.6972152386696,22.5106325159566,8.90969702322558));
#23971=CARTESIAN_POINT('Ctrl Pts',(53.61295242649,22.4368360558758,8.91696538760889));
#23972=CARTESIAN_POINT('Ctrl Pts',(53.544877953502,22.3678500138841,8.92346660530846));
#23973=CARTESIAN_POINT('Ctrl Pts',(53.3908566855825,22.1872056370252,8.93978124369797));
#23974=CARTESIAN_POINT('Ctrl Pts',(53.3112009007468,22.0708663402775,8.94973433659892));
#23975=CARTESIAN_POINT('Ctrl Pts',(53.221210813,21.9040632106936,8.96268211225823));
#23976=CARTESIAN_POINT('Ctrl Pts',(53.1995704370656,21.8601601820237,8.96597427577031));
#23977=CARTESIAN_POINT('Ctrl Pts',(53.1758700770358,21.8072541502299,8.9697705611805));
#23978=CARTESIAN_POINT('Ctrl Pts',(53.1722313380716,21.7989812043107,8.97035933823313));
#23979=CARTESIAN_POINT('Ctrl Pts',(53.1666938807424,21.7861555577526,8.97126433156741));
#23980=CARTESIAN_POINT('Ctrl Pts',(53.1647556669086,21.7816201935892,8.97158285507234));
#23981=CARTESIAN_POINT('Ctrl Pts',(53.161204803451,21.773225247675,8.97216961544013));
#23982=CARTESIAN_POINT('Ctrl Pts',(53.1595874814217,21.769367805741,8.97243812449693));
#23983=CARTESIAN_POINT('Ctrl Pts',(53.1559506165795,21.7606165005101,8.97304480842484));
#23984=CARTESIAN_POINT('Ctrl Pts',(53.1539384181995,21.7557196749461,8.97338253902017));
#23985=CARTESIAN_POINT('Ctrl Pts',(53.1480173183783,21.7411454903343,8.97438270951778));
#23986=CARTESIAN_POINT('Ctrl Pts',(53.1441647733724,21.7314452225663,8.975041871926));
#23987=CARTESIAN_POINT('Ctrl Pts',(53.1081432205923,21.6386300482876,8.98129093449804));
#23988=CARTESIAN_POINT('Ctrl Pts',(53.0814979678095,21.5534659608479,8.98658486183109));
#23989=CARTESIAN_POINT('Ctrl Pts',(53.0239144387665,21.3142273391484,9.00097818624058));
#23990=CARTESIAN_POINT('Ctrl Pts',(53.0053248753638,21.1578692761744,9.00990128748095));
#23991=CARTESIAN_POINT('Ctrl Pts',(53.0052293593294,20.9570860933998,9.02204741246955));
#23992=CARTESIAN_POINT('Ctrl Pts',(53.0066552475153,20.9132372818238,9.02473792250262));
#23993=CARTESIAN_POINT('Ctrl Pts',(53.0104081689307,20.8560068112216,9.02831515112903));
#23994=CARTESIAN_POINT('Ctrl Pts',(53.0114278745639,20.8425497525654,9.02916102115691));
#23995=CARTESIAN_POINT('Ctrl Pts',(53.0132917939263,20.8208734678944,9.03053158129461));
#23996=CARTESIAN_POINT('Ctrl Pts',(53.0140506732978,20.8126471803633,9.03105359058605));
#23997=CARTESIAN_POINT('Ctrl Pts',(53.0155971192309,20.7969502583354,9.03205333699379));
#23998=CARTESIAN_POINT('Ctrl Pts',(53.0163758305301,20.789478878596,9.03253078768805));
#23999=CARTESIAN_POINT('Ctrl Pts',(53.0182574576288,20.772363720409,9.03362825038121));
#24000=CARTESIAN_POINT('Ctrl Pts',(53.0193885941512,20.7627232975127,9.03424914005485));
#24001=CARTESIAN_POINT('Ctrl Pts',(53.0231200578368,20.7328089729646,9.03618443642928));
#24002=CARTESIAN_POINT('Ctrl Pts',(53.0259616040053,20.7125670335537,9.03750638663736));
#24003=CARTESIAN_POINT('Ctrl Pts',(53.0412203424669,20.6148082734827,9.04395305057753));
#24004=CARTESIAN_POINT('Ctrl Pts',(53.0578937853662,20.5380355193413,9.04921004377207));
#24005=CARTESIAN_POINT('Ctrl Pts',(53.1026180129301,20.3782110807948,9.06055287102911));
#24006=CARTESIAN_POINT('Ctrl Pts',(53.131706174058,20.2956163725933,9.06665359953203));
#24007=CARTESIAN_POINT('Ctrl Pts',(53.2069383676496,20.1198169091956,9.07998962500898));
#24008=CARTESIAN_POINT('Ctrl Pts',(53.2551421990155,20.0277511130764,9.08720641913862));
#24009=CARTESIAN_POINT('Ctrl Pts',(53.3187703281887,19.9263386748042,9.095137869918));
#24010=CARTESIAN_POINT('Ctrl Pts',(53.3274073950845,19.9129324459384,9.09618578738727));
#24011=CARTESIAN_POINT('Ctrl Pts',(53.3397253454162,19.8943072902267,9.09763925968634));
#24012=CARTESIAN_POINT('Ctrl Pts',(53.3432716547882,19.8890006795793,9.09805310170421));
#24013=CARTESIAN_POINT('Ctrl Pts',(53.3490358974462,19.8804641837295,9.09871826494411));
#24014=CARTESIAN_POINT('Ctrl Pts',(53.351237947853,19.8772237053252,9.09897063046831));
#24015=CARTESIAN_POINT('Ctrl Pts',(53.3559043584173,19.8704000728906,9.09950173292386));
#24016=CARTESIAN_POINT('Ctrl Pts',(53.3583709140122,19.8668184529106,9.09978031321923));
#24017=CARTESIAN_POINT('Ctrl Pts',(53.3644798354237,19.858009657165,9.10046507889342));
#24018=CARTESIAN_POINT('Ctrl Pts',(53.368135606698,19.8527917554333,9.10087036319758));
#24019=CARTESIAN_POINT('Ctrl Pts',(53.3816959994845,19.8336329180438,9.10235757787664));
#24020=CARTESIAN_POINT('Ctrl Pts',(53.3917551078741,19.8198015331193,9.10342950350796));
#24021=CARTESIAN_POINT('Ctrl Pts',(53.4614684098847,19.726491766176,9.11066181109657));
#24022=CARTESIAN_POINT('Ctrl Pts',(53.5268191609118,19.6514282370647,9.11648802513467));
#24023=CARTESIAN_POINT('Ctrl Pts',(53.7150938578208,19.465271821967,9.13188635193029));
#24024=CARTESIAN_POINT('Ctrl Pts',(53.8466732065391,19.3640887318318,9.14137026587759));
#24025=CARTESIAN_POINT('Ctrl Pts',(54.0071731164936,19.2697526713335,9.15284991809959));
#24026=CARTESIAN_POINT('Ctrl Pts',(54.0252858912514,19.2594847329466,9.15414314593222));
#24027=CARTESIAN_POINT('Ctrl Pts',(54.053326964079,19.2441635297375,9.15614349624497));
#24028=CARTESIAN_POINT('Ctrl Pts',(54.0631427418637,19.2389065847947,9.15684339233716));
#24029=CARTESIAN_POINT('Ctrl Pts',(54.079183825811,19.2304876718798,9.15798687499016));
#24030=CARTESIAN_POINT('Ctrl Pts',(54.0853827165975,19.2272756759996,9.15842868861326));
#24031=CARTESIAN_POINT('Ctrl Pts',(54.0984192082412,19.2206073123949,9.15935775303313));
#24032=CARTESIAN_POINT('Ctrl Pts',(54.1052601029896,19.2171576696808,9.15984523032363));
#24033=CARTESIAN_POINT('Ctrl Pts',(54.1216447020866,19.2090134973813,9.16101275583091));
#24034=CARTESIAN_POINT('Ctrl Pts',(54.131206334138,19.2043557588323,9.16169407085541));
#24035=CARTESIAN_POINT('Ctrl Pts',(54.1639900314562,19.1887090489447,9.16403028173517));
#24036=CARTESIAN_POINT('Ctrl Pts',(54.1873861187847,19.1780927151107,9.16569790883912));
#24037=CARTESIAN_POINT('Ctrl Pts',(54.2441225484733,19.1536579360666,9.16974471321265));
#24038=CARTESIAN_POINT('Ctrl Pts',(54.2776446312157,19.1402870679403,9.17213804879462));
#24039=CARTESIAN_POINT('Ctrl Pts',(54.5030978819956,19.0573764559177,9.18825062367529));
#24040=CARTESIAN_POINT('Ctrl Pts',(54.7043218741102,19.0167578997439,9.20287874953262));
#24041=CARTESIAN_POINT('Ctrl Pts',(54.9419964826815,19.0058061787746,9.21895459278164));
#24042=CARTESIAN_POINT('Ctrl Pts',(54.9758475440011,19.0051089282962,9.22121179612446));
#24043=CARTESIAN_POINT('Ctrl Pts',(55.0181148569268,19.0053145138905,9.22397674756928));
#24044=CARTESIAN_POINT('Ctrl Pts',(55.0265273256589,19.005408652488,9.22452440895585));
#24045=CARTESIAN_POINT('Ctrl Pts',(55.0397845747207,19.0056408960003,9.22538303529213));
#24046=CARTESIAN_POINT('Ctrl Pts',(55.0446297622598,19.0057434383643,9.22569590737434));
#24047=CARTESIAN_POINT('Ctrl Pts',(55.0536265986851,19.0059666501789,9.22627507257861));
#24048=CARTESIAN_POINT('Ctrl Pts',(55.0577782077696,19.0060826267299,9.22654161280454));
#24049=CARTESIAN_POINT('Ctrl Pts',(55.0673205532176,19.0063790238281,9.22715262934781));
#24050=CARTESIAN_POINT('Ctrl Pts',(55.0727109370606,19.0065683420808,9.22749660650284));
#24051=CARTESIAN_POINT('Ctrl Pts',(55.0893840827649,19.0072216476622,9.22855710210797));
#24052=CARTESIAN_POINT('Ctrl Pts',(55.1006639554874,19.0077595883337,9.22926964201022));
#24053=CARTESIAN_POINT('Ctrl Pts',(55.2089600504383,19.0138464086931,9.23606858192566));
#24054=CARTESIAN_POINT('Ctrl Pts',(55.3054669931247,19.026382644399,9.2418063193963));
#24055=CARTESIAN_POINT('Ctrl Pts',(55.569411066746,19.0805043635134,9.25751740813453));
#24056=CARTESIAN_POINT('Ctrl Pts',(55.7329266713993,19.1368020982042,9.2673378305571));
#24057=CARTESIAN_POINT('Ctrl Pts',(55.9096594649216,19.2245627876558,9.27947415646563));
#24058=CARTESIAN_POINT('Ctrl Pts',(55.9319279169679,19.2361496925807,9.28103152929472));
#24059=CARTESIAN_POINT('Ctrl Pts',(55.9625446956151,19.2528221108306,9.28321503672277));
#24060=CARTESIAN_POINT('Ctrl Pts',(55.9710838239005,19.2575537113019,9.283828671662));
#24061=CARTESIAN_POINT('Ctrl Pts',(55.9857564375379,19.2658252814945,9.28489128324927));
#24062=CARTESIAN_POINT('Ctrl Pts',(55.9919064914131,19.2693356135167,9.28533919434151));
#24063=CARTESIAN_POINT('Ctrl Pts',(56.0046051289737,19.2766736723116,9.28626933447792));
#24064=CARTESIAN_POINT('Ctrl Pts',(56.0111508226025,19.2805061476687,9.28675172968762));
#24065=CARTESIAN_POINT('Ctrl Pts',(56.0264466318976,19.2895793200534,9.28788598116039));
#24066=CARTESIAN_POINT('Ctrl Pts',(56.0351786623749,19.2948499417669,9.28853891878499));
#24067=CARTESIAN_POINT('Ctrl Pts',(56.0635755020996,19.3122886870644,9.29068032205804));
#24068=CARTESIAN_POINT('Ctrl Pts',(56.0830685981246,19.3247314658245,9.29217882191706));
#24069=CARTESIAN_POINT('Ctrl Pts',(56.1855396128492,19.3926764901948,9.30021255750873));
#24070=CARTESIAN_POINT('Ctrl Pts',(56.2644679970332,19.4540024334536,9.30696572640259));
#24071=CARTESIAN_POINT('Ctrl Pts',(56.4146819816097,19.5899402971232,9.32095582761771));
#24072=CARTESIAN_POINT('Ctrl Pts',(56.4854495143307,19.6646976543961,9.32818029282559));
#24073=CARTESIAN_POINT('Ctrl Pts',(56.5952461737899,19.8002692940285,9.34024499217286));
#24074=CARTESIAN_POINT('Ctrl Pts',(56.6373235791965,19.8583617326098,9.34513336584363));
#24075=CARTESIAN_POINT('Ctrl Pts',(56.6817449859255,19.9272155372272,9.3505126760969));
#24076=CARTESIAN_POINT('Ctrl Pts',(56.6872373920234,19.9358746808047,9.35118199529146));
#24077=CARTESIAN_POINT('Ctrl Pts',(56.6954435004558,19.9490354347774,9.3521879943068));
#24078=CARTESIAN_POINT('Ctrl Pts',(56.6982064849786,19.9535058927523,9.35252776400843));
#24079=CARTESIAN_POINT('Ctrl Pts',(56.7031357264068,19.9615522456961,9.35313574879399));
#24080=CARTESIAN_POINT('Ctrl Pts',(56.7053084284988,19.9651240626677,9.35340437794755));
#24081=CARTESIAN_POINT('Ctrl Pts',(56.7100360130028,19.9729513004549,9.35399029717136));
#24082=CARTESIAN_POINT('Ctrl Pts',(56.7125862438962,19.9772094273434,9.35430728535708));
#24083=CARTESIAN_POINT('Ctrl Pts',(56.7198093019939,19.9893725465656,9.35520787173452));
#24084=CARTESIAN_POINT('Ctrl Pts',(56.724443547311,19.9973004713793,9.35578903394519));
#24085=CARTESIAN_POINT('Ctrl Pts',(56.7550141846342,20.0504373215417,9.359647385122));
#24086=CARTESIAN_POINT('Ctrl Pts',(56.7792273373102,20.0966201267629,9.36282367694648));
#24087=CARTESIAN_POINT('Ctrl Pts',(56.8730928926753,20.2941084295497,9.37589965084349));
#24088=CARTESIAN_POINT('Ctrl Pts',(56.9254674504142,20.4528783903085,9.38525702384606));
#24089=CARTESIAN_POINT('Ctrl Pts',(56.9708737014861,20.6845371791889,9.39928848378233));
#24090=CARTESIAN_POINT('Ctrl Pts',(56.9806682984673,20.7534001810688,9.4034961820481));
#24091=CARTESIAN_POINT('Ctrl Pts',(56.9881040195518,20.8366925274336,9.40869655404811));
#24092=CARTESIAN_POINT('Ctrl Pts',(56.9892101300842,20.850768751831,9.40957909534679));
#24093=CARTESIAN_POINT('Ctrl Pts',(56.9907908982071,20.8740474375635,9.41104522297326));
#24094=CARTESIAN_POINT('Ctrl Pts',(56.9913514034661,20.8832437081452,9.41162612101356));
#24095=CARTESIAN_POINT('Ctrl Pts',(56.9922505513398,20.8998950916761,9.41268115224679));
#24096=CARTESIAN_POINT('Ctrl Pts',(56.9926111063721,20.9073488895248,9.41315459065557));
#24097=CARTESIAN_POINT('Ctrl Pts',(56.9932956278294,20.9233615014235,9.41417423461002));
#24098=CARTESIAN_POINT('Ctrl Pts',(56.9936063114761,20.9319207046477,9.414720846234));
#24099=CARTESIAN_POINT('Ctrl Pts',(56.9943057091162,20.955350446462,9.41622158666618));
#24100=CARTESIAN_POINT('Ctrl Pts',(56.9945832108337,20.9702235124484,9.41717916670178));
#24101=CARTESIAN_POINT('Ctrl Pts',(56.9951983594208,21.0525634948495,9.42250881270515));
#24102=CARTESIAN_POINT('Ctrl Pts',(56.9922792850737,21.1200037188107,9.42698145556755));
#24103=CARTESIAN_POINT('Ctrl Pts',(56.9702222630708,21.3540497173227,9.44288238969973));
#24104=CARTESIAN_POINT('Ctrl Pts',(56.9335246377157,21.5182646825302,9.45477990699314));
#24105=CARTESIAN_POINT('Ctrl Pts',(56.8585773263293,21.726352881823,9.46994083902021));
#24106=CARTESIAN_POINT('Ctrl Pts',(56.8383963050628,21.7760143876414,9.47355864971153));
#24107=CARTESIAN_POINT('Ctrl Pts',(56.8126013935012,21.8328151662349,9.47764945802753));
#24108=CARTESIAN_POINT('Ctrl Pts',(56.8089117960508,21.8407990448001,9.47822333777473));
#24109=CARTESIAN_POINT('Ctrl Pts',(56.8028675354923,21.853654191791,9.47914523944525));
#24110=CARTESIAN_POINT('Ctrl Pts',(56.8005456969913,21.8585406364357,9.47949516971337));
#24111=CARTESIAN_POINT('Ctrl Pts',(56.796389314544,21.8671969610889,9.48011410321708));
#24112=CARTESIAN_POINT('Ctrl Pts',(56.7945627373398,21.870970563018,9.48038358664463));
#24113=CARTESIAN_POINT('Ctrl Pts',(56.7905975957533,21.8790968835913,9.4809631785986));
#24114=CARTESIAN_POINT('Ctrl Pts',(56.7884550541399,21.8834475656139,9.48127303670872));
#24115=CARTESIAN_POINT('Ctrl Pts',(56.7824443704109,21.8955414828093,9.48213325156417));
#24116=CARTESIAN_POINT('Ctrl Pts',(56.7785416088597,21.9032675312896,9.482681504577));
#24117=CARTESIAN_POINT('Ctrl Pts',(56.7555413856911,21.9480725402264,9.48585486500409));
#24118=CARTESIAN_POINT('Ctrl Pts',(56.7353335566076,21.9845735704633,9.48841581318161));
#24119=CARTESIAN_POINT('Ctrl Pts',(56.6140519481253,22.1882902985709,9.50272240661046));
#24120=CARTESIAN_POINT('Ctrl Pts',(56.4899865186897,22.3405789551896,9.51357470973993));
#24121=CARTESIAN_POINT('Ctrl Pts',(56.3057793110954,22.5089399864189,9.52855564836426));
#24122=CARTESIAN_POINT('Ctrl Pts',(56.2643431466358,22.5438248310436,9.53185864310612));
#24123=CARTESIAN_POINT('Ctrl Pts',(56.2101671787729,22.5857900182673,9.53612657646227));
#24124=CARTESIAN_POINT('Ctrl Pts',(56.1986976254285,22.5944775220362,9.53702734443431));
#24125=CARTESIAN_POINT('Ctrl Pts',(56.1802720054852,22.6081226613883,9.53847052018481));
#24126=CARTESIAN_POINT('Ctrl Pts',(56.1733762018089,22.6131611160572,9.53900977543551));
#24127=CARTESIAN_POINT('Ctrl Pts',(56.1603925859709,22.6225203656348,9.54002361770805));
#24128=CARTESIAN_POINT('Ctrl Pts',(56.1543124423563,22.6268515830938,9.54049779162503));
#24129=CARTESIAN_POINT('Ctrl Pts',(56.1406463943505,22.6364714724732,9.54156230616939));
#24130=CARTESIAN_POINT('Ctrl Pts',(56.133047775967,22.6417417000798,9.54215333693578));
#24131=CARTESIAN_POINT('Ctrl Pts',(56.1104648720599,22.6571732280104,9.543907498452));
#24132=CARTESIAN_POINT('Ctrl Pts',(56.0953789108245,22.6671833569129,9.54507627933058));
#24133=CARTESIAN_POINT('Ctrl Pts',(55.9759476215912,22.7441099185196,9.55430806931044));
#24134=CARTESIAN_POINT('Ctrl Pts',(55.8657252718189,22.8013614109527,9.56272876173517));
#24135=CARTESIAN_POINT('Ctrl Pts',(55.6246755141659,22.8993099311404,9.58078487022611));
#24136=CARTESIAN_POINT('Ctrl Pts',(55.4935003345567,22.9375391560412,9.59041185895706));
#24137=CARTESIAN_POINT('Ctrl Pts',(55.3335268172887,22.9668456738974,9.60132154369132));
#24138=CARTESIAN_POINT('Ctrl Pts',(55.3075121090441,22.9710805429602,9.60306913891539));
#24139=CARTESIAN_POINT('Ctrl Pts',(55.2737130777706,22.9758970902215,9.60529897098501));
#24140=CARTESIAN_POINT('Ctrl Pts',(55.2659999741732,22.9769502215919,9.60580509539952));
#24141=CARTESIAN_POINT('Ctrl Pts',(55.2536624194026,22.9785612530703,9.60661009217361));
#24142=CARTESIAN_POINT('Ctrl Pts',(55.249041931907,22.979148143117,9.60691054363731));
#24143=CARTESIAN_POINT('Ctrl Pts',(55.2402146710695,22.9802379713847,9.6074825339107));
#24144=CARTESIAN_POINT('Ctrl Pts',(55.2360083347193,22.9807436930951,9.60775421922156));
#24145=CARTESIAN_POINT('Ctrl Pts',(55.2260819607302,22.9819050576226,9.60839334167342));
#24146=CARTESIAN_POINT('Ctrl Pts',(55.2203605894581,22.9825493494483,9.60876014451398));
#24147=CARTESIAN_POINT('Ctrl Pts',(55.2014487809749,22.9845961559468,9.60996763573801));
#24148=CARTESIAN_POINT('Ctrl Pts',(55.1882468111938,22.9858919089266,9.61080259174365));
#24149=CARTESIAN_POINT('Ctrl Pts',(55.1715051708299,22.9873666187572,9.61185243912581));
#24150=CARTESIAN_POINT('Ctrl Pts',(55.1679771143424,22.9876679272289,9.61207317488924));
#24151=CARTESIAN_POINT('Ctrl Pts',(55.1644483514339,22.9879598341543,9.61229346745724));
#24152=CARTESIAN_POINT('Origin',(55.,21.,6.22095488139522));
#24153=CARTESIAN_POINT('',(55.1644484221209,22.9879598283069,10.5696416509586));
#24154=CARTESIAN_POINT('',(55.1644480736098,22.9879598571365,10.4094440176549));
#24155=CARTESIAN_POINT('',(55.1644483516311,22.987959834138,6.22095488139522));
#24156=CARTESIAN_POINT('Ctrl Pts',(55.1644484221208,22.9879598283069,10.5696416509586));
#24157=CARTESIAN_POINT('Ctrl Pts',(55.1795206323429,22.9867130218304,10.5687444671462));
#24158=CARTESIAN_POINT('Ctrl Pts',(55.1945828596467,22.9852944580563,10.5678435263383));
#24159=CARTESIAN_POINT('Ctrl Pts',(55.2696887042474,22.9773574861964,10.5633257816232));
#24160=CARTESIAN_POINT('Ctrl Pts',(55.3294208840686,22.9682874363899,10.5596505977628));
#24161=CARTESIAN_POINT('Ctrl Pts',(55.4027795667775,22.9537153912676,10.5549916129971));
#24162=CARTESIAN_POINT('Ctrl Pts',(55.416882237778,22.9507548262385,10.5540892908252));
#24163=CARTESIAN_POINT('Ctrl Pts',(55.4392160211955,22.9458130688504,10.5526491969457));
#24164=CARTESIAN_POINT('Ctrl Pts',(55.4474689046702,22.94393178583,10.5521146235002));
#24165=CARTESIAN_POINT('Ctrl Pts',(55.4629884365706,22.9402899708852,10.5511046811371));
#24166=CARTESIAN_POINT('Ctrl Pts',(55.4702576670761,22.9385409945568,10.5506296909739));
#24167=CARTESIAN_POINT('Ctrl Pts',(55.4866087990222,22.9345095317817,10.5495568096997));
#24168=CARTESIAN_POINT('Ctrl Pts',(55.495684756322,22.9322038891503,10.5489581815596));
#24169=CARTESIAN_POINT('Ctrl Pts',(55.5188760701109,22.9261382513339,10.5474204155609));
#24170=CARTESIAN_POINT('Ctrl Pts',(55.5329667740397,22.9222870072679,10.5464783523423));
#24171=CARTESIAN_POINT('Ctrl Pts',(55.6229356397672,22.8966316510767,10.5404124605316));
#24172=CARTESIAN_POINT('Ctrl Pts',(55.6974957710561,22.8704965375062,10.5351486458867));
#24173=CARTESIAN_POINT('Ctrl Pts',(55.915360154888,22.7792898405105,10.5190563825482));
#24174=CARTESIAN_POINT('Ctrl Pts',(56.0527105175792,22.7016316892603,10.5079004743152));
#24175=CARTESIAN_POINT('Ctrl Pts',(56.2207120192313,22.5784485813475,10.4936490590936));
#24176=CARTESIAN_POINT('Ctrl Pts',(56.2607416901066,22.546663875978,10.4902067664466));
#24177=CARTESIAN_POINT('Ctrl Pts',(56.3064438923021,22.5074201296362,10.486261242281));
#24178=CARTESIAN_POINT('Ctrl Pts',(56.3133369122406,22.5014184139045,10.4856657394375));
#24179=CARTESIAN_POINT('Ctrl Pts',(56.3239031081325,22.4920900356861,10.4847525803468));
#24180=CARTESIAN_POINT('Ctrl Pts',(56.3276054380052,22.4887968016458,10.4844325532266));
#24181=CARTESIAN_POINT('Ctrl Pts',(56.3344104174009,22.4826981810303,10.4838442841236));
#24182=CARTESIAN_POINT('Ctrl Pts',(56.3375164984436,22.4798968460925,10.4835757603014));
#24183=CARTESIAN_POINT('Ctrl Pts',(56.3445157414662,22.4735442815818,10.4829706188889));
#24184=CARTESIAN_POINT('Ctrl Pts',(56.3484036506588,22.4699873894902,10.4826344346083));
#24185=CARTESIAN_POINT('Ctrl Pts',(56.3583980814003,22.4607708697612,10.4817699709026));
#24186=CARTESIAN_POINT('Ctrl Pts',(56.3644834184551,22.4550882749749,10.4812433762019));
#24187=CARTESIAN_POINT('Ctrl Pts',(56.4025171414656,22.4191232954154,10.4779492019119));
#24188=CARTESIAN_POINT('Ctrl Pts',(56.4334940266845,22.3878259222307,10.4752530810785));
#24189=CARTESIAN_POINT('Ctrl Pts',(56.5950300672367,22.2134333008162,10.4609485298516));
#24190=CARTESIAN_POINT('Ctrl Pts',(56.7052575256727,22.0529248693865,10.4501768174887));
#24191=CARTESIAN_POINT('Ctrl Pts',(56.8143032085948,21.8307941653473,10.4353071999285));
#24192=CARTESIAN_POINT('Ctrl Pts',(56.8360223931457,21.7816239961098,10.4320259216238));
#24193=CARTESIAN_POINT('Ctrl Pts',(56.8608276689748,21.7187079973365,10.427810160613));
#24194=CARTESIAN_POINT('Ctrl Pts',(56.8657908748884,21.7057231714724,10.426939253867));
#24195=CARTESIAN_POINT('Ctrl Pts',(56.8735183803376,21.6848548813037,10.4255377824128));
#24196=CARTESIAN_POINT('Ctrl Pts',(56.8763696333598,21.6770039331303,10.4250101227268));
#24197=CARTESIAN_POINT('Ctrl Pts',(56.8816857318872,21.6620744277449,10.4240058426936));
#24198=CARTESIAN_POINT('Ctrl Pts',(56.8841601586861,21.6549994163107,10.4235295503243));
#24199=CARTESIAN_POINT('Ctrl Pts',(56.8896955994152,21.6388812496589,10.4224435509722));
#24200=CARTESIAN_POINT('Ctrl Pts',(56.8927316640792,21.6298297803117,10.4218330324798));
#24201=CARTESIAN_POINT('Ctrl Pts',(56.9004360851584,21.6063015862427,10.4202442081911));
#24202=CARTESIAN_POINT('Ctrl Pts',(56.9050039695012,21.591792854098,10.4192626389861));
#24203=CARTESIAN_POINT('Ctrl Pts',(56.9374546471015,21.484450704609,10.4119857704737));
#24204=CARTESIAN_POINT('Ctrl Pts',(56.9586996647495,21.3897609629342,10.4054758463642));
#24205=CARTESIAN_POINT('Ctrl Pts',(56.9936729643665,21.1549935069952,10.3891627511229));
#24206=CARTESIAN_POINT('Ctrl Pts',(56.9996371091365,21.0142836089884,10.3792213080346));
#24207=CARTESIAN_POINT('Ctrl Pts',(56.9876878621724,20.8253113976752,10.3662861095082));
#24208=CARTESIAN_POINT('Ctrl Pts',(56.9828076118112,20.7766303340642,10.3629954559046));
#24209=CARTESIAN_POINT('Ctrl Pts',(56.9749105119812,20.7192194297392,10.3592005228039));
#24210=CARTESIAN_POINT('Ctrl Pts',(56.9736179383067,20.7102734047097,10.358611674832));
#24211=CARTESIAN_POINT('Ctrl Pts',(56.9715259256716,20.6964585285444,10.3577065292089));
#24212=CARTESIAN_POINT('Ctrl Pts',(56.9707691772453,20.6915834767926,10.3573879242289));
#24213=CARTESIAN_POINT('Ctrl Pts',(56.9693371394543,20.6825786655285,10.356800976771));
#24214=CARTESIAN_POINT('Ctrl Pts',(56.9686669459429,20.6784482484599,10.3565323622129));
#24215=CARTESIAN_POINT('Ctrl Pts',(56.9671189111275,20.6690939561572,10.3559253875376));
#24216=CARTESIAN_POINT('Ctrl Pts',(56.9662332580555,20.6638714578548,10.3555874723663));
#24217=CARTESIAN_POINT('Ctrl Pts',(56.9635394435155,20.6483616751497,10.3545866156838));
#24218=CARTESIAN_POINT('Ctrl Pts',(56.9616712420815,20.6380848070395,10.3539269566416));
#24219=CARTESIAN_POINT('Ctrl Pts',(56.9428147412148,20.538794713725,10.3475835476879));
#24220=CARTESIAN_POINT('Ctrl Pts',(56.9198576660616,20.4510096883611,10.3422058741129));
#24221=CARTESIAN_POINT('Ctrl Pts',(56.876685017568,20.322426888312,10.3342765213955));
#24222=CARTESIAN_POINT('Ctrl Pts',(56.8609245646122,20.2802695960269,10.3316683798425));
#24223=CARTESIAN_POINT('Ctrl Pts',(56.7875311271255,20.1025264200261,10.3205118204389));
#24224=CARTESIAN_POINT('Ctrl Pts',(56.716411283723,19.9730379598587,10.3119351046345));
#24225=CARTESIAN_POINT('Ctrl Pts',(56.6216903735703,19.8383416063287,10.3017164801438));
#24226=CARTESIAN_POINT('Ctrl Pts',(56.611503261823,19.8242504099524,10.3006307288792));
#24227=CARTESIAN_POINT('Ctrl Pts',(56.5957049678437,19.8029886959157,10.2989658290496));
#24228=CARTESIAN_POINT('Ctrl Pts',(56.5902265806609,19.7957202051706,10.2983918315538));
#24229=CARTESIAN_POINT('Ctrl Pts',(56.5806065655438,19.7831368835164,10.2973895290677));
#24230=CARTESIAN_POINT('Ctrl Pts',(56.5764873660172,19.7778050309933,10.2969621109597));
#24231=CARTESIAN_POINT('Ctrl Pts',(56.5671715202991,19.7658721433801,10.2959993413764));
#24232=CARTESIAN_POINT('Ctrl Pts',(56.5619600509643,19.7592828943902,10.2954634058619));
#24233=CARTESIAN_POINT('Ctrl Pts',(56.5478777633252,19.7417069543017,10.2940221595638));
#24234=CARTESIAN_POINT('Ctrl Pts',(56.538931777746,19.7307813720725,10.29311384348));
#24235=CARTESIAN_POINT('Ctrl Pts',(56.4979618246229,19.6818154517599,10.2889856273645));
#24236=CARTESIAN_POINT('Ctrl Pts',(56.4646406759797,19.6448885296077,10.2857130586245));
#24237=CARTESIAN_POINT('Ctrl Pts',(56.4107092626002,19.5894360406048,10.280539297426));
#24238=CARTESIAN_POINT('Ctrl Pts',(56.3910324151128,19.5700279661225,10.2786752822605));
#24239=CARTESIAN_POINT('Ctrl Pts',(56.2532534487236,19.4396663285438,10.2657869899643));
#24240=CARTESIAN_POINT('Ctrl Pts',(56.1224320156335,19.3430680847122,10.2542856715688));
#24241=CARTESIAN_POINT('Ctrl Pts',(55.9364239473574,19.2379545658489,10.2396646000273));
#24242=CARTESIAN_POINT('Ctrl Pts',(55.8904946390295,19.2143028689359,10.2361843352079));
#24243=CARTESIAN_POINT('Ctrl Pts',(55.8353913880244,19.188582664532,10.2322012152433));
#24244=CARTESIAN_POINT('Ctrl Pts',(55.8270609777398,19.1847640149892,10.2316041123578));
#24245=CARTESIAN_POINT('Ctrl Pts',(55.8141812216076,19.1789670227817,10.2306890275811));
#24246=CARTESIAN_POINT('Ctrl Pts',(55.8096504479534,19.1769480755715,10.2303686594285));
#24247=CARTESIAN_POINT('Ctrl Pts',(55.8012855295126,19.1732579396096,10.2297800708355));
#24248=CARTESIAN_POINT('Ctrl Pts',(55.7974536788799,19.1715819171647,10.2295115662224));
#24249=CARTESIAN_POINT('Ctrl Pts',(55.7887880234012,19.1678240491753,10.2289068529175));
#24250=CARTESIAN_POINT('Ctrl Pts',(55.7839512425792,19.1657492779251,10.2285710748013));
#24251=CARTESIAN_POINT('Ctrl Pts',(55.7696382818747,19.1596765891433,10.2275824294941));
#24252=CARTESIAN_POINT('Ctrl Pts',(55.7601391582848,19.1557327167166,10.226932727311));
#24253=CARTESIAN_POINT('Ctrl Pts',(55.6477146370237,19.110072189154,10.2193141769951));
#24254=CARTESIAN_POINT('Ctrl Pts',(55.5414930669802,19.0769415107323,10.2128081317863));
#24255=CARTESIAN_POINT('Ctrl Pts',(55.4081136221418,19.0472779223273,10.204864708389));
#24256=CARTESIAN_POINT('Ctrl Pts',(55.3830710095716,19.0422112340185,10.2033831658793));
#24257=CARTESIAN_POINT('Ctrl Pts',(55.2133409011632,19.0112523695962,10.1933733896659));
#24258=CARTESIAN_POINT('Ctrl Pts',(55.0662933991303,19.0009429734723,10.1848118993532));
#24259=CARTESIAN_POINT('Ctrl Pts',(54.9023164468414,19.0075693860421,10.1746249037469));
#24260=CARTESIAN_POINT('Ctrl Pts',(54.8851863519837,19.0084830843205,10.1735535111708));
#24261=CARTESIAN_POINT('Ctrl Pts',(54.8590370273013,19.0102163518508,10.1719061401668));
#24262=CARTESIAN_POINT('Ctrl Pts',(54.8500077779817,19.0108766113974,10.1713351448596));
#24263=CARTESIAN_POINT('Ctrl Pts',(54.8342720875987,19.0121350267007,10.1703361425292));
#24264=CARTESIAN_POINT('Ctrl Pts',(54.8275635491583,19.0127057184144,10.1699090032749));
#24265=CARTESIAN_POINT('Ctrl Pts',(54.8124570060249,19.0140678913751,10.1689443045834));
#24266=CARTESIAN_POINT('Ctrl Pts',(54.8040609150552,19.0148786973984,10.1684061460766));
#24267=CARTESIAN_POINT('Ctrl Pts',(54.7814695203678,19.0172050551753,10.1669526448141));
#24268=CARTESIAN_POINT('Ctrl Pts',(54.767285140299,19.0188197607885,10.1660342073491));
#24269=CARTESIAN_POINT('Ctrl Pts',(54.7021219411451,19.0269471763794,10.1617872190869));
#24270=CARTESIAN_POINT('Ctrl Pts',(54.6513933994135,19.0352757387631,10.1584021969025));
#24271=CARTESIAN_POINT('Ctrl Pts',(54.576925039719,19.0504766652584,10.1533125699924));
#24272=CARTESIAN_POINT('Ctrl Pts',(54.552897539851,19.0558464650124,10.1516516808575));
#24273=CARTESIAN_POINT('Ctrl Pts',(54.3582897542213,19.1031368510996,10.1380509986044));
#24274=CARTESIAN_POINT('Ctrl Pts',(54.1938526201807,19.166970179225,10.1255320731254));
#24275=CARTESIAN_POINT('Ctrl Pts',(54.0164081440846,19.2644040326048,10.11178927966));
#24276=CARTESIAN_POINT('Ctrl Pts',(53.9931697346657,19.2777807156589,10.1099864901516));
#24277=CARTESIAN_POINT('Ctrl Pts',(53.955158792097,19.3006933354577,10.1070409938576));
#24278=CARTESIAN_POINT('Ctrl Pts',(53.9402305228355,19.3099630192671,10.1058850703593));
#24279=CARTESIAN_POINT('Ctrl Pts',(53.920000630192,19.3228982160019,10.1043218888375));
#24280=CARTESIAN_POINT('Ctrl Pts',(53.9145919133018,19.3263936183257,10.1039042757848));
#24281=CARTESIAN_POINT('Ctrl Pts',(53.9055466381482,19.3323014530859,10.1032065502335));
#24282=CARTESIAN_POINT('Ctrl Pts',(53.9019009354994,19.3346997116779,10.1029255156929));
#24283=CARTESIAN_POINT('Ctrl Pts',(53.8950055229073,19.3392682221652,10.102394366364));
#24284=CARTESIAN_POINT('Ctrl Pts',(53.8917542811157,19.3414360851828,10.1021440908646));
#24285=CARTESIAN_POINT('Ctrl Pts',(53.8832606969587,19.3471355635611,10.1014906435867));
#24286=CARTESIAN_POINT('Ctrl Pts',(53.8780286823287,19.3506826014594,10.1010884987161));
#24287=CARTESIAN_POINT('Ctrl Pts',(53.8599677074106,19.3630527319684,10.0997012668809));
#24288=CARTESIAN_POINT('Ctrl Pts',(53.8472248667372,19.3720013778125,10.0987242282678));
#24289=CARTESIAN_POINT('Ctrl Pts',(53.7329013840021,19.4543003992377,10.0899614386239));
#24290=CARTESIAN_POINT('Ctrl Pts',(53.6383232387173,19.5369308320924,10.0827211583798));
#24291=CARTESIAN_POINT('Ctrl Pts',(53.4813570455697,19.7025668355284,10.0694823491994));
#24292=CARTESIAN_POINT('Ctrl Pts',(53.4164842929297,19.7825907976671,10.0635136726485));
#24293=CARTESIAN_POINT('Ctrl Pts',(53.3381185465214,19.8961826723291,10.0552181243478));
#24294=CARTESIAN_POINT('Ctrl Pts',(53.318930495592,19.9256314558589,10.0530831176812));
#24295=CARTESIAN_POINT('Ctrl Pts',(53.2873491047164,19.9770198857956,10.0493716383957));
#24296=CARTESIAN_POINT('Ctrl Pts',(53.2745748685276,19.9987161090958,10.047808845111));
#24297=CARTESIAN_POINT('Ctrl Pts',(53.2570342330625,20.0298406051479,10.0455699812799));
#24298=CARTESIAN_POINT('Ctrl Pts',(53.2519264740627,20.0390744788529,10.0449061457732));
#24299=CARTESIAN_POINT('Ctrl Pts',(53.2432437327223,20.0550695963877,10.0437566828101));
#24300=CARTESIAN_POINT('Ctrl Pts',(53.2396338928623,20.061811737189,10.0432723058929));
#24301=CARTESIAN_POINT('Ctrl Pts',(53.2327939387063,20.0747652661179,10.0423418660736));
#24302=CARTESIAN_POINT('Ctrl Pts',(53.2295575732429,20.0809732390525,10.0418960331024));
#24303=CARTESIAN_POINT('Ctrl Pts',(53.222034574125,20.0955910183694,10.0408463627554));
#24304=CARTESIAN_POINT('Ctrl Pts',(53.2177748504954,20.1040144124698,10.0402415919609));
#24305=CARTESIAN_POINT('Ctrl Pts',(53.2032669627714,20.1332158833563,10.0381451522156));
#24306=CARTESIAN_POINT('Ctrl Pts',(53.1933214229174,20.1541414089725,10.0366430526732));
#24307=CARTESIAN_POINT('Ctrl Pts',(53.1179175798902,20.3201919967116,10.0247203447313));
#24308=CARTESIAN_POINT('Ctrl Pts',(53.0696946030046,20.4724821288948,10.013698302132));
#24309=CARTESIAN_POINT('Ctrl Pts',(53.0189524927518,20.7404309869774,9.99467756171033));
#24310=CARTESIAN_POINT('Ctrl Pts',(53.0073868960935,20.8536299421846,9.98677158445842));
#24311=CARTESIAN_POINT('Ctrl Pts',(53.0053397121424,20.9781466270934,9.97858796111114));
#24312=CARTESIAN_POINT('Ctrl Pts',(53.0052498563847,20.989086183223,9.97787341146361));
#24313=CARTESIAN_POINT('Ctrl Pts',(53.0052500701672,21.0053517588649,9.97681810964014));
#24314=CARTESIAN_POINT('Ctrl Pts',(53.005271467191,21.0106773538269,9.97647372476639));
#24315=CARTESIAN_POINT('Ctrl Pts',(53.0053477781925,21.0201891749405,9.97586074038109));
#24316=CARTESIAN_POINT('Ctrl Pts',(53.0053945424089,21.0243753639959,9.97559169711591));
#24317=CARTESIAN_POINT('Ctrl Pts',(53.0055248150456,21.0334727401625,9.97500861879199));
#24318=CARTESIAN_POINT('Ctrl Pts',(53.0056132834093,21.0383837683754,9.97469486200405));
#24319=CARTESIAN_POINT('Ctrl Pts',(53.0059138901869,21.0522306622226,9.97381291934913));
#24320=CARTESIAN_POINT('Ctrl Pts',(53.0061679540123,21.0611656352677,9.97324701239955));
#24321=CARTESIAN_POINT('Ctrl Pts',(53.0081287048847,21.116926820828,9.96973350786472));
#24322=CARTESIAN_POINT('Ctrl Pts',(53.0114249745165,21.1636865571769,9.96686720927864));
#24323=CARTESIAN_POINT('Ctrl Pts',(53.0289237777837,21.3287496035733,9.95689740860245));
#24324=CARTESIAN_POINT('Ctrl Pts',(53.0520686542674,21.4458535077955,9.95008391346948));
#24325=CARTESIAN_POINT('Ctrl Pts',(53.1191695401638,21.6751700030247,9.93617338895022));
#24326=CARTESIAN_POINT('Ctrl Pts',(53.1630945331575,21.7868611038043,9.92909871552594));
#24327=CARTESIAN_POINT('Ctrl Pts',(53.2237440030765,21.9078460916274,9.9206992918665));
#24328=CARTESIAN_POINT('Ctrl Pts',(53.2308827035187,21.9216799132677,9.91972774268353));
#24329=CARTESIAN_POINT('Ctrl Pts',(53.2427096524673,21.9439551883925,9.9181445034958));
#24330=CARTESIAN_POINT('Ctrl Pts',(53.2472986494408,21.9524488089649,9.91753630976153));
#24331=CARTESIAN_POINT('Ctrl Pts',(53.2555657261075,21.9674879814617,9.91645122619231));
#24332=CARTESIAN_POINT('Ctrl Pts',(53.2592194704208,21.9740467522273,9.91597521052456));
#24333=CARTESIAN_POINT('Ctrl Pts',(53.2669872538054,21.9878072549158,9.91497053167083));
#24334=CARTESIAN_POINT('Ctrl Pts',(53.2711093480965,21.995004252088,9.914441585486));
#24335=CARTESIAN_POINT('Ctrl Pts',(53.2821260186248,22.0139637249509,9.91303880089399));
#24336=CARTESIAN_POINT('Ctrl Pts',(53.2890964179815,22.025681416974,9.91216223075927));
#24337=CARTESIAN_POINT('Ctrl Pts',(53.3224969844937,22.0805420078166,9.9080120400027));
#24338=CARTESIAN_POINT('Ctrl Pts',(53.3504401813715,22.1227372973583,9.90468335658888));
#24339=CARTESIAN_POINT('Ctrl Pts',(53.4787493468056,22.3013441928268,9.88997482482784));
#24340=CARTESIAN_POINT('Ctrl Pts',(53.5946455249131,22.4257148737387,9.87801656279692));
#24341=CARTESIAN_POINT('Ctrl Pts',(53.778748061302,22.578761900371,9.86147012798136));
#24342=CARTESIAN_POINT('Ctrl Pts',(53.8350080032798,22.6207224563182,9.85669087045085));
#24343=CARTESIAN_POINT('Ctrl Pts',(53.9018666495572,22.6653032950413,9.85141571472648));
#24344=CARTESIAN_POINT('Ctrl Pts',(53.9104096301998,22.6709053702993,9.85074892228964));
#24345=CARTESIAN_POINT('Ctrl Pts',(53.923406096089,22.6792857620684,9.84974589911488));
#24346=CARTESIAN_POINT('Ctrl Pts',(53.9278279745852,22.6821124379992,9.84940660599922));
#24347=CARTESIAN_POINT('Ctrl Pts',(53.9357931019677,22.6871599586991,9.8487990462518));
#24348=CARTESIAN_POINT('Ctrl Pts',(53.9393322078173,22.689387132563,9.84853036912762));
#24349=CARTESIAN_POINT('Ctrl Pts',(53.9470949764504,22.6942382644822,9.84794383917477));
#24350=CARTESIAN_POINT('Ctrl Pts',(53.9513214480039,22.6968575607091,9.84762629166891));
#24351=CARTESIAN_POINT('Ctrl Pts',(53.9634128843393,22.7042886266924,9.84672279428538));
#24352=CARTESIAN_POINT('Ctrl Pts',(53.9713016001252,22.7090617839363,9.84613930428496));
#24353=CARTESIAN_POINT('Ctrl Pts',(54.0247096959407,22.7408731795927,9.84222706680628));
#24354=CARTESIAN_POINT('Ctrl Pts',(54.071261233634,22.766147218667,9.83900246623963));
#24355=CARTESIAN_POINT('Ctrl Pts',(54.2755937829782,22.866767682836,9.82539106138797));
#24356=CARTESIAN_POINT('Ctrl Pts',(54.4418937823907,22.9230473161335,9.81559329286339));
#24357=CARTESIAN_POINT('Ctrl Pts',(54.6736350687004,22.96882758614,9.8014815943344));
#24358=CARTESIAN_POINT('Ctrl Pts',(54.7343717481186,22.9779374731696,9.79775058576003));
#24359=CARTESIAN_POINT('Ctrl Pts',(54.8102854479758,22.9857640973899,9.79300114406748));
#24360=CARTESIAN_POINT('Ctrl Pts',(54.8251596057183,22.9871289538257,9.79206656556284));
#24361=CARTESIAN_POINT('Ctrl Pts',(54.8486871492846,22.9890216470555,9.79058138184153));
#24362=CARTESIAN_POINT('Ctrl Pts',(54.8573312479694,22.9896603515687,9.79003425405877));
#24363=CARTESIAN_POINT('Ctrl Pts',(54.8734196517449,22.9907437279569,9.78901309741248));
#24364=CARTESIAN_POINT('Ctrl Pts',(54.8808628446574,22.9912030310109,9.78853953585866));
#24365=CARTESIAN_POINT('Ctrl Pts',(54.8973816832914,22.9921294204338,9.78748596601456));
#24366=CARTESIAN_POINT('Ctrl Pts',(54.9064582550317,22.9925762429868,9.78690533354469));
#24367=CARTESIAN_POINT('Ctrl Pts',(54.932840624997,22.9936943393587,9.78521245670083));
#24368=CARTESIAN_POINT('Ctrl Pts',(54.9501521548108,22.9942022619015,9.78409514241426));
#24369=CARTESIAN_POINT('Ctrl Pts',(55.0332518502922,22.9955577134741,9.77869925214527));
#24370=CARTESIAN_POINT('Ctrl Pts',(55.0989923360642,22.9933745134514,9.77433085642924));
#24371=CARTESIAN_POINT('Ctrl Pts',(55.1644488239152,22.9879597950695,9.76988214123148));
#24372=CARTESIAN_POINT('',(53.0052507630248,20.9982552688642,9.82018160501716));
#24373=CARTESIAN_POINT('Ctrl Pts',(55.1644483514339,22.9879598341543,9.61229346745724));
#24374=CARTESIAN_POINT('Ctrl Pts',(55.1089206062989,22.9925532097293,9.6157599371205));
#24375=CARTESIAN_POINT('Ctrl Pts',(55.0532179574516,22.9948186209764,9.61911693483845));
#24376=CARTESIAN_POINT('Ctrl Pts',(54.828641597696,22.9945357235973,9.63242345076764));
#24377=CARTESIAN_POINT('Ctrl Pts',(54.6605077658855,22.972887588271,9.64192717472063));
#24378=CARTESIAN_POINT('Ctrl Pts',(54.4433596053057,22.9163151125312,9.655385059149));
#24379=CARTESIAN_POINT('Ctrl Pts',(54.3902270624372,22.9000758553173,9.65877059251745));
#24380=CARTESIAN_POINT('Ctrl Pts',(54.324178751614,22.8768332590493,9.66313075487158));
#24381=CARTESIAN_POINT('Ctrl Pts',(54.3105660854473,22.8718756107253,9.66403763047418));
#24382=CARTESIAN_POINT('Ctrl Pts',(54.2889951653645,22.8637524017234,9.66548837687345));
#24383=CARTESIAN_POINT('Ctrl Pts',(54.2810010440419,22.8606830432491,9.6660290373258));
#24384=CARTESIAN_POINT('Ctrl Pts',(54.2660774768651,22.85484257715,9.66704412518632));
#24385=CARTESIAN_POINT('Ctrl Pts',(54.2591433169166,22.8520838611207,9.66751812953735));
#24386=CARTESIAN_POINT('Ctrl Pts',(54.2438512023699,22.8459003606792,9.66856874639529));
#24387=CARTESIAN_POINT('Ctrl Pts',(54.2355007381463,22.8424576032854,9.66914595777952));
#24388=CARTESIAN_POINT('Ctrl Pts',(54.2112748962757,22.8322766442381,9.67083091807161));
#24389=CARTESIAN_POINT('Ctrl Pts',(54.1954634880096,22.8253892626325,9.67194370169674));
#24390=CARTESIAN_POINT('Ctrl Pts',(54.1597332848822,22.8092709348884,9.67448884756032));
#24391=CARTESIAN_POINT('Ctrl Pts',(54.1398738621292,22.7999145624565,9.67592536619496));
#24392=CARTESIAN_POINT('Ctrl Pts',(54.075498693003,22.7682767872788,9.68065495851626));
#24393=CARTESIAN_POINT('Ctrl Pts',(54.0316646955993,22.7446579972047,9.68399186181687));
#24394=CARTESIAN_POINT('Ctrl Pts',(53.8917238715625,22.6623553175447,9.69502423074494));
#24395=CARTESIAN_POINT('Ctrl Pts',(53.7996971950423,22.5971757649185,9.70290045213956));
#24396=CARTESIAN_POINT('Ctrl Pts',(53.6383817256847,22.4610701747593,9.7176004675061));
#24397=CARTESIAN_POINT('Ctrl Pts',(53.5678947914932,22.392052336322,9.72440856365455));
#24398=CARTESIAN_POINT('Ctrl Pts',(53.4958897048283,22.3102628852506,9.73156477600034));
#24399=CARTESIAN_POINT('Ctrl Pts',(53.4890509243693,22.3023707270529,9.73224659161516));
#24400=CARTESIAN_POINT('Ctrl Pts',(53.4788378960835,22.290395853582,9.73326759706016));
#24401=CARTESIAN_POINT('Ctrl Pts',(53.4754175403764,22.2863529572833,9.73361001206823));
#24402=CARTESIAN_POINT('Ctrl Pts',(53.4693241745386,22.2790920916492,9.73422081099481));
#24403=CARTESIAN_POINT('Ctrl Pts',(53.4666451578864,22.2758793010241,9.73448962624893));
#24404=CARTESIAN_POINT('Ctrl Pts',(53.4608297910738,22.2688604932783,9.73507373096043));
#24405=CARTESIAN_POINT('Ctrl Pts',(53.4576974469312,22.2650512714969,9.73538873269542));
#24406=CARTESIAN_POINT('Ctrl Pts',(53.4488667860125,22.2542308166217,9.73627800198762));
#24407=CARTESIAN_POINT('Ctrl Pts',(53.4432018427416,22.2471923243029,9.73684992900172));
#24408=CARTESIAN_POINT('Ctrl Pts',(53.4072078995929,22.2018437357967,9.74049501572245));
#24409=CARTESIAN_POINT('Ctrl Pts',(53.3782446198489,22.1624652273901,9.7434796563598));
#24410=CARTESIAN_POINT('Ctrl Pts',(53.3179491720982,22.0738406719841,9.74990688179934));
#24411=CARTESIAN_POINT('Ctrl Pts',(53.2872724473465,22.0242039986909,9.75332355518599));
#24412=CARTESIAN_POINT('Ctrl Pts',(53.2132284499993,21.8917417964281,9.76215722426305));
#24413=CARTESIAN_POINT('Ctrl Pts',(53.1734298107725,21.8070916795067,9.76753375079514));
#24414=CARTESIAN_POINT('Ctrl Pts',(53.1302470164264,21.6955133203145,9.77458230322623));
#24415=CARTESIAN_POINT('Ctrl Pts',(53.1212670338371,21.670878063763,9.77613578402236));
#24416=CARTESIAN_POINT('Ctrl Pts',(53.0925895358491,21.5871091488461,9.78142207023171));
#24417=CARTESIAN_POINT('Ctrl Pts',(53.0751798652793,21.5272363010452,9.7852081562648));
#24418=CARTESIAN_POINT('Ctrl Pts',(53.0570931710659,21.4520681206928,9.79001927144593));
#24419=CARTESIAN_POINT('Ctrl Pts',(53.0537489847629,21.4374465658683,9.79095770021957));
#24420=CARTESIAN_POINT('Ctrl Pts',(53.0487302609538,21.4143058255575,9.7924475560164));
#24421=CARTESIAN_POINT('Ctrl Pts',(53.0469458623405,21.405810846487,9.79299546702962));
#24422=CARTESIAN_POINT('Ctrl Pts',(53.0437322794341,21.3899996595754,9.79401720308837));
#24423=CARTESIAN_POINT('Ctrl Pts',(53.0422885452528,21.3826865381464,9.79449055457193));
#24424=CARTESIAN_POINT('Ctrl Pts',(53.0395434151779,21.3683591104237,9.79541948950454));
#24425=CARTESIAN_POINT('Ctrl Pts',(53.0382385893137,21.3613455694539,9.79587495579915));
#24426=CARTESIAN_POINT('Ctrl Pts',(53.035396065226,21.3455974512142,9.79689936333328));
#24427=CARTESIAN_POINT('Ctrl Pts',(53.0338789489189,21.336859358037,9.79746894882525));
#24428=CARTESIAN_POINT('Ctrl Pts',(53.0302122539574,21.3148713635623,9.79890528514081));
#24429=CARTESIAN_POINT('Ctrl Pts',(53.0281380792995,21.3016095010591,9.7997743925597));
#24430=CARTESIAN_POINT('Ctrl Pts',(53.0121645468032,21.1922597552295,9.8069645009715));
#24431=CARTESIAN_POINT('Ctrl Pts',(53.0051658710303,21.0953121951049,9.81350083438465));
#24432=CARTESIAN_POINT('Ctrl Pts',(53.0052507630248,20.9982552688642,9.82018160501716));
#24433=CARTESIAN_POINT('Ctrl Pts',(53.005250761363,20.9982571697515,9.82018147417241));
#24434=CARTESIAN_POINT('Ctrl Pts',(53.0053860238156,20.8434430824682,9.83083787131134));
#24435=CARTESIAN_POINT('Ctrl Pts',(53.0235426954589,20.6891709665941,9.84183516337205));
#24436=CARTESIAN_POINT('Ctrl Pts',(53.0643763109955,20.5174454261476,9.85374121521571));
#24437=CARTESIAN_POINT('Ctrl Pts',(53.0697377928547,20.4964268908962,9.85519157367019));
#24438=CARTESIAN_POINT('Ctrl Pts',(53.0793804526472,20.4610449399489,9.85761676212631));
#24439=CARTESIAN_POINT('Ctrl Pts',(53.0834825035105,20.4466350929466,9.85859983518176));
#24440=CARTESIAN_POINT('Ctrl Pts',(53.0894674436144,20.4264762700555,9.85996729988876));
#24441=CARTESIAN_POINT('Ctrl Pts',(53.0912145998974,20.4206879800285,9.86035903571322));
#24442=CARTESIAN_POINT('Ctrl Pts',(53.0942450750124,20.4108106469673,9.86102584278744));
#24443=CARTESIAN_POINT('Ctrl Pts',(53.0955152951957,20.4067176571241,9.86130166491522));
#24444=CARTESIAN_POINT('Ctrl Pts',(53.0979930902177,20.398823500335,9.86183265704579));
#24445=CARTESIAN_POINT('Ctrl Pts',(53.0991988795002,20.3950218437027,9.86208793311688));
#24446=CARTESIAN_POINT('Ctrl Pts',(53.1021317941633,20.3858701760786,9.86270145548229));
#24447=CARTESIAN_POINT('Ctrl Pts',(53.1038701622996,20.3805237633552,9.86305905073341));
#24448=CARTESIAN_POINT('Ctrl Pts',(53.1103601236829,20.3608469393985,9.86437233852564));
#24449=CARTESIAN_POINT('Ctrl Pts',(53.1152519030948,20.3465628258817,9.8653202186519));
#24450=CARTESIAN_POINT('Ctrl Pts',(53.1657864938792,20.2042914657335,9.87471913212622));
#24451=CARTESIAN_POINT('Ctrl Pts',(53.2242387153877,20.0812106073078,9.88252414508266));
#24452=CARTESIAN_POINT('Ctrl Pts',(53.3411262959643,19.8886266585373,9.89559882675533));
#24453=CARTESIAN_POINT('Ctrl Pts',(53.3925691237987,19.8154422408353,9.90080285863356));
#24454=CARTESIAN_POINT('Ctrl Pts',(53.4840972510739,19.7022214201233,9.90953560841896));
#24455=CARTESIAN_POINT('Ctrl Pts',(53.5212840302733,19.660004259427,9.91296507026975));
#24456=CARTESIAN_POINT('Ctrl Pts',(53.5697088256334,19.6095024649562,9.91732498794597));
#24457=CARTESIAN_POINT('Ctrl Pts',(53.5793175406992,19.5996866160219,9.91818519222063));
#24458=CARTESIAN_POINT('Ctrl Pts',(53.5940701712906,19.5849241055802,9.91949894094766));
#24459=CARTESIAN_POINT('Ctrl Pts',(53.5991406520325,19.5799043851572,9.91994925322498));
#24460=CARTESIAN_POINT('Ctrl Pts',(53.6095635406865,19.5696959817292,9.92087249906618));
#24461=CARTESIAN_POINT('Ctrl Pts',(53.614918316631,19.5645098885753,9.9213455346968));
#24462=CARTESIAN_POINT('Ctrl Pts',(53.6265685843059,19.5533524972712,9.92237202297392));
#24463=CARTESIAN_POINT('Ctrl Pts',(53.6328741996721,19.5473920374311,9.92292592979462));
#24464=CARTESIAN_POINT('Ctrl Pts',(53.6501741495146,19.5312514704063,9.92444122024709));
#24465=CARTESIAN_POINT('Ctrl Pts',(53.6612444418464,19.5211539616983,9.92540608458443));
#24466=CARTESIAN_POINT('Ctrl Pts',(53.7187789283916,19.4698506877642,9.93039739347665));
#24467=CARTESIAN_POINT('Ctrl Pts',(53.7670308384599,19.4307103486029,9.93450802850537));
#24468=CARTESIAN_POINT('Ctrl Pts',(53.9064253901271,19.3280399673356,9.94618629897363));
#24469=CARTESIAN_POINT('Ctrl Pts',(54.0011588937457,19.2697781889932,9.95391597867084));
#24470=CARTESIAN_POINT('Ctrl Pts',(54.1928137539631,19.1729154613862,9.96889323116746));
#24471=CARTESIAN_POINT('Ctrl Pts',(54.2889100932658,19.1334141071176,9.97611319234276));
#24472=CARTESIAN_POINT('Ctrl Pts',(54.4042529823624,19.0962097414256,9.98415504305193));
#24473=CARTESIAN_POINT('Ctrl Pts',(54.4209249920805,19.0910725412147,9.98530250060205));
#24474=CARTESIAN_POINT('Ctrl Pts',(54.4438229980657,19.0843445174885,9.98685610919408));
#24475=CARTESIAN_POINT('Ctrl Pts',(54.4499918846678,19.08256424854,9.98727245729615));
#24476=CARTESIAN_POINT('Ctrl Pts',(54.4603630901044,19.0796254095803,9.98796860420361));
#24477=CARTESIAN_POINT('Ctrl Pts',(54.4645607629922,19.0784507847483,9.98824931684867));
#24478=CARTESIAN_POINT('Ctrl Pts',(54.4725305573907,19.0762487600357,9.98878025381009));
#24479=CARTESIAN_POINT('Ctrl Pts',(54.4763018925294,19.0752186776087,9.98903063651271));
#24480=CARTESIAN_POINT('Ctrl Pts',(54.4861924097688,19.0725484554969,9.98968508874297));
#24481=CARTESIAN_POINT('Ctrl Pts',(54.4923164795569,19.0709263513597,9.99008812460039));
#24482=CARTESIAN_POINT('Ctrl Pts',(54.5136067372658,19.0653955333222,9.99148200599353));
#24483=CARTESIAN_POINT('Ctrl Pts',(54.5288116083312,19.0616361580112,9.99246469852505));
#24484=CARTESIAN_POINT('Ctrl Pts',(54.6645245657791,19.0297727230483,10.0011353315304));
#24485=CARTESIAN_POINT('Ctrl Pts',(54.7873775010952,19.0127557975032,10.0082920154952));
#24486=CARTESIAN_POINT('Ctrl Pts',(55.0148564092826,19.0025995962209,10.021502455981));
#24487=CARTESIAN_POINT('Ctrl Pts',(55.1188820686405,19.0060857456181,10.0275293599991));
#24488=CARTESIAN_POINT('Ctrl Pts',(55.2572868489808,19.0215964207877,10.0358993944882));
#24489=CARTESIAN_POINT('Ctrl Pts',(55.2923052708476,19.0264664535093,10.038046577975));
#24490=CARTESIAN_POINT('Ctrl Pts',(55.3521204360537,19.0364118887832,10.04177728671));
#24491=CARTESIAN_POINT('Ctrl Pts',(55.3769844281821,19.0410335063928,10.04334693439));
#24492=CARTESIAN_POINT('Ctrl Pts',(55.4121056169208,19.0482550804524,10.0455938145312));
#24493=CARTESIAN_POINT('Ctrl Pts',(55.4224409870032,19.0504659848866,10.0462586876158));
#24494=CARTESIAN_POINT('Ctrl Pts',(55.4402250100831,19.0544183361036,10.0474092695448));
#24495=CARTESIAN_POINT('Ctrl Pts',(55.4476821852852,19.0561207010941,10.0478937200156));
#24496=CARTESIAN_POINT('Ctrl Pts',(55.4619394883548,19.0594618279327,10.0488238271638));
#24497=CARTESIAN_POINT('Ctrl Pts',(55.468741161628,19.061093553186,10.049269251386));
#24498=CARTESIAN_POINT('Ctrl Pts',(55.4846819633904,19.0650065416677,10.0503172361939));
#24499=CARTESIAN_POINT('Ctrl Pts',(55.4938137320586,19.067316817889,10.0509207235476));
#24500=CARTESIAN_POINT('Ctrl Pts',(55.5252461387917,19.0755063169654,10.0530090419226));
#24501=CARTESIAN_POINT('Ctrl Pts',(55.5474602745024,19.0817073695127,10.054504199108));
#24502=CARTESIAN_POINT('Ctrl Pts',(55.7233456083865,19.1341094372841,10.0665011740046));
#24503=CARTESIAN_POINT('Ctrl Pts',(55.871011779508,19.1983076357173,10.0776153039086));
#24504=CARTESIAN_POINT('Ctrl Pts',(56.0984202367432,19.3317191182351,10.0960035705854));
#24505=CARTESIAN_POINT('Ctrl Pts',(56.1832943463724,19.3908055477882,10.1031885348333));
#24506=CARTESIAN_POINT('Ctrl Pts',(56.2766898483492,19.4672268303226,10.1111956422059));
#24507=CARTESIAN_POINT('Ctrl Pts',(56.290017170908,19.4784263714656,10.1123406075176));
#24508=CARTESIAN_POINT('Ctrl Pts',(56.3080535284524,19.4939904770871,10.113891418136));
#24509=CARTESIAN_POINT('Ctrl Pts',(56.3128901799333,19.4982050424308,10.11430741403));
#24510=CARTESIAN_POINT('Ctrl Pts',(56.3209780621825,19.505321602619,10.1150031372963));
#24511=CARTESIAN_POINT('Ctrl Pts',(56.3242402348248,19.5082110223118,10.1152837761466));
#24512=CARTESIAN_POINT('Ctrl Pts',(56.3304116666648,19.5137134695487,10.1158146973886));
#24513=CARTESIAN_POINT('Ctrl Pts',(56.3333227447129,19.5163243910901,10.1160651374702));
#24514=CARTESIAN_POINT('Ctrl Pts',(56.3409336061122,19.5231909992929,10.1167199678861));
#24515=CARTESIAN_POINT('Ctrl Pts',(56.3456208566869,19.5274606038387,10.1171233222225));
#24516=CARTESIAN_POINT('Ctrl Pts',(56.3618379487831,19.5423748070291,10.1185194321854));
#24517=CARTESIAN_POINT('Ctrl Pts',(56.3732628300936,19.5531333726073,10.1195040001479));
#24518=CARTESIAN_POINT('Ctrl Pts',(56.4724009843591,19.6487219579918,10.1280692486186));
#24519=CARTESIAN_POINT('Ctrl Pts',(56.5522979821094,19.7413116948731,10.1351336542516));
#24520=CARTESIAN_POINT('Ctrl Pts',(56.6257699388341,19.8441805304635,10.1424677671659));
#24521=CARTESIAN_POINT('Ctrl Pts',(56.628290257078,19.84773380728,10.1427204952594));
#24522=CARTESIAN_POINT('Ctrl Pts',(56.7164763606485,19.9729303034087,10.1516047806492));
#24523=CARTESIAN_POINT('Ctrl Pts',(56.7882650465273,20.103750213979,10.1602610192741));
#24524=CARTESIAN_POINT('Ctrl Pts',(56.8514337335229,20.2573553406565,10.170568456624));
#24525=CARTESIAN_POINT('Ctrl Pts',(56.8578163317679,20.2734696101186,10.1716507864361));
#24526=CARTESIAN_POINT('Ctrl Pts',(56.8672244962511,20.2981575335159,10.1733114085919));
#24527=CARTESIAN_POINT('Ctrl Pts',(56.8704028819254,20.3066723559293,10.1738845894396));
#24528=CARTESIAN_POINT('Ctrl Pts',(56.8758348960301,20.3215338178489,10.1748858809387));
#24529=CARTESIAN_POINT('Ctrl Pts',(56.8781147958007,20.3278707494368,10.1753131093524));
#24530=CARTESIAN_POINT('Ctrl Pts',(56.8831680989866,20.3421427737342,10.1762759943016));
#24531=CARTESIAN_POINT('Ctrl Pts',(56.8859235095907,20.3500840580524,10.1768122377103));
#24532=CARTESIAN_POINT('Ctrl Pts',(56.8931821649248,20.3714389023648,10.1782556309659));
#24533=CARTESIAN_POINT('Ctrl Pts',(56.8975929531165,20.3848831572668,10.1791658030527));
#24534=CARTESIAN_POINT('Ctrl Pts',(56.9169568341294,20.4460961521693,10.1833173060348));
#24535=CARTESIAN_POINT('Ctrl Pts',(56.9302505830606,20.4943668082178,10.1866120476153));
#24536=CARTESIAN_POINT('Ctrl Pts',(56.9475476726069,20.5678724988019,10.1916639267382));
#24537=CARTESIAN_POINT('Ctrl Pts',(56.9529056014151,20.5927706539171,10.1933808858098));
#24538=CARTESIAN_POINT('Ctrl Pts',(56.989144349417,20.7783827888683,10.2062191387137));
#24539=CARTESIAN_POINT('Ctrl Pts',(57.0006156252319,20.9422282127028,10.2178364601352));
#24540=CARTESIAN_POINT('Ctrl Pts',(56.9892082568408,21.1573607329815,10.2325809890999));
#24541=CARTESIAN_POINT('Ctrl Pts',(56.9844499091691,21.2089772267665,10.236073312663));
#24542=CARTESIAN_POINT('Ctrl Pts',(56.9764895322872,21.2694452965424,10.2400682320909));
#24543=CARTESIAN_POINT('Ctrl Pts',(56.9752300571101,21.2785280386805,10.2406657120262));
#24544=CARTESIAN_POINT('Ctrl Pts',(56.9731927657954,21.2925106459984,10.2415811928331));
#24545=CARTESIAN_POINT('Ctrl Pts',(56.9724592472064,21.2974166915605,10.2419015839529));
#24546=CARTESIAN_POINT('Ctrl Pts',(56.9710737601621,21.3064527294174,10.2424901071771));
#24547=CARTESIAN_POINT('Ctrl Pts',(56.9704271118367,21.3105833879984,10.2427585241096));
#24548=CARTESIAN_POINT('Ctrl Pts',(56.9689377565809,21.3199051886331,10.2433628991531));
#24549=CARTESIAN_POINT('Ctrl Pts',(56.9680875070261,21.325095040289,10.2436984279468));
#24550=CARTESIAN_POINT('Ctrl Pts',(56.965516168633,21.34041039792,10.2446859258761));
#24551=CARTESIAN_POINT('Ctrl Pts',(56.9637373611646,21.3505262260751,10.2453347399971));
#24552=CARTESIAN_POINT('Ctrl Pts',(56.9488027052193,21.4317733840827,10.2505214668697));
#24553=CARTESIAN_POINT('Ctrl Pts',(56.9318630101755,21.5021633286191,10.2548654909627));
#24554=CARTESIAN_POINT('Ctrl Pts',(56.8786112774649,21.680245449581,10.2658233392881));
#24555=CARTESIAN_POINT('Ctrl Pts',(56.8368634439123,21.7860332648842,10.2723111754453));
#24556=CARTESIAN_POINT('Ctrl Pts',(56.7569574689906,21.9468305989645,10.2828355271104));
#24557=CARTESIAN_POINT('Ctrl Pts',(56.7246563837557,22.0044635619656,10.2867526187784));
#24558=CARTESIAN_POINT('Ctrl Pts',(56.668289269915,22.0942757430114,10.2931910403408));
#24559=CARTESIAN_POINT('Ctrl Pts',(56.646005966302,22.1275160797707,10.295652300041));
#24560=CARTESIAN_POINT('Ctrl Pts',(56.6154237536345,22.1702956459808,10.2989366625541));
#24561=CARTESIAN_POINT('Ctrl Pts',(56.6080116293105,22.1804593984034,10.2997259214886));
#24562=CARTESIAN_POINT('Ctrl Pts',(56.5956929516429,22.1970198593235,10.3010270369599));
#24563=CARTESIAN_POINT('Ctrl Pts',(56.5908427997072,22.2034582348631,10.3015366958463));
#24564=CARTESIAN_POINT('Ctrl Pts',(56.5813561869833,22.2158937588734,10.3025286088321));
#24565=CARTESIAN_POINT('Ctrl Pts',(56.5767242963471,22.2218942317902,10.3030106776787));
#24566=CARTESIAN_POINT('Ctrl Pts',(56.5659073101299,22.2357433853213,10.3041313998706));
#24567=CARTESIAN_POINT('Ctrl Pts',(56.5596972558805,22.2435722263983,10.3047710386005));
#24568=CARTESIAN_POINT('Ctrl Pts',(56.5392652172734,22.2689365252606,10.3068636067134));
#24569=CARTESIAN_POINT('Ctrl Pts',(56.5248047170542,22.2862767274663,10.308326086989));
#24570=CARTESIAN_POINT('Ctrl Pts',(56.3985891068265,22.4325074486482,10.3209407610409));
#24571=CARTESIAN_POINT('Ctrl Pts',(56.2710389719548,22.5467920526852,10.3327966342144));
#24572=CARTESIAN_POINT('Ctrl Pts',(56.0700775949723,22.6850366821492,10.3497978511851));
#24573=CARTESIAN_POINT('Ctrl Pts',(56.007353180692,22.7232688886676,10.3548926440658));
#24574=CARTESIAN_POINT('Ctrl Pts',(55.9221315553986,22.7689668090524,10.3614291946561));
#24575=CARTESIAN_POINT('Ctrl Pts',(55.9014104289643,22.7796149907972,10.3629897304113));
#24576=CARTESIAN_POINT('Ctrl Pts',(55.8663168042062,22.7968786364347,10.3655791628008));
#24577=CARTESIAN_POINT('Ctrl Pts',(55.852043945182,22.8036903261181,10.3666177409116));
#24578=CARTESIAN_POINT('Ctrl Pts',(55.8320845941086,22.8129260750081,10.3680484395896));
#24579=CARTESIAN_POINT('Ctrl Pts',(55.8264660156571,22.8154943273445,10.3684488188394));
#24580=CARTESIAN_POINT('Ctrl Pts',(55.8169071174857,22.8198101280026,10.3691258669876));
#24581=CARTESIAN_POINT('Ctrl Pts',(55.8129729263791,22.8215710699437,10.3694033434984));
#24582=CARTESIAN_POINT('Ctrl Pts',(55.8054159079038,22.8249242277133,10.3699340377519));
#24583=CARTESIAN_POINT('Ctrl Pts',(55.8017940255722,22.8265184266309,10.3701873808363));
#24584=CARTESIAN_POINT('Ctrl Pts',(55.7921286757762,22.8307384141293,10.3708608393988));
#24585=CARTESIAN_POINT('Ctrl Pts',(55.7860768378138,22.8333450815236,10.3712798028832));
#24586=CARTESIAN_POINT('Ctrl Pts',(55.7641699528139,22.8426524690202,10.3727870034766));
#24587=CARTESIAN_POINT('Ctrl Pts',(55.7482407275905,22.8491781144444,10.3738652321395));
#24588=CARTESIAN_POINT('Ctrl Pts',(55.5978827768747,22.9085133556632,10.3838953973148));
#24589=CARTESIAN_POINT('Ctrl Pts',(55.4581569276992,22.9467899973822,10.3921391989112));
#24590=CARTESIAN_POINT('Ctrl Pts',(55.2653737834051,22.9776708571072,10.4034861834246));
#24591=CARTESIAN_POINT('Ctrl Pts',(55.2149845040072,22.9837793810589,10.4064469079153));
#24592=CARTESIAN_POINT('Ctrl Pts',(55.1644480736098,22.9879598571365,10.4094440176549));
#24593=CARTESIAN_POINT('Origin',(55.,21.,6.22095488139522));
#24594=CARTESIAN_POINT('',(55.1644483680005,22.9879598327838,11.3667309363937));
#24595=CARTESIAN_POINT('',(55.1644483504356,22.9879598342369,11.2090168340879));
#24596=CARTESIAN_POINT('',(55.1644483516311,22.987959834138,6.22095488139522));
#24597=CARTESIAN_POINT('',(53.0052507453988,21.0017244615935,10.7798738016618));
#24598=CARTESIAN_POINT('Ctrl Pts',(55.1644483680005,22.9879598327838,11.3667309363937));
#24599=CARTESIAN_POINT('Ctrl Pts',(55.2668183824715,22.9794915621808,11.3603918485463));
#24600=CARTESIAN_POINT('Ctrl Pts',(55.3684168750213,22.9631256322943,11.3544005539574));
#24601=CARTESIAN_POINT('Ctrl Pts',(55.6191159170458,22.9025732145644,11.3394236116951));
#24602=CARTESIAN_POINT('Ctrl Pts',(55.7651174048343,22.8486964255162,11.3304829507699));
#24603=CARTESIAN_POINT('Ctrl Pts',(55.924298641941,22.767837415238,11.3194830744304));
#24604=CARTESIAN_POINT('Ctrl Pts',(55.9450095793867,22.7568534171218,11.3180269037287));
#24605=CARTESIAN_POINT('Ctrl Pts',(55.9738224391431,22.7409156810808,11.3159634403282));
#24606=CARTESIAN_POINT('Ctrl Pts',(55.98209041941,22.7362649437039,11.3153668921521));
#24607=CARTESIAN_POINT('Ctrl Pts',(55.9964121464573,22.7280739491388,11.3143256730236));
#24608=CARTESIAN_POINT('Ctrl Pts',(56.0024810278712,22.7245603863059,11.3138819658548));
#24609=CARTESIAN_POINT('Ctrl Pts',(56.0151210062071,22.7171532382289,11.3129525566407));
#24610=CARTESIAN_POINT('Ctrl Pts',(56.0216885079963,22.7132537730195,11.3124666467453));
#24611=CARTESIAN_POINT('Ctrl Pts',(56.0372290606589,22.7039054090287,11.3113096003018));
#24612=CARTESIAN_POINT('Ctrl Pts',(56.0461817395778,22.698423247601,11.3106372566652));
#24613=CARTESIAN_POINT('Ctrl Pts',(56.0761793682199,22.6797270680567,11.3083645971277));
#24614=CARTESIAN_POINT('Ctrl Pts',(56.097019867477,22.6661909775211,11.3067524688492));
#24615=CARTESIAN_POINT('Ctrl Pts',(56.1462210109412,22.632911140739,11.3028644633317));
#24616=CARTESIAN_POINT('Ctrl Pts',(56.1743313645086,22.6128133826787,11.3005758487876));
#24617=CARTESIAN_POINT('Ctrl Pts',(56.281644685509,22.5317954150987,11.2915715975044));
#24618=CARTESIAN_POINT('Ctrl Pts',(56.3567406605626,22.4656947013413,11.2846754087921));
#24619=CARTESIAN_POINT('Ctrl Pts',(56.441722152327,22.3787440751148,11.2762046689164));
#24620=CARTESIAN_POINT('Ctrl Pts',(56.4566281366828,22.3629865939187,11.2746915864095));
#24621=CARTESIAN_POINT('Ctrl Pts',(56.4764066300199,22.3413831651284,11.2726486410622));
#24622=CARTESIAN_POINT('Ctrl Pts',(56.4815070414649,22.3357478127075,11.2721185519505));
#24623=CARTESIAN_POINT('Ctrl Pts',(56.5265587813653,22.2853954861329,11.267407818775));
#24624=CARTESIAN_POINT('Ctrl Pts',(56.5645088241818,22.2389253510599,11.2632379049449));
#24625=CARTESIAN_POINT('Ctrl Pts',(56.6298007217073,22.1511810155058,11.2557602316587));
#24626=CARTESIAN_POINT('Ctrl Pts',(56.657812784585,22.1104619749982,11.252432760538));
#24627=CARTESIAN_POINT('Ctrl Pts',(56.6888933541455,22.0614804497966,11.2486302821579));
#24628=CARTESIAN_POINT('Ctrl Pts',(56.6934536542744,22.0541898473052,11.2480693564371));
#24629=CARTESIAN_POINT('Ctrl Pts',(56.7007755854378,22.0423140673116,11.24716410446));
#24630=CARTESIAN_POINT('Ctrl Pts',(56.7035661016564,22.0377469565569,11.2468179776615));
#24631=CARTESIAN_POINT('Ctrl Pts',(56.7085076370482,22.0295857225005,11.2462031137966));
#24632=CARTESIAN_POINT('Ctrl Pts',(56.7106657467263,22.0259960087207,11.24593392164));
#24633=CARTESIAN_POINT('Ctrl Pts',(56.7153201603359,22.0181985294533,11.2453519171114));
#24634=CARTESIAN_POINT('Ctrl Pts',(56.7178122926903,22.0139883757513,11.2450393742355));
#24635=CARTESIAN_POINT('Ctrl Pts',(56.7247682594399,22.0021378711376,11.244164295987));
#24636=CARTESIAN_POINT('Ctrl Pts',(56.7291968481554,21.9944768115866,11.243603983246));
#24637=CARTESIAN_POINT('Ctrl Pts',(56.7558984918794,21.9475676854414,11.2402043981201));
#24638=CARTESIAN_POINT('Ctrl Pts',(56.7768872557064,21.9075992616797,11.2374404428493));
#24639=CARTESIAN_POINT('Ctrl Pts',(56.844431519403,21.767633247628,11.2280916919654));
#24640=CARTESIAN_POINT('Ctrl Pts',(56.8840445319404,21.664506016896,11.221758379718));
#24641=CARTESIAN_POINT('Ctrl Pts',(56.9515483192831,21.4331078739736,11.2077534366685));
#24642=CARTESIAN_POINT('Ctrl Pts',(56.9757305176247,21.3043116452713,11.2000726095537));
#24643=CARTESIAN_POINT('Ctrl Pts',(56.9884874826193,21.1586940409902,11.1909990067534));
#24644=CARTESIAN_POINT('Ctrl Pts',(56.9896569452038,21.143288124396,11.1900346392103));
#24645=CARTESIAN_POINT('Ctrl Pts',(56.991263920786,21.1182712409262,11.1884608183101));
#24646=CARTESIAN_POINT('Ctrl Pts',(56.9918110848332,21.1086677770637,11.187854792455));
#24647=CARTESIAN_POINT('Ctrl Pts',(56.9926613957655,21.0915665240527,11.1867721380226));
#24648=CARTESIAN_POINT('Ctrl Pts',(56.9929917363589,21.084070225366,11.1862963692656));
#24649=CARTESIAN_POINT('Ctrl Pts',(56.9935988669506,21.0682658059252,11.1852907234725));
#24650=CARTESIAN_POINT('Ctrl Pts',(56.9938660335417,21.0599574799825,11.1847605546401));
#24651=CARTESIAN_POINT('Ctrl Pts',(56.9944364732796,21.0379332592708,11.1833510470357));
#24652=CARTESIAN_POINT('Ctrl Pts',(56.9946501856733,21.0242156829173,11.1824689294788));
#24653=CARTESIAN_POINT('Ctrl Pts',(56.9949937782996,20.958925206455,11.1782495463655));
#24654=CARTESIAN_POINT('Ctrl Pts',(56.9932650387472,20.907366358009,11.1748549551963));
#24655=CARTESIAN_POINT('Ctrl Pts',(56.9769148115492,20.6815676758152,11.1597028598214));
#24656=CARTESIAN_POINT('Ctrl Pts',(56.9414194939986,20.5096282067382,11.1473262299537));
#24657=CARTESIAN_POINT('Ctrl Pts',(56.878786097787,20.3295961860727,11.1341886500161));
#24658=CARTESIAN_POINT('Ctrl Pts',(56.8734031328936,20.3146977337771,11.1331008172196));
#24659=CARTESIAN_POINT('Ctrl Pts',(56.8506395016987,20.2539681956921,11.1286677791383));
#24660=CARTESIAN_POINT('Ctrl Pts',(56.831748361077,20.2087169627035,11.1253671613535));
#24661=CARTESIAN_POINT('Ctrl Pts',(56.8076122310888,20.1564128912273,11.1215914335513));
#24662=CARTESIAN_POINT('Ctrl Pts',(56.8039666946028,20.1486449864166,11.1210317356633));
#24663=CARTESIAN_POINT('Ctrl Pts',(56.7979684552558,20.1360754772306,11.1201280687724));
#24664=CARTESIAN_POINT('Ctrl Pts',(56.7956464181313,20.13125948074,11.1197823092696));
#24665=CARTESIAN_POINT('Ctrl Pts',(56.7914709777949,20.1226877193273,11.119167842648));
#24666=CARTESIAN_POINT('Ctrl Pts',(56.789625086559,20.1189284065651,11.1188986828282));
#24667=CARTESIAN_POINT('Ctrl Pts',(56.7855953811288,20.1107864867254,11.1183164561528));
#24668=CARTESIAN_POINT('Ctrl Pts',(56.7834072693113,20.1064061043683,11.1180036606244));
#24669=CARTESIAN_POINT('Ctrl Pts',(56.7772112752573,20.0941157498714,11.1171271551517));
#24670=CARTESIAN_POINT('Ctrl Pts',(56.7731666872081,20.0862242628169,11.1165656794886));
#24671=CARTESIAN_POINT('Ctrl Pts',(56.7480564551115,20.038025683833,11.1131428660878));
#24672=CARTESIAN_POINT('Ctrl Pts',(56.72566825211,19.9984183702538,11.1103580455712));
#24673=CARTESIAN_POINT('Ctrl Pts',(56.6397739885888,19.8579067435847,11.1004545116726));
#24674=CARTESIAN_POINT('Ctrl Pts',(56.5686093605042,19.7619754974629,11.0936347196209));
#24675=CARTESIAN_POINT('Ctrl Pts',(56.4812645169098,19.6639502743727,11.0859932787979));
#24676=CARTESIAN_POINT('Ctrl Pts',(56.4731478469768,19.6550060013989,11.0852894235209));
#24677=CARTESIAN_POINT('Ctrl Pts',(56.3907885692442,19.5658890235545,11.0782048107881));
#24678=CARTESIAN_POINT('Ctrl Pts',(56.3101686723837,19.49188180673,11.0717182834002));
#24679=CARTESIAN_POINT('Ctrl Pts',(56.2116735057882,19.4153502894543,11.0639760452976));
#24680=CARTESIAN_POINT('Ctrl Pts',(56.1993347959456,19.4059914003176,11.0630094481628));
#24681=CARTESIAN_POINT('Ctrl Pts',(56.1791488569266,19.3910474614843,11.0614327028074));
#24682=CARTESIAN_POINT('Ctrl Pts',(56.1713678022771,19.3853738003672,11.0608260033716));
#24683=CARTESIAN_POINT('Ctrl Pts',(56.1574501912089,19.3753791393151,11.0597425950025));
#24684=CARTESIAN_POINT('Ctrl Pts',(56.1513297161945,19.371035983149,11.0592667503456));
#24685=CARTESIAN_POINT('Ctrl Pts',(56.1383834803816,19.3619586035276,11.0582614090146));
#24686=CARTESIAN_POINT('Ctrl Pts',(56.1315523792665,19.3572322822449,11.0577316232943));
#24687=CARTESIAN_POINT('Ctrl Pts',(56.1133834827024,19.3448286288575,11.0563242225301));
#24688=CARTESIAN_POINT('Ctrl Pts',(56.1019959754553,19.3372252401561,11.0554438434826));
#24689=CARTESIAN_POINT('Ctrl Pts',(56.0476065227738,19.3017137651208,11.0512462931027));
#24690=CARTESIAN_POINT('Ctrl Pts',(56.0036208964796,19.2753551482622,11.0478725155148));
#24691=CARTESIAN_POINT('Ctrl Pts',(55.8074107151989,19.1678243935281,11.0329008379241));
#24692=CARTESIAN_POINT('Ctrl Pts',(55.6460465504788,19.1049045773506,11.0207018788349));
#24693=CARTESIAN_POINT('Ctrl Pts',(55.4574400959387,19.058286000775,11.0072958427948));
#24694=CARTESIAN_POINT('Ctrl Pts',(55.4361496230854,19.0533931435388,11.0057956343937));
#24695=CARTESIAN_POINT('Ctrl Pts',(55.369807161911,19.0392898166312,11.0011690891197));
#24696=CARTESIAN_POINT('Ctrl Pts',(55.3245105118912,19.031285842289,10.9980785624643));
#24697=CARTESIAN_POINT('Ctrl Pts',(55.2706268478495,19.0236751947435,10.994512796268));
#24698=CARTESIAN_POINT('Ctrl Pts',(55.2622721737798,19.0225491309478,10.993963056626));
#24699=CARTESIAN_POINT('Ctrl Pts',(55.2486525781655,19.0208012837882,10.9930722560897));
#24700=CARTESIAN_POINT('Ctrl Pts',(55.2433919761061,19.0201474776072,10.9927294852665));
#24701=CARTESIAN_POINT('Ctrl Pts',(55.2339739705637,19.0190150794591,10.9921182319632));
#24702=CARTESIAN_POINT('Ctrl Pts',(55.2298176223591,19.0185285932384,10.9918493162519));
#24703=CARTESIAN_POINT('Ctrl Pts',(55.220761025863,19.0174974301263,10.9912651957709));
#24704=CARTESIAN_POINT('Ctrl Pts',(55.2158602871363,19.0169578401349,10.9909502776134));
#24705=CARTESIAN_POINT('Ctrl Pts',(55.2019838591642,19.0154820432115,10.9900617510789));
#24706=CARTESIAN_POINT('Ctrl Pts',(55.1930036091368,19.0145885528791,10.9894904762116));
#24707=CARTESIAN_POINT('Ctrl Pts',(55.1356207302212,19.0092722631872,10.9858622039911));
#24708=CARTESIAN_POINT('Ctrl Pts',(55.0870718107209,19.0065584359232,10.9828927767209));
#24709=CARTESIAN_POINT('Ctrl Pts',(54.9360303379903,19.0036451147226,10.973832597907));
#24710=CARTESIAN_POINT('Ctrl Pts',(54.8335858656606,19.0095643446713,10.9679356839063));
#24711=CARTESIAN_POINT('Ctrl Pts',(54.5984807913196,19.0414349979441,10.9541583559392));
#24712=CARTESIAN_POINT('Ctrl Pts',(54.4671159485836,19.0730277110291,10.9462568724126));
#24713=CARTESIAN_POINT('Ctrl Pts',(54.3253670049151,19.1227316039943,10.9369328001878));
#24714=CARTESIAN_POINT('Ctrl Pts',(54.3108462343836,19.1280135216724,10.9359683500865));
#24715=CARTESIAN_POINT('Ctrl Pts',(54.2873874432543,19.136856570102,10.9343944208915));
#24716=CARTESIAN_POINT('Ctrl Pts',(54.2784110753953,19.1403146731038,10.9337883700867));
#24717=CARTESIAN_POINT('Ctrl Pts',(54.2624778729155,19.1465855888969,10.9327056877423));
#24718=CARTESIAN_POINT('Ctrl Pts',(54.2555111909248,19.149373004122,10.9322299161883));
#24719=CARTESIAN_POINT('Ctrl Pts',(54.2484051403963,19.1522628007106,10.9317421544061));
#24720=CARTESIAN_POINT('Ctrl Pts',(54.2482498099747,19.1523259913029,10.9317314912612));
#24721=CARTESIAN_POINT('Ctrl Pts',(54.2479536870199,19.1524465017919,10.9317111606623));
#24722=CARTESIAN_POINT('Ctrl Pts',(54.2478128891772,19.1525038197812,10.9317014930595));
#24723=CARTESIAN_POINT('Ctrl Pts',(54.2475444218924,19.1526131470431,10.9316830573906));
#24724=CARTESIAN_POINT('Ctrl Pts',(54.2474167555492,19.1526651517185,10.9316742897144));
#24725=CARTESIAN_POINT('Ctrl Pts',(54.2471732977741,19.1527643532698,10.9316575683275));
#24726=CARTESIAN_POINT('Ctrl Pts',(54.2470575054225,19.1528115477855,10.9316496146988));
#24727=CARTESIAN_POINT('Ctrl Pts',(54.2468366611527,19.1529015834592,10.9316344439024));
#24728=CARTESIAN_POINT('Ctrl Pts',(54.2467316084176,19.1529444227057,10.9316272267979));
#24729=CARTESIAN_POINT('Ctrl Pts',(54.2465312209705,19.1530261582444,10.9316134591566));
#24730=CARTESIAN_POINT('Ctrl Pts',(54.2464358855569,19.1530650529796,10.9316069086695));
#24731=CARTESIAN_POINT('Ctrl Pts',(54.2462540108407,19.1531392702581,10.9315944112028));
#24732=CARTESIAN_POINT('Ctrl Pts',(54.2461674710736,19.1531745914762,10.9315884642718));
#24733=CARTESIAN_POINT('Ctrl Pts',(54.2460023565476,19.1532419965324,10.9315771170385));
#24734=CARTESIAN_POINT('Ctrl Pts',(54.2459237813517,19.1532740793035,10.9315717167723));
#24735=CARTESIAN_POINT('Ctrl Pts',(54.2457738460258,19.1533353100513,10.9315614115192));
#24736=CARTESIAN_POINT('Ctrl Pts',(54.2457024855702,19.1533644571365,10.9315565065644));
#24737=CARTESIAN_POINT('Ctrl Pts',(54.2455663028737,19.1534200899924,10.931547145569));
#24738=CARTESIAN_POINT('Ctrl Pts',(54.2455014803539,19.1534465750336,10.9315426895541));
#24739=CARTESIAN_POINT('Ctrl Pts',(54.2453777623816,19.1534971310502,10.9315341845574));
#24740=CARTESIAN_POINT('Ctrl Pts',(54.2453188666397,19.1535212014491,10.9315301355926));
#24741=CARTESIAN_POINT('Ctrl Pts',(54.245177769322,19.1535788751045,10.9315204350148));
#24742=CARTESIAN_POINT('Ctrl Pts',(54.2450955687962,19.1536124810498,10.9315147833082));
#24743=CARTESIAN_POINT('Ctrl Pts',(54.2449329009808,19.1536789970222,10.9315035983899));
#24744=CARTESIAN_POINT('Ctrl Pts',(54.2448524335574,19.1537119068374,10.9314980651832));
#24745=CARTESIAN_POINT('Ctrl Pts',(54.2446931859958,19.1537770485491,10.9314871141471));
#24746=CARTESIAN_POINT('Ctrl Pts',(54.2446144057922,19.1538092802182,10.9314816963266));
#24747=CARTESIAN_POINT('Ctrl Pts',(54.2444584883135,19.1538730830289,10.9314709730527));
#24748=CARTESIAN_POINT('Ctrl Pts',(54.2443813509234,19.1539046539752,10.9314656676041));
#24749=CARTESIAN_POINT('Ctrl Pts',(54.2442286757409,19.1539671523534,10.931455166132));
#24750=CARTESIAN_POINT('Ctrl Pts',(54.2441531379659,19.1539980795471,10.9314499701218));
#24751=CARTESIAN_POINT('Ctrl Pts',(54.2440036202437,19.1540593068339,10.9314396846898));
#24752=CARTESIAN_POINT('Ctrl Pts',(54.2439296402393,19.1540896067299,10.9314345952756));
#24753=CARTESIAN_POINT('Ctrl Pts',(54.2437831977011,19.1541495952941,10.931424520294));
#24754=CARTESIAN_POINT('Ctrl Pts',(54.2437107349883,19.1541792838251,10.9314195347254));
#24755=CARTESIAN_POINT('Ctrl Pts',(54.2355026579802,19.1575427606296,10.9308547738208));
#24756=CARTESIAN_POINT('Ctrl Pts',(54.2273892818791,19.1609302517248,10.9302931858881));
#24757=CARTESIAN_POINT('Ctrl Pts',(54.2044748184771,19.1706758780015,10.9286974669543));
#24758=CARTESIAN_POINT('Ctrl Pts',(54.1897282545356,19.1771597077648,10.9276590854953));
#24759=CARTESIAN_POINT('Ctrl Pts',(54.1566999366788,19.192161705036,10.9253069124052));
#24760=CARTESIAN_POINT('Ctrl Pts',(54.1384658094063,19.2007798670462,10.9239897958124));
#24761=CARTESIAN_POINT('Ctrl Pts',(53.9665274189338,19.2852576357964,10.911390175425));
#24762=CARTESIAN_POINT('Ctrl Pts',(53.8230966453887,19.3803446406582,10.8994091001011));
#24763=CARTESIAN_POINT('Ctrl Pts',(53.6230839921941,19.5536803982552,10.8809917275003));
#24764=CARTESIAN_POINT('Ctrl Pts',(53.556921678593,19.6196858246545,10.8745568848178));
#24765=CARTESIAN_POINT('Ctrl Pts',(53.4887599033793,19.697966961325,10.8677402494761));
#24766=CARTESIAN_POINT('Ctrl Pts',(53.4819625987441,19.7058983335307,10.8670582596291));
#24767=CARTESIAN_POINT('Ctrl Pts',(53.471812472039,19.7179319439403,10.8660369854317));
#24768=CARTESIAN_POINT('Ctrl Pts',(53.468413302882,19.7219945963467,10.8656944744065));
#24769=CARTESIAN_POINT('Ctrl Pts',(53.4623579488112,19.7292907513778,10.8650834987691));
#24770=CARTESIAN_POINT('Ctrl Pts',(53.4596957262742,19.732519105665,10.8648146026209));
#24771=CARTESIAN_POINT('Ctrl Pts',(53.4539169413917,19.7395718680027,10.8642303100145));
#24772=CARTESIAN_POINT('Ctrl Pts',(53.4508044060781,19.7433994616067,10.863915201531));
#24773=CARTESIAN_POINT('Ctrl Pts',(53.4420296808376,19.7542722047618,10.8630255943933));
#24774=CARTESIAN_POINT('Ctrl Pts',(53.4364010420819,19.7613444541075,10.8624534382661));
#24775=CARTESIAN_POINT('Ctrl Pts',(53.4006303502014,19.8069218623397,10.8588057787777));
#24776=CARTESIAN_POINT('Ctrl Pts',(53.3718620015992,19.8464895939911,10.8558189291558));
#24777=CARTESIAN_POINT('Ctrl Pts',(53.2788507577538,19.9848399916961,10.8458232836809));
#24778=CARTESIAN_POINT('Ctrl Pts',(53.2219117192847,20.0882377405094,10.8390848626177));
#24779=CARTESIAN_POINT('Ctrl Pts',(53.1529876377438,20.244749665733,10.8291263213151));
#24780=CARTESIAN_POINT('Ctrl Pts',(53.1335039572553,20.2942735210264,10.8260097617835));
#24781=CARTESIAN_POINT('Ctrl Pts',(53.1052921918637,20.3753589883507,10.8209036776332));
#24782=CARTESIAN_POINT('Ctrl Pts',(53.0953202619795,20.4064606013586,10.8189445623523));
#24783=CARTESIAN_POINT('Ctrl Pts',(53.0746973840322,20.4766655414888,10.814506264319));
#24784=CARTESIAN_POINT('Ctrl Pts',(53.0644658403725,20.5158757536743,10.8120163845285));
#24785=CARTESIAN_POINT('Ctrl Pts',(53.0525133445694,20.568149124727,10.8086699809758));
#24786=CARTESIAN_POINT('Ctrl Pts',(53.0497171011338,20.5809581728341,10.8078478853144));
#24787=CARTESIAN_POINT('Ctrl Pts',(53.0453818911083,20.6018009269637,10.8065063942485));
#24788=CARTESIAN_POINT('Ctrl Pts',(53.0437656848052,20.609818306175,10.8059894713785));
#24789=CARTESIAN_POINT('Ctrl Pts',(53.0407544461699,20.6252450600583,10.804992992783));
#24790=CARTESIAN_POINT('Ctrl Pts',(53.0393520246413,20.6326528625748,10.8045136818204));
#24791=CARTESIAN_POINT('Ctrl Pts',(53.0366633021752,20.6473092452745,10.8035636930044));
#24792=CARTESIAN_POINT('Ctrl Pts',(53.0353750658187,20.6545573519588,10.8030930851169));
#24793=CARTESIAN_POINT('Ctrl Pts',(53.0324989239059,20.6712762642178,10.8020056345429));
#24794=CARTESIAN_POINT('Ctrl Pts',(53.0309392386597,20.6807516770672,10.801387908206));
#24795=CARTESIAN_POINT('Ctrl Pts',(53.0270893902751,20.705242487661,10.7997874992393));
#24796=CARTESIAN_POINT('Ctrl Pts',(53.0249022367707,20.7202732233222,10.7988016081118));
#24797=CARTESIAN_POINT('Ctrl Pts',(53.0110638895879,20.8236460265885,10.7919949654859));
#24798=CARTESIAN_POINT('Ctrl Pts',(53.0051737349807,20.9126436292466,10.7859966396632));
#24799=CARTESIAN_POINT('Ctrl Pts',(53.0052507453988,21.0017244615935,10.7798738016618));
#24800=CARTESIAN_POINT('Ctrl Pts',(53.0052507436693,21.0017224598663,10.7798739392475));
#24801=CARTESIAN_POINT('Ctrl Pts',(53.0053401082293,21.1052139218134,10.7727606100826));
#24802=CARTESIAN_POINT('Ctrl Pts',(53.0134834815291,21.2085419252929,10.7654959353685));
#24803=CARTESIAN_POINT('Ctrl Pts',(53.0415117213874,21.3862523847116,10.7530068709339));
#24804=CARTESIAN_POINT('Ctrl Pts',(53.0577462375717,21.460998914051,10.7477591986531));
#24805=CARTESIAN_POINT('Ctrl Pts',(53.0822721918839,21.549158293487,10.7417069013195));
#24806=CARTESIAN_POINT('Ctrl Pts',(53.0864768818613,21.5636347101916,10.7407176746211));
#24807=CARTESIAN_POINT('Ctrl Pts',(53.092602145558,21.5838644838402,10.739343108748));
#24808=CARTESIAN_POINT('Ctrl Pts',(53.0943853379086,21.5896584372072,10.7389503270862));
#24809=CARTESIAN_POINT('Ctrl Pts',(53.0974753413965,21.5995380592557,10.7382822242631));
#24810=CARTESIAN_POINT('Ctrl Pts',(53.0987689608607,21.6036277812199,10.7380061457142));
#24811=CARTESIAN_POINT('Ctrl Pts',(53.101290137837,21.6115098606777,10.7374750396282));
#24812=CARTESIAN_POINT('Ctrl Pts',(53.1025158758534,21.6153027301032,10.7372199038554));
#24813=CARTESIAN_POINT('Ctrl Pts',(53.105494283013,21.6244254392014,10.7366072314572));
#24814=CARTESIAN_POINT('Ctrl Pts',(53.1072580977335,21.6297516447312,10.7362503414788));
#24815=CARTESIAN_POINT('Ctrl Pts',(53.1138234486359,21.6493003229001,10.7349432016805));
#24816=CARTESIAN_POINT('Ctrl Pts',(53.1187631524077,21.6634763350936,10.7340006673194));
#24817=CARTESIAN_POINT('Ctrl Pts',(53.1705796033817,21.8069465170489,10.724503332196));
#24818=CARTESIAN_POINT('Ctrl Pts',(53.2305556955158,21.9311389198942,10.7166110483166));
#24819=CARTESIAN_POINT('Ctrl Pts',(53.3502739136803,22.1249793055242,10.7033867006442));
#24820=CARTESIAN_POINT('Ctrl Pts',(53.4028586232198,22.1984624953458,10.6981264450733));
#24821=CARTESIAN_POINT('Ctrl Pts',(53.4946415376753,22.3099055752745,10.6894539529229));
#24822=CARTESIAN_POINT('Ctrl Pts',(53.5307317734994,22.3502617528428,10.686150040811));
#24823=CARTESIAN_POINT('Ctrl Pts',(53.5778654044065,22.3988369784169,10.6819314277818));
#24824=CARTESIAN_POINT('Ctrl Pts',(53.5874139943019,22.4084787759432,10.6810814875969));
#24825=CARTESIAN_POINT('Ctrl Pts',(53.6021234090578,22.4230317396734,10.6797788315187));
#24826=CARTESIAN_POINT('Ctrl Pts',(53.6072135283177,22.4280140537797,10.6793292459085));
#24827=CARTESIAN_POINT('Ctrl Pts',(53.6176347302153,22.4381058198931,10.6784111360838));
#24828=CARTESIAN_POINT('Ctrl Pts',(53.6229677138441,22.4432131404622,10.6779425300285));
#24829=CARTESIAN_POINT('Ctrl Pts',(53.6346476617258,22.4542751789837,10.6769188116558));
#24830=CARTESIAN_POINT('Ctrl Pts',(53.6410054621656,22.4602181843866,10.6763632098797));
#24831=CARTESIAN_POINT('Ctrl Pts',(53.6584935857218,22.4763522077062,10.6748392707228));
#24832=CARTESIAN_POINT('Ctrl Pts',(53.6697008082327,22.4864586574664,10.6738673878544));
#24833=CARTESIAN_POINT('Ctrl Pts',(53.7287419271851,22.5384982602923,10.6687707313523));
#24834=CARTESIAN_POINT('Ctrl Pts',(53.7784421657646,22.5782486980455,10.6645574323274));
#24835=CARTESIAN_POINT('Ctrl Pts',(53.9697094048945,22.7167720033435,10.6486115837678));
#24836=CARTESIAN_POINT('Ctrl Pts',(54.1219852859054,22.7994116425068,10.6363529486174));
#24837=CARTESIAN_POINT('Ctrl Pts',(54.3321809163916,22.8803790437716,10.6209278774489));
#24838=CARTESIAN_POINT('Ctrl Pts',(54.382120722739,22.8973755447677,10.6173718475456));
#24839=CARTESIAN_POINT('Ctrl Pts',(54.4415103701549,22.9149939255439,10.6133138458856));
#24840=CARTESIAN_POINT('Ctrl Pts',(54.4503590526472,22.9175524082494,10.6127136263765));
#24841=CARTESIAN_POINT('Ctrl Pts',(54.46400946534,22.921396995067,10.6117947917815));
#24842=CARTESIAN_POINT('Ctrl Pts',(54.4687986708469,22.9227265575506,10.6114737603378));
#24843=CARTESIAN_POINT('Ctrl Pts',(54.477626350717,22.9251417661823,10.6108845475352));
#24844=CARTESIAN_POINT('Ctrl Pts',(54.4816632509689,22.9262326091559,10.6106160774727));
#24845=CARTESIAN_POINT('Ctrl Pts',(54.4907766289446,22.9286644830695,10.6100121842035));
#24846=CARTESIAN_POINT('Ctrl Pts',(54.4958549792744,22.9299981682587,10.6096771863157));
#24847=CARTESIAN_POINT('Ctrl Pts',(54.5108401365037,22.9338704137622,10.6086929816708));
#24848=CARTESIAN_POINT('Ctrl Pts',(54.5207614454318,22.9363529036814,10.6080468977304));
#24849=CARTESIAN_POINT('Ctrl Pts',(54.5991804092406,22.9553350923326,10.6029805855274));
#24850=CARTESIAN_POINT('Ctrl Pts',(54.6684975544394,22.9682733786652,10.5987441951056));
#24851=CARTESIAN_POINT('Ctrl Pts',(54.8796520606731,22.9962105182464,10.5861740484261));
#24852=CARTESIAN_POINT('Ctrl Pts',(55.0224939943398,22.9997026117018,10.5780915871545));
#24853=CARTESIAN_POINT('Ctrl Pts',(55.1644484221208,22.9879598283069,10.5696416509586));
#24854=CARTESIAN_POINT('Ctrl Pts',(55.1644480736098,22.9879598571365,10.4094440176549));
#24855=CARTESIAN_POINT('Ctrl Pts',(55.0863476134817,22.9944204856899,10.4140758376681));
#24856=CARTESIAN_POINT('Ctrl Pts',(55.0078958510275,22.9962763510142,10.4187968915192));
#24857=CARTESIAN_POINT('Ctrl Pts',(54.9125225979619,22.9929033495909,10.424722003396));
#24858=CARTESIAN_POINT('Ctrl Pts',(54.8955568817554,22.9920862591188,10.4257829955949));
#24859=CARTESIAN_POINT('Ctrl Pts',(54.869604315938,22.9905039122646,10.4274175598496));
#24860=CARTESIAN_POINT('Ctrl Pts',(54.8606085078574,22.9898941848176,10.4279862681447));
#24861=CARTESIAN_POINT('Ctrl Pts',(54.8442555387887,22.9886743629352,10.4290240905391));
#24862=CARTESIAN_POINT('Ctrl Pts',(54.8368970046441,22.988084371827,10.4294925663439));
#24863=CARTESIAN_POINT('Ctrl Pts',(54.8208781677725,22.9867104836328,10.430515682826));
#24864=CARTESIAN_POINT('Ctrl Pts',(54.812219407468,22.9859107788805,10.4310708106726));
#24865=CARTESIAN_POINT('Ctrl Pts',(54.7885737291298,22.9835708890003,10.432592641983));
#24866=CARTESIAN_POINT('Ctrl Pts',(54.7735988359574,22.9819175139124,10.4335628761634));
#24867=CARTESIAN_POINT('Ctrl Pts',(54.6958225854969,22.9724372954723,10.4386367051597));
#24868=CARTESIAN_POINT('Ctrl Pts',(54.6334072132447,22.9617953627795,10.4428278850709));
#24869=CARTESIAN_POINT('Ctrl Pts',(54.4027392660803,22.9110737283502,10.4587716167255));
#24870=CARTESIAN_POINT('Ctrl Pts',(54.2394431953386,22.8521510858263,10.4710549008445));
#24871=CARTESIAN_POINT('Ctrl Pts',(54.038910143789,22.7487473094079,10.4865057328242));
#24872=CARTESIAN_POINT('Ctrl Pts',(53.9929928237833,22.7227154422734,10.490063854692));
#24873=CARTESIAN_POINT('Ctrl Pts',(53.9403320782204,22.6900344036017,10.4941237899967));
#24874=CARTESIAN_POINT('Ctrl Pts',(53.9325399620683,22.6851235756166,10.4947239675833));
#24875=CARTESIAN_POINT('Ctrl Pts',(53.9205964309163,22.6774803100883,10.4956426939913));
#24876=CARTESIAN_POINT('Ctrl Pts',(53.9164208693105,22.6747861130678,10.4959636591205));
#24877=CARTESIAN_POINT('Ctrl Pts',(53.9087511630472,22.6697966985182,10.4965527228833));
#24878=CARTESIAN_POINT('Ctrl Pts',(53.9052541812232,22.6675061113563,10.4968211102632));
#24879=CARTESIAN_POINT('Ctrl Pts',(53.8973831557249,22.6623150125175,10.497424777244));
#24880=CARTESIAN_POINT('Ctrl Pts',(53.8930133506873,22.6594082276171,10.4977596320673));
#24881=CARTESIAN_POINT('Ctrl Pts',(53.8801677358121,22.650790029003,10.4987432952975));
#24882=CARTESIAN_POINT('Ctrl Pts',(53.8717241377704,22.6450305799475,10.4993889850816));
#24883=CARTESIAN_POINT('Ctrl Pts',(53.8055331675151,22.5991317683604,10.5044468271993));
#24884=CARTESIAN_POINT('Ctrl Pts',(53.7498941574263,22.5560241305798,10.5086758136785));
#24885=CARTESIAN_POINT('Ctrl Pts',(53.5683572067163,22.3993369449524,10.5228293258379));
#24886=CARTESIAN_POINT('Ctrl Pts',(53.4547065097968,22.2727196755946,10.5323833857303));
#24887=CARTESIAN_POINT('Ctrl Pts',(53.3395478249205,22.1059071106663,10.5445940705102));
#24888=CARTESIAN_POINT('Ctrl Pts',(53.3213550154786,22.0780922029669,10.5466164820234));
#24889=CARTESIAN_POINT('Ctrl Pts',(53.2911753873372,22.0293334992437,10.5501487454425));
#24890=CARTESIAN_POINT('Ctrl Pts',(53.278857876023,22.0086023599044,10.5516466613861));
#24891=CARTESIAN_POINT('Ctrl Pts',(53.261784537033,21.978643003503,10.5538082858875));
#24892=CARTESIAN_POINT('Ctrl Pts',(53.2567199182606,21.9695925299296,10.5544608960713));
#24893=CARTESIAN_POINT('Ctrl Pts',(53.2480599138474,21.9538298959036,10.5555970129156));
#24894=CARTESIAN_POINT('Ctrl Pts',(53.2444319253344,21.9471358236188,10.5560793459627));
#24895=CARTESIAN_POINT('Ctrl Pts',(53.2375241102379,21.934214023006,10.5570101927488));
#24896=CARTESIAN_POINT('Ctrl Pts',(53.2342387413204,21.9279893738779,10.55745850101));
#24897=CARTESIAN_POINT('Ctrl Pts',(53.2265527933008,21.9132385381556,10.558520715992));
#24898=CARTESIAN_POINT('Ctrl Pts',(53.2221806833218,21.9046977917732,10.559135613073));
#24899=CARTESIAN_POINT('Ctrl Pts',(53.2070464692638,21.8746003146458,10.5613022719627));
#24900=CARTESIAN_POINT('Ctrl Pts',(53.1966138178407,21.8528811566704,10.5628654117797));
#24901=CARTESIAN_POINT('Ctrl Pts',(53.1291282369546,21.7056092602686,10.573466397367));
#24902=CARTESIAN_POINT('Ctrl Pts',(53.0848448398029,21.5746420688875,10.5829409461477));
#24903=CARTESIAN_POINT('Ctrl Pts',(53.0331408493616,21.3461132024955,10.599270808405));
#24904=CARTESIAN_POINT('Ctrl Pts',(53.018707549087,21.2506216440511,10.6060259627357));
#24905=CARTESIAN_POINT('Ctrl Pts',(53.0091279141836,21.1272759435081,10.6144291612223));
#24906=CARTESIAN_POINT('Ctrl Pts',(53.0075742506162,21.1000530517522,10.6162632944604));
#24907=CARTESIAN_POINT('Ctrl Pts',(53.005929789255,21.0550275790471,10.6192542956688));
#24908=CARTESIAN_POINT('Ctrl Pts',(53.0055183123431,21.0372409770852,10.6204248762878));
#24909=CARTESIAN_POINT('Ctrl Pts',(53.0052817470962,21.012981164723,10.6220044057902));
#24910=CARTESIAN_POINT('Ctrl Pts',(53.0052501351687,21.0065114263768,10.6224239878818));
#24911=CARTESIAN_POINT('Ctrl Pts',(53.0052499184983,20.9961071431697,10.623095952249));
#24912=CARTESIAN_POINT('Ctrl Pts',(53.0052614767333,20.9921727119171,10.623349418505));
#24913=CARTESIAN_POINT('Ctrl Pts',(53.0053102159789,20.9839068224652,10.6238805467052));
#24914=CARTESIAN_POINT('Ctrl Pts',(53.0053498648552,20.9795754134117,10.6241580626731));
#24915=CARTESIAN_POINT('Ctrl Pts',(53.00548163476,20.9689586256248,10.6248363973381));
#24916=CARTESIAN_POINT('Ctrl Pts',(53.0055893589523,20.9626734191028,10.6252363531352));
#24917=CARTESIAN_POINT('Ctrl Pts',(53.0060881023872,20.9398666868124,10.6266820980133));
#24918=CARTESIAN_POINT('Ctrl Pts',(53.0066547317768,20.9233491393244,10.6277185948844));
#24919=CARTESIAN_POINT('Ctrl Pts',(53.0085800783319,20.8821684737605,10.6302805963666));
#24920=CARTESIAN_POINT('Ctrl Pts',(53.0101917251743,20.8575194171634,10.6317942822705));
#24921=CARTESIAN_POINT('Ctrl Pts',(53.0190449357502,20.7522025049653,10.6382008516644));
#24922=CARTESIAN_POINT('Ctrl Pts',(53.030738186202,20.6719808779836,10.6429296916237));
#24923=CARTESIAN_POINT('Ctrl Pts',(53.0797404901348,20.4370561549053,10.6568724428793));
#24924=CARTESIAN_POINT('Ctrl Pts',(53.1306864232294,20.2858831203412,10.6660183651889));
#24925=CARTESIAN_POINT('Ctrl Pts',(53.2089979286368,20.1214349631584,10.6772432172742));
#24926=CARTESIAN_POINT('Ctrl Pts',(53.2193284645256,20.1006815042349,10.6786834597493));
#24927=CARTESIAN_POINT('Ctrl Pts',(53.2343712847124,20.0717371517246,10.6807278666122));
#24928=CARTESIAN_POINT('Ctrl Pts',(53.238783911721,20.063391991698,10.6813215498073));
#24929=CARTESIAN_POINT('Ctrl Pts',(53.2465713550007,20.0489140176549,10.6823590971529));
#24930=CARTESIAN_POINT('Ctrl Pts',(53.2499195531022,20.0427670156791,10.682802013815));
#24931=CARTESIAN_POINT('Ctrl Pts',(53.2569919885059,20.029943777177,10.6837310788419));
#24932=CARTESIAN_POINT('Ctrl Pts',(53.2607223837042,20.0232710845121,10.6842174417203));
#24933=CARTESIAN_POINT('Ctrl Pts',(53.2696895185394,20.007445519221,10.685377988833));
#24934=CARTESIAN_POINT('Ctrl Pts',(53.2749606201221,19.9983124786803,10.6860534009788));
#24935=CARTESIAN_POINT('Ctrl Pts',(53.2930441441609,19.9675459192176,10.6883481585971));
#24936=CARTESIAN_POINT('Ctrl Pts',(53.3061926523336,19.9461137177736,10.6899796339915));
#24937=CARTESIAN_POINT('Ctrl Pts',(53.3386517077019,19.8953822200822,10.6939229361675));
#24938=CARTESIAN_POINT('Ctrl Pts',(53.3583365981146,19.8663335527262,10.696247987536));
#24939=CARTESIAN_POINT('Ctrl Pts',(53.4385467685856,19.7544415188165,10.705472508389));
#24940=CARTESIAN_POINT('Ctrl Pts',(53.5046538440628,19.6758068028398,10.7125624110261));
#24941=CARTESIAN_POINT('Ctrl Pts',(53.6645774879033,19.5128954462777,10.7284739885947));
#24942=CARTESIAN_POINT('Ctrl Pts',(53.7609407657918,19.4316980676334,10.737294803976));
#24943=CARTESIAN_POINT('Ctrl Pts',(53.8770984665918,19.3512545577252,10.7466502190346));
#24944=CARTESIAN_POINT('Ctrl Pts',(53.889986342729,19.3425504219906,10.7476717215669));
#24945=CARTESIAN_POINT('Ctrl Pts',(53.9082507330908,19.3305237348263,10.7490948943379));
#24946=CARTESIAN_POINT('Ctrl Pts',(53.9135428641555,19.3270749101136,10.749504410973));
#24947=CARTESIAN_POINT('Ctrl Pts',(53.922133946302,19.3215341558295,10.7501644950792));
#24948=CARTESIAN_POINT('Ctrl Pts',(53.9254227638834,19.3194267097131,10.7504160768911));
#24949=CARTESIAN_POINT('Ctrl Pts',(53.9323981383867,19.3149857974539,10.7509472847016));
#24950=CARTESIAN_POINT('Ctrl Pts',(53.9360862023527,19.3126547390706,10.7512267457311));
#24951=CARTESIAN_POINT('Ctrl Pts',(53.9452370776753,19.3069128151169,10.7519167596891));
#24952=CARTESIAN_POINT('Ctrl Pts',(53.9507088712456,19.3035162341499,10.7523263801556));
#24953=CARTESIAN_POINT('Ctrl Pts',(53.9711795197516,19.2909461404471,10.7538481305647));
#24954=CARTESIAN_POINT('Ctrl Pts',(53.9862835180061,19.2819442326525,10.7549496402534));
#24955=CARTESIAN_POINT('Ctrl Pts',(54.0247353603372,19.2597107979409,10.757705668641));
#24956=CARTESIAN_POINT('Ctrl Pts',(54.0482353895762,19.2467481946488,10.7593459406939));
#24957=CARTESIAN_POINT('Ctrl Pts',(54.2278400653979,19.1523543101309,10.7716068696709));
#24958=CARTESIAN_POINT('Ctrl Pts',(54.3938566153392,19.0914331684165,10.7814557470698));
#24959=CARTESIAN_POINT('Ctrl Pts',(54.5886988562286,19.0479721222878,10.7932998580453));
#24960=CARTESIAN_POINT('Ctrl Pts',(54.6117578094609,19.0432554036462,10.7947045893341));
#24961=CARTESIAN_POINT('Ctrl Pts',(54.6859286022279,19.0294463978242,10.7992409975649));
#24962=CARTESIAN_POINT('Ctrl Pts',(54.7373105820563,19.0219413789412,10.8024114347813));
#24963=CARTESIAN_POINT('Ctrl Pts',(54.8031661041818,19.0149334711471,10.8065373944642));
#24964=CARTESIAN_POINT('Ctrl Pts',(54.8174241481265,19.0135713584646,10.8074343410588));
#24965=CARTESIAN_POINT('Ctrl Pts',(54.8401091413842,19.0116504895956,10.8088677273408));
#24966=CARTESIAN_POINT('Ctrl Pts',(54.8485272785639,19.0109914848589,10.8094010191624));
#24967=CARTESIAN_POINT('Ctrl Pts',(54.8636611837316,19.0099033760352,10.8103623356527));
#24968=CARTESIAN_POINT('Ctrl Pts',(54.8703754554391,19.0094547678672,10.8107897418362));
#24969=CARTESIAN_POINT('Ctrl Pts',(54.8861096975345,19.008483443738,10.8117935198066));
#24970=CARTESIAN_POINT('Ctrl Pts',(54.8951311463981,19.0079880236381,10.8123707375738));
#24971=CARTESIAN_POINT('Ctrl Pts',(54.9212099366469,19.0067335315421,10.8140443640473));
#24972=CARTESIAN_POINT('Ctrl Pts',(54.9382737175133,19.0061321697954,10.8151456688436));
#24973=CARTESIAN_POINT('Ctrl Pts',(55.0920123057643,19.0026894959832,10.825126572705));
#24974=CARTESIAN_POINT('Ctrl Pts',(55.2286080024636,19.0136866690473,10.8344493562165));
#24975=CARTESIAN_POINT('Ctrl Pts',(55.5007456387436,19.0640479904935,10.8537019886178));
#24976=CARTESIAN_POINT('Ctrl Pts',(55.6354489756893,19.1039866388751,10.8635831338431));
#24977=CARTESIAN_POINT('Ctrl Pts',(55.7785533594583,19.1633993384021,10.8738321707524));
#24978=CARTESIAN_POINT('Ctrl Pts',(55.7921813340977,19.1692362007036,10.874805246222));
#24979=CARTESIAN_POINT('Ctrl Pts',(55.8108518904856,19.1774803269982,10.876133052349));
#24980=CARTESIAN_POINT('Ctrl Pts',(55.8159509163856,19.1797574747733,10.8764951315042));
#24981=CARTESIAN_POINT('Ctrl Pts',(55.8246659663949,19.1836934640961,10.8771129522546));
#24982=CARTESIAN_POINT('Ctrl Pts',(55.8282866794595,19.1853417495832,10.877369323172));
#24983=CARTESIAN_POINT('Ctrl Pts',(55.8358043837662,19.188791280658,10.8779009532396));
#24984=CARTESIAN_POINT('Ctrl Pts',(55.8397005126308,19.1905942847442,10.8781760929409));
#24985=CARTESIAN_POINT('Ctrl Pts',(55.8491065557515,19.1949840252407,10.8788394746496));
#24986=CARTESIAN_POINT('Ctrl Pts',(55.8546105688266,19.1975834582037,10.8792269415692));
#24987=CARTESIAN_POINT('Ctrl Pts',(55.8738492984546,19.2067774560459,10.8805790792168));
#24988=CARTESIAN_POINT('Ctrl Pts',(55.88752069153,19.2135043398012,10.8815359643569));
#24989=CARTESIAN_POINT('Ctrl Pts',(55.9708022716576,19.2556743111458,10.8873487008874));
#24990=CARTESIAN_POINT('Ctrl Pts',(56.03836577675,19.2950283191704,10.8919953393839));
#24991=CARTESIAN_POINT('Ctrl Pts',(56.1754259180519,19.3860403935082,10.901634897512));
#24992=CARTESIAN_POINT('Ctrl Pts',(56.2442183467279,19.4384581811158,10.9066039699284));
#24993=CARTESIAN_POINT('Ctrl Pts',(56.3937031051243,19.568529355335,10.9181642785256));
#24994=CARTESIAN_POINT('Ctrl Pts',(56.4716848614971,19.648831879445,10.924790366076));
#24995=CARTESIAN_POINT('Ctrl Pts',(56.5523619595254,19.7472268968791,10.9326880476692));
#24996=CARTESIAN_POINT('Ctrl Pts',(56.5620551696402,19.7593341597923,10.9336560555268));
#24997=CARTESIAN_POINT('Ctrl Pts',(56.5775398276772,19.7791443598114,10.9352345587421));
#24998=CARTESIAN_POINT('Ctrl Pts',(56.5834184832331,19.7867785429692,10.9358415911659));
#24999=CARTESIAN_POINT('Ctrl Pts',(56.5937764231715,19.800433169683,10.9369252515318));
#25000=CARTESIAN_POINT('Ctrl Pts',(56.5982775089211,19.806436901786,10.9374010123231));
#25001=CARTESIAN_POINT('Ctrl Pts',(56.6076856961254,19.8191345749633,10.9384058216565));
#25002=CARTESIAN_POINT('Ctrl Pts',(56.6125850965443,19.8258340183158,10.938935156982));
#25003=CARTESIAN_POINT('Ctrl Pts',(56.6254418086082,19.843646547678,10.9403405295749));
#25004=CARTESIAN_POINT('Ctrl Pts',(56.6333268420728,19.8548110237147,10.9412193179625));
#25005=CARTESIAN_POINT('Ctrl Pts',(56.6700953906675,19.9080241458768,10.9453989241804));
#25006=CARTESIAN_POINT('Ctrl Pts',(56.6974714155697,19.9510863281705,10.9487557684769));
#25007=CARTESIAN_POINT('Ctrl Pts',(56.8091290265989,20.1425616553439,10.9635848454274));
#25008=CARTESIAN_POINT('Ctrl Pts',(56.8758127496346,20.3003868733724,10.9756441788885));
#25009=CARTESIAN_POINT('Ctrl Pts',(56.9291081246865,20.4917145876265,10.9893610976861));
#25010=CARTESIAN_POINT('Ctrl Pts',(56.9360557960598,20.5188552390742,10.9912845861484));
#25011=CARTESIAN_POINT('Ctrl Pts',(56.9520588174631,20.5873440709998,10.9960696396937));
#25012=CARTESIAN_POINT('Ctrl Pts',(56.9603748341308,20.6288536002443,10.9989075895413));
#25013=CARTESIAN_POINT('Ctrl Pts',(56.9687234437182,20.6787161823642,11.0022188847232));
#25014=CARTESIAN_POINT('Ctrl Pts',(56.9700322187786,20.6868413311199,11.0027553807396));
#25015=CARTESIAN_POINT('Ctrl Pts',(56.9720918586113,20.7001521822417,11.0036289888374));
#25016=CARTESIAN_POINT('Ctrl Pts',(56.9728726285275,20.7053330596342,11.003967706459));
#25017=CARTESIAN_POINT('Ctrl Pts',(56.9742395924999,20.7146527275148,11.004574584836));
#25018=CARTESIAN_POINT('Ctrl Pts',(56.9748331954837,20.7187903175542,11.0048431527432));
#25019=CARTESIAN_POINT('Ctrl Pts',(56.9761050487182,20.7278581893583,11.0054298469648));
#25020=CARTESIAN_POINT('Ctrl Pts',(56.9767778552583,20.7327891451811,11.0057476655489));
#25021=CARTESIAN_POINT('Ctrl Pts',(56.9786477208445,20.7468869396925,11.006652981277));
#25022=CARTESIAN_POINT('Ctrl Pts',(56.9797995377598,20.7560597970045,11.0072380021392));
#25023=CARTESIAN_POINT('Ctrl Pts',(56.9871926395632,20.81844238832,11.0111912567426));
#25024=CARTESIAN_POINT('Ctrl Pts',(56.9913524696098,20.8718820089326,11.0144528132427));
#25025=CARTESIAN_POINT('Ctrl Pts',(57.0001561044924,21.1072124255164,11.0285193119082));
#25026=CARTESIAN_POINT('Ctrl Pts',(56.9820603494715,21.2890739800174,11.0386942731503));
#25027=CARTESIAN_POINT('Ctrl Pts',(56.9268088989984,21.5190520585236,11.05288844851));
#25028=CARTESIAN_POINT('Ctrl Pts',(56.9118843180983,21.5715812439113,11.0562176579839));
#25029=CARTESIAN_POINT('Ctrl Pts',(56.8903172671782,21.637131278653,11.0605151860148));
#25030=CARTESIAN_POINT('Ctrl Pts',(56.8856606196969,21.65078387111,11.0614182105881));
#25031=CARTESIAN_POINT('Ctrl Pts',(56.8780090932287,21.6724451575695,11.0628641821008));
#25032=CARTESIAN_POINT('Ctrl Pts',(56.8751100279728,21.680487342646,11.0634039551801));
#25033=CARTESIAN_POINT('Ctrl Pts',(56.869583038705,21.6955160229821,11.0644182524494));
#25034=CARTESIAN_POINT('Ctrl Pts',(56.8669674127983,21.7025069066608,11.0648923598461));
#25035=CARTESIAN_POINT('Ctrl Pts',(56.8610277556968,21.718114581362,11.0659560465079));
#25036=CARTESIAN_POINT('Ctrl Pts',(56.8576830101499,21.7267232544089,11.0665463111358));
#25037=CARTESIAN_POINT('Ctrl Pts',(56.8476261626221,21.7520843150178,11.0682959698374));
#25038=CARTESIAN_POINT('Ctrl Pts',(56.8407465073948,21.7687688298116,11.0694609705695));
#25039=CARTESIAN_POINT('Ctrl Pts',(56.7772639891107,21.9169869625614,11.0799384066852));
#25040=CARTESIAN_POINT('Ctrl Pts',(56.7068878785158,22.0421377925879,11.0897388464372));
#25041=CARTESIAN_POINT('Ctrl Pts',(56.547423800954,22.2656108585438,11.1088617377864));
#25042=CARTESIAN_POINT('Ctrl Pts',(56.4607182777498,22.3647706876262,11.1180995522249));
#25043=CARTESIAN_POINT('Ctrl Pts',(56.353748000368,22.465137231911,11.1278080420744));
#25044=CARTESIAN_POINT('Ctrl Pts',(56.3424916816967,22.4754581916811,11.1288108648397));
#25045=CARTESIAN_POINT('Ctrl Pts',(56.3264479063178,22.4898331534217,11.1302125882075));
#25046=CARTESIAN_POINT('Ctrl Pts',(56.3217584911805,22.493995102659,11.1306190305018));
#25047=CARTESIAN_POINT('Ctrl Pts',(56.3138310536264,22.5009643195365,11.1313005276575));
#25048=CARTESIAN_POINT('Ctrl Pts',(56.3106034944305,22.5037833645686,11.1315764455293));
#25049=CARTESIAN_POINT('Ctrl Pts',(56.303996286329,22.509516864062,11.1321380929205));
#25050=CARTESIAN_POINT('Ctrl Pts',(56.3006159044407,22.5124304108679,11.1324237564703));
#25051=CARTESIAN_POINT('Ctrl Pts',(56.2919804104933,22.5198229693003,11.133149311327));
#25052=CARTESIAN_POINT('Ctrl Pts',(56.2867117158611,22.5242861288953,11.1335880528652));
#25053=CARTESIAN_POINT('Ctrl Pts',(56.2652445372956,22.5422805519496,11.1353603070656));
#25054=CARTESIAN_POINT('Ctrl Pts',(56.2488542677394,22.555582251938,11.1366781445922));
#25055=CARTESIAN_POINT('Ctrl Pts',(56.2051633484334,22.5899043289703,11.1401086818659));
#25056=CARTESIAN_POINT('Ctrl Pts',(56.177523094036,22.6104825703722,11.1421966643194));
#25057=CARTESIAN_POINT('Ctrl Pts',(56.0190128724598,22.7222298954607,11.1538016024108));
#25058=CARTESIAN_POINT('Ctrl Pts',(55.8781088547683,22.7981642090705,11.1627836695983));
#25059=CARTESIAN_POINT('Ctrl Pts',(55.6583655650443,22.8845290961288,11.1767608648133));
#25060=CARTESIAN_POINT('Ctrl Pts',(55.5855267523175,22.9084159776087,11.1813810449807));
#25061=CARTESIAN_POINT('Ctrl Pts',(55.4974697671304,22.9317769309693,11.1870433802224));
#25062=CARTESIAN_POINT('Ctrl Pts',(55.4833990876776,22.9353458566353,11.1879503269007));
#25063=CARTESIAN_POINT('Ctrl Pts',(55.4602180578158,22.9409569915671,11.1894486027284));
#25064=CARTESIAN_POINT('Ctrl Pts',(55.4511299429852,22.9430894147258,11.1900370313199));
#25065=CARTESIAN_POINT('Ctrl Pts',(55.4347409688124,22.9468137263359,11.1911001638077));
#25066=CARTESIAN_POINT('Ctrl Pts',(55.4274454558664,22.9484285398212,11.1915741232999));
#25067=CARTESIAN_POINT('Ctrl Pts',(55.4118517250784,22.95178831408,11.1925887719289));
#25068=CARTESIAN_POINT('Ctrl Pts',(55.4035511311414,22.9535214222837,11.1931298297066));
#25069=CARTESIAN_POINT('Ctrl Pts',(55.3810414865539,22.9580716992059,11.1945997901621));
#25070=CARTESIAN_POINT('Ctrl Pts',(55.3668126078206,22.9607870578116,11.1955319107423));
#25071=CARTESIAN_POINT('Ctrl Pts',(55.2920186946362,22.9742177046213,11.2004478621077));
#25072=CARTESIAN_POINT('Ctrl Pts',(55.2310173881768,22.9822815330329,11.2045146079987));
#25073=CARTESIAN_POINT('Ctrl Pts',(55.1679803510715,22.9876652899753,11.208777821554));
#25074=CARTESIAN_POINT('Ctrl Pts',(55.1662144135544,22.9878137416641,11.2088972999258));
#25075=CARTESIAN_POINT('Ctrl Pts',(55.1644483504356,22.9879598342368,11.2090168340879));
#25076=CARTESIAN_POINT('Origin',(55.,21.,6.22095488139522));
#25077=CARTESIAN_POINT('',(55.1644487484638,22.9879598013111,12.1688212129648));
#25078=CARTESIAN_POINT('',(55.1644483513162,22.987959834164,12.0120574026292));
#25079=CARTESIAN_POINT('',(55.1644483516311,22.987959834138,6.22095488139522));
#25080=CARTESIAN_POINT('Ctrl Pts',(55.1644487484638,22.9879598013111,12.1688212129648));
#25081=CARTESIAN_POINT('Ctrl Pts',(55.2631352750185,22.9797962178365,12.1619316809086));
#25082=CARTESIAN_POINT('Ctrl Pts',(55.3611348208292,22.9642908938561,12.1549763628138));
#25083=CARTESIAN_POINT('Ctrl Pts',(55.5057090792001,22.9302138419902,12.1448260486904));
#25084=CARTESIAN_POINT('Ctrl Pts',(55.553351071021,22.9170995415923,12.1415015513099));
#25085=CARTESIAN_POINT('Ctrl Pts',(55.6091024829877,22.8995009454316,12.1376729441441));
#25086=CARTESIAN_POINT('Ctrl Pts',(55.6177253683065,22.8967142782554,12.1370825731292));
#25087=CARTESIAN_POINT('Ctrl Pts',(55.6310177236848,22.8923183087989,12.1361755929473));
#25088=CARTESIAN_POINT('Ctrl Pts',(55.6357005759918,22.890750308313,12.1358566619738));
#25089=CARTESIAN_POINT('Ctrl Pts',(55.6443402171008,22.8878216953807,12.1352694131176));
#25090=CARTESIAN_POINT('Ctrl Pts',(55.6482985248752,22.8864660325937,12.1350008209137));
#25091=CARTESIAN_POINT('Ctrl Pts',(55.6572523894426,22.8833679537104,12.1343942734837));
#25092=CARTESIAN_POINT('Ctrl Pts',(55.6622452898147,22.8816181148588,12.1340567605018));
#25093=CARTESIAN_POINT('Ctrl Pts',(55.6770460037066,22.8763647664406,12.1330582074837));
#25094=CARTESIAN_POINT('Ctrl Pts',(55.6868335866626,22.8728042244651,12.1324004275954));
#25095=CARTESIAN_POINT('Ctrl Pts',(55.7928628133062,22.8332897124292,12.1252978816355));
#25096=CARTESIAN_POINT('Ctrl Pts',(55.8862314384353,22.7900230343139,12.1192479228581));
#25097=CARTESIAN_POINT('Ctrl Pts',(56.0857559881973,22.678105529276,12.1059244111246));
#25098=CARTESIAN_POINT('Ctrl Pts',(56.1895574207462,22.6061929755261,12.0987010950092));
#25099=CARTESIAN_POINT('Ctrl Pts',(56.3313802924731,22.4866055976501,12.0875975717351));
#25100=CARTESIAN_POINT('Ctrl Pts',(56.3751359904194,22.4462260064698,12.0839740466369));
#25101=CARTESIAN_POINT('Ctrl Pts',(56.4271163297072,22.3937619531715,12.0793730888262));
#25102=CARTESIAN_POINT('Ctrl Pts',(56.4371036760274,22.3834617479255,12.0784746479543));
#25103=CARTESIAN_POINT('Ctrl Pts',(56.4527958218823,22.3669247523332,12.0770393254238));
#25104=CARTESIAN_POINT('Ctrl Pts',(56.4585737132153,22.3607577661646,12.0765056051589));
#25105=CARTESIAN_POINT('Ctrl Pts',(56.469390617376,22.349064381777,12.0754963839202));
#25106=CARTESIAN_POINT('Ctrl Pts',(56.4744380910323,22.3435459820297,12.0750212555272));
#25107=CARTESIAN_POINT('Ctrl Pts',(56.4857497723439,22.3310384156323,12.0739468639525));
#25108=CARTESIAN_POINT('Ctrl Pts',(56.4919958899653,22.3240331979445,12.0733468550987));
#25109=CARTESIAN_POINT('Ctrl Pts',(56.5078824515922,22.3059607545082,12.0718031844183));
#25110=CARTESIAN_POINT('Ctrl Pts',(56.5174504700025,22.2948308893866,12.0708565590061));
#25111=CARTESIAN_POINT('Ctrl Pts',(56.5788809417828,22.2217566477893,12.0646662578256));
#25112=CARTESIAN_POINT('Ctrl Pts',(56.6270557590762,22.1568236325913,12.0592757245517));
#25113=CARTESIAN_POINT('Ctrl Pts',(56.7560623550808,21.9588811601491,12.0431619940139));
#25114=CARTESIAN_POINT('Ctrl Pts',(56.8254348750708,21.8191394523889,12.0321326866493));
#25115=CARTESIAN_POINT('Ctrl Pts',(56.8950347166383,21.6248679264221,12.018017251915));
#25116=CARTESIAN_POINT('Ctrl Pts',(56.9103582040815,21.57632371177,12.014589430937));
#25117=CARTESIAN_POINT('Ctrl Pts',(56.9262227503621,21.5184369164717,12.0106582468343));
#25118=CARTESIAN_POINT('Ctrl Pts',(56.9285755338481,21.5096148921415,12.0100633606266));
#25119=CARTESIAN_POINT('Ctrl Pts',(56.9321111481933,21.4959824649405,12.0091509437773));
#25120=CARTESIAN_POINT('Ctrl Pts',(56.9333367362451,21.4911834281402,12.0088310481817));
#25121=CARTESIAN_POINT('Ctrl Pts',(56.935564374119,21.4823231416446,12.0082429020439));
#25122=CARTESIAN_POINT('Ctrl Pts',(56.9365715195632,21.4782633265508,12.0079743705631));
#25123=CARTESIAN_POINT('Ctrl Pts',(56.9388191724453,21.4690794941811,12.0073690629039));
#25124=CARTESIAN_POINT('Ctrl Pts',(56.940052139632,21.4639537178982,12.0070327210953));
#25125=CARTESIAN_POINT('Ctrl Pts',(56.9431817507256,21.4507124391296,12.0061675805054));
#25126=CARTESIAN_POINT('Ctrl Pts',(56.9450479048463,21.44258973409,12.0056404708632));
#25127=CARTESIAN_POINT('Ctrl Pts',(56.9564835935697,21.3913446108047,12.0023362793467));
#25128=CARTESIAN_POINT('Ctrl Pts',(56.9646702776822,21.3479224306536,11.9996311563216));
#25129=CARTESIAN_POINT('Ctrl Pts',(57.0009287208087,21.1129916093255,11.9853285054397));
#25130=CARTESIAN_POINT('Ctrl Pts',(57.002459280579,20.9184382887348,11.9745642776035));
#25131=CARTESIAN_POINT('Ctrl Pts',(56.9685782559503,20.6734833533486,11.9597044830606));
#25132=CARTESIAN_POINT('Ctrl Pts',(56.9590718734489,20.6205924524478,11.9564240929527));
#25133=CARTESIAN_POINT('Ctrl Pts',(56.9444341814658,20.5545828035843,11.9522093335986));
#25134=CARTESIAN_POINT('Ctrl Pts',(56.9412833107636,20.5410448205084,11.9513385026714));
#25135=CARTESIAN_POINT('Ctrl Pts',(56.9360129961446,20.5194263800957,11.9499371244364));
#25136=CARTESIAN_POINT('Ctrl Pts',(56.9339837933855,20.5113242292975,11.949409481457));
#25137=CARTESIAN_POINT('Ctrl Pts',(56.930037186238,20.4959759906576,11.948405214584));
#25138=CARTESIAN_POINT('Ctrl Pts',(56.9281297031506,20.4887274820909,11.9479289185434));
#25139=CARTESIAN_POINT('Ctrl Pts',(56.9236996635051,20.4722705965353,11.9468428849412));
#25140=CARTESIAN_POINT('Ctrl Pts',(56.9211517703889,20.4630692888816,11.9462323356768));
#25141=CARTESIAN_POINT('Ctrl Pts',(56.9143732180348,20.4392557114714,11.9446433785994));
#25142=CARTESIAN_POINT('Ctrl Pts',(56.9100413479069,20.4246731337317,11.9436617064761));
#25143=CARTESIAN_POINT('Ctrl Pts',(56.8768638605763,20.3174928965863,11.9363810722413));
#25144=CARTESIAN_POINT('Ctrl Pts',(56.8414702849752,20.2270730508161,11.9298672252395));
#25145=CARTESIAN_POINT('Ctrl Pts',(56.7390874875415,20.012925949443,11.913553398416));
#25146=CARTESIAN_POINT('Ctrl Pts',(56.6653267350473,19.8930108129447,11.9036156675666));
#25147=CARTESIAN_POINT('Ctrl Pts',(56.5497295423518,19.7431162454355,11.8906845348243));
#25148=CARTESIAN_POINT('Ctrl Pts',(56.5184527152197,19.7055037017738,11.8873943900699));
#25149=CARTESIAN_POINT('Ctrl Pts',(56.4797918206915,19.6623433100878,11.8835999635599));
#25150=CARTESIAN_POINT('Ctrl Pts',(56.4737155448948,19.6556519227367,11.8830111386633));
#25151=CARTESIAN_POINT('Ctrl Pts',(56.4642526644052,19.6453723631457,11.8821060208406));
#25152=CARTESIAN_POINT('Ctrl Pts',(56.4608979710776,19.6417551696668,11.8817874208047));
#25153=CARTESIAN_POINT('Ctrl Pts',(56.4546730262615,19.6350928752721,11.8812004779104));
#25154=CARTESIAN_POINT('Ctrl Pts',(56.4518066300993,19.6320443787096,11.8809318630061));
#25155=CARTESIAN_POINT('Ctrl Pts',(56.4452898942278,19.625157193333,11.8803248818203));
#25156=CARTESIAN_POINT('Ctrl Pts',(56.4416338496469,19.6213240168501,11.8799869605258));
#25157=CARTESIAN_POINT('Ctrl Pts',(56.4307232213335,19.6099756364407,11.8789860687615));
#25158=CARTESIAN_POINT('Ctrl Pts',(56.4234246971968,19.6025026619261,11.8783263811014));
#25159=CARTESIAN_POINT('Ctrl Pts',(56.3520806048194,19.5305921082013,11.8719683946961));
#25160=CARTESIAN_POINT('Ctrl Pts',(56.2837531162298,19.470534778132,11.8665777618287));
#25161=CARTESIAN_POINT('Ctrl Pts',(56.1759874395737,19.388141999106,11.8586480939982));
#25162=CARTESIAN_POINT('Ctrl Pts',(56.1395085309533,19.3621498568731,11.8560524078389));
#25163=CARTESIAN_POINT('Ctrl Pts',(56.0180815137242,19.2816520487818,11.8476002153413));
#25164=CARTESIAN_POINT('Ctrl Pts',(55.929872459968,19.2323618024046,11.8417390465924));
#25165=CARTESIAN_POINT('Ctrl Pts',(55.8067839593314,19.1753534620842,11.8335813899607));
#25166=CARTESIAN_POINT('Ctrl Pts',(55.7748739955947,19.1615752852851,11.8314693778516));
#25167=CARTESIAN_POINT('Ctrl Pts',(55.7194552126707,19.1393455994197,11.8277944042415));
#25168=CARTESIAN_POINT('Ctrl Pts',(55.6961171861329,19.1304890002642,11.8262447550373));
#25169=CARTESIAN_POINT('Ctrl Pts',(55.6627193013234,19.1185268306655,11.8240214948683));
#25170=CARTESIAN_POINT('Ctrl Pts',(55.6527909697619,19.1150591249916,11.8233598839936));
#25171=CARTESIAN_POINT('Ctrl Pts',(55.6356022147318,19.1092076326856,11.8222130515602));
#25172=CARTESIAN_POINT('Ctrl Pts',(55.6283545910332,19.1067867375952,11.8217290650948));
#25173=CARTESIAN_POINT('Ctrl Pts',(55.6144331262706,19.1022253516083,11.8207985178666));
#25174=CARTESIAN_POINT('Ctrl Pts',(55.6077615511641,19.1000782706646,11.8203521822108));
#25175=CARTESIAN_POINT('Ctrl Pts',(55.592049001603,19.0951128054936,11.8193000155293));
#25176=CARTESIAN_POINT('Ctrl Pts',(55.5829990594267,19.092323576788,11.8186932399595));
#25177=CARTESIAN_POINT('Ctrl Pts',(55.5515695416394,19.0828814052565,11.8165831409066));
#25178=CARTESIAN_POINT('Ctrl Pts',(55.5290939720605,19.0765572123083,11.8150692063539));
#25179=CARTESIAN_POINT('Ctrl Pts',(55.3550051518577,19.0308540692414,11.8032999802397));
#25180=CARTESIAN_POINT('Ctrl Pts',(55.1993666428328,19.0090708120618,11.7924648842068));
#25181=CARTESIAN_POINT('Ctrl Pts',(54.9266520592972,19.0032154415543,11.7734384541342));
#25182=CARTESIAN_POINT('Ctrl Pts',(54.8104759586204,19.0108757590796,11.7653414698039));
#25183=CARTESIAN_POINT('Ctrl Pts',(54.6850157650914,19.0302468268437,11.757002340096));
#25184=CARTESIAN_POINT('Ctrl Pts',(54.6744274600482,19.0319692164764,11.7563018570637));
#25185=CARTESIAN_POINT('Ctrl Pts',(54.6586454189903,19.0346673240608,11.7552632279788));
#25186=CARTESIAN_POINT('Ctrl Pts',(54.6534410362598,19.0355783641739,11.7549216106729));
#25187=CARTESIAN_POINT('Ctrl Pts',(54.6441222428118,19.0372478284839,11.7543115881144));
#25188=CARTESIAN_POINT('Ctrl Pts',(54.6400065568597,19.0379985252868,11.754042757162));
#25189=CARTESIAN_POINT('Ctrl Pts',(54.6310323252322,19.0396646053923,11.7534578629229));
#25190=CARTESIAN_POINT('Ctrl Pts',(54.6261748188598,19.0405851027411,11.7531420923399));
#25191=CARTESIAN_POINT('Ctrl Pts',(54.6126437690227,19.0432013856596,11.7522646343666));
#25192=CARTESIAN_POINT('Ctrl Pts',(54.6039778708655,19.044936792102,11.751705138172));
#25193=CARTESIAN_POINT('Ctrl Pts',(54.55668379339,19.0547351275433,11.7486637735827));
#25194=CARTESIAN_POINT('Ctrl Pts',(54.5182869711783,19.0638859210863,11.7462386609306));
#25195=CARTESIAN_POINT('Ctrl Pts',(54.2887643883916,19.1258381876529,11.7318713474258));
#25196=CARTESIAN_POINT('Ctrl Pts',(54.1061075545412,19.2057563340643,11.7208729410609));
#25197=CARTESIAN_POINT('Ctrl Pts',(53.8923655121536,19.3401481864385,11.7057058333443));
#25198=CARTESIAN_POINT('Ctrl Pts',(53.8477022933176,19.3708372086715,11.7023986329782));
#25199=CARTESIAN_POINT('Ctrl Pts',(53.7931904249005,19.4116573287015,11.6981536438975));
#25200=CARTESIAN_POINT('Ctrl Pts',(53.7821229462194,19.4201274550495,11.6972805350793));
#25201=CARTESIAN_POINT('Ctrl Pts',(53.7645596536865,19.4338631567189,11.6958763563653));
#25202=CARTESIAN_POINT('Ctrl Pts',(53.7580064869741,19.4390549108523,11.6953482116631));
#25203=CARTESIAN_POINT('Ctrl Pts',(53.7456418386923,19.4489779750794,11.69434354872));
#25204=CARTESIAN_POINT('Ctrl Pts',(53.739823989157,19.4537011486096,11.6938673620792));
#25205=CARTESIAN_POINT('Ctrl Pts',(53.7266655285193,19.4645073193536,11.6927823525119));
#25206=CARTESIAN_POINT('Ctrl Pts',(53.719341678164,19.4706103485131,11.6921727236547));
#25207=CARTESIAN_POINT('Ctrl Pts',(53.7004814143636,19.4865572378919,11.6905877362977));
#25208=CARTESIAN_POINT('Ctrl Pts',(53.6890131821451,19.4964804321471,11.6896091403857));
#25209=CARTESIAN_POINT('Ctrl Pts',(53.6062910070647,19.5697240323046,11.6824399163084));
#25210=CARTESIAN_POINT('Ctrl Pts',(53.5395545496119,19.6379396451916,11.6760420244124));
#25211=CARTESIAN_POINT('Ctrl Pts',(53.386222364542,19.8189448489081,11.6597497655824));
#25212=CARTESIAN_POINT('Ctrl Pts',(53.3063122174673,19.9367085869422,11.6497020523071));
#25213=CARTESIAN_POINT('Ctrl Pts',(53.2164807616161,20.1052940678408,11.6366505789264));
#25214=CARTESIAN_POINT('Ctrl Pts',(53.1949916236563,20.1494794311572,11.6333454799807));
#25215=CARTESIAN_POINT('Ctrl Pts',(53.1714996054309,20.2026946978422,11.6295361693965));
#25216=CARTESIAN_POINT('Ctrl Pts',(53.1679016374288,20.2109974428874,11.6289466686373));
#25217=CARTESIAN_POINT('Ctrl Pts',(53.1624286361944,20.223866374661,11.6280407366684));
#25218=CARTESIAN_POINT('Ctrl Pts',(53.16051389935,20.2284153913823,11.6277219919289));
#25219=CARTESIAN_POINT('Ctrl Pts',(53.1570070772543,20.236834121825,11.6271349153711));
#25220=CARTESIAN_POINT('Ctrl Pts',(53.1554102933403,20.2407017150396,11.6268663105117));
#25221=CARTESIAN_POINT('Ctrl Pts',(53.1518206883696,20.2494743020717,11.626259519524));
#25222=CARTESIAN_POINT('Ctrl Pts',(53.1498352205134,20.2543822148745,11.6259217771807));
#25223=CARTESIAN_POINT('Ctrl Pts',(53.1439956610321,20.2689840764529,11.6249219107452));
#25224=CARTESIAN_POINT('Ctrl Pts',(53.140197976249,20.2787005959249,11.6242630595177));
#25225=CARTESIAN_POINT('Ctrl Pts',(53.1051685963822,20.3704408350954,11.6180992784536));
#25226=CARTESIAN_POINT('Ctrl Pts',(53.0793019958035,20.4544232310117,11.6128812400732));
#25227=CARTESIAN_POINT('Ctrl Pts',(53.0233811802809,20.6902999501212,11.5986941594621));
#25228=CARTESIAN_POINT('Ctrl Pts',(53.0053276029801,20.8443816608655,11.5899035048977));
#25229=CARTESIAN_POINT('Ctrl Pts',(53.0052267963372,21.0458823035609,11.5777423438057));
#25230=CARTESIAN_POINT('Ctrl Pts',(53.0068559918777,21.0927456276598,11.5748714783639));
#25231=CARTESIAN_POINT('Ctrl Pts',(53.0111010944751,21.1532965630707,11.571087290186));
#25232=CARTESIAN_POINT('Ctrl Pts',(53.0122112894115,21.1670769866418,11.5702210738776));
#25233=CARTESIAN_POINT('Ctrl Pts',(53.0142203551788,21.1891461151503,11.5688253687914));
#25234=CARTESIAN_POINT('Ctrl Pts',(53.0150281160256,21.1974428197599,11.5682987422623));
#25235=CARTESIAN_POINT('Ctrl Pts',(53.0166612389442,21.2131927550693,11.5672952700931));
#25236=CARTESIAN_POINT('Ctrl Pts',(53.0174766734884,21.2206468881253,11.5668187446811));
#25237=CARTESIAN_POINT('Ctrl Pts',(53.0194291890744,21.2376100560971,11.5657305989657));
#25238=CARTESIAN_POINT('Ctrl Pts',(53.0205927522274,21.247115798819,11.565118155073));
#25239=CARTESIAN_POINT('Ctrl Pts',(53.0243657875763,21.2762013682682,11.5632358170011));
#25240=CARTESIAN_POINT('Ctrl Pts',(53.0271976154137,21.295750641479,11.56195896434));
#25241=CARTESIAN_POINT('Ctrl Pts',(53.0502114716813,21.4395392708815,11.5524782485069));
#25242=CARTESIAN_POINT('Ctrl Pts',(53.0818186012838,21.5616403593145,11.5439076383811));
#25243=CARTESIAN_POINT('Ctrl Pts',(53.1750397041502,21.8187499082045,11.5249080522552));
#25244=CARTESIAN_POINT('Ctrl Pts',(53.2406323403614,21.9515579530286,11.5144672985571));
#25245=CARTESIAN_POINT('Ctrl Pts',(53.3278687800013,22.0877510381737,11.5037808844716));
#25246=CARTESIAN_POINT('Ctrl Pts',(53.3355754483629,22.0995071971577,11.5028589530587));
#25247=CARTESIAN_POINT('Ctrl Pts',(53.3464559242026,22.1157282503815,11.50158867378));
#25248=CARTESIAN_POINT('Ctrl Pts',(53.3495246000604,22.1202626902689,11.5012337768756));
#25249=CARTESIAN_POINT('Ctrl Pts',(53.3548392649776,22.1280466839637,11.5006249677821));
#25250=CARTESIAN_POINT('Ctrl Pts',(53.3570762882495,22.1313022775959,11.5003704657262));
#25251=CARTESIAN_POINT('Ctrl Pts',(53.3617795141683,22.1381036228022,11.4998390829897));
#25252=CARTESIAN_POINT('Ctrl Pts',(53.3642475806087,22.1416480365481,11.4995623393017));
#25253=CARTESIAN_POINT('Ctrl Pts',(53.3702968201381,22.150275519039,11.4988890798134));
#25254=CARTESIAN_POINT('Ctrl Pts',(53.3738903247223,22.1553499688855,11.4984933962833));
#25255=CARTESIAN_POINT('Ctrl Pts',(53.3868549564786,22.1734772345215,11.4970806984183));
#25256=CARTESIAN_POINT('Ctrl Pts',(53.3963602867035,22.186433925702,11.496072426503));
#25257=CARTESIAN_POINT('Ctrl Pts',(53.420324791419,22.2182855952533,11.493593579931));
#25258=CARTESIAN_POINT('Ctrl Pts',(53.4349677003432,22.2370398378151,11.4921338590358));
#25259=CARTESIAN_POINT('Ctrl Pts',(53.4977850239629,22.3145931696544,11.4860757324437));
#25260=CARTESIAN_POINT('Ctrl Pts',(53.5489675929747,22.3708799375397,11.4816234613602));
#25261=CARTESIAN_POINT('Ctrl Pts',(53.7220832589124,22.540670525554,11.46751839284));
#25262=CARTESIAN_POINT('Ctrl Pts',(53.8550317554083,22.6418826472947,11.4579769379792));
#25263=CARTESIAN_POINT('Ctrl Pts',(54.0189056430745,22.7369545132371,11.4462934852197));
#25264=CARTESIAN_POINT('Ctrl Pts',(54.0390081523801,22.748156663136,11.444862853427));
#25265=CARTESIAN_POINT('Ctrl Pts',(54.0673804807265,22.7633299115681,11.4428451775209));
#25266=CARTESIAN_POINT('Ctrl Pts',(54.0754912062399,22.7675958334768,11.4422685614604));
#25267=CARTESIAN_POINT('Ctrl Pts',(54.0904066352814,22.7753100191394,11.441208349367));
#25268=CARTESIAN_POINT('Ctrl Pts',(54.0972023069245,22.7787754428094,11.4407253669514));
#25269=CARTESIAN_POINT('Ctrl Pts',(54.1110209980808,22.7857226382097,11.4397432935432));
#25270=CARTESIAN_POINT('Ctrl Pts',(54.1180449924229,22.7892021596768,11.4392441346096));
#25271=CARTESIAN_POINT('Ctrl Pts',(54.135450481615,22.7976970324064,11.4380071849368));
#25272=CARTESIAN_POINT('Ctrl Pts',(54.1458551944191,22.8026638987656,11.437267728263));
#25273=CARTESIAN_POINT('Ctrl Pts',(54.1849348252037,22.820904930627,11.4344898729507));
#25274=CARTESIAN_POINT('Ctrl Pts',(54.2138795093055,22.8335867555719,11.4324313528172));
#25275=CARTESIAN_POINT('Ctrl Pts',(54.2870555953743,22.8635969719461,11.4272214950505));
#25276=CARTESIAN_POINT('Ctrl Pts',(54.3316258143947,22.8800422215631,11.4240429056687));
#25277=CARTESIAN_POINT('Ctrl Pts',(54.5558123335365,22.9537814554232,11.4080368618407));
#25278=CARTESIAN_POINT('Ctrl Pts',(54.7423048084404,22.9869941550036,11.3945496455318));
#25279=CARTESIAN_POINT('Ctrl Pts',(54.9611802109403,22.9946058451654,11.3797971648179));
#25280=CARTESIAN_POINT('Ctrl Pts',(54.9917110429182,22.9949664133274,11.3777663921631));
#25281=CARTESIAN_POINT('Ctrl Pts',(55.0304528559179,22.9945344431834,11.3752335181439));
#25282=CARTESIAN_POINT('Ctrl Pts',(55.0386652157354,22.9943921450433,11.3746991235355));
#25283=CARTESIAN_POINT('Ctrl Pts',(55.0516287285123,22.9940874182917,11.3738597793968));
#25284=CARTESIAN_POINT('Ctrl Pts',(55.0563804709015,22.9939587260137,11.3735530148023));
#25285=CARTESIAN_POINT('Ctrl Pts',(55.0649191732513,22.9936969231477,11.3730034334469));
#25286=CARTESIAN_POINT('Ctrl Pts',(55.0687061802393,22.9935700091809,11.3727602815624));
#25287=CARTESIAN_POINT('Ctrl Pts',(55.0778224251352,22.9932384890046,11.3721763571656));
#25288=CARTESIAN_POINT('Ctrl Pts',(55.0831512263136,22.9930233011828,11.3718361784439));
#25289=CARTESIAN_POINT('Ctrl Pts',(55.0994459130319,22.9922998216434,11.3707992986495));
#25290=CARTESIAN_POINT('Ctrl Pts',(55.1104087390921,22.9917223682492,11.3701063239169));
#25291=CARTESIAN_POINT('Ctrl Pts',(55.1357406157966,22.9901782406948,11.3685146017251));
#25292=CARTESIAN_POINT('Ctrl Pts',(55.1501020651774,22.9891465902058,11.3676193066293));
#25293=CARTESIAN_POINT('Ctrl Pts',(55.1644483680005,22.9879598327838,11.3667309363937));
#25294=CARTESIAN_POINT('',(53.0052509133734,21.0017010510026,11.4203138250391));
#25295=CARTESIAN_POINT('Ctrl Pts',(55.1644483504356,22.9879598342368,11.2090168340879));
#25296=CARTESIAN_POINT('Ctrl Pts',(55.0092635275445,23.0007970594652,11.2195203588896));
#25297=CARTESIAN_POINT('Ctrl Pts',(54.8531129331955,22.9954176987343,11.2305157839018));
#25298=CARTESIAN_POINT('Ctrl Pts',(54.6305636587255,22.9614701310944,11.2460703318392));
#25299=CARTESIAN_POINT('Ctrl Pts',(54.5625115666673,22.9474224762946,11.2508003530778));
#25300=CARTESIAN_POINT('Ctrl Pts',(54.4854643150143,22.9272738401728,11.2560279776748));
#25301=CARTESIAN_POINT('Ctrl Pts',(54.4756241844518,22.9246198172001,11.2566931689445));
#25302=CARTESIAN_POINT('Ctrl Pts',(54.4607540810592,22.9204866257303,11.257694208272));
#25303=CARTESIAN_POINT('Ctrl Pts',(54.4557090645972,22.9190629014876,11.2580331020069));
#25304=CARTESIAN_POINT('Ctrl Pts',(54.4466511940752,22.9164681407743,11.2586401657986));
#25305=CARTESIAN_POINT('Ctrl Pts',(54.4426363755956,22.9153043692301,11.2589087441613));
#25306=CARTESIAN_POINT('Ctrl Pts',(54.4338518252682,22.9127280389225,11.2594953090228));
#25307=CARTESIAN_POINT('Ctrl Pts',(54.4290837170337,22.9113102589005,11.2598129887718));
#25308=CARTESIAN_POINT('Ctrl Pts',(54.415479625998,22.9072096803969,11.2607175110254));
#25309=CARTESIAN_POINT('Ctrl Pts',(54.4066567611096,22.9044833003496,11.2613018840446));
#25310=CARTESIAN_POINT('Ctrl Pts',(54.3474294313881,22.8857297414347,11.2652115678339));
#25311=CARTESIAN_POINT('Ctrl Pts',(54.2976558442485,22.8677630411592,11.2684329772281));
#25312=CARTESIAN_POINT('Ctrl Pts',(54.0869222641937,22.7820766527148,11.2820281991051));
#25313=CARTESIAN_POINT('Ctrl Pts',(53.9345226912043,22.6953683437328,11.2918141232181));
#25314=CARTESIAN_POINT('Ctrl Pts',(53.7462401284685,22.5527105818578,11.3059240181889));
#25315=CARTESIAN_POINT('Ctrl Pts',(53.698884397953,22.5132485020501,11.3096683678554));
#25316=CARTESIAN_POINT('Ctrl Pts',(53.6424043636519,22.4615694097543,11.3144326163687));
#25317=CARTESIAN_POINT('Ctrl Pts',(53.631489121791,22.4513541981226,11.3153679983759));
#25318=CARTESIAN_POINT('Ctrl Pts',(53.6144273536599,22.4350230512437,11.3168540796457));
#25319=CARTESIAN_POINT('Ctrl Pts',(53.6082039736144,22.4289879401122,11.317401292947));
#25320=CARTESIAN_POINT('Ctrl Pts',(53.596702403059,22.4176879038426,11.3184223765349));
#25321=CARTESIAN_POINT('Ctrl Pts',(53.5914139873357,22.4124335668404,11.3188957780785));
#25322=CARTESIAN_POINT('Ctrl Pts',(53.5811203974231,22.4020910014361,11.319824986378));
#25323=CARTESIAN_POINT('Ctrl Pts',(53.5761128289944,22.3970053059946,11.3202806768769));
#25324=CARTESIAN_POINT('Ctrl Pts',(53.5615285935287,22.3820336534091,11.3216186867654));
#25325=CARTESIAN_POINT('Ctrl Pts',(53.5520269790321,22.3720754794033,11.3225042432158));
#25326=CARTESIAN_POINT('Ctrl Pts',(53.5039366997201,22.3206185538755,11.3270587020972));
#25327=CARTESIAN_POINT('Ctrl Pts',(53.4670293770656,22.2775910017095,11.3307976974811));
#25328=CARTESIAN_POINT('Ctrl Pts',(53.3753119724221,22.1609600345688,11.3407643108629));
#25329=CARTESIAN_POINT('Ctrl Pts',(53.3236629926683,22.0850486193954,11.3470932208943));
#25330=CARTESIAN_POINT('Ctrl Pts',(53.2104036821105,21.8910876756606,11.3627353059699));
#25331=CARTESIAN_POINT('Ctrl Pts',(53.1550175119223,21.7698944862666,11.3720849517102));
#25332=CARTESIAN_POINT('Ctrl Pts',(53.1071866309821,21.629695378185,11.3818884861442));
#25333=CARTESIAN_POINT('Ctrl Pts',(53.1024419563184,21.6152497246356,11.3828868498333));
#25334=CARTESIAN_POINT('Ctrl Pts',(53.0959778487469,21.594782633348,11.3842834524343));
#25335=CARTESIAN_POINT('Ctrl Pts',(53.0941210194638,21.5888056109612,11.3846891610648));
#25336=CARTESIAN_POINT('Ctrl Pts',(53.0910409042435,21.5787236629315,11.385369784152));
#25337=CARTESIAN_POINT('Ctrl Pts',(53.0898026629017,21.5746233913022,11.385645556742));
#25338=CARTESIAN_POINT('Ctrl Pts',(53.0873003698219,21.5662399050228,11.3862072539579));
#25339=CARTESIAN_POINT('Ctrl Pts',(53.0860374807261,21.5619563871821,11.3864931106972));
#25340=CARTESIAN_POINT('Ctrl Pts',(53.0828546444564,21.5510255171634,11.3872197525877));
#25341=CARTESIAN_POINT('Ctrl Pts',(53.0809548588042,21.5443722846421,11.387659381144));
#25342=CARTESIAN_POINT('Ctrl Pts',(53.0733688615912,21.5172720962352,11.3894398270361));
#25343=CARTESIAN_POINT('Ctrl Pts',(53.0679742709805,21.4967440319597,11.3907647861303));
#25344=CARTESIAN_POINT('Ctrl Pts',(53.0247486871252,21.3208856877327,11.4019445983941));
#25345=CARTESIAN_POINT('Ctrl Pts',(53.0053872115722,21.1616005945455,11.410976491796));
#25346=CARTESIAN_POINT('Ctrl Pts',(53.0052507266776,21.0017026683888,11.4203134044792));
#25347=CARTESIAN_POINT('Ctrl Pts',(53.0052507252816,21.0017010321814,11.4203135000222));
#25348=CARTESIAN_POINT('Ctrl Pts',(53.0051572374266,20.892070636593,11.4267151440213));
#25349=CARTESIAN_POINT('Ctrl Pts',(53.0141013025501,20.782630020886,11.4332260894532));
#25350=CARTESIAN_POINT('Ctrl Pts',(53.0339269391734,20.6627682253071,11.4407719853798));
#25351=CARTESIAN_POINT('Ctrl Pts',(53.0359691189056,20.6510712981564,11.4415126386308));
#25352=CARTESIAN_POINT('Ctrl Pts',(53.0396035524338,20.631298114834,11.44277226009));
#25353=CARTESIAN_POINT('Ctrl Pts',(53.0411416071494,20.623212121656,11.4432895198122));
#25354=CARTESIAN_POINT('Ctrl Pts',(53.0440806736763,20.6082651601016,11.4442497712183));
#25355=CARTESIAN_POINT('Ctrl Pts',(53.0454678583589,20.6014015791052,11.4446923184997));
#25356=CARTESIAN_POINT('Ctrl Pts',(53.0484128523122,20.5872152918814,11.4456104047392));
#25357=CARTESIAN_POINT('Ctrl Pts',(53.0499758028653,20.5798937772887,11.4460861012174));
#25358=CARTESIAN_POINT('Ctrl Pts',(53.0536121467205,20.5633172314747,11.4471674519151));
#25359=CARTESIAN_POINT('Ctrl Pts',(53.0557103950992,20.5540678943392,11.4477738927616));
#25360=CARTESIAN_POINT('Ctrl Pts',(53.0612989868218,20.5302222059878,11.4493454596257));
#25361=CARTESIAN_POINT('Ctrl Pts',(53.0648881893086,20.5156498643212,11.450313734171));
#25362=CARTESIAN_POINT('Ctrl Pts',(53.091192792144,20.4138145658406,11.457136938735));
#25363=CARTESIAN_POINT('Ctrl Pts',(53.1196346496169,20.3281515108074,11.4631764553428));
#25364=CARTESIAN_POINT('Ctrl Pts',(53.1825251391162,20.1744208185732,11.4745572760756));
#25365=CARTESIAN_POINT('Ctrl Pts',(53.2152720838552,20.1058294333342,11.4798479270736));
#25366=CARTESIAN_POINT('Ctrl Pts',(53.2864244833405,19.9763591665243,11.4901526226349));
#25367=CARTESIAN_POINT('Ctrl Pts',(53.3243741494522,19.915352353179,11.4951581753171));
#25368=CARTESIAN_POINT('Ctrl Pts',(53.3934021762447,19.8166848419255,11.5033830221403));
#25369=CARTESIAN_POINT('Ctrl Pts',(53.422722308933,19.7778759107242,11.506654072731));
#25370=CARTESIAN_POINT('Ctrl Pts',(53.4591542392526,19.7331519687879,11.5104316678307));
#25371=CARTESIAN_POINT('Ctrl Pts',(53.4649222964603,19.7261687536437,11.511021733257));
#25372=CARTESIAN_POINT('Ctrl Pts',(53.4739073949583,19.7154404289153,11.5119282878644));
#25373=CARTESIAN_POINT('Ctrl Pts',(53.4770910215909,19.7116676765717,11.5122470962951));
#25374=CARTESIAN_POINT('Ctrl Pts',(53.4829980803338,19.7047200170124,11.512834143463));
#25375=CARTESIAN_POINT('Ctrl Pts',(53.4857174769498,19.7015418760913,11.5131026561841));
#25376=CARTESIAN_POINT('Ctrl Pts',(53.4918983824786,19.694364120022,11.5137090480604));
#25377=CARTESIAN_POINT('Ctrl Pts',(53.4953658095081,19.6903697108674,11.5140464850665));
#25378=CARTESIAN_POINT('Ctrl Pts',(53.5057066714863,19.6785525176881,11.5150448788717));
#25379=CARTESIAN_POINT('Ctrl Pts',(53.5126256456882,19.6707695680026,11.5157025761111));
#25380=CARTESIAN_POINT('Ctrl Pts',(53.5770610906316,19.5994211719596,11.5217371214622));
#25381=CARTESIAN_POINT('Ctrl Pts',(53.638565949665,19.5395626240716,11.5268404176045));
#25382=CARTESIAN_POINT('Ctrl Pts',(53.8391085800137,19.3681059569576,11.5422946471397));
#25383=CARTESIAN_POINT('Ctrl Pts',(53.9893551535685,19.2710285685206,11.5523818863077));
#25384=CARTESIAN_POINT('Ctrl Pts',(54.16915330935,19.1863995117723,11.5645463391755));
#25385=CARTESIAN_POINT('Ctrl Pts',(54.1879490573907,19.177906101846,11.5658177993362));
#25386=CARTESIAN_POINT('Ctrl Pts',(54.2219127987131,19.1631884818063,11.5681171483211));
#25387=CARTESIAN_POINT('Ctrl Pts',(54.2370323758092,19.1568568624621,11.5691413814286));
#25388=CARTESIAN_POINT('Ctrl Pts',(54.2604387865059,19.147392320132,11.5707287269994));
#25389=CARTESIAN_POINT('Ctrl Pts',(54.2686715640999,19.1441269658812,11.571287374166));
#25390=CARTESIAN_POINT('Ctrl Pts',(54.2831974580241,19.1384772460299,11.5722737427874));
#25391=CARTESIAN_POINT('Ctrl Pts',(54.2894814474216,19.1360696814637,11.5727006783515));
#25392=CARTESIAN_POINT('Ctrl Pts',(54.3036764827762,19.1307133979278,11.5736656611751));
#25393=CARTESIAN_POINT('Ctrl Pts',(54.3115942699557,19.1277830284518,11.5742043115461));
#25394=CARTESIAN_POINT('Ctrl Pts',(54.3329887459804,19.1200190074,11.575660977536));
#25395=CARTESIAN_POINT('Ctrl Pts',(54.3464990615563,19.1152801133211,11.5765821124985));
#25396=CARTESIAN_POINT('Ctrl Pts',(54.409170894297,19.0940521415599,11.580861762251));
#25397=CARTESIAN_POINT('Ctrl Pts',(54.4589086552098,19.0793397987693,11.5842778208237));
#25398=CARTESIAN_POINT('Ctrl Pts',(54.532199090119,19.0607334095589,11.5893430901695));
#25399=CARTESIAN_POINT('Ctrl Pts',(54.5553407059858,19.0552967725533,11.590946829943));
#25400=CARTESIAN_POINT('Ctrl Pts',(54.7053313614505,19.0228767757062,11.6013664212854));
#25401=CARTESIAN_POINT('Ctrl Pts',(54.8344518759403,19.0079071029959,11.6104798798371));
#25402=CARTESIAN_POINT('Ctrl Pts',(55.0404094597709,19.004199294438,11.6247792474022));
#25403=CARTESIAN_POINT('Ctrl Pts',(55.1167485002965,19.0072065845438,11.6300204205694));
#25404=CARTESIAN_POINT('Ctrl Pts',(55.2077268579707,19.0160383040455,11.6360659171033));
#25405=CARTESIAN_POINT('Ctrl Pts',(55.2227030327147,19.0176635375024,11.6370544377176));
#25406=CARTESIAN_POINT('Ctrl Pts',(55.2436759833015,19.0201802374449,11.6384281269656));
#25407=CARTESIAN_POINT('Ctrl Pts',(55.2496888517483,19.0209295725825,11.6388207273027));
#25408=CARTESIAN_POINT('Ctrl Pts',(55.2599508322496,19.0222559535175,11.6394885552299));
#25409=CARTESIAN_POINT('Ctrl Pts',(55.2642016426041,19.0228193198432,11.6397645393504));
#25410=CARTESIAN_POINT('Ctrl Pts',(55.2723993964584,19.0239326906237,11.6402954868059));
#25411=CARTESIAN_POINT('Ctrl Pts',(55.2763465275944,19.0244808176728,11.6405505581848));
#25412=CARTESIAN_POINT('Ctrl Pts',(55.2858459433756,19.0258290027477,11.6411631035316));
#25413=CARTESIAN_POINT('Ctrl Pts',(55.2913965855073,19.0266406658925,11.6415199309805));
#25414=CARTESIAN_POINT('Ctrl Pts',(55.3117878759537,19.0297103708436,11.6428270313982));
#25415=CARTESIAN_POINT('Ctrl Pts',(55.3266067684547,19.0321125660015,11.6437695879997));
#25416=CARTESIAN_POINT('Ctrl Pts',(55.4768775293681,19.058216271204,11.6532657208826));
#25417=CARTESIAN_POINT('Ctrl Pts',(55.6095814847158,19.0957001803611,11.6611569658742));
#25418=CARTESIAN_POINT('Ctrl Pts',(55.865579536064,19.1975478202201,11.6771490845713));
#25419=CARTESIAN_POINT('Ctrl Pts',(55.9881162101072,19.261701667652,11.685219061316));
#25420=CARTESIAN_POINT('Ctrl Pts',(56.1178032133245,19.3477720475628,11.6948743816671));
#25421=CARTESIAN_POINT('Ctrl Pts',(56.1324282389952,19.3577614416785,11.6959799994203));
#25422=CARTESIAN_POINT('Ctrl Pts',(56.1544180683807,19.3732146676621,11.6976690260852));
#25423=CARTESIAN_POINT('Ctrl Pts',(56.1618816593078,19.3785368954701,11.6982470465856));
#25424=CARTESIAN_POINT('Ctrl Pts',(56.1747712690332,19.3878630649504,11.6992536944825));
#25425=CARTESIAN_POINT('Ctrl Pts',(56.1802142029615,19.3918434574956,11.6996814088273));
#25426=CARTESIAN_POINT('Ctrl Pts',(56.1923543429414,19.4008163145345,11.7006413785659));
#25427=CARTESIAN_POINT('Ctrl Pts',(56.1990405505272,19.40582338065,11.7011741974879));
#25428=CARTESIAN_POINT('Ctrl Pts',(56.2167769579273,19.4192802584887,11.7025987324203));
#25429=CARTESIAN_POINT('Ctrl Pts',(56.2277703923831,19.4278037928207,11.7034933348982));
#25430=CARTESIAN_POINT('Ctrl Pts',(56.2760815680787,19.4660766001242,11.7074774426777));
#25431=CARTESIAN_POINT('Ctrl Pts',(56.3124111099828,19.4970423819774,11.7106152424014));
#25432=CARTESIAN_POINT('Ctrl Pts',(56.3706333108814,19.5503902479971,11.7158890542039));
#25433=CARTESIAN_POINT('Ctrl Pts',(56.3931733144877,19.5720391942206,11.7179962023984));
#25434=CARTESIAN_POINT('Ctrl Pts',(56.5286298779206,19.7084017366175,11.7310645854318));
#25435=CARTESIAN_POINT('Ctrl Pts',(56.6278131568691,19.8358901568559,11.7424877818989));
#25436=CARTESIAN_POINT('Ctrl Pts',(56.7283783599356,20.0035409787108,11.755865466038));
#25437=CARTESIAN_POINT('Ctrl Pts',(56.7453864953543,20.0336415783008,11.7582068080424));
#25438=CARTESIAN_POINT('Ctrl Pts',(56.7715301444128,20.0828543706097,11.7619216174066));
#25439=CARTESIAN_POINT('Ctrl Pts',(56.7811582356661,20.101695717181,11.7633179043396));
#25440=CARTESIAN_POINT('Ctrl Pts',(56.7935316211003,20.1268908157473,11.7651474646895));
#25441=CARTESIAN_POINT('Ctrl Pts',(56.7965458499883,20.1331099632523,11.7655960729122));
#25442=CARTESIAN_POINT('Ctrl Pts',(56.8014537776446,20.1433718562911,11.766331220129));
#25443=CARTESIAN_POINT('Ctrl Pts',(56.8033663054284,20.1474054545164,11.7666188973632));
#25444=CARTESIAN_POINT('Ctrl Pts',(56.8070878394178,20.1553228670937,11.7671810074644));
#25445=CARTESIAN_POINT('Ctrl Pts',(56.8088978946037,20.1592061336748,11.7674555013033));
#25446=CARTESIAN_POINT('Ctrl Pts',(56.8133239418719,20.1687821618061,11.7681295035288));
#25447=CARTESIAN_POINT('Ctrl Pts',(56.8159256810885,20.1744815350345,11.7685281428671));
#25448=CARTESIAN_POINT('Ctrl Pts',(56.8247646701282,20.1940882348842,11.7698912518608));
#25449=CARTESIAN_POINT('Ctrl Pts',(56.8308695340691,20.2080551427808,11.7708480402085));
#25450=CARTESIAN_POINT('Ctrl Pts',(56.8882789174613,20.3436113255428,11.7800103280332));
#25451=CARTESIAN_POINT('Ctrl Pts',(56.9275653013854,20.4699571327537,11.7876076710108));
#25452=CARTESIAN_POINT('Ctrl Pts',(56.9829277273967,20.739923636688,11.8035981121753));
#25453=CARTESIAN_POINT('Ctrl Pts',(56.9964983245879,20.8832562912275,11.811973697707));
#25454=CARTESIAN_POINT('Ctrl Pts',(56.9943352706789,21.0442697577232,11.8219654479741));
#25455=CARTESIAN_POINT('Ctrl Pts',(56.9938708842138,21.0617401814132,11.823056653864));
#25456=CARTESIAN_POINT('Ctrl Pts',(56.9928149652987,21.0883132223465,11.8247281066979));
#25457=CARTESIAN_POINT('Ctrl Pts',(56.9923904433903,21.0974219061135,11.8253031374082));
#25458=CARTESIAN_POINT('Ctrl Pts',(56.9915436669917,21.1132553857507,11.8263064701525));
#25459=CARTESIAN_POINT('Ctrl Pts',(56.9911497618781,21.1199815981227,11.8267338781739));
#25460=CARTESIAN_POINT('Ctrl Pts',(56.990189162716,21.1350739491969,11.82769561595));
#25461=CARTESIAN_POINT('Ctrl Pts',(56.9896037802113,21.1434387303775,11.8282305235063));
#25462=CARTESIAN_POINT('Ctrl Pts',(56.9878960213922,21.165814788267,11.8296665569888));
#25463=CARTESIAN_POINT('Ctrl Pts',(56.9866782750849,21.1798181036466,11.8305706518607));
#25464=CARTESIAN_POINT('Ctrl Pts',(56.9805393109561,21.2427041586252,11.8346558233155));
#25465=CARTESIAN_POINT('Ctrl Pts',(56.9739615287026,21.2914042809144,11.8378882491754));
#25466=CARTESIAN_POINT('Ctrl Pts',(56.9607006026724,21.3681109454481,11.8430925321384));
#25467=CARTESIAN_POINT('Ctrl Pts',(56.9551972352366,21.3963031285349,11.8450296427212));
#25468=CARTESIAN_POINT('Ctrl Pts',(56.9119954546371,21.5947264549333,11.8588307755259));
#25469=CARTESIAN_POINT('Ctrl Pts',(56.8527350294271,21.7594667432054,11.871254645442));
#25470=CARTESIAN_POINT('Ctrl Pts',(56.7605705553206,21.9381542627826,11.8849025633339));
#25471=CARTESIAN_POINT('Ctrl Pts',(56.7478401449521,21.9616637006251,11.8866999293232));
#25472=CARTESIAN_POINT('Ctrl Pts',(56.725984260694,22.0001566094142,11.889637457561));
#25473=CARTESIAN_POINT('Ctrl Pts',(56.7171271470828,22.0152878030526,11.8907907534902));
#25474=CARTESIAN_POINT('Ctrl Pts',(56.7047486629335,22.0358093173544,11.8923509123996));
#25475=CARTESIAN_POINT('Ctrl Pts',(56.7013993069672,22.0413017558374,11.8927680817718));
#25476=CARTESIAN_POINT('Ctrl Pts',(56.6957346523005,22.0504906346733,11.8934652157797));
#25477=CARTESIAN_POINT('Ctrl Pts',(56.6934337184912,22.054195819914,11.8937460997775));
#25478=CARTESIAN_POINT('Ctrl Pts',(56.6890484365095,22.0612060160192,11.8942770731162));
#25479=CARTESIAN_POINT('Ctrl Pts',(56.6869665056987,22.0645124887026,11.8945273224618));
#25480=CARTESIAN_POINT('Ctrl Pts',(56.6814899121684,22.0731538668655,11.8951808954572));
#25481=CARTESIAN_POINT('Ctrl Pts',(56.6780795409149,22.0784788378371,11.8955831908399));
#25482=CARTESIAN_POINT('Ctrl Pts',(56.6661729861896,22.0968765745039,11.8969718918525));
#25483=CARTESIAN_POINT('Ctrl Pts',(56.6575486488922,22.1098662764253,11.8979502247717));
#25484=CARTESIAN_POINT('Ctrl Pts',(56.5784345056262,22.2260459841081,11.9066936838913));
#25485=CARTESIAN_POINT('Ctrl Pts',(56.4985351391853,22.3225148223572,11.9139163581989));
#25486=CARTESIAN_POINT('Ctrl Pts',(56.3063961347223,22.5145504697821,11.9296762693822));
#25487=CARTESIAN_POINT('Ctrl Pts',(56.1915700024885,22.6064519239246,11.938199231451));
#25488=CARTESIAN_POINT('Ctrl Pts',(56.0511479447294,22.6954351446342,11.9484888866744));
#25489=CARTESIAN_POINT('Ctrl Pts',(56.0344255130896,22.7056893464353,11.9497114961709));
#25490=CARTESIAN_POINT('Ctrl Pts',(56.0093424929474,22.7205657396226,11.9515426309291));
#25491=CARTESIAN_POINT('Ctrl Pts',(56.0010952054297,22.7253773839345,11.9521442725404));
#25492=CARTESIAN_POINT('Ctrl Pts',(55.9863144022977,22.7338591680085,11.9532219162576));
#25493=CARTESIAN_POINT('Ctrl Pts',(55.9797941094481,22.7375520755519,11.9536970868383));
#25494=CARTESIAN_POINT('Ctrl Pts',(55.9659664286467,22.7452810971178,11.9547044167121));
#25495=CARTESIAN_POINT('Ctrl Pts',(55.9586542191973,22.7493082443502,11.9552368851356));
#25496=CARTESIAN_POINT('Ctrl Pts',(55.9391117640425,22.7599117826715,11.9566594913001));
#25497=CARTESIAN_POINT('Ctrl Pts',(55.9268379356385,22.7664064688035,11.9575525017668));
#25498=CARTESIAN_POINT('Ctrl Pts',(55.8722927082063,22.7945440224227,11.9615197257005));
#25499=CARTESIAN_POINT('Ctrl Pts',(55.8293271081332,22.8147999152168,11.9646417322663));
#25500=CARTESIAN_POINT('Ctrl Pts',(55.7565710933529,22.8459769336753,11.9699271254088));
#25501=CARTESIAN_POINT('Ctrl Pts',(55.7271679174722,22.8577559886089,11.9720626557149));
#25502=CARTESIAN_POINT('Ctrl Pts',(55.5349972932419,22.9294792850819,11.9860100040474));
#25503=CARTESIAN_POINT('Ctrl Pts',(55.3653019640875,22.9686690743636,11.9983679866657));
#25504=CARTESIAN_POINT('Ctrl Pts',(55.183281523058,22.9863345084838,12.0107810213343));
#25505=CARTESIAN_POINT('Ctrl Pts',(55.1738677419974,22.987180641727,12.0114204197375));
#25506=CARTESIAN_POINT('Ctrl Pts',(55.1644483513162,22.987959834164,12.0120574026292));
#25507=CARTESIAN_POINT('Origin',(55.,21.,6.22095488139522));
#25508=CARTESIAN_POINT('',(55.1641804122445,22.9848227319589,12.9685061347694));
#25509=CARTESIAN_POINT('',(55.1644480621455,22.9879598580848,12.8106050954514));
#25510=CARTESIAN_POINT('',(55.1644483516311,22.987959834138,6.22095488139522));
#25511=CARTESIAN_POINT('',(53.0027029554326,20.9989116431895,12.3790451186048));
#25512=CARTESIAN_POINT('Ctrl Pts',(53.0027029554326,20.9989116431895,12.3790451186048));
#25513=CARTESIAN_POINT('Ctrl Pts',(53.0022880654464,20.9358127580545,12.3830871152256));
#25514=CARTESIAN_POINT('Ctrl Pts',(53.0336285294611,20.2121000156345,12.429473543416));
#25515=CARTESIAN_POINT('Ctrl Pts',(53.9157199028027,18.906273152354,12.5182044031761));
#25516=CARTESIAN_POINT('Ctrl Pts',(56.1713030095069,18.9536850922569,12.6452376978851));
#25517=CARTESIAN_POINT('Ctrl Pts',(57.3544922361658,20.8746135909814,12.7722709925941));
#25518=CARTESIAN_POINT('Ctrl Pts',(56.5295840241903,22.6014213230593,12.8800271382222));
#25519=CARTESIAN_POINT('Ctrl Pts',(55.5256092840336,22.9540479213118,12.9454388522806));
#25520=CARTESIAN_POINT('Ctrl Pts',(55.1641804122445,22.9848227319589,12.9685061347694));
#25521=CARTESIAN_POINT('Ctrl Pts',(53.0052503456376,20.9988257252519,12.37758152771));
#25522=CARTESIAN_POINT('Ctrl Pts',(53.0051430199567,21.1811406948336,12.3666360704211));
#25523=CARTESIAN_POINT('Ctrl Pts',(53.0300289413803,21.3626262549886,12.3564518925146));
#25524=CARTESIAN_POINT('Ctrl Pts',(53.0957203442371,21.5970592726417,12.3418950490065));
#25525=CARTESIAN_POINT('Ctrl Pts',(53.1148994162989,21.6550995822071,12.338178036601));
#25526=CARTESIAN_POINT('Ctrl Pts',(53.1418726252789,21.7256716310185,12.333472085354));
#25527=CARTESIAN_POINT('Ctrl Pts',(53.147181766391,21.7391219334858,12.3325666701201));
#25528=CARTESIAN_POINT('Ctrl Pts',(53.1558339602003,21.7603624242075,12.3311227740389));
#25529=CARTESIAN_POINT('Ctrl Pts',(53.1590813119202,21.7681912384199,12.3305875209643));
#25530=CARTESIAN_POINT('Ctrl Pts',(53.1652864303741,21.7828854058785,12.3295769999928));
#25531=CARTESIAN_POINT('Ctrl Pts',(53.1682330963473,21.789755309888,12.3291021157517));
#25532=CARTESIAN_POINT('Ctrl Pts',(53.1749512600266,21.805178263954,12.3280304173673));
#25533=CARTESIAN_POINT('Ctrl Pts',(53.1787443842762,21.8137216460812,12.3274328729792));
#25534=CARTESIAN_POINT('Ctrl Pts',(53.1885960385503,21.835496878911,12.3258997374109));
#25535=CARTESIAN_POINT('Ctrl Pts',(53.1947394942185,21.8486894802329,12.3249612506893));
#25536=CARTESIAN_POINT('Ctrl Pts',(53.2345047469547,21.9316965807568,12.3189940258471));
#25537=CARTESIAN_POINT('Ctrl Pts',(53.2720221886558,21.9995609300389,12.3138306352353));
#25538=CARTESIAN_POINT('Ctrl Pts',(53.3980946607118,22.1992064979579,12.2977554127866));
#25539=CARTESIAN_POINT('Ctrl Pts',(53.4984918082965,22.3227482439987,12.2864988986357));
#25540=CARTESIAN_POINT('Ctrl Pts',(53.6371566220555,22.4570064550637,12.273293655286));
#25541=CARTESIAN_POINT('Ctrl Pts',(53.6624755690758,22.4802832691831,12.2709649059374));
#25542=CARTESIAN_POINT('Ctrl Pts',(53.6990670340759,22.5122175747127,12.2677276379227));
#25543=CARTESIAN_POINT('Ctrl Pts',(53.7098484448114,22.5214261615813,12.2667889012373));
#25544=CARTESIAN_POINT('Ctrl Pts',(53.7288695699239,22.5373248197416,12.2651602551429));
#25545=CARTESIAN_POINT('Ctrl Pts',(53.7370660771486,22.5440654422756,12.2644671840838));
#25546=CARTESIAN_POINT('Ctrl Pts',(53.7494236672406,22.5540638062983,12.2634357688251));
#25547=CARTESIAN_POINT('Ctrl Pts',(53.7535443801015,22.5573708188114,12.2630940574513));
#25548=CARTESIAN_POINT('Ctrl Pts',(53.7608641446128,22.5631975166084,12.2624910566183));
#25549=CARTESIAN_POINT('Ctrl Pts',(53.7640578209501,22.565723818292,12.2622293007716));
#25550=CARTESIAN_POINT('Ctrl Pts',(53.7710471285791,22.5712178764809,12.2616593827586));
#25551=CARTESIAN_POINT('Ctrl Pts',(53.7748457799041,22.5741816647757,12.2613515004976));
#25552=CARTESIAN_POINT('Ctrl Pts',(53.7852075692985,22.582205926672,12.2605166176702));
#25553=CARTESIAN_POINT('Ctrl Pts',(53.7917916526752,22.5872393767951,12.2599914797352));
#25554=CARTESIAN_POINT('Ctrl Pts',(53.8242569793778,22.6117396467035,12.2574272292566));
#25555=CARTESIAN_POINT('Ctrl Pts',(53.8505798941841,22.6306164603011,12.2554259711973));
#25556=CARTESIAN_POINT('Ctrl Pts',(54.0473379179107,22.7645828929135,12.2409354831692));
#25557=CARTESIAN_POINT('Ctrl Pts',(54.2342093319486,22.8533491080173,12.2295753213666));
#25558=CARTESIAN_POINT('Ctrl Pts',(54.4838990902971,22.9276075138342,12.2139335296876));
#25559=CARTESIAN_POINT('Ctrl Pts',(54.5370451251463,22.9410571444666,12.2105889408114));
#25560=CARTESIAN_POINT('Ctrl Pts',(54.6043639199794,22.9551714260069,12.2063018116373));
#25561=CARTESIAN_POINT('Ctrl Pts',(54.6180832965096,22.9578975531699,12.2054255616982));
#25562=CARTESIAN_POINT('Ctrl Pts',(54.6400578522198,22.962024286006,12.2040175211832));
#25563=CARTESIAN_POINT('Ctrl Pts',(54.6482953090117,22.9635176229156,12.2034886846738));
#25564=CARTESIAN_POINT('Ctrl Pts',(54.6639215644729,22.966248959863,12.2024834715809));
#25565=CARTESIAN_POINT('Ctrl Pts',(54.6713084315377,22.9674972775839,12.2020074317473));
#25566=CARTESIAN_POINT('Ctrl Pts',(54.6880919877947,22.9702364003703,12.2009238146141));
#25567=CARTESIAN_POINT('Ctrl Pts',(54.6974926081884,22.9717016392285,12.2003154392419));
#25568=CARTESIAN_POINT('Ctrl Pts',(54.7218407252643,22.9753184637094,12.1987358533831));
#25569=CARTESIAN_POINT('Ctrl Pts',(54.7368025956508,22.9773676240688,12.1977614419176));
#25570=CARTESIAN_POINT('Ctrl Pts',(54.8441954606282,22.9908355852994,12.1907390709385));
#25571=CARTESIAN_POINT('Ctrl Pts',(54.9372894314649,22.9959369468908,12.1844936593506));
#25572=CARTESIAN_POINT('Ctrl Pts',(55.0751646497579,22.993836315959,12.1750325650663));
#25573=CARTESIAN_POINT('Ctrl Pts',(55.119876720263,22.9916469051696,12.1719328881632));
#25574=CARTESIAN_POINT('Ctrl Pts',(55.1644487484638,22.9879598013111,12.1688212129648));
#25575=CARTESIAN_POINT('Ctrl Pts',(55.1644483513162,22.987959834164,12.0120574026292));
#25576=CARTESIAN_POINT('Ctrl Pts',(55.1472821333312,22.9893798609661,12.0132182619184));
#25577=CARTESIAN_POINT('Ctrl Pts',(55.1300972845231,22.9905775594477,12.0143711020113));
#25578=CARTESIAN_POINT('Ctrl Pts',(55.0954212548586,22.9925432918177,12.0166759024132));
#25579=CARTESIAN_POINT('Ctrl Pts',(55.0779313521235,22.9933039759507,12.0178274312678));
#25580=CARTESIAN_POINT('Ctrl Pts',(55.054006748931,22.9940291292229,12.0193856079272));
#25581=CARTESIAN_POINT('Ctrl Pts',(55.0475794876185,22.9941928422897,12.019802528981));
#25582=CARTESIAN_POINT('Ctrl Pts',(55.0367917232815,22.9944154398785,12.0204993644048));
#25583=CARTESIAN_POINT('Ctrl Pts',(55.0324316603022,22.9944911045778,12.0207801964675));
#25584=CARTESIAN_POINT('Ctrl Pts',(55.0241637830745,22.994607466636,12.021311158452));
#25585=CARTESIAN_POINT('Ctrl Pts',(55.0202560514173,22.9946509788424,12.02156144789));
#25586=CARTESIAN_POINT('Ctrl Pts',(55.0100215272797,22.9947348597406,12.0222152855486));
#25587=CARTESIAN_POINT('Ctrl Pts',(55.003694564455,22.9947566128423,12.0226178038764));
#25588=CARTESIAN_POINT('Ctrl Pts',(54.9817553038484,22.994727659288,12.0240080647338));
#25589=CARTESIAN_POINT('Ctrl Pts',(54.9661433147736,22.9945237687374,12.0249877104127));
#25590=CARTESIAN_POINT('Ctrl Pts',(54.825889647723,22.9910447290102,12.0337145852198));
#25591=CARTESIAN_POINT('Ctrl Pts',(54.7017906309722,22.9762726086229,12.0409219973607));
#25592=CARTESIAN_POINT('Ctrl Pts',(54.4789042336405,22.9282515429392,12.0541494699615));
#25593=CARTESIAN_POINT('Ctrl Pts',(54.3797853415393,22.8986907346663,12.0601408996262));
#25594=CARTESIAN_POINT('Ctrl Pts',(54.2336163804897,22.8424250740349,12.0695551386846));
#25595=CARTESIAN_POINT('Ctrl Pts',(54.1846185782496,22.8212705399329,12.0728136520983));
#25596=CARTESIAN_POINT('Ctrl Pts',(54.1240302640645,22.7921765732984,12.0770035744064));
#25597=CARTESIAN_POINT('Ctrl Pts',(54.1115932251664,22.786044018273,12.0778723665361));
#25598=CARTESIAN_POINT('Ctrl Pts',(54.0917769643718,22.7760146664026,12.0792711390396));
#25599=CARTESIAN_POINT('Ctrl Pts',(54.0843563559767,22.7722002966523,12.079798233098));
#25600=CARTESIAN_POINT('Ctrl Pts',(54.0703162897619,22.764871645857,12.0808018921727));
#25601=CARTESIAN_POINT('Ctrl Pts',(54.0636922647943,22.7613663871871,12.0812781324664));
#25602=CARTESIAN_POINT('Ctrl Pts',(54.0486673785466,22.7533069097825,12.0823646454591));
#25603=CARTESIAN_POINT('Ctrl Pts',(54.0402792244526,22.7487295114629,12.0829757339127));
#25604=CARTESIAN_POINT('Ctrl Pts',(54.01859545913,22.7366937226092,12.0845673272026));
#25605=CARTESIAN_POINT('Ctrl Pts',(54.0053520827729,22.729142983772,12.0855511155753));
#25606=CARTESIAN_POINT('Ctrl Pts',(53.9092048496818,22.6728544070532,12.0927810882019));
#25607=CARTESIAN_POINT('Ctrl Pts',(53.8298476360918,22.6183369474405,12.0992383245163));
#25608=CARTESIAN_POINT('Ctrl Pts',(53.6445384740878,22.4702554054835,12.1155364253462));
#25609=CARTESIAN_POINT('Ctrl Pts',(53.5439956726429,22.3707574159044,12.1255220984236));
#25610=CARTESIAN_POINT('Ctrl Pts',(53.4238104694147,22.2235415691796,12.1385054764302));
#25611=CARTESIAN_POINT('Ctrl Pts',(53.3942355254379,22.1844613763546,12.1418019695838));
#25612=CARTESIAN_POINT('Ctrl Pts',(53.3609408221187,22.1369231764249,12.1456025885097));
#25613=CARTESIAN_POINT('Ctrl Pts',(53.3558046977686,22.1294826750636,12.1461915779772));
#25614=CARTESIAN_POINT('Ctrl Pts',(53.3479445483716,22.1179287459472,12.1470968365637));
#25615=CARTESIAN_POINT('Ctrl Pts',(53.3451849768813,22.1138398164948,12.1474154147054));
#25616=CARTESIAN_POINT('Ctrl Pts',(53.3401133638309,22.1062646230099,12.1480022489089));
#25617=CARTESIAN_POINT('Ctrl Pts',(53.3377971339463,22.1027813444625,12.1482707773721));
#25618=CARTESIAN_POINT('Ctrl Pts',(53.3325743898537,22.0948732448941,12.1488774708408));
#25619=CARTESIAN_POINT('Ctrl Pts',(53.3296745266765,22.0904441308392,12.1492151917903));
#25620=CARTESIAN_POINT('Ctrl Pts',(53.3211113419756,22.0772508150296,12.1502152117901));
#25621=CARTESIAN_POINT('Ctrl Pts',(53.3154990143388,22.0684535015435,12.1508742355331));
#25622=CARTESIAN_POINT('Ctrl Pts',(53.2629161331407,21.9845856670118,12.1570874647548));
#25623=CARTESIAN_POINT('Ctrl Pts',(53.2209181614938,21.9064994454913,12.1623495492353));
#25624=CARTESIAN_POINT('Ctrl Pts',(53.1070969862126,21.6562528897742,12.1784337506831));
#25625=CARTESIAN_POINT('Ctrl Pts',(53.0541010424324,21.4766798628353,12.1889940505051));
#25626=CARTESIAN_POINT('Ctrl Pts',(53.0234716469356,21.2699560697406,12.2018864856461));
#25627=CARTESIAN_POINT('Ctrl Pts',(53.0205338348667,21.2474959515836,12.2032950122899));
#25628=CARTESIAN_POINT('Ctrl Pts',(53.0168382884031,21.2149407027535,12.2053499169677));
#25629=CARTESIAN_POINT('Ctrl Pts',(53.0157738585393,21.2048816573873,12.2059866733096));
#25630=CARTESIAN_POINT('Ctrl Pts',(53.0140465266381,21.1872797183465,12.2071042769734));
#25631=CARTESIAN_POINT('Ctrl Pts',(53.0133499749683,21.179740275745,12.2075840586401));
#25632=CARTESIAN_POINT('Ctrl Pts',(53.0119987423176,21.1641458840986,12.2085787341071));
#25633=CARTESIAN_POINT('Ctrl Pts',(53.0113500551597,21.1560905683706,12.2090938066963));
#25634=CARTESIAN_POINT('Ctrl Pts',(53.0098098111806,21.1353927633548,12.2104206327715));
#25635=CARTESIAN_POINT('Ctrl Pts',(53.0089897726282,21.1227454693597,12.2112346092121));
#25636=CARTESIAN_POINT('Ctrl Pts',(53.0062447238034,21.0730836660248,12.2144439925563));
#25637=CARTESIAN_POINT('Ctrl Pts',(53.0052310952104,21.0360282642891,12.2168675498722));
#25638=CARTESIAN_POINT('Ctrl Pts',(53.0052817453659,20.9381172869696,12.2233515297983));
#25639=CARTESIAN_POINT('Ctrl Pts',(53.0080975985821,20.8773051181598,12.2274615491898));
#25640=CARTESIAN_POINT('Ctrl Pts',(53.0213795755411,20.7333595634598,12.2373681098823));
#25641=CARTESIAN_POINT('Ctrl Pts',(53.0343112535921,20.6505686492285,12.2432105029038));
#25642=CARTESIAN_POINT('Ctrl Pts',(53.0603629422339,20.5328904330271,12.2516151296792));
#25643=CARTESIAN_POINT('Ctrl Pts',(53.0693154290845,20.4971675755938,12.2541793133802));
#25644=CARTESIAN_POINT('Ctrl Pts',(53.0800301865641,20.4589345690755,12.2569268177156));
#25645=CARTESIAN_POINT('Ctrl Pts',(53.0808147055468,20.4561583955903,12.2571263364176));
#25646=CARTESIAN_POINT('Ctrl Pts',(53.1008998768015,20.3856678098868,12.2621926687645));
#25647=CARTESIAN_POINT('Ctrl Pts',(53.1237686827481,20.3190127898694,12.2669919913282));
#25648=CARTESIAN_POINT('Ctrl Pts',(53.1539423563909,20.2442201089912,12.2722863230984));
#25649=CARTESIAN_POINT('Ctrl Pts',(53.1578399335318,20.2347690758087,12.2729535925007));
#25650=CARTESIAN_POINT('Ctrl Pts',(53.163848401717,20.2205114372457,12.2739571302829));
#25651=CARTESIAN_POINT('Ctrl Pts',(53.1659058199693,20.2156826843363,12.2742964665259));
#25652=CARTESIAN_POINT('Ctrl Pts',(53.1696361114668,20.2070226522457,12.274903996813));
#25653=CARTESIAN_POINT('Ctrl Pts',(53.1713019827506,20.2031884782498,12.2751726020627));
#25654=CARTESIAN_POINT('Ctrl Pts',(53.1749742992301,20.1948084431792,12.275758844669));
#25655=CARTESIAN_POINT('Ctrl Pts',(53.176985676469,20.1902648401207,12.2760761777264));
#25656=CARTESIAN_POINT('Ctrl Pts',(53.1827729190191,20.1773226082435,12.27697871971));
#25657=CARTESIAN_POINT('Ctrl Pts',(53.1865900496132,20.1689424121296,12.2775614760752));
#25658=CARTESIAN_POINT('Ctrl Pts',(53.2126470393962,20.1127708617911,12.2814585011983));
#25659=CARTESIAN_POINT('Ctrl Pts',(53.2367178338558,20.0658462498892,12.2846695391328));
#25660=CARTESIAN_POINT('Ctrl Pts',(53.3473309939483,19.869762140052,12.2981261516832));
#25661=CARTESIAN_POINT('Ctrl Pts',(53.4511517904791,19.7312095847649,12.3077963019268));
#25662=CARTESIAN_POINT('Ctrl Pts',(53.6159919661092,19.562080601039,12.3218839798161));
#25663=CARTESIAN_POINT('Ctrl Pts',(53.6626392790816,19.5185967795252,12.3257533886522));
#25664=CARTESIAN_POINT('Ctrl Pts',(53.7228073859863,19.4676702435436,12.3306580584848));
#25665=CARTESIAN_POINT('Ctrl Pts',(53.7344402308553,19.4580486691212,12.3316024761219));
#25666=CARTESIAN_POINT('Ctrl Pts',(53.7529494332447,19.4430901821095,12.3330997518733));
#25667=CARTESIAN_POINT('Ctrl Pts',(53.7597535867706,19.4376645278051,12.333649034611));
#25668=CARTESIAN_POINT('Ctrl Pts',(53.7723944876453,19.4277192489391,12.3346675434637));
#25669=CARTESIAN_POINT('Ctrl Pts',(53.7782212625553,19.4231871485653,12.3351362618696));
#25670=CARTESIAN_POINT('Ctrl Pts',(53.7912142997399,19.4131963433191,12.3361798471587));
#25671=CARTESIAN_POINT('Ctrl Pts',(53.7983926208869,19.4077536572273,12.3367553311327));
#25672=CARTESIAN_POINT('Ctrl Pts',(53.8191804163547,19.3922127434899,12.3384189711184));
#25673=CARTESIAN_POINT('Ctrl Pts',(53.8328817630903,19.3822392812993,12.3395119333565));
#25674=CARTESIAN_POINT('Ctrl Pts',(53.9500018678375,19.2992476787905,12.3488271845166));
#25675=CARTESIAN_POINT('Ctrl Pts',(54.0600094596274,19.2360664316792,12.3574255488432));
#25676=CARTESIAN_POINT('Ctrl Pts',(54.3006826264698,19.1267773209753,12.3757719254443));
#25677=CARTESIAN_POINT('Ctrl Pts',(54.4316916344296,19.0829614577896,12.3855058729236));
#25678=CARTESIAN_POINT('Ctrl Pts',(54.5901272621266,19.0476593254977,12.3963733902617));
#25679=CARTESIAN_POINT('Ctrl Pts',(54.614177589219,19.0427644572554,12.3979984186275));
#25680=CARTESIAN_POINT('Ctrl Pts',(54.6457664046384,19.0369402561056,12.4000953967686));
#25681=CARTESIAN_POINT('Ctrl Pts',(54.653227332864,19.035608562437,12.4005879623897));
#25682=CARTESIAN_POINT('Ctrl Pts',(54.665240349757,19.033534946345,12.4013764904729));
#25683=CARTESIAN_POINT('Ctrl Pts',(54.6697876495554,19.0327662479148,12.4016739233768));
#25684=CARTESIAN_POINT('Ctrl Pts',(54.6785341099816,19.0313188839393,12.4022439481143));
#25685=CARTESIAN_POINT('Ctrl Pts',(54.6827327970208,19.0306378755094,12.402516663384));
#25686=CARTESIAN_POINT('Ctrl Pts',(54.6927242454305,19.0290500892357,12.4031634989931));
#25687=CARTESIAN_POINT('Ctrl Pts',(54.6985189418029,19.0281554032504,12.4035369403434));
#25688=CARTESIAN_POINT('Ctrl Pts',(54.7180413803295,19.025229260629,12.4047896036267));
#25689=CARTESIAN_POINT('Ctrl Pts',(54.7317867191033,19.0233154531785,12.4056624873672));
#25690=CARTESIAN_POINT('Ctrl Pts',(54.8097936684789,19.0132829965273,12.4105705016985));
#25691=CARTESIAN_POINT('Ctrl Pts',(54.8744071625643,19.0081538540431,12.4144607834168));
#25692=CARTESIAN_POINT('Ctrl Pts',(55.1091116861522,19.0009922317899,12.4283215340788));
#25693=CARTESIAN_POINT('Ctrl Pts',(55.2790223518195,19.0175554539421,12.4379057308322));
#25694=CARTESIAN_POINT('Ctrl Pts',(55.4926448469044,19.0664178955266,12.4511093268226));
#25695=CARTESIAN_POINT('Ctrl Pts',(55.5400880121583,19.0791296147358,12.4541127327729));
#25696=CARTESIAN_POINT('Ctrl Pts',(55.6004422960877,19.0977134522889,12.4580484706044));
#25697=CARTESIAN_POINT('Ctrl Pts',(55.6138290485315,19.1019907946169,12.4589287874954));
#25698=CARTESIAN_POINT('Ctrl Pts',(55.6351286874522,19.1090453692252,12.4603417288893));
#25699=CARTESIAN_POINT('Ctrl Pts',(55.6430713518842,19.1117317197546,12.4608713611555));
#25700=CARTESIAN_POINT('Ctrl Pts',(55.6573656860306,19.1166669662475,12.4618295953628));
#25701=CARTESIAN_POINT('Ctrl Pts',(55.6637233780522,19.1188981322652,12.4622576049433));
#25702=CARTESIAN_POINT('Ctrl Pts',(55.6786591233846,19.1242248212353,12.463267443325));
#25703=CARTESIAN_POINT('Ctrl Pts',(55.6872274373432,19.1273470231185,12.4638501513042));
#25704=CARTESIAN_POINT('Ctrl Pts',(55.7121565979709,19.1366250750634,12.4655555780946));
#25705=CARTESIAN_POINT('Ctrl Pts',(55.7284579654797,19.1429372409208,12.4666834844914));
#25706=CARTESIAN_POINT('Ctrl Pts',(55.8781738369404,19.2031843337904,12.4771631661521));
#25707=CARTESIAN_POINT('Ctrl Pts',(56.0054424064446,19.2711835986645,12.487009264057));
#25708=CARTESIAN_POINT('Ctrl Pts',(56.2330030922954,19.426450392841,12.5061977560865));
#25709=CARTESIAN_POINT('Ctrl Pts',(56.3341352727608,19.5112274444425,12.5154534160502));
#25710=CARTESIAN_POINT('Ctrl Pts',(56.4368506154463,19.6162656768939,12.525176922097));
#25711=CARTESIAN_POINT('Ctrl Pts',(56.4473932059313,19.6272970789773,12.5261788955187));
#25712=CARTESIAN_POINT('Ctrl Pts',(56.4620866817271,19.6430293364719,12.5275796435325));
#25713=CARTESIAN_POINT('Ctrl Pts',(56.4663432664172,19.6476301267194,12.5279859460844));
#25714=CARTESIAN_POINT('Ctrl Pts',(56.4734732139227,19.6554098727559,12.5286672767197));
#25715=CARTESIAN_POINT('Ctrl Pts',(56.4763581225468,19.6585781358597,12.5289431668842));
#25716=CARTESIAN_POINT('Ctrl Pts',(56.4822271517121,19.6650654871403,12.5295048235805));
#25717=CARTESIAN_POINT('Ctrl Pts',(56.4852103749431,19.6683853312566,12.5297905237785));
#25718=CARTESIAN_POINT('Ctrl Pts',(56.4927821118931,19.6768685467284,12.5305162849049));
#25719=CARTESIAN_POINT('Ctrl Pts',(56.4973550399905,19.6820458415373,12.5309551947706));
#25720=CARTESIAN_POINT('Ctrl Pts',(56.5158057323754,19.7031550006155,12.5327290007357));
#25721=CARTESIAN_POINT('Ctrl Pts',(56.529457440082,19.7192837962775,12.5340481871007));
#25722=CARTESIAN_POINT('Ctrl Pts',(56.5647197993602,19.7623126913729,12.5374830758078));
#25723=CARTESIAN_POINT('Ctrl Pts',(56.5858939361749,19.7895626313357,12.5395739828232));
#25724=CARTESIAN_POINT('Ctrl Pts',(56.7012832206323,19.9462917703661,12.5512191647472));
#25725=CARTESIAN_POINT('Ctrl Pts',(56.7803484695527,20.0861993479898,12.5602350253372));
#25726=CARTESIAN_POINT('Ctrl Pts',(56.8549736365081,20.2656495393253,12.5717442870465));
#25727=CARTESIAN_POINT('Ctrl Pts',(56.8672937415927,20.2975672900258,12.5737871581258));
#25728=CARTESIAN_POINT('Ctrl Pts',(56.8942489202137,20.3731296524752,12.5786322489278));
#25729=CARTESIAN_POINT('Ctrl Pts',(56.9082055420327,20.4169935575018,12.5814517602672));
#25730=CARTESIAN_POINT('Ctrl Pts',(56.9243405481291,20.4745196754187,12.5851769928329));
#25731=CARTESIAN_POINT('Ctrl Pts',(56.9279121800348,20.4877786339558,12.5860374369));
#25732=CARTESIAN_POINT('Ctrl Pts',(56.9334260126977,20.5091226884102,12.5874259467901));
#25733=CARTESIAN_POINT('Ctrl Pts',(56.9354550878136,20.5171850444797,12.587951202039));
#25734=CARTESIAN_POINT('Ctrl Pts',(56.9392187717076,20.5325447869017,12.5889534386144));
#25735=CARTESIAN_POINT('Ctrl Pts',(56.9409627410528,20.5398397495211,12.5894301090741));
#25736=CARTESIAN_POINT('Ctrl Pts',(56.9448470814285,20.5565028365895,12.5905205168217));
#25737=CARTESIAN_POINT('Ctrl Pts',(56.946960969867,20.5658768831708,12.5911350917431));
#25738=CARTESIAN_POINT('Ctrl Pts',(56.9532507468649,20.5947392086233,12.5930310729589));
#25739=CARTESIAN_POINT('Ctrl Pts',(56.9572022541346,20.6142746083907,12.5943195872321));
#25740=CARTESIAN_POINT('Ctrl Pts',(56.988165915428,20.7801027148525,12.6053048193061));
#25741=CARTESIAN_POINT('Ctrl Pts',(56.9990217609752,20.92890758912,12.6155277282375));
#25742=CARTESIAN_POINT('Ctrl Pts',(56.9884937645123,21.1996626274797,12.6344190490827));
#25743=CARTESIAN_POINT('Ctrl Pts',(56.9725237052528,21.3211358229798,12.6429852309299));
#25744=CARTESIAN_POINT('Ctrl Pts',(56.942065947612,21.455690119339,12.6521215862779));
#25745=CARTESIAN_POINT('Ctrl Pts',(56.9384222750827,21.4709487763316,12.6531521526536));
#25746=CARTESIAN_POINT('Ctrl Pts',(56.9330538267193,21.4923115395515,12.6545857315329));
#25747=CARTESIAN_POINT('Ctrl Pts',(56.9314794833029,21.4984523620172,12.6549967401416));
#25748=CARTESIAN_POINT('Ctrl Pts',(56.9288867564663,21.5083686977236,12.6556585813069));
#25749=CARTESIAN_POINT('Ctrl Pts',(56.9278865149936,21.5121488436463,12.6559104384413));
#25750=CARTESIAN_POINT('Ctrl Pts',(56.9257480022462,21.5201357382218,12.6564416101157));
#25751=CARTESIAN_POINT('Ctrl Pts',(56.924607048358,21.5243417439176,12.6567207625699));
#25752=CARTESIAN_POINT('Ctrl Pts',(56.9217522522921,21.5347307823527,12.6574089495316));
#25753=CARTESIAN_POINT('Ctrl Pts',(56.9200223274211,21.5409094135891,12.6578170625234));
#25754=CARTESIAN_POINT('Ctrl Pts',(56.9134867695878,21.5638254828419,12.6593267419904));
#25755=CARTESIAN_POINT('Ctrl Pts',(56.9084916810993,21.5805086945546,12.6604179054473));
#25756=CARTESIAN_POINT('Ctrl Pts',(56.8723459490667,21.6957197390413,12.6679120361855));
#25757=CARTESIAN_POINT('Ctrl Pts',(56.8337947479746,21.7917749090959,12.6739546209566));
#25758=CARTESIAN_POINT('Ctrl Pts',(56.7168825881373,22.0281278918137,12.6892776771497));
#25759=CARTESIAN_POINT('Ctrl Pts',(56.6287410221259,22.1627249469042,12.6984950768967));
#25760=CARTESIAN_POINT('Ctrl Pts',(56.5105750059554,22.3029671262384,12.7097978950417));
#25761=CARTESIAN_POINT('Ctrl Pts',(56.4953996876077,22.3203559695638,12.7112318489837));
#25762=CARTESIAN_POINT('Ctrl Pts',(56.473608954287,22.3444675493928,12.7132687675036));
#25763=CARTESIAN_POINT('Ctrl Pts',(56.4672419791969,22.3514130793825,12.7138613542192));
#25764=CARTESIAN_POINT('Ctrl Pts',(56.4560626666892,22.363436103517,12.7148975315937));
#25765=CARTESIAN_POINT('Ctrl Pts',(56.4512723458348,22.3685339140433,12.7153401811585));
#25766=CARTESIAN_POINT('Ctrl Pts',(56.4411885518834,22.3791525003565,12.7162692270472));
#25767=CARTESIAN_POINT('Ctrl Pts',(56.4358899519485,22.3846682290482,12.7167558406816));
#25768=CARTESIAN_POINT('Ctrl Pts',(56.4231963690036,22.3977307667788,12.7179179899864));
#25769=CARTESIAN_POINT('Ctrl Pts',(56.4157729474788,22.4052494992777,12.7185947625495));
#25770=CARTESIAN_POINT('Ctrl Pts',(56.3903945800356,22.4305484909044,12.7208990529384));
#25771=CARTESIAN_POINT('Ctrl Pts',(56.3721622572503,22.4480458264579,12.7225388378732));
#25772=CARTESIAN_POINT('Ctrl Pts',(56.3276634364322,22.4891556374522,12.7265058763382));
#25773=CARTESIAN_POINT('Ctrl Pts',(56.3010933190893,22.5124254143664,12.728846565667));
#25774=CARTESIAN_POINT('Ctrl Pts',(56.194082888121,22.6012364256864,12.7381666435083));
#25775=CARTESIAN_POINT('Ctrl Pts',(56.1092057846088,22.6611592559875,12.7453408391161));
#25776=CARTESIAN_POINT('Ctrl Pts',(55.913495595774,22.7776196881566,12.7612165740381));
#25777=CARTESIAN_POINT('Ctrl Pts',(55.8012362967081,22.8309647146541,12.7699119264545));
#25778=CARTESIAN_POINT('Ctrl Pts',(55.6700406827082,22.8789140543262,12.779162060202));
#25779=CARTESIAN_POINT('Ctrl Pts',(55.6552767042515,22.8841138546774,12.7801903058312));
#25780=CARTESIAN_POINT('Ctrl Pts',(55.6344543631186,22.8911730054278,12.7816212204077));
#25781=CARTESIAN_POINT('Ctrl Pts',(55.6284464640087,22.8931779419426,12.7820318470124));
#25782=CARTESIAN_POINT('Ctrl Pts',(55.6187150681843,22.8963740422706,12.7826932381613));
#25783=CARTESIAN_POINT('Ctrl Pts',(55.614997500106,22.8975829150014,12.7829450246593));
#25784=CARTESIAN_POINT('Ctrl Pts',(55.6071268653632,22.9001167160696,12.7834762047339));
#25785=CARTESIAN_POINT('Ctrl Pts',(55.6029729634754,22.9014389738646,12.7837554354888));
#25786=CARTESIAN_POINT('Ctrl Pts',(55.5926887186397,22.9046755340704,12.7844440868829));
#25787=CARTESIAN_POINT('Ctrl Pts',(55.586553338804,22.906573888092,12.7848525832263));
#25788=CARTESIAN_POINT('Ctrl Pts',(55.5637079491971,22.913521786356,12.7863653246141));
#25789=CARTESIAN_POINT('Ctrl Pts',(55.5469404736724,22.9183817258926,12.7874591117626));
#25790=CARTESIAN_POINT('Ctrl Pts',(55.504489668697,22.9300839508081,12.7901918895449));
#25791=CARTESIAN_POINT('Ctrl Pts',(55.4787287766821,22.9366343950759,12.7918169379439));
#25792=CARTESIAN_POINT('Ctrl Pts',(55.3578541463681,22.9648107347426,12.7993198089275));
#25793=CARTESIAN_POINT('Ctrl Pts',(55.2614624560589,22.9799346311093,12.804957572981));
#25794=CARTESIAN_POINT('Ctrl Pts',(55.1644480621455,22.9879598580848,12.8106050954514));
#25795=CARTESIAN_POINT('Origin',(55.,21.,6.22095488139522));
#25796=CARTESIAN_POINT('',(55.164448547645,22.9879598179233,13.7675726541794));
#25797=CARTESIAN_POINT('',(55.1644483515698,22.987959834143,13.6085666014869));
#25798=CARTESIAN_POINT('',(55.1644483516311,22.987959834138,6.22095488139522));
#25799=CARTESIAN_POINT('',(53.0046129860205,21.0017710049344,13.1790451186048));
#25800=CARTESIAN_POINT('Ctrl Pts',(55.164448547645,22.9879598179233,13.7675726541794));
#25801=CARTESIAN_POINT('Ctrl Pts',(55.2645411203093,22.9796799331608,13.7616912993627));
#25802=CARTESIAN_POINT('Ctrl Pts',(55.3639264204527,22.9638475460295,13.7559274711235));
#25803=CARTESIAN_POINT('Ctrl Pts',(55.5560482604016,22.9181326220663,13.7443471394518));
#25804=CARTESIAN_POINT('Ctrl Pts',(55.6485702217839,22.8888556037384,13.738558262633));
#25805=CARTESIAN_POINT('Ctrl Pts',(55.7527207671479,22.8473414357672,13.7315963732279));
#25806=CARTESIAN_POINT('Ctrl Pts',(55.7667853435036,22.8415480310159,13.7306467045588));
#25807=CARTESIAN_POINT('Ctrl Pts',(55.7895674137876,22.831857529926,13.7290921738092));
#25808=CARTESIAN_POINT('Ctrl Pts',(55.7983257700313,22.8280576223582,13.728490600419));
#25809=CARTESIAN_POINT('Ctrl Pts',(55.8139107996568,22.8211625275556,13.7274129097854));
#25810=CARTESIAN_POINT('Ctrl Pts',(55.8207479853913,22.8180914398187,13.726937622937));
#25811=CARTESIAN_POINT('Ctrl Pts',(55.8351675299038,22.8115166370394,13.7259298682735));
#25812=CARTESIAN_POINT('Ctrl Pts',(55.8427454973394,22.8080036926101,13.7253970900889));
#25813=CARTESIAN_POINT('Ctrl Pts',(55.862875685628,22.798517819093,13.7239732284081));
#25814=CARTESIAN_POINT('Ctrl Pts',(55.8753877317645,22.7924611843187,13.7230792645785));
#25815=CARTESIAN_POINT('Ctrl Pts',(55.9359533689449,22.7623581360577,13.7187073703467));
#25816=CARTESIAN_POINT('Ctrl Pts',(55.9830813035911,22.7365094724083,13.71516695115));
#25817=CARTESIAN_POINT('Ctrl Pts',(56.1950437690573,22.6088569416073,13.698581020333));
#25818=CARTESIAN_POINT('Ctrl Pts',(56.3455060137317,22.4853090060613,13.6847601643102));
#25819=CARTESIAN_POINT('Ctrl Pts',(56.5054234895833,22.3094530632374,13.6685684700548));
#25820=CARTESIAN_POINT('Ctrl Pts',(56.5339692678035,22.2758942584669,13.6656118533761));
#25821=CARTESIAN_POINT('Ctrl Pts',(56.5665649913327,22.2348971736623,13.6621806787774));
#25822=CARTESIAN_POINT('Ctrl Pts',(56.5717064772905,22.2283467167808,13.6616377456301));
#25823=CARTESIAN_POINT('Ctrl Pts',(56.5800345638026,22.2175985011034,13.6607557500721));
#25824=CARTESIAN_POINT('Ctrl Pts',(56.583245753735,22.213420049912,13.6604150319014));
#25825=CARTESIAN_POINT('Ctrl Pts',(56.5889760054388,22.2059022813359,13.6598059648329));
#25826=CARTESIAN_POINT('Ctrl Pts',(56.5915011470311,22.2025677353074,13.6595371961136));
#25827=CARTESIAN_POINT('Ctrl Pts',(56.5969945682994,22.1952658533723,13.6589516814145));
#25828=CARTESIAN_POINT('Ctrl Pts',(56.5999585567207,22.1912953997557,13.6586352329643));
#25829=CARTESIAN_POINT('Ctrl Pts',(56.6083468890952,22.1799709108016,13.6577380046858));
#25830=CARTESIAN_POINT('Ctrl Pts',(56.6137356205523,22.1725904743565,13.6571596314389));
#25831=CARTESIAN_POINT('Ctrl Pts',(56.6488984283103,22.1237297750284,13.6533704960579));
#25832=CARTESIAN_POINT('Ctrl Pts',(56.6771239571451,22.0811525585331,13.6502565086701));
#25833=CARTESIAN_POINT('Ctrl Pts',(56.7853332757802,21.903467222576,13.6378049017059));
#25834=CARTESIAN_POINT('Ctrl Pts',(56.8508732117771,21.7602254709168,13.6289568401826));
#25835=CARTESIAN_POINT('Ctrl Pts',(56.9231994099082,21.5353573016456,13.6149925111427));
#25836=CARTESIAN_POINT('Ctrl Pts',(56.9429392385478,21.4585720594319,13.61022030477));
#25837=CARTESIAN_POINT('Ctrl Pts',(56.9608513376461,21.3664740892523,13.6043896997356));
#25838=CARTESIAN_POINT('Ctrl Pts',(56.9634840924494,21.3520957643995,13.603476532278));
#25839=CARTESIAN_POINT('Ctrl Pts',(56.9675443121326,21.3284580456637,13.6019699787483));
#25840=CARTESIAN_POINT('Ctrl Pts',(56.9690650175664,21.319215068157,13.6013795478635));
#25841=CARTESIAN_POINT('Ctrl Pts',(56.9716823816857,21.3025756984959,13.6003141133066));
#25842=CARTESIAN_POINT('Ctrl Pts',(56.9728026682736,21.2951831586224,13.5998398665341));
#25843=CARTESIAN_POINT('Ctrl Pts',(56.9751022692204,21.279410459865,13.5988260305627));
#25844=CARTESIAN_POINT('Ctrl Pts',(56.976269865866,21.2710287670917,13.598286081175));
#25845=CARTESIAN_POINT('Ctrl Pts',(56.9792801976098,21.2483643520073,13.5968226960539));
#25846=CARTESIAN_POINT('Ctrl Pts',(56.9810216255651,21.2340689065069,13.5958960927018));
#25847=CARTESIAN_POINT('Ctrl Pts',(56.9892474423376,21.1598567864132,13.591066319055));
#25848=CARTESIAN_POINT('Ctrl Pts',(56.9931682239661,21.0996932028106,13.5870836882978));
#25849=CARTESIAN_POINT('Ctrl Pts',(56.9974820998487,20.8816054562162,13.572396861648));
#25850=CARTESIAN_POINT('Ctrl Pts',(56.9818532004351,20.7239594403078,13.5612518135231));
#25851=CARTESIAN_POINT('Ctrl Pts',(56.9326339654805,20.5010915443035,13.5454757457249));
#25852=CARTESIAN_POINT('Ctrl Pts',(56.9138219791016,20.4331919712266,13.5406772282269));
#25853=CARTESIAN_POINT('Ctrl Pts',(56.8882089224664,20.3567277663116,13.535383527226));
#25854=CARTESIAN_POINT('Ctrl Pts',(56.8848868385247,20.3470576456336,13.5347161465374));
#25855=CARTESIAN_POINT('Ctrl Pts',(56.8797466075484,20.3324613748682,13.53371241615));
#25856=CARTESIAN_POINT('Ctrl Pts',(56.8779831845906,20.3275163313815,13.533372997786));
#25857=CARTESIAN_POINT('Ctrl Pts',(56.8747801286319,20.318645086479,13.5327653058439));
#25858=CARTESIAN_POINT('Ctrl Pts',(56.8733476612475,20.3147164163798,13.5324966209533));
#25859=CARTESIAN_POINT('Ctrl Pts',(56.8701853895074,20.3061276206417,13.5319101815815));
#25860=CARTESIAN_POINT('Ctrl Pts',(56.8684505205586,20.3014694541491,13.5315927317315));
#25861=CARTESIAN_POINT('Ctrl Pts',(56.8634505970886,20.2881964392939,13.530689792387));
#25862=CARTESIAN_POINT('Ctrl Pts',(56.8601431977251,20.2795975232187,13.5301067580012));
#25863=CARTESIAN_POINT('Ctrl Pts',(56.8374909093142,20.2219000201297,13.5262057465217));
#25864=CARTESIAN_POINT('Ctrl Pts',(56.8162619274268,20.1735581620475,13.5229912321826));
#25865=CARTESIAN_POINT('Ctrl Pts',(56.7173495965792,19.9705993389065,13.5094966225792));
#25866=CARTESIAN_POINT('Ctrl Pts',(56.6216520662475,19.8256033890593,13.4997952314163));
#25867=CARTESIAN_POINT('Ctrl Pts',(56.4671157630676,19.6470079556063,13.485702268875));
#25868=CARTESIAN_POINT('Ctrl Pts',(56.4235500937784,19.6012433881567,13.4818672973344));
#25869=CARTESIAN_POINT('Ctrl Pts',(56.3670011222939,19.5472225626512,13.4770010929343));
#25870=CARTESIAN_POINT('Ctrl Pts',(56.3559946118949,19.5369439710868,13.4760589336283));
#25871=CARTESIAN_POINT('Ctrl Pts',(56.3384508103132,19.5209284644668,13.4745643572861));
#25872=CARTESIAN_POINT('Ctrl Pts',(56.3319904284758,19.5151078579814,13.4740154925577));
#25873=CARTESIAN_POINT('Ctrl Pts',(56.3199738578989,19.5044228177999,13.4729972276797));
#25874=CARTESIAN_POINT('Ctrl Pts',(56.3144282954451,19.4995466194561,13.4725283315439));
#25875=CARTESIAN_POINT('Ctrl Pts',(56.3020475114025,19.4887815384675,13.4714836863161));
#25876=CARTESIAN_POINT('Ctrl Pts',(56.2951991875691,19.4829080382095,13.4709073152875));
#25877=CARTESIAN_POINT('Ctrl Pts',(56.2753292331169,19.466099073045,13.469239059142));
#25878=CARTESIAN_POINT('Ctrl Pts',(56.2622075710119,19.4552836103294,13.4681423279872));
#25879=CARTESIAN_POINT('Ctrl Pts',(56.1472786880102,19.3629961990947,13.4585763892694));
#25880=CARTESIAN_POINT('Ctrl Pts',(56.0378671951796,19.2915358036076,13.4497066591063));
#25881=CARTESIAN_POINT('Ctrl Pts',(55.7913750942179,19.1630048509287,13.4303939641486));
#25882=CARTESIAN_POINT('Ctrl Pts',(55.653281178563,19.109482864558,13.4199547862178));
#25883=CARTESIAN_POINT('Ctrl Pts',(55.4969848235204,19.0681019115907,13.4092725816642));
#25884=CARTESIAN_POINT('Ctrl Pts',(55.483393327991,19.0646563468419,13.4083530199176));
#25885=CARTESIAN_POINT('Ctrl Pts',(55.4644507615683,19.0600662471987,13.4070854601013));
#25886=CARTESIAN_POINT('Ctrl Pts',(55.4591299901158,19.0588000800896,13.4067309485673));
#25887=CARTESIAN_POINT('Ctrl Pts',(55.4499590378488,19.0566575141207,13.4061226243678));
#25888=CARTESIAN_POINT('Ctrl Pts',(55.4461113729665,19.0557706419407,13.4058682239236));
#25889=CARTESIAN_POINT('Ctrl Pts',(55.4380481568352,19.0539372977985,13.405336854783));
#25890=CARTESIAN_POINT('Ctrl Pts',(55.4338321316845,19.0529930892277,13.4050600240247));
#25891=CARTESIAN_POINT('Ctrl Pts',(55.4235340745671,19.0507218768237,13.4043862224153));
#25892=CARTESIAN_POINT('Ctrl Pts',(55.4174487679122,19.0494096169434,13.4039900870259));
#25893=CARTESIAN_POINT('Ctrl Pts',(55.3955882942872,19.044802523895,13.4025739727095));
#25894=CARTESIAN_POINT('Ctrl Pts',(55.3797789792539,19.0416702945803,13.4015627920337));
#25895=CARTESIAN_POINT('Ctrl Pts',(55.3404503183141,19.0343724768612,13.3990754211655));
#25896=CARTESIAN_POINT('Ctrl Pts',(55.3168903358608,19.030436952471,13.3976101813319));
#25897=CARTESIAN_POINT('Ctrl Pts',(55.217588755629,19.015677445536,13.3915171113919));
#25898=CARTESIAN_POINT('Ctrl Pts',(55.1413225463487,19.0087916625203,13.3870371664692));
#25899=CARTESIAN_POINT('Ctrl Pts',(54.8992270124374,19.000917611299,13.3729491147946));
#25900=CARTESIAN_POINT('Ctrl Pts',(54.7336042631521,19.0161872791028,13.3634474873401));
#25901=CARTESIAN_POINT('Ctrl Pts',(54.5492380183973,19.0567105431483,13.3518073002083));
#25902=CARTESIAN_POINT('Ctrl Pts',(54.5267839703626,19.0620560385604,13.350372478579));
#25903=CARTESIAN_POINT('Ctrl Pts',(54.4955409989107,19.0700692082408,13.3483498687426));
#25904=CARTESIAN_POINT('Ctrl Pts',(54.486669523148,19.0724099082579,13.347772577724));
#25905=CARTESIAN_POINT('Ctrl Pts',(54.4704496661712,19.0768093594841,13.3467115170287));
#25906=CARTESIAN_POINT('Ctrl Pts',(54.4630963124641,19.0788492449834,13.3462283646628));
#25907=CARTESIAN_POINT('Ctrl Pts',(54.4482171297583,19.0830689593022,13.3452463529093));
#25908=CARTESIAN_POINT('Ctrl Pts',(54.4406920828997,19.0852510342944,13.3447474278921));
#25909=CARTESIAN_POINT('Ctrl Pts',(54.4221425392805,19.0907486157959,13.343511825711));
#25910=CARTESIAN_POINT('Ctrl Pts',(54.4111336269255,19.09411530295,13.3427734905921));
#25911=CARTESIAN_POINT('Ctrl Pts',(54.3707823148277,19.1068383129956,13.3400483718986));
#25912=CARTESIAN_POINT('Ctrl Pts',(54.3416298428973,19.116778125334,13.3380426185486));
#25913=CARTESIAN_POINT('Ctrl Pts',(54.2693437578541,19.1433083184868,13.3329733310149));
#25914=CARTESIAN_POINT('Ctrl Pts',(54.2265363500068,19.1607294980157,13.329884019296));
#25915=CARTESIAN_POINT('Ctrl Pts',(54.0393943892088,19.24457884342,13.3159919039293));
#25916=CARTESIAN_POINT('Ctrl Pts',(53.9026983484603,19.3266242818743,13.3047395987014));
#25917=CARTESIAN_POINT('Ctrl Pts',(53.7684112136017,19.4308153483634,13.2930527205901));
#25918=CARTESIAN_POINT('Ctrl Pts',(53.7596758235183,19.4377108609447,13.2922896292018));
#25919=CARTESIAN_POINT('Ctrl Pts',(53.7129732974139,19.475215359519,13.2881961525032));
#25920=CARTESIAN_POINT('Ctrl Pts',(53.6760771125373,19.5071386553002,13.2849126123578));
#25921=CARTESIAN_POINT('Ctrl Pts',(53.6341152775534,19.5462256329398,13.2811539025904));
#25922=CARTESIAN_POINT('Ctrl Pts',(53.627882871414,19.5521065035471,13.2805949866178));
#25923=CARTESIAN_POINT('Ctrl Pts',(53.6178261271116,19.5617192575264,13.2796923293008));
#25924=CARTESIAN_POINT('Ctrl Pts',(53.6139786255047,19.5654265929834,13.2793468038399));
#25925=CARTESIAN_POINT('Ctrl Pts',(53.6071421037555,19.5720672352561,13.2787325900828));
#25926=CARTESIAN_POINT('Ctrl Pts',(53.6041473864516,19.5749945326054,13.2784634506081));
#25927=CARTESIAN_POINT('Ctrl Pts',(53.5976693035084,19.5813667914921,13.277881081201));
#25928=CARTESIAN_POINT('Ctrl Pts',(53.5941894079656,19.5848151558281,13.277568123768));
#25929=CARTESIAN_POINT('Ctrl Pts',(53.5848808793864,19.594107557082,13.27673053662));
#25930=CARTESIAN_POINT('Ctrl Pts',(53.5790756796207,19.5999750830932,13.2762077107941));
#25931=CARTESIAN_POINT('Ctrl Pts',(53.5459595599289,19.6338649133974,13.2732212839489));
#25932=CARTESIAN_POINT('Ctrl Pts',(53.5194394031791,19.6626520747054,13.2708141453961));
#25933=CARTESIAN_POINT('Ctrl Pts',(53.4352379247601,19.7596287730261,13.2630453911727));
#25934=CARTESIAN_POINT('Ctrl Pts',(53.3812832193677,19.8309150428113,13.2578574645044));
#25935=CARTESIAN_POINT('Ctrl Pts',(53.2514589230141,20.0287462853698,13.2441260073103));
#25936=CARTESIAN_POINT('Ctrl Pts',(53.1845356700698,20.1604687335485,13.235602286656));
#25937=CARTESIAN_POINT('Ctrl Pts',(53.1243437241021,20.3206555887834,13.2250636790948));
#25938=CARTESIAN_POINT('Ctrl Pts',(53.1163631891268,20.3431076315202,13.2235840197377));
#25939=CARTESIAN_POINT('Ctrl Pts',(53.105749718957,20.3747523148721,13.221492630919));
#25940=CARTESIAN_POINT('Ctrl Pts',(53.1027775750157,20.3838296826005,13.2208920413586));
#25941=CARTESIAN_POINT('Ctrl Pts',(53.0977316217409,20.3996234632718,13.2198457581887));
#25942=CARTESIAN_POINT('Ctrl Pts',(53.0956278912612,20.4063301943173,13.2194010521076));
#25943=CARTESIAN_POINT('Ctrl Pts',(53.0913160256364,20.420335278548,13.2184714948271));
#25944=CARTESIAN_POINT('Ctrl Pts',(53.0891142070655,20.4276354422244,13.217986445817));
#25945=CARTESIAN_POINT('Ctrl Pts',(53.0840013824067,20.4449454713224,13.2168349997103));
#25946=CARTESIAN_POINT('Ctrl Pts',(53.0811269049094,20.4549658079226,13.2161674268173));
#25947=CARTESIAN_POINT('Ctrl Pts',(53.0752349704908,20.4761293919263,13.2147551392495));
#25948=CARTESIAN_POINT('Ctrl Pts',(53.0722354535064,20.4872771930133,13.2140098703492));
#25949=CARTESIAN_POINT('Ctrl Pts',(53.0599119346415,20.5347153789783,13.2108323710528));
#25950=CARTESIAN_POINT('Ctrl Pts',(53.051515171606,20.5712366130093,13.2083708237553));
#25951=CARTESIAN_POINT('Ctrl Pts',(53.0181619612568,20.7376369355591,13.1970814761549));
#25952=CARTESIAN_POINT('Ctrl Pts',(53.0051351486799,20.8695447645175,13.1878996406867));
#25953=CARTESIAN_POINT('Ctrl Pts',(53.0052507628146,21.0017444908055,13.1786788122144));
#25954=CARTESIAN_POINT('Ctrl Pts',(55.1641804122445,22.9848227319589,12.9685061347694));
#25955=CARTESIAN_POINT('Ctrl Pts',(54.8621371071006,23.010541002547,12.9877832838503));
#25956=CARTESIAN_POINT('Ctrl Pts',(53.8801469710629,22.883843418079,13.0494048645008));
#25957=CARTESIAN_POINT('Ctrl Pts',(53.0767306724305,21.9309683111089,13.1195845257793));
#25958=CARTESIAN_POINT('Ctrl Pts',(53.0033791829374,21.1357025185976,13.1704870379768));
#25959=CARTESIAN_POINT('Ctrl Pts',(53.0046129860205,21.0017710049344,13.1790451186048));
#25960=CARTESIAN_POINT('',(53.005250339812,20.9988356633973,13.0222599084274));
#25961=CARTESIAN_POINT('Ctrl Pts',(55.1644480621455,22.9879598580848,12.8106050954514));
#25962=CARTESIAN_POINT('Ctrl Pts',(55.090601741016,22.9940685751985,12.8149039292751));
#25963=CARTESIAN_POINT('Ctrl Pts',(55.0163945770778,22.9960643557173,12.819207547069));
#25964=CARTESIAN_POINT('Ctrl Pts',(54.8653052417656,22.9916821606349,12.8281542158983));
#25965=CARTESIAN_POINT('Ctrl Pts',(54.788643138605,22.9850105172829,12.8327915704553));
#25966=CARTESIAN_POINT('Ctrl Pts',(54.698187344796,22.9718386664432,12.8384728806987));
#25967=CARTESIAN_POINT('Ctrl Pts',(54.6838352499383,22.9695883932003,12.8393805159609));
#25968=CARTESIAN_POINT('Ctrl Pts',(54.6602999956822,22.9656344204189,12.8408796981102));
#25969=CARTESIAN_POINT('Ctrl Pts',(54.6511017927926,22.9640226077863,12.8414683383457));
#25970=CARTESIAN_POINT('Ctrl Pts',(54.6345643437187,22.9610048905017,12.8425317003339));
#25971=CARTESIAN_POINT('Ctrl Pts',(54.6272209950825,22.9596222111577,12.8430056762876));
#25972=CARTESIAN_POINT('Ctrl Pts',(54.6115636737461,22.9565829009106,12.844020193514));
#25973=CARTESIAN_POINT('Ctrl Pts',(54.6032521684792,22.9549144692834,12.8445611024148));
#25974=CARTESIAN_POINT('Ctrl Pts',(54.5807780843412,22.9502538494799,12.8460302401133));
#25975=CARTESIAN_POINT('Ctrl Pts',(54.5666372474109,22.947160444935,12.8469616806759));
#25976=CARTESIAN_POINT('Ctrl Pts',(54.4927395575319,22.9301499766266,12.8518672143673));
#25977=CARTESIAN_POINT('Ctrl Pts',(54.4336203302244,22.9136365419279,12.8559238019402));
#25978=CARTESIAN_POINT('Ctrl Pts',(54.2481250303717,22.852474174311,12.8690840573301));
#25979=CARTESIAN_POINT('Ctrl Pts',(54.1254507255302,22.7978132357945,12.8784709237588));
#25980=CARTESIAN_POINT('Ctrl Pts',(53.9287558225416,22.6852458593228,12.8942390354748));
#25981=CARTESIAN_POINT('Ctrl Pts',(53.8516106033083,22.6336534551344,12.9006271974587));
#25982=CARTESIAN_POINT('Ctrl Pts',(53.7700805012206,22.5704885809255,12.9074001721675));
#25983=CARTESIAN_POINT('Ctrl Pts',(53.7618851245166,22.564035780502,12.9080811877692));
#25984=CARTESIAN_POINT('Ctrl Pts',(53.7496077151996,22.5542119264665,12.9091012338966));
#25985=CARTESIAN_POINT('Ctrl Pts',(53.7454880200296,22.5508885427193,12.9094434808455));
#25986=CARTESIAN_POINT('Ctrl Pts',(53.7381363042508,22.5449094062738,12.9100541008262));
#25987=CARTESIAN_POINT('Ctrl Pts',(53.7348993744885,22.5422598576809,12.9103229040934));
#25988=CARTESIAN_POINT('Ctrl Pts',(53.7316519924108,22.5395846500704,12.9105925215664));
#25989=CARTESIAN_POINT('Ctrl Pts',(53.7316332785217,22.5395692329136,12.910594075306));
#25990=CARTESIAN_POINT('Ctrl Pts',(53.7315960294229,22.5395385446623,12.9105971679473));
#25991=CARTESIAN_POINT('Ctrl Pts',(53.7315774941997,22.5395232735675,12.9105987068499));
#25992=CARTESIAN_POINT('Ctrl Pts',(53.7315405989734,22.5394928746224,12.9106017701045));
#25993=CARTESIAN_POINT('Ctrl Pts',(53.7315222390771,22.5394777468706,12.9106032944475));
#25994=CARTESIAN_POINT('Ctrl Pts',(53.7314856927541,22.5394476332009,12.9106063287281));
#25995=CARTESIAN_POINT('Ctrl Pts',(53.731467505689,22.5394326467672,12.9106078387187));
#25996=CARTESIAN_POINT('Ctrl Pts',(53.7314313011027,22.5394028125293,12.9106108446205));
#25997=CARTESIAN_POINT('Ctrl Pts',(53.7314132836658,22.5393879648047,12.9106123405248));
#25998=CARTESIAN_POINT('Ctrl Pts',(53.7313774155591,22.5393584057268,12.9106153184846));
#25999=CARTESIAN_POINT('Ctrl Pts',(53.7313595648514,22.5393436943519,12.9106168005433));
#26000=CARTESIAN_POINT('Ctrl Pts',(53.7313240278797,22.539314406088,12.9106197510049));
#26001=CARTESIAN_POINT('Ctrl Pts',(53.7313063413379,22.5392998289793,12.910621219431));
#26002=CARTESIAN_POINT('Ctrl Pts',(53.7312711294452,22.5392708065953,12.9106241428974));
#26003=CARTESIAN_POINT('Ctrl Pts',(53.7312536042865,22.5392563614875,12.9106255979219));
#26004=CARTESIAN_POINT('Ctrl Pts',(53.7274443994663,22.5361165160902,12.9109418564666));
#26005=CARTESIAN_POINT('Ctrl Pts',(53.7236642322047,22.5329770763307,12.911255641436));
#26006=CARTESIAN_POINT('Ctrl Pts',(53.7131144443147,22.5241493730663,12.9121313096567));
#26007=CARTESIAN_POINT('Ctrl Pts',(53.7063708873993,22.5184299360731,12.9126909887021));
#26008=CARTESIAN_POINT('Ctrl Pts',(53.6910832320592,22.5052881914442,12.9139602410067));
#26009=CARTESIAN_POINT('Ctrl Pts',(53.6825637472879,22.497837567254,12.91466790002));
#26010=CARTESIAN_POINT('Ctrl Pts',(53.6554994430845,22.4737591978603,12.9169187743747));
#26011=CARTESIAN_POINT('Ctrl Pts',(53.6372017879249,22.4568558853423,12.9184448473533));
#26012=CARTESIAN_POINT('Ctrl Pts',(53.5599272144776,22.3827395887461,12.9249333092508));
#26013=CARTESIAN_POINT('Ctrl Pts',(53.5041954484117,22.3222515925881,12.9297273084609));
#26014=CARTESIAN_POINT('Ctrl Pts',(53.3531267341063,22.1364728151092,12.943635928764));
#26015=CARTESIAN_POINT('Ctrl Pts',(53.2686933083185,22.0031614696136,12.9526911323066));
#26016=CARTESIAN_POINT('Ctrl Pts',(53.1907305006437,21.8403061687681,12.9638167272644));
#26017=CARTESIAN_POINT('Ctrl Pts',(53.1810379143992,21.8191138132981,12.9652643729206));
#26018=CARTESIAN_POINT('Ctrl Pts',(53.1679354725549,21.7890859497488,12.9673175922319));
#26019=CARTESIAN_POINT('Ctrl Pts',(53.164213629488,21.7803880225348,12.9679125623885));
#26020=CARTESIAN_POINT('Ctrl Pts',(53.1578440262373,21.7652045474106,12.96895171878));
#26021=CARTESIAN_POINT('Ctrl Pts',(53.1551682731058,21.7587308669457,12.9693949500095));
#26022=CARTESIAN_POINT('Ctrl Pts',(53.1496454496203,21.7451670784589,12.9703240432325));
#26023=CARTESIAN_POINT('Ctrl Pts',(53.1468049104564,21.7380744504134,12.970810116477));
#26024=CARTESIAN_POINT('Ctrl Pts',(53.140149954041,21.7211768540245,12.9719688056827));
#26025=CARTESIAN_POINT('Ctrl Pts',(53.1363722537278,21.7113577612832,12.9726426391501));
#26026=CARTESIAN_POINT('Ctrl Pts',(53.1238815080677,21.6781090073821,12.9749263716007));
#26027=CARTESIAN_POINT('Ctrl Pts',(53.1155315404224,21.6545463714167,12.9765482428566));
#26028=CARTESIAN_POINT('Ctrl Pts',(53.09661454438,21.5977992390173,12.9804641541126));
#26029=CARTESIAN_POINT('Ctrl Pts',(53.086469734562,21.5644836598201,12.9827711773309));
#26030=CARTESIAN_POINT('Ctrl Pts',(53.0293411308842,21.3575853021602,12.9971487807717));
#26031=CARTESIAN_POINT('Ctrl Pts',(53.0051454168276,21.1785904584044,13.0099083080189));
#26032=CARTESIAN_POINT('Ctrl Pts',(53.005250339812,20.9988356633973,13.0222599084274));
#26033=CARTESIAN_POINT('Ctrl Pts',(53.005250341493,20.9988327870284,13.022260106073));
#26034=CARTESIAN_POINT('Ctrl Pts',(53.0052832483541,20.9425954493867,13.0261243745321));
#26035=CARTESIAN_POINT('Ctrl Pts',(53.0076943804446,20.886377919827,13.0299328038307));
#26036=CARTESIAN_POINT('Ctrl Pts',(53.0131339377996,20.8226581779702,13.0341353458906));
#26037=CARTESIAN_POINT('Ctrl Pts',(53.0138334265883,20.814988600084,13.0346392835011));
#26038=CARTESIAN_POINT('Ctrl Pts',(53.0150629882058,20.8023186858579,13.0354684241452));
#26039=CARTESIAN_POINT('Ctrl Pts',(53.0155675734077,20.7973160382515,13.0357949417051));
#26040=CARTESIAN_POINT('Ctrl Pts',(53.0165080685925,20.7883319547842,13.0363797059881));
#26041=CARTESIAN_POINT('Ctrl Pts',(53.0169370624376,20.7843498442502,13.0366383258122));
#26042=CARTESIAN_POINT('Ctrl Pts',(53.0177928782713,20.7766243440384,13.0371389169336));
#26043=CARTESIAN_POINT('Ctrl Pts',(53.0182183117154,20.7728808731764,13.0373809574812));
#26044=CARTESIAN_POINT('Ctrl Pts',(53.0192248823116,20.7642420810879,13.0379382983765));
#26045=CARTESIAN_POINT('Ctrl Pts',(53.0198135602627,20.7593477024161,13.0382531712955));
#26046=CARTESIAN_POINT('Ctrl Pts',(53.0215009771349,20.7457437489847,13.039126003131));
#26047=CARTESIAN_POINT('Ctrl Pts',(53.0226390905044,20.7370390428146,13.0396818069246));
#26048=CARTESIAN_POINT('Ctrl Pts',(53.0290947901409,20.6900773215935,13.0426671880341));
#26049=CARTESIAN_POINT('Ctrl Pts',(53.0354656066091,20.6519705646401,13.0450424377492));
#26050=CARTESIAN_POINT('Ctrl Pts',(53.0495626594614,20.5804840546944,13.0494494397717));
#26051=CARTESIAN_POINT('Ctrl Pts',(53.0570495575807,20.547072597816,13.0514887575308));
#26052=CARTESIAN_POINT('Ctrl Pts',(53.1067224903387,20.3493941805232,13.0635180167238));
#26053=CARTESIAN_POINT('Ctrl Pts',(53.168855121851,20.1908656192521,13.0730791772929));
#26054=CARTESIAN_POINT('Ctrl Pts',(53.2661973624452,20.0130590307908,13.0852919090766));
#26055=CARTESIAN_POINT('Ctrl Pts',(53.282818787009,19.9844151609859,13.0873072953921));
#26056=CARTESIAN_POINT('Ctrl Pts',(53.3127276386172,19.9357078542538,13.0908283502564));
#26057=CARTESIAN_POINT('Ctrl Pts',(53.3256795619821,19.9154462732187,13.0923221873717));
#26058=CARTESIAN_POINT('Ctrl Pts',(53.3447307802516,19.8867979982509,13.0944789539835));
#26059=CARTESIAN_POINT('Ctrl Pts',(53.3505344182689,19.8782165205656,13.095130854771));
#26060=CARTESIAN_POINT('Ctrl Pts',(53.360717896488,19.8634087406332,13.096266138423));
#26061=CARTESIAN_POINT('Ctrl Pts',(53.365067057254,19.8571615267812,13.0967483525425));
#26062=CARTESIAN_POINT('Ctrl Pts',(53.3735078478127,19.8451838155702,13.0976792571661));
#26063=CARTESIAN_POINT('Ctrl Pts',(53.3775942783783,19.8394497799298,13.0981277437932));
#26064=CARTESIAN_POINT('Ctrl Pts',(53.3873269454354,19.8259448704966,13.0991908299515));
#26065=CARTESIAN_POINT('Ctrl Pts',(53.3929990821886,19.8181929629423,13.099806423757));
#26066=CARTESIAN_POINT('Ctrl Pts',(53.4131327453762,19.7910899641035,13.1019779293358));
#26067=CARTESIAN_POINT('Ctrl Pts',(53.4278891263184,19.7719615337871,13.1035452859635));
#26068=CARTESIAN_POINT('Ctrl Pts',(53.5223694695506,19.6539827676595,13.1134368684278));
#26069=CARTESIAN_POINT('Ctrl Pts',(53.6110207396983,19.5626827732422,13.122125740282));
#26070=CARTESIAN_POINT('Ctrl Pts',(53.7878355780693,19.4123152725683,13.1382779259167));
#26071=CARTESIAN_POINT('Ctrl Pts',(53.873205136614,19.3506303448776,13.1456630274263));
#26072=CARTESIAN_POINT('Ctrl Pts',(53.9874312587432,19.2811203656088,13.1547582378884));
#26073=CARTESIAN_POINT('Ctrl Pts',(54.0121373886634,19.2668034484959,13.1566814138544));
#26074=CARTESIAN_POINT('Ctrl Pts',(54.048052790003,19.247008489948,13.1594059694709));
#26075=CARTESIAN_POINT('Ctrl Pts',(54.0590183732447,19.2410979786583,13.160228498306));
#26076=CARTESIAN_POINT('Ctrl Pts',(54.0785703756557,19.2307945261308,13.1616776950129));
#26077=CARTESIAN_POINT('Ctrl Pts',(54.0871345399095,19.2263604587876,13.1623066232983));
#26078=CARTESIAN_POINT('Ctrl Pts',(54.1002229380178,19.2197039007833,13.1632585446028));
#26079=CARTESIAN_POINT('Ctrl Pts',(54.1047238499272,19.2174362343456,13.1635842429479));
#26080=CARTESIAN_POINT('Ctrl Pts',(54.1092450032001,19.215179813442,13.1639097148136));
#26081=CARTESIAN_POINT('Ctrl Pts',(54.1092566390746,19.2151740063422,13.1639105524537));
#26082=CARTESIAN_POINT('Ctrl Pts',(54.1092799495246,19.2151623731131,13.1639122304973));
#26083=CARTESIAN_POINT('Ctrl Pts',(54.1092916235084,19.2151565472799,13.1639130708582));
#26084=CARTESIAN_POINT('Ctrl Pts',(54.1093150101449,19.2151448766025,13.1639147543411));
#26085=CARTESIAN_POINT('Ctrl Pts',(54.1093267230482,19.2151390316343,13.163915597481));
#26086=CARTESIAN_POINT('Ctrl Pts',(54.1093501874704,19.2151273227164,13.1639172865178));
#26087=CARTESIAN_POINT('Ctrl Pts',(54.1093619392379,19.2151214586436,13.1639181324324));
#26088=CARTESIAN_POINT('Ctrl Pts',(54.1093854819581,19.2151097112353,13.1639198270595));
#26089=CARTESIAN_POINT('Ctrl Pts',(54.109397272649,19.2151038280313,13.1639206757529));
#26090=CARTESIAN_POINT('Ctrl Pts',(54.1094208933249,19.215092042309,13.1639223759452));
#26091=CARTESIAN_POINT('Ctrl Pts',(54.1094327234841,19.2150861397048,13.1639232274564));
#26092=CARTESIAN_POINT('Ctrl Pts',(54.109456423472,19.2150743149978,13.1639249333111));
#26093=CARTESIAN_POINT('Ctrl Pts',(54.1094682930403,19.2150683930258,13.1639257876356));
#26094=CARTESIAN_POINT('Ctrl Pts',(54.1094920720285,19.2150565294954,13.1639274991297));
#26095=CARTESIAN_POINT('Ctrl Pts',(54.1095039814809,19.2150505879217,13.1639283563015));
#26096=CARTESIAN_POINT('Ctrl Pts',(54.1095278401604,19.215038685229,13.1639300734843));
#26097=CARTESIAN_POINT('Ctrl Pts',(54.1095397897401,19.2150327239352,13.1639309335206));
#26098=CARTESIAN_POINT('Ctrl Pts',(54.1095637293307,19.2150207814778,13.1639326564794));
#26099=CARTESIAN_POINT('Ctrl Pts',(54.1095757189013,19.2150148005349,13.1639335193702));
#26100=CARTESIAN_POINT('Ctrl Pts',(54.109599738599,19.21500281872,13.1639352480467));
#26101=CARTESIAN_POINT('Ctrl Pts',(54.1096117688505,19.2149968177868,13.1639361138414));
#26102=CARTESIAN_POINT('Ctrl Pts',(54.1096358701259,19.2149847958867,13.163937848341));
#26103=CARTESIAN_POINT('Ctrl Pts',(54.1096479410245,19.2149787749833,13.1639387170368));
#26104=CARTESIAN_POINT('Ctrl Pts',(54.1096721235327,19.2149667131764,13.1639404573342));
#26105=CARTESIAN_POINT('Ctrl Pts',(54.1096842355944,19.2149606720484,13.1639413289681));
#26106=CARTESIAN_POINT('Ctrl Pts',(54.1097085013314,19.2149485693452,13.1639430752063));
#26107=CARTESIAN_POINT('Ctrl Pts',(54.1097206541766,19.214942508185,13.1639439497508));
#26108=CARTESIAN_POINT('Ctrl Pts',(54.1097450011706,19.2149303655754,13.1639457017875));
#26109=CARTESIAN_POINT('Ctrl Pts',(54.1097571959602,19.2149242838073,13.1639465793258));
#26110=CARTESIAN_POINT('Ctrl Pts',(54.1097816271545,19.2149120998295,13.1639483373723));
#26111=CARTESIAN_POINT('Ctrl Pts',(54.1097938633632,19.2149059977185,13.1639492178664));
#26112=CARTESIAN_POINT('Ctrl Pts',(54.1098183779925,19.2148937727608,13.1639509818671));
#26113=CARTESIAN_POINT('Ctrl Pts',(54.1098306561082,19.214887650067,13.1639518653518));
#26114=CARTESIAN_POINT('Ctrl Pts',(54.1098552540844,19.2148753841795,13.1639536352999));
#26115=CARTESIAN_POINT('Ctrl Pts',(54.1098675747664,19.2148692405772,13.1639545218223));
#26116=CARTESIAN_POINT('Ctrl Pts',(54.1098922585294,19.2148569325499,13.1639562978928));
#26117=CARTESIAN_POINT('Ctrl Pts',(54.1099046212595,19.214850768301,13.1639571874156));
#26118=CARTESIAN_POINT('Ctrl Pts',(54.1099293896163,19.2148384187353,13.1639589695221));
#26119=CARTESIAN_POINT('Ctrl Pts',(54.1099417951073,19.2148322334875,13.1639598620961));
#26120=CARTESIAN_POINT('Ctrl Pts',(54.1099666493497,19.214819841746,13.1639616503311));
#26121=CARTESIAN_POINT('Ctrl Pts',(54.1099790976895,19.2148136354588,13.1639625459625));
#26122=CARTESIAN_POINT('Ctrl Pts',(54.1100040372026,19.2148012018548,13.1639643402812));
#26123=CARTESIAN_POINT('Ctrl Pts',(54.110016529122,19.2147949741672,13.1639652390222));
#26124=CARTESIAN_POINT('Ctrl Pts',(54.1100416959498,19.2147824278949,13.1639670496434));
#26125=CARTESIAN_POINT('Ctrl Pts',(54.1100543702003,19.2147761096431,13.1639679614759));
#26126=CARTESIAN_POINT('Ctrl Pts',(54.1100799207794,19.214763372741,13.1639697996523));
#26127=CARTESIAN_POINT('Ctrl Pts',(54.1100927975956,19.2147569538531,13.1639707260309));
#26128=CARTESIAN_POINT('Ctrl Pts',(54.1101187570107,19.2147440138486,13.1639725935647));
#26129=CARTESIAN_POINT('Ctrl Pts',(54.1101318392338,19.2147374929248,13.1639735346924));
#26130=CARTESIAN_POINT('Ctrl Pts',(54.1101582133024,19.2147243469516,13.1639754319994));
#26131=CARTESIAN_POINT('Ctrl Pts',(54.1101715048128,19.2147177220749,13.1639763881542));
#26132=CARTESIAN_POINT('Ctrl Pts',(54.1101983004707,19.2147043667105,13.1639783157306));
#26133=CARTESIAN_POINT('Ctrl Pts',(54.1102118052133,19.2146976359322,13.1639792871947));
#26134=CARTESIAN_POINT('Ctrl Pts',(54.1102390312302,19.2146840668417,13.1639812456685));
#26135=CARTESIAN_POINT('Ctrl Pts',(54.1102527523704,19.2146772286024,13.1639822326682));
#26136=CARTESIAN_POINT('Ctrl Pts',(54.1102804149144,19.2146634427487,13.1639842224803));
#26137=CARTESIAN_POINT('Ctrl Pts',(54.1102943566378,19.2146564949814,13.1639852253152));
#26138=CARTESIAN_POINT('Ctrl Pts',(54.1140503420512,19.2127847789558,13.1642553908185));
#26139=CARTESIAN_POINT('Ctrl Pts',(54.1177981900082,19.2109318040402,13.1645238039627));
#26140=CARTESIAN_POINT('Ctrl Pts',(54.1262722930752,19.2067752234782,13.1651280909973));
#26141=CARTESIAN_POINT('Ctrl Pts',(54.1310018377536,19.2044785157176,13.1654635361336));
#26142=CARTESIAN_POINT('Ctrl Pts',(54.1449914117077,19.1977532815708,13.166450557768));
#26143=CARTESIAN_POINT('Ctrl Pts',(54.154276771849,19.1933774184629,13.167098983782));
#26144=CARTESIAN_POINT('Ctrl Pts',(54.263067348875,19.1431308214525,13.1746230639566));
#26145=CARTESIAN_POINT('Ctrl Pts',(54.3661707748302,19.1054550760183,13.1810481740207));
#26146=CARTESIAN_POINT('Ctrl Pts',(54.5519249078212,19.0544538498031,13.1922498803867));
#26147=CARTESIAN_POINT('Ctrl Pts',(54.6332832254596,19.0374914989848,13.1970369974516));
#26148=CARTESIAN_POINT('Ctrl Pts',(54.8072545128356,19.0124190516006,13.207366522913));
#26149=CARTESIAN_POINT('Ctrl Pts',(54.8998488882186,19.0056090324894,13.2129210942788));
#26150=CARTESIAN_POINT('Ctrl Pts',(55.0086644953452,19.0052039187941,13.219684646704));
#26151=CARTESIAN_POINT('Ctrl Pts',(55.0247550198719,19.0053387144123,13.2206905906412));
#26152=CARTESIAN_POINT('Ctrl Pts',(55.0496673900674,19.005848893205,13.2222577949478));
#26153=CARTESIAN_POINT('Ctrl Pts',(55.0584915752964,19.006088212097,13.2228148043749));
#26154=CARTESIAN_POINT('Ctrl Pts',(55.0740228197196,19.0066126198482,13.2237986305679));
#26155=CARTESIAN_POINT('Ctrl Pts',(55.0807306168594,19.0068730118513,13.2242246681378));
#26156=CARTESIAN_POINT('Ctrl Pts',(55.096038938696,19.007544674986,13.2251996019708));
#26157=CARTESIAN_POINT('Ctrl Pts',(55.1046383246279,19.0079777819749,13.2257491736448));
#26158=CARTESIAN_POINT('Ctrl Pts',(55.1279035185684,19.0093005934133,13.227241303376));
#26159=CARTESIAN_POINT('Ctrl Pts',(55.1425625105737,19.0102966681302,13.2281871676294));
#26160=CARTESIAN_POINT('Ctrl Pts',(55.2152295265051,19.0160415192611,13.2329052064708));
#26161=CARTESIAN_POINT('Ctrl Pts',(55.2730161530937,19.023165147672,13.2367508705642));
#26162=CARTESIAN_POINT('Ctrl Pts',(55.4906129060613,19.0597120256788,13.2515965390692));
#26163=CARTESIAN_POINT('Ctrl Pts',(55.6469242984393,19.1060900625544,13.2630786513237));
#26164=CARTESIAN_POINT('Ctrl Pts',(55.8382349054426,19.1893299055669,13.2774802506528));
#26165=CARTESIAN_POINT('Ctrl Pts',(55.8799670652333,19.2092396918734,13.2806395635415));
#26166=CARTESIAN_POINT('Ctrl Pts',(55.9363493045465,19.2385863482564,13.2848993423019));
#26167=CARTESIAN_POINT('Ctrl Pts',(55.9516218893416,19.2467904013168,13.2860522784054));
#26168=CARTESIAN_POINT('Ctrl Pts',(55.9778189193548,19.2613060024839,13.2880258522527));
#26169=CARTESIAN_POINT('Ctrl Pts',(55.9887938198554,19.2675238941072,13.2888514023551));
#26170=CARTESIAN_POINT('Ctrl Pts',(56.0045909633503,19.2766728742632,13.2900370588755));
#26171=CARTESIAN_POINT('Ctrl Pts',(56.0094606496076,19.2795208270001,13.2904021880637));
#26172=CARTESIAN_POINT('Ctrl Pts',(56.0179516095673,19.2845350810716,13.2910381109667));
#26173=CARTESIAN_POINT('Ctrl Pts',(56.0215781800895,19.2866922661739,13.2913094830586));
#26174=CARTESIAN_POINT('Ctrl Pts',(56.0292415573486,19.2912836400187,13.2918823961385));
#26175=CARTESIAN_POINT('Ctrl Pts',(56.0332765905225,19.2937206351729,13.292183751429));
#26176=CARTESIAN_POINT('Ctrl Pts',(56.0441687524262,19.3003518630932,13.292996514063));
#26177=CARTESIAN_POINT('Ctrl Pts',(56.0510093183234,19.3045733307325,13.2935061799832));
#26178=CARTESIAN_POINT('Ctrl Pts',(56.0822056767484,19.3240866770757,13.295827864345));
#26179=CARTESIAN_POINT('Ctrl Pts',(56.1062558862837,19.3398636476524,13.2976103086756));
#26180=CARTESIAN_POINT('Ctrl Pts',(56.1697479361262,19.3835072968306,13.3023196929081));
#26181=CARTESIAN_POINT('Ctrl Pts',(56.208534479318,19.4122960216605,13.3052007942238));
#26182=CARTESIAN_POINT('Ctrl Pts',(56.3193986718867,19.5010025360307,13.3135683086431));
#26183=CARTESIAN_POINT('Ctrl Pts',(56.3883436705159,19.5646223057637,13.3189509452437));
#26184=CARTESIAN_POINT('Ctrl Pts',(56.5330695691188,19.71839045646,13.3312541330218));
#26185=CARTESIAN_POINT('Ctrl Pts',(56.6058524116594,19.8108583526604,13.3382029864829));
#26186=CARTESIAN_POINT('Ctrl Pts',(56.6792525413191,19.9232362432246,13.3465386255131));
#26187=CARTESIAN_POINT('Ctrl Pts',(56.6882531349711,19.9374038346139,13.3475872789823));
#26188=CARTESIAN_POINT('Ctrl Pts',(56.7017900608253,19.9593181602232,13.3492067612603));
#26189=CARTESIAN_POINT('Ctrl Pts',(56.7064548180056,19.9669849697998,13.3497728669576));
#26190=CARTESIAN_POINT('Ctrl Pts',(56.7148613019076,19.981013861301,13.350808002227));
#26191=CARTESIAN_POINT('Ctrl Pts',(56.7186197754489,19.9873657616486,13.3512764107289));
#26192=CARTESIAN_POINT('Ctrl Pts',(56.7267479490431,20.0012781483663,13.3523018347732));
#26193=CARTESIAN_POINT('Ctrl Pts',(56.7311034107354,20.0088467354677,13.3528593530363));
#26194=CARTESIAN_POINT('Ctrl Pts',(56.7429169693733,20.0296908429339,13.3543940075389));
#26195=CARTESIAN_POINT('Ctrl Pts',(56.7502728491137,20.0430233259223,13.3553747734436));
#26196=CARTESIAN_POINT('Ctrl Pts',(56.7885183637418,20.1142593160344,13.3606117043748));
#26197=CARTESIAN_POINT('Ctrl Pts',(56.8166858774398,20.1735707601373,13.3649623631607));
#26198=CARTESIAN_POINT('Ctrl Pts',(56.9073418831237,20.3916014067321,13.3809261323497));
#26199=CARTESIAN_POINT('Ctrl Pts',(56.9523400268486,20.5567635717114,13.3930374396775));
#26200=CARTESIAN_POINT('Ctrl Pts',(56.983013953433,20.7776446074142,13.4083065002408));
#26201=CARTESIAN_POINT('Ctrl Pts',(56.9881817291651,20.8299390005005,13.4118483705794));
#26202=CARTESIAN_POINT('Ctrl Pts',(56.9918218090702,20.8915652872133,13.4158922598772));
#26203=CARTESIAN_POINT('Ctrl Pts',(56.9923007584585,20.9007533289248,13.4164917781646));
#26204=CARTESIAN_POINT('Ctrl Pts',(56.9929403771028,20.9149065935751,13.4174097114755));
#26205=CARTESIAN_POINT('Ctrl Pts',(56.9931460909666,20.9198695072251,13.4177305364264));
#26206=CARTESIAN_POINT('Ctrl Pts',(56.9934908010687,20.9290108054948,13.4183194679463));
#26207=CARTESIAN_POINT('Ctrl Pts',(56.9936351996028,20.9331888393247,13.4185878623057));
#26208=CARTESIAN_POINT('Ctrl Pts',(56.9939313351666,20.9426156452687,13.4191917011256));
#26209=CARTESIAN_POINT('Ctrl Pts',(56.9940754830542,20.9478645712495,13.4195267197051));
#26210=CARTESIAN_POINT('Ctrl Pts',(56.9944394192318,20.963343868403,13.4205113140172));
#26211=CARTESIAN_POINT('Ctrl Pts',(56.994601221146,20.9735756156382,13.4211577623104));
#26212=CARTESIAN_POINT('Ctrl Pts',(56.9952581150675,21.0545000958836,13.4262393051825));
#26213=CARTESIAN_POINT('Ctrl Pts',(56.9920736128489,21.1251808464537,13.4304893071425));
#26214=CARTESIAN_POINT('Ctrl Pts',(56.9696684273553,21.3526281485193,13.4439755165884));
#26215=CARTESIAN_POINT('Ctrl Pts',(56.9356078270219,21.5073113846432,13.4528976476747));
#26216=CARTESIAN_POINT('Ctrl Pts',(56.8639215187066,21.7130399933706,13.4659330209543));
#26217=CARTESIAN_POINT('Ctrl Pts',(56.8416275793222,21.7687888285813,13.4695860806875));
#26218=CARTESIAN_POINT('Ctrl Pts',(56.8109200389748,21.8365422702239,13.4742200466229));
#26219=CARTESIAN_POINT('Ctrl Pts',(56.8048424048327,21.8495753256964,13.4751205423652));
#26220=CARTESIAN_POINT('Ctrl Pts',(56.794967852447,21.8701663543857,13.4765582917405));
#26221=CARTESIAN_POINT('Ctrl Pts',(56.7912627897613,21.8777680160913,13.4770923638655));
#26222=CARTESIAN_POINT('Ctrl Pts',(56.7841917587462,21.8920443988625,13.478101714479));
#26223=CARTESIAN_POINT('Ctrl Pts',(56.7808363789624,21.8987242237698,13.4785766169138));
#26224=CARTESIAN_POINT('Ctrl Pts',(56.7731907237404,21.9137341050365,13.4796497759987));
#26225=CARTESIAN_POINT('Ctrl Pts',(56.7688791648874,21.9220530638426,13.4802487726748));
#26226=CARTESIAN_POINT('Ctrl Pts',(56.7576855390496,21.9432831840286,13.4817884164241));
#26227=CARTESIAN_POINT('Ctrl Pts',(56.7507198385662,21.9561493854894,13.4827320022363));
#26228=CARTESIAN_POINT('Ctrl Pts',(56.7049303252074,22.0385481025204,13.4888442212116));
#26229=CARTESIAN_POINT('Ctrl Pts',(56.6621184314045,22.1057707903553,13.4941553937547));
#26230=CARTESIAN_POINT('Ctrl Pts',(56.5235323631449,22.2970747430652,13.5102563425561));
#26231=CARTESIAN_POINT('Ctrl Pts',(56.4170510976158,22.4126264327628,13.5213656216321));
#26232=CARTESIAN_POINT('Ctrl Pts',(56.2594299682373,22.5477292524502,13.5355667301343));
#26233=CARTESIAN_POINT('Ctrl Pts',(56.2194363826203,22.5794320450986,13.5390035230186));
#26234=CARTESIAN_POINT('Ctrl Pts',(56.1708974109203,22.6149644716734,13.5429434687467));
#26235=CARTESIAN_POINT('Ctrl Pts',(56.1634900548479,22.6203091963027,13.5435386128046));
#26236=CARTESIAN_POINT('Ctrl Pts',(56.1520097383602,22.6284734129521,13.5444512824076));
#26237=CARTESIAN_POINT('Ctrl Pts',(56.1479626676961,22.6313288475467,13.5447711757342));
#26238=CARTESIAN_POINT('Ctrl Pts',(56.140479278764,22.636567157975,13.5453592324038));
#26239=CARTESIAN_POINT('Ctrl Pts',(56.1370461214531,22.6389542904317,13.54562767717));
#26240=CARTESIAN_POINT('Ctrl Pts',(56.1292704196938,22.6443246752342,13.5462326762208));
#26241=CARTESIAN_POINT('Ctrl Pts',(56.1249235552974,22.6473015251171,13.5465687972025));
#26242=CARTESIAN_POINT('Ctrl Pts',(56.112031417964,22.6560555797976,13.5475596704936));
#26243=CARTESIAN_POINT('Ctrl Pts',(56.1034529160478,22.6617838700465,13.5482112355812));
#26244=CARTESIAN_POINT('Ctrl Pts',(56.0301246618068,22.7099305611676,13.5537185541613));
#26245=CARTESIAN_POINT('Ctrl Pts',(55.9629927620481,22.7486186594499,13.5583517761349));
#26246=CARTESIAN_POINT('Ctrl Pts',(55.7723940951098,22.844144479652,13.5708872392046));
#26247=CARTESIAN_POINT('Ctrl Pts',(55.6451218917195,22.892427085968,13.5786099493198));
#26248=CARTESIAN_POINT('Ctrl Pts',(55.4669421871161,22.939937473651,13.5895516940523));
#26249=CARTESIAN_POINT('Ctrl Pts',(55.4195145791887,22.9507433009584,13.5924729413793));
#26250=CARTESIAN_POINT('Ctrl Pts',(55.3505204937149,22.9638303124372,13.5967656717079));
#26251=CARTESIAN_POINT('Ctrl Pts',(55.3292357823367,22.9675105738819,13.5980957392484));
#26252=CARTESIAN_POINT('Ctrl Pts',(55.2909138089191,22.9734974424378,13.6005032883256));
#26253=CARTESIAN_POINT('Ctrl Pts',(55.273898367483,22.9759308325099,13.6015767797631));
#26254=CARTESIAN_POINT('Ctrl Pts',(55.2478705667101,22.9793104373928,13.6032266120576));
#26255=CARTESIAN_POINT('Ctrl Pts',(55.2388794025959,22.9804156765837,13.6037979447293));
#26256=CARTESIAN_POINT('Ctrl Pts',(55.2224768187164,22.9823186397565,13.6048429208506));
#26257=CARTESIAN_POINT('Ctrl Pts',(55.2150678240449,22.9831361408097,13.6053159328538));
#26258=CARTESIAN_POINT('Ctrl Pts',(55.1990150365473,22.9848163733298,13.6063430302337));
#26259=CARTESIAN_POINT('Ctrl Pts',(55.1903698705967,22.9856642034945,13.6068975739475));
#26260=CARTESIAN_POINT('Ctrl Pts',(55.1759645977854,22.986981987716,13.6078240185887));
#26261=CARTESIAN_POINT('Ctrl Pts',(55.1702074762722,22.9874834268497,13.6081949181193));
#26262=CARTESIAN_POINT('Ctrl Pts',(55.1644483515698,22.987959834143,13.6085666014869));
#26263=CARTESIAN_POINT('Origin',(55.,21.,6.22095488139522));
#26264=CARTESIAN_POINT('',(55.1644484406754,22.987959826772,14.5675833348156));
#26265=CARTESIAN_POINT('',(55.1644483421761,22.9879598349201,14.4110001919405));
#26266=CARTESIAN_POINT('',(55.1644483516311,22.987959834138,6.22095488139522));
#26267=CARTESIAN_POINT('Ctrl Pts',(55.1644484406754,22.987959826772,14.5675833348156));
#26268=CARTESIAN_POINT('Ctrl Pts',(55.2293615346116,22.9825900718436,14.5630733720583));
#26269=CARTESIAN_POINT('Ctrl Pts',(55.2939982819238,22.9740420031108,14.5586139385604));
#26270=CARTESIAN_POINT('Ctrl Pts',(55.3751010560904,22.9592408043298,14.5531448422678));
#26271=CARTESIAN_POINT('Ctrl Pts',(55.3920364515031,22.9559224935625,14.552009956185));
#26272=CARTESIAN_POINT('Ctrl Pts',(55.4151860566451,22.9510738046064,14.5504703915496));
#26273=CARTESIAN_POINT('Ctrl Pts',(55.4214385526315,22.9497328026498,14.5500557501661));
#26274=CARTESIAN_POINT('Ctrl Pts',(55.43193773831,22.9474281279609,14.5493615957564));
#26275=CARTESIAN_POINT('Ctrl Pts',(55.4361878758565,22.946480583372,14.5490811806471));
#26276=CARTESIAN_POINT('Ctrl Pts',(55.4442538435536,22.9446545750929,14.5485501571781));
#26277=CARTESIAN_POINT('Ctrl Pts',(55.4480702321122,22.9437787841427,14.5482993939904));
#26278=CARTESIAN_POINT('Ctrl Pts',(55.4580825811185,22.9414500795779,14.5476427384746));
#26279=CARTESIAN_POINT('Ctrl Pts',(55.4642742718268,22.9399787281806,14.5472378927992));
#26280=CARTESIAN_POINT('Ctrl Pts',(55.4858401365881,22.9347447999691,14.5458317697475));
#26281=CARTESIAN_POINT('Ctrl Pts',(55.5011769514433,22.9308287805037,14.5448388348704));
#26282=CARTESIAN_POINT('Ctrl Pts',(55.6310014348631,22.8960289245606,14.5364810806502));
#26283=CARTESIAN_POINT('Ctrl Pts',(55.742587527945,22.8551711386366,14.5296025934339));
#26284=CARTESIAN_POINT('Ctrl Pts',(55.9875662338876,22.7397982313336,14.513890277932));
#26285=CARTESIAN_POINT('Ctrl Pts',(56.1173483031017,22.6594307872944,14.5050753123241));
#26286=CARTESIAN_POINT('Ctrl Pts',(56.2523901496823,22.5527217865993,14.4944263653171));
#26287=CARTESIAN_POINT('Ctrl Pts',(56.267865183234,22.540111640693,14.493182518623));
#26288=CARTESIAN_POINT('Ctrl Pts',(56.2905112953748,22.5210853523676,14.4913255888369));
#26289=CARTESIAN_POINT('Ctrl Pts',(56.2978297073094,22.5148458991882,14.4907196788233));
#26290=CARTESIAN_POINT('Ctrl Pts',(56.310777131024,22.5036446308662,14.4896371539748));
#26291=CARTESIAN_POINT('Ctrl Pts',(56.3164238407634,22.4987034837169,14.4891613981939));
#26292=CARTESIAN_POINT('Ctrl Pts',(56.3282680018735,22.4882206807575,14.4881556996631));
#26293=CARTESIAN_POINT('Ctrl Pts',(56.3344589414928,22.4826719156494,14.4876254646428));
#26294=CARTESIAN_POINT('Ctrl Pts',(56.3507772020487,22.4678613200574,14.4862155930389));
#26295=CARTESIAN_POINT('Ctrl Pts',(56.3608437945503,22.4585335291695,14.4853331751132));
#26296=CARTESIAN_POINT('Ctrl Pts',(56.4041756821201,22.4175427032645,14.4814784554678));
#26297=CARTESIAN_POINT('Ctrl Pts',(56.4364358929736,22.3848422343479,14.4784616381259));
#26298=CARTESIAN_POINT('Ctrl Pts',(56.4877853061844,22.3290659028967,14.473405281233));
#26299=CARTESIAN_POINT('Ctrl Pts',(56.507535789191,22.3066204478637,14.4713928337083));
#26300=CARTESIAN_POINT('Ctrl Pts',(56.6323850999874,22.1581351113796,14.4582267516101));
#26301=CARTESIAN_POINT('Ctrl Pts',(56.7220795815213,22.0199954993894,14.446576766347));
#26302=CARTESIAN_POINT('Ctrl Pts',(56.8165251011663,21.8258049566556,14.4317971794872));
#26303=CARTESIAN_POINT('Ctrl Pts',(56.8373829237018,21.7782944802025,14.4283012406006));
#26304=CARTESIAN_POINT('Ctrl Pts',(56.8597239486326,21.721483576121,14.4243026149135));
#26305=CARTESIAN_POINT('Ctrl Pts',(56.8630223335183,21.7129232134842,14.4237048590337));
#26306=CARTESIAN_POINT('Ctrl Pts',(56.8680137869616,21.6996975621244,14.4227889884675));
#26307=CARTESIAN_POINT('Ctrl Pts',(56.8697486460658,21.6950483354103,14.4224684812275));
#26308=CARTESIAN_POINT('Ctrl Pts',(56.8729136602905,21.6864688448005,14.4218797620316));
#26309=CARTESIAN_POINT('Ctrl Pts',(56.8743487978127,21.6825405764626,14.421611264952));
#26310=CARTESIAN_POINT('Ctrl Pts',(56.8775611433769,21.6736611803479,14.4210067249144));
#26311=CARTESIAN_POINT('Ctrl Pts',(56.8793311248382,21.6687075278258,14.4206711114234));
#26312=CARTESIAN_POINT('Ctrl Pts',(56.8838419450751,21.6559237076198,14.4198090990724));
#26313=CARTESIAN_POINT('Ctrl Pts',(56.8865536024371,21.6480832469886,14.4192843689955));
#26314=CARTESIAN_POINT('Ctrl Pts',(56.903174106196,21.5990384876873,14.4160252745442));
#26315=CARTESIAN_POINT('Ctrl Pts',(56.9157824355719,21.5574020826099,14.4133606354269));
#26316=CARTESIAN_POINT('Ctrl Pts',(56.9337224113522,21.4903244510905,14.4091802714765));
#26317=CARTESIAN_POINT('Ctrl Pts',(56.9399352393888,21.4651363090738,14.4076353521036));
#26318=CARTESIAN_POINT('Ctrl Pts',(56.9834248014552,21.2727550623486,14.3959758257715));
#26319=CARTESIAN_POINT('Ctrl Pts',(56.9995168696397,21.1015117574379,14.3863301297046));
#26320=CARTESIAN_POINT('Ctrl Pts',(56.9923528933298,20.8965718969566,14.3739844318136));
#26321=CARTESIAN_POINT('Ctrl Pts',(56.9903170430279,20.8628675703426,14.3719308129874));
#26322=CARTESIAN_POINT('Ctrl Pts',(56.9853372349462,20.8049115592792,14.3683487216906));
#26323=CARTESIAN_POINT('Ctrl Pts',(56.9828013029156,20.780631934187,14.3668326541626));
#26324=CARTESIAN_POINT('Ctrl Pts',(56.9785476254048,20.7460600248567,14.3646493098096));
#26325=CARTESIAN_POINT('Ctrl Pts',(56.9771936474027,20.735724592471,14.3639934431612));
#26326=CARTESIAN_POINT('Ctrl Pts',(56.9747090961813,20.7178481139968,14.3628533859654));
#26327=CARTESIAN_POINT('Ctrl Pts',(56.9736161642502,20.7103019936299,14.362370390806));
#26328=CARTESIAN_POINT('Ctrl Pts',(56.9714325966813,20.6958117558236,14.3614394946268));
#26329=CARTESIAN_POINT('Ctrl Pts',(56.9703484658814,20.688866761547,14.3609918060667));
#26330=CARTESIAN_POINT('Ctrl Pts',(56.9677045116741,20.672497690729,14.3599329655641));
#26331=CARTESIAN_POINT('Ctrl Pts',(56.9661136674601,20.6630788679681,14.3593208392441));
#26332=CARTESIAN_POINT('Ctrl Pts',(56.9603176986663,20.6302027495763,14.3571739963814));
#26333=CARTESIAN_POINT('Ctrl Pts',(56.9557600525039,20.6068104509004,14.3556281751802));
#26334=CARTESIAN_POINT('Ctrl Pts',(56.9200435820043,20.4395206975094,14.3444371656428));
#26335=CARTESIAN_POINT('Ctrl Pts',(56.8734616531101,20.2994070383391,14.3342872673897));
#26336=CARTESIAN_POINT('Ctrl Pts',(56.7600139272689,20.0530191940997,14.315369679798));
#26337=CARTESIAN_POINT('Ctrl Pts',(56.6977146555525,19.9453943315695,14.3066909156322));
#26338=CARTESIAN_POINT('Ctrl Pts',(56.6192988289345,19.8350857411271,14.297792523091));
#26339=CARTESIAN_POINT('Ctrl Pts',(56.6127081750923,19.8259785845401,14.2970579804466));
#26340=CARTESIAN_POINT('Ctrl Pts',(56.6028471213512,19.8125920405279,14.2959790385747));
#26341=CARTESIAN_POINT('Ctrl Pts',(56.599635952795,19.8082695871904,14.2956307715026));
#26342=CARTESIAN_POINT('Ctrl Pts',(56.5938942436287,19.80060587421,14.2950135831801));
#26343=CARTESIAN_POINT('Ctrl Pts',(56.5913706390698,19.7972595379314,14.2947441929351));
#26344=CARTESIAN_POINT('Ctrl Pts',(56.5858922482519,19.7900425417683,14.2941634390148));
#26345=CARTESIAN_POINT('Ctrl Pts',(56.582933834471,19.7861747445749,14.2938523343598));
#26346=CARTESIAN_POINT('Ctrl Pts',(56.5747656760069,19.7755764345018,14.2930001248658));
#26347=CARTESIAN_POINT('Ctrl Pts',(56.5695269000432,19.7688682774435,14.2924610134989));
#26348=CARTESIAN_POINT('Ctrl Pts',(56.5425096231466,19.7347259021575,14.2897174163848));
#26349=CARTESIAN_POINT('Ctrl Pts',(56.5200527158194,19.707833381212,14.2875574002061));
#26350=CARTESIAN_POINT('Ctrl Pts',(56.3754349317021,19.5436427760545,14.2742754877038));
#26351=CARTESIAN_POINT('Ctrl Pts',(56.23549082531,19.4231758216685,14.2640300362258));
#26352=CARTESIAN_POINT('Ctrl Pts',(56.0413734813089,19.2980029808521,14.2503078465309));
#26353=CARTESIAN_POINT('Ctrl Pts',(56.0008387005034,19.2738557376337,14.2474710488413));
#26354=CARTESIAN_POINT('Ctrl Pts',(55.9319258589028,19.2360470216284,14.2426630404869));
#26355=CARTESIAN_POINT('Ctrl Pts',(55.9040111801154,19.2215794835117,14.2407194429367));
#26356=CARTESIAN_POINT('Ctrl Pts',(55.8654286420034,19.2027261639514,14.2380328638508));
#26357=CARTESIAN_POINT('Ctrl Pts',(55.8550465092259,19.1977637684414,14.2373099264706));
#26358=CARTESIAN_POINT('Ctrl Pts',(55.8375251066228,19.18957446161,14.2360895807494));
#26359=CARTESIAN_POINT('Ctrl Pts',(55.8304086246978,19.1862992398256,14.235593849275));
#26360=CARTESIAN_POINT('Ctrl Pts',(55.816321535393,19.1799162218973,14.2346123106265));
#26361=CARTESIAN_POINT('Ctrl Pts',(55.8093520159161,19.1768063404754,14.2341265853721));
#26362=CARTESIAN_POINT('Ctrl Pts',(55.7939618311549,19.1700446959976,14.2330536715362));
#26363=CARTESIAN_POINT('Ctrl Pts',(55.7855335000787,19.1664109185617,14.2324658818037));
#26364=CARTESIAN_POINT('Ctrl Pts',(55.7558045348668,19.1538362148956,14.2303916459095));
#26365=CARTESIAN_POINT('Ctrl Pts',(55.734374620603,19.1452075429938,14.2288947230466));
#26366=CARTESIAN_POINT('Ctrl Pts',(55.5581554401755,19.0777862042917,14.2165666668146));
#26367=CARTESIAN_POINT('Ctrl Pts',(55.396773262277,19.0381149531003,14.2050784366996));
#26368=CARTESIAN_POINT('Ctrl Pts',(55.1338435051142,19.0072737116295,14.1866196242322));
#26369=CARTESIAN_POINT('Ctrl Pts',(55.0345638587751,19.0030820164188,14.179727857552));
#26370=CARTESIAN_POINT('Ctrl Pts',(54.918294947748,19.006850752652,14.1720124026656));
#26371=CARTESIAN_POINT('Ctrl Pts',(54.9012208300879,19.0076239409862,14.1708885968169));
#26372=CARTESIAN_POINT('Ctrl Pts',(54.8777983722197,19.008986462254,14.1693614917557));
#26373=CARTESIAN_POINT('Ctrl Pts',(54.8714403617689,19.009386886553,14.1689484334336));
#26374=CARTESIAN_POINT('Ctrl Pts',(54.8607447558036,19.0101119485195,14.1682561789776));
#26375=CARTESIAN_POINT('Ctrl Pts',(54.8564061461445,19.0104203240992,14.1679760913621));
#26376=CARTESIAN_POINT('Ctrl Pts',(54.8481594220523,19.011033593326,14.1674451230392));
#26377=CARTESIAN_POINT('Ctrl Pts',(54.8442511564492,19.0113358186032,14.1671940906777));
#26378=CARTESIAN_POINT('Ctrl Pts',(54.8339767208445,19.0121608128636,14.1665356775679));
#26379=CARTESIAN_POINT('Ctrl Pts',(54.8276120634056,19.0127026480322,14.1661293543224));
#26380=CARTESIAN_POINT('Ctrl Pts',(54.8053459822788,19.0147059760209,14.1647129268298));
#26381=CARTESIAN_POINT('Ctrl Pts',(54.7894591131672,19.0163278695472,14.16371132743));
#26382=CARTESIAN_POINT('Ctrl Pts',(54.665653337191,19.0304714109176,14.1559644317481));
#26383=CARTESIAN_POINT('Ctrl Pts',(54.5588866492733,19.0516017423512,14.149625526924));
#26384=CARTESIAN_POINT('Ctrl Pts',(54.360472960126,19.1080273245364,14.1376452646986));
#26385=CARTESIAN_POINT('Ctrl Pts',(54.2686733373609,19.1415824685915,14.1320134376288));
#26386=CARTESIAN_POINT('Ctrl Pts',(54.1362696029225,19.2013149978459,14.1233875266458));
#26387=CARTESIAN_POINT('Ctrl Pts',(54.0935550761498,19.2224581406175,14.1205230394317));
#26388=CARTESIAN_POINT('Ctrl Pts',(54.0237757220257,19.2601675587828,14.1156724185072));
#26389=CARTESIAN_POINT('Ctrl Pts',(53.9962748283227,19.2758867869798,14.1137145592166));
#26390=CARTESIAN_POINT('Ctrl Pts',(53.9592814076733,19.2982169517958,14.111011359504));
#26391=CARTESIAN_POINT('Ctrl Pts',(53.9494539757162,19.3042660074488,14.1102863937447));
#26392=CARTESIAN_POINT('Ctrl Pts',(53.9330384161305,19.3145677056132,14.1090635897438));
#26393=CARTESIAN_POINT('Ctrl Pts',(53.9264217966929,19.3187745900851,14.108567443592));
#26394=CARTESIAN_POINT('Ctrl Pts',(53.9134185719142,19.3271501777982,14.1075858367425));
#26395=CARTESIAN_POINT('Ctrl Pts',(53.9070307280628,19.3313167180536,14.1071004623603));
#26396=CARTESIAN_POINT('Ctrl Pts',(53.8930256300361,19.340566612275,14.106029240816));
#26397=CARTESIAN_POINT('Ctrl Pts',(53.8854192054744,19.3456659732998,14.1054427994931));
#26398=CARTESIAN_POINT('Ctrl Pts',(53.8588569140426,19.3637397284104,14.1033783509854));
#26399=CARTESIAN_POINT('Ctrl Pts',(53.8400908819979,19.3769886063771,14.1018899976664));
#26400=CARTESIAN_POINT('Ctrl Pts',(53.6869026723977,19.4891537960387,14.0894861330886));
#26401=CARTESIAN_POINT('Ctrl Pts',(53.565177328456,19.6042411258448,14.0779015065588));
#26402=CARTESIAN_POINT('Ctrl Pts',(53.4111161175704,19.7916073675277,14.0609893622592));
#26403=CARTESIAN_POINT('Ctrl Pts',(53.3663779420761,19.8528098698243,14.0557260601564));
#26404=CARTESIAN_POINT('Ctrl Pts',(53.3123304914988,19.9363445991311,14.0489967717729));
#26405=CARTESIAN_POINT('Ctrl Pts',(53.2997903433196,19.9565066314446,14.0474055263903));
#26406=CARTESIAN_POINT('Ctrl Pts',(53.2793841668678,19.9906605675428,14.0447705210168));
#26407=CARTESIAN_POINT('Ctrl Pts',(53.2713218852945,20.0045317934763,14.0437166607207));
#26408=CARTESIAN_POINT('Ctrl Pts',(53.2603700039721,20.0239089936291,14.0422685500441));
#26409=CARTESIAN_POINT('Ctrl Pts',(53.2573377199747,20.0293330354462,14.0418657810728));
#26410=CARTESIAN_POINT('Ctrl Pts',(53.2522412663261,20.0385502517893,14.0411858289364));
#26411=CARTESIAN_POINT('Ctrl Pts',(53.2501639925456,20.0423360935244,14.0409078227035));
#26412=CARTESIAN_POINT('Ctrl Pts',(53.2462097238927,20.0495985904577,14.0403769925807));
#26413=CARTESIAN_POINT('Ctrl Pts',(53.2443307494997,20.0530741025088,14.0401240383948));
#26414=CARTESIAN_POINT('Ctrl Pts',(53.2398710626449,20.0613820276678,14.0395218849998));
#26415=CARTESIAN_POINT('Ctrl Pts',(53.2372998903166,20.0662195658938,14.039173284125));
#26416=CARTESIAN_POINT('Ctrl Pts',(53.2281937837549,20.0835239130664,14.0379332814178));
#26417=CARTESIAN_POINT('Ctrl Pts',(53.2217707317588,20.0960495689596,14.0370485869542));
#26418=CARTESIAN_POINT('Ctrl Pts',(53.1495873117757,20.2405625449687,14.0269764460843));
#26419=CARTESIAN_POINT('Ctrl Pts',(53.0985149168603,20.3794032890881,14.0185596558212));
#26420=CARTESIAN_POINT('Ctrl Pts',(53.0358849707252,20.633502202271,14.0033530664845));
#26421=CARTESIAN_POINT('Ctrl Pts',(53.0181304662096,20.7465096121793,13.9966554336261));
#26422=CARTESIAN_POINT('Ctrl Pts',(53.0081882054466,20.8882347119888,13.9879364266095));
#26423=CARTESIAN_POINT('Ctrl Pts',(53.0068201074395,20.9160982666301,13.986207993474));
#26424=CARTESIAN_POINT('Ctrl Pts',(53.0057282057485,20.954963390269,13.983773398809));
#26425=CARTESIAN_POINT('Ctrl Pts',(53.0055103953854,20.9659486429579,13.9830826298762));
#26426=CARTESIAN_POINT('Ctrl Pts',(53.0052939779079,20.984663977028,13.9819010725921));
#26427=CARTESIAN_POINT('Ctrl Pts',(53.0052495282842,20.9923933567165,13.9814117250838));
#26428=CARTESIAN_POINT('Ctrl Pts',(53.0052504850896,21.0079467540437,13.9804242028299));
#26429=CARTESIAN_POINT('Ctrl Pts',(53.0052969989434,21.0157706322548,13.9799260021873));
#26430=CARTESIAN_POINT('Ctrl Pts',(53.005525073187,21.0350518205792,13.9786945822042));
#26431=CARTESIAN_POINT('Ctrl Pts',(53.0057593299444,21.0465081135775,13.9779597296151));
#26432=CARTESIAN_POINT('Ctrl Pts',(53.0069957512948,21.0890416510443,13.9752192726415));
#26433=CARTESIAN_POINT('Ctrl Pts',(53.0086257496548,21.1200948186305,13.9731942427279));
#26434=CARTESIAN_POINT('Ctrl Pts',(53.0145009090126,21.1974351800298,13.9680873232751));
#26435=CARTESIAN_POINT('Ctrl Pts',(53.0196391357429,21.2436341148892,13.9649795394447));
#26436=CARTESIAN_POINT('Ctrl Pts',(53.0517891573737,21.462728906901,13.9499746503123));
#26437=CARTESIAN_POINT('Ctrl Pts',(53.0998547917015,21.6317282184606,13.9375165699183));
#26438=CARTESIAN_POINT('Ctrl Pts',(53.1867708802,21.8325587071409,13.9226114738475));
#26439=CARTESIAN_POINT('Ctrl Pts',(53.2055291435125,21.8722550351427,13.9196653436872));
#26440=CARTESIAN_POINT('Ctrl Pts',(53.2293838955418,21.918703093575,13.9162447344476));
#26441=CARTESIAN_POINT('Ctrl Pts',(53.2332306394897,21.9260792601345,13.9157023496882));
#26442=CARTESIAN_POINT('Ctrl Pts',(53.2395882595204,21.9380862487584,13.9148210639096));
#26443=CARTESIAN_POINT('Ctrl Pts',(53.2420714866698,21.9427314833475,13.9144805114628));
#26444=CARTESIAN_POINT('Ctrl Pts',(53.2465595692612,21.9510476920887,13.9138716201301));
#26445=CARTESIAN_POINT('Ctrl Pts',(53.2485575889342,21.9547222310737,13.9136028625064));
#26446=CARTESIAN_POINT('Ctrl Pts',(53.2529486906367,21.9627376869267,13.9130172317539));
#26447=CARTESIAN_POINT('Ctrl Pts',(53.2553463953839,21.9670759704211,13.9127006570518));
#26448=CARTESIAN_POINT('Ctrl Pts',(53.2622149024497,21.9793948094236,13.9118027094929));
#26449=CARTESIAN_POINT('Ctrl Pts',(53.2667245328025,21.9873537362153,13.9112237493036));
#26450=CARTESIAN_POINT('Ctrl Pts',(53.2968703177657,22.0397141511899,13.907420811812));
#26451=CARTESIAN_POINT('Ctrl Pts',(53.3241578300516,22.0831483053803,13.9042944216293));
#26452=CARTESIAN_POINT('Ctrl Pts',(53.4426792464745,22.2565790427975,13.8917241216521));
#26453=CARTESIAN_POINT('Ctrl Pts',(53.547601651041,22.3765116959438,13.8827796187527));
#26454=CARTESIAN_POINT('Ctrl Pts',(53.723119961459,22.5344654540417,13.8688065725319));
#26455=CARTESIAN_POINT('Ctrl Pts',(53.7835509224349,22.5828001909222,13.8641442462939));
#26456=CARTESIAN_POINT('Ctrl Pts',(53.8584978242574,22.6359131807713,13.8584351832116));
#26457=CARTESIAN_POINT('Ctrl Pts',(53.8704572934478,22.644193543578,13.857526390785));
#26458=CARTESIAN_POINT('Ctrl Pts',(53.8902473645466,22.657577747841,13.8560255946221));
#26459=CARTESIAN_POINT('Ctrl Pts',(53.8980253083639,22.6627587546711,13.8554365071666));
#26460=CARTESIAN_POINT('Ctrl Pts',(53.9120894218765,22.6719850515613,13.8543725325962));
#26461=CARTESIAN_POINT('Ctrl Pts',(53.918362504011,22.6760500480064,13.8538983935244));
#26462=CARTESIAN_POINT('Ctrl Pts',(53.93179794511,22.684649456512,13.8528837389246));
#26463=CARTESIAN_POINT('Ctrl Pts',(53.9389666380248,22.6891736507874,13.8523428568426));
#26464=CARTESIAN_POINT('Ctrl Pts',(53.9584465043738,22.7012945514631,13.8508743197494));
#26465=CARTESIAN_POINT('Ctrl Pts',(53.97081164561,22.7088031331847,13.8499434588304));
#26466=CARTESIAN_POINT('Ctrl Pts',(54.0359005741929,22.7473648487979,13.8450493659504));
#26467=CARTESIAN_POINT('Ctrl Pts',(54.0899459354064,22.7761114503358,13.8410041104192));
#26468=CARTESIAN_POINT('Ctrl Pts',(54.2655814463229,22.8594089502896,13.8279080141916));
#26469=CARTESIAN_POINT('Ctrl Pts',(54.3913452861554,22.9042857210874,13.8185776021681));
#26470=CARTESIAN_POINT('Ctrl Pts',(54.6114865635207,22.9587871522235,13.8027955105519));
#26471=CARTESIAN_POINT('Ctrl Pts',(54.7038324356323,22.9748617112744,13.7963407463093));
#26472=CARTESIAN_POINT('Ctrl Pts',(54.8073661275801,22.9854543180277,13.7895059596357));
#26473=CARTESIAN_POINT('Ctrl Pts',(54.8177652173258,22.9864357913348,13.7888239877174));
#26474=CARTESIAN_POINT('Ctrl Pts',(54.8334490828663,22.987791843322,13.7878027350285));
#26475=CARTESIAN_POINT('Ctrl Pts',(54.838728233377,22.9882271095721,13.7874602277789));
#26476=CARTESIAN_POINT('Ctrl Pts',(54.8481807600026,22.9889685745262,13.7868492561749));
#26477=CARTESIAN_POINT('Ctrl Pts',(54.8523534102309,22.9892826741466,13.7865803603094));
#26478=CARTESIAN_POINT('Ctrl Pts',(54.8614477196279,22.9899384829904,13.7859960651939));
#26479=CARTESIAN_POINT('Ctrl Pts',(54.8663696600848,22.9902750649114,13.7856809539383));
#26480=CARTESIAN_POINT('Ctrl Pts',(54.8803126365673,22.9911765853319,13.7847913310554));
#26481=CARTESIAN_POINT('Ctrl Pts',(54.8893364731645,22.9916984837372,13.7842191620866));
#26482=CARTESIAN_POINT('Ctrl Pts',(54.9472040080615,22.9946507778431,13.7805712188871));
#26483=CARTESIAN_POINT('Ctrl Pts',(54.9961239825301,22.9953458342757,13.7775841143064));
#26484=CARTESIAN_POINT('Ctrl Pts',(55.084908104999,22.9933413419167,13.7722594047859));
#26485=CARTESIAN_POINT('Ctrl Pts',(55.1247339702184,22.9912450978968,13.7699062491208));
#26486=CARTESIAN_POINT('Ctrl Pts',(55.164448547645,22.9879598179233,13.7675726541794));
#26487=CARTESIAN_POINT('Ctrl Pts',(55.1644483515698,22.987959834143,13.6085666014869));
#26488=CARTESIAN_POINT('Ctrl Pts',(55.1552326810296,22.9887221744091,13.6091613639964));
#26489=CARTESIAN_POINT('Ctrl Pts',(55.1460118811662,22.9894204182803,13.6097581340933));
#26490=CARTESIAN_POINT('Ctrl Pts',(55.0742147507976,22.9943554019005,13.614418225141));
#26491=CARTESIAN_POINT('Ctrl Pts',(55.0114812601815,22.9957023950593,13.6185707941191));
#26492=CARTESIAN_POINT('Ctrl Pts',(54.7753659584723,22.9896392050039,13.634509728283));
#26493=CARTESIAN_POINT('Ctrl Pts',(54.6032901096987,22.9625831772774,13.64683481341));
#26494=CARTESIAN_POINT('Ctrl Pts',(54.3862326369373,22.898711765279,13.6623297639935));
#26495=CARTESIAN_POINT('Ctrl Pts',(54.3361748130347,22.8817954064775,13.6658917594645));
#26496=CARTESIAN_POINT('Ctrl Pts',(54.2782394161307,22.8596166521722,13.6699555182529));
#26497=CARTESIAN_POINT('Ctrl Pts',(54.2696584792937,22.8562633715277,13.6705558523518));
#26498=CARTESIAN_POINT('Ctrl Pts',(54.256484684089,22.8510097881214,13.6714747670405));
#26499=CARTESIAN_POINT('Ctrl Pts',(54.2518753173202,22.8491516220113,13.6717957654537));
#26500=CARTESIAN_POINT('Ctrl Pts',(54.2434015411673,22.8456987322848,13.6723848606567));
#26501=CARTESIAN_POINT('Ctrl Pts',(54.2395352176559,22.8441090948444,13.6726532464198));
#26502=CARTESIAN_POINT('Ctrl Pts',(54.230826724131,22.8404965556407,13.6732568727682));
#26503=CARTESIAN_POINT('Ctrl Pts',(54.225987531244,22.8384666979214,13.6735916888372));
#26504=CARTESIAN_POINT('Ctrl Pts',(54.2117498002453,22.8324283296861,13.674575131744));
#26505=CARTESIAN_POINT('Ctrl Pts',(54.2023738168039,22.8283666052521,13.6752206420438));
#26506=CARTESIAN_POINT('Ctrl Pts',(54.1287945310834,22.7958179472095,13.6802728110162));
#26507=CARTESIAN_POINT('Ctrl Pts',(54.0660977685595,22.7640266351161,13.6844967638576));
#26508=CARTESIAN_POINT('Ctrl Pts',(53.8584294408312,22.6445419023461,13.6986382274644));
#26509=CARTESIAN_POINT('Ctrl Pts',(53.7230098718175,22.5417522544769,13.7081850348504));
#26510=CARTESIAN_POINT('Ctrl Pts',(53.5661867791288,22.3877158739902,13.7214250823952));
#26511=CARTESIAN_POINT('Ctrl Pts',(53.5315324342184,22.3509915076265,13.7245127345336));
#26512=CARTESIAN_POINT('Ctrl Pts',(53.4893441650268,22.3027402092431,13.7285096865559));
#26513=CARTESIAN_POINT('Ctrl Pts',(53.480483681854,22.2923943859438,13.7293633304094));
#26514=CARTESIAN_POINT('Ctrl Pts',(53.4664026205106,22.2756078380143,13.7307434813898));
#26515=CARTESIAN_POINT('Ctrl Pts',(53.4611149262075,22.269223780535,13.7312672390336));
#26516=CARTESIAN_POINT('Ctrl Pts',(53.4511154310859,22.2569966170398,13.7322683437077));
#26517=CARTESIAN_POINT('Ctrl Pts',(53.4463965083495,22.251159498735,13.732745391274));
#26518=CARTESIAN_POINT('Ctrl Pts',(53.4356833825343,22.2377537301119,13.7338391010312));
#26519=CARTESIAN_POINT('Ctrl Pts',(53.4297109962708,22.2301679622852,13.7344566193493));
#26520=CARTESIAN_POINT('Ctrl Pts',(53.4142489581222,22.2102329316568,13.73607604599));
#26521=CARTESIAN_POINT('Ctrl Pts',(53.4048485997373,22.1978155547022,13.737081429881));
#26522=CARTESIAN_POINT('Ctrl Pts',(53.3226756472774,22.0865864480545,13.746059602146));
#26523=CARTESIAN_POINT('Ctrl Pts',(53.2590334048429,21.9813830255535,13.7543850699677));
#26524=CARTESIAN_POINT('Ctrl Pts',(53.1539588892651,21.7649011003796,13.7710729524641));
#26525=CARTESIAN_POINT('Ctrl Pts',(53.1119661341389,21.6544237371343,13.7793849919054));
#26526=CARTESIAN_POINT('Ctrl Pts',(53.0677109457882,21.4973270302254,13.7905067833987));
#26527=CARTESIAN_POINT('Ctrl Pts',(53.0569256536497,21.4533629566357,13.7935447706254));
#26528=CARTESIAN_POINT('Ctrl Pts',(53.0458288627724,21.4004011883377,13.797086959804));
#26529=CARTESIAN_POINT('Ctrl Pts',(53.0440709507393,21.3917237629658,13.7976635808229));
#26530=CARTESIAN_POINT('Ctrl Pts',(53.0414313645827,21.378233260775,13.7985539290278));
#26531=CARTESIAN_POINT('Ctrl Pts',(53.0405095527251,21.3734282896132,13.798869849064));
#26532=CARTESIAN_POINT('Ctrl Pts',(53.0388316660343,21.3645049518832,13.799454260354));
#26533=CARTESIAN_POINT('Ctrl Pts',(53.0380708849644,21.3603876276639,13.7997230056433));
#26534=CARTESIAN_POINT('Ctrl Pts',(53.0363678689131,21.3510057239655,13.8003333387237));
#26535=CARTESIAN_POINT('Ctrl Pts',(53.0354338392054,21.3457397373156,13.8006744596697));
#26536=CARTESIAN_POINT('Ctrl Pts',(53.0330550521478,21.3320073783509,13.8015603803308));
#26537=CARTESIAN_POINT('Ctrl Pts',(53.0316437571322,21.3235352138146,13.8021033521161));
#26538=CARTESIAN_POINT('Ctrl Pts',(53.022513574026,21.2664534518167,13.8057390894018));
#26539=CARTESIAN_POINT('Ctrl Pts',(53.0165406409558,21.2175772625025,13.8087422989965));
#26540=CARTESIAN_POINT('Ctrl Pts',(53.0113077993132,21.1558603929747,13.8124527177128));
#26541=CARTESIAN_POINT('Ctrl Pts',(53.010354985019,21.1431846913762,13.8132104534635));
#26542=CARTESIAN_POINT('Ctrl Pts',(53.0067133644929,21.0876404008832,13.8165151117823));
#26543=CARTESIAN_POINT('Ctrl Pts',(53.0052883198242,21.0446991606966,13.8190292034624));
#26544=CARTESIAN_POINT('Ctrl Pts',(53.0051004112123,20.8297844890478,13.8315441383399));
#26545=CARTESIAN_POINT('Ctrl Pts',(53.0271841667994,20.6585476207796,13.8413745515307));
#26546=CARTESIAN_POINT('Ctrl Pts',(53.076088910496,20.4727416621568,13.8532305597303));
#26547=CARTESIAN_POINT('Ctrl Pts',(53.0815242033495,20.4532955032256,13.8544853664092));
#26548=CARTESIAN_POINT('Ctrl Pts',(53.0903655818648,20.4234202470756,13.8564363483584));
#26549=CARTESIAN_POINT('Ctrl Pts',(53.0935641790469,20.412930774688,13.857125810002));
#26550=CARTESIAN_POINT('Ctrl Pts',(53.0991396392622,20.3951728152262,13.8583008293405));
#26551=CARTESIAN_POINT('Ctrl Pts',(53.1014721284444,20.3878905712694,13.8587849274342));
#26552=CARTESIAN_POINT('Ctrl Pts',(53.1062716892927,20.3731972748331,13.8597663084676));
#26553=CARTESIAN_POINT('Ctrl Pts',(53.1087405330266,20.3657869468544,13.8602636425215));
#26554=CARTESIAN_POINT('Ctrl Pts',(53.1149202533105,20.3475952809971,13.8614905357406));
#26555=CARTESIAN_POINT('Ctrl Pts',(53.1186801341652,20.3368310002522,13.8622217027224));
#26556=CARTESIAN_POINT('Ctrl Pts',(53.132906339246,20.2971971768613,13.8649334539297));
#26557=CARTESIAN_POINT('Ctrl Pts',(53.1439461598869,20.2685394646035,13.8669329419791));
#26558=CARTESIAN_POINT('Ctrl Pts',(53.2234973797775,20.0754477484288,13.880678381433));
#26559=CARTESIAN_POINT('Ctrl Pts',(53.313099378693,19.9206017473992,13.8931710848395));
#26560=CARTESIAN_POINT('Ctrl Pts',(53.4743873775082,19.7120326738856,13.9114860782814));
#26561=CARTESIAN_POINT('Ctrl Pts',(53.5310578951989,19.6477550954853,13.917365365667));
#26562=CARTESIAN_POINT('Ctrl Pts',(53.5990632581276,19.5799604876498,13.9236711847041));
#26563=CARTESIAN_POINT('Ctrl Pts',(53.6064946750295,19.5726672105381,13.9243509776469));
#26564=CARTESIAN_POINT('Ctrl Pts',(53.6177867970575,19.5617572533241,13.9253695567141));
#26565=CARTESIAN_POINT('Ctrl Pts',(53.6216052007718,19.5580973279101,13.9257115459211));
#26566=CARTESIAN_POINT('Ctrl Pts',(53.6284693276917,19.5515702733502,13.9263218908697));
#26567=CARTESIAN_POINT('Ctrl Pts',(53.6315095429552,19.548697506328,13.9265906751643));
#26568=CARTESIAN_POINT('Ctrl Pts',(53.6381576682861,19.5424550104279,13.9271750663853));
#26569=CARTESIAN_POINT('Ctrl Pts',(53.6417690524902,19.5390891103235,13.927490383341));
#26570=CARTESIAN_POINT('Ctrl Pts',(53.652042123791,19.5295853728367,13.9283814416333));
#26571=CARTESIAN_POINT('Ctrl Pts',(53.6587332771765,19.5234793609788,13.9289548274795));
#26572=CARTESIAN_POINT('Ctrl Pts',(53.7021494038424,19.4843986633062,13.9326323213344));
#26573=CARTESIAN_POINT('Ctrl Pts',(53.7400492425903,19.4527480578743,13.9356460848332));
#26574=CARTESIAN_POINT('Ctrl Pts',(53.8927069438089,19.3345955237736,13.9472160842204));
#26575=CARTESIAN_POINT('Ctrl Pts',(54.015500190837,19.2591853037528,13.9553533038039));
#26576=CARTESIAN_POINT('Ctrl Pts',(54.2297343189642,19.1575986300446,13.9692766790851));
#26577=CARTESIAN_POINT('Ctrl Pts',(54.3168277822866,19.1235606991914,13.974864813304));
#26578=CARTESIAN_POINT('Ctrl Pts',(54.4203994448019,19.0912519878277,13.9816025438931));
#26579=CARTESIAN_POINT('Ctrl Pts',(54.4348711646708,19.0869173678614,13.982545814019));
#26580=CARTESIAN_POINT('Ctrl Pts',(54.458535085499,19.0801214020428,13.9840918503576));
#26581=CARTESIAN_POINT('Ctrl Pts',(54.4676982955756,19.0775606706726,13.9846913868545));
#26582=CARTESIAN_POINT('Ctrl Pts',(54.4841069239701,19.0731014576758,13.9857666952262));
#26583=CARTESIAN_POINT('Ctrl Pts',(54.4913454228148,19.0711780338986,13.9862416494695));
#26584=CARTESIAN_POINT('Ctrl Pts',(54.5066933086353,19.0671921758369,13.9872500322995));
#26585=CARTESIAN_POINT('Ctrl Pts',(54.5148051649436,19.0651399158058,13.9877837790261));
#26586=CARTESIAN_POINT('Ctrl Pts',(54.5364992177966,19.0597964299018,13.9892134206866));
#26587=CARTESIAN_POINT('Ctrl Pts',(54.5501032971806,19.056596848612,13.9901122386008));
#26588=CARTESIAN_POINT('Ctrl Pts',(54.6170985919839,19.0415811776925,13.9945507300544));
#26589=CARTESIAN_POINT('Ctrl Pts',(54.6709220207241,19.0318220364986,13.9981552318035));
#26590=CARTESIAN_POINT('Ctrl Pts',(54.9273535185751,18.9961389185671,14.0155214132644));
#26591=CARTESIAN_POINT('Ctrl Pts',(55.132709605493,18.9992247218774,14.0301570547956));
#26592=CARTESIAN_POINT('Ctrl Pts',(55.3672970428133,19.0390662407924,14.0462332392441));
#26593=CARTESIAN_POINT('Ctrl Pts',(55.4004488271056,19.045566735589,14.0484853227566));
#26594=CARTESIAN_POINT('Ctrl Pts',(55.4416269381479,19.054732956356,14.051244887526));
#26595=CARTESIAN_POINT('Ctrl Pts',(55.4498206740082,19.0566113124633,14.0517921066951));
#26596=CARTESIAN_POINT('Ctrl Pts',(55.4627174697789,19.059653748901,14.0526501789461));
#26597=CARTESIAN_POINT('Ctrl Pts',(55.4674284692655,19.0607832358589,14.0529629355441));
#26598=CARTESIAN_POINT('Ctrl Pts',(55.4761706788522,19.0629129350446,14.0535419873109));
#26599=CARTESIAN_POINT('Ctrl Pts',(55.4802028440518,19.0639085657922,14.0538085288544));
#26600=CARTESIAN_POINT('Ctrl Pts',(55.4894661563551,19.066226601598,14.0544196701416));
#26601=CARTESIAN_POINT('Ctrl Pts',(55.4946950644523,19.0675576413675,14.0547637698372));
#26602=CARTESIAN_POINT('Ctrl Pts',(55.5108604042022,19.0717425075797,14.0558250399915));
#26603=CARTESIAN_POINT('Ctrl Pts',(55.5217782558515,19.0746681388843,14.0565382233852));
#26604=CARTESIAN_POINT('Ctrl Pts',(55.6266881328798,19.1037385498565,14.0633618606612));
#26605=CARTESIAN_POINT('Ctrl Pts',(55.7186809901207,19.1366566748165,14.0691208891382));
#26606=CARTESIAN_POINT('Ctrl Pts',(55.9701957201019,19.2480712858742,14.0851595728427));
#26607=CARTESIAN_POINT('Ctrl Pts',(56.1221468237173,19.3412910896098,14.095279618973));
#26608=CARTESIAN_POINT('Ctrl Pts',(56.2763957593493,19.4669305917009,14.107564665743));
#26609=CARTESIAN_POINT('Ctrl Pts',(56.2928117331088,19.4807483051178,14.1088997106308));
#26610=CARTESIAN_POINT('Ctrl Pts',(56.3165053711697,19.5013539194377,14.1108693038057));
#26611=CARTESIAN_POINT('Ctrl Pts',(56.3239605762672,19.5079360423095,14.1114953867825));
#26612=CARTESIAN_POINT('Ctrl Pts',(56.3370050112589,19.5196275798027,14.1126022813778));
#26613=CARTESIAN_POINT('Ctrl Pts',(56.3426149906431,19.52471362545,14.1130821079201));
#26614=CARTESIAN_POINT('Ctrl Pts',(56.3541506291313,19.5352922079741,14.1140767102123));
#26615=CARTESIAN_POINT('Ctrl Pts',(56.3600721395892,19.5407890439186,14.1145916637942));
#26616=CARTESIAN_POINT('Ctrl Pts',(56.3751900100117,19.55499466679,14.1159178315714));
#26617=CARTESIAN_POINT('Ctrl Pts',(56.3843370051199,19.5637552365189,14.1167312644698));
#26618=CARTESIAN_POINT('Ctrl Pts',(56.4225850927655,19.6010923231142,14.1201801946861));
#26619=CARTESIAN_POINT('Ctrl Pts',(56.4508878262971,19.6304690051292,14.122850579856));
#26620=CARTESIAN_POINT('Ctrl Pts',(56.5238546648181,19.7110064881066,14.1300649916758));
#26621=CARTESIAN_POINT('Ctrl Pts',(56.5668377417068,19.7636120208499,14.1346710711252));
#26622=CARTESIAN_POINT('Ctrl Pts',(56.670247848153,19.9042447540744,14.1466873406498));
#26623=CARTESIAN_POINT('Ctrl Pts',(56.7264463350414,19.9951174387021,14.1541844714237));
#26624=CARTESIAN_POINT('Ctrl Pts',(56.7849357355886,20.1092159277828,14.1630662903404));
#26625=CARTESIAN_POINT('Ctrl Pts',(56.794453949625,20.1285489648467,14.1645534724135));
#26626=CARTESIAN_POINT('Ctrl Pts',(56.8133940903769,20.168646192926,14.1675969791084));
#26627=CARTESIAN_POINT('Ctrl Pts',(56.8227771721309,20.1894256788189,14.1691521091866));
#26628=CARTESIAN_POINT('Ctrl Pts',(56.8456655685474,20.2425221898798,14.1730628060774));
#26629=CARTESIAN_POINT('Ctrl Pts',(56.8586805661273,20.2750441852979,14.1753999733126));
#26630=CARTESIAN_POINT('Ctrl Pts',(56.8737856235143,20.3158747167406,14.1782483943594));
#26631=CARTESIAN_POINT('Ctrl Pts',(56.8766869178166,20.3238741353695,14.178802410939));
#26632=CARTESIAN_POINT('Ctrl Pts',(56.8811674762443,20.3364789476145,14.1796687766491));
#26633=CARTESIAN_POINT('Ctrl Pts',(56.8827811801762,20.3410718632183,14.1799830888593));
#26634=CARTESIAN_POINT('Ctrl Pts',(56.885752499689,20.3496288533142,14.1805660679371));
#26635=CARTESIAN_POINT('Ctrl Pts',(56.8871144282388,20.3535912641945,14.1808349776391));
#26636=CARTESIAN_POINT('Ctrl Pts',(56.8901974933762,20.3626539619936,14.1814476624666));
#26637=CARTESIAN_POINT('Ctrl Pts',(56.8919104760574,20.3677569388699,14.1817909562176));
#26638=CARTESIAN_POINT('Ctrl Pts',(56.8971354101909,20.3835334132539,14.1828472500474));
#26639=CARTESIAN_POINT('Ctrl Pts',(56.900577922197,20.3942299176702,14.1835563167646));
#26640=CARTESIAN_POINT('Ctrl Pts',(56.9379355574339,20.5137609590034,14.1914069741198));
#26641=CARTESIAN_POINT('Ctrl Pts',(56.9625567734565,20.6252985017048,14.1980668246599));
#26642=CARTESIAN_POINT('Ctrl Pts',(56.9982640914052,20.8951620098877,14.2138806702175));
#26643=CARTESIAN_POINT('Ctrl Pts',(57.0002854480263,21.0538730371714,14.2229844269306));
#26644=CARTESIAN_POINT('Ctrl Pts',(56.9810830727581,21.2342594280995,14.234163188077));
#26645=CARTESIAN_POINT('Ctrl Pts',(56.9782195767754,21.2573224764076,14.2356069528073));
#26646=CARTESIAN_POINT('Ctrl Pts',(56.9736258783564,21.2896856142171,14.2376555528477));
#26647=CARTESIAN_POINT('Ctrl Pts',(56.9722314020644,21.2990320293709,14.238249848864));
#26648=CARTESIAN_POINT('Ctrl Pts',(56.9696881184416,21.3152860753282,14.2392881622505));
#26649=CARTESIAN_POINT('Ctrl Pts',(56.968569242743,21.3221982739227,14.2397312285548));
#26650=CARTESIAN_POINT('Ctrl Pts',(56.9661530929869,21.3366422234673,14.2406603062273));
#26651=CARTESIAN_POINT('Ctrl Pts',(56.9648488830199,21.3441726832681,14.2411465305528));
#26652=CARTESIAN_POINT('Ctrl Pts',(56.9616442947634,21.3620637733453,14.2423061899184));
#26653=CARTESIAN_POINT('Ctrl Pts',(56.9597050775083,21.3724171280815,14.2429808478972));
#26654=CARTESIAN_POINT('Ctrl Pts',(56.9528729210201,21.4073617313167,14.2452703336611));
#26655=CARTESIAN_POINT('Ctrl Pts',(56.9475985272008,21.4318751064799,14.2468972158502));
#26656=CARTESIAN_POINT('Ctrl Pts',(56.9338669976195,21.4903143579195,14.2508274124513));
#26657=CARTESIAN_POINT('Ctrl Pts',(56.9249774460853,21.5241291057028,14.253143835649));
#26658=CARTESIAN_POINT('Ctrl Pts',(56.8867005629468,21.6555782990492,14.2623159788075));
#26659=CARTESIAN_POINT('Ctrl Pts',(56.8507372021531,21.751125433209,14.2693597588999));
#26660=CARTESIAN_POINT('Ctrl Pts',(56.7790310395837,21.9047937759995,14.2811779849764));
#26661=CARTESIAN_POINT('Ctrl Pts',(56.7473274725101,21.9645984917734,14.2859083468611));
#26662=CARTESIAN_POINT('Ctrl Pts',(56.7003912857594,22.0432010491635,14.2922275432127));
#26663=CARTESIAN_POINT('Ctrl Pts',(56.6877678910154,22.0635029699285,14.2938691794522));
#26664=CARTESIAN_POINT('Ctrl Pts',(56.6504508708863,22.1211805295448,14.2985512865359));
#26665=CARTESIAN_POINT('Ctrl Pts',(56.6248574781147,22.1579605905424,14.3015596788477));
#26666=CARTESIAN_POINT('Ctrl Pts',(56.5930382263116,22.2005526893131,14.3050428551924));
#26667=CARTESIAN_POINT('Ctrl Pts',(56.5879890641782,22.207223379591,14.3055883576664));
#26668=CARTESIAN_POINT('Ctrl Pts',(56.5796844998341,22.2180526793506,14.3064736253656));
#26669=CARTESIAN_POINT('Ctrl Pts',(56.5764543479728,22.2222303952221,14.306815067054));
#26670=CARTESIAN_POINT('Ctrl Pts',(56.5706363010165,22.2296937275913,14.3074248286645));
#26671=CARTESIAN_POINT('Ctrl Pts',(56.5680546379799,22.2329840660302,14.307693573564));
#26672=CARTESIAN_POINT('Ctrl Pts',(56.5623989964131,22.2401457064855,14.3082783358295));
#26673=CARTESIAN_POINT('Ctrl Pts',(56.5593209753191,22.244013703508,14.3085940603173));
#26674=CARTESIAN_POINT('Ctrl Pts',(56.5505430761194,22.2549606888105,14.3094874355758));
#26675=CARTESIAN_POINT('Ctrl Pts',(56.5448090650583,22.2620123301088,14.3100627114176));
#26676=CARTESIAN_POINT('Ctrl Pts',(56.5072131176887,22.3076073258052,14.313782881599));
#26677=CARTESIAN_POINT('Ctrl Pts',(56.4739566353184,22.3449836698419,14.3168349971958));
#26678=CARTESIAN_POINT('Ctrl Pts',(56.3364950593736,22.4882433787389,14.3287283432958));
#26679=CARTESIAN_POINT('Ctrl Pts',(56.2220103895296,22.5835984311233,14.337125201163));
#26680=CARTESIAN_POINT('Ctrl Pts',(56.0244248342823,22.713868832438,14.3510551936972));
#26681=CARTESIAN_POINT('Ctrl Pts',(55.9477315762915,22.7574397888886,14.3563404981603));
#26682=CARTESIAN_POINT('Ctrl Pts',(55.8549404295896,22.802311978598,14.3627426891505));
#26683=CARTESIAN_POINT('Ctrl Pts',(55.8413926171499,22.8086763256673,14.3636774326731));
#26684=CARTESIAN_POINT('Ctrl Pts',(55.8191564738538,22.8188182866302,14.3652122668273));
#26685=CARTESIAN_POINT('Ctrl Pts',(55.8105104337895,22.8226876090458,14.365809206426));
#26686=CARTESIAN_POINT('Ctrl Pts',(55.7949834026363,22.8295040259626,14.3668816454909));
#26687=CARTESIAN_POINT('Ctrl Pts',(55.7881127198565,22.8324742644264,14.3673563444551));
#26688=CARTESIAN_POINT('Ctrl Pts',(55.7735036196259,22.8386925094156,14.3683660824166));
#26689=CARTESIAN_POINT('Ctrl Pts',(55.765761115191,22.8419304831257,14.3689014509013));
#26690=CARTESIAN_POINT('Ctrl Pts',(55.7449670824066,22.8504729358417,14.3703400232282));
#26691=CARTESIAN_POINT('Ctrl Pts',(55.7318795975686,22.8556880874539,14.3712462143558));
#26692=CARTESIAN_POINT('Ctrl Pts',(55.666396575968,22.8809815423083,14.375785018258));
#26693=CARTESIAN_POINT('Ctrl Pts',(55.6132299796831,22.8989797040246,14.3794860583233));
#26694=CARTESIAN_POINT('Ctrl Pts',(55.4303683420704,22.9524024021443,14.3922770566148));
#26695=CARTESIAN_POINT('Ctrl Pts',(55.2980493655483,22.9769080689736,14.4016636059742));
#26696=CARTESIAN_POINT('Ctrl Pts',(55.1644483421759,22.9879598349201,14.4110001919405));
#26697=CARTESIAN_POINT('Origin',(55.,21.,6.22095488139522));
#26698=CARTESIAN_POINT('',(55.1642080971762,22.984919470593,15.3685782038315));
#26699=CARTESIAN_POINT('',(55.1646076307061,22.9900841388564,15.2105321270573));
#26700=CARTESIAN_POINT('',(55.1644483516311,22.987959834138,6.22095488139522));
#26701=CARTESIAN_POINT('',(53.0046263220794,20.9982271535794,14.7790451186048));
#26702=CARTESIAN_POINT('Ctrl Pts',(53.0046263220794,20.9982271535794,14.7790451186048));
#26703=CARTESIAN_POINT('Ctrl Pts',(53.0033880615454,20.8638533255282,14.7876313150491));
#26704=CARTESIAN_POINT('Ctrl Pts',(53.0770257042585,20.0681393313831,14.8385619430631));
#26705=CARTESIAN_POINT('Ctrl Pts',(54.1456767166442,18.8023905785495,14.9318370026467));
#26706=CARTESIAN_POINT('Ctrl Pts',(56.3832764285273,19.090575541161,15.0588702973557));
#26707=CARTESIAN_POINT('Ctrl Pts',(57.354408655632,21.1269461461278,15.1859035920647));
#26708=CARTESIAN_POINT('Ctrl Pts',(56.3918339859998,22.6873870777271,15.28913956089));
#26709=CARTESIAN_POINT('Ctrl Pts',(55.4549141389281,22.9618400383867,15.3500310981456));
#26710=CARTESIAN_POINT('Ctrl Pts',(55.1642080971762,22.984919470593,15.3685782038315));
#26711=CARTESIAN_POINT('Ctrl Pts',(53.0052508056195,20.9982072316684,14.7786858855498));
#26712=CARTESIAN_POINT('Ctrl Pts',(53.0051093009901,21.1556543710583,14.7695402577617));
#26713=CARTESIAN_POINT('Ctrl Pts',(53.0236076901605,21.312552534886,14.7604750581731));
#26714=CARTESIAN_POINT('Ctrl Pts',(53.0641633313545,21.4814866269597,14.749769145838));
#26715=CARTESIAN_POINT('Ctrl Pts',(53.0681602132696,21.4972805989829,14.7487594584664));
#26716=CARTESIAN_POINT('Ctrl Pts',(53.075878523736,21.5262816119864,14.7468882376772));
#26717=CARTESIAN_POINT('Ctrl Pts',(53.0795436455624,21.5395027028071,14.7460285268067));
#26718=CARTESIAN_POINT('Ctrl Pts',(53.0856479955576,21.5606719783708,14.7446408189508));
#26719=CARTESIAN_POINT('Ctrl Pts',(53.0880010821416,21.5686447036245,14.7441156253189));
#26720=CARTESIAN_POINT('Ctrl Pts',(53.092572889085,21.5837856479163,14.7431132553435));
#26721=CARTESIAN_POINT('Ctrl Pts',(53.0947823623488,21.5909565270189,14.7426363883998));
#26722=CARTESIAN_POINT('Ctrl Pts',(53.0999163811918,21.6072909736035,14.7415451769942));
#26723=CARTESIAN_POINT('Ctrl Pts',(53.1028668375154,21.6164461400038,14.7409299917306));
#26724=CARTESIAN_POINT('Ctrl Pts',(53.1107285025393,21.6402495273016,14.7393209935814));
#26725=CARTESIAN_POINT('Ctrl Pts',(53.1157438035436,21.6548624375776,14.7383237790047));
#26726=CARTESIAN_POINT('Ctrl Pts',(53.1648368827078,21.7926684031044,14.7288278777595));
#26727=CARTESIAN_POINT('Ctrl Pts',(53.2207570566107,21.9112791596017,14.7199246561726));
#26728=CARTESIAN_POINT('Ctrl Pts',(53.3255730378848,22.086609720519,14.7057310781512));
#26729=CARTESIAN_POINT('Ctrl Pts',(53.3667306207798,22.1475440924894,14.7005850891718));
#26730=CARTESIAN_POINT('Ctrl Pts',(53.4582853228461,22.2681559085178,14.6900858798536));
#26731=CARTESIAN_POINT('Ctrl Pts',(53.5090192190398,22.3274346080632,14.6847479978984));
#26732=CARTESIAN_POINT('Ctrl Pts',(53.5705907605057,22.3913782638125,14.6789119312165));
#26733=CARTESIAN_POINT('Ctrl Pts',(53.5781465600205,22.3990986579342,14.6782059539672));
#26734=CARTESIAN_POINT('Ctrl Pts',(53.5888524565059,22.4098614614895,14.6772203570995));
#26735=CARTESIAN_POINT('Ctrl Pts',(53.5919502573058,22.4129552905459,14.6769368753826));
#26736=CARTESIAN_POINT('Ctrl Pts',(53.5981365333277,22.4190930860855,14.6763741957952));
#26737=CARTESIAN_POINT('Ctrl Pts',(53.601224810976,22.4221372430092,14.6760949834341));
#26738=CARTESIAN_POINT('Ctrl Pts',(53.6071324196211,22.4279225917131,14.6755641205512));
#26739=CARTESIAN_POINT('Ctrl Pts',(53.609949954986,22.4306655435169,14.6753123270914));
#26740=CARTESIAN_POINT('Ctrl Pts',(53.6174129771987,22.4378881507121,14.6746489899062));
#26741=CARTESIAN_POINT('Ctrl Pts',(53.6220721708681,22.4423536702372,14.6742385342098));
#26742=CARTESIAN_POINT('Ctrl Pts',(53.6386194410553,22.4580597404909,14.6727933379997));
#26743=CARTESIAN_POINT('Ctrl Pts',(53.6506244218265,22.469176920175,14.671767562946));
#26744=CARTESIAN_POINT('Ctrl Pts',(53.7567534380884,22.5650589808827,14.6628811330546));
#26745=CARTESIAN_POINT('Ctrl Pts',(53.8586295358653,22.6408394260659,14.6555717324402));
#26746=CARTESIAN_POINT('Ctrl Pts',(54.0534641712264,22.7587804738662,14.6423584557538));
#26747=CARTESIAN_POINT('Ctrl Pts',(54.1437573468979,22.8044626034304,14.6364893593641));
#26748=CARTESIAN_POINT('Ctrl Pts',(54.2692546348302,22.8564074377094,14.6283215275186));
#26749=CARTESIAN_POINT('Ctrl Pts',(54.3017335613391,22.8688662710383,14.6262078070782));
#26750=CARTESIAN_POINT('Ctrl Pts',(54.3578366913226,22.8887206223258,14.6225450979));
#26751=CARTESIAN_POINT('Ctrl Pts',(54.3813037084655,22.8965374024671,14.621009708445));
#26752=CARTESIAN_POINT('Ctrl Pts',(54.4150430480052,22.9070830223147,14.6187947846496));
#26753=CARTESIAN_POINT('Ctrl Pts',(54.425201842738,22.9101694587418,14.6181269312347));
#26754=CARTESIAN_POINT('Ctrl Pts',(54.442730913073,22.9153426313239,14.6169727086636));
#26755=CARTESIAN_POINT('Ctrl Pts',(54.4500895295623,22.917468305461,14.6164876180453));
#26756=CARTESIAN_POINT('Ctrl Pts',(54.4641843143264,22.9214520395255,14.6155573354789));
#26757=CARTESIAN_POINT('Ctrl Pts',(54.4709183735436,22.9233171916543,14.6151123820768));
#26758=CARTESIAN_POINT('Ctrl Pts',(54.4867195398463,22.9276044225198,14.6140671024935));
#26759=CARTESIAN_POINT('Ctrl Pts',(54.4957941554183,22.9299979538326,14.6134658624168));
#26760=CARTESIAN_POINT('Ctrl Pts',(54.5270237474313,22.9379998244758,14.6113933377087));
#26761=CARTESIAN_POINT('Ctrl Pts',(54.5492573440115,22.9432912394195,14.6099119345449));
#26762=CARTESIAN_POINT('Ctrl Pts',(54.7307005610402,22.9831919782937,14.5977703076172));
#26763=CARTESIAN_POINT('Ctrl Pts',(54.8934838760922,22.9985510965638,14.586476208462));
#26764=CARTESIAN_POINT('Ctrl Pts',(55.0923963267766,22.9929364532975,14.5725991760173));
#26765=CARTESIAN_POINT('Ctrl Pts',(55.128464834068,22.9909364704228,14.5700833654849));
#26766=CARTESIAN_POINT('Ctrl Pts',(55.1644484406754,22.987959826772,14.5675833348156));
#26767=CARTESIAN_POINT('',(53.008286603288,21.0001954942154,14.6208388173789));
#26768=CARTESIAN_POINT('Ctrl Pts',(55.1644483421759,22.9879598349201,14.4110001919405));
#26769=CARTESIAN_POINT('Ctrl Pts',(55.1025335197272,22.9930815631004,14.4153270529764));
#26770=CARTESIAN_POINT('Ctrl Pts',(55.0403429528252,22.9953139133895,14.4196373367823));
#26771=CARTESIAN_POINT('Ctrl Pts',(54.9391576233513,22.9942017486132,14.4265037334952));
#26772=CARTESIAN_POINT('Ctrl Pts',(54.9002566347636,22.9926349756726,14.4291080060147));
#26773=CARTESIAN_POINT('Ctrl Pts',(54.8526457235039,22.9893194070754,14.4322325079126));
#26774=CARTESIAN_POINT('Ctrl Pts',(54.843871854374,22.9886500434199,14.4328056692727));
#26775=CARTESIAN_POINT('Ctrl Pts',(54.8301851532795,22.9875147363219,14.4336953604483));
#26776=CARTESIAN_POINT('Ctrl Pts',(54.8252692631919,22.9870885939376,14.4340140251934));
#26777=CARTESIAN_POINT('Ctrl Pts',(54.8161889224585,22.9862674915272,14.4346009394302));
#26778=CARTESIAN_POINT('Ctrl Pts',(54.8120241578351,22.9858776758514,14.4348694619184));
#26779=CARTESIAN_POINT('Ctrl Pts',(54.8025929498459,22.9849649937103,14.4354760417209));
#26780=CARTESIAN_POINT('Ctrl Pts',(54.7973273504136,22.9844342690985,14.4358136556978));
#26781=CARTESIAN_POINT('Ctrl Pts',(54.7813468556045,22.9827593098309,14.4368352573577));
#26782=CARTESIAN_POINT('Ctrl Pts',(54.7706388539653,22.9815491806167,14.4375156758485));
#26783=CARTESIAN_POINT('Ctrl Pts',(54.7458760669907,22.9785472741259,14.4390807163507));
#26784=CARTESIAN_POINT('Ctrl Pts',(54.731829359033,22.9766923942108,14.4399621628217));
#26785=CARTESIAN_POINT('Ctrl Pts',(54.6837955439313,22.969828023617,14.4429583091842));
#26786=CARTESIAN_POINT('Ctrl Pts',(54.6499171229389,22.9640901080659,14.445040543394));
#26787=CARTESIAN_POINT('Ctrl Pts',(54.4609054062164,22.9270310622953,14.4565672192785));
#26788=CARTESIAN_POINT('Ctrl Pts',(54.309777818485,22.8782096791687,14.4654836054982));
#26789=CARTESIAN_POINT('Ctrl Pts',(54.0952420959614,22.7794685099114,14.4794549762261));
#26790=CARTESIAN_POINT('Ctrl Pts',(54.0264587439206,22.7427881013267,14.4841503144741));
#26791=CARTESIAN_POINT('Ctrl Pts',(53.9464756337429,22.6939200656817,14.4899755749277));
#26792=CARTESIAN_POINT('Ctrl Pts',(53.9330497691615,22.6854957612994,14.4909662574186));
#26793=CARTESIAN_POINT('Ctrl Pts',(53.912358916783,22.6721666288084,14.4925138332816));
#26794=CARTESIAN_POINT('Ctrl Pts',(53.9050232677481,22.6673722776486,14.4930666325735));
#26795=CARTESIAN_POINT('Ctrl Pts',(53.8919639779343,22.6587137862896,14.4940582822601));
#26796=CARTESIAN_POINT('Ctrl Pts',(53.8862283289142,22.6548679445042,14.4944964415168));
#26797=CARTESIAN_POINT('Ctrl Pts',(53.8802595549919,22.6508207025449,14.4949551911354));
#26798=CARTESIAN_POINT('Ctrl Pts',(53.8800063257327,22.6506489105012,14.4949746591452));
#26799=CARTESIAN_POINT('Ctrl Pts',(53.8795253008057,22.6503224190407,14.495011649832));
#26800=CARTESIAN_POINT('Ctrl Pts',(53.8792974976222,22.6501677307131,14.4950291720878));
#26801=CARTESIAN_POINT('Ctrl Pts',(53.8788616430457,22.649871634506,14.4950627054653));
#26802=CARTESIAN_POINT('Ctrl Pts',(53.8786535863363,22.6497302344156,14.4950787162922));
#26803=CARTESIAN_POINT('Ctrl Pts',(53.8782531247459,22.6494579608178,14.4951095403133));
#26804=CARTESIAN_POINT('Ctrl Pts',(53.8780607159613,22.6493270929619,14.4951243532949));
#26805=CARTESIAN_POINT('Ctrl Pts',(53.8776884852326,22.6490738229802,14.4951530161208));
#26806=CARTESIAN_POINT('Ctrl Pts',(53.8775086604149,22.6489514251107,14.4951668658026));
#26807=CARTESIAN_POINT('Ctrl Pts',(53.8771592385969,22.6487135072958,14.4951937826131));
#26808=CARTESIAN_POINT('Ctrl Pts',(53.8769896393652,22.648597990571,14.4952068496208));
#26809=CARTESIAN_POINT('Ctrl Pts',(53.8766588068039,22.6483725805295,14.495232343694));
#26810=CARTESIAN_POINT('Ctrl Pts',(53.8764975717951,22.6482626897404,14.4952447706619));
#26811=CARTESIAN_POINT('Ctrl Pts',(53.8761819658174,22.6480475185686,14.4952690997552));
#26812=CARTESIAN_POINT('Ctrl Pts',(53.8760275934384,22.647942240099,14.4952810018115));
#26813=CARTESIAN_POINT('Ctrl Pts',(53.875724476518,22.6477354588122,14.4953043758796));
#26814=CARTESIAN_POINT('Ctrl Pts',(53.8755757309428,22.6476339575533,14.4953158478311));
#26815=CARTESIAN_POINT('Ctrl Pts',(53.8752828315722,22.6474340302458,14.4953384411914));
#26816=CARTESIAN_POINT('Ctrl Pts',(53.8751386769664,22.6473356054281,14.4953495625522));
#26817=CARTESIAN_POINT('Ctrl Pts',(53.8748540759329,22.6471412328596,14.495371522582));
#26818=CARTESIAN_POINT('Ctrl Pts',(53.8747136288809,22.6470452860819,14.4953823612124));
#26819=CARTESIAN_POINT('Ctrl Pts',(53.8744356769868,22.6468553503576,14.4954038146436));
#26820=CARTESIAN_POINT('Ctrl Pts',(53.874298171582,22.6467613621098,14.4954144294208));
#26821=CARTESIAN_POINT('Ctrl Pts',(53.8740254277067,22.6465748849939,14.4954354870817));
#26822=CARTESIAN_POINT('Ctrl Pts',(53.8738901889127,22.6464823967223,14.4954459299397));
#26823=CARTESIAN_POINT('Ctrl Pts',(53.873621374154,22.6462985087565,14.4954666902657));
#26824=CARTESIAN_POINT('Ctrl Pts',(53.8734877978484,22.6462071094185,14.4954770077237));
#26825=CARTESIAN_POINT('Ctrl Pts',(53.8732217582993,22.6460250248098,14.4954975596111));
#26826=CARTESIAN_POINT('Ctrl Pts',(53.8730892949882,22.6459343398811,14.4955077940219));
#26827=CARTESIAN_POINT('Ctrl Pts',(53.8651859058975,22.6405222458142,14.4961185142975));
#26828=CARTESIAN_POINT('Ctrl Pts',(53.857452866986,22.6351459601498,14.4967210803998));
#26829=CARTESIAN_POINT('Ctrl Pts',(53.8328907857349,22.6178102131982,14.4986512397652));
#26830=CARTESIAN_POINT('Ctrl Pts',(53.8162096629667,22.6056444776907,14.4999867032378));
#26831=CARTESIAN_POINT('Ctrl Pts',(53.7358047920365,22.5450702047642,14.5065473137775));
#26832=CARTESIAN_POINT('Ctrl Pts',(53.6748522179466,22.4931215575001,14.5119100962587));
#26833=CARTESIAN_POINT('Ctrl Pts',(53.519837697439,22.3440210519825,14.526622370619));
#26834=CARTESIAN_POINT('Ctrl Pts',(53.4322504196806,22.2407378132037,14.5361592718706));
#26835=CARTESIAN_POINT('Ctrl Pts',(53.3473020019213,22.1170680822263,14.5464974362038));
#26836=CARTESIAN_POINT('Ctrl Pts',(53.3389631226623,22.104630382423,14.5475256766446));
#26837=CARTESIAN_POINT('Ctrl Pts',(53.3037601590698,22.0508239224615,14.5519215548976));
#26838=CARTESIAN_POINT('Ctrl Pts',(53.2782930410174,22.0085566723762,14.5552436711169));
#26839=CARTESIAN_POINT('Ctrl Pts',(53.250258121056,21.9578646940406,14.5590407028151));
#26840=CARTESIAN_POINT('Ctrl Pts',(53.2461476171676,21.9503174420168,14.5596012747505));
#26841=CARTESIAN_POINT('Ctrl Pts',(53.2395576314333,21.9380292361754,14.560506017031));
#26842=CARTESIAN_POINT('Ctrl Pts',(53.2370482726526,21.9333045535219,14.5608519853716));
#26843=CARTESIAN_POINT('Ctrl Pts',(53.2326087691644,21.9248639531808,14.5614666056552));
#26844=CARTESIAN_POINT('Ctrl Pts',(53.2306712912535,21.9211520049568,14.5617357120715));
#26845=CARTESIAN_POINT('Ctrl Pts',(53.2264957827786,21.9130905102161,14.5623175688376));
#26846=CARTESIAN_POINT('Ctrl Pts',(53.2242620610533,21.9087388303437,14.5626300496195));
#26847=CARTESIAN_POINT('Ctrl Pts',(53.2180327110184,21.8964922953067,14.5635050410681));
#26848=CARTESIAN_POINT('Ctrl Pts',(53.2140735127537,21.8885788899191,14.5640653290017));
#26849=CARTESIAN_POINT('Ctrl Pts',(53.1902325619024,21.8401239507384,14.5674665658638));
#26850=CARTESIAN_POINT('Ctrl Pts',(53.1716777679201,21.7989398953987,14.5702321044402));
#26851=CARTESIAN_POINT('Ctrl Pts',(53.1144998916092,21.6595770000029,14.5792934216638));
#26852=CARTESIAN_POINT('Ctrl Pts',(53.0822639643949,21.5589671205267,14.5853631052236));
#26853=CARTESIAN_POINT('Ctrl Pts',(53.0297027811058,21.335270770168,14.598705662906));
#26854=CARTESIAN_POINT('Ctrl Pts',(53.0126463155418,21.2118908127092,14.605980964456));
#26855=CARTESIAN_POINT('Ctrl Pts',(53.0063349151494,21.0685313378505,14.6148170626009));
#26856=CARTESIAN_POINT('Ctrl Pts',(53.0057671401622,21.0493181132451,14.6160086110643));
#26857=CARTESIAN_POINT('Ctrl Pts',(53.005326135664,21.0200959110041,14.6178333923284));
#26858=CARTESIAN_POINT('Ctrl Pts',(53.0052504320197,21.0100908251943,14.6184603853498));
#26859=CARTESIAN_POINT('Ctrl Pts',(53.0052500018438,21.0000857659472,14.6190897100634));
#26860=CARTESIAN_POINT('Ctrl Pts',(53.0084881004496,21.0002027753601,14.6209548813952));
#26861=CARTESIAN_POINT('Ctrl Pts',(53.0088012939876,20.6548595780746,14.6429136572615));
#26862=CARTESIAN_POINT('Ctrl Pts',(53.2585703182277,19.6431460319286,14.7072168646974));
#26863=CARTESIAN_POINT('Ctrl Pts',(54.8687658122962,18.6458264387637,14.813864503703));
#26864=CARTESIAN_POINT('Ctrl Pts',(56.9069018544316,19.6132480805813,14.940897798412));
#26865=CARTESIAN_POINT('Ctrl Pts',(57.199161840635,21.8503192148488,15.0679310931209));
#26866=CARTESIAN_POINT('Ctrl Pts',(55.981387458458,22.8822711615308,15.1578092026694));
#26867=CARTESIAN_POINT('Ctrl Pts',(55.2454399918933,22.9840771000814,15.2053428806482));
#26868=CARTESIAN_POINT('Ctrl Pts',(55.1646076307061,22.9900841388564,15.2105321270573));
#26869=CARTESIAN_POINT('Origin',(55.,21.,6.22095488139522));
#26870=CARTESIAN_POINT('',(55.1644483516311,22.987959834138,16.1684645359809));
#26871=CARTESIAN_POINT('',(55.1644482585673,22.9879598418364,16.0088160704683));
#26872=CARTESIAN_POINT('',(55.1644483516311,22.987959834138,6.22095488139522));
#26873=CARTESIAN_POINT('',(53.0052502923665,21.0010799982591,15.5790451544755));
#26874=CARTESIAN_POINT('Ctrl Pts',(53.0052502923665,21.0010799982591,15.5790451544755));
#26875=CARTESIAN_POINT('Ctrl Pts',(53.0052131657774,20.9325074313172,15.5834434861452));
#26876=CARTESIAN_POINT('Ctrl Pts',(53.0087162052572,20.8637923838756,15.5878418178149));
#26877=CARTESIAN_POINT('Ctrl Pts',(53.0157771547505,20.7953362198876,15.5922401494845));
#26878=CARTESIAN_POINT('Ctrl Pts',(53.022827440247,20.7269834437393,15.5966318384506));
#26879=CARTESIAN_POINT('Ctrl Pts',(53.0334249181497,20.6588892708525,15.6010235274166));
#26880=CARTESIAN_POINT('Ctrl Pts',(53.0475353187344,20.5914547382354,15.6054152163827));
#26881=CARTESIAN_POINT('Ctrl Pts',(53.061633981611,20.5240763008969,15.6098032521312));
#26882=CARTESIAN_POINT('Ctrl Pts',(53.0792396735167,20.4573569060938,15.6141912878797));
#26883=CARTESIAN_POINT('Ctrl Pts',(53.1002665442361,20.3916905725279,15.6185793236282));
#26884=CARTESIAN_POINT('Ctrl Pts',(53.1212834799863,20.3260552655952,15.6229652860773));
#26885=CARTESIAN_POINT('Ctrl Pts',(53.1457182362593,20.2614725111638,15.6273512485263));
#26886=CARTESIAN_POINT('Ctrl Pts',(53.1734347757927,20.1983223564196,15.6317372109753));
#26887=CARTESIAN_POINT('Ctrl Pts',(53.2011481786548,20.1351793483568,15.6361226770665));
#26888=CARTESIAN_POINT('Ctrl Pts',(53.2321424242669,20.0734690776151,15.6405081431577));
#26889=CARTESIAN_POINT('Ctrl Pts',(53.2662336402944,20.0135509275928,15.6448936092488));
#26890=CARTESIAN_POINT('Ctrl Pts',(53.3003564985035,19.9535771638022,15.6492831457643));
#26891=CARTESIAN_POINT('Ctrl Pts',(53.3375818183001,19.8953992801179,15.6536726822798));
#26892=CARTESIAN_POINT('Ctrl Pts',(53.3776806739743,19.8393503685851,15.6580622187953));
#26893=CARTESIAN_POINT('Ctrl Pts',(53.4177985411012,19.7832748834453,15.6624538364541));
#26894=CARTESIAN_POINT('Ctrl Pts',(53.4607923417108,19.7293307723388,15.6668454541129));
#26895=CARTESIAN_POINT('Ctrl Pts',(53.5063926899687,19.677818179704,15.6712370717717));
#26896=CARTESIAN_POINT('Ctrl Pts',(53.5520741810312,19.6262139238168,15.6756365040238));
#26897=CARTESIAN_POINT('Ctrl Pts',(53.6003711274293,19.5770501834321,15.6800359362758));
#26898=CARTESIAN_POINT('Ctrl Pts',(53.6509777244895,19.5305897568492,15.6844353685279));
#26899=CARTESIAN_POINT('Ctrl Pts',(53.6877926491778,19.496791058557,15.6876358359855));
#26900=CARTESIAN_POINT('Ctrl Pts',(53.7258291234092,19.4644221954192,15.690836303443));
#26901=CARTESIAN_POINT('Ctrl Pts',(53.7649596425576,19.4335700213579,15.6940367709006));
#26902=CARTESIAN_POINT('Ctrl Pts',(53.819423624556,19.3906282897056,15.6984913553475));
#26903=CARTESIAN_POINT('Ctrl Pts',(53.8762374044059,19.3504456850435,15.7029459397944));
#26904=CARTESIAN_POINT('Ctrl Pts',(53.935089962567,19.3132889474855,15.7074005242413));
#26905=CARTESIAN_POINT('Ctrl Pts',(53.9938542289503,19.276187953204,15.711848425832));
#26906=CARTESIAN_POINT('Ctrl Pts',(54.0546507925009,19.2421040753733,15.7162963274228));
#26907=CARTESIAN_POINT('Ctrl Pts',(54.1171366007932,19.211263076682,15.7207442290135));
#26908=CARTESIAN_POINT('Ctrl Pts',(54.1795489420745,19.1804583389603,15.7251869010322));
#26909=CARTESIAN_POINT('Ctrl Pts',(54.2436461466312,19.1528891232233,15.7296295730509));
#26910=CARTESIAN_POINT('Ctrl Pts',(54.3090588417498,19.128736288404,15.7340722450696));
#26911=CARTESIAN_POINT('Ctrl Pts',(54.3744304090047,19.1045986395436,15.7385121237833));
#26912=CARTESIAN_POINT('Ctrl Pts',(54.4411153679474,19.0838732794765,15.742952002497));
#26913=CARTESIAN_POINT('Ctrl Pts',(54.5087239574729,19.0666931406166,15.7473918812107));
#26914=CARTESIAN_POINT('Ctrl Pts',(54.5763129955656,19.0495179700061,15.7518304759752));
#26915=CARTESIAN_POINT('Ctrl Pts',(54.6448246598927,19.0358861057982,15.7562690707398));
#26916=CARTESIAN_POINT('Ctrl Pts',(54.7138553196154,19.0258802507478,15.7607076655043));
#26917=CARTESIAN_POINT('Ctrl Pts',(54.7828894559218,19.0158738917736,15.7651464838093));
#26918=CARTESIAN_POINT('Ctrl Pts',(54.8524421548205,19.0094939723416,15.7695853021143));
#26919=CARTESIAN_POINT('Ctrl Pts',(54.9221026877489,19.0067715707315,15.7740241204193));
#26920=CARTESIAN_POINT('Ctrl Pts',(54.9918369190813,19.0040462889159,15.7784676348386));
#26921=CARTESIAN_POINT('Ctrl Pts',(55.0616787221389,19.0049862673432,15.7829111492579));
#26922=CARTESIAN_POINT('Ctrl Pts',(55.1312163458724,19.0095704400618,15.7873546636772));
#26923=CARTESIAN_POINT('Ctrl Pts',(55.2007946366043,19.0141572936966,15.791800776753));
#26924=CARTESIAN_POINT('Ctrl Pts',(55.2700679078115,19.0223925257482,15.7962468898287));
#26925=CARTESIAN_POINT('Ctrl Pts',(55.3386312988932,19.0342033660854,15.8006930029045));
#26926=CARTESIAN_POINT('Ctrl Pts',(55.4073138594396,19.0460347347468,15.8051468437327));
#26927=CARTESIAN_POINT('Ctrl Pts',(55.4752835997395,19.0614540089214,15.8096006845609));
#26928=CARTESIAN_POINT('Ctrl Pts',(55.5421483674747,19.0803378656273,15.8140545253892));
#26929=CARTESIAN_POINT('Ctrl Pts',(55.577256078285,19.0902529375354,15.816393038796));
#26930=CARTESIAN_POINT('Ctrl Pts',(55.6120594570637,19.1011223144444,15.8187315522028));
#26931=CARTESIAN_POINT('Ctrl Pts',(55.646504023642,19.112922865934,15.8210700656096));
#26932=CARTESIAN_POINT('Ctrl Pts',(55.7121167458579,19.135401485461,15.8255246500565));
#26933=CARTESIAN_POINT('Ctrl Pts',(55.7766852636897,19.1613505471637,15.8299792345034));
#26934=CARTESIAN_POINT('Ctrl Pts',(55.8398168110724,19.1906533537378,15.8344338189503));
#26935=CARTESIAN_POINT('Ctrl Pts',(55.9028536472525,19.2199121996589,15.838881720541));
#26936=CARTESIAN_POINT('Ctrl Pts',(55.9644573513741,19.2525145999698,15.8433296221317));
#26937=CARTESIAN_POINT('Ctrl Pts',(56.0242522191242,19.2882947233478,15.8477775237224));
#26938=CARTESIAN_POINT('Ctrl Pts',(56.0839767837076,19.324032778634,15.8522201957412));
#26939=CARTESIAN_POINT('Ctrl Pts',(56.1418963179344,19.3629408863146,15.8566628677599));
#26940=CARTESIAN_POINT('Ctrl Pts',(56.1976585757808,19.4048067520332,15.8611055397786));
#26941=CARTESIAN_POINT('Ctrl Pts',(56.2533857734214,19.4466462948244,15.8655454184923));
#26942=CARTESIAN_POINT('Ctrl Pts',(56.3069579949739,19.4914396132661,15.8699852972059));
#26943=CARTESIAN_POINT('Ctrl Pts',(56.3580522089396,19.5389312951493,15.8744251759196));
#26944=CARTESIAN_POINT('Ctrl Pts',(56.4091316471927,19.5864092431203,15.8788637706842));
#26945=CARTESIAN_POINT('Ctrl Pts',(56.457734142166,19.6365836723948,15.8833023654487));
#26946=CARTESIAN_POINT('Ctrl Pts',(56.5035713466246,19.6891602813046,15.8877409602132));
#26947=CARTESIAN_POINT('Ctrl Pts',(56.5494108595773,19.7417395381245,15.8921797785182));
#26948=CARTESIAN_POINT('Ctrl Pts',(56.5924844857156,19.796720844287,15.8966185968233));
#26949=CARTESIAN_POINT('Ctrl Pts',(56.6325434059738,19.8537759424478,15.9010574151283));
#26950=CARTESIAN_POINT('Ctrl Pts',(56.6726447071665,19.9108914029041,15.9055009295476));
#26951=CARTESIAN_POINT('Ctrl Pts',(56.709724654796,19.9700846330709,15.9099444439669));
#26952=CARTESIAN_POINT('Ctrl Pts',(56.7435776888094,20.0309982427332,15.9143879583862));
#26953=CARTESIAN_POINT('Ctrl Pts',(56.7774505207568,20.0919474758975,15.9188340714619));
#26954=CARTESIAN_POINT('Ctrl Pts',(56.8080924678627,20.1546186513152,15.9232801845377));
#26955=CARTESIAN_POINT('Ctrl Pts',(56.8353451499069,20.2186321332349,15.9277262976134));
#26956=CARTESIAN_POINT('Ctrl Pts',(56.8626451996131,20.2827568764597,15.9321801384416));
#26957=CARTESIAN_POINT('Ctrl Pts',(56.886544057494,20.3482281236182,15.9366339792699));
#26958=CARTESIAN_POINT('Ctrl Pts',(56.9069327103309,20.4146495060479,15.9410878200981));
#26959=CARTESIAN_POINT('Ctrl Pts',(56.917637883651,20.4495244149868,15.9434263335049));
#26960=CARTESIAN_POINT('Ctrl Pts',(56.927376200681,20.4846610583987,15.9457648469118));
#26961=CARTESIAN_POINT('Ctrl Pts',(56.9361375560808,20.5200011182998,15.9481033603186));
#26962=CARTESIAN_POINT('Ctrl Pts',(56.9528268756218,20.5873196466979,15.9525579447655));
#26963=CARTESIAN_POINT('Ctrl Pts',(56.9660340164727,20.655642547169,15.9570125292124));
#26964=CARTESIAN_POINT('Ctrl Pts',(56.9756440654991,20.7245765279461,15.9614671136593));
#26965=CARTESIAN_POINT('Ctrl Pts',(56.9852396973388,20.7934070925945,15.96591501525));
#26966=CARTESIAN_POINT('Ctrl Pts',(56.9912488810164,20.8628464371986,15.9703629168407));
#26967=CARTESIAN_POINT('Ctrl Pts',(56.9936072387921,20.9324889643411,15.9748108184314));
#26968=CARTESIAN_POINT('Ctrl Pts',(56.9959628237542,21.0020496100382,15.9792534904501));
#26969=CARTESIAN_POINT('Ctrl Pts',(56.9946760916894,21.0718124770158,15.9836961624689));
#26970=CARTESIAN_POINT('Ctrl Pts',(56.9897344243389,21.1413664850692,15.9881388344876));
#26971=CARTESIAN_POINT('Ctrl Pts',(56.9847958640339,21.2108767614316,15.9925787132013));
#26972=CARTESIAN_POINT('Ctrl Pts',(56.9762069618547,21.2801779523193,15.9970185919149));
#26973=CARTESIAN_POINT('Ctrl Pts',(56.9640071694412,21.3488601451638,16.0014584706286));
#26974=CARTESIAN_POINT('Ctrl Pts',(56.9518109050323,21.4175224761049,16.0058970653932));
#26975=CARTESIAN_POINT('Ctrl Pts',(56.9360059089185,21.4855656827349,16.0103356601577));
#26976=CARTESIAN_POINT('Ctrl Pts',(56.9166831156036,21.5525879087167,16.0147742549222));
#26977=CARTESIAN_POINT('Ctrl Pts',(56.8973593491372,21.6196135101313,16.0192130732272));
#26978=CARTESIAN_POINT('Ctrl Pts',(56.8745175716195,21.6856175592179,16.0236518915322));
#26979=CARTESIAN_POINT('Ctrl Pts',(56.8482986813516,21.7502130010964,16.0280907098372));
#26980=CARTESIAN_POINT('Ctrl Pts',(56.822052052416,21.81487678269,16.0325342242565));
#26981=CARTESIAN_POINT('Ctrl Pts',(56.7924213639965,21.8781285282594,16.0369777386758));
#26982=CARTESIAN_POINT('Ctrl Pts',(56.7595954488438,21.9396017341982,16.0414212530951));
#26983=CARTESIAN_POINT('Ctrl Pts',(56.7267503364369,22.001110890902,16.0458673661709));
#26984=CARTESIAN_POINT('Ctrl Pts',(56.6907065309271,22.0608390185728,16.0503134792466));
#26985=CARTESIAN_POINT('Ctrl Pts',(56.6516971384873,22.1184471937526,16.0547595923223));
#26986=CARTESIAN_POINT('Ctrl Pts',(56.612619944144,22.1761554972268,16.0592134331506));
#26987=CARTESIAN_POINT('Ctrl Pts',(56.5705671690884,22.2317361028605,16.0636672739788));
#26988=CARTESIAN_POINT('Ctrl Pts',(56.525812746943,22.2848824941473,16.068121114807));
#26989=CARTESIAN_POINT('Ctrl Pts',(56.502314193618,22.3127872966186,16.0704596282139));
#26990=CARTESIAN_POINT('Ctrl Pts',(56.478071471137,22.3400216303825,16.0727981416207));
#26991=CARTESIAN_POINT('Ctrl Pts',(56.4531281009969,22.3665453832907,16.0751366550276));
#26992=CARTESIAN_POINT('Ctrl Pts',(56.4056260482042,22.4170571106084,16.0795901104623));
#26993=CARTESIAN_POINT('Ctrl Pts',(56.3553933595571,22.4651887889572,16.0840435658969));
#26994=CARTESIAN_POINT('Ctrl Pts',(56.3026979752753,22.5106308442878,16.0884970213315));
#26995=CARTESIAN_POINT('Ctrl Pts',(56.2500754348441,22.5560100824602,16.0929443204994));
#26996=CARTESIAN_POINT('Ctrl Pts',(56.1949973185801,22.5987067557146,16.0973916196673));
#26997=CARTESIAN_POINT('Ctrl Pts',(56.1377693807795,22.6384469471608,16.1018389188352));
#26998=CARTESIAN_POINT('Ctrl Pts',(56.0806011129274,22.6781457026359,16.1062815809304));
#26999=CARTESIAN_POINT('Ctrl Pts',(56.0212878714928,22.714893815648,16.1107242430255));
#27000=CARTESIAN_POINT('Ctrl Pts',(55.9601682043401,22.7484577724024,16.1151669051206));
#27001=CARTESIAN_POINT('Ctrl Pts',(55.8990649478455,22.7820127172193,16.119608374359));
#27002=CARTESIAN_POINT('Ctrl Pts',(55.8361566447006,22.8123849462518,16.1240498435973));
#27003=CARTESIAN_POINT('Ctrl Pts',(55.7718094973695,22.839385131578,16.1284913128357));
#27004=CARTESIAN_POINT('Ctrl Pts',(55.7075011255453,22.8663690466278,16.1329301056505));
#27005=CARTESIAN_POINT('Ctrl Pts',(55.6417560895648,22.889984779647,16.1373688984653));
#27006=CARTESIAN_POINT('Ctrl Pts',(55.5749614015851,22.9100908222352,16.1418076912801));
#27007=CARTESIAN_POINT('Ctrl Pts',(55.5081063016138,22.930215049594,16.1462504987302));
#27008=CARTESIAN_POINT('Ctrl Pts',(55.4402001196311,22.9468230912987,16.1506933061804));
#27009=CARTESIAN_POINT('Ctrl Pts',(55.3716455595063,22.9598232421826,16.1551361136305));
#27010=CARTESIAN_POINT('Ctrl Pts',(55.3030909993815,22.9728233930666,16.1595789210806));
#27011=CARTESIAN_POINT('Ctrl Pts',(55.2338885481216,22.9822155903893,16.1640217285307));
#27012=CARTESIAN_POINT('Ctrl Pts',(55.1644483516311,22.987959834138,16.1684645359809));
#27013=CARTESIAN_POINT('Ctrl Pts',(55.1642080971762,22.984919470593,15.3685782038315));
#27014=CARTESIAN_POINT('Ctrl Pts',(54.791210469995,23.0145321109006,15.3923755297153));
#27015=CARTESIAN_POINT('Ctrl Pts',(53.7301334665886,22.8199335201067,15.4585172871686));
#27016=CARTESIAN_POINT('Ctrl Pts',(53.033386236972,21.787011120162,15.5286729254264));
#27017=CARTESIAN_POINT('Ctrl Pts',(53.0022835510889,21.0637411429413,15.5750312378004));
#27018=CARTESIAN_POINT('Ctrl Pts',(53.0026935992604,21.0010819424674,15.5790451186048));
#27019=CARTESIAN_POINT('',(53.0049939673739,20.9981913424498,15.420954726227));
#27020=CARTESIAN_POINT('Ctrl Pts',(55.1646076307061,22.9900841388564,15.2105321270573));
#27021=CARTESIAN_POINT('Ctrl Pts',(54.5858451071959,23.0330947458601,15.2476873122178));
#27022=CARTESIAN_POINT('Ctrl Pts',(53.4459374565242,22.6200279605996,15.3178281786077));
#27023=CARTESIAN_POINT('Ctrl Pts',(53.0097639809454,21.5146609743285,15.3879690449977));
#27024=CARTESIAN_POINT('Ctrl Pts',(53.0049939673739,20.9981913424498,15.420954726227));
#27025=CARTESIAN_POINT('Ctrl Pts',(53.0052508126406,20.9981994364738,15.421102452815));
#27026=CARTESIAN_POINT('Ctrl Pts',(53.0053510647738,20.8871353955393,15.4288471065411));
#27027=CARTESIAN_POINT('Ctrl Pts',(53.0147268740369,20.7762621275074,15.4366195681347));
#27028=CARTESIAN_POINT('Ctrl Pts',(53.0358535934502,20.6515856253841,15.4450663374528));
#27029=CARTESIAN_POINT('Ctrl Pts',(53.0385958981777,20.6364650443494,15.4460855343218));
#27030=CARTESIAN_POINT('Ctrl Pts',(53.0430393883581,20.6134803797667,15.447625344939));
#27031=CARTESIAN_POINT('Ctrl Pts',(53.044613804336,20.6055927444684,15.4481520552864));
#27032=CARTESIAN_POINT('Ctrl Pts',(53.0472783225556,20.5926520778961,15.4490131476044));
#27033=CARTESIAN_POINT('Ctrl Pts',(53.0483404165262,20.5875934640958,15.4493489897642));
#27034=CARTESIAN_POINT('Ctrl Pts',(53.0504417930872,20.5777748266234,15.4499992860299));
#27035=CARTESIAN_POINT('Ctrl Pts',(53.0514788748356,20.5730143735494,15.4503138585225));
#27036=CARTESIAN_POINT('Ctrl Pts',(53.0534401713326,20.5641675232971,15.450897067657));
#27037=CARTESIAN_POINT('Ctrl Pts',(53.0543598103192,20.5600802719784,15.4511659489515));
#27038=CARTESIAN_POINT('Ctrl Pts',(53.0564891954052,20.5507537121437,15.4517782449666));
#27039=CARTESIAN_POINT('Ctrl Pts',(53.057707252214,20.5455163828505,15.4521211807054));
#27040=CARTESIAN_POINT('Ctrl Pts',(53.0609480313193,20.531832879904,15.4530149642999));
#27041=CARTESIAN_POINT('Ctrl Pts',(53.0630047877747,20.5233947714788,15.4535639306557));
#27042=CARTESIAN_POINT('Ctrl Pts',(53.0775106488955,20.4655279175796,15.4573152138641));
#27043=CARTESIAN_POINT('Ctrl Pts',(53.0917964143046,20.4165741158235,15.4604214481491));
#27044=CARTESIAN_POINT('Ctrl Pts',(53.1265071875482,20.3126226641734,15.4669770490478));
#27045=CARTESIAN_POINT('Ctrl Pts',(53.1475131868166,20.2578704837039,15.4704052142044));
#27046=CARTESIAN_POINT('Ctrl Pts',(53.199646474455,20.1380571884916,15.4780054269643));
#27047=CARTESIAN_POINT('Ctrl Pts',(53.2319496750776,20.0736004266553,15.482163236072));
#27048=CARTESIAN_POINT('Ctrl Pts',(53.3095873765614,19.9376058068315,15.4913240550353));
#27049=CARTESIAN_POINT('Ctrl Pts',(53.3561278307007,19.8669252611186,15.4963407569303));
#27050=CARTESIAN_POINT('Ctrl Pts',(53.424769591956,19.7758482276004,15.5033274168221));
#27051=CARTESIAN_POINT('Ctrl Pts',(53.4430508267868,19.7526798599785,15.5051535362483));
#27052=CARTESIAN_POINT('Ctrl Pts',(53.4673484216776,19.7232535144209,15.5075414701357));
#27053=CARTESIAN_POINT('Ctrl Pts',(53.4729015951414,19.7166166172613,15.5080846876073));
#27054=CARTESIAN_POINT('Ctrl Pts',(53.4839058463224,19.7036373901723,15.5091563130192));
#27055=CARTESIAN_POINT('Ctrl Pts',(53.4893539751192,19.6972927869107,15.5096845944947));
#27056=CARTESIAN_POINT('Ctrl Pts',(53.4997573297919,19.6853306111869,15.5106891903622));
#27057=CARTESIAN_POINT('Ctrl Pts',(53.5047046289526,19.6797063121373,15.5111651711632));
#27058=CARTESIAN_POINT('Ctrl Pts',(53.5160128131169,19.6669957742144,15.5122492577886));
#27059=CARTESIAN_POINT('Ctrl Pts',(53.5223929602089,19.6599269917066,15.5128581656974));
#27060=CARTESIAN_POINT('Ctrl Pts',(53.5390432124855,19.6417430860713,15.5144403536542));
#27061=CARTESIAN_POINT('Ctrl Pts',(53.5493894799272,19.63069883615,15.515416853504));
#27062=CARTESIAN_POINT('Ctrl Pts',(53.6251179301101,19.5516831335772,15.52251811737));
#27063=CARTESIAN_POINT('Ctrl Pts',(53.6951126523438,19.4883165584853,15.5288455890199));
#27064=CARTESIAN_POINT('Ctrl Pts',(53.8796696204105,19.3436337221625,15.5449443628457));
#27065=CARTESIAN_POINT('Ctrl Pts',(53.9988289071187,19.2690051793327,15.5548666078106));
#27066=CARTESIAN_POINT('Ctrl Pts',(54.1559900269391,19.1922728174744,15.5668354460668));
#27067=CARTESIAN_POINT('Ctrl Pts',(54.1875491778496,19.1778709304201,15.5691849132651));
#27068=CARTESIAN_POINT('Ctrl Pts',(54.2325937796785,19.1587182072989,15.5724480395552));
#27069=CARTESIAN_POINT('Ctrl Pts',(54.2457778625774,19.1532785969797,15.5733924161728));
#27070=CARTESIAN_POINT('Ctrl Pts',(54.26886377943,19.1440420773241,15.5750260999898));
#27071=CARTESIAN_POINT('Ctrl Pts',(54.2787395059834,19.140181918746,15.5757186584927));
#27072=CARTESIAN_POINT('Ctrl Pts',(54.2936749708942,19.1344809050779,15.5767560703827));
#27073=CARTESIAN_POINT('Ctrl Pts',(54.2987119649171,19.1325815590081,15.5771042384922));
#27074=CARTESIAN_POINT('Ctrl Pts',(54.3076475988664,19.1292533696836,15.577718804945));
#27075=CARTESIAN_POINT('Ctrl Pts',(54.3115430694272,19.1278162862421,15.5779856856377));
#27076=CARTESIAN_POINT('Ctrl Pts',(54.3200012351053,19.1247259420911,15.5785628963511));
#27077=CARTESIAN_POINT('Ctrl Pts',(54.3245654795197,19.1230771666686,15.5788729602611));
#27078=CARTESIAN_POINT('Ctrl Pts',(54.3370865803329,19.1186056664744,15.5797198085754));
#27079=CARTESIAN_POINT('Ctrl Pts',(54.3450555206016,19.1158167352598,15.5802546396508));
#27080=CARTESIAN_POINT('Ctrl Pts',(54.3854046404801,19.1019824655199,15.5829429356349));
#27081=CARTESIAN_POINT('Ctrl Pts',(54.4180495829951,19.0917201314812,15.5850540264259));
#27082=CARTESIAN_POINT('Ctrl Pts',(54.6467879518315,19.0262301317743,15.5995096514263));
#27083=CARTESIAN_POINT('Ctrl Pts',(54.8500772925075,19.0004829399303,15.6107753321542));
#27084=CARTESIAN_POINT('Ctrl Pts',(55.0898157958883,19.0069466924209,15.6251774586414));
#27085=CARTESIAN_POINT('Ctrl Pts',(55.1258346128224,19.0088963392613,15.627366717883));
#27086=CARTESIAN_POINT('Ctrl Pts',(55.1873749884919,19.0139039163861,15.6311640848457));
#27087=CARTESIAN_POINT('Ctrl Pts',(55.2129271045245,19.016480654527,15.6327576236345));
#27088=CARTESIAN_POINT('Ctrl Pts',(55.2489789875215,19.0208208512984,15.6350328265464));
#27089=CARTESIAN_POINT('Ctrl Pts',(55.259525994957,19.0221762237738,15.6357016962004));
#27090=CARTESIAN_POINT('Ctrl Pts',(55.2776517809216,19.0246530079171,15.636857015901));
#27091=CARTESIAN_POINT('Ctrl Pts',(55.2852359360596,19.0257338809846,15.6373421796931));
#27092=CARTESIAN_POINT('Ctrl Pts',(55.2997195491981,19.0278832446124,15.6382721448998));
#27093=CARTESIAN_POINT('Ctrl Pts',(55.3066200054796,19.0289443246694,15.6387167053303));
#27094=CARTESIAN_POINT('Ctrl Pts',(55.3245121673585,19.0317918240676,15.6398733577671));
#27095=CARTESIAN_POINT('Ctrl Pts',(55.3354946183994,19.0336340820527,15.6405872072601));
#27096=CARTESIAN_POINT('Ctrl Pts',(55.366969499728,19.0391852114591,15.6426444666741));
#27097=CARTESIAN_POINT('Ctrl Pts',(55.3874195375099,19.0431230758806,15.6439950729244));
#27098=CARTESIAN_POINT('Ctrl Pts',(55.5695746424837,19.0811660688116,15.656154097486));
#27099=CARTESIAN_POINT('Ctrl Pts',(55.726490755741,19.1349185502859,15.66761913074));
#27100=CARTESIAN_POINT('Ctrl Pts',(55.9643466985291,19.2510120140521,15.6860743573232));
#27101=CARTESIAN_POINT('Ctrl Pts',(56.0503650492637,19.3012767270346,15.6929849056846));
#27102=CARTESIAN_POINT('Ctrl Pts',(56.1463660861621,19.3674666680496,15.7007189508597));
#27103=CARTESIAN_POINT('Ctrl Pts',(56.1603267673647,19.3773595211226,15.7018440168585));
#27104=CARTESIAN_POINT('Ctrl Pts',(56.1793102119633,19.3911819276813,15.7033724649419));
#27105=CARTESIAN_POINT('Ctrl Pts',(56.1844435239027,19.3949574126409,15.7037856299161));
#27106=CARTESIAN_POINT('Ctrl Pts',(56.1930497245641,19.4013509359045,15.7044779539706));
#27107=CARTESIAN_POINT('Ctrl Pts',(56.1965322703681,19.403955826883,15.7047580055549));
#27108=CARTESIAN_POINT('Ctrl Pts',(56.2031360869384,19.4089291437047,15.7052888202313));
#27109=CARTESIAN_POINT('Ctrl Pts',(56.2062589321402,19.4112954010498,15.7055397353665));
#27110=CARTESIAN_POINT('Ctrl Pts',(56.2144500535848,19.4175400925288,15.7061976760657));
#27111=CARTESIAN_POINT('Ctrl Pts',(56.2195067747011,19.4214337136054,15.7066036464607));
#27112=CARTESIAN_POINT('Ctrl Pts',(56.2371288197154,19.4351377148775,15.7080180300434));
#27113=CARTESIAN_POINT('Ctrl Pts',(56.2495955400678,19.4450746924914,15.7090179690062));
#27114=CARTESIAN_POINT('Ctrl Pts',(56.3425424270726,19.5210007662374,15.7164795315619));
#27115=CARTESIAN_POINT('Ctrl Pts',(56.4178772283359,19.5930569827258,15.7225686810504));
#27116=CARTESIAN_POINT('Ctrl Pts',(56.5459493232423,19.736344009908,15.733737998096));
#27117=CARTESIAN_POINT('Ctrl Pts',(56.6002325990108,19.8058304624465,15.7388172137825));
#27118=CARTESIAN_POINT('Ctrl Pts',(56.693438013054,19.9429584678914,15.7485954786565));
#27119=CARTESIAN_POINT('Ctrl Pts',(56.7333325504978,20.0097346900497,15.7532599707987));
#27120=CARTESIAN_POINT('Ctrl Pts',(56.7786199567316,20.096699307806,15.7593239639879));
#27121=CARTESIAN_POINT('Ctrl Pts',(56.7877358534907,20.1148776572217,15.7605907246089));
#27122=CARTESIAN_POINT('Ctrl Pts',(56.8007815396024,20.1419165237639,15.7624752277464));
#27123=CARTESIAN_POINT('Ctrl Pts',(56.8049274160698,20.1506717813744,15.763085476846));
#27124=CARTESIAN_POINT('Ctrl Pts',(56.8121738857521,20.1662675657669,15.7641727507067));
#27125=CARTESIAN_POINT('Ctrl Pts',(56.8152999499695,20.1730961040024,15.7646488870201));
#27126=CARTESIAN_POINT('Ctrl Pts',(56.821788261661,20.187483214042,15.7656523060847));
#27127=CARTESIAN_POINT('Ctrl Pts',(56.8251421917617,20.1950453588913,15.7661798627511));
#27128=CARTESIAN_POINT('Ctrl Pts',(56.8338631098235,20.2150432450993,15.7675754555429));
#27129=CARTESIAN_POINT('Ctrl Pts',(56.8391505714553,20.2275129948412,15.7684461747148));
#27130=CARTESIAN_POINT('Ctrl Pts',(56.8611862392841,20.2809899762186,15.7721830428967));
#27131=CARTESIAN_POINT('Ctrl Pts',(56.8766919126076,20.3224923753097,15.7750904201147));
#27132=CARTESIAN_POINT('Ctrl Pts',(56.9008850360456,20.3944711901988,15.7801485536937));
#27133=CARTESIAN_POINT('Ctrl Pts',(56.9102518419404,20.4247028664337,15.7822775480933));
#27134=CARTESIAN_POINT('Ctrl Pts',(56.9637764852852,20.6132078173788,15.7955749725531));
#27135=CARTESIAN_POINT('Ctrl Pts',(56.9889509824335,20.7761897219217,15.8072399424666));
#27136=CARTESIAN_POINT('Ctrl Pts',(56.9954095805707,20.9922599737663,15.8220352273783));
#27137=CARTESIAN_POINT('Ctrl Pts',(56.9949360426966,21.0441647537622,15.8255325184685));
#27138=CARTESIAN_POINT('Ctrl Pts',(56.9919973395273,21.1051584314049,15.8295323510324));
#27139=CARTESIAN_POINT('Ctrl Pts',(56.991492720431,21.1143173155307,15.8301300373187));
#27140=CARTESIAN_POINT('Ctrl Pts',(56.9906178405321,21.1284242523775,15.8310457664564));
#27141=CARTESIAN_POINT('Ctrl Pts',(56.9902922745852,21.133374805227,15.8313662015449));
#27142=CARTESIAN_POINT('Ctrl Pts',(56.9896583126334,21.1424950594003,15.8319547660829));
#27143=CARTESIAN_POINT('Ctrl Pts',(56.9893552788833,21.1466649854575,15.8322231806606));
#27144=CARTESIAN_POINT('Ctrl Pts',(56.9886415322621,21.1560771170274,15.8328275010635));
#27145=CARTESIAN_POINT('Ctrl Pts',(56.9882232021661,21.1613186604016,15.8331629779209));
#27146=CARTESIAN_POINT('Ctrl Pts',(56.9869268873471,21.1767894595909,15.8341501801768));
#27147=CARTESIAN_POINT('Ctrl Pts',(56.985990634628,21.1870138456729,15.834798753373));
#27148=CARTESIAN_POINT('Ctrl Pts',(56.9778388503983,21.2690552478096,15.8399752858079));
#27149=CARTESIAN_POINT('Ctrl Pts',(56.9668082552577,21.3404482004662,15.8443102160548));
#27150=CARTESIAN_POINT('Ctrl Pts',(56.9273018802228,21.5280300268974,15.8556123745615));
#27151=CARTESIAN_POINT('Ctrl Pts',(56.8922156163492,21.642518338818,15.8624316182027));
#27152=CARTESIAN_POINT('Ctrl Pts',(56.8235955137034,21.8108016259018,15.8731077873845));
#27153=CARTESIAN_POINT('Ctrl Pts',(56.7974176398596,21.8672881821525,15.8768088409536));
#27154=CARTESIAN_POINT('Ctrl Pts',(56.7568188653363,21.9451290613063,15.8821466575709));
#27155=CARTESIAN_POINT('Ctrl Pts',(56.7445590247577,21.9675718010639,15.8837145451998));
#27156=CARTESIAN_POINT('Ctrl Pts',(56.7221218777678,22.0068316089218,15.8865133001155));
#27157=CARTESIAN_POINT('Ctrl Pts',(56.7121209576025,22.0237457859437,15.8877379710291));
#27158=CARTESIAN_POINT('Ctrl Pts',(56.6968880429045,22.0486609687559,15.8895716007625));
#27159=CARTESIAN_POINT('Ctrl Pts',(56.6918455731269,22.0567768965679,15.8901736480195));
#27160=CARTESIAN_POINT('Ctrl Pts',(56.682744427713,22.0711932210145,15.8912517426868));
#27161=CARTESIAN_POINT('Ctrl Pts',(56.6787081609313,22.077507602602,15.8917269558936));
#27162=CARTESIAN_POINT('Ctrl Pts',(56.6701028680966,22.0908041057353,15.8927340874224));
#27163=CARTESIAN_POINT('Ctrl Pts',(56.6655254325671,22.0977805869562,15.8932663131576));
#27164=CARTESIAN_POINT('Ctrl Pts',(56.6532233680654,22.1162761371856,15.8946875839482));
#27165=CARTESIAN_POINT('Ctrl Pts',(56.6454222554634,22.1277435454362,15.8955794922305));
#27166=CARTESIAN_POINT('Ctrl Pts',(56.6104754159754,22.1779797876132,15.8995350519953));
#27167=CARTESIAN_POINT('Ctrl Pts',(56.5820764511271,22.2158539887533,15.9026461518083));
#27168=CARTESIAN_POINT('Ctrl Pts',(56.5322868832193,22.277554746381,15.9079395564349));
#27169=CARTESIAN_POINT('Ctrl Pts',(56.5116201375564,22.3019422460328,15.910094705495));
#27170=CARTESIAN_POINT('Ctrl Pts',(56.3835366004,22.4459229836597,15.9231987164374));
#27171=CARTESIAN_POINT('Ctrl Pts',(56.2625848720434,22.5526552544748,15.9346065389171));
#27172=CARTESIAN_POINT('Ctrl Pts',(56.1016783652932,22.6632876981583,15.947968312459));
#27173=CARTESIAN_POINT('Ctrl Pts',(56.0727039430594,22.6821200072393,15.9503084949259));
#27174=CARTESIAN_POINT('Ctrl Pts',(56.0252272170605,22.7112521738022,15.9540216769226));
#27175=CARTESIAN_POINT('Ctrl Pts',(56.0070254402028,22.7220263350432,15.9554174729121));
#27176=CARTESIAN_POINT('Ctrl Pts',(55.9826532764748,22.7359342871923,15.9572464948717));
#27177=CARTESIAN_POINT('Ctrl Pts',(55.9766338002893,22.7393279549175,15.957695044553));
#27178=CARTESIAN_POINT('Ctrl Pts',(55.9666969727923,22.7448623013406,15.9584301207717));
#27179=CARTESIAN_POINT('Ctrl Pts',(55.9627899149645,22.7470211986254,15.958717785127));
#27180=CARTESIAN_POINT('Ctrl Pts',(55.955118585176,22.7512265437838,15.9592798909439));
#27181=CARTESIAN_POINT('Ctrl Pts',(55.9513549238789,22.7532740027557,15.9595543932637));
#27182=CARTESIAN_POINT('Ctrl Pts',(55.9420710718735,22.7582857893503,15.9602284482935));
#27183=CARTESIAN_POINT('Ctrl Pts',(55.9365433956169,22.7612362965137,15.9606271316407));
#27184=CARTESIAN_POINT('Ctrl Pts',(55.9175182367484,22.7712764572299,15.9619905488729));
#27185=CARTESIAN_POINT('Ctrl Pts',(55.9039530359682,22.7782375951068,15.962947596788));
#27186=CARTESIAN_POINT('Ctrl Pts',(55.7722955602515,22.8439031476453,15.9721043985158));
#27187=CARTESIAN_POINT('Ctrl Pts',(55.648718233845,22.8909241010592,15.9796968742609));
#27188=CARTESIAN_POINT('Ctrl Pts',(55.4045043574775,22.9570558279542,15.9943773613061));
#27189=CARTESIAN_POINT('Ctrl Pts',(55.2850325860818,22.9779848502632,16.0014269554212));
#27190=CARTESIAN_POINT('Ctrl Pts',(55.1644482585673,22.9879598418364,16.0088160704683));
#27191=CARTESIAN_POINT('Origin',(55.,21.,6.22095488139522));
#27192=CARTESIAN_POINT('',(55.164448352281,22.9879598340842,16.9667227887628));
#27193=CARTESIAN_POINT('',(55.1644482145651,22.9879598454763,16.809768216174));
#27194=CARTESIAN_POINT('',(55.1644483516311,22.987959834138,6.22095488139522));
#27195=CARTESIAN_POINT('',(53.0052503038905,21.0011010772302,16.3790451185582));
#27196=CARTESIAN_POINT('Ctrl Pts',(55.164448352281,22.9879598340842,16.9667227887628));
#27197=CARTESIAN_POINT('Ctrl Pts',(55.1692009938859,22.9875666852552,16.9664083972774));
#27198=CARTESIAN_POINT('Ctrl Pts',(55.1739524101488,22.9871564778586,16.9660947938768));
#27199=CARTESIAN_POINT('Ctrl Pts',(55.1875134282772,22.9859366901065,16.9652018433256));
#27200=CARTESIAN_POINT('Ctrl Pts',(55.1963191738424,22.9850855426879,16.9646245499614));
#27201=CARTESIAN_POINT('Ctrl Pts',(55.2105165670934,22.9836178515125,16.9636981958022));
#27202=CARTESIAN_POINT('Ctrl Pts',(55.2159117548901,22.9830378517935,16.9633471983118));
#27203=CARTESIAN_POINT('Ctrl Pts',(55.225473779728,22.9819704175264,16.9627270217624));
#27204=CARTESIAN_POINT('Ctrl Pts',(55.2296415139441,22.9814918464494,16.9624573560035));
#27205=CARTESIAN_POINT('Ctrl Pts',(55.238615882347,22.9804326453078,16.9618780937649));
#27206=CARTESIAN_POINT('Ctrl Pts',(55.2434219164473,22.9798476642679,16.9615687434008));
#27207=CARTESIAN_POINT('Ctrl Pts',(55.2567731786842,22.978173223809,16.9607116378098));
#27208=CARTESIAN_POINT('Ctrl Pts',(55.2653136733424,22.9770458846017,16.9601659608864));
#27209=CARTESIAN_POINT('Ctrl Pts',(55.3144452030712,22.9702364501159,16.9570403652911));
#27210=CARTESIAN_POINT('Ctrl Pts',(55.3548639020246,22.9633592665141,16.9545223625556));
#27211=CARTESIAN_POINT('Ctrl Pts',(55.4901309344792,22.9360293465946,16.9461892884863));
#27212=CARTESIAN_POINT('Ctrl Pts',(55.5836963506633,22.9099056232083,16.9405775967386));
#27213=CARTESIAN_POINT('Ctrl Pts',(55.8040647442482,22.83066124531,16.9269913086181));
#27214=CARTESIAN_POINT('Ctrl Pts',(55.9279867779923,22.7710661630308,16.9190152345749));
#27215=CARTESIAN_POINT('Ctrl Pts',(56.0653447613261,22.6866087935056,16.9090877407181));
#27216=CARTESIAN_POINT('Ctrl Pts',(56.0856486198404,22.6736115675758,16.9075910366386));
#27217=CARTESIAN_POINT('Ctrl Pts',(56.1137002628937,22.6549294302224,16.9054794049525));
#27218=CARTESIAN_POINT('Ctrl Pts',(56.1216506054828,22.6495513355606,16.9048759086679));
#27219=CARTESIAN_POINT('Ctrl Pts',(56.1353649035642,22.6401291629907,16.9038259767214));
#27220=CARTESIAN_POINT('Ctrl Pts',(56.1411468822823,22.6361115263113,16.9033805457489));
#27221=CARTESIAN_POINT('Ctrl Pts',(56.153138781588,22.6276844038495,16.9024508471324));
#27222=CARTESIAN_POINT('Ctrl Pts',(56.159344950756,22.6232698021744,16.9019663887765));
#27223=CARTESIAN_POINT('Ctrl Pts',(56.1739440513228,22.6127586720863,16.9008188336992));
#27224=CARTESIAN_POINT('Ctrl Pts',(56.1823149433281,22.6066320481306,16.9001545828806));
#27225=CARTESIAN_POINT('Ctrl Pts',(56.2099860704517,22.5860462890327,16.8979376195425));
#27226=CARTESIAN_POINT('Ctrl Pts',(56.2290712406905,22.5713029378016,16.8963738688555));
#27227=CARTESIAN_POINT('Ctrl Pts',(56.2738118004669,22.5354268408576,16.8926228891196));
#27228=CARTESIAN_POINT('Ctrl Pts',(56.2992148486119,22.5139922888557,16.8904240795533));
#27229=CARTESIAN_POINT('Ctrl Pts',(56.4508703444832,22.3794002869036,16.8768655771366));
#27230=CARTESIAN_POINT('Ctrl Pts',(56.5627958792803,22.2511685191208,16.8648934034886));
#27231=CARTESIAN_POINT('Ctrl Pts',(56.6962548256279,22.0519908726685,16.8483220833582));
#27232=CARTESIAN_POINT('Ctrl Pts',(56.7322621149789,21.991582272053,16.8435328520369));
#27233=CARTESIAN_POINT('Ctrl Pts',(56.7697706705476,21.9203498178749,16.8382480931461));
#27234=CARTESIAN_POINT('Ctrl Pts',(56.7744629825528,21.9112700740082,16.8375809970704));
#27235=CARTESIAN_POINT('Ctrl Pts',(56.7814593753626,21.8974729014788,16.8365776088219));
#27236=CARTESIAN_POINT('Ctrl Pts',(56.783814876006,21.8927819468527,16.8362382510271));
#27237=CARTESIAN_POINT('Ctrl Pts',(56.788013564466,21.88433734614,16.8356306229828));
#27238=CARTESIAN_POINT('Ctrl Pts',(56.7898634820035,21.880587170739,16.8353619418176));
#27239=CARTESIAN_POINT('Ctrl Pts',(56.7938869304648,21.8723657250095,16.8347754585405));
#27240=CARTESIAN_POINT('Ctrl Pts',(56.7960555401853,21.8678921449888,16.8344579613945));
#27241=CARTESIAN_POINT('Ctrl Pts',(56.8021966100727,21.8551022632328,16.83355475198));
#27242=CARTESIAN_POINT('Ctrl Pts',(56.8061282537045,21.8467663437419,16.8329714971264));
#27243=CARTESIAN_POINT('Ctrl Pts',(56.832217227101,21.7904436923842,16.82906506185));
#27244=CARTESIAN_POINT('Ctrl Pts',(56.8525196391284,21.7416153109182,16.8258456744038));
#27245=CARTESIAN_POINT('Ctrl Pts',(56.9311791830559,21.5289652230822,16.8122949692424));
#27246=CARTESIAN_POINT('Ctrl Pts',(56.9699222991364,21.3587072633161,16.8025473092958));
#27247=CARTESIAN_POINT('Ctrl Pts',(56.9918956429076,21.1235369204037,16.7884454381991));
#27248=CARTESIAN_POINT('Ctrl Pts',(56.9947818396309,21.0612688575145,16.7846604075312));
#27249=CARTESIAN_POINT('Ctrl Pts',(56.994742004622,20.983971465127,16.7798503057266));
#27250=CARTESIAN_POINT('Ctrl Pts',(56.9945650682515,20.9689718180639,16.7789117796303));
#27251=CARTESIAN_POINT('Ctrl Pts',(56.9940186576918,20.9452959064464,16.7774217045518));
#27252=CARTESIAN_POINT('Ctrl Pts',(56.9937616681672,20.9366174174814,16.7768736719055));
#27253=CARTESIAN_POINT('Ctrl Pts',(56.9931786696285,20.9204892840428,16.7758516686435));
#27254=CARTESIAN_POINT('Ctrl Pts',(56.9928675281707,20.913039228937,16.7753781715842));
#27255=CARTESIAN_POINT('Ctrl Pts',(56.9920853600501,20.8965314350179,16.7743258091181));
#27256=CARTESIAN_POINT('Ctrl Pts',(56.991594314281,20.8874748539177,16.7737463267742));
#27257=CARTESIAN_POINT('Ctrl Pts',(56.9899911584643,20.8612205040897,16.7720601110615));
#27258=CARTESIAN_POINT('Ctrl Pts',(56.9887179430646,20.8440337496564,16.7709483688317));
#27259=CARTESIAN_POINT('Ctrl Pts',(56.9742301474694,20.6777435705585,16.7601123378514));
#27260=CARTESIAN_POINT('Ctrl Pts',(56.9444969341449,20.5305870650988,16.749849142564));
#27261=CARTESIAN_POINT('Ctrl Pts',(56.8599975006504,20.2683728634241,16.7306477137786));
#27262=CARTESIAN_POINT('Ctrl Pts',(56.8101381590583,20.1524893418869,16.7218164502821));
#27263=CARTESIAN_POINT('Ctrl Pts',(56.7422183842659,20.0284319769945,16.7124517881987));
#27264=CARTESIAN_POINT('Ctrl Pts',(56.7345920591683,20.0148808468637,16.7114304245822));
#27265=CARTESIAN_POINT('Ctrl Pts',(56.7236453030853,19.9959510269611,16.7100073399107));
#27266=CARTESIAN_POINT('Ctrl Pts',(56.7204568096393,19.9904972313567,16.7095977753863));
#27267=CARTESIAN_POINT('Ctrl Pts',(56.7152544960523,19.9816951139194,16.7089375820725));
#27268=CARTESIAN_POINT('Ctrl Pts',(56.7132566850449,19.978337453443,16.7086859388631));
#27269=CARTESIAN_POINT('Ctrl Pts',(56.7090062536041,19.9712414098123,16.7081545671353));
#27270=CARTESIAN_POINT('Ctrl Pts',(56.706751203372,19.9675045074013,16.7078750038496));
#27271=CARTESIAN_POINT('Ctrl Pts',(56.7011366164711,19.9582690875789,16.7071846723091));
#27272=CARTESIAN_POINT('Ctrl Pts',(56.697762633779,19.9527793337171,16.7067748377424));
#27273=CARTESIAN_POINT('Ctrl Pts',(56.6850753347306,19.9323585117788,16.7052518831588));
#27274=CARTESIAN_POINT('Ctrl Pts',(56.6755908484767,19.9175340236898,16.7041494032243));
#27275=CARTESIAN_POINT('Ctrl Pts',(56.6511350026874,19.8804007616584,16.7013905816269));
#27276=CARTESIAN_POINT('Ctrl Pts',(56.6359065034463,19.8582647826906,16.6997485210992));
#27277=CARTESIAN_POINT('Ctrl Pts',(56.5172455584056,19.6930314137088,16.6874562583192));
#27278=CARTESIAN_POINT('Ctrl Pts',(56.3956665757374,19.5639194193307,16.6775814557249));
#27279=CARTESIAN_POINT('Ctrl Pts',(56.2368861875563,19.4347752909524,16.6654349612381));
#27280=CARTESIAN_POINT('Ctrl Pts',(56.2147340674437,19.4175219162812,16.6637567420029));
#27281=CARTESIAN_POINT('Ctrl Pts',(56.1540501191195,19.372282822589,16.6591911215947));
#27282=CARTESIAN_POINT('Ctrl Pts',(56.114870265604,19.3452013337919,16.6562763333413));
#27283=CARTESIAN_POINT('Ctrl Pts',(56.0630498502284,19.3120586974552,16.6524418759761));
#27284=CARTESIAN_POINT('Ctrl Pts',(56.0512606494066,19.30469122092,16.6515709118317));
#27285=CARTESIAN_POINT('Ctrl Pts',(56.0322663016953,19.2930953114743,16.6501693698176));
#27286=CARTESIAN_POINT('Ctrl Pts',(56.0251097901661,19.2887877840569,16.6496416974955));
#27287=CARTESIAN_POINT('Ctrl Pts',(56.0114806703002,19.2807005512516,16.6486374075272));
#27288=CARTESIAN_POINT('Ctrl Pts',(56.005013385158,19.2769121223814,16.6481611179534));
#27289=CARTESIAN_POINT('Ctrl Pts',(55.9902604337306,19.2683813999167,16.6470751445737));
#27290=CARTESIAN_POINT('Ctrl Pts',(55.9819618142033,19.2636619876952,16.6464646494043));
#27291=CARTESIAN_POINT('Ctrl Pts',(55.9565240021682,19.249436229654,16.6445942311671));
#27292=CARTESIAN_POINT('Ctrl Pts',(55.9392787230937,19.2401229828121,16.6433274772234));
#27293=CARTESIAN_POINT('Ctrl Pts',(55.7994760401723,19.1672632845178,16.6330652475449));
#27294=CARTESIAN_POINT('Ctrl Pts',(55.6707831660314,19.1163539614051,16.6236218065157));
#27295=CARTESIAN_POINT('Ctrl Pts',(55.4086661765892,19.042954192605,16.6046687614064));
#27296=CARTESIAN_POINT('Ctrl Pts',(55.2761091690908,19.0198975414158,16.5952240105739));
#27297=CARTESIAN_POINT('Ctrl Pts',(55.1271090824598,19.0092461877652,16.5853385427881));
#27298=CARTESIAN_POINT('Ctrl Pts',(55.1119729223528,19.0083374889978,16.5843429435877));
#27299=CARTESIAN_POINT('Ctrl Pts',(55.0912016265966,19.0073280377456,16.5829898176994));
#27300=CARTESIAN_POINT('Ctrl Pts',(55.0855747022773,19.0070784616458,16.5826245776483));
#27301=CARTESIAN_POINT('Ctrl Pts',(55.0759581087713,19.0066927324711,16.5820027127483));
#27302=CARTESIAN_POINT('Ctrl Pts',(55.0719689887494,19.0065447177287,16.5817454413407));
#27303=CARTESIAN_POINT('Ctrl Pts',(55.0636967529413,19.0062626430168,16.5812134022792));
#27304=CARTESIAN_POINT('Ctrl Pts',(55.0594136292264,19.0061304089862,16.5809387470931));
#27305=CARTESIAN_POINT('Ctrl Pts',(55.0490936678046,19.0058450811369,16.5802788886029));
#27306=CARTESIAN_POINT('Ctrl Pts',(55.043056432992,19.0057055948272,16.5798944391587));
#27307=CARTESIAN_POINT('Ctrl Pts',(55.0220921888015,19.0053164734428,16.578564609522));
#27308=CARTESIAN_POINT('Ctrl Pts',(55.0071626477137,19.0052069872387,16.5776266750933));
#27309=CARTESIAN_POINT('Ctrl Pts',(54.917293458193,19.0055569260401,16.5720279247323));
#27310=CARTESIAN_POINT('Ctrl Pts',(54.8424214330629,19.0100716007706,16.5675600042198));
#27311=CARTESIAN_POINT('Ctrl Pts',(54.7379279784377,19.0223091880352,16.5613862278743));
#27312=CARTESIAN_POINT('Ctrl Pts',(54.7079656367682,19.0265110379746,16.559623328537));
#27313=CARTESIAN_POINT('Ctrl Pts',(54.5182033169,19.057539366651,16.5484468153891));
#27314=CARTESIAN_POINT('Ctrl Pts',(54.3620974008528,19.1030668153155,16.5391392346602));
#27315=CARTESIAN_POINT('Ctrl Pts',(54.1921499278254,19.1760121731134,16.5277389116158));
#27316=CARTESIAN_POINT('Ctrl Pts',(54.1712374394313,19.1854185378954,16.5263140528486));
#27317=CARTESIAN_POINT('Ctrl Pts',(54.1419890983342,19.1991854120023,16.5242878696667));
#27318=CARTESIAN_POINT('Ctrl Pts',(54.1335143178166,19.2032478063324,16.5236967738899));
#27319=CARTESIAN_POINT('Ctrl Pts',(54.1187861915353,19.210436182173,16.5226623690225));
#27320=CARTESIAN_POINT('Ctrl Pts',(54.1125199362212,19.2135354555224,16.5222199918878));
#27321=CARTESIAN_POINT('Ctrl Pts',(54.0995617657419,19.2200295355763,16.5213003891382));
#27322=CARTESIAN_POINT('Ctrl Pts',(54.0928724652831,19.2234292861906,16.5208229959894));
#27323=CARTESIAN_POINT('Ctrl Pts',(54.0770816103596,19.2315672204121,16.5196896267859));
#27324=CARTESIAN_POINT('Ctrl Pts',(54.0679971897672,19.2363380128089,16.5190325107134));
#27325=CARTESIAN_POINT('Ctrl Pts',(54.048796528662,19.2466112446011,16.517632631883));
#27326=CARTESIAN_POINT('Ctrl Pts',(54.0386903527454,19.2521316055534,16.5168892502653));
#27327=CARTESIAN_POINT('Ctrl Pts',(54.0112721417145,19.2674181523139,16.5148542450719));
#27328=CARTESIAN_POINT('Ctrl Pts',(53.9940577480851,19.2773558767347,16.5135565783449));
#27329=CARTESIAN_POINT('Ctrl Pts',(53.9399395243347,19.3096856762955,16.5094122072797));
#27330=CARTESIAN_POINT('Ctrl Pts',(53.9036145453936,19.3330179339152,16.5065329230525));
#27331=CARTESIAN_POINT('Ctrl Pts',(53.7407008959973,19.4452898824258,16.4931670650648));
#27332=CARTESIAN_POINT('Ctrl Pts',(53.6239757863481,19.5475863994228,16.4822395871003));
#27333=CARTESIAN_POINT('Ctrl Pts',(53.5026158694608,19.6818344082034,16.4697438130851));
#27334=CARTESIAN_POINT('Ctrl Pts',(53.485359817934,19.7016991986294,16.4679370865997));
#27335=CARTESIAN_POINT('Ctrl Pts',(53.4407229885164,19.755185824174,16.4631938762394));
#27336=CARTESIAN_POINT('Ctrl Pts',(53.4140347933791,19.7893711831262,16.4602846732763));
#27337=CARTESIAN_POINT('Ctrl Pts',(53.3835952187077,19.8310980181733,16.4569013550973));
#27338=CARTESIAN_POINT('Ctrl Pts',(53.3787521612786,19.8378245781031,16.4563609742489));
#27339=CARTESIAN_POINT('Ctrl Pts',(53.3709054811579,19.8488674021876,16.4554822826097));
#27340=CARTESIAN_POINT('Ctrl Pts',(53.3678768066826,19.8531656211811,16.4551423361829));
#27341=CARTESIAN_POINT('Ctrl Pts',(53.3624697575195,19.8609039735684,16.4545340864696));
#27342=CARTESIAN_POINT('Ctrl Pts',(53.3600851843463,19.8643396410598,16.4542653684119));
#27343=CARTESIAN_POINT('Ctrl Pts',(53.3548937345172,19.8718698744083,16.4536793087167));
#27344=CARTESIAN_POINT('Ctrl Pts',(53.3520913359052,19.8759674199143,16.4533622688072));
#27345=CARTESIAN_POINT('Ctrl Pts',(53.3441490531959,19.8876738267091,16.452461669025));
#27346=CARTESIAN_POINT('Ctrl Pts',(53.3390462886722,19.8953078934184,16.4518805443269));
#27347=CARTESIAN_POINT('Ctrl Pts',(53.3053656082326,19.9464573615876,16.4480260052497));
#27348=CARTESIAN_POINT('Ctrl Pts',(53.2784452242897,19.9910460821894,16.4448532469008));
#27349=CARTESIAN_POINT('Ctrl Pts',(53.1674216491063,20.1923470796031,16.4311052411632));
#27350=CARTESIAN_POINT('Ctrl Pts',(53.1027473074923,20.3588393303913,16.4211498793913));
#27351=CARTESIAN_POINT('Ctrl Pts',(53.0492599558051,20.5803090361699,16.4075228954763));
#27352=CARTESIAN_POINT('Ctrl Pts',(53.0393547499554,20.6293292144935,16.4044897790563));
#27353=CARTESIAN_POINT('Ctrl Pts',(53.0279513405126,20.6991940287121,16.4001139789896));
#27354=CARTESIAN_POINT('Ctrl Pts',(53.0249222454511,20.7197715922117,16.3988188233113));
#27355=CARTESIAN_POINT('Ctrl Pts',(53.0209567938934,20.7499818078036,16.396906556824));
#27356=CARTESIAN_POINT('Ctrl Pts',(53.0197678201504,20.7595803322233,16.3962973910627));
#27357=CARTESIAN_POINT('Ctrl Pts',(53.0177772108139,20.7766681747287,16.395209930527));
#27358=CARTESIAN_POINT('Ctrl Pts',(53.0169480952719,20.7841541504632,16.3947325093959));
#27359=CARTESIAN_POINT('Ctrl Pts',(53.0154314506239,20.7985947534022,16.393809520598));
#27360=CARTESIAN_POINT('Ctrl Pts',(53.0147380335559,20.8055486614254,16.3933641455118));
#27361=CARTESIAN_POINT('Ctrl Pts',(53.0133242675411,20.8205231379393,16.3924030695235));
#27362=CARTESIAN_POINT('Ctrl Pts',(53.0126159195606,20.8285446891409,16.3918869994485));
#27363=CARTESIAN_POINT('Ctrl Pts',(53.0110196869293,20.8479620823592,16.3906346898616));
#27364=CARTESIAN_POINT('Ctrl Pts',(53.0101811533913,20.8593615883424,16.3898969205667));
#27365=CARTESIAN_POINT('Ctrl Pts',(53.0066214187238,20.9141919281727,16.3863356068006));
#27366=CARTESIAN_POINT('Ctrl Pts',(53.005224130425,20.9576934333355,16.383471389899));
#27367=CARTESIAN_POINT('Ctrl Pts',(53.0052503625455,21.0012026534312,16.3805665413763));
#27368=CARTESIAN_POINT('Ctrl Pts',(55.1644483516311,22.987959834138,16.1684645359809));
#27369=CARTESIAN_POINT('Ctrl Pts',(55.0949564505043,22.9937083550063,16.1729106515113));
#27370=CARTESIAN_POINT('Ctrl Pts',(55.0252269405976,22.9958034934844,16.1773567670417));
#27371=CARTESIAN_POINT('Ctrl Pts',(54.9556709906544,22.9942573809392,16.1818028825721));
#27372=CARTESIAN_POINT('Ctrl Pts',(54.8859941619893,22.992708581462,16.1862567248428));
#27373=CARTESIAN_POINT('Ctrl Pts',(54.8164919833358,22.9875059359452,16.1907105671135));
#27374=CARTESIAN_POINT('Ctrl Pts',(54.7475705257622,22.978713451472,16.1951644093842));
#27375=CARTESIAN_POINT('Ctrl Pts',(54.7114345318024,22.9741034914247,16.1974995895017));
#27376=CARTESIAN_POINT('Ctrl Pts',(54.6754580112511,22.9685075475329,16.1998347696191));
#27377=CARTESIAN_POINT('Ctrl Pts',(54.639698020522,22.9619403778108,16.2021699497366));
#27378=CARTESIAN_POINT('Ctrl Pts',(54.5714823409985,22.9494128593185,16.2066245341835));
#27379=CARTESIAN_POINT('Ctrl Pts',(54.5037861158996,22.9332986294088,16.2110791186304));
#27380=CARTESIAN_POINT('Ctrl Pts',(54.4370150511099,22.9136550132726,16.2155337030772));
#27381=CARTESIAN_POINT('Ctrl Pts',(54.3703441575992,22.8940408668798,16.219981604668));
#27382=CARTESIAN_POINT('Ctrl Pts',(54.3045961353565,22.8709079803606,16.2244295062587));
#27383=CARTESIAN_POINT('Ctrl Pts',(54.240167082901,22.8443647959644,16.2288774078494));
#27384=CARTESIAN_POINT('Ctrl Pts',(54.1758137822046,22.8178528194291,16.2333200798681));
#27385=CARTESIAN_POINT('Ctrl Pts',(54.1127768216026,22.7879386942306,16.2377627518869));
#27386=CARTESIAN_POINT('Ctrl Pts',(54.0514359710254,22.7547802840913,16.2422054239056));
#27387=CARTESIAN_POINT('Ctrl Pts',(53.9901336881627,22.7216427221157,16.2466453026193));
#27388=CARTESIAN_POINT('Ctrl Pts',(53.9305258293109,22.6852651539973,16.2510851813329));
#27389=CARTESIAN_POINT('Ctrl Pts',(53.8729696481371,22.6458524078665,16.2555250600466));
#27390=CARTESIAN_POINT('Ctrl Pts',(53.8154301113842,22.6064510593356,16.2599636548112));
#27391=CARTESIAN_POINT('Ctrl Pts',(53.7599414780685,22.5640165516394,16.2644022495757));
#27392=CARTESIAN_POINT('Ctrl Pts',(53.706832450642,22.5187973043785,16.2688408443403));
#27393=CARTESIAN_POINT('Ctrl Pts',(53.6537207484914,22.4735757797456,16.2732796626453));
#27394=CARTESIAN_POINT('Ctrl Pts',(53.6029892612418,22.425569556217,16.2777184809502));
#27395=CARTESIAN_POINT('Ctrl Pts',(53.5549326198038,22.3750664817357,16.2821572992552));
#27396=CARTESIAN_POINT('Ctrl Pts',(53.5068251361222,22.3245099767703,16.2866008136745));
#27397=CARTESIAN_POINT('Ctrl Pts',(53.4613984845393,22.2714517037136,16.2910443280939));
#27398=CARTESIAN_POINT('Ctrl Pts',(53.4189088213326,22.2162147208615,16.2954878425132));
#27399=CARTESIAN_POINT('Ctrl Pts',(53.3763943093178,22.1609454343129,16.2999339555889));
#27400=CARTESIAN_POINT('Ctrl Pts',(53.3368204821056,22.103495305066,16.3043800686647));
#27401=CARTESIAN_POINT('Ctrl Pts',(53.3004001250256,22.0442163700532,16.3088261817404));
#27402=CARTESIAN_POINT('Ctrl Pts',(53.2639164660232,21.9848344028122,16.3132800225686));
#27403=CARTESIAN_POINT('Ctrl Pts',(53.2305974519699,21.9236177146054,16.3177338633969));
#27404=CARTESIAN_POINT('Ctrl Pts',(53.2006095188318,21.8609421924736,16.3221877042251));
#27405=CARTESIAN_POINT('Ctrl Pts',(53.1848641910595,21.8280340679049,16.3245262176319));
#27406=CARTESIAN_POINT('Ctrl Pts',(53.1700363772471,21.7947240924266,16.3268647310387));
#27407=CARTESIAN_POINT('Ctrl Pts',(53.1561446966371,21.7610684481441,16.3292032444456));
#27408=CARTESIAN_POINT('Ctrl Pts',(53.1265894763852,21.6894644423068,16.3341785444644));
#27409=CARTESIAN_POINT('Ctrl Pts',(53.1011757332561,21.6160560788944,16.3391538444832));
#27410=CARTESIAN_POINT('Ctrl Pts',(53.0801012621631,21.5413098917924,16.3441291445021));
#27411=CARTESIAN_POINT('Ctrl Pts',(53.0591002696496,21.4668243159117,16.3490870975623));
#27412=CARTESIAN_POINT('Ctrl Pts',(53.042408496276,21.3910104768948,16.3540450506225));
#27413=CARTESIAN_POINT('Ctrl Pts',(53.0301750919772,21.314352340906,16.3590030036827));
#27414=CARTESIAN_POINT('Ctrl Pts',(53.0180122992591,21.2381366780028,16.3639323392875));
#27415=CARTESIAN_POINT('Ctrl Pts',(53.0102566807941,21.1610867026744,16.3688616748924));
#27416=CARTESIAN_POINT('Ctrl Pts',(53.0070066496492,21.0836962840125,16.3737910104972));
#27417=CARTESIAN_POINT('Ctrl Pts',(53.0058519291347,21.0561998385727,16.3755423798508));
#27418=CARTESIAN_POINT('Ctrl Pts',(53.0052655163887,21.0286605665352,16.3772937492045));
#27419=CARTESIAN_POINT('Ctrl Pts',(53.0052503038905,21.0011010772302,16.3790451185582));
#27420=CARTESIAN_POINT('Ctrl Pts',(55.1644482585673,22.9879598418364,16.0088160704683));
#27421=CARTESIAN_POINT('Ctrl Pts',(55.1457889506031,22.989503379405,16.0099594675921));
#27422=CARTESIAN_POINT('Ctrl Pts',(55.1271029719689,22.9907846175602,16.0111105027836));
#27423=CARTESIAN_POINT('Ctrl Pts',(55.0885664790205,22.9928818093192,16.013498622497));
#27424=CARTESIAN_POINT('Ctrl Pts',(55.06872277886,22.9936647317237,16.0147361448708));
#27425=CARTESIAN_POINT('Ctrl Pts',(55.0392785788694,22.994386329206,16.0165853219081));
#27426=CARTESIAN_POINT('Ctrl Pts',(55.029684485984,22.9945521961065,16.0171898897632));
#27427=CARTESIAN_POINT('Ctrl Pts',(55.012591174321,22.9947243565124,16.0182707931545));
#27428=CARTESIAN_POINT('Ctrl Pts',(55.0050923645821,22.9947575946588,16.0187462778363));
#27429=CARTESIAN_POINT('Ctrl Pts',(54.9892722264279,22.9947385099822,16.019752208976));
#27430=CARTESIAN_POINT('Ctrl Pts',(54.9809510746703,22.9946764006515,16.0202829523085));
#27431=CARTESIAN_POINT('Ctrl Pts',(54.9588658666389,22.9943733478775,16.0216960681835));
#27432=CARTESIAN_POINT('Ctrl Pts',(54.9451036948436,22.9940419874137,16.0225812462238));
#27433=CARTESIAN_POINT('Ctrl Pts',(54.8850280974205,22.9919731292414,16.0264661235822));
#27434=CARTESIAN_POINT('Ctrl Pts',(54.8387830086853,22.9887644352494,16.0295112098734));
#27435=CARTESIAN_POINT('Ctrl Pts',(54.7591401374331,22.9804424463828,16.0348535462997));
#27436=CARTESIAN_POINT('Ctrl Pts',(54.7256816112575,22.9760857719085,16.0371279668841));
#27437=CARTESIAN_POINT('Ctrl Pts',(54.5216007139205,22.9442293553838,16.0511777547821));
#27438=CARTESIAN_POINT('Ctrl Pts',(54.3550595163861,22.895504348459,16.0634895911408));
#27439=CARTESIAN_POINT('Ctrl Pts',(54.1725059008658,22.8152109195625,16.0770257718055));
#27440=CARTESIAN_POINT('Ctrl Pts',(54.1483379122983,22.8039980593172,16.0788167511038));
#27441=CARTESIAN_POINT('Ctrl Pts',(54.1086890281423,22.784628275968,16.0817449757792));
#27442=CARTESIAN_POINT('Ctrl Pts',(54.0930783862331,22.7767460619921,16.0828952554278));
#27443=CARTESIAN_POINT('Ctrl Pts',(54.0718746616439,22.7656874635857,16.0844520305494));
#27444=CARTESIAN_POINT('Ctrl Pts',(54.0661908340431,22.7626880912674,16.0848687758715));
#27445=CARTESIAN_POINT('Ctrl Pts',(54.0566752679509,22.757607755675,16.0855654000156));
#27446=CARTESIAN_POINT('Ctrl Pts',(54.052835716761,22.755541624276,16.085846195349));
#27447=CARTESIAN_POINT('Ctrl Pts',(54.0455672927288,22.7515995676119,16.0863771494168));
#27448=CARTESIAN_POINT('Ctrl Pts',(54.0421371184375,22.7497261324949,16.0866274673211));
#27449=CARTESIAN_POINT('Ctrl Pts',(54.03316649505,22.7447924224116,16.0872814927629));
#27450=CARTESIAN_POINT('Ctrl Pts',(54.0276350120165,22.7417158081494,16.0876841692534));
#27451=CARTESIAN_POINT('Ctrl Pts',(54.0084975014811,22.7309519261793,16.0890755366784));
#27452=CARTESIAN_POINT('Ctrl Pts',(53.9949668246376,22.723130908364,16.0900561136177));
#27453=CARTESIAN_POINT('Ctrl Pts',(53.87478628257,22.6517667126262,16.0987501399567));
#27454=CARTESIAN_POINT('Ctrl Pts',(53.7741781525531,22.5785463603168,16.1059285814372));
#27455=CARTESIAN_POINT('Ctrl Pts',(53.603251589636,22.4278894387557,16.1191470705425));
#27456=CARTESIAN_POINT('Ctrl Pts',(53.5309475554904,22.3533873067313,16.1251595485079));
#27457=CARTESIAN_POINT('Ctrl Pts',(53.4306264773859,22.2324581660068,16.134603087711));
#27458=CARTESIAN_POINT('Ctrl Pts',(53.3981591576725,22.1899544245668,16.1378684833555));
#27459=CARTESIAN_POINT('Ctrl Pts',(53.3594667012605,22.1348438701116,16.1420661687461));
#27460=CARTESIAN_POINT('Ctrl Pts',(53.3516121522717,22.1234044693955,16.1429355520399));
#27461=CARTESIAN_POINT('Ctrl Pts',(53.3392258182463,22.1049553521019,16.1443350513175));
#27462=CARTESIAN_POINT('Ctrl Pts',(53.3346174785919,22.0979973892846,16.144862275591));
#27463=CARTESIAN_POINT('Ctrl Pts',(53.3259542686719,22.0847371158717,16.1458660367145));
#27464=CARTESIAN_POINT('Ctrl Pts',(53.3218909760959,22.078440458489,16.1463422478664));
#27465=CARTESIAN_POINT('Ctrl Pts',(53.312729314577,22.0640659940059,16.147428491456));
#27466=CARTESIAN_POINT('Ctrl Pts',(53.3076533244991,22.0559742090416,16.1480393381325));
#27467=CARTESIAN_POINT('Ctrl Pts',(53.2946342094077,22.034885067494,16.1496298877366));
#27468=CARTESIAN_POINT('Ctrl Pts',(53.2867816135123,22.0218328246239,16.1506128670995));
#27469=CARTESIAN_POINT('Ctrl Pts',(53.2296205148942,21.9243107983856,16.1579483172394));
#27470=CARTESIAN_POINT('Ctrl Pts',(53.1864421929583,21.8364191017131,16.164519497285));
#27471=CARTESIAN_POINT('Ctrl Pts',(53.0862567539958,21.5878639483914,16.1829444895923));
#27472=CARTESIAN_POINT('Ctrl Pts',(53.0430946428215,21.4225134798834,16.1950806723162));
#27473=CARTESIAN_POINT('Ctrl Pts',(53.019560450095,21.2389708759667,16.207429839885));
#27474=CARTESIAN_POINT('Ctrl Pts',(53.0178369812036,21.224226863223,16.2084136164476));
#27475=CARTESIAN_POINT('Ctrl Pts',(53.0151045608743,21.1983496313746,16.2101242684407));
#27476=CARTESIAN_POINT('Ctrl Pts',(53.0140243256173,21.1872247716244,16.2108545328205));
#27477=CARTESIAN_POINT('Ctrl Pts',(53.012563477568,21.1707409752606,16.2119283601322));
#27478=CARTESIAN_POINT('Ctrl Pts',(53.0121109345581,21.1653888643838,16.2122757404523));
#27479=CARTESIAN_POINT('Ctrl Pts',(53.0113439388647,21.1558594884621,16.2128918921499));
#27480=CARTESIAN_POINT('Ctrl Pts',(53.0110210213271,21.1516830021988,16.2131611271738));
#27481=CARTESIAN_POINT('Ctrl Pts',(53.0103506777345,21.1426426084044,16.2137421494669));
#27482=CARTESIAN_POINT('Ctrl Pts',(53.0100079292455,21.1377784413014,16.2140536741187));
#27483=CARTESIAN_POINT('Ctrl Pts',(53.0091136985282,21.1243877079883,16.2149083929715));
#27484=CARTESIAN_POINT('Ctrl Pts',(53.0085991502623,21.1158586603934,16.2154495736587));
#27485=CARTESIAN_POINT('Ctrl Pts',(53.0062315447716,21.0719184875,16.2182222715861));
#27486=CARTESIAN_POINT('Ctrl Pts',(53.005268012528,21.0364634276237,16.220408186291));
#27487=CARTESIAN_POINT('Ctrl Pts',(53.0052114627833,20.9235559606981,16.2272590344726));
#27488=CARTESIAN_POINT('Ctrl Pts',(53.0096826393143,20.8461699327346,16.231791070704));
#27489=CARTESIAN_POINT('Ctrl Pts',(53.0376471964672,20.6060655371141,16.2458467845655));
#27490=CARTESIAN_POINT('Ctrl Pts',(53.0767300789211,20.4458884136019,16.255272797407));
#27491=CARTESIAN_POINT('Ctrl Pts',(53.1432410906208,20.270607673638,16.2668316519313));
#27492=CARTESIAN_POINT('Ctrl Pts',(53.1518577358801,20.2490426677452,16.2682751043158));
#27493=CARTESIAN_POINT('Ctrl Pts',(53.1644092478992,20.2191551260109,16.2703077732677));
#27494=CARTESIAN_POINT('Ctrl Pts',(53.1680284209469,20.2107014155392,16.2708863488285));
#27495=CARTESIAN_POINT('Ctrl Pts',(53.1747591454076,20.1952754035754,16.2719489257832));
#27496=CARTESIAN_POINT('Ctrl Pts',(53.1778525359606,20.1882953307888,16.2724323022653));
#27497=CARTESIAN_POINT('Ctrl Pts',(53.1841974042331,20.1741975246071,16.2734138946782));
#27498=CARTESIAN_POINT('Ctrl Pts',(53.1874508439226,20.1670808267956,16.2739121712414));
#27499=CARTESIAN_POINT('Ctrl Pts',(53.1955770116634,20.1495784302649,16.2751445222893));
#27500=CARTESIAN_POINT('Ctrl Pts',(53.2004975722282,20.1392153751135,16.2758802367237));
#27501=CARTESIAN_POINT('Ctrl Pts',(53.2191328965773,20.1008262304549,16.278628594994));
#27502=CARTESIAN_POINT('Ctrl Pts',(53.2334146535228,20.0730819135206,16.280660813995));
#27503=CARTESIAN_POINT('Ctrl Pts',(53.2706802502663,20.0046803400512,16.2857900156761));
#27504=CARTESIAN_POINT('Ctrl Pts',(53.2944512999519,19.9644754515107,16.2889131877857));
#27505=CARTESIAN_POINT('Ctrl Pts',(53.4153373850623,19.7754865697994,16.3041177557704));
#27506=CARTESIAN_POINT('Ctrl Pts',(53.5306127163732,19.6393095934495,16.3167788658583));
#27507=CARTESIAN_POINT('Ctrl Pts',(53.6929151901574,19.4926012712055,16.331650335323));
#27508=CARTESIAN_POINT('Ctrl Pts',(53.7242983911151,19.4659505916624,16.3344083711954));
#27509=CARTESIAN_POINT('Ctrl Pts',(53.7628670143991,19.4352009290907,16.3376385935785));
#27510=CARTESIAN_POINT('Ctrl Pts',(53.769279073216,19.4301528220171,16.3381705209695));
#27511=CARTESIAN_POINT('Ctrl Pts',(53.779841816629,19.4219414461249,16.3390382089016));
#27512=CARTESIAN_POINT('Ctrl Pts',(53.7839741802801,19.4187549212141,16.3393755394956));
#27513=CARTESIAN_POINT('Ctrl Pts',(53.7914383943204,19.4130457247644,16.3399809625644));
#27514=CARTESIAN_POINT('Ctrl Pts',(53.7947656909792,19.4105172892665,16.3402494530888));
#27515=CARTESIAN_POINT('Ctrl Pts',(53.8020869206996,19.4049900439929,16.3408371885131));
#27516=CARTESIAN_POINT('Ctrl Pts',(53.8060841713356,19.4019957757557,16.34115611786));
#27517=CARTESIAN_POINT('Ctrl Pts',(53.8175791558619,19.3934522983513,16.3420677915827));
#27518=CARTESIAN_POINT('Ctrl Pts',(53.8251047437251,19.3879405360954,16.3426580048986));
#27519=CARTESIAN_POINT('Ctrl Pts',(53.8777816013139,19.3499246865882,16.3467454085895));
#27520=CARTESIAN_POINT('Ctrl Pts',(53.9242412615003,19.31926591777,16.3501274585887));
#27521=CARTESIAN_POINT('Ctrl Pts',(54.0549708930179,19.2406426252822,16.3592251429767));
#27522=CARTESIAN_POINT('Ctrl Pts',(54.1415488574591,19.1968133497588,16.3648035508219));
#27523=CARTESIAN_POINT('Ctrl Pts',(54.3534521741567,19.1082750677843,16.3781430333399));
#27524=CARTESIAN_POINT('Ctrl Pts',(54.4807143850366,19.0694604406214,16.3859326024104));
#27525=CARTESIAN_POINT('Ctrl Pts',(54.6260522568909,19.0405536513744,16.395130678593));
#27526=CARTESIAN_POINT('Ctrl Pts',(54.6412600799103,19.0377124175135,16.3960963192744));
#27527=CARTESIAN_POINT('Ctrl Pts',(54.6659791115634,19.0333911863508,16.3976717178932));
#27528=CARTESIAN_POINT('Ctrl Pts',(54.675470869626,19.0318025967531,16.3982780355323));
#27529=CARTESIAN_POINT('Ctrl Pts',(54.6923817387835,19.0290979598449,16.399360895248));
#27530=CARTESIAN_POINT('Ctrl Pts',(54.6997963992206,19.0279549594167,16.3998365749015));
#27531=CARTESIAN_POINT('Ctrl Pts',(54.7154333123549,19.0256346962244,16.4008417044252));
#27532=CARTESIAN_POINT('Ctrl Pts',(54.723656805477,19.0244669104591,16.4013714439846));
#27533=CARTESIAN_POINT('Ctrl Pts',(54.7454592099145,19.0215096321512,16.4027790394612));
#27534=CARTESIAN_POINT('Ctrl Pts',(54.7590494791707,19.0198086000397,16.4036596620654));
#27535=CARTESIAN_POINT('Ctrl Pts',(54.8236584247461,19.0123967445265,16.4078621950756));
#27536=CARTESIAN_POINT('Ctrl Pts',(54.8748635201592,19.0085173571559,16.4112408832987));
#27537=CARTESIAN_POINT('Ctrl Pts',(55.0990859493058,19.0002113142077,16.4262556258336));
#27538=CARTESIAN_POINT('Ctrl Pts',(55.2720999440669,19.0163373238995,16.4384970524789));
#27539=CARTESIAN_POINT('Ctrl Pts',(55.4605248569908,19.0590330781742,16.451824864577));
#27540=CARTESIAN_POINT('Ctrl Pts',(55.4801601745615,19.0637970192429,16.4532124640954));
#27541=CARTESIAN_POINT('Ctrl Pts',(55.5451225170653,19.0806072815599,16.45779257595));
#27542=CARTESIAN_POINT('Ctrl Pts',(55.5901006235765,19.0939546155396,16.460946542983));
#27543=CARTESIAN_POINT('Ctrl Pts',(55.6426049299667,19.1115725339209,16.4645757495137));
#27544=CARTESIAN_POINT('Ctrl Pts',(55.6506227064949,19.1143198864729,16.4651284776957));
#27545=CARTESIAN_POINT('Ctrl Pts',(55.6636387322246,19.1188728292564,16.4660230887076));
#27546=CARTESIAN_POINT('Ctrl Pts',(55.6686476066829,19.1206474042688,16.466366705827));
#27547=CARTESIAN_POINT('Ctrl Pts',(55.6775880103507,19.1238551334369,16.4669787924025));
#27548=CARTESIAN_POINT('Ctrl Pts',(55.6815221667754,19.1252806585091,16.4672477010287));
#27549=CARTESIAN_POINT('Ctrl Pts',(55.6900701921505,19.1284084643146,16.4678310216155));
#27550=CARTESIAN_POINT('Ctrl Pts',(55.6946822540327,19.1301154276973,16.4681451521033));
#27551=CARTESIAN_POINT('Ctrl Pts',(55.7076888940472,19.1349840603751,16.4690294770064));
#27552=CARTESIAN_POINT('Ctrl Pts',(55.7160686529637,19.1381853697941,16.4695973719998));
#27553=CARTESIAN_POINT('Ctrl Pts',(55.7687123792409,19.1587047971324,16.4731550793167));
#27554=CARTESIAN_POINT('Ctrl Pts',(55.8123710089035,19.1775453629133,16.4760611975641));
#27555=CARTESIAN_POINT('Ctrl Pts',(55.9172009039299,19.2273008779699,16.4830268194116));
#27556=CARTESIAN_POINT('Ctrl Pts',(55.9775332045311,19.2598420691,16.4870259601096));
#27557=CARTESIAN_POINT('Ctrl Pts',(56.1728184389423,19.3785403082978,16.5003053403762));
#27558=CARTESIAN_POINT('Ctrl Pts',(56.2990479960508,19.477796743011,16.5095064997491));
#27559=CARTESIAN_POINT('Ctrl Pts',(56.4283795654249,19.6074149562052,16.5207916209559));
#27560=CARTESIAN_POINT('Ctrl Pts',(56.4444114981475,19.6240506396237,16.5222270383163));
#27561=CARTESIAN_POINT('Ctrl Pts',(56.4665726693188,19.6478605748917,16.5242656996864));
#27562=CARTESIAN_POINT('Ctrl Pts',(56.4729458644109,19.6548060009975,16.5248585418334));
#27563=CARTESIAN_POINT('Ctrl Pts',(56.4839631225199,19.6669846351443,16.525895038272));
#27564=CARTESIAN_POINT('Ctrl Pts',(56.4886293608479,19.6721976291882,16.5263377499807));
#27565=CARTESIAN_POINT('Ctrl Pts',(56.4983385426044,19.6831599719289,16.5272667999152));
#27566=CARTESIAN_POINT('Ctrl Pts',(56.5033760311357,19.6889139791321,16.5277533547985));
#27567=CARTESIAN_POINT('Ctrl Pts',(56.515291062202,19.7026827317148,16.5289151292469));
#27568=CARTESIAN_POINT('Ctrl Pts',(56.5221382309122,19.7107233436249,16.5295915836029));
#27569=CARTESIAN_POINT('Ctrl Pts',(56.5451317183074,19.7381630232643,16.5318936416007));
#27570=CARTESIAN_POINT('Ctrl Pts',(56.5609730477529,19.7578133674733,16.5335314801522));
#27571=CARTESIAN_POINT('Ctrl Pts',(56.5980423517159,19.8056250313779,16.5374929556275));
#27572=CARTESIAN_POINT('Ctrl Pts',(56.6189041182807,19.8340582662579,16.5398299786787));
#27573=CARTESIAN_POINT('Ctrl Pts',(56.6979812095146,19.9480517405075,16.5491275802197));
#27574=CARTESIAN_POINT('Ctrl Pts',(56.7502502868686,20.0375267274254,16.5562819317914));
#27575=CARTESIAN_POINT('Ctrl Pts',(56.8495589492488,20.2426120419385,16.5721658004954));
#27576=CARTESIAN_POINT('Ctrl Pts',(56.8931895521639,20.3594193327613,16.580890335521));
#27577=CARTESIAN_POINT('Ctrl Pts',(56.9297335230146,20.4946284319398,16.5901651817147));
#27578=CARTESIAN_POINT('Ctrl Pts',(56.9336345488825,20.5097660156899,16.5911920441129));
#27579=CARTESIAN_POINT('Ctrl Pts',(56.9388648674058,20.5310963239378,16.5926213706501));
#27580=CARTESIAN_POINT('Ctrl Pts',(56.9403431168462,20.5372514472932,16.5930317695687));
#27581=CARTESIAN_POINT('Ctrl Pts',(56.9426866973043,20.5472183363115,16.5936928925391));
#27582=CARTESIAN_POINT('Ctrl Pts',(56.9435701542898,20.5510257302973,16.5939446369818));
#27583=CARTESIAN_POINT('Ctrl Pts',(56.9454154319158,20.559085757558,16.59447582234));
#27584=CARTESIAN_POINT('Ctrl Pts',(56.946374511523,20.5633389947533,16.5947550999943));
#27585=CARTESIAN_POINT('Ctrl Pts',(56.9487125913686,20.5738684586513,16.5954440292946));
#27586=CARTESIAN_POINT('Ctrl Pts',(56.9500752383944,20.5801483337848,16.59585275498));
#27587=CARTESIAN_POINT('Ctrl Pts',(56.9550319564925,20.6035366091234,16.5973673306903));
#27588=CARTESIAN_POINT('Ctrl Pts',(56.9584315491732,20.6206860301097,16.5984626898699));
#27589=CARTESIAN_POINT('Ctrl Pts',(56.9664395307292,20.6640651294788,16.6012001961631));
#27590=CARTESIAN_POINT('Ctrl Pts',(56.9707490718081,20.6903471285931,16.6028283394322));
#27591=CARTESIAN_POINT('Ctrl Pts',(56.9990482898444,20.887591833986,16.6148731472246));
#27592=CARTESIAN_POINT('Ctrl Pts',(57.0012812043129,21.0609456362895,16.6245431781641));
#27593=CARTESIAN_POINT('Ctrl Pts',(56.9771446920451,21.2666737381516,16.6368093550055));
#27594=CARTESIAN_POINT('Ctrl Pts',(56.9722409103681,21.3008016651394,16.6388680968441));
#27595=CARTESIAN_POINT('Ctrl Pts',(56.9587562077782,21.3800080994893,16.643720968125));
#27596=CARTESIAN_POINT('Ctrl Pts',(56.9494997089953,21.424949908316,16.6465317899244));
#27597=CARTESIAN_POINT('Ctrl Pts',(56.9354743870564,21.4828608366111,16.6502470679314));
#27598=CARTESIAN_POINT('Ctrl Pts',(56.9321085390098,21.4961575043093,16.6511065531592));
#27599=CARTESIAN_POINT('Ctrl Pts',(56.9264836019209,21.5174529507766,16.6524938843764));
#27600=CARTESIAN_POINT('Ctrl Pts',(56.9243111407577,21.5254743142202,16.6530189284386));
#27601=CARTESIAN_POINT('Ctrl Pts',(56.92008247535,21.5407098296726,16.6540210039146));
#27602=CARTESIAN_POINT('Ctrl Pts',(56.9180355717871,21.5479264320045,16.6544977260633));
#27603=CARTESIAN_POINT('Ctrl Pts',(56.9132720092965,21.564367117701,16.655588592212));
#27604=CARTESIAN_POINT('Ctrl Pts',(56.9105292757201,21.57358339094,16.6562035764157));
#27605=CARTESIAN_POINT('Ctrl Pts',(56.9018876950974,21.6018714846647,16.6581020777423));
#27606=CARTESIAN_POINT('Ctrl Pts',(56.895769243688,21.6208743958594,16.6593927302699));
#27607=CARTESIAN_POINT('Ctrl Pts',(56.8418651447053,21.7800608989802,16.6703374175295));
#27608=CARTESIAN_POINT('Ctrl Pts',(56.778897755014,21.9145866874014,16.6805124866896));
#27609=CARTESIAN_POINT('Ctrl Pts',(56.6375284497124,22.1456987581866,16.6994001612998));
#27610=CARTESIAN_POINT('Ctrl Pts',(56.5638594129683,22.2443770308778,16.7080119947219));
#27611=CARTESIAN_POINT('Ctrl Pts',(56.471073987426,22.3472990300759,16.7171888389506));
#27612=CARTESIAN_POINT('Ctrl Pts',(56.4604391214733,22.3588196944641,16.7182188162755));
#27613=CARTESIAN_POINT('Ctrl Pts',(56.4453156391032,22.3748201459238,16.7196517189097));
#27614=CARTESIAN_POINT('Ctrl Pts',(56.4409401371259,22.3794053987654,16.7200626305579));
#27615=CARTESIAN_POINT('Ctrl Pts',(56.4338300562903,22.3867855709037,16.7207243574907));
#27616=CARTESIAN_POINT('Ctrl Pts',(56.4311090268805,22.3895933951395,16.7209761966869));
#27617=CARTESIAN_POINT('Ctrl Pts',(56.4253375241308,22.3955140627817,16.7215073704384));
#27618=CARTESIAN_POINT('Ctrl Pts',(56.4222850715316,22.3986249436822,16.7217865427214));
#27619=CARTESIAN_POINT('Ctrl Pts',(56.4147126925049,22.4062918425188,16.722474847349));
#27620=CARTESIAN_POINT('Ctrl Pts',(56.4101808816058,22.4108361465969,16.722883057474));
#27621=CARTESIAN_POINT('Ctrl Pts',(56.3932638787373,22.4276368350131,16.7243935122706));
#27622=CARTESIAN_POINT('Ctrl Pts',(56.3807397681024,22.4397530726264,16.7254853400426));
#27623=CARTESIAN_POINT('Ctrl Pts',(56.2927548360319,22.5226683776526,16.7329886492401));
#27624=CARTESIAN_POINT('Ctrl Pts',(56.2120341576318,22.5876752337866,16.7390388118718));
#27625=CARTESIAN_POINT('Ctrl Pts',(55.9944577645075,22.7365861631073,16.7543595782276));
#27626=CARTESIAN_POINT('Ctrl Pts',(55.8518958447368,22.8107857545053,16.7635678864731));
#27627=CARTESIAN_POINT('Ctrl Pts',(55.6803890940358,22.8752683604837,16.7748607244433));
#27628=CARTESIAN_POINT('Ctrl Pts',(55.6586368096638,22.883018382106,16.776295422476));
#27629=CARTESIAN_POINT('Ctrl Pts',(55.6278242752848,22.8933972273267,16.7783332271837));
#27630=CARTESIAN_POINT('Ctrl Pts',(55.6188718945133,22.8963422566568,16.7789259437965));
#27631=CARTESIAN_POINT('Ctrl Pts',(55.6032382395922,22.9013627037559,16.7799622834222));
#27632=CARTESIAN_POINT('Ctrl Pts',(55.5965662407865,22.9034666330844,16.7804049645839));
#27633=CARTESIAN_POINT('Ctrl Pts',(55.582577433782,22.9077970510717,16.7813340124989));
#27634=CARTESIAN_POINT('Ctrl Pts',(55.5752586251918,22.9100166402144,16.7818205962305));
#27635=CARTESIAN_POINT('Ctrl Pts',(55.5578010711509,22.915201585621,16.7829825547831));
#27636=CARTESIAN_POINT('Ctrl Pts',(55.5476512611181,22.9181285769288,16.7836591654271));
#27637=CARTESIAN_POINT('Ctrl Pts',(55.5131590942342,22.9277793074789,16.7859623196652));
#27638=CARTESIAN_POINT('Ctrl Pts',(55.4887133005297,22.9341211252453,16.7876011139753));
#27639=CARTESIAN_POINT('Ctrl Pts',(55.429835511088,22.9482079500885,16.7915653208806));
#27640=CARTESIAN_POINT('Ctrl Pts',(55.3953064592348,22.9555064135001,16.7939041439786));
#27641=CARTESIAN_POINT('Ctrl Pts',(55.2956630533863,22.9738213409399,16.8006939504547));
#27642=CARTESIAN_POINT('Ctrl Pts',(55.230196952794,22.9825209717304,16.8052054740242));
#27643=CARTESIAN_POINT('Ctrl Pts',(55.1644482145651,22.9879598454764,16.809768216174));
#27644=CARTESIAN_POINT('Origin',(55.,21.,6.22095488139522));
#27645=CARTESIAN_POINT('',(55.1644483624361,22.9879598332441,17.7696788290115));
#27646=CARTESIAN_POINT('',(55.1644483516309,22.987959834138,17.6123430797447));
#27647=CARTESIAN_POINT('',(55.1644483516311,22.987959834138,6.22095488139522));
#27648=CARTESIAN_POINT('Ctrl Pts',(55.1644483624361,22.9879598332441,17.7696788290115));
#27649=CARTESIAN_POINT('Ctrl Pts',(55.1727211370528,22.9872754913295,17.7691119138002));
#27650=CARTESIAN_POINT('Ctrl Pts',(55.1809902822389,22.9865394563269,17.7685438340102));
#27651=CARTESIAN_POINT('Ctrl Pts',(55.3342501289964,22.9719327759608,17.7579896043575));
#27652=CARTESIAN_POINT('Ctrl Pts',(55.4772844216076,22.942276542055,17.7476720793255));
#27653=CARTESIAN_POINT('Ctrl Pts',(55.6630129392337,22.8819947351274,17.7343263805435));
#27654=CARTESIAN_POINT('Ctrl Pts',(55.7096317441393,22.8649166339012,17.7309856455773));
#27655=CARTESIAN_POINT('Ctrl Pts',(55.7639655352898,22.8426791733497,17.7271408954905));
#27656=CARTESIAN_POINT('Ctrl Pts',(55.7723387837987,22.8391853320381,17.7265498015878));
#27657=CARTESIAN_POINT('Ctrl Pts',(55.7852346520752,22.8337007699802,17.7256419507824));
#27658=CARTESIAN_POINT('Ctrl Pts',(55.7897740721651,22.8317502255672,17.7253228651882));
#27659=CARTESIAN_POINT('Ctrl Pts',(55.7981441236325,22.8281167974787,17.7247354730493));
#27660=CARTESIAN_POINT('Ctrl Pts',(55.8019766854936,22.826438738037,17.7244668911211));
#27661=CARTESIAN_POINT('Ctrl Pts',(55.8106409613816,22.8226126171648,17.7238605448605));
#27662=CARTESIAN_POINT('Ctrl Pts',(55.8154694237916,22.8204573988237,17.7235232214984));
#27663=CARTESIAN_POINT('Ctrl Pts',(55.82976969201,22.8140060611981,17.7225257536937));
#27664=CARTESIAN_POINT('Ctrl Pts',(55.8392167053402,22.8096549572621,17.7218688589099));
#27665=CARTESIAN_POINT('Ctrl Pts',(55.9420755893927,22.7613015174512,17.7147344541242));
#27666=CARTESIAN_POINT('Ctrl Pts',(56.0319838577951,22.7101768510187,17.7086558723331));
#27667=CARTESIAN_POINT('Ctrl Pts',(56.2215883363034,22.5819381445825,17.6953264893371));
#27668=CARTESIAN_POINT('Ctrl Pts',(56.3187526462928,22.5018975623111,17.6881240682622));
#27669=CARTESIAN_POINT('Ctrl Pts',(56.449843344617,22.3713178956923,17.6770487735918));
#27670=CARTESIAN_POINT('Ctrl Pts',(56.4900444139618,22.3275259363384,17.6734308050266));
#27671=CARTESIAN_POINT('Ctrl Pts',(56.5374449600636,22.2710217147678,17.6688360902894));
#27672=CARTESIAN_POINT('Ctrl Pts',(56.5465423610585,22.2599364718552,17.6679380709916));
#27673=CARTESIAN_POINT('Ctrl Pts',(56.5608087049701,22.2421655041724,17.6665032667212));
#27674=CARTESIAN_POINT('Ctrl Pts',(56.5660561595535,22.2355432225677,17.6659696391487));
#27675=CARTESIAN_POINT('Ctrl Pts',(56.5758687535112,22.2229967978546,17.6649604958994));
#27676=CARTESIAN_POINT('Ctrl Pts',(56.5804429689339,22.2170799132784,17.664485352131));
#27677=CARTESIAN_POINT('Ctrl Pts',(56.5906836826698,22.2036781610116,17.6634107947475));
#27678=CARTESIAN_POINT('Ctrl Pts',(56.5963308018917,22.1961787740802,17.6628106345124));
#27679=CARTESIAN_POINT('Ctrl Pts',(56.6106751101889,22.1768470138711,17.6612663160671));
#27680=CARTESIAN_POINT('Ctrl Pts',(56.6192948340342,22.1649581219788,17.660319190064));
#27681=CARTESIAN_POINT('Ctrl Pts',(56.6745942781716,22.0868858081109,17.6541153324867));
#27682=CARTESIAN_POINT('Ctrl Pts',(56.7173318081134,22.0180153344787,17.6487109847649));
#27683=CARTESIAN_POINT('Ctrl Pts',(56.8162142209219,21.8346356495947,17.634500610101));
#27684=CARTESIAN_POINT('Ctrl Pts',(56.865787044583,21.7169973038166,17.6255363549217));
#27685=CARTESIAN_POINT('Ctrl Pts',(56.9248551351996,21.5281419240925,17.6118278296533));
#27686=CARTESIAN_POINT('Ctrl Pts',(56.9423250724568,21.459757043164,17.6070005688506));
#27687=CARTESIAN_POINT('Ctrl Pts',(56.9589731226165,21.3763796971723,17.6013819138472));
#27688=CARTESIAN_POINT('Ctrl Pts',(56.9616546305764,21.3621443237195,17.6004319136836));
#27689=CARTESIAN_POINT('Ctrl Pts',(56.9652214123138,21.3420057867138,17.5991022549349));
#27690=CARTESIAN_POINT('Ctrl Pts',(56.9662355536595,21.3361263264149,17.5987157738654));
#27691=CARTESIAN_POINT('Ctrl Pts',(56.9679305830337,21.3260291911563,17.5980550892619));
#27692=CARTESIAN_POINT('Ctrl Pts',(56.9686243242136,21.3218137421265,17.5977801694701));
#27693=CARTESIAN_POINT('Ctrl Pts',(56.9699431343234,21.3136362502739,17.5972486542128));
#27694=CARTESIAN_POINT('Ctrl Pts',(56.9705697986139,21.3096745379212,17.5969919651593));
#27695=CARTESIAN_POINT('Ctrl Pts',(56.9722360397465,21.2989308303612,17.5962979873865));
#27696=CARTESIAN_POINT('Ctrl Pts',(56.9732525937669,21.2921452418095,17.5958619817642));
#27697=CARTESIAN_POINT('Ctrl Pts',(56.9769530600663,21.266543441906,17.594225159882));
#27698=CARTESIAN_POINT('Ctrl Pts',(56.9794031119317,21.247693744364,17.5930367277394));
#27699=CARTESIAN_POINT('Ctrl Pts',(56.9979493596186,21.0870768118537,17.5830300119546));
#27700=CARTESIAN_POINT('Ctrl Pts',(56.9990639254823,20.9439758305669,17.5748856529494));
#27701=CARTESIAN_POINT('Ctrl Pts',(56.9721269600911,20.6739874262591,17.5591149443914));
#27702=CARTESIAN_POINT('Ctrl Pts',(56.9470139027634,20.5475628890419,17.5515500306981));
#27703=CARTESIAN_POINT('Ctrl Pts',(56.9050123411785,20.408185958683,17.5425121361114));
#27704=CARTESIAN_POINT('Ctrl Pts',(56.8999057734108,20.3919918555079,17.5414514650829));
#27705=CARTESIAN_POINT('Ctrl Pts',(56.8917718970462,20.3673010524774,17.539817191712));
#27706=CARTESIAN_POINT('Ctrl Pts',(56.8888925825961,20.3587561495401,17.539248448773));
#27707=CARTESIAN_POINT('Ctrl Pts',(56.8835501137769,20.3432496218506,17.538210455999));
#27708=CARTESIAN_POINT('Ctrl Pts',(56.8811060357845,20.3362815581554,17.5377418439537));
#27709=CARTESIAN_POINT('Ctrl Pts',(56.8756982038185,20.3211336634636,17.5367183022653));
#27710=CARTESIAN_POINT('Ctrl Pts',(56.87271952222,20.3129593594056,17.5361628843627));
#27711=CARTESIAN_POINT('Ctrl Pts',(56.8644324160613,20.2906716606282,17.5346399306964));
#27712=CARTESIAN_POINT('Ctrl Pts',(56.8590173722913,20.2765987863634,17.5336688570134));
#27713=CARTESIAN_POINT('Ctrl Pts',(56.8299940618303,20.2036502384309,17.5285846948711));
#27714=CARTESIAN_POINT('Ctrl Pts',(56.8037491725794,20.1458696502639,17.524383602192));
#27715=CARTESIAN_POINT('Ctrl Pts',(56.6959452379606,19.935745355291,17.5084392774208));
#27716=CARTESIAN_POINT('Ctrl Pts',(56.5974757924373,19.7929679034666,17.4961674473908));
#27717=CARTESIAN_POINT('Ctrl Pts',(56.446552971803,19.6254840691648,17.4807284424302));
#27718=CARTESIAN_POINT('Ctrl Pts',(56.4097007471355,19.5877130492383,17.4771711809947));
#27719=CARTESIAN_POINT('Ctrl Pts',(56.3647017797651,19.5451111837247,17.4731119635997));
#27720=CARTESIAN_POINT('Ctrl Pts',(56.3579685440455,19.5388244949092,17.4725116942493));
#27721=CARTESIAN_POINT('Ctrl Pts',(56.3475354173537,19.5292177025552,17.4715927996984));
#27722=CARTESIAN_POINT('Ctrl Pts',(56.3438663695168,19.52586450769,17.4712717576575));
#27723=CARTESIAN_POINT('Ctrl Pts',(56.3370874547228,19.5197155044717,17.4706825348509));
#27724=CARTESIAN_POINT('Ctrl Pts',(56.3339813442382,19.5169157734268,17.4704140653092));
#27725=CARTESIAN_POINT('Ctrl Pts',(56.326955473649,19.5106228487159,17.4698101850031));
#27726=CARTESIAN_POINT('Ctrl Pts',(56.3230307201806,19.5071353568412,17.4694751994743));
#27727=CARTESIAN_POINT('Ctrl Pts',(56.3114213973615,19.4969011845475,17.4684910651037));
#27728=CARTESIAN_POINT('Ctrl Pts',(56.3036985283561,19.4901979308098,17.4678450384129));
#27729=CARTESIAN_POINT('Ctrl Pts',(56.2423831296835,19.4377990172389,17.4627805203232));
#27730=CARTESIAN_POINT('Ctrl Pts',(56.1864498876303,19.394906012039,17.4585457210283));
#27731=CARTESIAN_POINT('Ctrl Pts',(55.9883735449417,19.2590342867202,17.4443698665764));
#27732=CARTESIAN_POINT('Ctrl Pts',(55.8367087728335,19.1812738922679,17.4347996376259));
#27733=CARTESIAN_POINT('Ctrl Pts',(55.6459759638719,19.1124533991687,17.4225818331388));
#27734=CARTESIAN_POINT('Ctrl Pts',(55.6146550000423,19.1020231377892,17.4205726507406));
#27735=CARTESIAN_POINT('Ctrl Pts',(55.5601498832996,19.0853629241264,17.4170614155901));
#27736=CARTESIAN_POINT('Ctrl Pts',(55.5370850522489,19.0787653465232,17.4155711009342));
#27737=CARTESIAN_POINT('Ctrl Pts',(55.5039053807717,19.0699186321814,17.4134184167345));
#27738=CARTESIAN_POINT('Ctrl Pts',(55.4938827112266,19.0673296762664,17.4127670150505));
#27739=CARTESIAN_POINT('Ctrl Pts',(55.4764554173765,19.0629724456127,17.411632206341));
#27740=CARTESIAN_POINT('Ctrl Pts',(55.4690599165999,19.0611683148806,17.4111499640131));
#27741=CARTESIAN_POINT('Ctrl Pts',(55.4547996665773,19.0577758956194,17.4102187218161));
#27742=CARTESIAN_POINT('Ctrl Pts',(55.4479364619659,19.0561815588124,17.4097699243761));
#27743=CARTESIAN_POINT('Ctrl Pts',(55.4298682306864,19.0520850430731,17.4085867425501));
#27744=CARTESIAN_POINT('Ctrl Pts',(55.4186499263322,19.0496432107887,17.4078504392147));
#27745=CARTESIAN_POINT('Ctrl Pts',(55.3791285066018,19.0413974679117,17.405250224726));
#27746=CARTESIAN_POINT('Ctrl Pts',(55.350722097956,19.0361119766629,17.4033699724366));
#27747=CARTESIAN_POINT('Ctrl Pts',(55.1336625962208,19.0005837761638,17.388909471515));
#27748=CARTESIAN_POINT('Ctrl Pts',(54.9416818636509,18.9969771899368,17.3754473186876));
#27749=CARTESIAN_POINT('Ctrl Pts',(54.7010742129763,19.0271027123333,17.3586600033628));
#27750=CARTESIAN_POINT('Ctrl Pts',(54.6502315123305,19.0354789221204,17.3551270455247));
#27751=CARTESIAN_POINT('Ctrl Pts',(54.5815218559772,19.0495512179538,17.350417226066));
#27752=CARTESIAN_POINT('Ctrl Pts',(54.563329282594,19.0535434381311,17.3491764989184));
#27753=CARTESIAN_POINT('Ctrl Pts',(54.5322131563923,19.0608298707927,17.3470682356078));
#27754=CARTESIAN_POINT('Ctrl Pts',(54.519262091081,19.0639998948768,17.3461948901747));
#27755=CARTESIAN_POINT('Ctrl Pts',(54.5007525320873,19.0687276667856,17.3449536162804));
#27756=CARTESIAN_POINT('Ctrl Pts',(54.4951678304224,19.0701799716471,17.3445800042905));
#27757=CARTESIAN_POINT('Ctrl Pts',(54.4854910175825,19.0727413138723,17.3439342992412));
#27758=CARTESIAN_POINT('Ctrl Pts',(54.4813960244936,19.073839193056,17.3436615733915));
#27759=CARTESIAN_POINT('Ctrl Pts',(54.4728131920417,19.0761696304915,17.3430910838046));
#27760=CARTESIAN_POINT('Ctrl Pts',(54.468326149636,19.0774048426558,17.3427934749137));
#27761=CARTESIAN_POINT('Ctrl Pts',(54.456364918728,19.080742658224,17.342001735944));
#27762=CARTESIAN_POINT('Ctrl Pts',(54.4488985230971,19.0828732403836,17.3415091954168));
#27763=CARTESIAN_POINT('Ctrl Pts',(54.4163336554861,19.0923717952355,17.3393675308833));
#27764=CARTESIAN_POINT('Ctrl Pts',(54.3913677678926,19.1001898174323,17.3377426940248));
#27765=CARTESIAN_POINT('Ctrl Pts',(54.1650774284183,19.1759713614955,17.3231105887006));
#27766=CARTESIAN_POINT('Ctrl Pts',(53.9756480155405,19.2752087188727,17.3114183926279));
#27767=CARTESIAN_POINT('Ctrl Pts',(53.7611385650347,19.4356123219912,17.2953408045764));
#27768=CARTESIAN_POINT('Ctrl Pts',(53.7182454651794,19.4705586211622,17.2919662809799));
#27769=CARTESIAN_POINT('Ctrl Pts',(53.6663646236829,19.5165442291925,17.2876454266519));
#27770=CARTESIAN_POINT('Ctrl Pts',(53.6559656773835,19.5259592730773,17.2867666912311));
#27771=CARTESIAN_POINT('Ctrl Pts',(53.6395141801564,19.5411730290735,17.2853555949521));
#27772=CARTESIAN_POINT('Ctrl Pts',(53.6333972541059,19.5469016796722,17.2848262110897));
#27773=CARTESIAN_POINT('Ctrl Pts',(53.6218821568268,19.5578228704351,17.2838205594798));
#27774=CARTESIAN_POINT('Ctrl Pts',(53.6164767648721,19.5630076137764,17.2833446325426));
#27775=CARTESIAN_POINT('Ctrl Pts',(53.6042825750738,19.5748366181754,17.2822621013265));
#27776=CARTESIAN_POINT('Ctrl Pts',(53.597511819851,19.5814991383441,17.2816547051114));
#27777=CARTESIAN_POINT('Ctrl Pts',(53.5801362097604,19.5988430032695,17.2800793348104));
#27778=CARTESIAN_POINT('Ctrl Pts',(53.5696043582906,19.6095963176532,17.2791081880461));
#27779=CARTESIAN_POINT('Ctrl Pts',(53.4959217533156,19.6865515447671,17.2721960569072));
#27780=CARTESIAN_POINT('Ctrl Pts',(53.4372786470323,19.7569006716248,17.2660648101233));
#27781=CARTESIAN_POINT('Ctrl Pts',(53.298438532853,19.9488714009877,17.2498215277306));
#27782=CARTESIAN_POINT('Ctrl Pts',(53.2263529908419,20.0756863860817,17.2395187277375));
#27783=CARTESIAN_POINT('Ctrl Pts',(53.149033594468,20.2547409998105,17.226189050458));
#27784=CARTESIAN_POINT('Ctrl Pts',(53.1310739760065,20.3009978180914,17.2228502222859));
#27785=CARTESIAN_POINT('Ctrl Pts',(53.1118905809067,20.3564530527736,17.219007367434));
#27786=CARTESIAN_POINT('Ctrl Pts',(53.1089834404711,20.3650462765884,17.2184163581595));
#27787=CARTESIAN_POINT('Ctrl Pts',(53.1045837023256,20.3783497539317,17.2175086092736));
#27788=CARTESIAN_POINT('Ctrl Pts',(53.1030498576763,20.3830460886352,17.2171895417771));
#27789=CARTESIAN_POINT('Ctrl Pts',(53.1002492861543,20.3917300823297,17.2166021664195));
#27790=CARTESIAN_POINT('Ctrl Pts',(53.0989776641877,20.3957160048397,17.2163335832994));
#27791=CARTESIAN_POINT('Ctrl Pts',(53.0961272337681,20.4047487805527,17.2157272135416));
#27792=CARTESIAN_POINT('Ctrl Pts',(53.0945559490641,20.4097979205734,17.2153898680229));
#27793=CARTESIAN_POINT('Ctrl Pts',(53.0905445382888,20.4228711235624,17.2145204112469));
#27794=CARTESIAN_POINT('Ctrl Pts',(53.0881348760144,20.4309045301535,17.2139900173989));
#27795=CARTESIAN_POINT('Ctrl Pts',(53.073075665954,20.4822847281425,17.2106210336925));
#27796=CARTESIAN_POINT('Ctrl Pts',(53.0618493043905,20.5260389516752,17.2078576814511));
#27797=CARTESIAN_POINT('Ctrl Pts',(53.0471334016904,20.5927231404566,17.2037525131035));
#27798=CARTESIAN_POINT('Ctrl Pts',(53.0425427310998,20.6153917667218,17.2023753145903));
#27799=CARTESIAN_POINT('Ctrl Pts',(53.0164266325669,20.7569661677294,17.1938600935992));
#27800=CARTESIAN_POINT('Ctrl Pts',(53.0053482399933,20.8775452457192,17.1869681386615));
#27801=CARTESIAN_POINT('Ctrl Pts',(53.0051725872726,21.0950537116775,17.1742123628961));
#27802=CARTESIAN_POINT('Ctrl Pts',(53.0121208370533,21.1915841068912,17.1684384195527));
#27803=CARTESIAN_POINT('Ctrl Pts',(53.0282260160935,21.3022682024253,17.1614932105762));
#27804=CARTESIAN_POINT('Ctrl Pts',(53.0305870496939,21.3172874421646,17.1605439941625));
#27805=CARTESIAN_POINT('Ctrl Pts',(53.0347094477701,21.3416894991796,17.1589900572137));
#27806=CARTESIAN_POINT('Ctrl Pts',(53.0363669180387,21.351089422884,17.1583886211391));
#27807=CARTESIAN_POINT('Ctrl Pts',(53.039446211268,21.3678485820801,17.1573110830264));
#27808=CARTESIAN_POINT('Ctrl Pts',(53.0408421787836,21.3752124290471,17.1568358104766));
#27809=CARTESIAN_POINT('Ctrl Pts',(53.0438817756099,21.390766992798,17.1558279880372));
#27810=CARTESIAN_POINT('Ctrl Pts',(53.0455354211034,21.3989555824773,17.155295127194));
#27811=CARTESIAN_POINT('Ctrl Pts',(53.0500787943295,21.4207472473699,17.1538708106436));
#27812=CARTESIAN_POINT('Ctrl Pts',(53.0530593799626,21.4343307038317,17.1529764713609));
#27813=CARTESIAN_POINT('Ctrl Pts',(53.0682623591484,21.5003120457261,17.1485996333796));
#27814=CARTESIAN_POINT('Ctrl Pts',(53.0824582988953,21.5522276395413,17.1450544744596));
#27815=CARTESIAN_POINT('Ctrl Pts',(53.1575551697278,21.7888119097579,17.1284151964815));
#27816=CARTESIAN_POINT('Ctrl Pts',(53.2431358141639,21.9644865340944,17.114539294953));
#27817=CARTESIAN_POINT('Ctrl Pts',(53.3771894969855,22.1607716562556,17.0983561041384));
#27818=CARTESIAN_POINT('Ctrl Pts',(53.4027861275306,22.1957479873078,17.0954487816379));
#27819=CARTESIAN_POINT('Ctrl Pts',(53.4346130811539,22.2363899179212,17.0920673616161));
#27820=CARTESIAN_POINT('Ctrl Pts',(53.4397630794305,22.2428825335638,17.0915270815543));
#27821=CARTESIAN_POINT('Ctrl Pts',(53.4482463724457,22.2534416155369,17.0906485204068));
#27822=CARTESIAN_POINT('Ctrl Pts',(53.4515554864122,22.2575272538061,17.0903086044777));
#27823=CARTESIAN_POINT('Ctrl Pts',(53.4575257571423,22.2648392239252,17.0897003870114));
#27824=CARTESIAN_POINT('Ctrl Pts',(53.460180929635,22.2680702992331,17.0894316709026));
#27825=CARTESIAN_POINT('Ctrl Pts',(53.4660102950184,22.2751187371143,17.0888455894302));
#27826=CARTESIAN_POINT('Ctrl Pts',(53.4691885780625,22.2789326020124,17.0885285259616));
#27827=CARTESIAN_POINT('Ctrl Pts',(53.4782868494599,22.289767806072,17.0876277917881));
#27828=CARTESIAN_POINT('Ctrl Pts',(53.4842412267826,22.2967602921213,17.0870465574006));
#27829=CARTESIAN_POINT('Ctrl Pts',(53.5242952520686,22.3431446411389,17.0831893733766));
#27830=CARTESIAN_POINT('Ctrl Pts',(53.5598818965131,22.3812323923223,17.0800142384225));
#27831=CARTESIAN_POINT('Ctrl Pts',(53.7151413161528,22.534870245432,17.0669520766201));
#27832=CARTESIAN_POINT('Ctrl Pts',(53.8475294004122,22.6366145161376,17.0576060951706));
#27833=CARTESIAN_POINT('Ctrl Pts',(54.0511572360998,22.7560139947072,17.0435772240663));
#27834=CARTESIAN_POINT('Ctrl Pts',(54.113097599399,22.788096837687,17.0393578806663));
#27835=CARTESIAN_POINT('Ctrl Pts',(54.1894605549981,22.8227049086856,17.0341442132824));
#27836=CARTESIAN_POINT('Ctrl Pts',(54.2023969634172,22.8284027882109,17.0332606849461));
#27837=CARTESIAN_POINT('Ctrl Pts',(54.2238692035841,22.8375890601044,17.0317931618583));
#27838=CARTESIAN_POINT('Ctrl Pts',(54.2323707497069,22.8411566735212,17.0312118631701));
#27839=CARTESIAN_POINT('Ctrl Pts',(54.2478000530563,22.8475060298456,17.0301562682346));
#27840=CARTESIAN_POINT('Ctrl Pts',(54.2547193117933,22.8503080780797,17.0296826686529));
#27841=CARTESIAN_POINT('Ctrl Pts',(54.2696106760838,22.8562414596052,17.028662859584));
#27842=CARTESIAN_POINT('Ctrl Pts',(54.2775875237172,22.8593604091688,17.0281162449008));
#27843=CARTESIAN_POINT('Ctrl Pts',(54.2994661794092,22.8677529271903,17.0266159645061));
#27844=CARTESIAN_POINT('Ctrl Pts',(54.3134070308409,22.8729225039108,17.0256588526289));
#27845=CARTESIAN_POINT('Ctrl Pts',(54.3907645191626,22.9006286356879,17.0203404472342));
#27846=CARTESIAN_POINT('Ctrl Pts',(54.4552258628825,22.920098034461,17.0158790951855));
#27847=CARTESIAN_POINT('Ctrl Pts',(54.6821159162959,22.976280384899,17.0000704083081));
#27848=CARTESIAN_POINT('Ctrl Pts',(54.8480585653068,22.9959051086786,16.9882598562966));
#27849=CARTESIAN_POINT('Ctrl Pts',(55.0645299534269,22.9943342479137,16.973410028092));
#27850=CARTESIAN_POINT('Ctrl Pts',(55.1145566822883,22.9920869813143,16.9700231672771));
#27851=CARTESIAN_POINT('Ctrl Pts',(55.164448352281,22.9879598340842,16.9667227887628));
#27852=CARTESIAN_POINT('',(53.0052507533592,21.0011686008279,17.0195584283291));
#27853=CARTESIAN_POINT('Ctrl Pts',(55.1644482145651,22.9879598454764,16.809768216174));
#27854=CARTESIAN_POINT('Ctrl Pts',(55.1270233745594,22.9910557068607,16.8123653746829));
#27855=CARTESIAN_POINT('Ctrl Pts',(55.0895069287072,22.9930950923982,16.8149786665284));
#27856=CARTESIAN_POINT('Ctrl Pts',(54.9277669391599,22.9973082404018,16.8262571771688));
#27857=CARTESIAN_POINT('Ctrl Pts',(54.8035490652872,22.988936975352,16.8349678322256));
#27858=CARTESIAN_POINT('Ctrl Pts',(54.6654731627478,22.9665614313119,16.8442306065549));
#27859=CARTESIAN_POINT('Ctrl Pts',(54.6500672154177,22.963878598751,16.8452578452758));
#27860=CARTESIAN_POINT('Ctrl Pts',(54.6284699684782,22.9598553719831,16.8466876038589));
#27861=CARTESIAN_POINT('Ctrl Pts',(54.622251540512,22.9586663185466,16.8470980647222));
#27862=CARTESIAN_POINT('Ctrl Pts',(54.6122032007223,22.9566952963273,16.8477592606505));
#27863=CARTESIAN_POINT('Ctrl Pts',(54.6083698031279,22.9559316526256,16.8480110165315));
#27864=CARTESIAN_POINT('Ctrl Pts',(54.6002653966804,22.954292408274,16.8485422004317));
#27865=CARTESIAN_POINT('Ctrl Pts',(54.5959949664327,22.9534140635474,16.8488214653095));
#27866=CARTESIAN_POINT('Ctrl Pts',(54.5854385510223,22.9512067154736,16.8495103189212));
#27867=CARTESIAN_POINT('Ctrl Pts',(54.5791559770559,22.9498613162404,16.8499189821482));
#27868=CARTESIAN_POINT('Ctrl Pts',(54.5558104933033,22.944743841768,16.8514330581171));
#27869=CARTESIAN_POINT('Ctrl Pts',(54.5387902910449,22.9407778290165,16.8525279889959));
#27870=CARTESIAN_POINT('Ctrl Pts',(54.4959850095967,22.9302084850896,16.8552642067769));
#27871=CARTESIAN_POINT('Ctrl Pts',(54.4702752776269,22.9233116659363,16.8568915066384));
#27872=CARTESIAN_POINT('Ctrl Pts',(54.2791252386108,22.867910245082,16.8689215851795));
#27873=CARTESIAN_POINT('Ctrl Pts',(54.1204494749173,22.7986525842951,16.8785794332166));
#27874=CARTESIAN_POINT('Ctrl Pts',(53.9072096408508,22.6705282122025,16.8933090557485));
#27875=CARTESIAN_POINT('Ctrl Pts',(53.8440912404547,22.6274913894997,16.8979143554293));
#27876=CARTESIAN_POINT('Ctrl Pts',(53.7721360340915,22.5721281151553,16.9035575948327));
#27877=CARTESIAN_POINT('Ctrl Pts',(53.7607701400038,22.5631845911631,16.9044612488006));
#27878=CARTESIAN_POINT('Ctrl Pts',(53.7422425684839,22.5482766685299,16.905955190256));
#27879=CARTESIAN_POINT('Ctrl Pts',(53.7350235306683,22.5423841694385,16.9065426062463));
#27880=CARTESIAN_POINT('Ctrl Pts',(53.7220918787951,22.5316769267259,16.9076046421431));
#27881=CARTESIAN_POINT('Ctrl Pts',(53.7163644909864,22.5268802348656,16.9080785243193));
#27882=CARTESIAN_POINT('Ctrl Pts',(53.7044268244303,22.5167677912694,16.9090737030635));
#27883=CARTESIAN_POINT('Ctrl Pts',(53.6982220187961,22.5114458211461,16.9095952498259));
#27884=CARTESIAN_POINT('Ctrl Pts',(53.6816560379525,22.4970592105694,16.9109993828928));
#27885=CARTESIAN_POINT('Ctrl Pts',(53.6713558472513,22.4879253280386,16.9118848323158));
#27886=CARTESIAN_POINT('Ctrl Pts',(53.6488121421553,22.4675135456373,16.9138507936399));
#27887=CARTESIAN_POINT('Ctrl Pts',(53.6366136964173,22.4561876229523,16.9149332907983));
#27888=CARTESIAN_POINT('Ctrl Pts',(53.6002464329836,22.4215640562012,16.9182182046268));
#27889=CARTESIAN_POINT('Ctrl Pts',(53.5765235694982,22.3978086588392,16.9204397750863));
#27890=CARTESIAN_POINT('Ctrl Pts',(53.4908320714251,22.3075551326671,16.9287647626614));
#27891=CARTESIAN_POINT('Ctrl Pts',(53.4328362517925,22.237450121718,16.9350150246275));
#27892=CARTESIAN_POINT('Ctrl Pts',(53.2974014799077,22.0488804840534,16.9511623833349));
#27893=CARTESIAN_POINT('Ctrl Pts',(53.2273978641206,21.92567777455,16.961131717472));
#27894=CARTESIAN_POINT('Ctrl Pts',(53.1651243630623,21.7826082134327,16.9714511792834));
#27895=CARTESIAN_POINT('Ctrl Pts',(53.1593992663036,21.7690469351358,16.9724172569298));
#27896=CARTESIAN_POINT('Ctrl Pts',(53.1517150514553,21.7502675131983,16.9737372671607));
#27897=CARTESIAN_POINT('Ctrl Pts',(53.1496270661421,21.7451030799978,16.9740984357724));
#27898=CARTESIAN_POINT('Ctrl Pts',(53.1460864180662,21.7362389488729,16.9747151061792));
#27899=CARTESIAN_POINT('Ctrl Pts',(53.1446231426043,21.7325435665087,16.9749712322888));
#27900=CARTESIAN_POINT('Ctrl Pts',(53.1416012497567,21.72484488184,16.9755027967752));
#27901=CARTESIAN_POINT('Ctrl Pts',(53.1400445107646,21.7208408951201,16.9757781135687));
#27902=CARTESIAN_POINT('Ctrl Pts',(53.1363078168127,21.7111372905205,16.9764426437643));
#27903=CARTESIAN_POINT('Ctrl Pts',(53.1341410337677,21.7054325765969,16.9768310753747));
#27904=CARTESIAN_POINT('Ctrl Pts',(53.1266220836563,21.6853596369317,16.9781902681982));
#27905=CARTESIAN_POINT('Ctrl Pts',(53.1214092688239,21.6709393027526,16.9791531351863));
#27906=CARTESIAN_POINT('Ctrl Pts',(53.090322711761,21.5817399506995,16.9850342022889));
#27907=CARTESIAN_POINT('Ctrl Pts',(53.0687483153913,21.5055279359674,16.9897378428035));
#27908=CARTESIAN_POINT('Ctrl Pts',(53.0209256920076,21.2879566568982,17.0027834515498));
#27909=CARTESIAN_POINT('Ctrl Pts',(53.0053346483509,21.1447775937495,17.0109571210933));
#27910=CARTESIAN_POINT('Ctrl Pts',(53.0052503437261,21.0011710231689,17.0195575702349));
#27911=CARTESIAN_POINT('Ctrl Pts',(53.0052503422808,21.0011685585087,17.0195577178409));
#27912=CARTESIAN_POINT('Ctrl Pts',(53.0052282297145,20.9634220241211,17.0218183198799));
#27913=CARTESIAN_POINT('Ctrl Pts',(53.0062775294282,20.9256837997141,17.0241037505693));
#27914=CARTESIAN_POINT('Ctrl Pts',(53.0096914951773,20.8649765409554,17.0278357116731));
#27915=CARTESIAN_POINT('Ctrl Pts',(53.0113852710205,20.8419788892939,17.0292623188599));
#27916=CARTESIAN_POINT('Ctrl Pts',(53.0143580688015,20.8093486808741,17.0313069960328));
#27917=CARTESIAN_POINT('Ctrl Pts',(53.0153094101569,20.7996875896606,17.0319149414409));
#27918=CARTESIAN_POINT('Ctrl Pts',(53.0171097776151,20.7826784927092,17.0329899684286));
#27919=CARTESIAN_POINT('Ctrl Pts',(53.017929230875,20.7753274930776,17.0334561211071));
#27920=CARTESIAN_POINT('Ctrl Pts',(53.0196191109161,20.7608975871625,17.034374290602));
#27921=CARTESIAN_POINT('Ctrl Pts',(53.020486657703,20.7538184507588,17.0348262105417));
#27922=CARTESIAN_POINT('Ctrl Pts',(53.0222878775683,20.7397460872159,17.0357275702168));
#27923=CARTESIAN_POINT('Ctrl Pts',(53.0232207252282,20.7327528577128,17.0361769777382));
#27924=CARTESIAN_POINT('Ctrl Pts',(53.025776933553,20.7143358919914,17.0373644847243));
#27925=CARTESIAN_POINT('Ctrl Pts',(53.0274623303945,20.7029211697004,17.0381045310651));
#27926=CARTESIAN_POINT('Ctrl Pts',(53.0337741641412,20.6625971794646,17.0407334996856));
#27927=CARTESIAN_POINT('Ctrl Pts',(53.0389377224389,20.6337769892865,17.0426392514805));
#27928=CARTESIAN_POINT('Ctrl Pts',(53.0544905074254,20.5567740484736,17.0478058798917));
#27929=CARTESIAN_POINT('Ctrl Pts',(53.0660337898085,20.5088478201049,17.0511012989055));
#27930=CARTESIAN_POINT('Ctrl Pts',(53.1266152446108,20.2928123345647,17.0663141948278));
#27931=CARTESIAN_POINT('Ctrl Pts',(53.1958738204969,20.1312061570943,17.0787840294952));
#27932=CARTESIAN_POINT('Ctrl Pts',(53.3075152487275,19.9433976242558,17.0936528268165));
#27933=CARTESIAN_POINT('Ctrl Pts',(53.3309189772368,19.9068017566302,17.0965648605047));
#27934=CARTESIAN_POINT('Ctrl Pts',(53.3604553582758,19.8637792628891,17.0999802740345));
#27935=CARTESIAN_POINT('Ctrl Pts',(53.3654575988638,19.8565948481283,17.1005503368414));
#27936=CARTESIAN_POINT('Ctrl Pts',(53.3733166215605,19.8454643898302,17.1014327700867));
#27937=CARTESIAN_POINT('Ctrl Pts',(53.3761407612178,19.8414955922848,17.1017472728104));
#27938=CARTESIAN_POINT('Ctrl Pts',(53.381420996735,19.8341324579373,17.1023304202088));
#27939=CARTESIAN_POINT('Ctrl Pts',(53.3838732277932,19.8307355422858,17.1025993090487));
#27940=CARTESIAN_POINT('Ctrl Pts',(53.3894980944814,19.8229952831613,17.1032117089723));
#27941=CARTESIAN_POINT('Ctrl Pts',(53.3926776033082,19.8186570329224,17.1035547404343));
#27942=CARTESIAN_POINT('Ctrl Pts',(53.4010399306432,19.8073433962147,17.1044489393539));
#27943=CARTESIAN_POINT('Ctrl Pts',(53.4062509173405,19.8003888355234,17.1049982224616));
#27944=CARTESIAN_POINT('Ctrl Pts',(53.4423669258554,19.7528393008698,17.1087527985512));
#27945=CARTESIAN_POINT('Ctrl Pts',(53.4747769367784,19.7134051967517,17.1118618325421));
#27946=CARTESIAN_POINT('Ctrl Pts',(53.6215576721776,19.5481667098535,17.1250819054131));
#27947=CARTESIAN_POINT('Ctrl Pts',(53.7502330640489,19.4360264659343,17.1346223656856));
#27948=CARTESIAN_POINT('Ctrl Pts',(53.9287744385668,19.3166982308119,17.1474081622781));
#27949=CARTESIAN_POINT('Ctrl Pts',(53.9667934505477,19.2930984582603,17.1501039250887));
#27950=CARTESIAN_POINT('Ctrl Pts',(54.0232386120249,19.2606380225472,17.1540911993001));
#27951=CARTESIAN_POINT('Ctrl Pts',(54.041059514219,19.2507498758644,17.1553478977601));
#27952=CARTESIAN_POINT('Ctrl Pts',(54.0733735368401,19.2334622438081,17.1576248513136));
#27953=CARTESIAN_POINT('Ctrl Pts',(54.0878117648029,19.2259636854803,17.1586415890998));
#27954=CARTESIAN_POINT('Ctrl Pts',(54.1102094533104,19.2146770588854,17.1602186208604));
#27955=CARTESIAN_POINT('Ctrl Pts',(54.1181052242804,19.2107636205405,17.1607745244843));
#27956=CARTESIAN_POINT('Ctrl Pts',(54.126097447189,19.2068681317572,17.1613372440087));
#27957=CARTESIAN_POINT('Ctrl Pts',(54.1261683301154,19.2068335879165,17.1613422347632));
#27958=CARTESIAN_POINT('Ctrl Pts',(54.1263115822088,19.206763786447,17.16135232092));
#27959=CARTESIAN_POINT('Ctrl Pts',(54.1263839515305,19.2067285289625,17.1613574163333));
#27960=CARTESIAN_POINT('Ctrl Pts',(54.1265302143088,19.2066572824081,17.1613677144761));
#27961=CARTESIAN_POINT('Ctrl Pts',(54.1266041078101,19.2066212935464,17.1613729172089));
#27962=CARTESIAN_POINT('Ctrl Pts',(54.1267534577984,19.2065485660112,17.1613834327266));
#27963=CARTESIAN_POINT('Ctrl Pts',(54.1268289143291,19.2065118275573,17.1613887455146));
#27964=CARTESIAN_POINT('Ctrl Pts',(54.1269814301541,19.2064375821987,17.1613994839439));
#27965=CARTESIAN_POINT('Ctrl Pts',(54.1270584895868,19.2064000754788,17.161404909595));
#27966=CARTESIAN_POINT('Ctrl Pts',(54.1272142523196,19.2063242743443,17.1614158766449));
#27967=CARTESIAN_POINT('Ctrl Pts',(54.1272929557242,19.2062859801429,17.1614214180511));
#27968=CARTESIAN_POINT('Ctrl Pts',(54.1334147112952,19.2033078558133,17.1618524432571));
#27969=CARTESIAN_POINT('Ctrl Pts',(54.1394725171775,19.2003986071688,17.1622789821813));
#27970=CARTESIAN_POINT('Ctrl Pts',(54.1533654548371,19.1938127407448,17.1632573008765));
#27971=CARTESIAN_POINT('Ctrl Pts',(54.161210002858,19.1901564141182,17.1638097717616));
#27972=CARTESIAN_POINT('Ctrl Pts',(54.1826120144117,19.18035001467,17.1653173824498));
#27973=CARTESIAN_POINT('Ctrl Pts',(54.196214715213,19.1743005767348,17.1662759446621));
#27974=CARTESIAN_POINT('Ctrl Pts',(54.265604693008,19.1443670294446,17.1711685403789));
#27975=CARTESIAN_POINT('Ctrl Pts',(54.3223881671798,19.1228875648691,17.1751827828518));
#27976=CARTESIAN_POINT('Ctrl Pts',(54.5469272948283,19.049467937643,17.1911038657804));
#27977=CARTESIAN_POINT('Ctrl Pts',(54.7202659108089,19.0171775457291,17.2035801827156));
#27978=CARTESIAN_POINT('Ctrl Pts',(54.9484848791322,19.0052108601123,17.2192326395157));
#27979=CARTESIAN_POINT('Ctrl Pts',(55.0015162116316,19.0045460869513,17.2228082920327));
#27980=CARTESIAN_POINT('Ctrl Pts',(55.0637332178123,19.0062470905787,17.2268855274453));
#27981=CARTESIAN_POINT('Ctrl Pts',(55.0729489975857,19.006563008638,17.2274864112289));
#27982=CARTESIAN_POINT('Ctrl Pts',(55.0871297543628,19.0071476009795,17.2284059871015));
#27983=CARTESIAN_POINT('Ctrl Pts',(55.0920963248733,19.0073709460541,17.22872710234));
#27984=CARTESIAN_POINT('Ctrl Pts',(55.1012374127485,19.0078162676123,17.2293163079198));
#27985=CARTESIAN_POINT('Ctrl Pts',(55.1054120488351,19.0080327969816,17.2295846880311));
#27986=CARTESIAN_POINT('Ctrl Pts',(55.1148235951357,19.008550623565,17.2301881719018));
#27987=CARTESIAN_POINT('Ctrl Pts',(55.120060006064,19.0088594541408,17.2305228520609));
#27988=CARTESIAN_POINT('Ctrl Pts',(55.135482498669,19.0098300959499,17.231505522582));
#27989=CARTESIAN_POINT('Ctrl Pts',(55.1456649715014,19.010549452499,17.2321504037089));
#27990=CARTESIAN_POINT('Ctrl Pts',(55.2255554787207,19.0168101095267,17.2371824809964));
#27991=CARTESIAN_POINT('Ctrl Pts',(55.2949420943089,19.0259359612075,17.2413885968003));
#27992=CARTESIAN_POINT('Ctrl Pts',(55.5301343028818,19.069550926971,17.255509836364));
#27993=CARTESIAN_POINT('Ctrl Pts',(55.6919465233094,19.1214664013584,17.2650516446389));
#27994=CARTESIAN_POINT('Ctrl Pts',(55.8912991074485,19.2147279031276,17.2783045908966));
#27995=CARTESIAN_POINT('Ctrl Pts',(55.9364905981275,19.2380138331888,17.2814127320696));
#27996=CARTESIAN_POINT('Ctrl Pts',(55.9926286619352,19.2697103514369,17.2854328500481));
#27997=CARTESIAN_POINT('Ctrl Pts',(56.0044468267607,19.2765440284278,17.2862883594516));
#27998=CARTESIAN_POINT('Ctrl Pts',(56.0233326361246,19.2877246994094,17.2876708034926));
#27999=CARTESIAN_POINT('Ctrl Pts',(56.0304450579602,19.2919955010819,17.2881949719419));
#28000=CARTESIAN_POINT('Ctrl Pts',(56.0439400335977,19.300213811629,17.2891963846448));
#28001=CARTESIAN_POINT('Ctrl Pts',(56.0503273707911,19.3041532228507,17.2896733262955));
#28002=CARTESIAN_POINT('Ctrl Pts',(56.0648703657362,19.3132363420414,17.2907661182679));
#28003=CARTESIAN_POINT('Ctrl Pts',(56.0730112120985,19.3184032983662,17.2913828195811));
#28004=CARTESIAN_POINT('Ctrl Pts',(56.0941672214076,19.3320470927586,17.2929987012246));
#28005=CARTESIAN_POINT('Ctrl Pts',(56.1071211977915,19.3406171508883,17.2940013323799));
#28006=CARTESIAN_POINT('Ctrl Pts',(56.2288240594514,19.4231924622085,17.303549098214));
#28007=CARTESIAN_POINT('Ctrl Pts',(56.3300818856742,19.5076190556918,17.3125032713316));
#28008=CARTESIAN_POINT('Ctrl Pts',(56.4990739640982,19.6794696141971,17.329253380577));
#28009=CARTESIAN_POINT('Ctrl Pts',(56.5693067563976,19.7637553713725,17.3369560473026));
#28010=CARTESIAN_POINT('Ctrl Pts',(56.6581158761281,19.8901795060794,17.3474820975607));
#28011=CARTESIAN_POINT('Ctrl Pts',(56.6827155839725,19.9278438729621,17.350500671266));
#28012=CARTESIAN_POINT('Ctrl Pts',(56.7106030373156,19.9738699256933,17.3540233582064));
#28013=CARTESIAN_POINT('Ctrl Pts',(56.7151329768377,19.9814595936254,17.3545989923099));
#28014=CARTESIAN_POINT('Ctrl Pts',(56.7220902604696,19.9932941828284,17.3554881498165));
#28015=CARTESIAN_POINT('Ctrl Pts',(56.7245526280848,19.9975182287229,17.35580385691));
#28016=CARTESIAN_POINT('Ctrl Pts',(56.7290950245993,20.005376707975,17.3563880770171));
#28017=CARTESIAN_POINT('Ctrl Pts',(56.7311791244573,20.0090086091838,17.3566568425868));
#28018=CARTESIAN_POINT('Ctrl Pts',(56.7359012342226,20.0172980524552,17.3572674803803));
#28019=CARTESIAN_POINT('Ctrl Pts',(56.7385319412906,20.0219596616678,17.3576088838684));
#28020=CARTESIAN_POINT('Ctrl Pts',(56.7453421432941,20.0341416319052,17.3584960273213));
#28021=CARTESIAN_POINT('Ctrl Pts',(56.7494918565667,20.0416786371629,17.3590399310725));
#28022=CARTESIAN_POINT('Ctrl Pts',(56.7772000836354,20.0927841420803,17.3626960678013));
#28023=CARTESIAN_POINT('Ctrl Pts',(56.799179723665,20.1371941269563,17.3657175979258));
#28024=CARTESIAN_POINT('Ctrl Pts',(56.825032587595,20.1947256362167,17.3694950294889));
#28025=CARTESIAN_POINT('Ctrl Pts',(56.8304545148343,20.2071273568894,17.3703014121258));
#28026=CARTESIAN_POINT('Ctrl Pts',(56.888977488126,20.3447891594825,17.3791754100728));
#28027=CARTESIAN_POINT('Ctrl Pts',(56.9292577720349,20.4751145380018,17.3869001552498));
#28028=CARTESIAN_POINT('Ctrl Pts',(56.9717024110678,20.6871871098442,17.3996379146852));
#28029=CARTESIAN_POINT('Ctrl Pts',(56.9826844779074,20.7667138796778,17.4044450714505));
#28030=CARTESIAN_POINT('Ctrl Pts',(56.9904379101828,20.8672905262963,17.4106814756371));
#28031=CARTESIAN_POINT('Ctrl Pts',(56.9917062433862,20.8879238251917,17.4119688461712));
#28032=CARTESIAN_POINT('Ctrl Pts',(56.9931005896258,20.9183134770827,17.4138782126926));
#28033=CARTESIAN_POINT('Ctrl Pts',(56.9934760871349,20.9280574327564,17.4144924220295));
#28034=CARTESIAN_POINT('Ctrl Pts',(56.9940145442228,20.9453183233746,17.4155841670529));
#28035=CARTESIAN_POINT('Ctrl Pts',(56.9942064773797,20.9528342138752,17.4160607880231));
#28036=CARTESIAN_POINT('Ctrl Pts',(56.9945197054289,20.9685896442367,17.4170626046355));
#28037=CARTESIAN_POINT('Ctrl Pts',(56.9946324413719,20.9768291937568,17.4175880587941));
#28038=CARTESIAN_POINT('Ctrl Pts',(56.9947944057266,20.9984668341991,17.4189720913434));
#28039=CARTESIAN_POINT('Ctrl Pts',(56.9947597048359,21.0118649546367,17.4198332731779));
#28040=CARTESIAN_POINT('Ctrl Pts',(56.9940456106234,21.068248321421,17.4234756260347));
#28041=CARTESIAN_POINT('Ctrl Pts',(56.9921117113091,21.1112033659112,17.4262954821884));
#28042=CARTESIAN_POINT('Ctrl Pts',(56.9865147359738,21.1834559463117,17.4311177745792));
#28043=CARTESIAN_POINT('Ctrl Pts',(56.9835862190795,21.2127967441085,17.4330980854677));
#28044=CARTESIAN_POINT('Ctrl Pts',(56.9596587964209,21.4085182984303,17.4464515129929));
#28045=CARTESIAN_POINT('Ctrl Pts',(56.9184043192903,21.5717202820277,17.458360223942));
#28046=CARTESIAN_POINT('Ctrl Pts',(56.8381678069039,21.7764634803227,17.4734146017883));
#28047=CARTESIAN_POINT('Ctrl Pts',(56.8172023502372,21.8243379752131,17.4769366710391));
#28048=CARTESIAN_POINT('Ctrl Pts',(56.7903659012228,21.8796032744308,17.4809609988127));
#28049=CARTESIAN_POINT('Ctrl Pts',(56.7862953168531,21.8878406554434,17.4815597076296));
#28050=CARTESIAN_POINT('Ctrl Pts',(56.7799378063459,21.9004852103375,17.4824766670891));
#28051=CARTESIAN_POINT('Ctrl Pts',(56.7776911648896,21.9049123339151,17.4827973198358));
#28052=CARTESIAN_POINT('Ctrl Pts',(56.7735221463885,21.9130521548027,17.4833860891038));
#28053=CARTESIAN_POINT('Ctrl Pts',(56.771604634777,21.9167671785994,17.4836544922397));
#28054=CARTESIAN_POINT('Ctrl Pts',(56.7672509304274,21.9251374580231,17.4842585430835));
#28055=CARTESIAN_POINT('Ctrl Pts',(56.7648080212372,21.929789125036,17.4845937635503));
#28056=CARTESIAN_POINT('Ctrl Pts',(56.7584689293285,21.9417447173621,17.4854542599012));
#28057=CARTESIAN_POINT('Ctrl Pts',(56.7545455630325,21.9490342253862,17.4859778761507));
#28058=CARTESIAN_POINT('Ctrl Pts',(56.7298679116876,21.9942085004141,17.4892176432448));
#28059=CARTESIAN_POINT('Ctrl Pts',(56.7079312678399,22.0314382875009,17.4918650088071));
#28060=CARTESIAN_POINT('Ctrl Pts',(56.6706518018995,22.0902516273973,17.496058411627));
#28061=CARTESIAN_POINT('Ctrl Pts',(56.656059795806,22.112291373541,17.4976325065464));
#28062=CARTESIAN_POINT('Ctrl Pts',(56.5530661637046,22.2613308368027,17.5083409481435));
#28063=CARTESIAN_POINT('Ctrl Pts',(56.4505873391505,22.3779582975479,17.5170882911868));
#28064=CARTESIAN_POINT('Ctrl Pts',(56.2870519022641,22.5253875142597,17.53021665306));
#28065=CARTESIAN_POINT('Ctrl Pts',(56.23632679504,22.5667815379512,17.534188922913));
#28066=CARTESIAN_POINT('Ctrl Pts',(56.1717919965796,22.6143570207519,17.5391810022206));
#28067=CARTESIAN_POINT('Ctrl Pts',(56.1598244592822,22.622976364248,17.5401041941419));
#28068=CARTESIAN_POINT('Ctrl Pts',(56.1407803563322,22.6363742309858,17.5415698395245));
#28069=CARTESIAN_POINT('Ctrl Pts',(56.1337666460221,22.6412414916542,17.5421088927472));
#28070=CARTESIAN_POINT('Ctrl Pts',(56.1205615670358,22.6502803001597,17.5431225523562));
#28071=CARTESIAN_POINT('Ctrl Pts',(56.1143775855266,22.6544624169216,17.5435967470435));
#28072=CARTESIAN_POINT('Ctrl Pts',(56.1004775738827,22.6637494606909,17.544661566767));
#28073=CARTESIAN_POINT('Ctrl Pts',(56.0927492503656,22.668835590952,17.5452528837576));
#28074=CARTESIAN_POINT('Ctrl Pts',(56.0730328309638,22.6816155959624,17.5467597816189));
#28075=CARTESIAN_POINT('Ctrl Pts',(56.0609973484829,22.6892350570445,17.5476780928876));
#28076=CARTESIAN_POINT('Ctrl Pts',(55.9880687607172,22.7343180603892,17.5532343389441));
#28077=CARTESIAN_POINT('Ctrl Pts',(55.9252859664274,22.7686104150834,17.5579862155025));
#28078=CARTESIAN_POINT('Ctrl Pts',(55.7123592879946,22.8704679564178,17.5740010576374));
#28079=CARTESIAN_POINT('Ctrl Pts',(55.5557191482132,22.9228294359365,17.5856835241405));
#28080=CARTESIAN_POINT('Ctrl Pts',(55.343557311208,22.9656272243959,17.6004974378189));
#28081=CARTESIAN_POINT('Ctrl Pts',(55.2922877788073,22.9739024557423,17.6039965427397));
#28082=CARTESIAN_POINT('Ctrl Pts',(55.2316426747659,22.981275697247,17.607998169059));
#28083=CARTESIAN_POINT('Ctrl Pts',(55.2225284005698,22.9823200639648,17.6085959305618));
#28084=CARTESIAN_POINT('Ctrl Pts',(55.2084741055388,22.9838323329807,17.6095117502064));
#28085=CARTESIAN_POINT('Ctrl Pts',(55.2035391449796,22.9843447270625,17.6098322013106));
#28086=CARTESIAN_POINT('Ctrl Pts',(55.1944420827845,22.985254975888,17.6104207808997));
#28087=CARTESIAN_POINT('Ctrl Pts',(55.1902806623755,22.9856581561204,17.6106891946222));
#28088=CARTESIAN_POINT('Ctrl Pts',(55.1808830002383,22.9865388361046,17.6112934951304));
#28089=CARTESIAN_POINT('Ctrl Pts',(55.1756461292743,22.9870087181303,17.6116289530757));
#28090=CARTESIAN_POINT('Ctrl Pts',(55.1684213005163,22.9876281849431,17.6120900505316));
#28091=CARTESIAN_POINT('Ctrl Pts',(55.1664349523431,22.9877954982159,17.6122166442961));
#28092=CARTESIAN_POINT('Ctrl Pts',(55.1644483516309,22.987959834138,17.6123430797447));
#28093=CARTESIAN_POINT('Origin',(55.,21.,6.22095488139522));
#28094=CARTESIAN_POINT('',(55.1644483870895,22.9879598312048,18.5698477239299));
#28095=CARTESIAN_POINT('',(55.1644483276976,22.9879598361178,18.4096837786395));
#28096=CARTESIAN_POINT('',(55.1644483516311,22.987959834138,6.22095488139522));
#28097=CARTESIAN_POINT('',(53.005250018775,20.9997263157889,17.977164327174));
#28098=CARTESIAN_POINT('Ctrl Pts',(55.1644483870895,22.9879598312048,18.5698477239299));
#28099=CARTESIAN_POINT('Ctrl Pts',(55.2202125884814,22.9833468944481,18.5664985446111));
#28100=CARTESIAN_POINT('Ctrl Pts',(55.2757651209119,22.9763890857523,18.5630945022204));
#28101=CARTESIAN_POINT('Ctrl Pts',(55.345429404889,22.9646682653898,18.5587047603187));
#28102=CARTESIAN_POINT('Ctrl Pts',(55.3598716684571,22.9620742164863,18.557788148223));
#28103=CARTESIAN_POINT('Ctrl Pts',(55.3835013436058,22.9575603049037,18.5562770626812));
#28104=CARTESIAN_POINT('Ctrl Pts',(55.392706313787,22.9557344845718,18.5556855752152));
#28105=CARTESIAN_POINT('Ctrl Pts',(55.4092231058344,22.9523370458588,18.5546189895675));
#28106=CARTESIAN_POINT('Ctrl Pts',(55.4165396644161,22.9507891214737,18.5541446552504));
#28107=CARTESIAN_POINT('Ctrl Pts',(55.4321058374983,22.9474043074352,18.5531314494343));
#28108=CARTESIAN_POINT('Ctrl Pts',(55.4403528068018,22.9455560627577,18.5525922226949));
#28109=CARTESIAN_POINT('Ctrl Pts',(55.4625706111333,22.9404282850618,18.5511328271776));
#28110=CARTESIAN_POINT('Ctrl Pts',(55.4765179982505,22.9370503553693,18.5502095202972));
#28111=CARTESIAN_POINT('Ctrl Pts',(55.5481631395077,22.918877954508,18.5454287629383));
#28112=CARTESIAN_POINT('Ctrl Pts',(55.6052083342172,22.901656402103,18.5414937754309));
#28113=CARTESIAN_POINT('Ctrl Pts',(55.8080857904678,22.8303555804687,18.5270216142908));
#28114=CARTESIAN_POINT('Ctrl Pts',(55.9482365999881,22.7618286765473,18.5160567343815));
#28115=CARTESIAN_POINT('Ctrl Pts',(56.0848077522488,22.6739975041881,18.5048197954305));
#28116=CARTESIAN_POINT('Ctrl Pts',(56.0906118277199,22.6702219450827,18.5043412342372));
#28117=CARTESIAN_POINT('Ctrl Pts',(56.1156936467252,22.6537196992259,18.5022691095257));
#28118=CARTESIAN_POINT('Ctrl Pts',(56.1347696941903,22.6406885623914,18.5006826648513));
#28119=CARTESIAN_POINT('Ctrl Pts',(56.1905374747404,22.6011547035486,18.4960220325946));
#28120=CARTESIAN_POINT('Ctrl Pts',(56.2265612268519,22.5737293719741,18.4929814162581));
#28121=CARTESIAN_POINT('Ctrl Pts',(56.2681240496237,22.5397919946942,18.4894657435641));
#28122=CARTESIAN_POINT('Ctrl Pts',(56.2745911126011,22.5344430565401,18.4889184978524));
#28123=CARTESIAN_POINT('Ctrl Pts',(56.2850790040417,22.5256564145294,18.4880309224914));
#28124=CARTESIAN_POINT('Ctrl Pts',(56.2891201776302,22.5222433153131,18.4876889028458));
#28125=CARTESIAN_POINT('Ctrl Pts',(56.2963334785277,22.5161017711609,18.487078451632));
#28126=CARTESIAN_POINT('Ctrl Pts',(56.2995106313505,22.5133793933153,18.4868095917362));
#28127=CARTESIAN_POINT('Ctrl Pts',(56.306419722873,22.5074214622475,18.4862249701831));
#28128=CARTESIAN_POINT('Ctrl Pts',(56.3101482119455,22.5041820438922,18.4859094990922));
#28129=CARTESIAN_POINT('Ctrl Pts',(56.3206857875882,22.494957789727,18.4850178319057));
#28130=CARTESIAN_POINT('Ctrl Pts',(56.3274662671838,22.4889402471251,18.4844439955723));
#28131=CARTESIAN_POINT('Ctrl Pts',(56.3709811532486,22.4497880963588,18.4807589261419));
#28132=CARTESIAN_POINT('Ctrl Pts',(56.4065165324325,22.4153398879028,18.4777384577085));
#28133=CARTESIAN_POINT('Ctrl Pts',(56.5406647906645,22.2752471144406,18.466114250022));
#28134=CARTESIAN_POINT('Ctrl Pts',(56.6289641326701,22.1603382267268,18.457933684225));
#28135=CARTESIAN_POINT('Ctrl Pts',(56.7521688761919,21.9578573946524,18.4440097988615));
#28136=CARTESIAN_POINT('Ctrl Pts',(56.7946968886593,21.8755834700867,18.4384725327784));
#28137=CARTESIAN_POINT('Ctrl Pts',(56.8373387112217,21.7768149834651,18.4317913221677));
#28138=CARTESIAN_POINT('Ctrl Pts',(56.843159787831,21.7629004097895,18.4308495168397));
#28139=CARTESIAN_POINT('Ctrl Pts',(56.8523923454617,21.7401084879591,18.4293053128249));
#28140=CARTESIAN_POINT('Ctrl Pts',(56.8558991930661,21.7312702343236,18.4287061296352));
#28141=CARTESIAN_POINT('Ctrl Pts',(56.8620555756946,21.7154248465002,18.4276310888642));
#28142=CARTESIAN_POINT('Ctrl Pts',(56.8647290979311,21.7084271781865,18.4271560458992));
#28143=CARTESIAN_POINT('Ctrl Pts',(56.8703080200864,21.6935745189449,18.4261470872008));
#28144=CARTESIAN_POINT('Ctrl Pts',(56.8732034860626,21.6857159759003,18.4256128508302));
#28145=CARTESIAN_POINT('Ctrl Pts',(56.8808075065142,21.6646704084152,18.4241809628902));
#28146=CARTESIAN_POINT('Ctrl Pts',(56.8854267721292,21.6514518391507,18.4232803735629));
#28147=CARTESIAN_POINT('Ctrl Pts',(56.9074990060411,21.5860877360653,18.4188202022194));
#28148=CARTESIAN_POINT('Ctrl Pts',(56.922928281924,21.5332889833962,18.4151950318157));
#28149=CARTESIAN_POINT('Ctrl Pts',(56.986222630186,21.2779409735762,18.3975451254666));
#28150=CARTESIAN_POINT('Ctrl Pts',(57.0043675350158,21.06941396785,18.3826081914984));
#28151=CARTESIAN_POINT('Ctrl Pts',(56.9878730977885,20.8317792311816,18.3665679747899));
#28152=CARTESIAN_POINT('Ctrl Pts',(56.9851015121624,20.8017327510515,18.364561594309));
#28153=CARTESIAN_POINT('Ctrl Pts',(56.980713358151,20.7636336529914,18.3620546121964));
#28154=CARTESIAN_POINT('Ctrl Pts',(56.979727535631,20.7555141161702,18.3615224875028));
#28155=CARTESIAN_POINT('Ctrl Pts',(56.9780908080833,20.7426931011819,18.3606858942117));
#28156=CARTESIAN_POINT('Ctrl Pts',(56.9774730306547,20.7379875968981,18.3603796300042));
#28157=CARTESIAN_POINT('Ctrl Pts',(56.9763316031958,20.7295275866611,18.3598304533164));
#28158=CARTESIAN_POINT('Ctrl Pts',(56.9758140492738,20.7257724026701,18.3595872092326));
#28159=CARTESIAN_POINT('Ctrl Pts',(56.9745408872015,20.7167255415235,18.3590024230482));
#28160=CARTESIAN_POINT('Ctrl Pts',(56.9737747108645,20.7114354034022,18.3586614796522));
#28161=CARTESIAN_POINT('Ctrl Pts',(56.9713610039278,20.6952292231322,18.3576199293075));
#28162=CARTESIAN_POINT('Ctrl Pts',(56.9696440790612,20.6843235054932,18.3569230977361));
#28163=CARTESIAN_POINT('Ctrl Pts',(56.9497303468782,20.5643270280834,18.3492950633841));
#28164=CARTESIAN_POINT('Ctrl Pts',(56.9225786224382,20.4568996828676,18.3428184475189));
#28165=CARTESIAN_POINT('Ctrl Pts',(56.8339257917892,20.1986810104784,18.3269484744231));
#28166=CARTESIAN_POINT('Ctrl Pts',(56.7626484749413,20.0521286071546,18.3176222977082));
#28167=CARTESIAN_POINT('Ctrl Pts',(56.6619496819017,19.8966071660058,18.3062011074394));
#28168=CARTESIAN_POINT('Ctrl Pts',(56.6491672172954,19.877591913113,18.3047773687284));
#28169=CARTESIAN_POINT('Ctrl Pts',(56.6306855909202,19.8510960302802,18.3027525202415));
#28170=CARTESIAN_POINT('Ctrl Pts',(56.62525642031,19.8434286051115,18.3021616208862));
#28171=CARTESIAN_POINT('Ctrl Pts',(56.615693738953,19.830123867528,18.3011274610985));
#28172=CARTESIAN_POINT('Ctrl Pts',(56.6115843523806,19.8244693553302,18.3006851314795));
#28173=CARTESIAN_POINT('Ctrl Pts',(56.6029112088682,19.8126660734097,18.2997558291476));
#28174=CARTESIAN_POINT('Ctrl Pts',(56.5983416052488,19.8065217609895,18.2992686342007));
#28175=CARTESIAN_POINT('Ctrl Pts',(56.5873590699229,19.7919307901023,18.2981033663541));
#28176=CARTESIAN_POINT('Ctrl Pts',(56.5809139841092,19.7835087339296,18.2974240402795));
#28177=CARTESIAN_POINT('Ctrl Pts',(56.5587470114853,19.7550159351203,18.2951025025564));
#28178=CARTESIAN_POINT('Ctrl Pts',(56.5427081649495,19.7351960683515,18.2934477762744));
#28179=CARTESIAN_POINT('Ctrl Pts',(56.5032928554732,19.6883542950074,18.2894381428955));
#28180=CARTESIAN_POINT('Ctrl Pts',(56.4795623183198,19.6616431909438,18.28706941898));
#28181=CARTESIAN_POINT('Ctrl Pts',(56.319862845399,19.4913260526437,18.2714147125477));
#28182=CARTESIAN_POINT('Ctrl Pts',(56.1639299389151,19.3680133961798,18.2572811155302));
#28183=CARTESIAN_POINT('Ctrl Pts',(55.9577238662413,19.2497446771605,18.2411368997023));
#28184=CARTESIAN_POINT('Ctrl Pts',(55.9224194627306,19.2308839644028,18.2384575581676));
#28185=CARTESIAN_POINT('Ctrl Pts',(55.8786186609643,19.2091522745397,18.2352560130777));
#28186=CARTESIAN_POINT('Ctrl Pts',(55.8706420409106,19.2052608070149,18.2346778420237));
#28187=CARTESIAN_POINT('Ctrl Pts',(55.8581742485012,19.1992809638347,18.2337819990987));
#28188=CARTESIAN_POINT('Ctrl Pts',(55.8537009403369,19.197155915294,18.2334621466761));
#28189=CARTESIAN_POINT('Ctrl Pts',(55.8454347400095,19.1932667158331,18.2328740408688));
#28190=CARTESIAN_POINT('Ctrl Pts',(55.8416442331606,19.1914978448726,18.2326055068407));
#28191=CARTESIAN_POINT('Ctrl Pts',(55.8330630260706,19.1875261771249,18.2320001444627));
#28192=CARTESIAN_POINT('Ctrl Pts',(55.8282691473866,19.1853304474255,18.2316637508312));
#28193=CARTESIAN_POINT('Ctrl Pts',(55.8137451246246,19.1787475861821,18.2306498185943));
#28194=CARTESIAN_POINT('Ctrl Pts',(55.8039882351973,19.1744194314529,18.2299757700748));
#28195=CARTESIAN_POINT('Ctrl Pts',(55.7813582296454,19.1645973849098,18.2284276529297));
#28196=CARTESIAN_POINT('Ctrl Pts',(55.7684609545631,19.1591601841217,18.2275566643062));
#28197=CARTESIAN_POINT('Ctrl Pts',(55.7242738048925,19.141077217006,18.2246074913335));
#28198=CARTESIAN_POINT('Ctrl Pts',(55.6927193180748,19.1290893488974,18.2225606579838));
#28199=CARTESIAN_POINT('Ctrl Pts',(55.5183778678744,19.0678714553228,18.2114948815126));
#28200=CARTESIAN_POINT('Ctrl Pts',(55.3706537662896,19.0341774636865,18.2029643591093));
#28201=CARTESIAN_POINT('Ctrl Pts',(55.1355711628408,19.0080271136283,18.1890247390312));
#28202=CARTESIAN_POINT('Ctrl Pts',(55.0500986170244,19.0040483494604,18.1838906530859));
#28203=CARTESIAN_POINT('Ctrl Pts',(54.9497892416695,19.0058267161011,18.1776580658687));
#28204=CARTESIAN_POINT('Ctrl Pts',(54.9349412163163,19.0062558984568,18.1767303323942));
#28205=CARTESIAN_POINT('Ctrl Pts',(54.9106679695835,19.0072289517114,18.1752046208743));
#28206=CARTESIAN_POINT('Ctrl Pts',(54.9012391984114,19.0076739820777,18.1746097291929));
#28207=CARTESIAN_POINT('Ctrl Pts',(54.8843412544219,19.0085917985542,18.1735394184055));
#28208=CARTESIAN_POINT('Ctrl Pts',(54.8768708670858,19.0090397331067,18.1730647856077));
#28209=CARTESIAN_POINT('Ctrl Pts',(54.8610045068052,19.0100807408148,18.1720535309262));
#28210=CARTESIAN_POINT('Ctrl Pts',(54.852609434091,19.0106849362897,18.1715165694118));
#28211=CARTESIAN_POINT('Ctrl Pts',(54.8300695381513,19.012450598502,18.1700696687479));
#28212=CARTESIAN_POINT('Ctrl Pts',(54.8159330798686,19.0137099061572,18.1691566831818));
#28213=CARTESIAN_POINT('Ctrl Pts',(54.7446656905325,19.0208258890891,18.1645251761169));
#28214=CARTESIAN_POINT('Ctrl Pts',(54.6877982594137,19.0289965153539,18.1607348160656));
#28215=CARTESIAN_POINT('Ctrl Pts',(54.5214216863452,19.0602820491896,18.1493578524263));
#28216=CARTESIAN_POINT('Ctrl Pts',(54.4134219282403,19.0901665261438,18.1415873595785));
#28217=CARTESIAN_POINT('Ctrl Pts',(54.204424388932,19.1674061561086,18.1260456705321));
#28218=CARTESIAN_POINT('Ctrl Pts',(54.1037211095135,19.2144945524295,18.1183043979673));
#28219=CARTESIAN_POINT('Ctrl Pts',(53.9936629048854,19.2776278481176,18.1098988340941));
#28220=CARTESIAN_POINT('Ctrl Pts',(53.9799707464633,19.2857011524708,18.1088543676414));
#28221=CARTESIAN_POINT('Ctrl Pts',(53.9610134601336,19.2971864913064,18.107411577396));
#28222=CARTESIAN_POINT('Ctrl Pts',(53.9556661370826,19.3004607504565,18.1070049789038));
#28223=CARTESIAN_POINT('Ctrl Pts',(53.9467445197301,19.3059816185808,18.1063273403788));
#28224=CARTESIAN_POINT('Ctrl Pts',(53.9431618040958,19.3082144309057,18.106055417801));
#28225=CARTESIAN_POINT('Ctrl Pts',(53.9359489083239,19.3127414904947,18.105508420365));
#28226=CARTESIAN_POINT('Ctrl Pts',(53.9323189970091,19.3150361190162,18.1052333744081));
#28227=CARTESIAN_POINT('Ctrl Pts',(53.9249611539264,19.3197206629811,18.1046762671901));
#28228=CARTESIAN_POINT('Ctrl Pts',(53.9212337082464,19.3221113089179,18.1043942555766));
#28229=CARTESIAN_POINT('Ctrl Pts',(53.9122873276334,19.3278913226216,18.1037178310794));
#28230=CARTESIAN_POINT('Ctrl Pts',(53.9070761941631,19.3312927627624,18.1033241875757));
#28231=CARTESIAN_POINT('Ctrl Pts',(53.8680422959972,19.3570324758745,18.1003776665499));
#28232=CARTESIAN_POINT('Ctrl Pts',(53.8348888402359,19.3803744132371,18.0978866511344));
#28233=CARTESIAN_POINT('Ctrl Pts',(53.7264717610765,19.4617597363295,18.0896971088378));
#28234=CARTESIAN_POINT('Ctrl Pts',(53.6546436625375,19.5241692333759,18.0841941283589));
#28235=CARTESIAN_POINT('Ctrl Pts',(53.4888799811698,19.6903956552318,18.0705749288932));
#28236=CARTESIAN_POINT('Ctrl Pts',(53.40090425155,19.7994026292388,18.0624607386536));
#28237=CARTESIAN_POINT('Ctrl Pts',(53.311973076662,19.9369046592596,18.0523783459512));
#28238=CARTESIAN_POINT('Ctrl Pts',(53.2992721075174,19.9573441816079,18.05088428344));
#28239=CARTESIAN_POINT('Ctrl Pts',(53.2820303870684,19.9862446230175,18.0487757877934));
#28240=CARTESIAN_POINT('Ctrl Pts',(53.2771759181116,19.9945166669516,18.0481727405671));
#28241=CARTESIAN_POINT('Ctrl Pts',(53.2688625729294,20.0089196206766,18.0471233726622));
#28242=CARTESIAN_POINT('Ctrl Pts',(53.2653761151732,20.0150344748127,18.0466780540171));
#28243=CARTESIAN_POINT('Ctrl Pts',(53.2581841963012,20.0278049091693,18.045748379084));
#28244=CARTESIAN_POINT('Ctrl Pts',(53.2544843548618,20.0344635073783,18.0452638309936));
#28245=CARTESIAN_POINT('Ctrl Pts',(53.2458326394616,20.050246240761,18.0441156820576));
#28246=CARTESIAN_POINT('Ctrl Pts',(53.2409137129459,20.0593880928241,18.0434509238052));
#28247=CARTESIAN_POINT('Ctrl Pts',(53.224784615579,20.0899331561639,18.0412304976867));
#28248=CARTESIAN_POINT('Ctrl Pts',(53.2138923275532,20.1115009180208,18.0396637443223));
#28249=CARTESIAN_POINT('Ctrl Pts',(53.1889188276402,20.163266777723,18.0359042936883));
#28250=CARTESIAN_POINT('Ctrl Pts',(53.1751975650715,20.193629516267,18.0336999461982));
#28251=CARTESIAN_POINT('Ctrl Pts',(53.0963511761303,20.3804339800807,18.0201404974891));
#28252=CARTESIAN_POINT('Ctrl Pts',(53.0506263109386,20.5442951756006,18.0081741166929));
#28253=CARTESIAN_POINT('Ctrl Pts',(53.0183460487092,20.765471068342,17.9927254304657));
#28254=CARTESIAN_POINT('Ctrl Pts',(53.0127123528883,20.8193209261681,17.9890251584671));
#28255=CARTESIAN_POINT('Ctrl Pts',(53.0079015399726,20.8949310862832,17.9839693754571));
#28256=CARTESIAN_POINT('Ctrl Pts',(53.0068789659841,20.9165470964787,17.9825399757031));
#28257=CARTESIAN_POINT('Ctrl Pts',(53.0059889285599,20.9452505700444,17.9806667847098));
#28258=CARTESIAN_POINT('Ctrl Pts',(53.0058072219952,20.9523258885091,17.9802070541033));
#28259=CARTESIAN_POINT('Ctrl Pts',(53.0055702728741,20.9639658246103,17.9794541920673));
#28260=CARTESIAN_POINT('Ctrl Pts',(53.0054930359905,20.9685298589266,17.9791598692181));
#28261=CARTESIAN_POINT('Ctrl Pts',(53.0053776218438,20.9770856796647,17.9786098177043));
#28262=CARTESIAN_POINT('Ctrl Pts',(53.0053357599012,20.9810773405698,17.9783538897146));
#28263=CARTESIAN_POINT('Ctrl Pts',(53.0052817465577,20.9882932692173,17.9778924539535));
#28264=CARTESIAN_POINT('Ctrl Pts',(53.0052654298016,20.9915174903657,17.9776867142566));
#28265=CARTESIAN_POINT('Ctrl Pts',(53.0052525506544,20.9964032715986,17.9773755954274));
#28266=CARTESIAN_POINT('Ctrl Pts',(53.0052502467401,20.9980647900871,17.9772699057812));
#28267=CARTESIAN_POINT('Ctrl Pts',(53.005250018775,20.9997263157889,17.977164327174));
#28268=CARTESIAN_POINT('Ctrl Pts',(53.0052500188593,20.9997257026673,17.9771643661337));
#28269=CARTESIAN_POINT('Ctrl Pts',(53.0052494450772,21.0038983710389,17.9768992214964));
#28270=CARTESIAN_POINT('Ctrl Pts',(53.0052619640291,21.0080710814626,17.9766347773869));
#28271=CARTESIAN_POINT('Ctrl Pts',(53.0053538573503,21.0230420189037,17.9756884241139));
#28272=CARTESIAN_POINT('Ctrl Pts',(53.005507822225,21.0338398229537,17.9750103918437));
#28273=CARTESIAN_POINT('Ctrl Pts',(53.0071547221884,21.1074199519088,17.9704176544664));
#28274=CARTESIAN_POINT('Ctrl Pts',(53.0115242338651,21.1701089876393,17.9666413452699));
#28275=CARTESIAN_POINT('Ctrl Pts',(53.0387504349818,21.4021129147237,17.9528371188982));
#28276=CARTESIAN_POINT('Ctrl Pts',(53.0803544361884,21.5684703042354,17.9432174536033));
#28277=CARTESIAN_POINT('Ctrl Pts',(53.1612566031942,21.7750193040438,17.9298618881239));
#28278=CARTESIAN_POINT('Ctrl Pts',(53.1816851286079,21.8218044507097,17.926741108731));
#28279=CARTESIAN_POINT('Ctrl Pts',(53.2098315604115,21.8800633292514,17.9227065457421));
#28280=CARTESIAN_POINT('Ctrl Pts',(53.2159057361774,21.8923128087379,17.9218497314756));
#28281=CARTESIAN_POINT('Ctrl Pts',(53.2258698832391,21.911898470956,17.9204655842242));
#28282=CARTESIAN_POINT('Ctrl Pts',(53.2296806400684,21.9192746341561,17.9199410285296));
#28283=CARTESIAN_POINT('Ctrl Pts',(53.2370240187829,21.9332735882501,17.9189391422026));
#28284=CARTESIAN_POINT('Ctrl Pts',(53.2405481991838,21.9399006644069,17.9184621161182));
#28285=CARTESIAN_POINT('Ctrl Pts',(53.2486829115608,21.9549915760907,17.9173695054215));
#28286=CARTESIAN_POINT('Ctrl Pts',(53.2533175241753,21.96344215079,17.916753072165));
#28287=CARTESIAN_POINT('Ctrl Pts',(53.2655714428253,21.9854064195783,17.9151386657299));
#28288=CARTESIAN_POINT('Ctrl Pts',(53.2732873599082,21.9988651899356,17.9141372533314));
#28289=CARTESIAN_POINT('Ctrl Pts',(53.3472771587176,22.1245050057304,17.904671824096));
#28290=CARTESIAN_POINT('Ctrl Pts',(53.4242234170566,22.2300084939949,17.8958069767272));
#28291=CARTESIAN_POINT('Ctrl Pts',(53.5722309234845,22.3960669040283,17.8803521929355));
#28292=CARTESIAN_POINT('Ctrl Pts',(53.6382716916887,22.4605559430281,17.8738812392954));
#28293=CARTESIAN_POINT('Ctrl Pts',(53.7406474613458,22.5475251183407,17.8646335643374));
#28294=CARTESIAN_POINT('Ctrl Pts',(53.7736169143373,22.5737813678214,17.8617621345993));
#28295=CARTESIAN_POINT('Ctrl Pts',(53.8204541377859,22.6087151778961,17.8578529871092));
#28296=CARTESIAN_POINT('Ctrl Pts',(53.8336323024185,22.6182952129195,17.8567710266859));
#28297=CARTESIAN_POINT('Ctrl Pts',(53.8567349434588,22.634661141775,17.8549071425359));
#28298=CARTESIAN_POINT('Ctrl Pts',(53.8666059702485,22.6415206451121,17.8541209796374));
#28299=CARTESIAN_POINT('Ctrl Pts',(53.8810525446767,22.6513673107975,17.8529858737762));
#28300=CARTESIAN_POINT('Ctrl Pts',(53.8855790877041,22.6544254092883,17.8526323942762));
#28301=CARTESIAN_POINT('Ctrl Pts',(53.8934926366194,22.65972452833,17.8520182980648));
#28302=CARTESIAN_POINT('Ctrl Pts',(53.896873999554,22.6619738516238,17.8517571298189));
#28303=CARTESIAN_POINT('Ctrl Pts',(53.9040795682481,22.6667354032401,17.8512032186045));
#28304=CARTESIAN_POINT('Ctrl Pts',(53.9079055554001,22.6692448059649,17.8509106628627));
#28305=CARTESIAN_POINT('Ctrl Pts',(53.9180341847305,22.6758382794084,17.8501401838109));
#28306=CARTESIAN_POINT('Ctrl Pts',(53.9243513879879,22.6799000065192,17.8496637194643));
#28307=CARTESIAN_POINT('Ctrl Pts',(53.9520022329641,22.6974585470658,17.8475952425497));
#28308=CARTESIAN_POINT('Ctrl Pts',(53.9735691118003,22.710586042899,17.8460258710962));
#28309=CARTESIAN_POINT('Ctrl Pts',(54.1798420557591,22.8308353659649,17.8313698557903));
#28310=CARTESIAN_POINT('Ctrl Pts',(54.3803894157015,22.9080688046697,17.8196276533187));
#28311=CARTESIAN_POINT('Ctrl Pts',(54.6435865608881,22.963431601144,17.8034844103809));
#28312=CARTESIAN_POINT('Ctrl Pts',(54.6982247080355,22.9725681278073,17.8001057467596));
#28313=CARTESIAN_POINT('Ctrl Pts',(54.7670941439632,22.9811560661568,17.7957802291301));
#28314=CARTESIAN_POINT('Ctrl Pts',(54.7810372469934,22.982745519,17.794901152001));
#28315=CARTESIAN_POINT('Ctrl Pts',(54.8033331284136,22.9850491074886,17.7934896356091));
#28316=CARTESIAN_POINT('Ctrl Pts',(54.8116758145035,22.9858579544376,17.7929601765003));
#28317=CARTESIAN_POINT('Ctrl Pts',(54.8274824888452,22.9872899556359,17.791954464385));
#28318=CARTESIAN_POINT('Ctrl Pts',(54.834945391041,22.9879236989832,17.7914785527464));
#28319=CARTESIAN_POINT('Ctrl Pts',(54.8518789490896,22.9892656711317,17.7903961697416));
#28320=CARTESIAN_POINT('Ctrl Pts',(54.8613513944569,22.9899483197032,17.7897889072776));
#28321=CARTESIAN_POINT('Ctrl Pts',(54.8858414105554,22.9915375276376,17.7882141125563));
#28322=CARTESIAN_POINT('Ctrl Pts',(54.9008647894016,22.9923418624736,17.7872434114754));
#28323=CARTESIAN_POINT('Ctrl Pts',(54.9987883104993,22.9964742798257,17.7808848360862));
#28324=CARTESIAN_POINT('Ctrl Pts',(55.0817996358081,22.9947967157224,17.7753425660883));
#28325=CARTESIAN_POINT('Ctrl Pts',(55.1644483624361,22.9879598332441,17.7696788290115));
#28326=CARTESIAN_POINT('Ctrl Pts',(55.1644483516309,22.987959834138,17.6123430797447));
#28327=CARTESIAN_POINT('Ctrl Pts',(55.1562045015407,22.9886417833077,17.6128677523061));
#28328=CARTESIAN_POINT('Ctrl Pts',(55.1479563026721,22.9892724618085,17.6133896986423));
#28329=CARTESIAN_POINT('Ctrl Pts',(55.0677606366728,22.9949028679997,17.6184373849476));
#28330=CARTESIAN_POINT('Ctrl Pts',(54.9955872414676,22.9960490787526,17.6227690321975));
#28331=CARTESIAN_POINT('Ctrl Pts',(54.8040372429016,22.988697859225,17.6340712088978));
#28332=CARTESIAN_POINT('Ctrl Pts',(54.6852244011128,22.9733824803268,17.6408932882945));
#28333=CARTESIAN_POINT('Ctrl Pts',(54.4852692573094,22.9290791790024,17.6529245798835));
#28334=CARTESIAN_POINT('Ctrl Pts',(54.4033195040415,22.9053251999907,17.6580186770147));
#28335=CARTESIAN_POINT('Ctrl Pts',(54.3030787995379,22.8691665230097,17.6646019813089));
#28336=CARTESIAN_POINT('Ctrl Pts',(54.2831296890994,22.8616067127958,17.6659298580941));
#28337=CARTESIAN_POINT('Ctrl Pts',(54.2541292348581,22.8500815880836,17.6678880000106));
#28338=CARTESIAN_POINT('Ctrl Pts',(54.2449795764475,22.8463664953737,17.668509886183));
#28339=CARTESIAN_POINT('Ctrl Pts',(54.2288974532969,22.8396970421661,17.6696103633674));
#28340=CARTESIAN_POINT('Ctrl Pts',(54.2219533876263,22.8367710284402,17.6700879885599));
#28341=CARTESIAN_POINT('Ctrl Pts',(54.2075044672345,22.830586063314,17.6710870168727));
#28342=CARTESIAN_POINT('Ctrl Pts',(54.2000027644792,22.8273201483388,17.6716086499419));
#28343=CARTESIAN_POINT('Ctrl Pts',(54.1805134167674,22.8186923198195,17.6729716623769));
#28344=CARTESIAN_POINT('Ctrl Pts',(54.1685584088082,22.8132580845056,17.6738155028113));
#28345=CARTESIAN_POINT('Ctrl Pts',(54.1197620705901,22.7904933282162,17.6772922870721));
#28346=CARTESIAN_POINT('Ctrl Pts',(54.0834040458055,22.7721559259544,17.6799596723616));
#28347=CARTESIAN_POINT('Ctrl Pts',(53.9238312740723,22.6854497877812,17.6920224988731));
#28348=CARTESIAN_POINT('Ctrl Pts',(53.8075206808867,22.6052606332593,17.701825405699));
#28349=CARTESIAN_POINT('Ctrl Pts',(53.6250892957,22.4486422179421,17.7185907525939));
#28350=CARTESIAN_POINT('Ctrl Pts',(53.5544889031656,22.3782036715191,17.7255086726988));
#28351=CARTESIAN_POINT('Ctrl Pts',(53.4782604843642,22.2898175871467,17.7332500684554));
#28352=CARTESIAN_POINT('Ctrl Pts',(53.4672480082366,22.2767113772083,17.7343756775415));
#28353=CARTESIAN_POINT('Ctrl Pts',(53.4523683839545,22.2585327019815,17.7359047365575));
#28354=CARTESIAN_POINT('Ctrl Pts',(53.448355185388,22.253581490339,17.7363179793279));
#28355=CARTESIAN_POINT('Ctrl Pts',(53.4416433816397,22.2452193090097,17.7370103967235));
#28356=CARTESIAN_POINT('Ctrl Pts',(53.4389321025213,22.2418186252974,17.7372904643731));
#28357=CARTESIAN_POINT('Ctrl Pts',(53.4337996127573,22.2353377104096,17.7378212816247));
#28358=CARTESIAN_POINT('Ctrl Pts',(53.4313763284458,22.2322591811168,17.738072183426));
#28359=CARTESIAN_POINT('Ctrl Pts',(53.4250302557155,22.2241481042436,17.7387300372019));
#28360=CARTESIAN_POINT('Ctrl Pts',(53.4211224777992,22.219103789306,17.7391359345444));
#28361=CARTESIAN_POINT('Ctrl Pts',(53.4075409594136,22.2013973826035,17.7405498094826));
#28362=CARTESIAN_POINT('Ctrl Pts',(53.3979944938757,22.188637818215,17.7415493208835));
#28363=CARTESIAN_POINT('Ctrl Pts',(53.3233700787058,22.0863642451851,17.749420566706));
#28364=CARTESIAN_POINT('Ctrl Pts',(53.2656825385003,21.9916776715775,17.7558701204304));
#28365=CARTESIAN_POINT('Ctrl Pts',(53.1659830209991,21.792447182916,17.7688056194371));
#28366=CARTESIAN_POINT('Ctrl Pts',(53.1243633307069,21.688168563644,17.7752727116892));
#28367=CARTESIAN_POINT('Ctrl Pts',(53.0749785239509,21.5259515459231,17.7854357337141));
#28368=CARTESIAN_POINT('Ctrl Pts',(53.0606218528491,21.4702596896598,17.78893955973));
#28369=CARTESIAN_POINT('Ctrl Pts',(53.0457447154624,21.4001441262871,17.7934057894077));
#28370=CARTESIAN_POINT('Ctrl Pts',(53.0429469182247,21.3862282454544,17.794294799184));
#28371=CARTESIAN_POINT('Ctrl Pts',(53.0387272992062,21.3640161793848,17.795718427982));
#28372=CARTESIAN_POINT('Ctrl Pts',(53.0372090268368,21.3557386370439,17.7962499738281));
#28373=CARTESIAN_POINT('Ctrl Pts',(53.0344400697943,21.3400848337445,17.7972572138348));
#28374=CARTESIAN_POINT('Ctrl Pts',(53.0331784118291,21.3327106418171,17.7977325503167));
#28375=CARTESIAN_POINT('Ctrl Pts',(53.0304196251321,21.3160216987476,17.7988103008251));
#28376=CARTESIAN_POINT('Ctrl Pts',(53.028947044128,21.3067031255748,17.7994134810618));
#28377=CARTESIAN_POINT('Ctrl Pts',(53.0253279823429,21.2826982085954,17.8009710425391));
#28378=CARTESIAN_POINT('Ctrl Pts',(53.0232792450156,21.2679979319093,17.8019284794512));
#28379=CARTESIAN_POINT('Ctrl Pts',(53.0105718795586,21.168727525581,17.8084195391141));
#28380=CARTESIAN_POINT('Ctrl Pts',(53.0051808167741,21.0835833700158,17.814117348025));
#28381=CARTESIAN_POINT('Ctrl Pts',(53.0053221874591,20.9111163160786,17.8259064425452));
#28382=CARTESIAN_POINT('Ctrl Pts',(53.011117899514,20.8239711767105,17.8319914019213));
#28383=CARTESIAN_POINT('Ctrl Pts',(53.0362352718391,20.6347694196324,17.8453021719777));
#28384=CARTESIAN_POINT('Ctrl Pts',(53.0578570235185,20.5332556518522,17.8525094658393));
#28385=CARTESIAN_POINT('Ctrl Pts',(53.0917985374451,20.4185800854817,17.8604324808444));
#28386=CARTESIAN_POINT('Ctrl Pts',(53.096508475266,20.4033409746875,17.861480581088));
#28387=CARTESIAN_POINT('Ctrl Pts',(53.1033587664401,20.382083873452,17.862934291384));
#28388=CARTESIAN_POINT('Ctrl Pts',(53.105345853607,20.376017647246,17.8633481905447));
#28389=CARTESIAN_POINT('Ctrl Pts',(53.1085996399528,20.366243269563,17.8640134398983));
#28390=CARTESIAN_POINT('Ctrl Pts',(53.1098481853777,20.3625291899305,17.8642658345858));
#28391=CARTESIAN_POINT('Ctrl Pts',(53.1125054868191,20.3547008941483,17.8647969611761));
#28392=CARTESIAN_POINT('Ctrl Pts',(53.1139167669824,20.3505875639856,17.8650755365102));
#28393=CARTESIAN_POINT('Ctrl Pts',(53.1174286831053,20.3404597164924,17.8657602819341));
#28394=CARTESIAN_POINT('Ctrl Pts',(53.1195447246738,20.3344505210533,17.8661655510608));
#28395=CARTESIAN_POINT('Ctrl Pts',(53.1274463675306,20.3123497530297,17.8676526786476));
#28396=CARTESIAN_POINT('Ctrl Pts',(53.1334102185185,20.2963220888684,17.868724533539));
#28397=CARTESIAN_POINT('Ctrl Pts',(53.1754252388377,20.187702567236,17.8759560006637));
#28398=CARTESIAN_POINT('Ctrl Pts',(53.2181494670196,20.0978283067108,17.8817815184293));
#28399=CARTESIAN_POINT('Ctrl Pts',(53.3493547384341,19.8678564877928,17.8971798982329));
#28400=CARTESIAN_POINT('Ctrl Pts',(53.4488439872008,19.7349752051024,17.9066644753506));
#28401=CARTESIAN_POINT('Ctrl Pts',(53.5780304856674,19.6009061297597,17.9181448238755));
#28402=CARTESIAN_POINT('Ctrl Pts',(53.5927089817492,19.5861425471189,17.9194379305167));
#28403=CARTESIAN_POINT('Ctrl Pts',(53.6155882352154,19.5638399828379,17.9214381078498));
#28404=CARTESIAN_POINT('Ctrl Pts',(53.6236258274172,19.5561351661683,17.9221379533497));
#28405=CARTESIAN_POINT('Ctrl Pts',(53.6368073602356,19.543709463285,17.9232813597396));
#28406=CARTESIAN_POINT('Ctrl Pts',(53.6419123990199,19.5389475141249,17.9237231479039));
#28407=CARTESIAN_POINT('Ctrl Pts',(53.6526718425486,19.5290162844542,17.9246521637944));
#28408=CARTESIAN_POINT('Ctrl Pts',(53.658331230077,19.5238525939511,17.9251396180283));
#28409=CARTESIAN_POINT('Ctrl Pts',(53.6719178870085,19.5115986510805,17.9263070973087));
#28410=CARTESIAN_POINT('Ctrl Pts',(53.6798723257742,19.5045390039179,17.9269883891786));
#28411=CARTESIAN_POINT('Ctrl Pts',(53.7072329406929,19.4806445791536,17.9293245609996));
#28412=CARTESIAN_POINT('Ctrl Pts',(53.7269070304031,19.4641218300135,17.9309921727932));
#28413=CARTESIAN_POINT('Ctrl Pts',(53.7749703286756,19.4253152597557,17.9350389534557));
#28414=CARTESIAN_POINT('Ctrl Pts',(53.8036550615148,19.4034135649357,17.9374322816553));
#28415=CARTESIAN_POINT('Ctrl Pts',(53.9984469996218,19.2628814157508,17.9535434791861));
#28416=CARTESIAN_POINT('Ctrl Pts',(54.1812864394909,19.1695972228511,17.9681701016849));
#28417=CARTESIAN_POINT('Ctrl Pts',(54.4072482774499,19.0950535110198,17.9842474096289));
#28418=CARTESIAN_POINT('Ctrl Pts',(54.4396947113639,19.0852587539316,17.9865069636685));
#28419=CARTESIAN_POINT('Ctrl Pts',(54.480492657853,19.0740689264257,17.9892743459269));
#28420=CARTESIAN_POINT('Ctrl Pts',(54.4886223565755,19.0718943777495,17.9898221735318));
#28421=CARTESIAN_POINT('Ctrl Pts',(54.5014555291512,19.0685486125408,17.9906809883666));
#28422=CARTESIAN_POINT('Ctrl Pts',(54.5061498145874,19.0673430084171,17.990993884413));
#28423=CARTESIAN_POINT('Ctrl Pts',(54.5148747243736,19.065136108919,17.9915730569207));
#28424=CARTESIAN_POINT('Ctrl Pts',(54.5189040459838,19.0641303004787,17.9918395807374));
#28425=CARTESIAN_POINT('Ctrl Pts',(54.528172512234,19.0618474099565,17.9924505047803));
#28426=CARTESIAN_POINT('Ctrl Pts',(54.5334137106305,19.0605789841502,17.9927944062752));
#28427=CARTESIAN_POINT('Ctrl Pts',(54.549640293066,19.0567215650556,17.9938544513704));
#28428=CARTESIAN_POINT('Ctrl Pts',(54.5606427811524,19.0542044841279,17.9945666211606));
#28429=CARTESIAN_POINT('Ctrl Pts',(54.6663645224537,19.030960599864,18.0013518295103));
#28430=CARTESIAN_POINT('Ctrl Pts',(54.7624683906608,19.017069679181,18.007077724491));
#28431=CARTESIAN_POINT('Ctrl Pts',(55.0302602034514,18.9981220000316,18.0227330081393));
#28432=CARTESIAN_POINT('Ctrl Pts',(55.202135997427,19.0081245413483,18.032509369554));
#28433=CARTESIAN_POINT('Ctrl Pts',(55.3959612922766,19.0447742476639,18.0446333951751));
#28434=CARTESIAN_POINT('Ctrl Pts',(55.4212135645324,19.0500584301943,18.0462332173317));
#28435=CARTESIAN_POINT('Ctrl Pts',(55.4570432278468,19.0582844437768,18.0485352313109));
#28436=CARTESIAN_POINT('Ctrl Pts',(55.4677104729348,19.060826279257,18.0492246675227));
#28437=CARTESIAN_POINT('Ctrl Pts',(55.4857795428145,19.0652896162356,18.0503996564562));
#28438=CARTESIAN_POINT('Ctrl Pts',(55.4931923447348,19.0671659818529,18.05088374976));
#28439=CARTESIAN_POINT('Ctrl Pts',(55.5081550219907,19.0710450896589,18.0518651320567));
#28440=CARTESIAN_POINT('Ctrl Pts',(55.5157042836134,19.0730496473672,18.0523624722264));
#28441=CARTESIAN_POINT('Ctrl Pts',(55.5342447022756,19.0780894460937,18.0535894009449));
#28442=CARTESIAN_POINT('Ctrl Pts',(55.5452218722551,19.0811746613631,18.0543205975186));
#28443=CARTESIAN_POINT('Ctrl Pts',(55.5856651498453,19.0929166052565,18.0570325855697));
#28444=CARTESIAN_POINT('Ctrl Pts',(55.6149553597626,19.102158996729,18.0590322851738));
#28445=CARTESIAN_POINT('Ctrl Pts',(55.8126117461888,19.1695845628228,18.0727779922741));
#28446=CARTESIAN_POINT('Ctrl Pts',(55.9727162279006,19.2494122324784,18.0852707420328));
#28447=CARTESIAN_POINT('Ctrl Pts',(56.1908819300966,19.3974541575924,18.1035854257354));
#28448=CARTESIAN_POINT('Ctrl Pts',(56.2585466056439,19.4500268158847,18.1094643958355));
#28449=CARTESIAN_POINT('Ctrl Pts',(56.3304248252236,19.5136939228655,18.1157699205793));
#28450=CARTESIAN_POINT('Ctrl Pts',(56.3381649037691,19.5206587033246,18.1164497107711));
#28451=CARTESIAN_POINT('Ctrl Pts',(56.3497541224738,19.5312524568443,18.1174682865368));
#28452=CARTESIAN_POINT('Ctrl Pts',(56.3536438009291,19.5348365284269,18.1178102751639));
#28453=CARTESIAN_POINT('Ctrl Pts',(56.3605839747286,19.5412826504657,18.1184206194939));
#28454=CARTESIAN_POINT('Ctrl Pts',(56.363639755466,19.5441388539873,18.1186894037461));
#28455=CARTESIAN_POINT('Ctrl Pts',(56.3702825341245,19.5503870482726,18.1192737953573));
#28456=CARTESIAN_POINT('Ctrl Pts',(56.373865926059,19.553782743973,18.1195891127425));
#28457=CARTESIAN_POINT('Ctrl Pts',(56.3839884990392,19.563446678012,18.1204801734757));
#28458=CARTESIAN_POINT('Ctrl Pts',(56.3904977429562,19.5697462999101,18.1210535613128));
#28459=CARTESIAN_POINT('Ctrl Pts',(56.4321962417984,19.6106557036476,18.1247310997206));
#28460=CARTESIAN_POINT('Ctrl Pts',(56.4661367907011,19.6465202396826,18.1277449032578));
#28461=CARTESIAN_POINT('Ctrl Pts',(56.5935327507123,19.7915610197578,18.1393152319278));
#28462=CARTESIAN_POINT('Ctrl Pts',(56.676415330692,19.9094456753282,18.1474527152592));
#28463=CARTESIAN_POINT('Ctrl Pts',(56.7910905743534,20.1169679609911,18.1613760968619));
#28464=CARTESIAN_POINT('Ctrl Pts',(56.8304615896814,20.2017781649908,18.1669639254012));
#28465=CARTESIAN_POINT('Ctrl Pts',(56.8691292678486,20.3031416551187,18.1737013152484));
#28466=CARTESIAN_POINT('Ctrl Pts',(56.8743529720651,20.3173165526956,18.1746445756106));
#28467=CARTESIAN_POINT('Ctrl Pts',(56.8826033392081,20.340513267139,18.176190599125));
#28468=CARTESIAN_POINT('Ctrl Pts',(56.885727395688,20.3494999863818,18.1767901326521));
#28469=CARTESIAN_POINT('Ctrl Pts',(56.8911956139495,20.3656004350518,18.1778654377349));
#28470=CARTESIAN_POINT('Ctrl Pts',(56.8935642401564,20.3727057117032,18.1783403916789));
#28471=CARTESIAN_POINT('Ctrl Pts',(56.898494255385,20.3877768873769,18.1793487760228));
#28472=CARTESIAN_POINT('Ctrl Pts',(56.9010456424856,20.3957458820755,18.1798825245754));
#28473=CARTESIAN_POINT('Ctrl Pts',(56.9077242778553,20.4170669405824,18.1813121762884));
#28474=CARTESIAN_POINT('Ctrl Pts',(56.9117614128221,20.43044652926,18.1822110025009));
#28475=CARTESIAN_POINT('Ctrl Pts',(56.9309034563253,20.4963832933026,18.1866496052671));
#28476=CARTESIAN_POINT('Ctrl Pts',(56.9439820569651,20.5494994476613,18.1902542139655));
#28477=CARTESIAN_POINT('Ctrl Pts',(56.995502981766,20.8032450654264,18.2076218195061));
#28478=CARTESIAN_POINT('Ctrl Pts',(57.0051560067028,21.0084170783801,18.2222589669907));
#28479=CARTESIAN_POINT('Ctrl Pts',(56.9799318898453,21.2450240881615,18.2383349641945));
#28480=CARTESIAN_POINT('Ctrl Pts',(56.9755016666597,21.2784970004414,18.2405858010395));
#28481=CARTESIAN_POINT('Ctrl Pts',(56.9689097393642,21.3201447108673,18.2433440609429));
#28482=CARTESIAN_POINT('Ctrl Pts',(56.9675433722257,21.3284376380569,18.2438911783563));
#28483=CARTESIAN_POINT('Ctrl Pts',(56.9653069034859,21.3414964167728,18.2447491264122));
#28484=CARTESIAN_POINT('Ctrl Pts',(56.9644718043535,21.3462680445421,18.2450618596848));
#28485=CARTESIAN_POINT('Ctrl Pts',(56.9628884082495,21.3551252030003,18.245640891276));
#28486=CARTESIAN_POINT('Ctrl Pts',(56.9621447403126,21.3592114022993,18.2459074358058));
#28487=CARTESIAN_POINT('Ctrl Pts',(56.960405526547,21.3686012096881,18.2465186135264));
#28488=CARTESIAN_POINT('Ctrl Pts',(56.9594012198622,21.3739031178642,18.2468627464483));
#28489=CARTESIAN_POINT('Ctrl Pts',(56.9562262718579,21.3903000701685,18.2479242220518));
#28490=CARTESIAN_POINT('Ctrl Pts',(56.9539827702364,21.4013810149472,18.2486375754434));
#28491=CARTESIAN_POINT('Ctrl Pts',(56.9314523282586,21.507993252029,18.2554676872703));
#28492=CARTESIAN_POINT('Ctrl Pts',(56.9042667132261,21.6019458019501,18.2612322963091));
#28493=CARTESIAN_POINT('Ctrl Pts',(56.808634556282,21.8598419475643,18.2772686881828));
#28494=CARTESIAN_POINT('Ctrl Pts',(56.7250710365429,22.0171587037543,18.2873818537632));
#28495=CARTESIAN_POINT('Ctrl Pts',(56.6093125594821,22.1788137130835,18.29965958357));
#28496=CARTESIAN_POINT('Ctrl Pts',(56.5965297125613,22.1960691892853,18.3009956821411));
#28497=CARTESIAN_POINT('Ctrl Pts',(56.577421007896,22.2210116694871,18.3029665504077));
#28498=CARTESIAN_POINT('Ctrl Pts',(56.5713119480881,22.2288634135698,18.3035928390739));
#28499=CARTESIAN_POINT('Ctrl Pts',(56.5604496049368,22.2426109372477,18.3046999735444));
#28500=CARTESIAN_POINT('Ctrl Pts',(56.5557209666886,22.2485260037902,18.3051798329161));
#28501=CARTESIAN_POINT('Ctrl Pts',(56.5458787301679,22.260694956201,18.3061743820476));
#28502=CARTESIAN_POINT('Ctrl Pts',(56.5407606011256,22.2669449821651,18.3066892489413));
#28503=CARTESIAN_POINT('Ctrl Pts',(56.5275247612064,22.2829091653812,18.3080149371423));
#28504=CARTESIAN_POINT('Ctrl Pts',(56.5193523815999,22.2925773288248,18.3088279740569));
#28505=CARTESIAN_POINT('Ctrl Pts',(56.4844998806572,22.3330216229214,18.3122729252365));
#28506=CARTESIAN_POINT('Ctrl Pts',(56.456974049518,22.3630527353309,18.314939626909));
#28507=CARTESIAN_POINT('Ctrl Pts',(56.3812563343511,22.4407463800846,18.3221411966938));
#28508=CARTESIAN_POINT('Ctrl Pts',(56.3315252068369,22.4868282534473,18.3267378413131));
#28509=CARTESIAN_POINT('Ctrl Pts',(56.2001581392498,22.5966708849461,18.3385245556724));
#28510=CARTESIAN_POINT('Ctrl Pts',(56.1157217532898,22.656774264336,18.3457926163767));
#28511=CARTESIAN_POINT('Ctrl Pts',(55.9587613575349,22.7510402709429,18.3584895285864));
#28512=CARTESIAN_POINT('Ctrl Pts',(55.8881122679599,22.7879107729435,18.3639416023737));
#28513=CARTESIAN_POINT('Ctrl Pts',(55.8059883029279,22.8246966031938,18.369850279464));
#28514=CARTESIAN_POINT('Ctrl Pts',(55.796502784846,22.8288570646599,18.3705264605794));
#28515=CARTESIAN_POINT('Ctrl Pts',(55.7821356742016,22.8350256677382,18.3715407043809));
#28516=CARTESIAN_POINT('Ctrl Pts',(55.7772779868933,22.8370885516932,18.3718819308855));
#28517=CARTESIAN_POINT('Ctrl Pts',(55.7685563061934,22.8407515465929,18.3724914635764));
#28518=CARTESIAN_POINT('Ctrl Pts',(55.7646954300366,22.842358801205,18.3727601933346));
#28519=CARTESIAN_POINT('Ctrl Pts',(55.7562575598405,22.8458403305667,18.373345102971));
#28520=CARTESIAN_POINT('Ctrl Pts',(55.7516786483577,22.8477097265659,18.3736609888215));
#28521=CARTESIAN_POINT('Ctrl Pts',(55.738654751645,22.8529704632052,18.3745552820806));
#28522=CARTESIAN_POINT('Ctrl Pts',(55.7301933149097,22.8563211225432,18.3751313068388));
#28523=CARTESIAN_POINT('Ctrl Pts',(55.6748456596824,22.8778013369524,18.3788686023687));
#28524=CARTESIAN_POINT('Ctrl Pts',(55.6273070024344,22.8942126062599,18.3819361079782));
#28525=CARTESIAN_POINT('Ctrl Pts',(55.4441175609856,22.9497981757071,18.3934013495461));
#28526=CARTESIAN_POINT('Ctrl Pts',(55.3050908075108,22.9763255866786,18.4014016019433));
#28527=CARTESIAN_POINT('Ctrl Pts',(55.1644483276976,22.9879598361178,18.4096837786395));
#28528=CARTESIAN_POINT('Origin',(55.,21.,6.22095488139522));
#28529=CARTESIAN_POINT('',(55.1644484414293,22.9879598267097,19.3668580791575));
#28530=CARTESIAN_POINT('',(55.1644482551197,22.9879598421216,19.2088565303878));
#28531=CARTESIAN_POINT('',(55.1644483516311,22.987959834138,6.22095488139522));
#28532=CARTESIAN_POINT('Ctrl Pts',(55.1644484414294,22.9879598267096,19.3668580791575));
#28533=CARTESIAN_POINT('Ctrl Pts',(55.2859411225326,22.9779096829471,19.3594542727769));
#28534=CARTESIAN_POINT('Ctrl Pts',(55.4063260452155,22.9567375761454,19.3524631524528));
#28535=CARTESIAN_POINT('Ctrl Pts',(55.6455879656927,22.8915870241497,19.3380541657924));
#28536=CARTESIAN_POINT('Ctrl Pts',(55.763668940839,22.8470758363702,19.3306581368666));
#28537=CARTESIAN_POINT('Ctrl Pts',(55.8945022252663,22.7830545490934,19.3216439778995));
#28538=CARTESIAN_POINT('Ctrl Pts',(55.9121147099626,22.7741094860059,19.320412915732));
#28539=CARTESIAN_POINT('Ctrl Pts',(55.9380642882356,22.7604416118804,19.3185714466332));
#28540=CARTESIAN_POINT('Ctrl Pts',(55.9465052330122,22.7559177419324,19.3179680374095));
#28541=CARTESIAN_POINT('Ctrl Pts',(55.9614967478699,22.7477436299196,19.3168883043627));
#28542=CARTESIAN_POINT('Ctrl Pts',(55.9680599695535,22.7441168782306,19.3164128230613));
#28543=CARTESIAN_POINT('Ctrl Pts',(55.9818757293327,22.7363804600097,19.3154059585645));
#28544=CARTESIAN_POINT('Ctrl Pts',(55.9891232510803,22.7322621742828,19.3148742727427));
#28545=CARTESIAN_POINT('Ctrl Pts',(56.0083213540756,22.7211934036829,19.313456421284));
#28546=CARTESIAN_POINT('Ctrl Pts',(56.0202256836369,22.7141640016197,19.3125674180118));
#28547=CARTESIAN_POINT('Ctrl Pts',(56.0721720160992,22.6827573541728,19.3086440047641));
#28548=CARTESIAN_POINT('Ctrl Pts',(56.1114177796997,22.6570983842651,19.305563096701));
#28549=CARTESIAN_POINT('Ctrl Pts',(56.1733121277617,22.6134434068244,19.3005079660549));
#28550=CARTESIAN_POINT('Ctrl Pts',(56.1965384618161,22.5962946341269,19.2985639143542));
#28551=CARTESIAN_POINT('Ctrl Pts',(56.3592069202022,22.4706458575167,19.2846133016888));
#28552=CARTESIAN_POINT('Ctrl Pts',(56.4840430907995,22.3445625351326,19.2720196080004));
#28553=CARTESIAN_POINT('Ctrl Pts',(56.6068527546109,22.1822748165837,19.2582023413602));
#28554=CARTESIAN_POINT('Ctrl Pts',(56.6226328388219,22.1605224399621,19.256395412602));
#28555=CARTESIAN_POINT('Ctrl Pts',(56.6480140422458,22.1240049075826,19.2534438913056));
#28556=CARTESIAN_POINT('Ctrl Pts',(56.6578674368494,22.1094200867443,19.2522860172605));
#28557=CARTESIAN_POINT('Ctrl Pts',(56.6710632659378,22.0893193505371,19.250720648619));
#28558=CARTESIAN_POINT('Ctrl Pts',(56.6745735682473,22.0839153350375,19.2503027622713));
#28559=CARTESIAN_POINT('Ctrl Pts',(56.6804174688579,22.0748226563168,19.2496047080065));
#28560=CARTESIAN_POINT('Ctrl Pts',(56.6827652343025,22.0711432114743,19.2493236162086));
#28561=CARTESIAN_POINT('Ctrl Pts',(56.6871916767807,22.0641555678516,19.24879245394));
#28562=CARTESIAN_POINT('Ctrl Pts',(56.6892727365996,22.0608489283642,19.2485422222219));
#28563=CARTESIAN_POINT('Ctrl Pts',(56.6946931116549,22.0521799866763,19.2478890643441));
#28564=CARTESIAN_POINT('Ctrl Pts',(56.6980167260998,22.0468078465211,19.2474871633156));
#28565=CARTESIAN_POINT('Ctrl Pts',(56.7094314437805,22.0281602021427,19.2461016374019));
#28566=CARTESIAN_POINT('Ctrl Pts',(56.717393071944,22.0148055645266,19.2451260345438));
#28567=CARTESIAN_POINT('Ctrl Pts',(56.7885443434707,21.8922220883278,19.2363087268229));
#28568=CARTESIAN_POINT('Ctrl Pts',(56.8414010223003,21.7773045663453,19.2290205339028));
#28569=CARTESIAN_POINT('Ctrl Pts',(56.9322448850836,21.5173886680701,19.2130470023684));
#28570=CARTESIAN_POINT('Ctrl Pts',(56.9654983874495,21.3715773312364,19.2043735255265));
#28571=CARTESIAN_POINT('Ctrl Pts',(56.9841432547822,21.2061672739225,19.1940435979984));
#28572=CARTESIAN_POINT('Ctrl Pts',(56.9858635750629,21.1888788810052,19.1929587154274));
#28573=CARTESIAN_POINT('Ctrl Pts',(56.9881404233005,21.1625054168029,19.1912948756796));
#28574=CARTESIAN_POINT('Ctrl Pts',(56.9888609877338,21.1534350686597,19.1907210593371));
#28575=CARTESIAN_POINT('Ctrl Pts',(56.9900591919319,21.1369218599516,19.1896733626656));
#28576=CARTESIAN_POINT('Ctrl Pts',(56.9905571965844,21.1294806077392,19.1892001295129));
#28577=CARTESIAN_POINT('Ctrl Pts',(56.9915431674171,21.1133946330175,19.1881746404512));
#28578=CARTESIAN_POINT('Ctrl Pts',(56.9920165990437,21.1047492038947,19.1876219390821));
#28579=CARTESIAN_POINT('Ctrl Pts',(56.9931513650979,21.0812224525582,19.1861135261575));
#28580=CARTESIAN_POINT('Ctrl Pts',(56.9937023063196,21.0663366021663,19.1851543875142));
#28581=CARTESIAN_POINT('Ctrl Pts',(56.9956548405061,20.9906553271943,19.1802529698554));
#28582=CARTESIAN_POINT('Ctrl Pts',(56.9944424018773,20.9298304569224,19.1762301306353));
#28583=CARTESIAN_POINT('Ctrl Pts',(56.9789477710719,20.6941106977564,19.1603083652287));
#28584=CARTESIAN_POINT('Ctrl Pts',(56.9443974063182,20.5213485816138,19.147841826439));
#28585=CARTESIAN_POINT('Ctrl Pts',(56.8705912524161,20.3052159700822,19.1321993940028));
#28586=CARTESIAN_POINT('Ctrl Pts',(56.8514700241245,20.2557578829777,19.128624413463));
#28587=CARTESIAN_POINT('Ctrl Pts',(56.8267337208243,20.1986533035171,19.1245477093294));
#28588=CARTESIAN_POINT('Ctrl Pts',(56.8230092300837,20.1902160969155,19.1239467257505));
#28589=CARTESIAN_POINT('Ctrl Pts',(56.8171865895121,20.1772696739806,19.1230269720805));
#28590=CARTESIAN_POINT('Ctrl Pts',(56.815129928672,20.1727420995832,19.1227057782285));
#28591=CARTESIAN_POINT('Ctrl Pts',(56.8113126842604,20.1644215130259,19.122116412038));
#28592=CARTESIAN_POINT('Ctrl Pts',(56.8095571130897,20.1606263626173,19.1218479498882));
#28593=CARTESIAN_POINT('Ctrl Pts',(56.805571516607,20.1520810199969,19.1212442549411));
#28594=CARTESIAN_POINT('Ctrl Pts',(56.803334678042,20.1473340990033,19.1209094461875));
#28595=CARTESIAN_POINT('Ctrl Pts',(56.7966893743056,20.1333748480332,19.1199263165851));
#28596=CARTESIAN_POINT('Ctrl Pts',(56.7922287849532,20.1241873176264,19.1192811083811));
#28597=CARTESIAN_POINT('Ctrl Pts',(56.7566305321969,20.0522761580961,19.1142425209722));
#28598=CARTESIAN_POINT('Ctrl Pts',(56.7222764159288,19.9911900500591,19.1100307326643));
#28599=CARTESIAN_POINT('Ctrl Pts',(56.5942065319402,19.7891531139887,19.0959099571347));
#28600=CARTESIAN_POINT('Ctrl Pts',(56.4858333894587,19.6583792528013,19.086372882142));
#28601=CARTESIAN_POINT('Ctrl Pts',(56.3251399575892,19.508151174059,19.0731264165011));
#28602=CARTESIAN_POINT('Ctrl Pts',(56.286717084246,19.4748877726493,19.0700192992901));
#28603=CARTESIAN_POINT('Ctrl Pts',(56.2364131051047,19.434593793396,19.0660001799576));
#28604=CARTESIAN_POINT('Ctrl Pts',(56.2256702745376,19.4261682677051,19.0651446028397));
#28605=CARTESIAN_POINT('Ctrl Pts',(56.2082604099772,19.412800201317,19.063761976281));
#28606=CARTESIAN_POINT('Ctrl Pts',(56.2016474232291,19.4077877383555,19.063237693029));
#28607=CARTESIAN_POINT('Ctrl Pts',(56.1889927101028,19.3983195539257,19.0622360118921));
#28608=CARTESIAN_POINT('Ctrl Pts',(56.1829567160759,19.393856382082,19.0617589164768));
#28609=CARTESIAN_POINT('Ctrl Pts',(56.1691072327962,19.3837361315295,19.0606657015447));
#28610=CARTESIAN_POINT('Ctrl Pts',(56.1612776604253,19.3781014815065,19.0600487299997));
#28611=CARTESIAN_POINT('Ctrl Pts',(56.1407279121673,19.3635376811794,19.0584319890772));
#28612=CARTESIAN_POINT('Ctrl Pts',(56.127943908675,19.3547001468704,19.0574287642209));
#28613=CARTESIAN_POINT('Ctrl Pts',(56.0185596456632,19.2809572269973,19.0488645519399));
#28614=CARTESIAN_POINT('Ctrl Pts',(55.9165700116096,19.2244823821459,19.0409883898205));
#28615=CARTESIAN_POINT('Ctrl Pts',(55.7339085957034,19.1432860802634,19.0271511329896));
#28616=CARTESIAN_POINT('Ctrl Pts',(55.6555040412386,19.1141785838989,19.0212947313369));
#28617=CARTESIAN_POINT('Ctrl Pts',(55.5022637327687,19.0680034849264,19.0101841413865));
#28618=CARTESIAN_POINT('Ctrl Pts',(55.4278024087881,19.0501623323476,19.0049307881534));
#28619=CARTESIAN_POINT('Ctrl Pts',(55.3376492762529,19.0339766083183,18.9988726566501));
#28620=CARTESIAN_POINT('Ctrl Pts',(55.3227749481266,19.0314799020175,18.9978829148723));
#28621=CARTESIAN_POINT('Ctrl Pts',(55.3018825969923,19.0282162331309,18.9965077607259));
#28622=CARTESIAN_POINT('Ctrl Pts',(55.2958876562402,19.0273077222059,18.9961148975625));
#28623=CARTESIAN_POINT('Ctrl Pts',(55.2856445244367,19.0258031585704,18.9954466984697));
#28624=CARTESIAN_POINT('Ctrl Pts',(55.2813984089412,19.0251934525496,18.9951706046192));
#28625=CARTESIAN_POINT('Ctrl Pts',(55.2732032762931,19.0240436700801,18.994639502561));
#28626=CARTESIAN_POINT('Ctrl Pts',(55.2692545880594,19.0235017289619,18.9943843859319));
#28627=CARTESIAN_POINT('Ctrl Pts',(55.259744688178,19.0222255626833,18.9937718050246));
#28628=CARTESIAN_POINT('Ctrl Pts',(55.2541819139722,19.0215029481025,18.9934149869697));
#28629=CARTESIAN_POINT('Ctrl Pts',(55.2337303375651,19.0189339300017,18.9921084385052));
#28630=CARTESIAN_POINT('Ctrl Pts',(55.218823443012,19.0172319911626,18.991166414364));
#28631=CARTESIAN_POINT('Ctrl Pts',(55.0669568627943,19.0016268389757,18.9816611373217));
#28632=CARTESIAN_POINT('Ctrl Pts',(54.9289057299566,19.0017669528759,18.9737617623569));
#28633=CARTESIAN_POINT('Ctrl Pts',(54.6538696557266,19.0306096821275,18.9577096318486));
#28634=CARTESIAN_POINT('Ctrl Pts',(54.5176951447003,19.0594641864507,18.9495869235747));
#28635=CARTESIAN_POINT('Ctrl Pts',(54.3693612343454,19.1074845707804,18.9399081266529));
#28636=CARTESIAN_POINT('Ctrl Pts',(54.3531632342526,19.112959440672,18.9388401922774));
#28637=CARTESIAN_POINT('Ctrl Pts',(54.3285103167869,19.1216467532982,18.9371970450356));
#28638=CARTESIAN_POINT('Ctrl Pts',(54.3200032794803,19.124709683864,18.9366267752276));
#28639=CARTESIAN_POINT('Ctrl Pts',(54.3051994858916,19.1301537166707,18.935628567122));
#28640=CARTESIAN_POINT('Ctrl Pts',(54.2988933664387,19.1325090725132,18.9352014919745));
#28641=CARTESIAN_POINT('Ctrl Pts',(54.2847045013276,19.1378906565276,18.9342363096098));
#28642=CARTESIAN_POINT('Ctrl Pts',(54.2768288441288,19.1409350917279,18.9336975996116));
#28643=CARTESIAN_POINT('Ctrl Pts',(54.2556543266914,19.1492752815392,18.9322410558365));
#28644=CARTESIAN_POINT('Ctrl Pts',(54.2423929518496,19.1546642560872,18.9313201049836));
#28645=CARTESIAN_POINT('Ctrl Pts',(54.1814180226552,19.1802104598729,18.927044303893));
#28646=CARTESIAN_POINT('Ctrl Pts',(54.1344467672732,19.2020769736481,18.9236320436585));
#28647=CARTESIAN_POINT('Ctrl Pts',(53.9238397523617,19.3102874238033,18.9077713883804));
#28648=CARTESIAN_POINT('Ctrl Pts',(53.7718659321933,19.4173070585869,18.8946186371054));
#28649=CARTESIAN_POINT('Ctrl Pts',(53.5975470639746,19.5804750873222,18.8782569343677));
#28650=CARTESIAN_POINT('Ctrl Pts',(53.5597485021142,19.6188403492554,18.8746241484992));
#28651=CARTESIAN_POINT('Ctrl Pts',(53.5173204782722,19.6655432969737,18.8704904622032));
#28652=CARTESIAN_POINT('Ctrl Pts',(53.5111434503766,19.6724385366253,18.8698871852652));
#28653=CARTESIAN_POINT('Ctrl Pts',(53.5017174151732,19.6831090932932,18.8689646735319));
#28654=CARTESIAN_POINT('Ctrl Pts',(53.4984342698925,19.6868538833614,18.8686429926959));
#28655=CARTESIAN_POINT('Ctrl Pts',(53.4924205767139,19.6937652099313,18.8680531653004));
#28656=CARTESIAN_POINT('Ctrl Pts',(53.4896859709943,19.6969280224366,18.8677847256112));
#28657=CARTESIAN_POINT('Ctrl Pts',(53.483547535146,19.704072947265,18.8671816196277));
#28658=CARTESIAN_POINT('Ctrl Pts',(53.4801494412468,19.7080598757135,18.8668473735814));
#28659=CARTESIAN_POINT('Ctrl Pts',(53.4702000527617,19.7198269135833,18.8658674391641));
#28660=CARTESIAN_POINT('Ctrl Pts',(53.4636923930911,19.7276439346457,18.8652248333013));
#28661=CARTESIAN_POINT('Ctrl Pts',(53.4137008338015,19.7886367311673,18.8602723444036));
#28662=CARTESIAN_POINT('Ctrl Pts',(53.3729251067131,19.8439829344545,18.8561371453906));
#28663=CARTESIAN_POINT('Ctrl Pts',(53.2412452134526,20.0435295706021,18.8420128218157));
#28664=CARTESIAN_POINT('Ctrl Pts',(53.1660131308663,20.1971618808354,18.83241418035));
#28665=CARTESIAN_POINT('Ctrl Pts',(53.0948243031391,20.4067614341369,18.8190863012976));
#28666=CARTESIAN_POINT('Ctrl Pts',(53.0802871436911,20.4556395411664,18.8159688878775));
#28667=CARTESIAN_POINT('Ctrl Pts',(53.0642471398112,20.5182581239285,18.8119381294669));
#28668=CARTESIAN_POINT('Ctrl Pts',(53.0609918215238,20.5315326692724,18.8110816194378));
#28669=CARTESIAN_POINT('Ctrl Pts',(53.055979048103,20.5529216924376,18.8096978461553));
#28670=CARTESIAN_POINT('Ctrl Pts',(53.054135352594,20.5610156664466,18.8091733574607));
#28671=CARTESIAN_POINT('Ctrl Pts',(53.0507208803157,20.5764497454351,18.8081715216709));
#28672=CARTESIAN_POINT('Ctrl Pts',(53.0491409042501,20.5837876856904,18.8076944786128));
#28673=CARTESIAN_POINT('Ctrl Pts',(53.0456264614121,20.6005696988359,18.8066017196924));
#28674=CARTESIAN_POINT('Ctrl Pts',(53.0437189770464,20.6100191701411,18.8059851543555));
#28675=CARTESIAN_POINT('Ctrl Pts',(53.0389194403859,20.6347172589119,18.8043701752034));
#28676=CARTESIAN_POINT('Ctrl Pts',(53.0361367730995,20.6499862207568,18.803368318183));
#28677=CARTESIAN_POINT('Ctrl Pts',(53.0146074315655,20.7764724624523,18.7950390063809));
#28678=CARTESIAN_POINT('Ctrl Pts',(53.0051492669158,20.8890447531017,18.7874166042857));
#28679=CARTESIAN_POINT('Ctrl Pts',(53.0053603005261,21.1233753678906,18.7712141163126));
#28680=CARTESIAN_POINT('Ctrl Pts',(53.0165845065903,21.244687115159,18.7626384351935));
#28681=CARTESIAN_POINT('Ctrl Pts',(53.0479813616346,21.4137492010836,18.750874704986));
#28682=CARTESIAN_POINT('Ctrl Pts',(53.0590530088554,21.4629156453414,18.7474797070929));
#28683=CARTESIAN_POINT('Ctrl Pts',(53.07419398738,21.5199745951858,18.7436097376684));
#28684=CARTESIAN_POINT('Ctrl Pts',(53.07646683976,21.5283205142837,18.7430454720404));
#28685=CARTESIAN_POINT('Ctrl Pts',(53.0802379140464,21.5418209141714,18.7421359098346));
#28686=CARTESIAN_POINT('Ctrl Pts',(53.0817027498944,21.5469844893309,18.7417887852761));
#28687=CARTESIAN_POINT('Ctrl Pts',(53.0843481357721,21.556168186226,18.7411728398162));
#28688=CARTESIAN_POINT('Ctrl Pts',(53.0855205256801,21.5601905567017,18.7409035573398));
#28689=CARTESIAN_POINT('Ctrl Pts',(53.0880863509747,21.5688915457478,18.7403221450275));
#28690=CARTESIAN_POINT('Ctrl Pts',(53.0894842876925,21.5735687460209,18.7400102797632));
#28691=CARTESIAN_POINT('Ctrl Pts',(53.0934499994578,21.5866618075168,18.7391390256548));
#28692=CARTESIAN_POINT('Ctrl Pts',(53.0960563457867,21.5950660041951,18.7385818283651));
#28693=CARTESIAN_POINT('Ctrl Pts',(53.1120900707537,21.6455830041664,18.7352433522298));
#28694=CARTESIAN_POINT('Ctrl Pts',(53.1268596743861,21.6872607255614,18.7325342811241));
#28695=CARTESIAN_POINT('Ctrl Pts',(53.1816596222082,21.8269655643011,18.7234994424352));
#28696=CARTESIAN_POINT('Ctrl Pts',(53.2281023500646,21.9222883818736,18.7174066970902));
#28697=CARTESIAN_POINT('Ctrl Pts',(53.3511608409721,22.1309036358589,18.7033441619654));
#28698=CARTESIAN_POINT('Ctrl Pts',(53.432271159131,22.2409000095519,18.6953577156356));
#28699=CARTESIAN_POINT('Ctrl Pts',(53.5342969807604,22.3531365666591,18.685941551004));
#28700=CARTESIAN_POINT('Ctrl Pts',(53.5447688712159,22.3643922638929,18.6849818853084));
#28701=CARTESIAN_POINT('Ctrl Pts',(53.5619867986147,22.3824752005507,18.6834142329667));
#28702=CARTESIAN_POINT('Ctrl Pts',(53.568653971561,22.3893769068135,18.682809629137));
#28703=CARTESIAN_POINT('Ctrl Pts',(53.5806208511983,22.4015871923155,18.6817285638286));
#28704=CARTESIAN_POINT('Ctrl Pts',(53.5859012261112,22.4069145250838,18.6812529527673));
#28705=CARTESIAN_POINT('Ctrl Pts',(53.5971054056754,22.4180915445048,18.680246651841));
#28706=CARTESIAN_POINT('Ctrl Pts',(53.6030360230924,22.42393416812,18.6797156643237));
#28707=CARTESIAN_POINT('Ctrl Pts',(53.6188770319087,22.4393459248997,18.6783016540643));
#28708=CARTESIAN_POINT('Ctrl Pts',(53.6288501356403,22.4488496741154,18.677415820841));
#28709=CARTESIAN_POINT('Ctrl Pts',(53.6771102268659,22.4938939737484,18.6731493125576));
#28710=CARTESIAN_POINT('Ctrl Pts',(53.7166819983548,22.5280218010313,18.6697097423274));
#28711=CARTESIAN_POINT('Ctrl Pts',(53.835507587072,22.622626286645,18.6595392475672));
#28712=CARTESIAN_POINT('Ctrl Pts',(53.9180039774493,22.6787611985284,18.6526617795959));
#28713=CARTESIAN_POINT('Ctrl Pts',(54.1169543912512,22.7933622779506,18.6366662995435));
#28714=CARTESIAN_POINT('Ctrl Pts',(54.2356484977355,22.8470761231287,18.6275336185841));
#28715=CARTESIAN_POINT('Ctrl Pts',(54.3732785186139,22.8938013930089,18.6179124591341));
#28716=CARTESIAN_POINT('Ctrl Pts',(54.38788147624,22.8985716944163,18.6169035935973));
#28717=CARTESIAN_POINT('Ctrl Pts',(54.4085360592497,22.9050557691459,18.6154948596926));
#28718=CARTESIAN_POINT('Ctrl Pts',(54.4145424755502,22.9069102145659,18.615087352264));
#28719=CARTESIAN_POINT('Ctrl Pts',(54.424662054852,22.9099822538324,18.6144045269025));
#28720=CARTESIAN_POINT('Ctrl Pts',(54.4287705250835,22.9112150190991,18.6141283391773));
#28721=CARTESIAN_POINT('Ctrl Pts',(54.4371590525104,22.9137025690496,18.6135665807633));
#28722=CARTESIAN_POINT('Ctrl Pts',(54.4414393901271,22.9149562660828,18.6132810736569));
#28723=CARTESIAN_POINT('Ctrl Pts',(54.4523418269694,22.9181098896567,18.6125566627342));
#28724=CARTESIAN_POINT('Ctrl Pts',(54.4589696951312,22.9199899051409,18.612118900844));
#28725=CARTESIAN_POINT('Ctrl Pts',(54.4858090013379,22.9274529419544,18.6103563046855));
#28726=CARTESIAN_POINT('Ctrl Pts',(54.5060989900034,22.9327516917152,18.6090469285729));
#28727=CARTESIAN_POINT('Ctrl Pts',(54.5596293300779,22.9458331019816,18.605643821469));
#28728=CARTESIAN_POINT('Ctrl Pts',(54.5929934487368,22.95308441272,18.603574315374));
#28729=CARTESIAN_POINT('Ctrl Pts',(54.7793468777514,22.988602877633,18.5922184537084));
#28730=CARTESIAN_POINT('Ctrl Pts',(54.9350536377415,22.9997543790344,18.5834452992847));
#28731=CARTESIAN_POINT('Ctrl Pts',(55.1151708305678,22.9915757571036,18.5727943099788));
#28732=CARTESIAN_POINT('Ctrl Pts',(55.1398302308105,22.9899962989591,18.5713262821773));
#28733=CARTESIAN_POINT('Ctrl Pts',(55.1644483870895,22.9879598312048,18.5698477239299));
#28734=CARTESIAN_POINT('',(53.0052494851995,20.9997435532217,18.6227928887582));
#28735=CARTESIAN_POINT('Ctrl Pts',(55.1644483276976,22.9879598361178,18.4096837786395));
#28736=CARTESIAN_POINT('Ctrl Pts',(55.1550885057686,22.9887341007864,18.4102349613203));
#28737=CARTESIAN_POINT('Ctrl Pts',(55.1457215198892,22.989442403148,18.4107872590292));
#28738=CARTESIAN_POINT('Ctrl Pts',(55.1025841399482,22.9923979045278,18.4133348257717));
#28739=CARTESIAN_POINT('Ctrl Pts',(55.0687679341149,22.9938514852108,18.4153435664557));
#28740=CARTESIAN_POINT('Ctrl Pts',(54.9795085102815,22.9954148400144,18.4206979885749));
#28741=CARTESIAN_POINT('Ctrl Pts',(54.9240728494658,22.9940748504138,18.4240771874888));
#28742=CARTESIAN_POINT('Ctrl Pts',(54.8543195138251,22.9894759199281,18.4284303062247));
#28743=CARTESIAN_POINT('Ctrl Pts',(54.8398817502561,22.9883660047059,18.4293367516838));
#28744=CARTESIAN_POINT('Ctrl Pts',(54.8169289460162,22.9863498814668,18.4307869649421));
#28745=CARTESIAN_POINT('Ctrl Pts',(54.8084052687768,22.9855458487978,18.4313275264826));
#28746=CARTESIAN_POINT('Ctrl Pts',(54.7924618242377,22.9839382963969,18.4323425262472));
#28747=CARTESIAN_POINT('Ctrl Pts',(54.7850408547072,22.9831479575876,18.4328165421133));
#28748=CARTESIAN_POINT('Ctrl Pts',(54.7684638842948,22.9812883596184,18.4338790073341));
#28749=CARTESIAN_POINT('Ctrl Pts',(54.7593105551118,22.9801972435193,18.4344681349272));
#28750=CARTESIAN_POINT('Ctrl Pts',(54.7323455245529,22.9767931725836,18.4362111026556));
#28751=CARTESIAN_POINT('Ctrl Pts',(54.7145575059956,22.9743030955237,18.4373704850324));
#28752=CARTESIAN_POINT('Ctrl Pts',(54.6742428158626,22.9681033907971,18.4400206626057));
#28753=CARTESIAN_POINT('Ctrl Pts',(54.6517416569175,22.9642466126832,18.4415159195772));
#28754=CARTESIAN_POINT('Ctrl Pts',(54.5775504343614,22.9502151320402,18.4465005513552));
#28755=CARTESIAN_POINT('Ctrl Pts',(54.5262006422796,22.9383797554411,18.4500391954169));
#28756=CARTESIAN_POINT('Ctrl Pts',(54.347440951541,22.889650692891,18.4626600303391));
#28757=CARTESIAN_POINT('Ctrl Pts',(54.223301076904,22.8421039058492,18.4720010607957));
#28758=CARTESIAN_POINT('Ctrl Pts',(54.0386104597179,22.7493557372527,18.4863063329261));
#28759=CARTESIAN_POINT('Ctrl Pts',(53.97430490171,22.7124448646036,18.4913652834678));
#28760=CARTESIAN_POINT('Ctrl Pts',(53.9035830886952,22.6664342458163,18.4969044543053));
#28761=CARTESIAN_POINT('Ctrl Pts',(53.8950135514606,22.6607643115071,18.4975751844623));
#28762=CARTESIAN_POINT('Ctrl Pts',(53.8821239031164,22.6520920861037,18.4985828813699));
#28763=CARTESIAN_POINT('Ctrl Pts',(53.8777713830982,22.6491386120931,18.4989229530907));
#28764=CARTESIAN_POINT('Ctrl Pts',(53.8700764270214,22.6438725013522,18.4995237428057));
#28765=CARTESIAN_POINT('Ctrl Pts',(53.8667293412371,22.6415668418983,18.4997849183142));
#28766=CARTESIAN_POINT('Ctrl Pts',(53.8633680990657,22.6392362504958,18.5000470433025));
#28767=CARTESIAN_POINT('Ctrl Pts',(53.8633469696672,22.6392215993564,18.5000486910634));
#28768=CARTESIAN_POINT('Ctrl Pts',(53.8633048768407,22.6391924109563,18.5000519736303));
#28769=CARTESIAN_POINT('Ctrl Pts',(53.8632839137361,22.6391778739294,18.5000536084111));
#28770=CARTESIAN_POINT('Ctrl Pts',(53.863242150943,22.6391489120114,18.5000568652175));
#28771=CARTESIAN_POINT('Ctrl Pts',(53.8632213509964,22.6391344869504,18.5000584872632));
#28772=CARTESIAN_POINT('Ctrl Pts',(53.8631799101496,22.6391057459613,18.5000617189402));
#28773=CARTESIAN_POINT('Ctrl Pts',(53.8631592696543,22.6390914303229,18.5000633285401));
#28774=CARTESIAN_POINT('Ctrl Pts',(53.863118144229,22.6390629057911,18.5000665355972));
#28775=CARTESIAN_POINT('Ctrl Pts',(53.8630976596403,22.639048697143,18.5000681330279));
#28776=CARTESIAN_POINT('Ctrl Pts',(53.8630568434283,22.6390203848144,18.5000713159497));
#28777=CARTESIAN_POINT('Ctrl Pts',(53.8630365115884,22.639006280992,18.5000729014578));
#28778=CARTESIAN_POINT('Ctrl Pts',(53.8629959978564,22.6389781762467,18.5000760607699));
#28779=CARTESIAN_POINT('Ctrl Pts',(53.862975815614,22.6389641750888,18.5000776346013));
#28780=CARTESIAN_POINT('Ctrl Pts',(53.8629355981506,22.638936273667,18.5000807707886));
#28781=CARTESIAN_POINT('Ctrl Pts',(53.862915562651,22.6389223732176,18.5000823331663));
#28782=CARTESIAN_POINT('Ctrl Pts',(53.8628756340883,22.6388946700555,18.5000854468038));
#28783=CARTESIAN_POINT('Ctrl Pts',(53.8628557416861,22.6388808678088,18.5000869980122));
#28784=CARTESIAN_POINT('Ctrl Pts',(53.8628160973718,22.6388533597248,18.5000900894632));
#28785=CARTESIAN_POINT('Ctrl Pts',(53.8627963453358,22.6388396538088,18.5000916297155));
#28786=CARTESIAN_POINT('Ctrl Pts',(53.862756978903,22.6388123364303,18.5000946994769));
#28787=CARTESIAN_POINT('Ctrl Pts',(53.8627373644,22.6387987249013,18.5000962289944));
#28788=CARTESIAN_POINT('Ctrl Pts',(53.8586701621368,22.6359761724477,18.5004133839195));
#28789=CARTESIAN_POINT('Ctrl Pts',(53.854632942132,22.6331522095715,18.5007279856178));
#28790=CARTESIAN_POINT('Ctrl Pts',(53.8462369048929,22.6272328850598,18.5013818936148));
#28791=CARTESIAN_POINT('Ctrl Pts',(53.8418799778788,22.6241348951849,18.501721022344));
#28792=CARTESIAN_POINT('Ctrl Pts',(53.8306498442973,22.6160815481713,18.5025947651682));
#28793=CARTESIAN_POINT('Ctrl Pts',(53.8237955823877,22.611099789195,18.5031276862468));
#28794=CARTESIAN_POINT('Ctrl Pts',(53.8036536372127,22.5962633269787,18.5046933262786));
#28795=CARTESIAN_POINT('Ctrl Pts',(53.7904562363721,22.5862865916265,18.5057186431587));
#28796=CARTESIAN_POINT('Ctrl Pts',(53.7433236293698,22.5497258539722,18.5093846405643));
#28797=CARTESIAN_POINT('Ctrl Pts',(53.7101263146181,22.5222063212168,18.511974882489));
#28798=CARTESIAN_POINT('Ctrl Pts',(53.575545856806,22.4030763258956,18.5226325200484));
#28799=CARTESIAN_POINT('Ctrl Pts',(53.4828182024347,22.3022500541807,18.5303886168244));
#28800=CARTESIAN_POINT('Ctrl Pts',(53.3499079523017,22.1240817051133,18.5434873898295));
#28801=CARTESIAN_POINT('Ctrl Pts',(53.3031753228346,22.0522104306539,18.5486308867433));
#28802=CARTESIAN_POINT('Ctrl Pts',(53.2539276187076,21.9646136738307,18.5548737786316));
#28803=CARTESIAN_POINT('Ctrl Pts',(53.2467916214334,21.9515821893404,18.5558017067762));
#28804=CARTESIAN_POINT('Ctrl Pts',(53.2353613305279,21.930143547732,18.557327582821));
#28805=CARTESIAN_POINT('Ctrl Pts',(53.230979888414,21.9217833221826,18.5579224419543));
#28806=CARTESIAN_POINT('Ctrl Pts',(53.2232320915487,21.9067410543683,18.5589925919422));
#28807=CARTESIAN_POINT('Ctrl Pts',(53.21984366561,21.9000705321351,18.5594670960113));
#28808=CARTESIAN_POINT('Ctrl Pts',(53.2127250609459,21.885859261093,18.5604779661414));
#28809=CARTESIAN_POINT('Ctrl Pts',(53.2090049093078,21.8783136796017,18.5610146709743));
#28810=CARTESIAN_POINT('Ctrl Pts',(53.1991422028856,21.8579859377695,18.5624606071198));
#28811=CARTESIAN_POINT('Ctrl Pts',(53.1930881335572,21.8451616203493,18.5633728791751));
#28812=CARTESIAN_POINT('Ctrl Pts',(53.1632549635988,21.7801801176472,18.5679966090179));
#28813=CARTESIAN_POINT('Ctrl Pts',(53.1415972910451,21.7270843242576,18.5717796241899));
#28814=CARTESIAN_POINT('Ctrl Pts',(53.0861655787287,21.5724546300179,18.582817890383));
#28815=CARTESIAN_POINT('Ctrl Pts',(53.0582333669201,21.469046053463,18.5902349100963));
#28816=CARTESIAN_POINT('Ctrl Pts',(53.0164415917545,21.2438109623391,18.6062119264787));
#28817=CARTESIAN_POINT('Ctrl Pts',(53.005234400944,21.1219108081174,18.6147522648045));
#28818=CARTESIAN_POINT('Ctrl Pts',(53.0052500162953,20.9997450290738,18.6227937120875));
#28819=CARTESIAN_POINT('Ctrl Pts',(53.0052500164767,20.9997436136241,18.6227938052581));
#28820=CARTESIAN_POINT('Ctrl Pts',(53.0052508228815,20.9934695837175,18.6232067871531));
#28821=CARTESIAN_POINT('Ctrl Pts',(53.0052812295882,20.9871954844429,18.6236183689611));
#28822=CARTESIAN_POINT('Ctrl Pts',(53.0054036384665,20.9743976083966,18.6244549063218));
#28823=CARTESIAN_POINT('Ctrl Pts',(53.0054980455807,20.9678739275997,18.6248797358704));
#28824=CARTESIAN_POINT('Ctrl Pts',(53.0057060265368,20.9571417189301,18.625575880343));
#28825=CARTESIAN_POINT('Ctrl Pts',(53.0058009183083,20.9529329391716,18.6258481869857));
#28826=CARTESIAN_POINT('Ctrl Pts',(53.0060117717511,20.9447329124107,18.6263773290831));
#28827=CARTESIAN_POINT('Ctrl Pts',(53.0061263948672,20.9407416397901,18.6266342372098));
#28828=CARTESIAN_POINT('Ctrl Pts',(53.0063978370226,20.9321852354407,18.6271835742972));
#28829=CARTESIAN_POINT('Ctrl Pts',(53.0065583523545,20.9276202723663,18.6274757948803));
#28830=CARTESIAN_POINT('Ctrl Pts',(53.0070192428518,20.9156807415714,18.6282379373242));
#28831=CARTESIAN_POINT('Ctrl Pts',(53.0073448721434,20.9083071365057,18.6287064723275));
#28832=CARTESIAN_POINT('Ctrl Pts',(53.0088491839476,20.8780539245543,18.6306206308297));
#28833=CARTESIAN_POINT('Ctrl Pts',(53.0103811057744,20.8551926124682,18.6320478496479));
#28834=CARTESIAN_POINT('Ctrl Pts',(53.0163547483494,20.7843629450692,18.636423954629));
#28835=CARTESIAN_POINT('Ctrl Pts',(53.0221404518353,20.7365230494234,18.639314563721));
#28836=CARTESIAN_POINT('Ctrl Pts',(53.0565943291302,20.5182844616601,18.652388534347));
#28837=CARTESIAN_POINT('Ctrl Pts',(53.1055892988108,20.3518587322202,18.6621091859325));
#28838=CARTESIAN_POINT('Ctrl Pts',(53.1961502569472,20.1468965143007,18.6755976310348));
#28839=CARTESIAN_POINT('Ctrl Pts',(53.2186849502699,20.1007917580869,18.678734267687));
#28840=CARTESIAN_POINT('Ctrl Pts',(53.2494529895803,20.0435481028146,18.6827865920195));
#28841=CARTESIAN_POINT('Ctrl Pts',(53.2560597815123,20.0315540454702,18.6836446733391));
#28842=CARTESIAN_POINT('Ctrl Pts',(53.266871289259,20.0123961252027,18.6850302788032));
#28843=CARTESIAN_POINT('Ctrl Pts',(53.2709982532485,20.0051887124398,18.6855550136619));
#28844=CARTESIAN_POINT('Ctrl Pts',(53.2789386319406,19.9915201459098,18.6865568541372));
#28845=CARTESIAN_POINT('Ctrl Pts',(53.2827437322724,19.9850543082703,18.687033652837));
#28846=CARTESIAN_POINT('Ctrl Pts',(53.2915135587098,19.9703426378938,18.6881251943778));
#28847=CARTESIAN_POINT('Ctrl Pts',(53.2965016427007,19.9621110152232,18.6887407812074));
#28848=CARTESIAN_POINT('Ctrl Pts',(53.3096643504369,19.9407396796292,18.6903518310582));
#28849=CARTESIAN_POINT('Ctrl Pts',(53.3179325240055,19.9276586279107,18.6913507113138));
#28850=CARTESIAN_POINT('Ctrl Pts',(53.3984520140796,19.8034918173579,18.700957262903));
#28851=CARTESIAN_POINT('Ctrl Pts',(53.4814378430074,19.6997905442718,18.7099805762316));
#28852=CARTESIAN_POINT('Ctrl Pts',(53.6410368518047,19.536641868137,18.7258447849989));
#28853=CARTESIAN_POINT('Ctrl Pts',(53.7128447848687,19.4730979473654,18.7325680028708));
#28854=CARTESIAN_POINT('Ctrl Pts',(53.8194027678941,19.3916817949866,18.7417737253925));
#28855=CARTESIAN_POINT('Ctrl Pts',(53.8505320890769,19.3692881435037,18.7443786988831));
#28856=CARTESIAN_POINT('Ctrl Pts',(53.8949430311443,19.3392441323328,18.7479597324971));
#28857=CARTESIAN_POINT('Ctrl Pts',(53.9076950912779,19.3308292555581,18.7489728983643));
#28858=CARTESIAN_POINT('Ctrl Pts',(53.9272789220579,19.3182267650912,18.7505045605717));
#28859=CARTESIAN_POINT('Ctrl Pts',(53.9340410368713,19.3139326174054,18.751029080199));
#28860=CARTESIAN_POINT('Ctrl Pts',(53.9451974662106,19.3069418928873,18.7518870993712));
#28861=CARTESIAN_POINT('Ctrl Pts',(53.9495766200719,19.3042214579562,18.7522220448244));
#28862=CARTESIAN_POINT('Ctrl Pts',(53.9580400840686,19.2990091164134,18.752865757851));
#28863=CARTESIAN_POINT('Ctrl Pts',(53.9621229043583,19.2965148700495,18.7531746724887));
#28864=CARTESIAN_POINT('Ctrl Pts',(53.9696612779904,19.2919467451694,18.753742013591));
#28865=CARTESIAN_POINT('Ctrl Pts',(53.9731141180961,19.2898686631034,18.7540007060626));
#28866=CARTESIAN_POINT('Ctrl Pts',(53.9810914230275,19.2851004167674,18.7545957079765));
#28867=CARTESIAN_POINT('Ctrl Pts',(53.9856202486522,19.2824176903602,18.7549315336374));
#28868=CARTESIAN_POINT('Ctrl Pts',(53.9990360537877,19.2745421819368,18.755920723018));
#28869=CARTESIAN_POINT('Ctrl Pts',(54.0079528263097,19.2694001272963,18.7565709156031));
#28870=CARTESIAN_POINT('Ctrl Pts',(54.1107066663573,19.2112000149813,18.7639852005353));
#28871=CARTESIAN_POINT('Ctrl Pts',(54.2086709083405,19.165755446381,18.7703134755018));
#28872=CARTESIAN_POINT('Ctrl Pts',(54.4245021411702,19.0861648989031,18.7836954551731));
#28873=CARTESIAN_POINT('Ctrl Pts',(54.5427996290358,19.0545106843378,18.7907147107882));
#28874=CARTESIAN_POINT('Ctrl Pts',(54.7209853631643,19.023991434884,18.801541812735));
#28875=CARTESIAN_POINT('Ctrl Pts',(54.7791259874304,19.0166511402908,18.8051099869406));
#28876=CARTESIAN_POINT('Ctrl Pts',(54.8517297169933,19.0107168929062,18.8096485719435));
#28877=CARTESIAN_POINT('Ctrl Pts',(54.8659697024608,19.0097067503554,18.8105426065393));
#28878=CARTESIAN_POINT('Ctrl Pts',(54.8886373473691,19.0083431402858,18.8119724128908));
#28879=CARTESIAN_POINT('Ctrl Pts',(54.8970586980233,19.0078901204862,18.8125050642727));
#28880=CARTESIAN_POINT('Ctrl Pts',(54.9129527438069,19.0071361645025,18.8135132213141));
#28881=CARTESIAN_POINT('Ctrl Pts',(54.9204247717523,19.0068238230911,18.8139883612269));
#28882=CARTESIAN_POINT('Ctrl Pts',(54.9372978334304,19.0062135350853,18.815064070495));
#28883=CARTESIAN_POINT('Ctrl Pts',(54.9466995209903,19.0059400502247,18.8156653944411));
#28884=CARTESIAN_POINT('Ctrl Pts',(54.9708473502626,19.0054085138189,18.8172149985182));
#28885=CARTESIAN_POINT('Ctrl Pts',(54.9855948468531,19.0052474975823,18.8181662821324));
#28886=CARTESIAN_POINT('Ctrl Pts',(55.0830677673982,19.0052642313653,18.8244874088679));
#28887=CARTESIAN_POINT('Ctrl Pts',(55.1657010683349,19.0104244140644,18.8300115289142));
#28888=CARTESIAN_POINT('Ctrl Pts',(55.4002460553659,19.0397844651118,18.8461485552684));
#28889=CARTESIAN_POINT('Ctrl Pts',(55.5499937451085,19.0764243864063,18.8570456105036));
#28890=CARTESIAN_POINT('Ctrl Pts',(55.7258940761164,19.1417052287217,18.86987739487));
#28891=CARTESIAN_POINT('Ctrl Pts',(55.7574383189822,19.1543377533466,18.8721773553897));
#28892=CARTESIAN_POINT('Ctrl Pts',(55.8078384912854,19.1760314912753,18.8758340144915));
#28893=CARTESIAN_POINT('Ctrl Pts',(55.8269007222035,19.1845938668317,18.8772127140775));
#28894=CARTESIAN_POINT('Ctrl Pts',(55.8520556419838,19.1963714172464,18.8790229733888));
#28895=CARTESIAN_POINT('Ctrl Pts',(55.8582704862637,19.1993205012178,18.879469472828));
#28896=CARTESIAN_POINT('Ctrl Pts',(55.8684867444005,19.2042332551658,18.8802020628601));
#28897=CARTESIAN_POINT('Ctrl Pts',(55.8724969923835,19.2061782623995,18.8804892765138));
#28898=CARTESIAN_POINT('Ctrl Pts',(55.8803538291335,19.210021481499,18.881051236974));
#28899=CARTESIAN_POINT('Ctrl Pts',(55.8842008600772,19.2119186817273,18.8813260406449));
#28900=CARTESIAN_POINT('Ctrl Pts',(55.8936745482161,19.2166287724571,18.8820019655575));
#28901=CARTESIAN_POINT('Ctrl Pts',(55.8992941366587,19.2194559281791,18.88240220631));
#28902=CARTESIAN_POINT('Ctrl Pts',(55.9186199264016,19.2292933636027,18.8837765290042));
#28903=CARTESIAN_POINT('Ctrl Pts',(55.9322586938332,19.2364359032744,18.8847427592111));
#28904=CARTESIAN_POINT('Ctrl Pts',(56.0595658203018,19.304995550461,18.8937399942552));
#28905=CARTESIAN_POINT('Ctrl Pts',(56.1671140392041,19.3771709353203,18.9011894054926));
#28906=CARTESIAN_POINT('Ctrl Pts',(56.3797709982094,19.5520358888799,18.9171628638262));
#28907=CARTESIAN_POINT('Ctrl Pts',(56.4820569208504,19.656918540189,18.9256729962863));
#28908=CARTESIAN_POINT('Ctrl Pts',(56.5827496905881,19.7858181602609,18.9358218910243));
#28909=CARTESIAN_POINT('Ctrl Pts',(56.5933458396525,19.7997570547188,18.9369151002039));
#28910=CARTESIAN_POINT('Ctrl Pts',(56.6091831877372,19.821169943452,18.9385889967104));
#28911=CARTESIAN_POINT('Ctrl Pts',(56.6145590233695,19.8285436459229,18.9391644440272));
#28912=CARTESIAN_POINT('Ctrl Pts',(56.6238162816745,19.8414260260623,18.9401682375366));
#28913=CARTESIAN_POINT('Ctrl Pts',(56.6277207655822,19.8469180093384,18.9405956870642));
#28914=CARTESIAN_POINT('Ctrl Pts',(56.6364186979856,19.8592845912053,18.9415571721671));
#28915=CARTESIAN_POINT('Ctrl Pts',(56.641196777209,19.8661697949329,18.9420917835269));
#28916=CARTESIAN_POINT('Ctrl Pts',(56.6538604544527,19.8846659006487,18.9435261857914));
#28917=CARTESIAN_POINT('Ctrl Pts',(56.6616670175088,19.8963300936447,18.9444289338833));
#28918=CARTESIAN_POINT('Ctrl Pts',(56.6961341467995,19.9490239280437,18.9484997829654));
#28919=CARTESIAN_POINT('Ctrl Pts',(56.7214007537069,19.990940783661,18.9517187949409));
#28920=CARTESIAN_POINT('Ctrl Pts',(56.8275093696642,20.1825768818737,18.9663612683641));
#28921=CARTESIAN_POINT('Ctrl Pts',(56.8905319436068,20.3413320469431,18.9783755644266));
#28922=CARTESIAN_POINT('Ctrl Pts',(56.9487071097244,20.5689800820716,18.9946153425056));
#28923=CARTESIAN_POINT('Ctrl Pts',(56.9616968761499,20.6325974655493,18.999042275886));
#28924=CARTESIAN_POINT('Ctrl Pts',(56.9736747446051,20.7104685202268,19.0042442285143));
#28925=CARTESIAN_POINT('Ctrl Pts',(56.9756429530676,20.7242185227259,19.0051545938565));
#28926=CARTESIAN_POINT('Ctrl Pts',(56.9782378569705,20.7438029162838,19.0064385917439));
#28927=CARTESIAN_POINT('Ctrl Pts',(56.9789826328377,20.7496208764765,19.0068184463785));
#28928=CARTESIAN_POINT('Ctrl Pts',(56.980223270161,20.7596638648082,19.0074713231178));
#28929=CARTESIAN_POINT('Ctrl Pts',(56.980731294894,20.7638873227034,19.0077450187738));
#28930=CARTESIAN_POINT('Ctrl Pts',(56.9817618282143,20.7726921051408,19.0083137663207));
#28931=CARTESIAN_POINT('Ctrl Pts',(56.9822819656755,20.7772736377574,19.0086086852659));
#28932=CARTESIAN_POINT('Ctrl Pts',(56.9836145891381,20.789386367956,19.0093857825045));
#28933=CARTESIAN_POINT('Ctrl Pts',(56.9844000809099,20.7969205487186,19.0098664725015));
#28934=CARTESIAN_POINT('Ctrl Pts',(56.9875450505553,20.8288484750968,19.0118929118764));
#28935=CARTESIAN_POINT('Ctrl Pts',(56.9894979076109,20.853281301279,19.0134174621401));
#28936=CARTESIAN_POINT('Ctrl Pts',(56.9994446793162,21.0152710298696,19.0233887507599));
#28937=CARTESIAN_POINT('Ctrl Pts',(56.9936185569763,21.1533185713378,19.0312550500828));
#28938=CARTESIAN_POINT('Ctrl Pts',(56.9633649545991,21.3594405805898,19.0433684390515));
#28939=CARTESIAN_POINT('Ctrl Pts',(56.9494338727199,21.4286095605217,19.0474941419294));
#28940=CARTESIAN_POINT('Ctrl Pts',(56.9168038199123,21.5554721118379,19.0553294145845));
#28941=CARTESIAN_POINT('Ctrl Pts',(56.8990813714044,21.6133310825879,19.059010236262));
#28942=CARTESIAN_POINT('Ctrl Pts',(56.8739157975448,21.6838676103112,19.0636753812177));
#28943=CARTESIAN_POINT('Ctrl Pts',(56.868925403165,21.6973902385962,19.064577949759));
#28944=CARTESIAN_POINT('Ctrl Pts',(56.8607727625021,21.718765557537,19.0660182472214));
#28945=CARTESIAN_POINT('Ctrl Pts',(56.8577062624627,21.7266544152496,19.066552774916));
#28946=CARTESIAN_POINT('Ctrl Pts',(56.851837472589,21.741472454897,19.0675625117386));
#28947=CARTESIAN_POINT('Ctrl Pts',(56.8490462549128,21.7484058865056,19.0680373415218));
#28948=CARTESIAN_POINT('Ctrl Pts',(56.8426724697429,21.7639851541,19.0691096997419));
#28949=CARTESIAN_POINT('Ctrl Pts',(56.8390679101149,21.7726217467077,19.0697079636187));
#28950=CARTESIAN_POINT('Ctrl Pts',(56.8296872124572,21.7946604581037,19.0712444747469));
#28951=CARTESIAN_POINT('Ctrl Pts',(56.8238246087663,21.8080249481113,19.0721856405075));
#28952=CARTESIAN_POINT('Ctrl Pts',(56.7854309130868,21.8930008009626,19.0782314167247));
#28953=CARTESIAN_POINT('Ctrl Pts',(56.7488389785588,21.9626907338934,19.0834749306784));
#28954=CARTESIAN_POINT('Ctrl Pts',(56.6433048237484,22.1377114784355,19.09739769515));
#28955=CARTESIAN_POINT('Ctrl Pts',(56.5683430000971,22.239005197639,19.1062382761555));
#28956=CARTESIAN_POINT('Ctrl Pts',(56.4333577097724,22.389367217848,19.1202550848713));
#28957=CARTESIAN_POINT('Ctrl Pts',(56.3791340580155,22.4432073183055,19.1254893040685));
#28958=CARTESIAN_POINT('Ctrl Pts',(56.3119880604447,22.502628334578,19.1314041193109));
#28959=CARTESIAN_POINT('Ctrl Pts',(56.3019361160822,22.5113460739271,19.1322756212419));
#28960=CARTESIAN_POINT('Ctrl Pts',(56.2874049583898,22.5236959226534,19.133514692726));
#28961=CARTESIAN_POINT('Ctrl Pts',(56.2829963113869,22.5274099837878,19.133887920117));
#28962=CARTESIAN_POINT('Ctrl Pts',(56.2753188896451,22.5338211270435,19.1345331175107));
#28963=CARTESIAN_POINT('Ctrl Pts',(56.2720575298319,22.5365269806357,19.1348057181737));
#28964=CARTESIAN_POINT('Ctrl Pts',(56.265196074598,22.5421829066819,19.1353761067526));
#28965=CARTESIAN_POINT('Ctrl Pts',(56.2615942647183,22.545130783185,19.1356737389799));
#28966=CARTESIAN_POINT('Ctrl Pts',(56.2519521153634,22.5529661410109,19.1364658617054));
#28967=CARTESIAN_POINT('Ctrl Pts',(56.2458934082106,22.5578310416755,19.1369587592221));
#28968=CARTESIAN_POINT('Ctrl Pts',(56.2192646124145,22.5789581827537,19.1391048146271));
#28969=CARTESIAN_POINT('Ctrl Pts',(56.1984023821149,22.5948501572263,19.1407335595669));
#28970=CARTESIAN_POINT('Ctrl Pts',(56.0057508557561,22.7356883109164,19.155364529448));
#28971=CARTESIAN_POINT('Ctrl Pts',(55.8153320901779,22.8328687894064,19.1670536088278));
#28972=CARTESIAN_POINT('Ctrl Pts',(55.5605167343166,22.9151780027317,19.1831270554104));
#28973=CARTESIAN_POINT('Ctrl Pts',(55.5072127802324,22.9299793118287,19.1865012302363));
#28974=CARTESIAN_POINT('Ctrl Pts',(55.4397086254523,22.9457339430014,19.1908215268714));
#28975=CARTESIAN_POINT('Ctrl Pts',(55.4260180932031,22.9487772629551,19.191700066807));
#28976=CARTESIAN_POINT('Ctrl Pts',(55.4040994593774,22.9534076343674,19.1931108235232));
#28977=CARTESIAN_POINT('Ctrl Pts',(55.3958913136936,22.9550876766389,19.1936400645022));
#28978=CARTESIAN_POINT('Ctrl Pts',(55.3803279771533,22.9581711514163,19.1946454273428));
#28979=CARTESIAN_POINT('Ctrl Pts',(55.3729749745889,22.9595849801089,19.1951212084902));
#28980=CARTESIAN_POINT('Ctrl Pts',(55.3562793278265,22.9626978303845,19.1962033830579));
#28981=CARTESIAN_POINT('Ctrl Pts',(55.3469322156051,22.9643715955625,19.1968105677649));
#28982=CARTESIAN_POINT('Ctrl Pts',(55.3227450990553,22.9685247095706,19.198385334843));
#28983=CARTESIAN_POINT('Ctrl Pts',(55.3078885737934,22.9709029749561,19.1993560871394));
#28984=CARTESIAN_POINT('Ctrl Pts',(55.2503105410471,22.9794533020705,19.2031325060876));
#28985=CARTESIAN_POINT('Ctrl Pts',(55.2074350719438,22.9844038814477,19.2059750470036));
#28986=CARTESIAN_POINT('Ctrl Pts',(55.1644482551197,22.9879598421216,19.2088565303878));
#28987=CARTESIAN_POINT('Origin',(55.,21.,6.22095488139522));
#28988=CARTESIAN_POINT('',(55.1644485224877,22.9879598200043,20.1685383772559));
#28989=CARTESIAN_POINT('',(55.1644483497948,22.9879598342899,20.0118645378774));
#28990=CARTESIAN_POINT('',(55.1644483516311,22.987959834138,6.22095488139522));
#28991=CARTESIAN_POINT('',(53.0052501477468,20.9992322527395,19.5807109120749));
#28992=CARTESIAN_POINT('Ctrl Pts',(55.1644485224877,22.9879598200043,20.1685383772559));
#28993=CARTESIAN_POINT('Ctrl Pts',(55.2068925657508,22.9844487529632,20.1655689947827));
#28994=CARTESIAN_POINT('Ctrl Pts',(55.2492396823092,22.9795771043672,20.1625933152215));
#28995=CARTESIAN_POINT('Ctrl Pts',(55.3776735384323,22.9606099556836,20.1535712346217));
#28996=CARTESIAN_POINT('Ctrl Pts',(55.4630056307296,22.9422301896129,20.147577910066));
#28997=CARTESIAN_POINT('Ctrl Pts',(55.5568977412209,22.9154637043003,20.141166337482));
#28998=CARTESIAN_POINT('Ctrl Pts',(55.5669034753316,22.9125262763177,20.1404855109366));
#28999=CARTESIAN_POINT('Ctrl Pts',(55.5819530740513,22.9079796123358,20.1394656324163));
#29000=CARTESIAN_POINT('Ctrl Pts',(55.5870141353317,22.9064285950373,20.1391233664781));
#29001=CARTESIAN_POINT('Ctrl Pts',(55.5960646797729,22.9036154988886,20.1385126525331));
#29002=CARTESIAN_POINT('Ctrl Pts',(55.600056408017,22.9023610010509,20.13824377459));
#29003=CARTESIAN_POINT('Ctrl Pts',(55.6087487066744,22.8995991526048,20.1376593184724));
#29004=CARTESIAN_POINT('Ctrl Pts',(55.6134476314019,22.8980869140415,20.1373440295626));
#29005=CARTESIAN_POINT('Ctrl Pts',(55.626747170255,22.8937522229867,20.1364533975958));
#29006=CARTESIAN_POINT('Ctrl Pts',(55.6353343864784,22.8908886065108,20.1358804056323));
#29007=CARTESIAN_POINT('Ctrl Pts',(55.6904512913292,22.872090664813,20.1322142100668));
#29008=CARTESIAN_POINT('Ctrl Pts',(55.7364019065688,22.8544971200174,20.1292107028611));
#29009=CARTESIAN_POINT('Ctrl Pts',(55.9126743407584,22.7794190039197,20.1177256518476));
#29010=CARTESIAN_POINT('Ctrl Pts',(56.0373446780462,22.7097450354183,20.1096565212819));
#29011=CARTESIAN_POINT('Ctrl Pts',(56.2308614065062,22.5725745027399,20.0957351796463));
#29012=CARTESIAN_POINT('Ctrl Pts',(56.3041702827222,22.5123315865029,20.0900687275271));
#29013=CARTESIAN_POINT('Ctrl Pts',(56.3839052386286,22.4366848540956,20.0832434936051));
#29014=CARTESIAN_POINT('Ctrl Pts',(56.3947764399891,22.426133143199,20.0822975786373));
#29015=CARTESIAN_POINT('Ctrl Pts',(56.4122876962951,22.4087447684215,20.0807479769109));
#29016=CARTESIAN_POINT('Ctrl Pts',(56.419000932948,22.4019824203177,20.08014754381));
#29017=CARTESIAN_POINT('Ctrl Pts',(56.4309062958685,22.389816852452,20.0790711186767));
#29018=CARTESIAN_POINT('Ctrl Pts',(56.4361169455721,22.3844319510374,20.0785959495107));
#29019=CARTESIAN_POINT('Ctrl Pts',(56.4470787788155,22.3729750595595,20.0775876269041));
#29020=CARTESIAN_POINT('Ctrl Pts',(56.4528223499427,22.3668960173567,20.0770541582223));
#29021=CARTESIAN_POINT('Ctrl Pts',(56.4680431136402,22.3505819301759,20.075626496364));
#29022=CARTESIAN_POINT('Ctrl Pts',(56.4774513255192,22.340283439406,20.0747293957232));
#29023=CARTESIAN_POINT('Ctrl Pts',(56.5229678364551,22.2893981528988,20.0703159827555));
#29024=CARTESIAN_POINT('Ctrl Pts',(56.5575128165892,22.2474500041035,20.0667357340029));
#29025=CARTESIAN_POINT('Ctrl Pts',(56.7110285342887,22.0447040053157,20.0496818824254));
#29026=CARTESIAN_POINT('Ctrl Pts',(56.8070677364786,21.8680489617466,20.0353749807913));
#29027=CARTESIAN_POINT('Ctrl Pts',(56.888131111058,21.6445302884007,20.0192556003222));
#29028=CARTESIAN_POINT('Ctrl Pts',(56.9000145208163,21.6086079578724,20.0167264169441));
#29029=CARTESIAN_POINT('Ctrl Pts',(56.9133725609547,21.5640115935997,20.0136791359467));
#29030=CARTESIAN_POINT('Ctrl Pts',(56.9158204343277,21.5556399057395,20.0131110669112));
#29031=CARTESIAN_POINT('Ctrl Pts',(56.9195624907968,21.5425233534145,20.012227518829));
#29032=CARTESIAN_POINT('Ctrl Pts',(56.9208941362448,21.5377894231772,20.0119099514943));
#29033=CARTESIAN_POINT('Ctrl Pts',(56.9233268667823,21.529016869178,20.0113239570294));
#29034=CARTESIAN_POINT('Ctrl Pts',(56.9244327389331,21.5249797312436,20.0110552649709));
#29035=CARTESIAN_POINT('Ctrl Pts',(56.9269146787255,21.515805837139,20.0104469017423));
#29036=CARTESIAN_POINT('Ctrl Pts',(56.9282829170921,21.5106670480304,20.0101076842579));
#29037=CARTESIAN_POINT('Ctrl Pts',(56.932392922781,21.4949787484439,20.00907665891));
#29038=CARTESIAN_POINT('Ctrl Pts',(56.9350688413667,21.4844119747152,20.0083885163746));
#29039=CARTESIAN_POINT('Ctrl Pts',(56.94107266634,21.4598598798263,20.006803049675));
#29040=CARTESIAN_POINT('Ctrl Pts',(56.9443363169651,21.4458593022139,20.0059090169516));
#29041=CARTESIAN_POINT('Ctrl Pts',(56.9824281581862,21.2740720558003,19.9950484346713));
#29042=CARTESIAN_POINT('Ctrl Pts',(56.9981154240316,21.1126331009586,19.9859281415125));
#29043=CARTESIAN_POINT('Ctrl Pts',(56.9915269694546,20.8442136350118,19.9702403132308));
#29044=CARTESIAN_POINT('Ctrl Pts',(56.9803234833983,20.7377720854204,19.9638886483225));
#29045=CARTESIAN_POINT('Ctrl Pts',(56.9578064547157,20.617560178734,19.9562969303724));
#29046=CARTESIAN_POINT('Ctrl Pts',(56.9547852568531,20.6024060996335,19.9553324358982));
#29047=CARTESIAN_POINT('Ctrl Pts',(56.9495980750784,20.5778774511832,19.953758448497));
#29048=CARTESIAN_POINT('Ctrl Pts',(56.9475397526504,20.5684805830598,19.9531523842822));
#29049=CARTESIAN_POINT('Ctrl Pts',(56.9437550286249,20.5517810174614,19.9520696869347));
#29050=CARTESIAN_POINT('Ctrl Pts',(56.9420552260762,20.5444724333594,19.9515939138762));
#29051=CARTESIAN_POINT('Ctrl Pts',(56.9383856057007,20.5290882241893,19.9505882855224));
#29052=CARTESIAN_POINT('Ctrl Pts',(56.936406469353,20.5210149908562,19.9500581385882));
#29053=CARTESIAN_POINT('Ctrl Pts',(56.9310276047434,20.4996519950869,19.9486487514117));
#29054=CARTESIAN_POINT('Ctrl Pts',(56.9275411953813,20.4863847151677,19.9477667332299));
#29055=CARTESIAN_POINT('Ctrl Pts',(56.9103017794413,20.4234303167523,19.943548601787));
#29056=CARTESIAN_POINT('Ctrl Pts',(56.8947638294469,20.3742566725778,19.9401552042871));
#29057=CARTESIAN_POINT('Ctrl Pts',(56.8182924566594,20.161336567381,19.9250135828607));
#29058=CARTESIAN_POINT('Ctrl Pts',(56.7379064757038,20.0054107632745,19.9126472932553));
#29059=CARTESIAN_POINT('Ctrl Pts',(56.6290782609817,19.8487435828613,19.8994990849802));
#29060=CARTESIAN_POINT('Ctrl Pts',(56.6197231540655,19.8356185147986,19.8983922274142));
#29061=CARTESIAN_POINT('Ctrl Pts',(56.5813444803813,19.7831315618491,19.8939481734097));
#29062=CARTESIAN_POINT('Ctrl Pts',(56.5510343901165,19.7447261804967,19.89065524359));
#29063=CARTESIAN_POINT('Ctrl Pts',(56.5137840228758,19.7009391742751,19.8868871761587));
#29064=CARTESIAN_POINT('Ctrl Pts',(56.5081853980093,19.6944434487974,19.8863278299679));
#29065=CARTESIAN_POINT('Ctrl Pts',(56.4990294406559,19.6839578783113,19.885424617158));
#29066=CARTESIAN_POINT('Ctrl Pts',(56.4954977253194,19.6799459536861,19.8850789629116));
#29067=CARTESIAN_POINT('Ctrl Pts',(56.4891700794169,19.6728159224833,19.8844646100367));
#29068=CARTESIAN_POINT('Ctrl Pts',(56.4863804195372,19.6696923849885,19.8841954593919));
#29069=CARTESIAN_POINT('Ctrl Pts',(56.4803070036286,19.6629350338627,19.8836131686394));
#29070=CARTESIAN_POINT('Ctrl Pts',(56.4770197005771,19.6593045259956,19.8833003003856));
#29071=CARTESIAN_POINT('Ctrl Pts',(56.4677394973076,19.6491310001588,19.8824233839512));
#29072=CARTESIAN_POINT('Ctrl Pts',(56.461716175867,19.6426157084796,19.8818615734112));
#29073=CARTESIAN_POINT('Ctrl Pts',(56.4244841058512,19.6028778546974,19.8784320280204));
#29074=CARTESIAN_POINT('Ctrl Pts',(56.3921850067446,19.5706900649949,19.8756411600798));
#29075=CARTESIAN_POINT('Ctrl Pts',(56.2711269226517,19.4580506009503,19.8656981913342));
#29076=CARTESIAN_POINT('Ctrl Pts',(56.1762697154891,19.3845231516665,19.8588476372468));
#29077=CARTESIAN_POINT('Ctrl Pts',(55.9738486166519,19.2549557580819,19.8448576589149));
#29078=CARTESIAN_POINT('Ctrl Pts',(55.8666466787993,19.199311704218,19.8377406684143));
#29079=CARTESIAN_POINT('Ctrl Pts',(55.7406842837202,19.1477968583911,19.829294390675));
#29080=CARTESIAN_POINT('Ctrl Pts',(55.7262137737636,19.1420755614667,19.8283232495568));
#29081=CARTESIAN_POINT('Ctrl Pts',(55.7026612586077,19.1330806443398,19.8267405453512));
#29082=CARTESIAN_POINT('Ctrl Pts',(55.6936196485723,19.1297025630317,19.8261324746091));
#29083=CARTESIAN_POINT('Ctrl Pts',(55.6775023375678,19.1238138394213,19.8250475289918));
#29084=CARTESIAN_POINT('Ctrl Pts',(55.670436261774,19.121277257566,19.8245715274688));
#29085=CARTESIAN_POINT('Ctrl Pts',(55.6555332613929,19.1160221572389,19.8235667945475));
#29086=CARTESIAN_POINT('Ctrl Pts',(55.6476933788636,19.1133125186303,19.8230377796548));
#29087=CARTESIAN_POINT('Ctrl Pts',(55.6269187105331,19.1062770762251,19.8216346175487));
#29088=CARTESIAN_POINT('Ctrl Pts',(55.6139562465485,19.1020349598471,19.8207577359749));
#29089=CARTESIAN_POINT('Ctrl Pts',(55.5526555776869,19.0826672925725,19.8166036979754));
#29090=CARTESIAN_POINT('Ctrl Pts',(55.5037999514034,19.0692546150528,19.813271354255));
#29091=CARTESIAN_POINT('Ctrl Pts',(55.2896497763713,19.0191439196562,19.7985610711798));
#29092=CARTESIAN_POINT('Ctrl Pts',(55.1205826956811,19.0017178666944,19.7866052978476));
#29093=CARTESIAN_POINT('Ctrl Pts',(54.8813061483446,19.0075508506724,19.7700633461535));
#29094=CARTESIAN_POINT('Ctrl Pts',(54.8113555479435,19.012952615346,19.7652859010389));
#29095=CARTESIAN_POINT('Ctrl Pts',(54.7316989150764,19.0233496943716,19.7600124900731));
#29096=CARTESIAN_POINT('Ctrl Pts',(54.7215801589999,19.0247495587463,19.7593457524462));
#29097=CARTESIAN_POINT('Ctrl Pts',(54.7062796539748,19.0269861984518,19.7583427951155));
#29098=CARTESIAN_POINT('Ctrl Pts',(54.7010899026329,19.0277657699983,19.7580035136203));
#29099=CARTESIAN_POINT('Ctrl Pts',(54.6917705275639,19.0292032980762,19.7573959660451));
#29100=CARTESIAN_POINT('Ctrl Pts',(54.6876398614154,19.0298537635999,19.7571272895497));
#29101=CARTESIAN_POINT('Ctrl Pts',(54.6786017645963,19.0313061535103,19.7565407508599));
#29102=CARTESIAN_POINT('Ctrl Pts',(54.6736952850307,19.0321134379197,19.7562231940534));
#29103=CARTESIAN_POINT('Ctrl Pts',(54.659699085798,19.0344700785973,19.7553196439212));
#29104=CARTESIAN_POINT('Ctrl Pts',(54.6506168770577,19.0360641493851,19.7547361109213));
#29105=CARTESIAN_POINT('Ctrl Pts',(54.5894479640549,19.0472380207953,19.7508228152732));
#29106=CARTESIAN_POINT('Ctrl Pts',(54.5377445535237,19.0588268201204,19.7475972640817));
#29107=CARTESIAN_POINT('Ctrl Pts',(54.3174720489465,19.1175010831857,19.7339747062371));
#29108=CARTESIAN_POINT('Ctrl Pts',(54.1550424812256,19.1845934450898,19.7241677248914));
#29109=CARTESIAN_POINT('Ctrl Pts',(53.9504336949272,19.3025953076205,19.7100558375068));
#29110=CARTESIAN_POINT('Ctrl Pts',(53.898864081405,19.3355869801227,19.7063364495535));
#29111=CARTESIAN_POINT('Ctrl Pts',(53.8366943943565,19.379515250865,19.7015990230936));
#29112=CARTESIAN_POINT('Ctrl Pts',(53.8245907743834,19.3882730108671,19.700664253588));
#29113=CARTESIAN_POINT('Ctrl Pts',(53.8056216393073,19.402325741884,19.6991788331372));
#29114=CARTESIAN_POINT('Ctrl Pts',(53.7986901565374,19.4075310490625,19.6986316615048));
#29115=CARTESIAN_POINT('Ctrl Pts',(53.7860799382922,19.417130076053,19.6976280383304));
#29116=CARTESIAN_POINT('Ctrl Pts',(53.7803905503967,19.4215096134015,19.6971721492099));
#29117=CARTESIAN_POINT('Ctrl Pts',(53.7746202439719,19.4260012599635,19.6967065927026));
#29118=CARTESIAN_POINT('Ctrl Pts',(53.7745155054043,19.426082805982,19.6966981411737));
#29119=CARTESIAN_POINT('Ctrl Pts',(53.774310284996,19.4262426167749,19.6966815794954));
#29120=CARTESIAN_POINT('Ctrl Pts',(53.7742098024999,19.4263208807273,19.6966734693784));
#29121=CARTESIAN_POINT('Ctrl Pts',(53.7740128039319,19.4264743495741,19.6966575673437));
#29122=CARTESIAN_POINT('Ctrl Pts',(53.7739162873851,19.426549553646,19.6966497754639));
#29123=CARTESIAN_POINT('Ctrl Pts',(53.7737269564555,19.4266971051241,19.6966344887941));
#29124=CARTESIAN_POINT('Ctrl Pts',(53.7736341415466,19.4267694518703,19.6966269940299));
#29125=CARTESIAN_POINT('Ctrl Pts',(53.7734519725674,19.4269114736481,19.696612282306));
#29126=CARTESIAN_POINT('Ctrl Pts',(53.7733626179518,19.426981148142,19.6966050653637));
#29127=CARTESIAN_POINT('Ctrl Pts',(53.7731871484474,19.4271179949871,19.696590891606));
#29128=CARTESIAN_POINT('Ctrl Pts',(53.7731010331595,19.427185166781,19.6965839348141));
#29129=CARTESIAN_POINT('Ctrl Pts',(53.7658317660991,19.4328563131827,19.6959966283242));
#29130=CARTESIAN_POINT('Ctrl Pts',(53.758687185818,19.438509347611,19.6954143322578));
#29131=CARTESIAN_POINT('Ctrl Pts',(53.743874080362,19.450395890613,19.6941963105001));
#29132=CARTESIAN_POINT('Ctrl Pts',(53.7362126675136,19.4566378279134,19.6935602554901));
#29133=CARTESIAN_POINT('Ctrl Pts',(53.7163741286914,19.4730475299799,19.6918971411821));
#29134=CARTESIAN_POINT('Ctrl Pts',(53.7042715482737,19.4833039267833,19.6908665168312));
#29135=CARTESIAN_POINT('Ctrl Pts',(53.6686113282836,19.5142627181813,19.6877810675712));
#29136=CARTESIAN_POINT('Ctrl Pts',(53.6454190792924,19.535376698602,19.6857096885247));
#29137=CARTESIAN_POINT('Ctrl Pts',(53.5106817081229,19.6639786375248,19.6732814911991));
#29138=CARTESIAN_POINT('Ctrl Pts',(53.4114802739554,19.7836063389707,19.6624158048673));
#29139=CARTESIAN_POINT('Ctrl Pts',(53.2792396776596,19.9872108322123,19.6455412103445));
#29140=CARTESIAN_POINT('Ctrl Pts',(53.2362702536912,20.0640411028892,19.6394949453696));
#29141=CARTESIAN_POINT('Ctrl Pts',(53.1940278570395,20.1528866520976,19.6330344712594));
#29142=CARTESIAN_POINT('Ctrl Pts',(53.1896219453678,20.1623439154723,19.6323532998204));
#29143=CARTESIAN_POINT('Ctrl Pts',(53.1830922351114,20.1766520983904,19.6313330074889));
#29144=CARTESIAN_POINT('Ctrl Pts',(53.1809133008997,20.181477443241,19.6309906688664));
#29145=CARTESIAN_POINT('Ctrl Pts',(53.1770467441223,20.1901318023486,19.630379877338));
#29146=CARTESIAN_POINT('Ctrl Pts',(53.175351939108,20.1939574914394,19.6301109940216));
#29147=CARTESIAN_POINT('Ctrl Pts',(53.1716843337103,20.2023072368301,19.6295265865118));
#29148=CARTESIAN_POINT('Ctrl Pts',(53.1697162839979,20.2068332834615,19.6292113511998));
#29149=CARTESIAN_POINT('Ctrl Pts',(53.164187932384,20.2196773245214,19.6283210237136));
#29150=CARTESIAN_POINT('Ctrl Pts',(53.1606673421879,20.2280124309603,19.6277482800863));
#29151=CARTESIAN_POINT('Ctrl Pts',(53.1384078926944,20.2817291656545,19.6240876069672));
#29152=CARTESIAN_POINT('Ctrl Pts',(53.1212915379535,20.3277697052877,19.6210890625608));
#29153=CARTESIAN_POINT('Ctrl Pts',(53.0393055075407,20.5759958794105,19.6054175802769));
#29154=CARTESIAN_POINT('Ctrl Pts',(53.0053318643117,20.7869174531364,19.5936625725931));
#29155=CARTESIAN_POINT('Ctrl Pts',(53.0052501477468,20.9992322527395,19.5807109120749));
#29156=CARTESIAN_POINT('Ctrl Pts',(53.0052501469746,20.9992342617848,19.5807107895187));
#29157=CARTESIAN_POINT('Ctrl Pts',(53.0052371631856,21.0330570625816,19.5786475248104));
#29158=CARTESIAN_POINT('Ctrl Pts',(53.0060844221468,21.0668734766943,19.5765607928456));
#29159=CARTESIAN_POINT('Ctrl Pts',(53.0082529989016,21.1097966440269,19.5738751223118));
#29160=CARTESIAN_POINT('Ctrl Pts',(53.0087780256483,21.1189389080265,19.5733009712841));
#29161=CARTESIAN_POINT('Ctrl Pts',(53.0098294143081,21.135280079236,19.5722707643735));
#29162=CARTESIAN_POINT('Ctrl Pts',(53.0103319388128,21.1424803989021,19.5718154567695));
#29163=CARTESIAN_POINT('Ctrl Pts',(53.0114234462309,21.156985869494,19.5708953708877));
#29164=CARTESIAN_POINT('Ctrl Pts',(53.0120136320268,21.1642908148114,19.5704305618937));
#29165=CARTESIAN_POINT('Ctrl Pts',(53.0133666780071,21.1799615911391,19.5694302443483));
#29166=CARTESIAN_POINT('Ctrl Pts',(53.0141421543837,21.1883261632965,19.5688943483502));
#29167=CARTESIAN_POINT('Ctrl Pts',(53.0163624924566,21.2107347144899,19.5674533198062));
#29168=CARTESIAN_POINT('Ctrl Pts',(53.0179036343077,21.2247684615977,19.5665451835389));
#29169=CARTESIAN_POINT('Ctrl Pts',(53.025169795944,21.2850318402525,19.5626203544289));
#29170=CARTESIAN_POINT('Ctrl Pts',(53.0323638547637,21.3310662888805,19.5595580230171));
#29171=CARTESIAN_POINT('Ctrl Pts',(53.0778666466899,21.5676153984877,19.5434780508149));
#29172=CARTESIAN_POINT('Ctrl Pts',(53.1422567129725,21.7520306695359,19.5296374991767));
#29173=CARTESIAN_POINT('Ctrl Pts',(53.2556018130522,21.9688355601604,19.5129086321886));
#29174=CARTESIAN_POINT('Ctrl Pts',(53.2806371710585,22.0126005140549,19.5095144760629));
#29175=CARTESIAN_POINT('Ctrl Pts',(53.3121247011643,22.0631027681698,19.5056166761565));
#29176=CARTESIAN_POINT('Ctrl Pts',(53.3169965703753,22.0707987596201,19.5050232392136));
#29177=CARTESIAN_POINT('Ctrl Pts',(53.3245963776032,22.0826240113679,19.5041125670641));
#29178=CARTESIAN_POINT('Ctrl Pts',(53.32728717751,22.0867768228566,19.5037929807899));
#29179=CARTESIAN_POINT('Ctrl Pts',(53.332281251709,22.0944218742721,19.5032051232543));
#29180=CARTESIAN_POINT('Ctrl Pts',(53.3345800453534,22.0979168627573,19.5029365731739));
#29181=CARTESIAN_POINT('Ctrl Pts',(53.3398040465678,22.105805052509,19.5023308718945));
#29182=CARTESIAN_POINT('Ctrl Pts',(53.3427357003899,22.1101938842967,19.5019941575711));
#29183=CARTESIAN_POINT('Ctrl Pts',(53.3514705647922,22.123158709302,19.5010001715235));
#29184=CARTESIAN_POINT('Ctrl Pts',(53.3573232774822,22.1317013657367,19.5003461159191));
#29185=CARTESIAN_POINT('Ctrl Pts',(53.4092020266819,22.206173445886,19.4946484646242));
#29186=CARTESIAN_POINT('Ctrl Pts',(53.4591147094195,22.2693180566445,19.4898451893965));
#29187=CARTESIAN_POINT('Ctrl Pts',(53.5957691520135,22.4222161164272,19.477805380152));
#29188=CARTESIAN_POINT('Ctrl Pts',(53.687355306074,22.5071587836494,19.4706957785555));
#29189=CARTESIAN_POINT('Ctrl Pts',(53.8288123647533,22.615617778181,19.4601615225846));
#29190=CARTESIAN_POINT('Ctrl Pts',(53.8726488913392,22.6465054272489,19.456953440164));
#29191=CARTESIAN_POINT('Ctrl Pts',(53.9370828462569,22.6881257579331,19.4522742454483));
#29192=CARTESIAN_POINT('Ctrl Pts',(53.9567076222584,22.7003242042576,19.450853806563));
#29193=CARTESIAN_POINT('Ctrl Pts',(53.987515511676,22.7187397268907,19.4486284417327));
#29194=CARTESIAN_POINT('Ctrl Pts',(53.9985543751627,22.7251949850885,19.4478319507107));
#29195=CARTESIAN_POINT('Ctrl Pts',(54.0193504056747,22.7370891465052,19.4463326301377));
#29196=CARTESIAN_POINT('Ctrl Pts',(54.0290927122807,22.7425531154884,19.4456307237154));
#29197=CARTESIAN_POINT('Ctrl Pts',(54.0456129294963,22.7516369248106,19.4444410495563));
#29198=CARTESIAN_POINT('Ctrl Pts',(54.0523668748041,22.7552999897592,19.4439548334359));
#29199=CARTESIAN_POINT('Ctrl Pts',(54.0658674139152,22.7625215038587,19.4429831605944));
#29200=CARTESIAN_POINT('Ctrl Pts',(54.0726135905341,22.7660804581988,19.4424977322375));
#29201=CARTESIAN_POINT('Ctrl Pts',(54.0875067382461,22.7738284950377,19.441426249969));
#29202=CARTESIAN_POINT('Ctrl Pts',(54.0956624534876,22.7780003036803,19.4408396008201));
#29203=CARTESIAN_POINT('Ctrl Pts',(54.1243865609606,22.7924444886978,19.4387736458949));
#29204=CARTESIAN_POINT('Ctrl Pts',(54.145102900839,22.8024169928704,19.4372839739443));
#29205=CARTESIAN_POINT('Ctrl Pts',(54.3173800160284,22.8817101429592,19.4248937712895));
#29206=CARTESIAN_POINT('Ctrl Pts',(54.4768823188497,22.932130734221,19.4133262550094));
#29207=CARTESIAN_POINT('Ctrl Pts',(54.7154101072182,22.9758028013711,19.3964193239194));
#29208=CARTESIAN_POINT('Ctrl Pts',(54.7907916730864,22.9852006129768,19.3911449524743));
#29209=CARTESIAN_POINT('Ctrl Pts',(54.8902459032051,22.9918701242246,19.3844030382907));
#29210=CARTESIAN_POINT('Ctrl Pts',(54.9139898417861,22.9930366057191,19.3828098068299));
#29211=CARTESIAN_POINT('Ctrl Pts',(54.95379973578,22.9942795547432,19.3801718621156));
#29212=CARTESIAN_POINT('Ctrl Pts',(54.9698555359257,22.9945868638877,19.3791170211022));
#29213=CARTESIAN_POINT('Ctrl Pts',(54.9921299514766,22.9947441605632,19.3776677986508));
#29214=CARTESIAN_POINT('Ctrl Pts',(54.9983462787192,22.9947590008506,19.3772648817731));
#29215=CARTESIAN_POINT('Ctrl Pts',(55.0088813151271,22.9947349035656,19.3765847534222));
#29216=CARTESIAN_POINT('Ctrl Pts',(55.0131999822727,22.9947110003732,19.3763067179034));
#29217=CARTESIAN_POINT('Ctrl Pts',(55.0214688473508,22.9946383774056,19.3757758886985));
#29218=CARTESIAN_POINT('Ctrl Pts',(55.0254190081611,22.9945919489241,19.3755229643999));
#29219=CARTESIAN_POINT('Ctrl Pts',(55.0348448988605,22.9944531548722,19.3749209568026));
#29220=CARTESIAN_POINT('Ctrl Pts',(55.0403204729803,22.9943499730766,19.3745724711733));
#29221=CARTESIAN_POINT('Ctrl Pts',(55.059856266311,22.9939013505279,19.3733332932094));
#29222=CARTESIAN_POINT('Ctrl Pts',(55.0739135629932,22.9934297529035,19.3724492966085));
#29223=CARTESIAN_POINT('Ctrl Pts',(55.1134988303262,22.9916824086026,19.3699786420784));
#29224=CARTESIAN_POINT('Ctrl Pts',(55.138997925654,22.9900651497633,19.3684090424697));
#29225=CARTESIAN_POINT('Ctrl Pts',(55.1644484414294,22.9879598267096,19.3668580791575));
#29226=CARTESIAN_POINT('Ctrl Pts',(55.1644482551197,22.9879598421216,19.2088565303878));
#29227=CARTESIAN_POINT('Ctrl Pts',(55.1164235541647,22.9919325472575,19.2120757121755));
#29228=CARTESIAN_POINT('Ctrl Pts',(55.0682598856658,22.9941646009509,19.2153436145953));
#29229=CARTESIAN_POINT('Ctrl Pts',(54.8745044393767,22.9961123335879,19.2286277370617));
#29230=CARTESIAN_POINT('Ctrl Pts',(54.7292455990042,22.9816412960441,19.2389382050322));
#29231=CARTESIAN_POINT('Ctrl Pts',(54.5383242544354,22.941222362976,19.2522759805422));
#29232=CARTESIAN_POINT('Ctrl Pts',(54.490185009616,22.9291392781345,19.2556155999308));
#29233=CARTESIAN_POINT('Ctrl Pts',(54.433833685962,22.9127377060894,19.259459113372));
#29234=CARTESIAN_POINT('Ctrl Pts',(54.4251422512942,22.9101435557911,19.2600500342616));
#29235=CARTESIAN_POINT('Ctrl Pts',(54.4117454702894,22.9060452687648,19.2609576191734));
#29236=CARTESIAN_POINT('Ctrl Pts',(54.4070276443249,22.9045828270238,19.2612766105901));
#29237=CARTESIAN_POINT('Ctrl Pts',(54.3983247978874,22.9018496280869,19.2618638273113));
#29238=CARTESIAN_POINT('Ctrl Pts',(54.394338365156,22.9005838685347,19.2621323278565));
#29239=CARTESIAN_POINT('Ctrl Pts',(54.3853229523286,22.8976900771953,19.2627384815896));
#29240=CARTESIAN_POINT('Ctrl Pts',(54.3802964521158,22.896054592123,19.2630756941362));
#29241=CARTESIAN_POINT('Ctrl Pts',(54.3673156402131,22.8917738579905,19.2639447506841));
#29242=CARTESIAN_POINT('Ctrl Pts',(54.3593712999462,22.8890983837241,19.2644748792226));
#29243=CARTESIAN_POINT('Ctrl Pts',(54.3087899700228,22.8717079563113,19.267840481561));
#29244=CARTESIAN_POINT('Ctrl Pts',(54.2666419600412,22.855599273756,19.2706008833762));
#29245=CARTESIAN_POINT('Ctrl Pts',(54.2036781179509,22.8290538877672,19.2747087804833));
#29246=CARTESIAN_POINT('Ctrl Pts',(54.1824417261714,22.8196607363434,19.2760914732854));
#29247=CARTESIAN_POINT('Ctrl Pts',(54.0052082832568,22.7375386556203,19.287645036104));
#29248=CARTESIAN_POINT('Ctrl Pts',(53.8590674237203,22.6452742426492,19.2973325736992));
#29249=CARTESIAN_POINT('Ctrl Pts',(53.7005386125679,22.5137940129388,19.3097310430515));
#29250=CARTESIAN_POINT('Ctrl Pts',(53.675051928234,22.4915376723493,19.3117888414203));
#29251=CARTESIAN_POINT('Ctrl Pts',(53.6321441004869,22.4521003878389,19.3153775061418));
#29252=CARTESIAN_POINT('Ctrl Pts',(53.6144500044582,22.4352269599802,19.3168959022713));
#29253=CARTESIAN_POINT('Ctrl Pts',(53.5896577241284,22.4106987554048,19.3190819021862));
#29254=CARTESIAN_POINT('Ctrl Pts',(53.5823021147227,22.4033064572881,19.3197380544933));
#29255=CARTESIAN_POINT('Ctrl Pts',(53.5696699360315,22.3904105851689,19.3208783377645));
#29256=CARTESIAN_POINT('Ctrl Pts',(53.5643662833939,22.3849337588327,19.321361270751));
#29257=CARTESIAN_POINT('Ctrl Pts',(53.5542360562668,22.3743520421015,19.3222918543878));
#29258=CARTESIAN_POINT('Ctrl Pts',(53.5494047897019,22.3692517848848,19.3227392916359));
#29259=CARTESIAN_POINT('Ctrl Pts',(53.5380750332793,22.3571639583152,19.3237972382723));
#29260=CARTESIAN_POINT('Ctrl Pts',(53.531599587864,22.3501551179287,19.3244087188796));
#29261=CARTESIAN_POINT('Ctrl Pts',(53.5091619929107,22.3255169476345,19.3265517176119));
#29262=CARTESIAN_POINT('Ctrl Pts',(53.4934655467442,22.3076494185639,19.3280942903949));
#29263=CARTESIAN_POINT('Ctrl Pts',(53.3821769886106,22.1763039006498,19.339356246757));
#29264=CARTESIAN_POINT('Ctrl Pts',(53.2992079854051,22.0527739587075,19.3495891113861));
#29265=CARTESIAN_POINT('Ctrl Pts',(53.1750738120978,21.8143620607659,19.3683360480522));
#29266=CARTESIAN_POINT('Ctrl Pts',(53.1292260147525,21.7026747310107,19.3767583772891));
#29267=CARTESIAN_POINT('Ctrl Pts',(53.0899288958268,21.5751721234695,19.3855546121299));
#29268=CARTESIAN_POINT('Ctrl Pts',(53.0862423046888,21.5627842386849,19.3864008089817));
#29269=CARTESIAN_POINT('Ctrl Pts',(53.0811043915696,21.5448850006598,19.3876105057389));
#29270=CARTESIAN_POINT('Ctrl Pts',(53.0795559647117,21.5394021962001,19.3879793094464));
#29271=CARTESIAN_POINT('Ctrl Pts',(53.0768994922329,21.5298394770684,19.3886194243245));
#29272=CARTESIAN_POINT('Ctrl Pts',(53.0757808965114,21.5257625676637,19.3888913375845));
#29273=CARTESIAN_POINT('Ctrl Pts',(53.0734497681459,21.5171592826609,19.3894630285431));
#29274=CARTESIAN_POINT('Ctrl Pts',(53.0722402196731,21.5126321780285,19.3897626344889));
#29275=CARTESIAN_POINT('Ctrl Pts',(53.0690312899238,21.5004498001904,19.3905656931775));
#29276=CARTESIAN_POINT('Ctrl Pts',(53.0670614579455,21.4927867281508,19.3910674749642));
#29277=CARTESIAN_POINT('Ctrl Pts',(53.0584401785665,21.4584008689281,19.3933048578202));
#29278=CARTESIAN_POINT('Ctrl Pts',(53.0522965714095,21.431552348586,19.3950134281741));
#29279=CARTESIAN_POINT('Ctrl Pts',(53.0192661032615,21.2720845587933,19.4049820283951));
#29280=CARTESIAN_POINT('Ctrl Pts',(53.0053715179969,21.1371217686103,19.4127076039949));
#29281=CARTESIAN_POINT('Ctrl Pts',(53.0052400231811,20.9897047796908,19.4212811242379));
#29282=CARTESIAN_POINT('Ctrl Pts',(53.0053388864299,20.9776304700278,19.4219841569368));
#29283=CARTESIAN_POINT('Ctrl Pts',(53.0074951688973,20.8527658903822,19.429267747121));
#29284=CARTESIAN_POINT('Ctrl Pts',(53.0190067377703,20.740357836622,19.4359529339334));
#29285=CARTESIAN_POINT('Ctrl Pts',(53.0428354453693,20.6142860386737,19.4439164798049));
#29286=CARTESIAN_POINT('Ctrl Pts',(53.0458951129595,20.5990730452447,19.4448849878315));
#29287=CARTESIAN_POINT('Ctrl Pts',(53.0511423179492,20.5744718761667,19.4464641469683));
#29288=CARTESIAN_POINT('Ctrl Pts',(53.053221000515,20.5650609571702,19.4470713303533));
#29289=CARTESIAN_POINT('Ctrl Pts',(53.0570392923982,20.5483501792133,19.4481551599258));
#29290=CARTESIAN_POINT('Ctrl Pts',(53.0587520607387,20.5410443292631,19.4486309379635));
#29291=CARTESIAN_POINT('Ctrl Pts',(53.062445683413,20.5256797513961,19.4496356802081));
#29292=CARTESIAN_POINT('Ctrl Pts',(53.0644356816222,20.5176233899194,19.4501649305873));
#29293=CARTESIAN_POINT('Ctrl Pts',(53.0698347957964,20.4963369153628,19.4515698360714));
#29294=CARTESIAN_POINT('Ctrl Pts',(53.073329615684,20.4831291910576,19.4524482390299));
#29295=CARTESIAN_POINT('Ctrl Pts',(53.0904968011746,20.4208450125265,19.4566230466793));
#29296=CARTESIAN_POINT('Ctrl Pts',(53.1059092393993,20.3722720515927,19.4599753212668));
#29297=CARTESIAN_POINT('Ctrl Pts',(53.180796879,20.1642486584671,19.4747661500816));
#29298=CARTESIAN_POINT('Ctrl Pts',(53.2586757381836,20.0121974587063,19.4867880933559));
#29299=CARTESIAN_POINT('Ctrl Pts',(53.3938778456414,19.8150294730267,19.5033030612794));
#29300=CARTESIAN_POINT('Ctrl Pts',(53.4358067592171,19.7602076220886,19.5080000140803));
#29301=CARTESIAN_POINT('Ctrl Pts',(53.4870892855641,19.6999106561882,19.5131958264936));
#29302=CARTESIAN_POINT('Ctrl Pts',(53.4937419824709,19.6922087602041,19.513860061296));
#29303=CARTESIAN_POINT('Ctrl Pts',(53.5039082788993,19.6806196263997,19.5148599504606));
#29304=CARTESIAN_POINT('Ctrl Pts',(53.5073786077768,19.6766948994329,19.5151986403122));
#29305=CARTESIAN_POINT('Ctrl Pts',(53.513645543789,19.6696634016772,19.515805489465));
#29306=CARTESIAN_POINT('Ctrl Pts',(53.5164364759301,19.6665517237775,19.5160740557362));
#29307=CARTESIAN_POINT('Ctrl Pts',(53.5225719554495,19.6597542369672,19.5166607704125));
#29308=CARTESIAN_POINT('Ctrl Pts',(53.5259205168586,19.6560721705251,19.5169786109325));
#29309=CARTESIAN_POINT('Ctrl Pts',(53.535529347177,19.6455854542032,19.5178840520559));
#29310=CARTESIAN_POINT('Ctrl Pts',(53.5418232935969,19.6388116384558,19.5184691753026));
#29311=CARTESIAN_POINT('Ctrl Pts',(53.5849303019189,19.5930601528613,19.5224250037372));
#29312=CARTESIAN_POINT('Ctrl Pts',(53.6232583050245,19.5555328261958,19.5256888725022));
#29313=CARTESIAN_POINT('Ctrl Pts',(53.798407688852,19.3973568163892,19.5397852195365));
#29314=CARTESIAN_POINT('Ctrl Pts',(53.9498845304327,19.2942582737765,19.5499850027547));
#29315=CARTESIAN_POINT('Ctrl Pts',(54.1617773051667,19.1891045072329,19.5641852042072));
#29316=CARTESIAN_POINT('Ctrl Pts',(54.2112390945761,19.1670201268651,19.5674883514007));
#29317=CARTESIAN_POINT('Ctrl Pts',(54.2749009167004,19.1416496814903,19.5717564531704));
#29318=CARTESIAN_POINT('Ctrl Pts',(54.288323927706,19.1364679402001,19.572657230165));
#29319=CARTESIAN_POINT('Ctrl Pts',(54.3098017083296,19.128442675443,19.5741004146536));
#29320=CARTESIAN_POINT('Ctrl Pts',(54.3178208802088,19.125504829087,19.5746396694983));
#29321=CARTESIAN_POINT('Ctrl Pts',(54.3328843918502,19.1200957325136,19.5756535073451));
#29322=CARTESIAN_POINT('Ctrl Pts',(54.3399242398537,19.1176123465302,19.5761276772201));
#29323=CARTESIAN_POINT('Ctrl Pts',(54.3557154848138,19.1121412823444,19.5771921778424));
#29324=CARTESIAN_POINT('Ctrl Pts',(54.3644740064394,19.1091748412168,19.5777831986893));
#29325=CARTESIAN_POINT('Ctrl Pts',(54.390439946614,19.1005811780775,19.579537314554));
#29326=CARTESIAN_POINT('Ctrl Pts',(54.4077033284704,19.0951273174334,19.5807060593448));
#29327=CARTESIAN_POINT('Ctrl Pts',(54.5437218857599,19.0541839786941,19.5899369008179));
#29328=CARTESIAN_POINT('Ctrl Pts',(54.6654553813722,19.0296041974743,19.5983565985381));
#29329=CARTESIAN_POINT('Ctrl Pts',(54.9241372785108,19.0020424536455,19.6164096001258));
#29330=CARTESIAN_POINT('Ctrl Pts',(55.0607383076031,19.0015247788187,19.6260344543267));
#29331=CARTESIAN_POINT('Ctrl Pts',(55.2225932696649,19.0175327654814,19.6369451841208));
#29332=CARTESIAN_POINT('Ctrl Pts',(55.2488045419604,19.020651480542,19.6386954191261));
#29333=CARTESIAN_POINT('Ctrl Pts',(55.2826620000217,19.025363218265,19.6409280968758));
#29334=CARTESIAN_POINT('Ctrl Pts',(55.2903701386604,19.0264819703274,19.6414345004279));
#29335=CARTESIAN_POINT('Ctrl Pts',(55.3026778258275,19.0283419674287,19.642239834126));
#29336=CARTESIAN_POINT('Ctrl Pts',(55.307281577987,19.0290542126776,19.6425403456731));
#29337=CARTESIAN_POINT('Ctrl Pts',(55.316067037083,19.0304449394086,19.6431123749036));
#29338=CARTESIAN_POINT('Ctrl Pts',(55.3202490940301,19.0311206165215,19.6433840395558));
#29339=CARTESIAN_POINT('Ctrl Pts',(55.3301076813416,19.0327456685199,19.6440230075638));
#29340=CARTESIAN_POINT('Ctrl Pts',(55.3357823608304,19.0337063052159,19.6443896775027));
#29341=CARTESIAN_POINT('Ctrl Pts',(55.354509903229,19.0369600302397,19.6455962784053));
#29342=CARTESIAN_POINT('Ctrl Pts',(55.3675444013262,19.0393586942867,19.6464304885923));
#29343=CARTESIAN_POINT('Ctrl Pts',(55.4386234464613,19.0531727326352,19.6509537413615));
#29344=CARTESIAN_POINT('Ctrl Pts',(55.4961675879103,19.0670369808496,19.6545216768063));
#29345=CARTESIAN_POINT('Ctrl Pts',(55.6907079419305,19.1231708011607,19.6665196744245));
#29346=CARTESIAN_POINT('Ctrl Pts',(55.8237199279675,19.1776241095011,19.6746406379077));
#29347=CARTESIAN_POINT('Ctrl Pts',(56.0186852213769,19.2831853301941,19.6877531701362));
#29348=CARTESIAN_POINT('Ctrl Pts',(56.0853503538962,19.324534492639,19.6924771274866));
#29349=CARTESIAN_POINT('Ctrl Pts',(56.1613242034307,19.3780979286924,19.6982541700892));
#29350=CARTESIAN_POINT('Ctrl Pts',(56.1731503187056,19.3866313048789,19.6991652478416));
#29351=CARTESIAN_POINT('Ctrl Pts',(56.1924076933736,19.4008505449274,19.7006689605137));
#29352=CARTESIAN_POINT('Ctrl Pts',(56.1998945291834,19.4064604802815,19.701258658233));
#29353=CARTESIAN_POINT('Ctrl Pts',(56.2132909750004,19.4166464602075,19.7023231684609));
#29354=CARTESIAN_POINT('Ctrl Pts',(56.2192148883148,19.4212034723824,19.7027972282011));
#29355=CARTESIAN_POINT('Ctrl Pts',(56.2317941480738,19.4309931763722,19.7038110962697));
#29356=CARTESIAN_POINT('Ctrl Pts',(56.2384420535122,19.4362351480266,19.7043512671971));
#29357=CARTESIAN_POINT('Ctrl Pts',(56.256325265804,19.4505218857369,19.7058163277697));
#29358=CARTESIAN_POINT('Ctrl Pts',(56.267495997736,19.4596463140994,19.7067443988404));
#29359=CARTESIAN_POINT('Ctrl Pts',(56.3250977554175,19.5077471845461,19.7115987559919));
#29360=CARTESIAN_POINT('Ctrl Pts',(56.3698288833484,19.5487005617066,19.7156054870268));
#29361=CARTESIAN_POINT('Ctrl Pts',(56.4625974085047,19.641748762918,19.7244542463367));
#29362=CARTESIAN_POINT('Ctrl Pts',(56.5098648005875,19.6944945810795,19.7293180844682));
#29363=CARTESIAN_POINT('Ctrl Pts',(56.6411803330977,19.8577223324104,19.7438601814206));
#29364=CARTESIAN_POINT('Ctrl Pts',(56.7166253647752,19.9745869600304,19.7536621172669));
#29365=CARTESIAN_POINT('Ctrl Pts',(56.7899214054424,20.1192290840442,19.764504966925));
#29366=CARTESIAN_POINT('Ctrl Pts',(56.8001393510069,20.1403055911879,19.7660544001512));
#29367=CARTESIAN_POINT('Ctrl Pts',(56.8131133997085,20.1683132894064,19.7680688623158));
#29368=CARTESIAN_POINT('Ctrl Pts',(56.8162047712208,20.1750859329538,19.7685526011871));
#29369=CARTESIAN_POINT('Ctrl Pts',(56.8211374434818,20.1860546894093,19.769330406236));
#29370=CARTESIAN_POINT('Ctrl Pts',(56.8230022942124,20.19024003988,19.7696258736925));
#29371=CARTESIAN_POINT('Ctrl Pts',(56.8265756783595,20.1983348232381,19.7701947325401));
#29372=CARTESIAN_POINT('Ctrl Pts',(56.8282861015554,20.2022433356164,19.7704682319084));
#29373=CARTESIAN_POINT('Ctrl Pts',(56.8323473828459,20.2116054927032,19.7711206168165));
#29374=CARTESIAN_POINT('Ctrl Pts',(56.8346864747123,20.2170642604663,19.7714987912119));
#29375=CARTESIAN_POINT('Ctrl Pts',(56.8425846236466,20.2357260401746,19.7727843913507));
#29376=CARTESIAN_POINT('Ctrl Pts',(56.8480259710898,20.2489788158847,19.7736850170145));
#29377=CARTESIAN_POINT('Ctrl Pts',(56.8788412980894,20.3263950835175,19.7788809541708));
#29378=CARTESIAN_POINT('Ctrl Pts',(56.9010179035226,20.3917885517414,19.7830122320168));
#29379=CARTESIAN_POINT('Ctrl Pts',(56.9741705522803,20.6509936759879,19.7988689494135));
#29380=CARTESIAN_POINT('Ctrl Pts',(56.9992281490352,20.8508609233056,19.810123257884));
#29381=CARTESIAN_POINT('Ctrl Pts',(56.9935140332236,21.073779096414,19.8238797470968));
#29382=CARTESIAN_POINT('Ctrl Pts',(56.9925467620333,21.096430760457,19.8252895498713));
#29383=CARTESIAN_POINT('Ctrl Pts',(56.9906500318475,21.1281521353835,19.8272825816398));
#29384=CARTESIAN_POINT('Ctrl Pts',(56.9900441448628,21.1372399948239,19.8278557222121));
#29385=CARTESIAN_POINT('Ctrl Pts',(56.988817645199,21.1539151901534,19.8289114713054));
#29386=CARTESIAN_POINT('Ctrl Pts',(56.9882157936343,21.1615037675762,19.8293934846216));
#29387=CARTESIAN_POINT('Ctrl Pts',(56.9869047567751,21.1769144917045,19.8303756008559));
#29388=CARTESIAN_POINT('Ctrl Pts',(56.9861927804803,21.1847362599377,19.8308757831142));
#29389=CARTESIAN_POINT('Ctrl Pts',(56.9843137250247,21.2041113491262,19.8321190959192));
#29390=CARTESIAN_POINT('Ctrl Pts',(56.9830919314014,21.2156589537308,19.8328639314231));
#29391=CARTESIAN_POINT('Ctrl Pts',(56.9781005907492,21.2591972566589,19.835687021727));
#29392=CARTESIAN_POINT('Ctrl Pts',(56.9736573347616,21.2911042584922,19.8377862612634));
#29393=CARTESIAN_POINT('Ctrl Pts',(56.9605518089326,21.3710002985612,19.8431223992178));
#29394=CARTESIAN_POINT('Ctrl Pts',(56.9508992139678,21.4188033403561,19.8463882742498));
#29395=CARTESIAN_POINT('Ctrl Pts',(56.9156101561332,21.5656138861686,19.8566399746164));
#29396=CARTESIAN_POINT('Ctrl Pts',(56.8841081750391,21.6630343102633,19.8637692015355));
#29397=CARTESIAN_POINT('Ctrl Pts',(56.8064411892692,21.8522068062502,19.8780297204591));
#29398=CARTESIAN_POINT('Ctrl Pts',(56.7603782294296,21.9436943121763,19.8851386057246));
#29399=CARTESIAN_POINT('Ctrl Pts',(56.6992634622289,22.0448851041563,19.8929700113413));
#29400=CARTESIAN_POINT('Ctrl Pts',(56.690866785817,22.0584189841168,19.8940165535413));
#29401=CARTESIAN_POINT('Ctrl Pts',(56.6788807662267,22.0772314658685,19.8954684742823));
#29402=CARTESIAN_POINT('Ctrl Pts',(56.6754270788242,22.0825951988191,19.8958821157221));
#29403=CARTESIAN_POINT('Ctrl Pts',(56.6698110200541,22.0912259468111,19.8965470609926));
#29404=CARTESIAN_POINT('Ctrl Pts',(56.6676646866509,22.0945032678046,19.8967994075373));
#29405=CARTESIAN_POINT('Ctrl Pts',(56.6631150393526,22.1014058499247,19.8973305368456));
#29406=CARTESIAN_POINT('Ctrl Pts',(56.6607094990114,22.1050296108641,19.8976091625521));
#29407=CARTESIAN_POINT('Ctrl Pts',(56.6547491547136,22.1139449871829,19.8982942096986));
#29408=CARTESIAN_POINT('Ctrl Pts',(56.6511807632165,22.1192275413642,19.8986997283771));
#29409=CARTESIAN_POINT('Ctrl Pts',(56.6379319843243,22.1386394157245,19.9001888235182));
#29410=CARTESIAN_POINT('Ctrl Pts',(56.6280947391582,22.152661472925,19.9012623618939));
#29411=CARTESIAN_POINT('Ctrl Pts',(56.559770566702,22.2474309105063,19.9085164198208));
#29412=CARTESIAN_POINT('Ctrl Pts',(56.4954742589598,22.3238314791382,19.9143606224698));
#29413=CARTESIAN_POINT('Ctrl Pts',(56.3103674702416,22.5130004445966,19.9297520586874));
#29414=CARTESIAN_POINT('Ctrl Pts',(56.1808476884012,22.6161144661068,19.939213404145));
#29415=CARTESIAN_POINT('Ctrl Pts',(56.0203583561287,22.7141857284793,19.9508104067281));
#29416=CARTESIAN_POINT('Ctrl Pts',(56.0003890583831,22.7259158580431,19.9522500019627));
#29417=CARTESIAN_POINT('Ctrl Pts',(55.9722204093258,22.7418092370725,19.9542781309132));
#29418=CARTESIAN_POINT('Ctrl Pts',(55.9641891513502,22.7462677969175,19.9548560877129));
#29419=CARTESIAN_POINT('Ctrl Pts',(55.9494291120574,22.7543289814693,19.9559178857759));
#29420=CARTESIAN_POINT('Ctrl Pts',(55.9427098694798,22.7579487800826,19.956401105518));
#29421=CARTESIAN_POINT('Ctrl Pts',(55.9290570262866,22.7652030725092,19.957382749616));
#29422=CARTESIAN_POINT('Ctrl Pts',(55.9221224782036,22.7688354863034,19.9578812367055));
#29423=CARTESIAN_POINT('Ctrl Pts',(55.904959673297,22.7776972503598,19.9591148034006));
#29424=CARTESIAN_POINT('Ctrl Pts',(55.8947073837488,22.7828791917985,19.9598515301343));
#29425=CARTESIAN_POINT('Ctrl Pts',(55.8563444936526,22.8018551943899,19.9626080957199));
#29426=CARTESIAN_POINT('Ctrl Pts',(55.8279563185152,22.8150747046868,19.9646476619746));
#29427=CARTESIAN_POINT('Ctrl Pts',(55.7562817474945,22.8464200269799,19.969799423453));
#29428=CARTESIAN_POINT('Ctrl Pts',(55.7126465679376,22.8636961382306,19.9729381041316));
#29429=CARTESIAN_POINT('Ctrl Pts',(55.5058007313037,22.9372642745294,19.9878199946336));
#29430=CARTESIAN_POINT('Ctrl Pts',(55.336389978457,22.9737364497894,20.000100773204));
#29431=CARTESIAN_POINT('Ctrl Pts',(55.1644483497948,22.9879598342899,20.0118645378774));
#29432=CARTESIAN_POINT('Origin',(55.,21.,6.22095488139522));
#29433=CARTESIAN_POINT('',(55.164448351653,22.9879598341362,20.9703924394033));
#29434=CARTESIAN_POINT('',(55.1644479523467,22.9879598671676,20.810886410834));
#29435=CARTESIAN_POINT('',(55.1644483516311,22.987959834138,6.22095488139522));
#29436=CARTESIAN_POINT('Ctrl Pts',(55.164448351653,22.9879598341362,20.9703924394033));
#29437=CARTESIAN_POINT('Ctrl Pts',(55.1674230284317,22.9877137624175,20.9702048747357));
#29438=CARTESIAN_POINT('Ctrl Pts',(55.1703971503059,22.9874610141927,20.9700171029999));
#29439=CARTESIAN_POINT('Ctrl Pts',(55.1816941270429,22.986475424851,20.9693029362251));
#29440=CARTESIAN_POINT('Ctrl Pts',(55.1900128099936,22.9856969803913,20.9687751308099));
#29441=CARTESIAN_POINT('Ctrl Pts',(55.2057839210713,22.9841211435724,20.9677707359783));
#29442=CARTESIAN_POINT('Ctrl Pts',(55.2132372426693,22.9833339633978,20.9672944756293));
#29443=CARTESIAN_POINT('Ctrl Pts',(55.2301702614005,22.9814490358388,20.9662087748862));
#29444=CARTESIAN_POINT('Ctrl Pts',(55.2396468165603,22.980325233122,20.9655985246649));
#29445=CARTESIAN_POINT('Ctrl Pts',(55.2641928228773,22.9772356114773,20.9640108576897));
#29446=CARTESIAN_POINT('Ctrl Pts',(55.2792482977141,22.9751655317869,20.9630301853784));
#29447=CARTESIAN_POINT('Ctrl Pts',(55.3896647822656,22.9586959759476,20.9557860260432));
#29448=CARTESIAN_POINT('Ctrl Pts',(55.4838793385295,22.9375717834717,20.9493101660023));
#29449=CARTESIAN_POINT('Ctrl Pts',(55.7110793384366,22.8690228625102,20.9330034180314));
#29450=CARTESIAN_POINT('Ctrl Pts',(55.8412732870271,22.8141491572639,20.9230297150245));
#29451=CARTESIAN_POINT('Ctrl Pts',(56.0074579539029,22.7223396428782,20.910059195898));
#29452=CARTESIAN_POINT('Ctrl Pts',(56.0494372138678,22.6970880352632,20.9067641324717));
#29453=CARTESIAN_POINT('Ctrl Pts',(56.098019053344,22.6653718720301,20.9029648095425));
#29454=CARTESIAN_POINT('Ctrl Pts',(56.1055565950768,22.660377648669,20.9023757618624));
#29455=CARTESIAN_POINT('Ctrl Pts',(56.1171545444495,22.6525790845585,20.9014703756665));
#29456=CARTESIAN_POINT('Ctrl Pts',(56.1212388260881,22.6498107173418,20.9011517279255));
#29457=CARTESIAN_POINT('Ctrl Pts',(56.1287678509004,22.6446665956117,20.9005647409862));
#29458=CARTESIAN_POINT('Ctrl Pts',(56.1322153697563,22.6422951710914,20.9002961294141));
#29459=CARTESIAN_POINT('Ctrl Pts',(56.1400095241046,22.6368976438306,20.8996892110244));
#29460=CARTESIAN_POINT('Ctrl Pts',(56.144351579208,22.633865072811,20.8993513487972));
#29461=CARTESIAN_POINT('Ctrl Pts',(56.1572175527002,22.6248027912319,20.8983507955241));
#29462=CARTESIAN_POINT('Ctrl Pts',(56.1657064220464,22.6187233004501,20.8976913840031));
#29463=CARTESIAN_POINT('Ctrl Pts',(56.2464132023215,22.559959199221,20.8914251855198));
#29464=CARTESIAN_POINT('Ctrl Pts',(56.3150703335734,22.5025354666116,20.8861161382822));
#29465=CARTESIAN_POINT('Ctrl Pts',(56.4665497277803,22.3574741599096,20.8738493725367));
#29466=CARTESIAN_POINT('Ctrl Pts',(56.5457399134418,22.2665671157769,20.8669703483775));
#29467=CARTESIAN_POINT('Ctrl Pts',(56.6459214280707,22.1280657288151,20.85684456982));
#29468=CARTESIAN_POINT('Ctrl Pts',(56.6740132769748,22.0859413573564,20.8538086046394));
#29469=CARTESIAN_POINT('Ctrl Pts',(56.7120818784239,22.0238634975641,20.8493609680054));
#29470=CARTESIAN_POINT('Ctrl Pts',(56.7233749312408,22.004738577009,20.8479942972763));
#29471=CARTESIAN_POINT('Ctrl Pts',(56.7430277870541,21.9701497536569,20.8455261127801));
#29472=CARTESIAN_POINT('Ctrl Pts',(56.7515070562206,21.954756205564,20.8444288937728));
#29473=CARTESIAN_POINT('Ctrl Pts',(56.7640854927739,21.9311892845362,20.8427500044087));
#29474=CARTESIAN_POINT('Ctrl Pts',(56.768333830923,21.9230961853327,20.8421736211191));
#29475=CARTESIAN_POINT('Ctrl Pts',(56.7756187688728,21.9089834996872,20.8411686811578));
#29476=CARTESIAN_POINT('Ctrl Pts',(56.7786807745463,21.9029771400828,20.8407410265619));
#29477=CARTESIAN_POINT('Ctrl Pts',(56.7854781175839,21.8894748980991,20.8397797104226));
#29478=CARTESIAN_POINT('Ctrl Pts',(56.7891967967909,21.8819708167198,20.839245476425));
#29479=CARTESIAN_POINT('Ctrl Pts',(56.7990062384634,21.8618585601611,20.8378136015503));
#29480=CARTESIAN_POINT('Ctrl Pts',(56.80501159718,21.8492094801694,20.836913023009));
#29481=CARTESIAN_POINT('Ctrl Pts',(56.8312572660477,21.7923918759971,20.8328668456321));
#29482=CARTESIAN_POINT('Ctrl Pts',(56.8500115510239,21.747559124156,20.8296710939062));
#29483=CARTESIAN_POINT('Ctrl Pts',(56.876626825179,21.6767795062985,20.8246176764712));
#29484=CARTESIAN_POINT('Ctrl Pts',(56.8856281868899,21.6512794933545,20.8227956035008));
#29485=CARTESIAN_POINT('Ctrl Pts',(56.9494568421169,21.4580292435766,20.8089809449915));
#29486=CARTESIAN_POINT('Ctrl Pts',(56.9823164063856,21.2838734544756,20.7964017044736));
#29487=CARTESIAN_POINT('Ctrl Pts',(56.9932913339742,21.0808613355804,20.7825988310038));
#29488=CARTESIAN_POINT('Ctrl Pts',(56.9941994478126,21.0540148703273,20.7807926985989));
#29489=CARTESIAN_POINT('Ctrl Pts',(56.9948046623135,21.009564387303,20.7778423363127));
#29490=CARTESIAN_POINT('Ctrl Pts',(56.9948114365766,20.9919686815038,20.7766848374015));
#29491=CARTESIAN_POINT('Ctrl Pts',(56.9945026232366,20.9679319188483,20.7751198893588));
#29492=CARTESIAN_POINT('Ctrl Pts',(56.9943886368266,20.9614896896558,20.7747020555433));
#29493=CARTESIAN_POINT('Ctrl Pts',(56.9941450829581,20.9506846997236,20.7740040644679));
#29494=CARTESIAN_POINT('Ctrl Pts',(56.9940324086913,20.9463216532779,20.7737229836803));
#29495=CARTESIAN_POINT('Ctrl Pts',(56.9937917295154,20.9380535137136,20.7731918239267));
#29496=CARTESIAN_POINT('Ctrl Pts',(56.9936665700738,20.9341483799728,20.7729415838163));
#29497=CARTESIAN_POINT('Ctrl Pts',(56.9933090045446,20.9239297108976,20.7722883704098));
#29498=CARTESIAN_POINT('Ctrl Pts',(56.9930580745282,20.9176168060753,20.771886422586));
#29499=CARTESIAN_POINT('Ctrl Pts',(56.9920856822456,20.8957693146422,20.7705005692399));
#29500=CARTESIAN_POINT('Ctrl Pts',(56.9912125346022,20.8802415833859,20.7695246907944));
#29501=CARTESIAN_POINT('Ctrl Pts',(56.9816277673975,20.7392309537141,20.7607323535998));
#29502=CARTESIAN_POINT('Ctrl Pts',(56.9612455081957,20.6148064370411,20.7534658079392));
#29503=CARTESIAN_POINT('Ctrl Pts',(56.8912471377406,20.3483818893744,20.7374846252002));
#29504=CARTESIAN_POINT('Ctrl Pts',(56.8370611430115,20.2084063475262,20.728781679857));
#29505=CARTESIAN_POINT('Ctrl Pts',(56.7597290742827,20.0604894283604,20.7184225061462));
#29506=CARTESIAN_POINT('Ctrl Pts',(56.7515194567132,20.0452717180328,20.7173427181159));
#29507=CARTESIAN_POINT('Ctrl Pts',(56.738697742356,20.0222269171076,20.7156850963962));
#29508=CARTESIAN_POINT('Ctrl Pts',(56.7342281513733,20.0143211702162,20.7151123437113));
#29509=CARTESIAN_POINT('Ctrl Pts',(56.7259905209259,19.9999800538894,20.7140657564104));
#29510=CARTESIAN_POINT('Ctrl Pts',(56.7222400641669,19.9935347348997,20.7135925619177));
#29511=CARTESIAN_POINT('Ctrl Pts',(56.7140499061264,19.9796394295651,20.7125662011117));
#29512=CARTESIAN_POINT('Ctrl Pts',(56.709597597621,19.9721970886018,20.7120125833335));
#29513=CARTESIAN_POINT('Ctrl Pts',(56.6973344622424,19.9519985627831,20.7104992690216));
#29514=CARTESIAN_POINT('Ctrl Pts',(56.689428587873,19.9393010250909,20.7095361082156));
#29515=CARTESIAN_POINT('Ctrl Pts',(56.6481878988791,19.8746956875284,20.7045734428999));
#29516=CARTESIAN_POINT('Ctrl Pts',(56.6126040650623,19.8242704762318,20.7004909205695));
#29517=CARTESIAN_POINT('Ctrl Pts',(56.4676178674006,19.6378017786085,20.6845618592019));
#29518=CARTESIAN_POINT('Ctrl Pts',(56.3428742196192,19.5146847552323,20.6721602944548));
#29519=CARTESIAN_POINT('Ctrl Pts',(56.1615462750977,19.3774594662395,20.6565862895012));
#29520=CARTESIAN_POINT('Ctrl Pts',(56.1180939983872,19.3472161556225,20.6530171864849));
#29521=CARTESIAN_POINT('Ctrl Pts',(56.0657163263958,19.3137730697115,20.648946281753));
#29522=CARTESIAN_POINT('Ctrl Pts',(56.0579118228645,19.3088657262903,20.6483455344967));
#29523=CARTESIAN_POINT('Ctrl Pts',(56.0458461140064,19.3013952229324,20.647426065082));
#29524=CARTESIAN_POINT('Ctrl Pts',(56.0416090018581,19.2987936717097,20.6471049214531));
#29525=CARTESIAN_POINT('Ctrl Pts',(56.0337904688587,19.2940333195063,20.6465156027183));
#29526=CARTESIAN_POINT('Ctrl Pts',(56.0302120031055,19.2918699470695,20.6462471381438));
#29527=CARTESIAN_POINT('Ctrl Pts',(56.022126734077,19.2870166236971,20.645643381968));
#29528=CARTESIAN_POINT('Ctrl Pts',(56.0176161102669,19.284333202032,20.6453085148042));
#29529=CARTESIAN_POINT('Ctrl Pts',(56.0042936433659,19.2764785384598,20.6443250532595));
#29530=CARTESIAN_POINT('Ctrl Pts',(55.9954524427132,19.2713570654234,20.6436795746621));
#29531=CARTESIAN_POINT('Ctrl Pts',(55.9255935344047,19.2316033645784,20.6386323612639));
#29532=CARTESIAN_POINT('Ctrl Pts',(55.8628193852695,19.2001402744882,20.6344129152759));
#29533=CARTESIAN_POINT('Ctrl Pts',(55.6433143105828,19.1042530800487,20.620274017616));
#29534=CARTESIAN_POINT('Ctrl Pts',(55.4801207465749,19.0564989924778,20.6107261049396));
#29535=CARTESIAN_POINT('Ctrl Pts',(55.2629546702188,19.0220124120218,20.5974824352307));
#29536=CARTESIAN_POINT('Ctrl Pts',(55.2127782967319,19.0159877021967,20.5943922231503));
#29537=CARTESIAN_POINT('Ctrl Pts',(55.1488478241707,19.0107645681261,20.5903922177872));
#29538=CARTESIAN_POINT('Ctrl Pts',(55.1352545862278,19.0097941160572,20.5895381798738));
#29539=CARTESIAN_POINT('Ctrl Pts',(55.1133756637403,19.0084573097662,20.5881574452446));
#29540=CARTESIAN_POINT('Ctrl Pts',(55.1050956238109,19.0080032041589,20.5876335009309));
#29541=CARTESIAN_POINT('Ctrl Pts',(55.0893137710545,19.0072363448163,20.5866320739116));
#29542=CARTESIAN_POINT('Ctrl Pts',(55.0818125368117,19.0069142915034,20.5861548910852));
#29543=CARTESIAN_POINT('Ctrl Pts',(55.0646597454618,19.0062748605324,20.5850609188074));
#29544=CARTESIAN_POINT('Ctrl Pts',(55.0550074029834,19.0059852070202,20.5844432730887));
#29545=CARTESIAN_POINT('Ctrl Pts',(55.0297816716614,19.0054115158649,20.5828236068537));
#29546=CARTESIAN_POINT('Ctrl Pts',(55.0142066330443,19.005239784399,20.5818181104334));
#29547=CARTESIAN_POINT('Ctrl Pts',(54.8755670251517,19.0053348955324,20.5728172585312));
#29548=CARTESIAN_POINT('Ctrl Pts',(54.7527968477784,19.0168073208097,20.5644671001361));
#29549=CARTESIAN_POINT('Ctrl Pts',(54.5174745044657,19.0609930284037,20.5478608836285));
#29550=CARTESIAN_POINT('Ctrl Pts',(54.4051636237486,19.0924493833604,20.5396599905331));
#29551=CARTESIAN_POINT('Ctrl Pts',(54.2528736897793,19.1498709640958,20.528560729112));
#29552=CARTESIAN_POINT('Ctrl Pts',(54.2100902752486,19.1677285765733,20.5254473195951));
#29553=CARTESIAN_POINT('Ctrl Pts',(54.1598644909494,19.19077936269,20.5218293675881));
#29554=CARTESIAN_POINT('Ctrl Pts',(54.1517895058775,19.1945510384253,20.521248871853));
#29555=CARTESIAN_POINT('Ctrl Pts',(54.139308794379,19.2004827645161,20.5203537929136));
#29556=CARTESIAN_POINT('Ctrl Pts',(54.1348854247366,19.2026051059486,20.5200369810864));
#29557=CARTESIAN_POINT('Ctrl Pts',(54.1267015664905,19.2065689475409,20.5194516742339));
#29558=CARTESIAN_POINT('Ctrl Pts',(54.1229390723983,19.2084059545516,20.5191829195049));
#29559=CARTESIAN_POINT('Ctrl Pts',(54.1143971941174,19.2126098143923,20.5185735171007));
#29560=CARTESIAN_POINT('Ctrl Pts',(54.1096215063393,19.2149839930656,20.5182333296135));
#29561=CARTESIAN_POINT('Ctrl Pts',(54.0972266198962,19.2212080901248,20.5173516188828));
#29562=CARTESIAN_POINT('Ctrl Pts',(54.0896224169046,19.2250878622303,20.5168118944855));
#29563=CARTESIAN_POINT('Ctrl Pts',(54.039336206552,19.2511527954617,20.513249162095));
#29564=CARTESIAN_POINT('Ctrl Pts',(53.9974399770341,19.2748287901999,20.5103116558492));
#29565=CARTESIAN_POINT('Ctrl Pts',(53.941344621708,19.3092634803323,20.5063649352237));
#29566=CARTESIAN_POINT('Ctrl Pts',(53.926375630425,19.3187290731782,20.5053103886359));
#29567=CARTESIAN_POINT('Ctrl Pts',(53.7656887926224,19.4233601835461,20.4939536770142));
#29568=CARTESIAN_POINT('Ctrl Pts',(53.6329003794888,19.5370031223853,20.4841682600082));
#29569=CARTESIAN_POINT('Ctrl Pts',(53.4821303526843,19.704720603262,20.4705945041983));
#29570=CARTESIAN_POINT('Ctrl Pts',(53.4492162693372,19.7443144851912,20.4674477287167));
#29571=CARTESIAN_POINT('Ctrl Pts',(53.4095218062548,19.79600886326,20.4633837887107));
#29572=CARTESIAN_POINT('Ctrl Pts',(53.4012841473777,19.806968923359,20.4625246370339));
#29573=CARTESIAN_POINT('Ctrl Pts',(53.3882357586937,19.8247074145035,20.4611376165708));
#29574=CARTESIAN_POINT('Ctrl Pts',(53.3833531787427,19.8314326365131,20.4606125460986));
#29575=CARTESIAN_POINT('Ctrl Pts',(53.374142225133,19.8442879386755,20.4596102698405));
#29576=CARTESIAN_POINT('Ctrl Pts',(53.3698061285429,19.850412329691,20.4591333725194));
#29577=CARTESIAN_POINT('Ctrl Pts',(53.3599888609184,19.8644456773597,20.4580418926502));
#29578=CARTESIAN_POINT('Ctrl Pts',(53.3545301886841,19.8723700737114,20.4574264677949));
#29579=CARTESIAN_POINT('Ctrl Pts',(53.340450359488,19.8931298093583,20.4558164317961));
#29580=CARTESIAN_POINT('Ctrl Pts',(53.3319208587762,19.9060262413924,20.4548184117751));
#29581=CARTESIAN_POINT('Ctrl Pts',(53.2525376226562,20.029139215747,20.4453095200631));
#29582=CARTESIAN_POINT('Ctrl Pts',(53.1925686254404,20.1459651661725,20.4363929075652));
#29583=CARTESIAN_POINT('Ctrl Pts',(53.1040966006011,20.3701682368526,20.4196446705431));
#29584=CARTESIAN_POINT('Ctrl Pts',(53.0722422031285,20.4757015867278,20.4119042718392));
#29585=CARTESIAN_POINT('Ctrl Pts',(53.0398376707431,20.6274100019294,20.4013343876645));
#29586=CARTESIAN_POINT('Ctrl Pts',(53.0319175842728,20.6718049617459,20.3983082367895));
#29587=CARTESIAN_POINT('Ctrl Pts',(53.0242506916948,20.725190089852,20.3947778141092));
#29588=CARTESIAN_POINT('Ctrl Pts',(53.0230513959082,20.7339548163091,20.3942016750867));
#29589=CARTESIAN_POINT('Ctrl Pts',(53.0212794990037,20.7475783857891,20.3933118511797));
#29590=CARTESIAN_POINT('Ctrl Pts',(53.0206664157599,20.75243171461,20.3929959782657));
#29591=CARTESIAN_POINT('Ctrl Pts',(53.0195615352845,20.7614447773959,20.3924115183356));
#29592=CARTESIAN_POINT('Ctrl Pts',(53.0190649894414,20.7656037730739,20.3921426781295));
#29593=CARTESIAN_POINT('Ctrl Pts',(53.0179637055182,20.7750814756494,20.3915319499965));
#29594=CARTESIAN_POINT('Ctrl Pts',(53.0173672742555,20.7804010663618,20.391190530508));
#29595=CARTESIAN_POINT('Ctrl Pts',(53.0158682594814,20.7942749709469,20.3903034921914));
#29596=CARTESIAN_POINT('Ctrl Pts',(53.014999569509,20.8028329425468,20.3897597081598));
#29597=CARTESIAN_POINT('Ctrl Pts',(53.0095102181503,20.8606305249053,20.3861083325675));
#29598=CARTESIAN_POINT('Ctrl Pts',(53.0066663550327,20.9100261099869,20.3830911672217));
#29599=CARTESIAN_POINT('Ctrl Pts',(53.0053965898443,20.9725231609778,20.3793472544449));
#29600=CARTESIAN_POINT('Ctrl Pts',(53.0052595471134,20.9855681999382,20.3785698364135));
#29601=CARTESIAN_POINT('Ctrl Pts',(53.0051605434955,21.1280385974422,20.370114841767));
#29602=CARTESIAN_POINT('Ctrl Pts',(53.0176666334288,21.2571685736435,20.3627516861738));
#29603=CARTESIAN_POINT('Ctrl Pts',(53.0606284182064,21.4760589360895,20.3496536461333));
#29604=CARTESIAN_POINT('Ctrl Pts',(53.0851053900687,21.5665417532498,20.3440526453093));
#29605=CARTESIAN_POINT('Ctrl Pts',(53.1208059723588,21.6692427601496,20.3373003989082));
#29606=CARTESIAN_POINT('Ctrl Pts',(53.1259313573745,21.6834638019527,20.3363565432676));
#29607=CARTESIAN_POINT('Ctrl Pts',(53.1345467272863,21.7065424647017,20.3348096461472));
#29608=CARTESIAN_POINT('Ctrl Pts',(53.1379394274192,21.7154359412877,20.3342098391779));
#29609=CARTESIAN_POINT('Ctrl Pts',(53.1441160321685,21.7312854383,20.3331341078978));
#29610=CARTESIAN_POINT('Ctrl Pts',(53.1468757374519,21.7382507428896,20.3326590023201));
#29611=CARTESIAN_POINT('Ctrl Pts',(53.1528011265525,21.752963429734,20.331650362858));
#29612=CARTESIAN_POINT('Ctrl Pts',(53.1559764523568,21.7607067482283,20.3311165110364));
#29613=CARTESIAN_POINT('Ctrl Pts',(53.1645841243105,21.7813267191913,20.3296867401662));
#29614=CARTESIAN_POINT('Ctrl Pts',(53.1701031472025,21.7941664627037,20.3287878985512));
#29615=CARTESIAN_POINT('Ctrl Pts',(53.1978660935373,21.8569294210491,20.3243512290707));
#29616=CARTESIAN_POINT('Ctrl Pts',(53.2220185390199,21.9059777127488,20.320748646002));
#29617=CARTESIAN_POINT('Ctrl Pts',(53.3456460786204,22.1330046286085,20.3034093914893));
#29618=CARTESIAN_POINT('Ctrl Pts',(53.4699834378642,22.2959986858709,20.2888023758561));
#29619=CARTESIAN_POINT('Ctrl Pts',(53.6414155634742,22.4609721945682,20.2727232123482));
#29620=CARTESIAN_POINT('Ctrl Pts',(53.6666020427726,22.4839951629618,20.270447895774));
#29621=CARTESIAN_POINT('Ctrl Pts',(53.6987390984976,22.5118924555845,20.2676639237699));
#29622=CARTESIAN_POINT('Ctrl Pts',(53.7051449215525,22.5173823061244,20.2671147168241));
#29623=CARTESIAN_POINT('Ctrl Pts',(53.7152897943443,22.5259655284435,20.2662541627227));
#29624=CARTESIAN_POINT('Ctrl Pts',(53.7190055438801,22.5290861032402,20.2659408950456));
#29625=CARTESIAN_POINT('Ctrl Pts',(53.7259231839884,22.5348527885235,20.265361306799));
#29626=CARTESIAN_POINT('Ctrl Pts',(53.7291219247398,22.537502433754,20.2650947367863));
#29627=CARTESIAN_POINT('Ctrl Pts',(53.7364890013257,22.5435661787747,20.2644840499161));
#29628=CARTESIAN_POINT('Ctrl Pts',(53.7406629059793,22.5469733925608,20.264140429536));
#29629=CARTESIAN_POINT('Ctrl Pts',(53.7536007086018,22.5574476283076,20.2630824341896));
#29630=CARTESIAN_POINT('Ctrl Pts',(53.7624108484027,22.5644575463269,20.2623720098396));
#29631=CARTESIAN_POINT('Ctrl Pts',(53.8467941030825,22.6304393881571,20.2556572531532));
#29632=CARTESIAN_POINT('Ctrl Pts',(53.9264770258553,22.6839744214656,20.2499922583744));
#29633=CARTESIAN_POINT('Ctrl Pts',(54.1552643952985,22.814817960271,20.2346174489977));
#29634=CARTESIAN_POINT('Ctrl Pts',(54.3107173179637,22.8793690659443,20.2250608349423));
#29635=CARTESIAN_POINT('Ctrl Pts',(54.5007371812649,22.9314830994437,20.2129921582343));
#29636=CARTESIAN_POINT('Ctrl Pts',(54.5292309243637,22.9386249416802,20.2111749281898));
#29637=CARTESIAN_POINT('Ctrl Pts',(54.5691380299008,22.9476958266206,20.2086147682938));
#29638=CARTESIAN_POINT('Ctrl Pts',(54.5804270376897,22.9501588629238,20.2078888948675));
#29639=CARTESIAN_POINT('Ctrl Pts',(54.5986468384981,22.9539685363602,20.2067144664454));
#29640=CARTESIAN_POINT('Ctrl Pts',(54.6055646051,22.9553767203535,20.2062678818821));
#29641=CARTESIAN_POINT('Ctrl Pts',(54.619947656748,22.9582251102734,20.2053379041096));
#29642=CARTESIAN_POINT('Ctrl Pts',(54.6274139807704,22.9596594147358,20.2048543311882));
#29643=CARTESIAN_POINT('Ctrl Pts',(54.6450098508634,22.9629354433468,20.2037126920569));
#29644=CARTESIAN_POINT('Ctrl Pts',(54.6551457406575,22.9647414827317,20.2030535046837));
#29645=CARTESIAN_POINT('Ctrl Pts',(54.688623608902,22.9704396199011,20.2008708831504));
#29646=CARTESIAN_POINT('Ctrl Pts',(54.7120201477154,22.9739947004307,20.1993368744682));
#29647=CARTESIAN_POINT('Ctrl Pts',(54.7676193837334,22.9814334865604,20.1956695590525));
#29648=CARTESIAN_POINT('Ctrl Pts',(54.7998636694171,22.9849495366825,20.1935253475222));
#29649=CARTESIAN_POINT('Ctrl Pts',(54.9428175769606,22.9970193138447,20.1839410375635));
#29650=CARTESIAN_POINT('Ctrl Pts',(55.053961948805,22.9970995187115,20.176268010679));
#29651=CARTESIAN_POINT('Ctrl Pts',(55.1644485224877,22.9879598200043,20.1685383772559));
#29652=CARTESIAN_POINT('',(53.0052506746727,20.9991991220829,20.2192088779402));
#29653=CARTESIAN_POINT('Ctrl Pts',(55.1644483497948,22.9879598342899,20.0118645378774));
#29654=CARTESIAN_POINT('Ctrl Pts',(55.1566329193673,22.9886063436481,20.0123992477384));
#29655=CARTESIAN_POINT('Ctrl Pts',(55.1488122479989,22.9892068830392,20.0129327173509));
#29656=CARTESIAN_POINT('Ctrl Pts',(55.1027605991908,22.9924699232624,20.0160639036847));
#29657=CARTESIAN_POINT('Ctrl Pts',(55.0644612791749,22.9940765621712,20.018627077361));
#29658=CARTESIAN_POINT('Ctrl Pts',(55.0173804434754,22.9946935019973,20.0217093294711));
#29659=CARTESIAN_POINT('Ctrl Pts',(55.0086233865615,22.994750583586,20.0222797101055));
#29660=CARTESIAN_POINT('Ctrl Pts',(54.9949413723923,22.9947496647945,20.0231660164658));
#29661=CARTESIAN_POINT('Ctrl Pts',(54.9900166520139,22.9947310969016,20.0234840517854));
#29662=CARTESIAN_POINT('Ctrl Pts',(54.9809082541158,22.9946630222509,20.0240703858775));
#29663=CARTESIAN_POINT('Ctrl Pts',(54.9767246902512,22.9946185920111,20.0243389533152));
#29664=CARTESIAN_POINT('Ctrl Pts',(54.9672370138689,22.9944879765663,20.0249463661045));
#29665=CARTESIAN_POINT('Ctrl Pts',(54.961933094064,22.9943937961616,20.0252847628645));
#29666=CARTESIAN_POINT('Ctrl Pts',(54.9457935346285,22.9940428019841,20.0263111073102));
#29667=CARTESIAN_POINT('Ctrl Pts',(54.9349593432274,22.9937188273287,20.0269954370683));
#29668=CARTESIAN_POINT('Ctrl Pts',(54.8070971436177,22.9888519617868,20.0350226279865));
#29669=CARTESIAN_POINT('Ctrl Pts',(54.6906672441414,22.9740985651303,20.0418539099103));
#29670=CARTESIAN_POINT('Ctrl Pts',(54.4243140087695,22.9161863867218,20.0576831805409));
#29671=CARTESIAN_POINT('Ctrl Pts',(54.2768356094417,22.8655325390301,20.0666402517219));
#29672=CARTESIAN_POINT('Ctrl Pts',(54.1156290181243,22.7881453356953,20.0776576226879));
#29673=CARTESIAN_POINT('Ctrl Pts',(54.0947019890323,22.777642037903,20.0791120607571));
#29674=CARTESIAN_POINT('Ctrl Pts',(54.0655689754216,22.7623722902422,20.0811733624578));
#29675=CARTESIAN_POINT('Ctrl Pts',(54.0572042040394,22.7579116904035,20.0817695097477));
#29676=CARTESIAN_POINT('Ctrl Pts',(54.0427101802509,22.7500493988139,20.0828101388912));
#29677=CARTESIAN_POINT('Ctrl Pts',(54.0365664261213,22.7466746817789,20.0832536588524));
#29678=CARTESIAN_POINT('Ctrl Pts',(54.0239002526467,22.7396300913181,20.0841731096089));
#29679=CARTESIAN_POINT('Ctrl Pts',(54.0173804528119,22.7359557581859,20.0846491947927));
#29680=CARTESIAN_POINT('Ctrl Pts',(54.0020409894496,22.7271968659256,20.0857760290131));
#29681=CARTESIAN_POINT('Ctrl Pts',(53.9932393348237,22.7220813445061,20.0864278864217));
#29682=CARTESIAN_POINT('Ctrl Pts',(53.9746754343755,22.711101045727,20.0878141544641));
#29683=CARTESIAN_POINT('Ctrl Pts',(53.9649235148682,22.705219608894,20.0885491548534));
#29684=CARTESIAN_POINT('Ctrl Pts',(53.9385593557217,22.6890097553492,20.0905549330596));
#29685=CARTESIAN_POINT('Ctrl Pts',(53.9220481689928,22.6785201816267,20.0918315373929));
#29686=CARTESIAN_POINT('Ctrl Pts',(53.799734437143,22.5982651012062,20.1014446963132));
#29687=CARTESIAN_POINT('Ctrl Pts',(53.7006584225284,22.5188121813552,20.1101443146449));
#29688=CARTESIAN_POINT('Ctrl Pts',(53.515187165902,22.3385680694808,20.1281578835595));
#29689=CARTESIAN_POINT('Ctrl Pts',(53.4299214652856,22.2374541144539,20.1374355271461));
#29690=CARTESIAN_POINT('Ctrl Pts',(53.3466356361515,22.1160852140934,20.1471776157299));
#29691=CARTESIAN_POINT('Ctrl Pts',(53.3381547518389,22.1034175681686,20.1481786198885));
#29692=CARTESIAN_POINT('Ctrl Pts',(53.3263940015529,22.0854076552707,20.1495782548254));
#29693=CARTESIAN_POINT('Ctrl Pts',(53.3229930655321,22.0801456200284,20.1499843979058));
#29694=CARTESIAN_POINT('Ctrl Pts',(53.3173082956327,22.0712583938614,20.1506655385312));
#29695=CARTESIAN_POINT('Ctrl Pts',(53.3150112661832,22.0676417406842,20.1509413970973));
#29696=CARTESIAN_POINT('Ctrl Pts',(53.3103447846438,22.0602418319038,20.1515030645192));
#29697=CARTESIAN_POINT('Ctrl Pts',(53.3079763529492,22.0564579819734,20.1517888066249));
#29698=CARTESIAN_POINT('Ctrl Pts',(53.3019737727127,22.0467961836572,20.1525148035911));
#29699=CARTESIAN_POINT('Ctrl Pts',(53.2983573946826,22.0409071840548,20.1529539059083));
#29700=CARTESIAN_POINT('Ctrl Pts',(53.2837958406155,22.0169160832294,20.1547294876088));
#29701=CARTESIAN_POINT('Ctrl Pts',(53.2731078714952,21.9986584494134,20.1560502176154));
#29702=CARTESIAN_POINT('Ctrl Pts',(53.2457293605358,21.9501349421749,20.1594900885044));
#29703=CARTESIAN_POINT('Ctrl Pts',(53.2295308993368,21.9195984587963,20.1615843445483));
#29704=CARTESIAN_POINT('Ctrl Pts',(53.1236474573046,21.7068119815938,20.1758044579148));
#29705=CARTESIAN_POINT('Ctrl Pts',(53.0614625627725,21.5122166207992,20.1870894103567));
#29706=CARTESIAN_POINT('Ctrl Pts',(53.0236449015922,21.2730703255374,20.2017943876848));
#29707=CARTESIAN_POINT('Ctrl Pts',(53.0186867722596,21.2344023426098,20.2041919383045));
#29708=CARTESIAN_POINT('Ctrl Pts',(53.0135996032508,21.1827770779012,20.2074303062342));
#29709=CARTESIAN_POINT('Ctrl Pts',(53.0124590742998,21.169926609611,20.2082394417033));
#29710=CARTESIAN_POINT('Ctrl Pts',(53.0108030558203,21.1489603783053,20.2095649259071));
#29711=CARTESIAN_POINT('Ctrl Pts',(53.0102123916873,21.1408507993118,20.2100789117005));
#29712=CARTESIAN_POINT('Ctrl Pts',(53.0091929700689,21.1255651606017,20.2110502562633));
#29713=CARTESIAN_POINT('Ctrl Pts',(53.0087533901421,21.118389934071,20.2115072678539));
#29714=CARTESIAN_POINT('Ctrl Pts',(53.0079440432529,21.1038957658281,20.212432632476));
#29715=CARTESIAN_POINT('Ctrl Pts',(53.0075758047057,21.0965768533619,20.2129010261413));
#29716=CARTESIAN_POINT('Ctrl Pts',(53.0066503942713,21.0759159418415,20.2142265338185));
#29717=CARTESIAN_POINT('Ctrl Pts',(53.0061868645549,21.0625703397498,20.2150865585809));
#29718=CARTESIAN_POINT('Ctrl Pts',(53.0054458586132,21.032549395174,20.2170301178252));
#29719=CARTESIAN_POINT('Ctrl Pts',(53.0052434517756,21.0158734438085,20.2181159179354));
#29720=CARTESIAN_POINT('Ctrl Pts',(53.0052501614646,20.9991974023945,20.2192080988249));
#29721=CARTESIAN_POINT('Ctrl Pts',(53.0052501607968,20.9991990637311,20.2192079900173));
#29722=CARTESIAN_POINT('Ctrl Pts',(53.0053403195642,20.7746566204111,20.2339141702458));
#29723=CARTESIAN_POINT('Ctrl Pts',(53.0433501436141,20.5517424599308,20.2499366245077));
#29724=CARTESIAN_POINT('Ctrl Pts',(53.1338646609569,20.2936191810681,20.2686246850473));
#29725=CARTESIAN_POINT('Ctrl Pts',(53.1518051562617,20.2479284074731,20.2719265187195));
#29726=CARTESIAN_POINT('Ctrl Pts',(53.1750281533055,20.1946509312683,20.2757324527616));
#29727=CARTESIAN_POINT('Ctrl Pts',(53.1786985269636,20.1863844178494,20.2763216833574));
#29728=CARTESIAN_POINT('Ctrl Pts',(53.1844578210452,20.1736474720491,20.2772272324041));
#29729=CARTESIAN_POINT('Ctrl Pts',(53.1865072581479,20.1691594734588,20.2775458621683));
#29730=CARTESIAN_POINT('Ctrl Pts',(53.1903250497029,20.1608804407195,20.27813274407));
#29731=CARTESIAN_POINT('Ctrl Pts',(53.1920886666457,20.1570873878118,20.2784012689636));
#29732=CARTESIAN_POINT('Ctrl Pts',(53.1961108902961,20.1485073946983,20.2790078946423));
#29733=CARTESIAN_POINT('Ctrl Pts',(53.1983766220866,20.1437238864098,20.2793455517999));
#29734=CARTESIAN_POINT('Ctrl Pts',(53.2051635369318,20.1295412615098,20.280345206341));
#29735=CARTESIAN_POINT('Ctrl Pts',(53.2097395093082,20.1201683506742,20.2810039319593));
#29736=CARTESIAN_POINT('Ctrl Pts',(53.253516195955,20.0322568472779,20.2871682187445));
#29737=CARTESIAN_POINT('Ctrl Pts',(53.297792716928,19.9563396634317,20.2923868143711));
#29738=CARTESIAN_POINT('Ctrl Pts',(53.4334088231285,19.7555351393658,20.3065677298066));
#29739=CARTESIAN_POINT('Ctrl Pts',(53.5344627596391,19.6379793421624,20.3153520336596));
#29740=CARTESIAN_POINT('Ctrl Pts',(53.67134187088,19.5118142698688,20.326586243232));
#29741=CARTESIAN_POINT('Ctrl Pts',(53.6951191596315,19.4909224586767,20.3285151054779));
#29742=CARTESIAN_POINT('Ctrl Pts',(53.7316234030019,19.4603561226493,20.3314506204188));
#29743=CARTESIAN_POINT('Ctrl Pts',(53.7439866679006,19.4502539085609,20.3324405264744));
#29744=CARTESIAN_POINT('Ctrl Pts',(53.7642286633495,19.4341151899381,20.334055215494));
#29745=CARTESIAN_POINT('Ctrl Pts',(53.7720336692597,19.4279870484575,20.3346763848127));
#29746=CARTESIAN_POINT('Ctrl Pts',(53.7871142530653,19.4163272892635,20.3358740645364));
#29747=CARTESIAN_POINT('Ctrl Pts',(53.7943827751812,19.4107869266249,20.3364502126285));
#29748=CARTESIAN_POINT('Ctrl Pts',(53.8017798890779,19.4052284987491,20.3370355133223));
#29749=CARTESIAN_POINT('Ctrl Pts',(53.8018707661501,19.4051602229645,20.3370427038622));
#29750=CARTESIAN_POINT('Ctrl Pts',(53.8020555593073,19.4050214128996,20.3370573250788));
#29751=CARTESIAN_POINT('Ctrl Pts',(53.8021494757282,19.4049508791899,20.3370647557713));
#29752=CARTESIAN_POINT('Ctrl Pts',(53.8023405620233,19.4048073947359,20.3370798742274));
#29753=CARTESIAN_POINT('Ctrl Pts',(53.8024377324258,19.4047344445057,20.3370875620209));
#29754=CARTESIAN_POINT('Ctrl Pts',(53.8026355618305,19.4045859532567,20.337103213247));
#29755=CARTESIAN_POINT('Ctrl Pts',(53.802736221174,19.4045104129923,20.3371111766935));
#29756=CARTESIAN_POINT('Ctrl Pts',(53.8029412855932,19.4043565517957,20.3371273995285));
#29757=CARTESIAN_POINT('Ctrl Pts',(53.8030456912114,19.4042782315808,20.3371356589452));
#29758=CARTESIAN_POINT('Ctrl Pts',(53.8032585307919,19.4041186019172,20.3371524960335));
#29759=CARTESIAN_POINT('Ctrl Pts',(53.8033669654118,19.4040372932298,20.3371610737409));
#29760=CARTESIAN_POINT('Ctrl Pts',(53.8035881742186,19.4038714570896,20.3371785719805));
#29761=CARTESIAN_POINT('Ctrl Pts',(53.8037009491561,19.403786930478,20.3371874925538));
#29762=CARTESIAN_POINT('Ctrl Pts',(53.8039311826814,19.4036144048888,20.3372057036876));
#29763=CARTESIAN_POINT('Ctrl Pts',(53.8040486419052,19.403526407011,20.3372149942778));
#29764=CARTESIAN_POINT('Ctrl Pts',(53.8042886244024,19.4033466587275,20.3372339754716));
#29765=CARTESIAN_POINT('Ctrl Pts',(53.8044111485808,19.4032549094197,20.3372436661238));
#29766=CARTESIAN_POINT('Ctrl Pts',(53.8046616835939,19.4030673472566,20.3372634807965));
#29767=CARTESIAN_POINT('Ctrl Pts',(53.8047896954448,19.4029715356475,20.3372736048716));
#29768=CARTESIAN_POINT('Ctrl Pts',(53.805051676911,19.4027755024296,20.3372943235698));
#29769=CARTESIAN_POINT('Ctrl Pts',(53.8051856474742,19.4026752823892,20.3373049182387));
#29770=CARTESIAN_POINT('Ctrl Pts',(53.8053956221648,19.4025182467516,20.3373215229405));
#29771=CARTESIAN_POINT('Ctrl Pts',(53.8054716177938,19.4024614196807,20.337327532531));
#29772=CARTESIAN_POINT('Ctrl Pts',(53.8056425644816,19.4023336103003,20.3373410504267));
#29773=CARTESIAN_POINT('Ctrl Pts',(53.8057375178363,19.4022626310153,20.3373485588524));
#29774=CARTESIAN_POINT('Ctrl Pts',(53.805951791935,19.4021024871712,20.3373655021698));
#29775=CARTESIAN_POINT('Ctrl Pts',(53.806071116382,19.4020133274804,20.3373749372561));
#29776=CARTESIAN_POINT('Ctrl Pts',(53.8063414911553,19.4018113495877,20.337396315415));
#29777=CARTESIAN_POINT('Ctrl Pts',(53.8064925474982,19.4016985394279,20.3374082588024));
#29778=CARTESIAN_POINT('Ctrl Pts',(53.8068366455046,19.4014416400969,20.3374354642049));
#29779=CARTESIAN_POINT('Ctrl Pts',(53.8070296971665,19.4012975645593,20.3374507267399));
#29780=CARTESIAN_POINT('Ctrl Pts',(53.8074725503158,19.4009671856527,20.3374857368146));
#29781=CARTESIAN_POINT('Ctrl Pts',(53.807722369393,19.4007809058282,20.3375054852754));
#29782=CARTESIAN_POINT('Ctrl Pts',(53.813836058201,19.3962244080137,20.3379887503409));
#29783=CARTESIAN_POINT('Ctrl Pts',(53.8197238087314,19.3918864603942,20.3384535154984));
#29784=CARTESIAN_POINT('Ctrl Pts',(53.8333588035398,19.3819557549988,20.3395284342928));
#29785=CARTESIAN_POINT('Ctrl Pts',(53.8411225948208,19.3763861251602,20.3401394666954));
#29786=CARTESIAN_POINT('Ctrl Pts',(53.8613739974453,19.3620773223339,20.3417308180093));
#29787=CARTESIAN_POINT('Ctrl Pts',(53.8739221032475,19.3534252459284,20.3427144188101));
#29788=CARTESIAN_POINT('Ctrl Pts',(53.9673687209747,19.2905604031253,20.3500230239132));
#29789=CARTESIAN_POINT('Ctrl Pts',(54.0520291948315,19.2422009869957,20.3565647329655));
#29790=CARTESIAN_POINT('Ctrl Pts',(54.2662014451588,19.139846297466,20.3728822910458));
#29791=CARTESIAN_POINT('Ctrl Pts',(54.3985303097303,19.0929435951701,20.3827920588229));
#29792=CARTESIAN_POINT('Ctrl Pts',(54.5821668682738,19.048890518195,20.3956923159089));
#29793=CARTESIAN_POINT('Ctrl Pts',(54.6300646841011,19.039244665239,20.3989784177812));
#29794=CARTESIAN_POINT('Ctrl Pts',(54.6871877961556,19.0299092168263,20.4027686921682));
#29795=CARTESIAN_POINT('Ctrl Pts',(54.6961131446509,19.0285127554538,20.4033572108659));
#29796=CARTESIAN_POINT('Ctrl Pts',(54.7099250600226,19.0264477685282,20.4042619023432));
#29797=CARTESIAN_POINT('Ctrl Pts',(54.7148049983627,19.0257366706874,20.4045803796771));
#29798=CARTESIAN_POINT('Ctrl Pts',(54.7238293357576,19.0244558151327,20.405167120805));
#29799=CARTESIAN_POINT('Ctrl Pts',(54.7279728646564,19.0238810004604,20.405435656307));
#29800=CARTESIAN_POINT('Ctrl Pts',(54.7373662011215,19.02260800636,20.4060424824625));
#29801=CARTESIAN_POINT('Ctrl Pts',(54.7426169915334,19.0219176970264,20.4063803282222));
#29802=CARTESIAN_POINT('Ctrl Pts',(54.7582308092374,19.0199282087064,20.4073810634377));
#29803=CARTESIAN_POINT('Ctrl Pts',(54.7686015496836,19.0186894719334,20.408040670648));
#29804=CARTESIAN_POINT('Ctrl Pts',(54.8699296938782,19.0073927619749,20.4144400243648));
#29805=CARTESIAN_POINT('Ctrl Pts',(54.9614804101356,19.0035224452643,20.4198675447271));
#29806=CARTESIAN_POINT('Ctrl Pts',(55.1742802323822,19.0091767730949,20.4323082048308));
#29807=CARTESIAN_POINT('Ctrl Pts',(55.2950260752195,19.0234600784067,20.4392474172708));
#29808=CARTESIAN_POINT('Ctrl Pts',(55.4613563915135,19.0587250241781,20.449335555546));
#29809=CARTESIAN_POINT('Ctrl Pts',(55.5085987887294,19.0705635478535,20.452260273667));
#29810=CARTESIAN_POINT('Ctrl Pts',(55.5761220434655,19.0901365745287,20.4565576935917));
#29811=CARTESIAN_POINT('Ctrl Pts',(55.59678574912,19.0964922830254,20.4578888736637));
#29812=CARTESIAN_POINT('Ctrl Pts',(55.6336970749415,19.1085055061932,20.4602982659284));
#29813=CARTESIAN_POINT('Ctrl Pts',(55.6499827001584,19.1140398033436,20.4613724789185));
#29814=CARTESIAN_POINT('Ctrl Pts',(55.6747353528252,19.1228101126171,20.4630231922844));
#29815=CARTESIAN_POINT('Ctrl Pts',(55.6832555378721,19.1258944706238,20.4635946760777));
#29816=CARTESIAN_POINT('Ctrl Pts',(55.698745816016,19.1316217164249,20.4646398090001));
#29817=CARTESIAN_POINT('Ctrl Pts',(55.7057227081686,19.134245840781,20.4651128256796));
#29818=CARTESIAN_POINT('Ctrl Pts',(55.7207960586341,19.140011820763,20.4661397952983));
#29819=CARTESIAN_POINT('Ctrl Pts',(55.7288870076235,19.1431675597338,20.4666942057045));
#29820=CARTESIAN_POINT('Ctrl Pts',(55.7509119887205,19.151924170374,20.468212193807));
#29821=CARTESIAN_POINT('Ctrl Pts',(55.7648035637279,19.1576296313476,20.4691792728014));
#29822=CARTESIAN_POINT('Ctrl Pts',(55.8362542196819,19.187922740249,20.4742045540793));
#29823=CARTESIAN_POINT('Ctrl Pts',(55.8926916595462,19.2150503381232,20.4783483361877));
#29824=CARTESIAN_POINT('Ctrl Pts',(55.9674512363783,19.2554179112062,20.4840813191748));
#29825=CARTESIAN_POINT('Ctrl Pts',(55.9869654597915,19.2663830624136,20.4856011458115));
#29826=CARTESIAN_POINT('Ctrl Pts',(56.1264336521346,19.3478690979151,20.4966294480829));
#29827=CARTESIAN_POINT('Ctrl Pts',(56.238899543939,19.4304419632926,20.5064579534391));
#29828=CARTESIAN_POINT('Ctrl Pts',(56.3851888059707,19.5634377843653,20.5200806281248));
#29829=CARTESIAN_POINT('Ctrl Pts',(56.4267802694536,19.6047371532754,20.5240622904371));
#29830=CARTESIAN_POINT('Ctrl Pts',(56.4754356628923,19.6575056608068,20.5287963236997));
#29831=CARTESIAN_POINT('Ctrl Pts',(56.484278382368,19.6672887964536,20.529659956273));
#29832=CARTESIAN_POINT('Ctrl Pts',(56.4968326966673,19.6814582181467,20.5308899032649));
#29833=CARTESIAN_POINT('Ctrl Pts',(56.5006231512401,19.6857737210601,20.5312617642927));
#29834=CARTESIAN_POINT('Ctrl Pts',(56.5071756085384,19.6932991244838,20.5319053878705));
#29835=CARTESIAN_POINT('Ctrl Pts',(56.5099461070008,19.6965015349573,20.5321777722523));
#29836=CARTESIAN_POINT('Ctrl Pts',(56.5153641628133,19.7028047025723,20.5327109148783));
#29837=CARTESIAN_POINT('Ctrl Pts',(56.5180124119615,19.705904754872,20.5329717303642));
#29838=CARTESIAN_POINT('Ctrl Pts',(56.5253103928492,19.7145010324666,20.533691174219));
#29839=CARTESIAN_POINT('Ctrl Pts',(56.5299399603325,19.7200144095966,20.5341483487297));
#29840=CARTESIAN_POINT('Ctrl Pts',(56.5482646518245,19.7420788517825,20.5359616435059));
#29841=CARTESIAN_POINT('Ctrl Pts',(56.5617224449554,19.7588263052324,20.5373016945309));
#29842=CARTESIAN_POINT('Ctrl Pts',(56.708638651417,19.9478291851451,20.5520672808868));
#29843=CARTESIAN_POINT('Ctrl Pts',(56.8132943612363,20.1406377052644,20.5640205393494));
#29844=CARTESIAN_POINT('Ctrl Pts',(56.8967253479837,20.3812841817354,20.5793051169766));
#29845=CARTESIAN_POINT('Ctrl Pts',(56.9077942179297,20.4163071924218,20.5815330574227));
#29846=CARTESIAN_POINT('Ctrl Pts',(56.9250479874808,20.4766494398764,20.5853915908788));
#29847=CARTESIAN_POINT('Ctrl Pts',(56.9317151793355,20.5018213864632,20.587006962931));
#29848=CARTESIAN_POINT('Ctrl Pts',(56.9404222412177,20.5375030707621,20.5893080180752));
#29849=CARTESIAN_POINT('Ctrl Pts',(56.9428733631361,20.5479104386847,20.5899805024602));
#29850=CARTESIAN_POINT('Ctrl Pts',(56.9469392486697,20.5658180360187,20.5911401162445));
#29851=CARTESIAN_POINT('Ctrl Pts',(56.9485946461366,20.5733088725716,20.5916259340584));
#29852=CARTESIAN_POINT('Ctrl Pts',(56.9516715395003,20.5876235360544,20.5925558092941));
#29853=CARTESIAN_POINT('Ctrl Pts',(56.9531005625663,20.594445642871,20.5929996181203));
#29854=CARTESIAN_POINT('Ctrl Pts',(56.9567069356368,20.6121235769475,20.5941513911293));
#29855=CARTESIAN_POINT('Ctrl Pts',(56.9588296856044,20.6229901776666,20.594861083312));
#29856=CARTESIAN_POINT('Ctrl Pts',(56.9646401154627,20.654109084914,20.5968985559233));
#29857=CARTESIAN_POINT('Ctrl Pts',(56.9681048236525,20.6744010766302,20.5982333352745));
#29858=CARTESIAN_POINT('Ctrl Pts',(56.9969610546452,20.8607453010119,20.6105510200239));
#29859=CARTESIAN_POINT('Ctrl Pts',(57.0015904874806,21.0293004509427,20.6222154024361));
#29860=CARTESIAN_POINT('Ctrl Pts',(56.9745337637511,21.3027693295947,20.6413733031866));
#29861=CARTESIAN_POINT('Ctrl Pts',(56.9554755471391,21.4081343772677,20.6487886074502));
#29862=CARTESIAN_POINT('Ctrl Pts',(56.9254036700948,21.52149373697,20.6564878113769));
#29863=CARTESIAN_POINT('Ctrl Pts',(56.9226676680258,21.5314922952844,20.657164379718));
#29864=CARTESIAN_POINT('Ctrl Pts',(56.918439575517,21.5464835773153,20.6581745273555));
#29865=CARTESIAN_POINT('Ctrl Pts',(56.917005714003,21.551492338263,20.6585113114148));
#29866=CARTESIAN_POINT('Ctrl Pts',(56.9144992754106,21.5601199266028,20.6590901133012));
#29867=CARTESIAN_POINT('Ctrl Pts',(56.9134360393161,21.5637413697549,20.6593326643263));
#29868=CARTESIAN_POINT('Ctrl Pts',(56.9109874208129,21.5719947666808,20.6598845213071));
#29869=CARTESIAN_POINT('Ctrl Pts',(56.9095954761666,21.5766247082971,20.6601934410468));
#29870=CARTESIAN_POINT('Ctrl Pts',(56.905749752708,21.5892498495434,20.6610341366492));
#29871=CARTESIAN_POINT('Ctrl Pts',(56.9032624711348,21.5972348591337,20.6615640056688));
#29872=CARTESIAN_POINT('Ctrl Pts',(56.8906303508372,21.6369077306927,20.6641885124695));
#29873=CARTESIAN_POINT('Ctrl Pts',(56.8797433796901,21.6683559757757,20.666243131886));
#29874=CARTESIAN_POINT('Ctrl Pts',(56.7962869280656,21.8912273795385,20.6807166516061));
#29875=CARTESIAN_POINT('Ctrl Pts',(56.6954149776349,22.0707571048413,20.6920310262491));
#29876=CARTESIAN_POINT('Ctrl Pts',(56.5351783112772,22.2748529366196,20.707612679437));
#29877=CARTESIAN_POINT('Ctrl Pts',(56.499629453004,22.3164851469472,20.7109527195792));
#29878=CARTESIAN_POINT('Ctrl Pts',(56.4529097316357,22.3668490324397,20.7152345588774));
#29879=CARTESIAN_POINT('Ctrl Pts',(56.4432957732682,22.3769968267517,20.7161102629293));
#29880=CARTESIAN_POINT('Ctrl Pts',(56.4277573257056,22.3930565705028,20.7175175330834));
#29881=CARTESIAN_POINT('Ctrl Pts',(56.4219007941711,22.3990338515577,20.7180461495342));
#29882=CARTESIAN_POINT('Ctrl Pts',(56.4107317234163,22.4102906298756,20.7190510121644));
#29883=CARTESIAN_POINT('Ctrl Pts',(56.4054267089373,22.4155774155677,20.7195269222617));
#29884=CARTESIAN_POINT('Ctrl Pts',(56.393316125218,22.4275112030276,20.7206103365117));
#29885=CARTESIAN_POINT('Ctrl Pts',(56.3864925660458,22.4341396092007,20.7212186389543));
#29886=CARTESIAN_POINT('Ctrl Pts',(56.368714126246,22.4511641144675,20.7227982183236));
#29887=CARTESIAN_POINT('Ctrl Pts',(56.3576882871739,22.4614849094497,20.7237726974782));
#29888=CARTESIAN_POINT('Ctrl Pts',(56.277738870225,22.5346364542036,20.7308035971634));
#29889=CARTESIAN_POINT('Ctrl Pts',(56.2046109017385,22.592681309524,20.7370580497102));
#29890=CARTESIAN_POINT('Ctrl Pts',(56.0090667701674,22.7267011837668,20.7533245050715));
#29891=CARTESIAN_POINT('Ctrl Pts',(55.8819954002998,22.7949356057058,20.7635097693315));
#29892=CARTESIAN_POINT('Ctrl Pts',(55.7029321584625,22.8674452504992,20.77671117087));
#29893=CARTESIAN_POINT('Ctrl Pts',(55.6564908908065,22.8842733358081,20.7800344203223));
#29894=CARTESIAN_POINT('Ctrl Pts',(55.6008431127187,22.9021296436412,20.783861658913));
#29895=CARTESIAN_POINT('Ctrl Pts',(55.5921983921175,22.9048387593697,20.7844518508895));
#29896=CARTESIAN_POINT('Ctrl Pts',(55.5788144436279,22.9089331509356,20.7853585579187));
#29897=CARTESIAN_POINT('Ctrl Pts',(55.5740881596831,22.9103598407331,20.785677393425));
#29898=CARTESIAN_POINT('Ctrl Pts',(55.5653477694354,22.9129628741586,20.7862644656622));
#29899=CARTESIAN_POINT('Ctrl Pts',(55.561335283529,22.9141441320708,20.7865329765632));
#29900=CARTESIAN_POINT('Ctrl Pts',(55.5522407772353,22.9167904575629,20.787139333119));
#29901=CARTESIAN_POINT('Ctrl Pts',(55.547156635804,22.918247938014,20.7874767368483));
#29902=CARTESIAN_POINT('Ctrl Pts',(55.5339899558722,22.9219658489357,20.7883466161601));
#29903=CARTESIAN_POINT('Ctrl Pts',(55.5258987441039,22.9241955498973,20.7888773708691));
#29904=CARTESIAN_POINT('Ctrl Pts',(55.4740513917151,22.938131691854,20.7922554989259));
#29905=CARTESIAN_POINT('Ctrl Pts',(55.4299176142441,22.94839696424,20.7950271583184));
#29906=CARTESIAN_POINT('Ctrl Pts',(55.3630092057832,22.9615748485849,20.7991261236621));
#29907=CARTESIAN_POINT('Ctrl Pts',(55.3404743331046,22.9656115735928,20.8004893063809));
#29908=CARTESIAN_POINT('Ctrl Pts',(55.2669545374997,22.9774790071089,20.8048944116465));
#29909=CARTESIAN_POINT('Ctrl Pts',(55.2157737787945,22.983714093799,20.8078956609588));
#29910=CARTESIAN_POINT('Ctrl Pts',(55.1644479523467,22.9879598671676,20.810886410834));
#29911=CARTESIAN_POINT('Origin',(55.,21.,6.22095488139522));
#29912=CARTESIAN_POINT('',(55.1644483608155,22.9879598333782,21.7678366528264));
#29913=CARTESIAN_POINT('',(55.1644483516286,22.9879598341382,21.6085614209934));
#29914=CARTESIAN_POINT('',(55.1644483516311,22.987959834138,6.22095488139522));
#29915=CARTESIAN_POINT('',(53.005250485173,21.0016376188735,21.1784010577392));
#29916=CARTESIAN_POINT('Ctrl Pts',(55.1644483608155,22.9879598333782,21.7678366528264));
#29917=CARTESIAN_POINT('Ctrl Pts',(55.1754894884733,22.9870464872862,21.7671913811389));
#29918=CARTESIAN_POINT('Ctrl Pts',(55.186524561825,22.9860410289883,21.7665469511083));
#29919=CARTESIAN_POINT('Ctrl Pts',(55.3566374547529,22.9691104636088,21.7566134017014));
#29920=CARTESIAN_POINT('Ctrl Pts',(55.5132226965071,22.9342136858194,21.7474202726949));
#29921=CARTESIAN_POINT('Ctrl Pts',(55.6857571425906,22.8733123194524,21.7361438131223));
#29922=CARTESIAN_POINT('Ctrl Pts',(55.7074187567911,22.865240075279,21.7347075812375));
#29923=CARTESIAN_POINT('Ctrl Pts',(55.7377126217523,22.8533473987926,21.7326678499848));
#29924=CARTESIAN_POINT('Ctrl Pts',(55.746466045348,22.8498391635904,21.7320747651588));
#29925=CARTESIAN_POINT('Ctrl Pts',(55.7616719325975,22.8436193782962,21.7310378769034));
#29926=CARTESIAN_POINT('Ctrl Pts',(55.7681356622597,22.8409356716817,21.7305950170133));
#29927=CARTESIAN_POINT('Ctrl Pts',(55.7816344208231,22.8352475886342,21.7296656876547));
#29928=CARTESIAN_POINT('Ctrl Pts',(55.7886665457517,22.8322366540207,21.7291790015679));
#29929=CARTESIAN_POINT('Ctrl Pts',(55.8053673427886,22.824971940078,21.7280169708546));
#29930=CARTESIAN_POINT('Ctrl Pts',(55.8150198087588,22.820681697367,21.727340391222));
#29931=CARTESIAN_POINT('Ctrl Pts',(55.8476196067839,22.8058808406385,21.7250381717774));
#29932=CARTESIAN_POINT('Ctrl Pts',(55.8704005881403,22.7950117903822,21.7234002974448));
#29933=CARTESIAN_POINT('Ctrl Pts',(55.9244977183062,22.7679295165084,21.7194388900537));
#29934=CARTESIAN_POINT('Ctrl Pts',(55.9556012842391,22.7513128616017,21.7171019741812));
#29935=CARTESIAN_POINT('Ctrl Pts',(56.0761757063756,22.6827290970373,21.70780576173));
#29936=CARTESIAN_POINT('Ctrl Pts',(56.1619791273868,22.6246634769503,21.7006527744721));
#29937=CARTESIAN_POINT('Ctrl Pts',(56.3402035016434,22.4826879312896,21.6847691182636));
#29938=CARTESIAN_POINT('Ctrl Pts',(56.430064454559,22.3962199072172,21.6760433662476));
#29939=CARTESIAN_POINT('Ctrl Pts',(56.5214903327015,22.2900926597736,21.6667673882018));
#29940=CARTESIAN_POINT('Ctrl Pts',(56.5315534803265,22.2781298355654,21.6657404996085));
#29941=CARTESIAN_POINT('Ctrl Pts',(56.5454936556161,22.2611570110496,21.6643110716069));
#29942=CARTESIAN_POINT('Ctrl Pts',(56.5494887350424,22.2562453218568,21.6639005976305));
#29943=CARTESIAN_POINT('Ctrl Pts',(56.5559128907119,22.2482699721786,21.6632393334997));
#29944=CARTESIAN_POINT('Ctrl Pts',(56.5583564243787,22.2452180942187,21.6629875226884));
#29945=CARTESIAN_POINT('Ctrl Pts',(56.5635069596301,22.2387463712643,21.6624561743527));
#29946=CARTESIAN_POINT('Ctrl Pts',(56.566211747806,22.2353247940739,21.6621768002988));
#29947=CARTESIAN_POINT('Ctrl Pts',(56.5728755534315,22.2268379622701,21.6614875878043));
#29948=CARTESIAN_POINT('Ctrl Pts',(56.5768213882813,22.2217623354988,21.6610786763415));
#29949=CARTESIAN_POINT('Ctrl Pts',(56.5914130371749,22.2028042885497,21.659563126334));
#29950=CARTESIAN_POINT('Ctrl Pts',(56.6019009888056,22.1888006068924,21.6584669942006));
#29951=CARTESIAN_POINT('Ctrl Pts',(56.6278988651188,22.1531189057719,21.6557272927243));
#29952=CARTESIAN_POINT('Ctrl Pts',(56.6431614383659,22.1312641394717,21.6540977535843));
#29953=CARTESIAN_POINT('Ctrl Pts',(56.7541733029399,21.9653149961845,21.6420296782565));
#29954=CARTESIAN_POINT('Ctrl Pts',(56.8312565757016,21.8096095261305,21.6323404206636));
#29955=CARTESIAN_POINT('Ctrl Pts',(56.8980562515523,21.614423849292,21.6201214441714));
#29956=CARTESIAN_POINT('Ctrl Pts',(56.9080383943767,21.5826864830215,21.6181349409194));
#29957=CARTESIAN_POINT('Ctrl Pts',(56.9300694382814,21.5059891492683,21.6133175783544));
#29958=CARTESIAN_POINT('Ctrl Pts',(56.9413470110015,21.4608300347892,21.6104673293146));
#29959=CARTESIAN_POINT('Ctrl Pts',(56.9539056028261,21.4018340241064,21.6067067435587));
#29960=CARTESIAN_POINT('Ctrl Pts',(56.9566365082675,21.3883184866554,21.6058427742874));
#29961=CARTESIAN_POINT('Ctrl Pts',(56.9607916846872,21.3665963534099,21.6044498315883));
#29962=CARTESIAN_POINT('Ctrl Pts',(56.9623050887383,21.358407104246,21.6039237000099));
#29963=CARTESIAN_POINT('Ctrl Pts',(56.9650839410229,21.3428249141041,21.6029206109956));
#29964=CARTESIAN_POINT('Ctrl Pts',(56.9663590624453,21.3354338265832,21.6024439700584));
#29965=CARTESIAN_POINT('Ctrl Pts',(56.9691697124369,21.3185752592298,21.6013547772683));
#29966=CARTESIAN_POINT('Ctrl Pts',(56.9706786930536,21.3091036001149,21.6007413959425));
#29967=CARTESIAN_POINT('Ctrl Pts',(56.9750974198979,21.280019390093,21.598853308166));
#29968=CARTESIAN_POINT('Ctrl Pts',(56.9777830365202,21.2603745192495,21.5975715812533));
#29969=CARTESIAN_POINT('Ctrl Pts',(56.9965179649881,21.1062430202525,21.5874619331828));
#29970=CARTESIAN_POINT('Ctrl Pts',(56.999122018261,20.9705028515897,21.5782046123475));
#29971=CARTESIAN_POINT('Ctrl Pts',(56.9767024712422,20.6994497282687,21.5592737915135));
#29972=CARTESIAN_POINT('Ctrl Pts',(56.9514920369751,20.5648360703416,21.5496525999555));
#29973=CARTESIAN_POINT('Ctrl Pts',(56.90844468956,20.4194025784161,21.5396169532412));
#29974=CARTESIAN_POINT('Ctrl Pts',(56.9040054368081,20.4050060266285,21.5386278836632));
#29975=CARTESIAN_POINT('Ctrl Pts',(56.8976871924466,20.3853110990607,21.5372821197988));
#29976=CARTESIAN_POINT('Ctrl Pts',(56.8959484116859,20.3799687528978,21.5369178184527));
#29977=CARTESIAN_POINT('Ctrl Pts',(56.8929368025121,20.3708468166067,21.5362971409745));
#29978=CARTESIAN_POINT('Ctrl Pts',(56.8916751796471,20.3670636036148,21.5360401234846));
#29979=CARTESIAN_POINT('Ctrl Pts',(56.8890335177551,20.3592205390198,21.5355081650716));
#29980=CARTESIAN_POINT('Ctrl Pts',(56.8876517272158,20.3551613334286,21.5352333387765));
#29981=CARTESIAN_POINT('Ctrl Pts',(56.8842875030629,20.3453819294345,21.5345723489344));
#29982=CARTESIAN_POINT('Ctrl Pts',(56.8822920758952,20.3396661784901,21.5341869458362));
#29983=CARTESIAN_POINT('Ctrl Pts',(56.8752544124114,20.3197984494964,21.5328502320829));
#29984=CARTESIAN_POINT('Ctrl Pts',(56.8700782014229,20.305694006168,21.531906470716));
#29985=CARTESIAN_POINT('Ctrl Pts',(56.8377901240749,20.2206952473293,21.5262428437303));
#29986=CARTESIAN_POINT('Ctrl Pts',(56.8068063973553,20.1513294801846,21.5217207456113));
#29987=CARTESIAN_POINT('Ctrl Pts',(56.7365571746062,20.0154530975152,21.5127490369553));
#29988=CARTESIAN_POINT('Ctrl Pts',(56.6972378428167,19.949120564546,21.5083083001996));
#29989=CARTESIAN_POINT('Ctrl Pts',(56.5851592601602,19.7828102857856,21.4966416191271));
#29990=CARTESIAN_POINT('Ctrl Pts',(56.5067868852725,19.6870384723547,21.4893611461833));
#29991=CARTESIAN_POINT('Ctrl Pts',(56.4091330501258,19.5880459794073,21.4807310768693));
#29992=CARTESIAN_POINT('Ctrl Pts',(56.3980666344491,19.5770875735389,21.4797591004909));
#29993=CARTESIAN_POINT('Ctrl Pts',(56.3799328673812,19.5595465696808,21.4781753011375));
#29994=CARTESIAN_POINT('Ctrl Pts',(56.3729439014042,19.5528836115514,21.4775669785422));
#29995=CARTESIAN_POINT('Ctrl Pts',(56.3604351997828,19.5411305742946,21.476481750257));
#29996=CARTESIAN_POINT('Ctrl Pts',(56.3549345471546,19.5360203879577,21.4760057195867));
#29997=CARTESIAN_POINT('Ctrl Pts',(56.3432978951763,19.5253315294743,21.4750010967602));
#29998=CARTESIAN_POINT('Ctrl Pts',(56.3371557074732,19.519759835805,21.4744722221224));
#29999=CARTESIAN_POINT('Ctrl Pts',(56.3208274874634,19.5051327604296,21.473069831216));
#30000=CARTESIAN_POINT('Ctrl Pts',(56.3105832246439,19.4961433208029,21.472193585967));
#30001=CARTESIAN_POINT('Ctrl Pts',(56.2619216879253,19.4543171986168,21.4680474063985));
#30002=CARTESIAN_POINT('Ctrl Pts',(56.2223606117604,19.4228457771348,21.4647225389661));
#30003=CARTESIAN_POINT('Ctrl Pts',(56.0451968588485,19.2925818247809,21.4500158228365));
#30004=CARTESIAN_POINT('Ctrl Pts',(55.8965315001714,19.2100479370119,21.4380549550473));
#30005=CARTESIAN_POINT('Ctrl Pts',(55.6741095994358,19.1212968819479,21.4215038495744));
#30006=CARTESIAN_POINT('Ctrl Pts',(55.6076172798366,19.0987497276618,21.4167227152394));
#30007=CARTESIAN_POINT('Ctrl Pts',(55.5302334514801,19.0769855891393,21.4114457524316));
#30008=CARTESIAN_POINT('Ctrl Pts',(55.5203772594771,19.0742950755907,21.4107789029419));
#30009=CARTESIAN_POINT('Ctrl Pts',(55.5054271191087,19.070337196855,21.4097758111305));
#30010=CARTESIAN_POINT('Ctrl Pts',(55.5003483028555,19.0690140642844,21.4094365058221));
#30011=CARTESIAN_POINT('Ctrl Pts',(55.4912136058819,19.0666727536332,21.4088289331351));
#30012=CARTESIAN_POINT('Ctrl Pts',(55.4871597116672,19.0656472750652,21.408560255185));
#30013=CARTESIAN_POINT('Ctrl Pts',(55.4782784517001,19.0634303506945,21.4079737338022));
#30014=CARTESIAN_POINT('Ctrl Pts',(55.4734498542741,19.0622442050764,21.4076561956255));
#30015=CARTESIAN_POINT('Ctrl Pts',(55.4596555001715,19.05891025977,21.4067527518928));
#30016=CARTESIAN_POINT('Ctrl Pts',(55.4506790785466,19.0568065113292,21.4061693057533));
#30017=CARTESIAN_POINT('Ctrl Pts',(55.3900748667853,19.0430456213015,21.4022581545981));
#30018=CARTESIAN_POINT('Ctrl Pts',(55.3380104075157,19.0333838973928,21.3990345301306));
#30019=CARTESIAN_POINT('Ctrl Pts',(55.1127857324754,19.0007993257279,21.3854345428394));
#30020=CARTESIAN_POINT('Ctrl Pts',(54.9374141623584,18.9985968571262,21.3756462024406));
#30021=CARTESIAN_POINT('Ctrl Pts',(54.7028584519862,19.0265451035192,21.3615363721819));
#30022=CARTESIAN_POINT('Ctrl Pts',(54.6421050202241,19.0366540328981,21.3577952093318));
#30023=CARTESIAN_POINT('Ctrl Pts',(54.5673036422746,19.0526877794598,21.3530343675713));
#30024=CARTESIAN_POINT('Ctrl Pts',(54.5527230945712,19.0559849864387,21.3520990454241));
#30025=CARTESIAN_POINT('Ctrl Pts',(54.5297464152499,19.0614530428467,21.3506129401895));
#30026=CARTESIAN_POINT('Ctrl Pts',(54.5213248296027,19.0635153456678,21.3500656418491));
#30027=CARTESIAN_POINT('Ctrl Pts',(54.5056855770255,19.067453383774,21.3490443259059));
#30028=CARTESIAN_POINT('Ctrl Pts',(54.4984644408627,19.0693148228947,21.3485707767908));
#30029=CARTESIAN_POINT('Ctrl Pts',(54.4824701749443,19.0735335544117,21.3475174359662));
#30030=CARTESIAN_POINT('Ctrl Pts',(54.4737024101165,19.0759103637894,21.3469370214494));
#30031=CARTESIAN_POINT('Ctrl Pts',(54.4482827831913,19.0829879880305,21.3452454080577));
#30032=CARTESIAN_POINT('Ctrl Pts',(54.4316758056237,19.0878455815143,21.3441291508789));
#30033=CARTESIAN_POINT('Ctrl Pts',(54.3943128178246,19.0993040957775,21.3415919297114));
#30034=CARTESIAN_POINT('Ctrl Pts',(54.373597776892,19.1060300751715,21.3401670290836));
#30035=CARTESIAN_POINT('Ctrl Pts',(54.3064508589294,19.1290541181105,21.3354876701956));
#30036=CARTESIAN_POINT('Ctrl Pts',(54.2605140003076,19.1467302658298,21.3321904197213));
#30037=CARTESIAN_POINT('Ctrl Pts',(54.0576257492687,19.2335447568475,21.317201284429));
#30038=CARTESIAN_POINT('Ctrl Pts',(53.9093485913713,19.3210409730612,21.3049954994048));
#30039=CARTESIAN_POINT('Ctrl Pts',(53.7401932157377,19.4528215092422,21.2904000484629));
#30040=CARTESIAN_POINT('Ctrl Pts',(53.7071510813313,19.4803234842571,21.2875169677071));
#30041=CARTESIAN_POINT('Ctrl Pts',(53.6688408555479,19.5143650381535,21.2841600287597));
#30042=CARTESIAN_POINT('Ctrl Pts',(53.6626950440673,19.5198948117678,21.2836210549439));
#30043=CARTESIAN_POINT('Ctrl Pts',(53.6527016922874,19.528999520398,21.2827441852063));
#30044=CARTESIAN_POINT('Ctrl Pts',(53.6488336494572,19.5325516582693,21.2824046646985));
#30045=CARTESIAN_POINT('Ctrl Pts',(53.6419107752789,19.5389597174383,21.2817968649623));
#30046=CARTESIAN_POINT('Ctrl Pts',(53.6388508698496,19.5418099931583,21.2815281737523));
#30047=CARTESIAN_POINT('Ctrl Pts',(53.6328993700287,19.5473888217791,21.281005487869));
#30048=CARTESIAN_POINT('Ctrl Pts',(53.6300069857988,19.550116380785,21.2807514218127));
#30049=CARTESIAN_POINT('Ctrl Pts',(53.6217101913731,19.5579873691435,21.2800224372482));
#30050=CARTESIAN_POINT('Ctrl Pts',(53.6163263857495,19.5631525628869,21.2795491560039));
#30051=CARTESIAN_POINT('Ctrl Pts',(53.590967083496,19.5877568591018,21.2773179696235));
#30052=CARTESIAN_POINT('Ctrl Pts',(53.5713703758551,19.6075841025924,21.2755881774862));
#30053=CARTESIAN_POINT('Ctrl Pts',(53.5166298381279,19.6653414379712,21.2707166801807));
#30054=CARTESIAN_POINT('Ctrl Pts',(53.4825348362847,19.7042373872366,21.2676335129944));
#30055=CARTESIAN_POINT('Ctrl Pts',(53.4046658687933,19.8003663151258,21.2603500855115));
#30056=CARTESIAN_POINT('Ctrl Pts',(53.3624054867302,19.8587301986654,21.2561907234951));
#30057=CARTESIAN_POINT('Ctrl Pts',(53.2492689929766,20.0342434705624,21.2440673642995));
#30058=CARTESIAN_POINT('Ctrl Pts',(53.1871822114731,20.15653730859,21.2360548292074));
#30059=CARTESIAN_POINT('Ctrl Pts',(53.1325808302092,20.2985659809651,21.2266086550836));
#30060=CARTESIAN_POINT('Ctrl Pts',(53.1272290215093,20.312982620174,21.225648729359));
#30061=CARTESIAN_POINT('Ctrl Pts',(53.1188087439455,20.3364948153727,21.224080735826));
#30062=CARTESIAN_POINT('Ctrl Pts',(53.1156382386956,20.3455533488254,21.2234760532983));
#30063=CARTESIAN_POINT('Ctrl Pts',(53.1101064464288,20.3617318869616,21.2223949001358));
#30064=CARTESIAN_POINT('Ctrl Pts',(53.1077197036348,20.3688430421607,21.2219192804384));
#30065=CARTESIAN_POINT('Ctrl Pts',(53.102768938251,20.3838740728872,21.2209130162123));
#30066=CARTESIAN_POINT('Ctrl Pts',(53.1002142767571,20.391796857929,21.2203820743571));
#30067=CARTESIAN_POINT('Ctrl Pts',(53.0935647224293,20.4128698701276,21.2189683152526));
#30068=CARTESIAN_POINT('Ctrl Pts',(53.0895563650892,20.4260467275007,21.2180826892937));
#30069=CARTESIAN_POINT('Ctrl Pts',(53.0810829516582,20.4549743812938,21.2161345767535));
#30070=CARTESIAN_POINT('Ctrl Pts',(53.0766747347695,20.4707406484973,21.2150703190758));
#30071=CARTESIAN_POINT('Ctrl Pts',(53.027692490045,20.6546277544868,21.2026265739537));
#30072=CARTESIAN_POINT('Ctrl Pts',(53.0051081067482,20.8277933531142,21.1905097787254));
#30073=CARTESIAN_POINT('Ctrl Pts',(53.0052506707585,21.0016358455293,21.1784008569847));
#30074=CARTESIAN_POINT('Ctrl Pts',(53.005250672195,21.0016375962395,21.1784007350398));
#30075=CARTESIAN_POINT('Ctrl Pts',(53.0053322847788,21.1010495530643,21.1714762398423));
#30076=CARTESIAN_POINT('Ctrl Pts',(53.0128454026382,21.2003316121899,21.1646030799111));
#30077=CARTESIAN_POINT('Ctrl Pts',(53.0288374103171,21.305941096795,21.157590323553));
#30078=CARTESIAN_POINT('Ctrl Pts',(53.0299815660941,21.3132240151852,21.1571082961377));
#30079=CARTESIAN_POINT('Ctrl Pts',(53.0319522638281,21.3253300052478,21.1563098624624));
#30080=CARTESIAN_POINT('Ctrl Pts',(53.0327562126103,21.3301566088289,21.1559922762268));
#30081=CARTESIAN_POINT('Ctrl Pts',(53.0342446887376,21.3388943543456,21.1554187516605));
#30082=CARTESIAN_POINT('Ctrl Pts',(53.0349231460854,21.34280648483,21.1551624821585));
#30083=CARTESIAN_POINT('Ctrl Pts',(53.0363404120851,21.3508362660986,21.1546375714133));
#30084=CARTESIAN_POINT('Ctrl Pts',(53.0370804846131,21.354953573736,21.154369017967));
#30085=CARTESIAN_POINT('Ctrl Pts',(53.0387837606977,21.3642612959843,21.1537632468667));
#30086=CARTESIAN_POINT('Ctrl Pts',(53.0397546169511,21.3694502251133,21.1534264665324));
#30087=CARTESIAN_POINT('Ctrl Pts',(53.0426917494388,21.3848107322295,21.1524321033939));
#30088=CARTESIAN_POINT('Ctrl Pts',(53.0447167141181,21.394971100467,21.1517777403337));
#30089=CARTESIAN_POINT('Ctrl Pts',(53.0632279488014,21.4842191290419,21.1460558551156));
#30090=CARTESIAN_POINT('Ctrl Pts',(53.084427682745,21.5622633851735,21.1412309674618));
#30091=CARTESIAN_POINT('Ctrl Pts',(53.1266578367985,21.6871853962932,21.1334902187382));
#30092=CARTESIAN_POINT('Ctrl Pts',(53.1448610539504,21.7349111127156,21.1305286757426));
#30093=CARTESIAN_POINT('Ctrl Pts',(53.2199468207642,21.9111408890913,21.1194153198988));
#30094=CARTESIAN_POINT('Ctrl Pts',(53.2885113574716,22.0341990223419,21.111257545834));
#30095=CARTESIAN_POINT('Ctrl Pts',(53.3834686793468,22.1689517127133,21.101105735441));
#30096=CARTESIAN_POINT('Ctrl Pts',(53.3978717768692,22.1886154522353,21.0995919441415));
#30097=CARTESIAN_POINT('Ctrl Pts',(53.4189398004808,22.2162996055119,21.0974113080032));
#30098=CARTESIAN_POINT('Ctrl Pts',(53.4253132701114,22.2245398241708,21.0967558338938));
#30099=CARTESIAN_POINT('Ctrl Pts',(53.4364622905516,22.2387233410145,21.0956162387663));
#30100=CARTESIAN_POINT('Ctrl Pts',(53.4412079527354,22.2446899353636,21.0951333104319));
#30101=CARTESIAN_POINT('Ctrl Pts',(53.4503955428175,22.2561062924043,21.0942023865234));
#30102=CARTESIAN_POINT('Ctrl Pts',(53.4548323155932,22.2615600724975,21.0937546025345));
#30103=CARTESIAN_POINT('Ctrl Pts',(53.4653686668489,22.2743726257586,21.0926952935831));
#30104=CARTESIAN_POINT('Ctrl Pts',(53.471492444971,22.281711187017,21.092082792144));
#30105=CARTESIAN_POINT('Ctrl Pts',(53.4930903730536,22.3072186088595,21.089933357403));
#30106=CARTESIAN_POINT('Ctrl Pts',(53.508837134781,22.3251529506211,21.0883852841783));
#30107=CARTESIAN_POINT('Ctrl Pts',(53.6234263253456,22.4510319975778,21.0772485765513));
#30108=CARTESIAN_POINT('Ctrl Pts',(53.7335461640153,22.5480725214266,21.0671618433791));
#30109=CARTESIAN_POINT('Ctrl Pts',(53.947353604871,22.6982892958558,21.0489388683708));
#30110=CARTESIAN_POINT('Ctrl Pts',(54.0469939028785,22.7561420860029,21.0408955937351));
#30111=CARTESIAN_POINT('Ctrl Pts',(54.1622700084183,22.8103560858603,21.0324335956188));
#30112=CARTESIAN_POINT('Ctrl Pts',(54.1735172351009,22.8155183703401,21.0316165697683));
#30113=CARTESIAN_POINT('Ctrl Pts',(54.193537021413,22.8244825056827,21.0301783693731));
#30114=CARTESIAN_POINT('Ctrl Pts',(54.2022901381784,22.8283265393486,21.0295549474005));
#30115=CARTESIAN_POINT('Ctrl Pts',(54.2157007015176,22.8341013014988,21.0286083928622));
#30116=CARTESIAN_POINT('Ctrl Pts',(54.2203382469923,22.8360774836633,21.028282619978));
#30117=CARTESIAN_POINT('Ctrl Pts',(54.2249951480002,22.8380410882356,21.0279570831576));
#30118=CARTESIAN_POINT('Ctrl Pts',(54.2250070003433,22.8380460856977,21.0279562546397));
#30119=CARTESIAN_POINT('Ctrl Pts',(54.2250307442186,22.8380560968752,21.0279545948851));
#30120=CARTESIAN_POINT('Ctrl Pts',(54.2250426358363,22.8380611106258,21.0279537636426));
#30121=CARTESIAN_POINT('Ctrl Pts',(54.2250664589854,22.8380711546831,21.0279520983883));
#30122=CARTESIAN_POINT('Ctrl Pts',(54.225078389809,22.8380761846906,21.0279512644262));
#30123=CARTESIAN_POINT('Ctrl Pts',(54.2251022913704,22.8380862612591,21.0279495937329));
#30124=CARTESIAN_POINT('Ctrl Pts',(54.2251142621585,22.8380913078405,21.0279487569983));
#30125=CARTESIAN_POINT('Ctrl Pts',(54.2251382431699,22.8381014173521,21.0279470807938));
#30126=CARTESIAN_POINT('Ctrl Pts',(54.225150254146,22.8381064805989,21.0279462412714));
#30127=CARTESIAN_POINT('Ctrl Pts',(54.2251743160498,22.8381166236564,21.0279445594553));
#30128=CARTESIAN_POINT('Ctrl Pts',(54.22518636697,22.8381217034631,21.0279437171623));
#30129=CARTESIAN_POINT('Ctrl Pts',(54.2252105096485,22.8381318800111,21.0279420297433));
#30130=CARTESIAN_POINT('Ctrl Pts',(54.2252226008182,22.8381369765034,21.0279411846586));
#30131=CARTESIAN_POINT('Ctrl Pts',(54.2252468237802,22.8381471863294,21.0279394916714));
#30132=CARTESIAN_POINT('Ctrl Pts',(54.2252589559682,22.8381522998288,21.0279386437415));
#30133=CARTESIAN_POINT('Ctrl Pts',(54.2252832614519,22.8381625438704,21.0279369450302));
#30134=CARTESIAN_POINT('Ctrl Pts',(54.2252954342968,22.8381676742216,21.0279360942805));
#30135=CARTESIAN_POINT('Ctrl Pts',(54.2253198208907,22.8381779518781,21.0279343899441));
#30136=CARTESIAN_POINT('Ctrl Pts',(54.2253320352925,22.8381830994576,21.027933536312));
#30137=CARTESIAN_POINT('Ctrl Pts',(54.2253565055625,22.8381934118048,21.0279318261717));
#30138=CARTESIAN_POINT('Ctrl Pts',(54.2253687610663,22.8381985764179,21.0279309696892));
#30139=CARTESIAN_POINT('Ctrl Pts',(54.225393313842,22.8382089229567,21.0279292538272));
#30140=CARTESIAN_POINT('Ctrl Pts',(54.2254056111861,22.8382141049116,21.0279283944428));
#30141=CARTESIAN_POINT('Ctrl Pts',(54.2254302477906,22.8382244861936,21.0279266727672));
#30142=CARTESIAN_POINT('Ctrl Pts',(54.2254425870652,22.8382296855255,21.027925810475));
#30143=CARTESIAN_POINT('Ctrl Pts',(54.2254673075629,22.8382401015718,21.0279240829816));
#30144=CARTESIAN_POINT('Ctrl Pts',(54.2254796891657,22.8382453184452,21.0279232177539));
#30145=CARTESIAN_POINT('Ctrl Pts',(54.2255044947943,22.8382557697714,21.0279214843568));
#30146=CARTESIAN_POINT('Ctrl Pts',(54.2255169186937,22.83826100417,21.0279206161962));
#30147=CARTESIAN_POINT('Ctrl Pts',(54.2255418089976,22.8382714905781,21.0279188769275));
#30148=CARTESIAN_POINT('Ctrl Pts',(54.2255542757953,22.8382767427523,21.0279180057921));
#30149=CARTESIAN_POINT('Ctrl Pts',(54.2255792523612,22.8382872649047,21.0279162605416));
#30150=CARTESIAN_POINT('Ctrl Pts',(54.2255917619571,22.8382925348093,21.0279153864386));
#30151=CARTESIAN_POINT('Ctrl Pts',(54.2256168241989,22.8383030924528,21.0279136352477));
#30152=CARTESIAN_POINT('Ctrl Pts',(54.225629377232,22.8383083803539,21.0279127581327));
#30153=CARTESIAN_POINT('Ctrl Pts',(54.2256545279549,22.8383189746641,21.0279110008058));
#30154=CARTESIAN_POINT('Ctrl Pts',(54.2256671237389,22.8383242802694,21.0279101207271));
#30155=CARTESIAN_POINT('Ctrl Pts',(54.2256923587314,22.8383349094659,21.027908357559));
#30156=CARTESIAN_POINT('Ctrl Pts',(54.2257049994303,22.8383402336839,21.0279074743655));
#30157=CARTESIAN_POINT('Ctrl Pts',(54.2257303246679,22.8383509002773,21.0279057049391));
#30158=CARTESIAN_POINT('Ctrl Pts',(54.2257430087781,22.8383562424714,21.0279048187363));
#30159=CARTESIAN_POINT('Ctrl Pts',(54.2257684214111,22.8383669452551,21.0279030432513));
#30160=CARTESIAN_POINT('Ctrl Pts',(54.2257811500112,22.8383723058763,21.0279021539638));
#30161=CARTESIAN_POINT('Ctrl Pts',(54.2258066517887,22.8383830455804,21.0279003722985));
#30162=CARTESIAN_POINT('Ctrl Pts',(54.2258194249518,22.8383884246562,21.0278994799217));
#30163=CARTESIAN_POINT('Ctrl Pts',(54.2258450164915,22.8383992015344,21.0278976920333));
#30164=CARTESIAN_POINT('Ctrl Pts',(54.2258578343551,22.8384045991196,21.0278967965577));
#30165=CARTESIAN_POINT('Ctrl Pts',(54.2258835147597,22.8384154127873,21.0278950025096));
#30166=CARTESIAN_POINT('Ctrl Pts',(54.2258963782554,22.8384208292708,21.0278941038705));
#30167=CARTESIAN_POINT('Ctrl Pts',(54.2259223469412,22.838431763688,21.0278922897321));
#30168=CARTESIAN_POINT('Ctrl Pts',(54.2259354515801,22.8384372813837,21.0278913742718));
#30169=CARTESIAN_POINT('Ctrl Pts',(54.2259618723448,22.8384484054889,21.0278895286029));
#30170=CARTESIAN_POINT('Ctrl Pts',(54.2259751888655,22.8384540120593,21.027888598367));
#30171=CARTESIAN_POINT('Ctrl Pts',(54.2260020374324,22.838465315598,21.0278867228658));
#30172=CARTESIAN_POINT('Ctrl Pts',(54.2260155689803,22.8384710123509,21.0278857776358));
#30173=CARTESIAN_POINT('Ctrl Pts',(54.22988310725,22.840099187491,21.0276156192607));
#30174=CARTESIAN_POINT('Ctrl Pts',(54.2337421568283,22.8417095228866,21.0273471556168));
#30175=CARTESIAN_POINT('Ctrl Pts',(54.2424559505845,22.8453135553225,21.0267434228915));
#30176=CARTESIAN_POINT('Ctrl Pts',(54.2473135065905,22.8473002323446,21.0264085780969));
#30177=CARTESIAN_POINT('Ctrl Pts',(54.259832454678,22.8523627406793,21.0255498640903));
#30178=CARTESIAN_POINT('Ctrl Pts',(54.2675052925616,22.8554102585024,21.0250276423215));
#30179=CARTESIAN_POINT('Ctrl Pts',(54.3149519512032,22.8739150443583,21.021822183402));
#30180=CARTESIAN_POINT('Ctrl Pts',(54.3551975520365,22.8881416333466,21.019206035753));
#30181=CARTESIAN_POINT('Ctrl Pts',(54.5817331220043,22.9601309526944,21.0048847124341));
#30182=CARTESIAN_POINT('Ctrl Pts',(54.7752579932607,22.9916237211284,20.994046820029));
#30183=CARTESIAN_POINT('Ctrl Pts',(55.0241517734538,22.9953310106371,20.9790903481579));
#30184=CARTESIAN_POINT('Ctrl Pts',(55.0780184315487,22.993951225774,20.9758013057958));
#30185=CARTESIAN_POINT('Ctrl Pts',(55.1426627704664,22.9896719049851,20.9717628580345));
#30186=CARTESIAN_POINT('Ctrl Pts',(55.1535592789421,22.9888606018617,20.9710790367903));
#30187=CARTESIAN_POINT('Ctrl Pts',(55.164448351653,22.9879598341362,20.9703924394033));
#30188=CARTESIAN_POINT('Ctrl Pts',(55.1644479523467,22.9879598671676,20.810886410834));
#30189=CARTESIAN_POINT('Ctrl Pts',(55.0607747998254,22.996535914364,20.8169274332477));
#30190=CARTESIAN_POINT('Ctrl Pts',(54.9565102499621,22.9969957235706,20.8229336150651));
#30191=CARTESIAN_POINT('Ctrl Pts',(54.7871697271686,22.9844485452913,20.8330572124156));
#30192=CARTESIAN_POINT('Ctrl Pts',(54.7220202242319,22.9763751295009,20.8370398260191));
#30193=CARTESIAN_POINT('Ctrl Pts',(54.6428512111315,22.9625723296193,20.8420434974395));
#30194=CARTESIAN_POINT('Ctrl Pts',(54.6283399102779,22.9598760587348,20.8429673847499));
#30195=CARTESIAN_POINT('Ctrl Pts',(54.6054820931037,22.9553659781349,20.8444338846554));
#30196=CARTESIAN_POINT('Ctrl Pts',(54.5971148275945,22.9536591364652,20.8449730902119));
#30197=CARTESIAN_POINT('Ctrl Pts',(54.5814541126815,22.9503596158121,20.8459868844609));
#30198=CARTESIAN_POINT('Ctrl Pts',(54.5741581212833,22.9487796136636,20.8464610603752));
#30199=CARTESIAN_POINT('Ctrl Pts',(54.5578435286914,22.9451505725202,20.8475256388784));
#30200=CARTESIAN_POINT('Ctrl Pts',(54.54883000943,22.9430797023654,20.8481167320197));
#30201=CARTESIAN_POINT('Ctrl Pts',(54.5259819443459,22.9376627757252,20.8496226781042));
#30202=CARTESIAN_POINT('Ctrl Pts',(54.512168395776,22.934231231783,20.8505402554928));
#30203=CARTESIAN_POINT('Ctrl Pts',(54.4295138122808,22.9127565646085,20.8560744079859));
#30204=CARTESIAN_POINT('Ctrl Pts',(54.3616495662766,22.8911897913354,20.8608038358385));
#30205=CARTESIAN_POINT('Ctrl Pts',(54.1408558293645,22.8077835037583,20.8768148038097));
#30206=CARTESIAN_POINT('Ctrl Pts',(53.9944622246104,22.7306340577721,20.8885199670784));
#30207=CARTESIAN_POINT('Ctrl Pts',(53.8166267864544,22.606659065544,20.9033580391712));
#30208=CARTESIAN_POINT('Ctrl Pts',(53.7751892755048,22.5752984623301,20.9068594888647));
#30209=CARTESIAN_POINT('Ctrl Pts',(53.7279255786372,22.5365345459115,20.9108634338554));
#30210=CARTESIAN_POINT('Ctrl Pts',(53.720871427009,22.5306671244297,20.9114612925065));
#30211=CARTESIAN_POINT('Ctrl Pts',(53.7100651988452,22.5215519675486,20.9123772290469));
#30212=CARTESIAN_POINT('Ctrl Pts',(53.7062844471068,22.5183386482216,20.9126977008354));
#30213=CARTESIAN_POINT('Ctrl Pts',(53.6993400526779,22.5123917297111,20.9132862998663));
#30214=CARTESIAN_POINT('Ctrl Pts',(53.696173029607,22.5096623048016,20.9135547124873));
#30215=CARTESIAN_POINT('Ctrl Pts',(53.6890428222301,22.5034781279048,20.9141589873155));
#30216=CARTESIAN_POINT('Ctrl Pts',(53.6850847075932,22.5000176593484,20.9144944208466));
#30217=CARTESIAN_POINT('Ctrl Pts',(53.6734401596926,22.4897556485784,20.9154813764055));
#30218=CARTESIAN_POINT('Ctrl Pts',(53.6657923467358,22.4829102639633,20.9161297485774));
#30219=CARTESIAN_POINT('Ctrl Pts',(53.6048867112353,22.4275423767511,20.9212978745806));
#30220=CARTESIAN_POINT('Ctrl Pts',(53.5542341825184,22.3762201717164,20.9256253066365));
#30221=CARTESIAN_POINT('Ctrl Pts',(53.4271726144829,22.2327004626461,20.9369275071537));
#30222=CARTESIAN_POINT('Ctrl Pts',(53.3560959872718,22.1361855191913,20.9437532269365));
#30223=CARTESIAN_POINT('Ctrl Pts',(53.2499066655382,21.9609729685995,20.9557888787442));
#30224=CARTESIAN_POINT('Ctrl Pts',(53.2104437629289,21.8853144724378,20.9608834796954));
#30225=CARTESIAN_POINT('Ctrl Pts',(53.1673086845007,21.7878611814792,20.9674673932946));
#30226=CARTESIAN_POINT('Ctrl Pts',(53.1589876256663,21.76821616887,20.9687953401201));
#30227=CARTESIAN_POINT('Ctrl Pts',(53.14727819746,21.7392881761845,20.9707535662719));
#30228=CARTESIAN_POINT('Ctrl Pts',(53.1436409897681,21.730107050058,20.9713754655968));
#30229=CARTESIAN_POINT('Ctrl Pts',(53.137348871242,21.7138733203298,20.9724759578109));
#30230=CARTESIAN_POINT('Ctrl Pts',(53.1346654511749,21.7068319201607,20.9729535847927));
#30231=CARTESIAN_POINT('Ctrl Pts',(53.1291518034536,21.6921138118543,20.9739526086676));
#30232=CARTESIAN_POINT('Ctrl Pts',(53.1263287859798,21.6844345706829,20.9744742354621));
#30233=CARTESIAN_POINT('Ctrl Pts',(53.1190980852496,21.6643854226842,20.9758372133588));
#30234=CARTESIAN_POINT('Ctrl Pts',(53.114765224729,21.6519891342783,20.9766810252979));
#30235=CARTESIAN_POINT('Ctrl Pts',(53.0975028005418,21.6009902497448,20.9801575439806));
#30236=CARTESIAN_POINT('Ctrl Pts',(53.0856348185771,21.5620413017555,20.9828246855955));
#30237=CARTESIAN_POINT('Ctrl Pts',(53.028566217451,21.3518890833527,20.9972889867062));
#30238=CARTESIAN_POINT('Ctrl Pts',(53.0051280468784,21.1756195821554,21.0097777439398));
#30239=CARTESIAN_POINT('Ctrl Pts',(53.0052524267199,20.9958016574577,21.0222204356035));
#30240=CARTESIAN_POINT('Ctrl Pts',(53.0052603502379,20.9929831433015,21.0224153664104));
#30241=CARTESIAN_POINT('Ctrl Pts',(53.0056217097114,20.9196951694295,21.0274813119119));
#30242=CARTESIAN_POINT('Ctrl Pts',(53.0097033071661,20.8492852761408,21.0322848098706));
#30243=CARTESIAN_POINT('Ctrl Pts',(53.0186359288415,20.7690703041183,21.0375831626515));
#30244=CARTESIAN_POINT('Ctrl Pts',(53.019845685345,20.7589170107111,21.0382505606658));
#30245=CARTESIAN_POINT('Ctrl Pts',(53.0217945846738,20.7435658944533,21.0392542530492));
#30246=CARTESIAN_POINT('Ctrl Pts',(53.0224762402142,20.7383611329974,21.039593616657));
#30247=CARTESIAN_POINT('Ctrl Pts',(53.0237376682904,20.7290161721705,21.040201175821));
#30248=CARTESIAN_POINT('Ctrl Pts',(53.0243099149544,20.7248750692493,21.040469782762));
#30249=CARTESIAN_POINT('Ctrl Pts',(53.0255907784974,20.7158161258814,21.0410560055694));
#30250=CARTESIAN_POINT('Ctrl Pts',(53.0263047505476,20.7108991320484,21.0413733172875));
#30251=CARTESIAN_POINT('Ctrl Pts',(53.0283941097554,20.6968786728761,21.042275737437));
#30252=CARTESIAN_POINT('Ctrl Pts',(53.0298141815836,20.687781848586,21.0428583943469));
#30253=CARTESIAN_POINT('Ctrl Pts',(53.0397818503727,20.6267078666301,21.046752979971));
#30254=CARTESIAN_POINT('Ctrl Pts',(53.0503232228468,20.5750720645046,21.0499618260359));
#30255=CARTESIAN_POINT('Ctrl Pts',(53.1039549720638,20.3568568521578,21.06339359009));
#30256=CARTESIAN_POINT('Ctrl Pts',(53.1664488662943,20.1958125201965,21.0730432686712));
#30257=CARTESIAN_POINT('Ctrl Pts',(53.2795393011145,19.9884895491317,21.0871270167766));
#30258=CARTESIAN_POINT('Ctrl Pts',(53.3129355221435,19.9337211433496,21.0910184663241));
#30259=CARTESIAN_POINT('Ctrl Pts',(53.3573943226106,19.8681418585539,21.095947964784));
#30260=CARTESIAN_POINT('Ctrl Pts',(53.3660223049345,19.8557215653789,21.0968940302188));
#30261=CARTESIAN_POINT('Ctrl Pts',(53.3798399594767,19.8363055184964,21.0983933471359));
#30262=CARTESIAN_POINT('Ctrl Pts',(53.3849357712523,19.8292434342186,21.0989430068283));
#30263=CARTESIAN_POINT('Ctrl Pts',(53.3944359884939,19.8162575216839,21.0999618720456));
#30264=CARTESIAN_POINT('Ctrl Pts',(53.3988273641279,19.8103243140464,21.1004305672717));
#30265=CARTESIAN_POINT('Ctrl Pts',(53.4086466367444,19.7972103007902,21.1014736744091));
#30266=CARTESIAN_POINT('Ctrl Pts',(53.4140903863336,19.7900416204828,21.1020487005374));
#30267=CARTESIAN_POINT('Ctrl Pts',(53.4299018347962,19.7695101116523,21.1037097077394));
#30268=CARTESIAN_POINT('Ctrl Pts',(53.4403910053048,19.7562422389693,21.1048004714814));
#30269=CARTESIAN_POINT('Ctrl Pts',(53.5294789626568,19.646453003812,21.1139754182195));
#30270=CARTESIAN_POINT('Ctrl Pts',(53.616770879032,19.5573674759639,21.1224223843391));
#30271=CARTESIAN_POINT('Ctrl Pts',(53.8135955734517,19.3908833003054,21.1403054012116));
#30272=CARTESIAN_POINT('Ctrl Pts',(53.9237962988855,19.3151855115299,21.1497241419293));
#30273=CARTESIAN_POINT('Ctrl Pts',(54.0670432726131,19.236616875302,21.1607240020551));
#30274=CARTESIAN_POINT('Ctrl Pts',(54.0936814613359,19.2227787874426,21.1627197828048));
#30275=CARTESIAN_POINT('Ctrl Pts',(54.1279498230423,19.2059479731373,21.165215402546));
#30276=CARTESIAN_POINT('Ctrl Pts',(54.1352983669861,19.2023945712077,21.1657464343511));
#30277=CARTESIAN_POINT('Ctrl Pts',(54.1469496903084,19.1968485334546,21.166581646576));
#30278=CARTESIAN_POINT('Ctrl Pts',(54.1512380200002,19.1948260071072,21.1668876135982));
#30279=CARTESIAN_POINT('Ctrl Pts',(54.1593501879724,19.1910353228318,21.1674636400885));
#30280=CARTESIAN_POINT('Ctrl Pts',(54.1631723725153,19.1892640082249,21.1677338828896));
#30281=CARTESIAN_POINT('Ctrl Pts',(54.1720788830915,19.1851706892469,21.168360949825));
#30282=CARTESIAN_POINT('Ctrl Pts',(54.1771673837641,19.1828579333268,21.1687172061123));
#30283=CARTESIAN_POINT('Ctrl Pts',(54.1935110091238,19.175512380475,21.1698552619206));
#30284=CARTESIAN_POINT('Ctrl Pts',(54.2048033565135,19.1705624136211,21.1706321985194));
#30285=CARTESIAN_POINT('Ctrl Pts',(54.3130659566382,19.1242976845961,21.1779983881825));
#30286=CARTESIAN_POINT('Ctrl Pts',(54.4131355355802,19.0906195111814,21.1841829062938));
#30287=CARTESIAN_POINT('Ctrl Pts',(54.6765656156305,19.0246474760511,21.1999787370729));
#30288=CARTESIAN_POINT('Ctrl Pts',(54.8421114337565,19.0045820930814,21.2095028665368));
#30289=CARTESIAN_POINT('Ctrl Pts',(55.0312670312721,19.0053619564736,21.2211675716505));
#30290=CARTESIAN_POINT('Ctrl Pts',(55.0543058831779,19.0058562352423,21.2226001082778));
#30291=CARTESIAN_POINT('Ctrl Pts',(55.0864909194811,19.0071048881377,21.2246199266721));
#30292=CARTESIAN_POINT('Ctrl Pts',(55.0956488701582,19.007523426694,21.2251967483059));
#30293=CARTESIAN_POINT('Ctrl Pts',(55.1124205152232,19.0084058219758,21.2262571184485));
#30294=CARTESIAN_POINT('Ctrl Pts',(55.1200350921361,19.0088502526915,21.2267400516506));
#30295=CARTESIAN_POINT('Ctrl Pts',(55.1354650635701,19.0098396660368,21.2277217957827));
#30296=CARTESIAN_POINT('Ctrl Pts',(55.1432801648812,19.0103870402011,21.2282206733199));
#30297=CARTESIAN_POINT('Ctrl Pts',(55.1625749229147,19.0118527264968,21.2294564913953));
#30298=CARTESIAN_POINT('Ctrl Pts',(55.1740501233725,19.0128244335148,21.2301950923758));
#30299=CARTESIAN_POINT('Ctrl Pts',(55.2168979160124,19.0168267173064,21.232966910265));
#30300=CARTESIAN_POINT('Ctrl Pts',(55.2482042892155,19.0205012205246,21.2350201391712));
#30301=CARTESIAN_POINT('Ctrl Pts',(55.3262796039344,19.0315462930793,21.2402139339355));
#30302=CARTESIAN_POINT('Ctrl Pts',(55.3728959275262,19.0398427568471,21.2433815418917));
#30303=CARTESIAN_POINT('Ctrl Pts',(55.6011945313129,19.0889122944167,21.2592164764453));
#30304=CARTESIAN_POINT('Ctrl Pts',(55.7768184069374,19.1533185692433,21.2725258087657));
#30305=CARTESIAN_POINT('Ctrl Pts',(55.9698275937065,19.2565740163141,21.2873009953332));
#30306=CARTESIAN_POINT('Ctrl Pts',(55.9983168572191,19.2727294738059,21.2894827237641));
#30307=CARTESIAN_POINT('Ctrl Pts',(56.0335291870929,19.2938598645046,21.2921685141227));
#30308=CARTESIAN_POINT('Ctrl Pts',(56.040634390702,19.2981842599001,21.292709890484));
#30309=CARTESIAN_POINT('Ctrl Pts',(56.0518175443412,19.3050868201141,21.2935608294094));
#30310=CARTESIAN_POINT('Ctrl Pts',(56.0559134506624,19.3076354943915,21.2938722448973));
#30311=CARTESIAN_POINT('Ctrl Pts',(56.0631986742712,19.3122054633305,21.2944256496041));
#30312=CARTESIAN_POINT('Ctrl Pts',(56.0663914773328,19.3142209408065,21.2946680067641));
#30313=CARTESIAN_POINT('Ctrl Pts',(56.0739884292041,19.319046785339,21.2952442704191));
#30314=CARTESIAN_POINT('Ctrl Pts',(56.0783872735819,19.3218653970495,21.2955776266578));
#30315=CARTESIAN_POINT('Ctrl Pts',(56.0915406858704,19.3303666790431,21.296573638163));
#30316=CARTESIAN_POINT('Ctrl Pts',(56.1002619431771,19.3361009156461,21.2972329814958));
#30317=CARTESIAN_POINT('Ctrl Pts',(56.1202460294453,19.3494663094813,21.298742363761));
#30318=CARTESIAN_POINT('Ctrl Pts',(56.1314767223204,19.3571448393298,21.2995895330275));
#30319=CARTESIAN_POINT('Ctrl Pts',(56.2619017494144,19.448289590134,21.3094263295463));
#30320=CARTESIAN_POINT('Ctrl Pts',(56.3717131834456,19.5444534397024,21.3177161122047));
#30321=CARTESIAN_POINT('Ctrl Pts',(56.5540551939484,19.743269896032,21.3334073631076));
#30322=CARTESIAN_POINT('Ctrl Pts',(56.6292704697401,19.8424466390739,21.3407275117804));
#30323=CARTESIAN_POINT('Ctrl Pts',(56.7029816580882,19.9611913644653,21.3494017022039));
#30324=CARTESIAN_POINT('Ctrl Pts',(56.7110366769455,19.9745131021159,21.3503732839847));
#30325=CARTESIAN_POINT('Ctrl Pts',(56.7238322627505,19.996245514217,21.3519564735784));
#30326=CARTESIAN_POINT('Ctrl Pts',(56.7286692408183,20.0045988806489,21.3525645841544));
#30327=CARTESIAN_POINT('Ctrl Pts',(56.7371592383367,20.0195094696699,21.3536494538004));
#30328=CARTESIAN_POINT('Ctrl Pts',(56.7408362584413,20.0260528668419,21.3541253385847));
#30329=CARTESIAN_POINT('Ctrl Pts',(56.7484968557265,20.0398671750079,21.3551296727905));
#30330=CARTESIAN_POINT('Ctrl Pts',(56.7524721997206,20.0471424650565,21.3556584046452));
#30331=CARTESIAN_POINT('Ctrl Pts',(56.7628611281296,20.0664402124841,21.3570604589492));
#30332=CARTESIAN_POINT('Ctrl Pts',(56.7691969863179,20.0785038023653,21.3579365093459));
#30333=CARTESIAN_POINT('Ctrl Pts',(56.7984458378421,20.1356078710089,21.3620821703625));
#30334=CARTESIAN_POINT('Ctrl Pts',(56.8197637408343,20.1814400748867,21.365406704984));
#30335=CARTESIAN_POINT('Ctrl Pts',(56.9048436615531,20.3841535851292,21.3801096309927));
#30336=CARTESIAN_POINT('Ctrl Pts',(56.9502184612566,20.5479734915179,21.3920666625641));
#30337=CARTESIAN_POINT('Ctrl Pts',(56.9843732330964,20.7850104029219,21.4086188480275));
#30338=CARTESIAN_POINT('Ctrl Pts',(56.9907118387547,20.8549957456817,21.4134042527843));
#30339=CARTESIAN_POINT('Ctrl Pts',(56.9937294037265,20.9353857572704,21.4186851829452));
#30340=CARTESIAN_POINT('Ctrl Pts',(56.994034192838,20.9455979405845,21.4193520264535));
#30341=CARTESIAN_POINT('Ctrl Pts',(56.9943767550672,20.9610583036605,21.4203550522592));
#30342=CARTESIAN_POINT('Ctrl Pts',(56.994472294889,20.9663048472962,21.4206942978672));
#30343=CARTESIAN_POINT('Ctrl Pts',(56.9946067502484,20.9757317128183,21.4213017325349));
#30344=CARTESIAN_POINT('Ctrl Pts',(56.9946532289398,20.9799118152751,21.4215703322063));
#30345=CARTESIAN_POINT('Ctrl Pts',(56.99472620223,20.9890619470939,21.4221566404961));
#30346=CARTESIAN_POINT('Ctrl Pts',(56.99474726377,20.9940319312183,21.4224740443147));
#30347=CARTESIAN_POINT('Ctrl Pts',(56.994754359979,21.0082155637527,21.4233769903446));
#30348=CARTESIAN_POINT('Ctrl Pts',(56.9946951348694,21.0174292525742,21.4239600765463));
#30349=CARTESIAN_POINT('Ctrl Pts',(56.9938663718061,21.0794742271517,21.4278652099643));
#30350=CARTESIAN_POINT('Ctrl Pts',(56.9910617767251,21.1322624146185,21.4310835330584));
#30351=CARTESIAN_POINT('Ctrl Pts',(56.9700641526076,21.3578375476791,21.4446236098807));
#30352=CARTESIAN_POINT('Ctrl Pts',(56.9314432155635,21.5279536848423,21.4543625777956));
#30353=CARTESIAN_POINT('Ctrl Pts',(56.8496301055514,21.7495326483003,21.4684633052654));
#30354=CARTESIAN_POINT('Ctrl Pts',(56.8252509618901,21.8070864101332,21.4722582973101));
#30355=CARTESIAN_POINT('Ctrl Pts',(56.7917169003763,21.8769283875758,21.4770794163882));
#30356=CARTESIAN_POINT('Ctrl Pts',(56.7850678907986,21.8903850031676,21.4780184950567));
#30357=CARTESIAN_POINT('Ctrl Pts',(56.7743338627806,21.9115055111915,21.4795091565845));
#30358=CARTESIAN_POINT('Ctrl Pts',(56.7703494838012,21.9192201340762,21.4800572170207));
#30359=CARTESIAN_POINT('Ctrl Pts',(56.7628511511322,21.9335089427907,21.4810790941734));
#30360=CARTESIAN_POINT('Ctrl Pts',(56.7593504551725,21.9400899428951,21.4815524363039));
#30361=CARTESIAN_POINT('Ctrl Pts',(56.7515117324157,21.9546289122639,21.4826042289621));
#30362=CARTESIAN_POINT('Ctrl Pts',(56.74715620859,21.9625772110469,21.4831832945347));
#30363=CARTESIAN_POINT('Ctrl Pts',(56.734373421082,21.9855316321404,21.4848675933793));
#30364=CARTESIAN_POINT('Ctrl Pts',(56.7258060968734,22.0004584183694,21.4859778196608));
#30365=CARTESIAN_POINT('Ctrl Pts',(56.6405111098911,22.1447108748809,21.4968565678298));
#30366=CARTESIAN_POINT('Ctrl Pts',(56.5495998539401,22.2650544288523,21.5071694225535));
#30367=CARTESIAN_POINT('Ctrl Pts',(56.3598350097278,22.4647680912651,21.5263720659762));
#30368=CARTESIAN_POINT('Ctrl Pts',(56.2652530472732,22.5472029663485,21.5351529765438));
#30369=CARTESIAN_POINT('Ctrl Pts',(56.1509071064076,22.6293198204467,21.544474575585));
#30370=CARTESIAN_POINT('Ctrl Pts',(56.138147191481,22.6382586033366,21.5454979167646));
#30371=CARTESIAN_POINT('Ctrl Pts',(56.1200640508208,22.6506132321084,21.546923200572));
#30372=CARTESIAN_POINT('Ctrl Pts',(56.1148276929897,22.6541543874514,21.5473330198673));
#30373=CARTESIAN_POINT('Ctrl Pts',(56.1063278124381,22.659843847393,21.5479934602868));
#30374=CARTESIAN_POINT('Ctrl Pts',(56.1030747080913,22.6620075256498,21.5482450978259));
#30375=CARTESIAN_POINT('Ctrl Pts',(56.0961762140934,22.6665666192721,21.5487762975754));
#30376=CARTESIAN_POINT('Ctrl Pts',(56.0925292833072,22.6689596623734,21.5490556954033));
#30377=CARTESIAN_POINT('Ctrl Pts',(56.0834826152054,22.6748535450024,21.5497453358728));
#30378=CARTESIAN_POINT('Ctrl Pts',(56.0780736755366,22.6783402895473,21.5501546482921));
#30379=CARTESIAN_POINT('Ctrl Pts',(56.057853627364,22.6912365795538,21.5516739254081));
#30380=CARTESIAN_POINT('Ctrl Pts',(56.0429349256264,22.7004770670982,21.5527733145567));
#30381=CARTESIAN_POINT('Ctrl Pts',(56.0049592949829,22.7233109551089,21.5555229530364));
#30382=CARTESIAN_POINT('Ctrl Pts',(55.9817465824911,22.736639750144,21.5571590397498));
#30383=CARTESIAN_POINT('Ctrl Pts',(55.8049074105282,22.8335017918676,21.5693444579776));
#30384=CARTESIAN_POINT('Ctrl Pts',(55.6411540643684,22.896981199066,21.5791308292728));
#30385=CARTESIAN_POINT('Ctrl Pts',(55.4447679317786,22.9447234839942,21.5911137334633));
#30386=CARTESIAN_POINT('Ctrl Pts',(55.4182001129528,22.9506092706598,21.5927380726587));
#30387=CARTESIAN_POINT('Ctrl Pts',(55.3425947421727,22.9657431390859,21.5973810647784));
#30388=CARTESIAN_POINT('Ctrl Pts',(55.293321824915,22.9736967658627,21.6004316912233));
#30389=CARTESIAN_POINT('Ctrl Pts',(55.2297754113078,22.9815223062263,21.6044215584806));
#30390=CARTESIAN_POINT('Ctrl Pts',(55.2157276950928,22.9831008383366,21.6053069753338));
#30391=CARTESIAN_POINT('Ctrl Pts',(55.193304867483,22.985379409242,21.6067261868673));
#30392=CARTESIAN_POINT('Ctrl Pts',(55.1849398880045,22.9861760759709,21.6072569419339));
#30393=CARTESIAN_POINT('Ctrl Pts',(55.1725306376143,22.9872788402075,21.6080463271743));
#30394=CARTESIAN_POINT('Ctrl Pts',(55.1684899938156,22.9876255007255,21.6083036807173));
#30395=CARTESIAN_POINT('Ctrl Pts',(55.1644483516286,22.9879598341382,21.6085614209934));
#30396=CARTESIAN_POINT('Origin',(55.,21.,6.22095488139522));
#30397=CARTESIAN_POINT('',(55.1644483539992,22.9879598339421,22.5673314474745));
#30398=CARTESIAN_POINT('',(55.1644481205599,22.9879598532527,22.4107149109706));
#30399=CARTESIAN_POINT('',(55.1644483516311,22.987959834138,6.22095488139522));
#30400=CARTESIAN_POINT('Ctrl Pts',(55.1644483539992,22.9879598339421,22.5673314474745));
#30401=CARTESIAN_POINT('Ctrl Pts',(55.186432793039,22.986141233409,22.5658143404452));
#30402=CARTESIAN_POINT('Ctrl Pts',(55.2083957798684,22.9839572318376,22.5643048457936));
#30403=CARTESIAN_POINT('Ctrl Pts',(55.256762560822,22.9783348456478,22.5609999925179));
#30404=CARTESIAN_POINT('Ctrl Pts',(55.2831340326463,22.9747331557386,22.5592108152993));
#30405=CARTESIAN_POINT('Ctrl Pts',(55.3266898114089,22.9678939729726,22.5562851459592));
#30406=CARTESIAN_POINT('Ctrl Pts',(55.3439171797484,22.9649564741999,22.5551356491862));
#30407=CARTESIAN_POINT('Ctrl Pts',(55.3674242420906,22.9606295627408,22.5535796769631));
#30408=CARTESIAN_POINT('Ctrl Pts',(55.3737385194787,22.9594357294347,22.5531629670468));
#30409=CARTESIAN_POINT('Ctrl Pts',(55.3843280287401,22.9573805317714,22.552466327442));
#30410=CARTESIAN_POINT('Ctrl Pts',(55.3886063608675,22.9565356314759,22.5521854817854));
#30411=CARTESIAN_POINT('Ctrl Pts',(55.3967153781305,22.9549065858725,22.5516543737523));
#30412=CARTESIAN_POINT('Ctrl Pts',(55.4005465732233,22.9541251991764,22.5514039524426));
#30413=CARTESIAN_POINT('Ctrl Pts',(55.4105778031784,22.952048551499,22.5507495425099));
#30414=CARTESIAN_POINT('Ctrl Pts',(55.4167740706285,22.9507350041827,22.5503465867116));
#30415=CARTESIAN_POINT('Ctrl Pts',(55.4382556611008,22.9460740938313,22.5489536808659));
#30416=CARTESIAN_POINT('Ctrl Pts',(55.4535082362513,22.9425763095891,22.5479718670198));
#30417=CARTESIAN_POINT('Ctrl Pts',(55.5895301826335,22.9096937250625,22.5392676660209));
#30418=CARTESIAN_POINT('Ctrl Pts',(55.7073653737135,22.8692562263404,22.5320814118752));
#30419=CARTESIAN_POINT('Ctrl Pts',(55.9150440257904,22.7755113217992,22.5188622893732));
#30420=CARTESIAN_POINT('Ctrl Pts',(56.0059423165852,22.7256372722638,22.5128573205838));
#30421=CARTESIAN_POINT('Ctrl Pts',(56.1220667603981,22.6496175422141,22.5045152693617));
#30422=CARTESIAN_POINT('Ctrl Pts',(56.1510606292004,22.6295186605663,22.5023725840844));
#30423=CARTESIAN_POINT('Ctrl Pts',(56.1998664097338,22.5937332342405,22.4986489231873));
#30424=CARTESIAN_POINT('Ctrl Pts',(56.2199415630545,22.5784193094521,22.497081750701));
#30425=CARTESIAN_POINT('Ctrl Pts',(56.2479963034211,22.5561633572653,22.4948376907151));
#30426=CARTESIAN_POINT('Ctrl Pts',(56.2562202119917,22.5495321680906,22.4941731170456));
#30427=CARTESIAN_POINT('Ctrl Pts',(56.2703077222298,22.537987117644,22.4930227805335));
#30428=CARTESIAN_POINT('Ctrl Pts',(56.276196499834,22.533104228143,22.4925382733645));
#30429=CARTESIAN_POINT('Ctrl Pts',(56.287418532211,22.5236896218897,22.4916078660918));
#30430=CARTESIAN_POINT('Ctrl Pts',(56.2927563201373,22.5191634657357,22.4911621975115));
#30431=CARTESIAN_POINT('Ctrl Pts',(56.3052296449744,22.5084734153937,22.4901133453566));
#30432=CARTESIAN_POINT('Ctrl Pts',(56.3123454654043,22.5022868718878,22.489509232005));
#30433=CARTESIAN_POINT('Ctrl Pts',(56.3367487826879,22.4807647644597,22.4874172586597));
#30434=CARTESIAN_POINT('Ctrl Pts',(56.3538129422668,22.4651798656036,22.4859190267315));
#30435=CARTESIAN_POINT('Ctrl Pts',(56.4868386154005,22.3393778084727,22.4739499211205));
#30436=CARTESIAN_POINT('Ctrl Pts',(56.5894079160468,22.2158885896307,22.4628709241762));
#30437=CARTESIAN_POINT('Ctrl Pts',(56.7322939258679,21.9944456003329,22.4444902770158));
#30438=CARTESIAN_POINT('Ctrl Pts',(56.781609773601,21.9031251905772,22.4372784732087));
#30439=CARTESIAN_POINT('Ctrl Pts',(56.8306760746122,21.7924372089665,22.4292445757396));
#30440=CARTESIAN_POINT('Ctrl Pts',(56.8375335377547,21.7764033538807,22.4280975714684));
#30441=CARTESIAN_POINT('Ctrl Pts',(56.8466273112094,21.7543449879316,22.4265443965355));
#30442=CARTESIAN_POINT('Ctrl Pts',(56.8490458531047,21.7483971026065,22.4261280379886));
#30443=CARTESIAN_POINT('Ctrl Pts',(56.8530583666099,21.7383909940816,22.4254318207307));
#30444=CARTESIAN_POINT('Ctrl Pts',(56.8546678119975,21.7343390759437,22.4251510484128));
#30445=CARTESIAN_POINT('Ctrl Pts',(56.8576957873248,21.7266424290724,22.4246199557235));
#30446=CARTESIAN_POINT('Ctrl Pts',(56.8591168997318,21.7229987633105,22.424369477113));
#30447=CARTESIAN_POINT('Ctrl Pts',(56.8628132478653,21.7134385381294,22.4237146897338));
#30448=CARTESIAN_POINT('Ctrl Pts',(56.8650710359686,21.707515213637,22.4233114161112));
#30449=CARTESIAN_POINT('Ctrl Pts',(56.8728146583173,21.6869050946895,22.4219162867283));
#30450=CARTESIAN_POINT('Ctrl Pts',(56.8781557215798,21.6721640238599,22.4209326017128));
#30451=CARTESIAN_POINT('Ctrl Pts',(56.9238985156207,21.5411120730095,22.4122993674739));
#30452=CARTESIAN_POINT('Ctrl Pts',(56.9536298756021,21.4213389799999,22.4051756549556));
#30453=CARTESIAN_POINT('Ctrl Pts',(56.9949659144926,21.1492202161439,22.3892073187235));
#30454=CARTESIAN_POINT('Ctrl Pts',(57.0005342842458,20.9967693489157,22.3803749343104));
#30455=CARTESIAN_POINT('Ctrl Pts',(56.9873879101523,20.8279043227772,22.3698632487092));
#30456=CARTESIAN_POINT('Ctrl Pts',(56.9858185384235,20.8106528839217,22.3687815087444));
#30457=CARTESIAN_POINT('Ctrl Pts',(56.9830835419132,20.7843850042937,22.3671215044268));
#30458=CARTESIAN_POINT('Ctrl Pts',(56.9820806023704,20.7753521825726,22.366548343963));
#30459=CARTESIAN_POINT('Ctrl Pts',(56.9801423910683,20.7589205802785,22.3655013317745));
#30460=CARTESIAN_POINT('Ctrl Pts',(56.9792272836039,20.7515195523053,22.3650281228777));
#30461=CARTESIAN_POINT('Ctrl Pts',(56.9771589418926,20.7355284535045,22.3640020982716));
#30462=CARTESIAN_POINT('Ctrl Pts',(56.975991183469,20.7269404472431,22.3634488334084));
#30463=CARTESIAN_POINT('Ctrl Pts',(56.972659003923,20.703576258734,22.3619374071075));
#30464=CARTESIAN_POINT('Ctrl Pts',(56.970384590497,20.6888165725106,22.360975795742));
#30465=CARTESIAN_POINT('Ctrl Pts',(56.9579208864861,20.6135582510611,22.3560367769279));
#30466=CARTESIAN_POINT('Ctrl Pts',(56.9451111442671,20.5535330703515,22.3519773049891));
#30467=CARTESIAN_POINT('Ctrl Pts',(56.8852156597996,20.3250407551035,22.3360510705103));
#30468=CARTESIAN_POINT('Ctrl Pts',(56.8188212607718,20.1624539020487,22.323624433701));
#30469=CARTESIAN_POINT('Ctrl Pts',(56.7058461536601,19.9646643552094,22.3080240171846));
#30470=CARTESIAN_POINT('Ctrl Pts',(56.6777623502385,19.9197474425884,22.3044526377261));
#30471=CARTESIAN_POINT('Ctrl Pts',(56.6427262691075,19.8683803734763,22.3003794866864));
#30472=CARTESIAN_POINT('Ctrl Pts',(56.6374780034222,19.8607992404511,22.2997786478299));
#30473=CARTESIAN_POINT('Ctrl Pts',(56.6293187819763,19.849186117349,22.2988590682349));
#30474=CARTESIAN_POINT('Ctrl Pts',(56.6264450841888,19.8451282862459,22.2985379051383));
#30475=CARTESIAN_POINT('Ctrl Pts',(56.6211267593407,19.8376777217778,22.2979485680108));
#30476=CARTESIAN_POINT('Ctrl Pts',(56.618686648255,19.8342819450345,22.2976801043787));
#30477=CARTESIAN_POINT('Ctrl Pts',(56.613159982681,19.8266415831078,22.2970763719475));
#30478=CARTESIAN_POINT('Ctrl Pts',(56.6100673510037,19.8224014984017,22.2967415274334));
#30479=CARTESIAN_POINT('Ctrl Pts',(56.6009057007454,19.809944180552,22.2957581946121));
#30480=CARTESIAN_POINT('Ctrl Pts',(56.5947901440049,19.8017611577271,22.295112820871));
#30481=CARTESIAN_POINT('Ctrl Pts',(56.5462118519476,19.7377909432844,22.2900689454476));
#30482=CARTESIAN_POINT('Ctrl Pts',(56.5008926521083,19.6842240660056,22.285852462382));
#30483=CARTESIAN_POINT('Ctrl Pts',(56.3368445128139,19.5098553343201,22.2717206005191));
#30484=CARTESIAN_POINT('Ctrl Pts',(56.2056289350415,19.4018305251734,22.2621769037627));
#30485=CARTESIAN_POINT('Ctrl Pts',(56.0194893756974,19.2847062601307,22.2489321614414));
#30486=CARTESIAN_POINT('Ctrl Pts',(55.9756268141322,19.2593843441645,22.2458353891472));
#30487=CARTESIAN_POINT('Ctrl Pts',(55.9187896486327,19.2293958308093,22.2418279658114));
#30488=CARTESIAN_POINT('Ctrl Pts',(55.9066634231176,19.2231558974031,22.2409733294865));
#30489=CARTESIAN_POINT('Ctrl Pts',(55.8870604384689,19.2133214776944,22.2395918593199));
#30490=CARTESIAN_POINT('Ctrl Pts',(55.8796234395096,19.2096483683755,22.239067783237));
#30491=CARTESIAN_POINT('Ctrl Pts',(55.8654118127666,19.2027392170357,22.2380662575772));
#30492=CARTESIAN_POINT('Ctrl Pts',(55.8586413864248,19.1994948223767,22.2375891088872));
#30493=CARTESIAN_POINT('Ctrl Pts',(55.843124660319,19.1921666161996,22.2364954317892));
#30494=CARTESIAN_POINT('Ctrl Pts',(55.8343667633765,19.1881079405279,22.235878048766));
#30495=CARTESIAN_POINT('Ctrl Pts',(55.8114129816927,19.1776721695777,22.2342595225954));
#30496=CARTESIAN_POINT('Ctrl Pts',(55.7971715403123,19.1713974568206,22.2332549115109));
#30497=CARTESIAN_POINT('Ctrl Pts',(55.6730060746916,19.1184168796701,22.2244907514905));
#30498=CARTESIAN_POINT('Ctrl Pts',(55.5591856972935,19.081512438334,22.2163982511514));
#30499=CARTESIAN_POINT('Ctrl Pts',(55.3263066041796,19.0284986624644,22.1998502090009));
#30500=CARTESIAN_POINT('Ctrl Pts',(55.2077007994765,19.0125004598778,22.1914300298946));
#30501=CARTESIAN_POINT('Ctrl Pts',(55.0415072454109,19.0051301587212,22.1800807204054));
#30502=CARTESIAN_POINT('Ctrl Pts',(54.9945756370025,19.0047055589642,22.1769277564013));
#30503=CARTESIAN_POINT('Ctrl Pts',(54.9387306776766,19.0061711263204,22.173270215637));
#30504=CARTESIAN_POINT('Ctrl Pts',(54.9297940400536,19.0064657921702,22.1726877995586));
#30505=CARTESIAN_POINT('Ctrl Pts',(54.9159509820275,19.0070154399804,22.1717904051859));
#30506=CARTESIAN_POINT('Ctrl Pts',(54.9110431499649,19.0072284691933,22.1714731802757));
#30507=CARTESIAN_POINT('Ctrl Pts',(54.9019543107122,19.0076566231179,22.1708874981278));
#30508=CARTESIAN_POINT('Ctrl Pts',(54.8977732226408,19.0078667777706,22.170618778328));
#30509=CARTESIAN_POINT('Ctrl Pts',(54.8882755867065,19.008374138957,22.1700099471002));
#30510=CARTESIAN_POINT('Ctrl Pts',(54.8829595550001,19.0086794706226,22.1696702922901));
#30511=CARTESIAN_POINT('Ctrl Pts',(54.869152377627,19.0095279819264,22.1687908821062));
#30512=CARTESIAN_POINT('Ctrl Pts',(54.8606632672851,19.0101042147853,22.1682529101566));
#30513=CARTESIAN_POINT('Ctrl Pts',(54.8047780828098,19.0142570364843,22.1647277380575));
#30514=CARTESIAN_POINT('Ctrl Pts',(54.757514940367,19.0194726668748,22.1618239958289));
#30515=CARTESIAN_POINT('Ctrl Pts',(54.5389940172617,19.0515285284883,22.1485745228542));
#30516=CARTESIAN_POINT('Ctrl Pts',(54.3715119980335,19.0989268251903,22.1388622988844));
#30517=CARTESIAN_POINT('Ctrl Pts',(54.1495507206926,19.1943361415193,22.1244817679848));
#30518=CARTESIAN_POINT('Ctrl Pts',(54.0882765217809,19.2244874683744,22.1203444552746));
#30519=CARTESIAN_POINT('Ctrl Pts',(54.0156348040346,19.2649854395657,22.1151673053542));
#30520=CARTESIAN_POINT('Ctrl Pts',(54.0026797402316,19.2723997440683,22.1142331184199));
#30521=CARTESIAN_POINT('Ctrl Pts',(53.9824130131017,19.2843025142795,22.1127538640252));
#30522=CARTESIAN_POINT('Ctrl Pts',(53.9750448407289,19.2886940495118,22.1122123043797));
#30523=CARTESIAN_POINT('Ctrl Pts',(53.9613185619704,19.2969955539218,22.1111962508325));
#30524=CARTESIAN_POINT('Ctrl Pts',(53.9549536127928,19.3008939647057,22.1107221854369));
#30525=CARTESIAN_POINT('Ctrl Pts',(53.9407901968371,19.3096784790632,22.1096606739608));
#30526=CARTESIAN_POINT('Ctrl Pts',(53.9330034012854,19.3145829878334,22.1090725566859));
#30527=CARTESIAN_POINT('Ctrl Pts',(53.9133895010384,19.3271271931885,22.107579546365));
#30528=CARTESIAN_POINT('Ctrl Pts',(53.9016089855882,19.3348384562449,22.1066720103993));
#30529=CARTESIAN_POINT('Ctrl Pts',(53.8326951372653,19.3809974282371,22.1012980722475));
#30530=CARTESIAN_POINT('Ctrl Pts',(53.7775082899416,19.4222541037242,22.096726233571));
#30531=CARTESIAN_POINT('Ctrl Pts',(53.5960062618436,19.5731895882687,22.0807350084138));
#30532=CARTESIAN_POINT('Ctrl Pts',(53.481413737206,19.6958252626058,22.0688614487301));
#30533=CARTESIAN_POINT('Ctrl Pts',(53.3629398511127,19.8596977920986,22.0550185152881));
#30534=CARTESIAN_POINT('Ctrl Pts',(53.3431633339902,19.8886280507945,22.0526443634274));
#30535=CARTESIAN_POINT('Ctrl Pts',(53.3163679968268,19.9301321941513,22.049350299199));
#30536=CARTESIAN_POINT('Ctrl Pts',(53.3087081990368,19.9422826868989,22.0483990748917));
#30537=CARTESIAN_POINT('Ctrl Pts',(53.295471169318,19.9637916850545,22.0467395440868));
#30538=CARTESIAN_POINT('Ctrl Pts',(53.2898381929057,19.9731149952555,22.0460281107478));
#30539=CARTESIAN_POINT('Ctrl Pts',(53.281569917422,19.9870568247403,22.0449764997441));
#30540=CARTESIAN_POINT('Ctrl Pts',(53.278876367199,19.9916403086119,22.0446327254326));
#30541=CARTESIAN_POINT('Ctrl Pts',(53.274094843857,19.9998517734236,22.044020397084));
#30542=CARTESIAN_POINT('Ctrl Pts',(53.2719999411686,20.0034755994611,22.0437514032716));
#30543=CARTESIAN_POINT('Ctrl Pts',(53.2674681049062,20.0113721688824,22.0431679361548));
#30544=CARTESIAN_POINT('Ctrl Pts',(53.2650355666977,20.0156473333128,22.0428537442523));
#30545=CARTESIAN_POINT('Ctrl Pts',(53.2583311442625,20.0275323570095,22.0419848522127));
#30546=CARTESIAN_POINT('Ctrl Pts',(53.2540932855144,20.0351614276703,22.0414322752435));
#30547=CARTESIAN_POINT('Ctrl Pts',(53.231723197053,20.0760625074127,22.0384959727651));
#30548=CARTESIAN_POINT('Ctrl Pts',(53.2144903982374,20.1098206706753,22.0361644874006));
#30549=CARTESIAN_POINT('Ctrl Pts',(53.1206209176822,20.3074159671148,22.0229236652895));
#30550=CARTESIAN_POINT('Ctrl Pts',(53.0655852170667,20.4805861575663,22.0128265340167));
#30551=CARTESIAN_POINT('Ctrl Pts',(53.0266136607683,20.7050787864988,21.9992874647207));
#30552=CARTESIAN_POINT('Ctrl Pts',(53.0202191052899,20.7516065246491,21.9964632277785));
#30553=CARTESIAN_POINT('Ctrl Pts',(53.0123044070312,20.8294848118171,21.9916745650311));
#30554=CARTESIAN_POINT('Ctrl Pts',(53.0098715395249,20.8607242195519,21.9897374552123));
#30555=CARTESIAN_POINT('Ctrl Pts',(53.0075532874913,20.9034819731368,21.9870584401019));
#30556=CARTESIAN_POINT('Ctrl Pts',(53.007030306562,20.9149622207173,21.9863364295341));
#30557=CARTESIAN_POINT('Ctrl Pts',(53.0063178076254,20.934271758601,21.9851172066318));
#30558=CARTESIAN_POINT('Ctrl Pts',(53.0060751404237,20.9420988995984,21.9846216642222));
#30559=CARTESIAN_POINT('Ctrl Pts',(53.0056869306216,20.9575591320441,21.9836401542223));
#30560=CARTESIAN_POINT('Ctrl Pts',(53.005539108197,20.9651920358087,21.983154266534));
#30561=CARTESIAN_POINT('Ctrl Pts',(53.005309941177,20.9820125375752,21.9820805713036));
#30562=CARTESIAN_POINT('Ctrl Pts',(53.0052482514913,20.9912001865167,21.9814921593815));
#30563=CARTESIAN_POINT('Ctrl Pts',(53.0052545405657,21.0235489877355,21.9794133965494));
#30564=CARTESIAN_POINT('Ctrl Pts',(53.0056624310092,21.0467074799556,21.9779125082573));
#30565=CARTESIAN_POINT('Ctrl Pts',(53.0099793257329,21.169907119395,21.9698572499644));
#30566=CARTESIAN_POINT('Ctrl Pts',(53.0210120454064,21.2695405343755,21.9630836386395));
#30567=CARTESIAN_POINT('Ctrl Pts',(53.0595322021014,21.4748061766944,21.9486597695539));
#30568=CARTESIAN_POINT('Ctrl Pts',(53.088299572222,21.5798765704903,21.9410071814636));
#30569=CARTESIAN_POINT('Ctrl Pts',(53.1322777321936,21.7007392469975,21.9321353382661));
#30570=CARTESIAN_POINT('Ctrl Pts',(53.13934689952,21.7192996871774,21.9307713489112));
#30571=CARTESIAN_POINT('Ctrl Pts',(53.1641047985049,21.7814940467824,21.9262016597919));
#30572=CARTESIAN_POINT('Ctrl Pts',(53.1830621659017,21.8246101130648,21.9230350417638));
#30573=CARTESIAN_POINT('Ctrl Pts',(53.2072178089171,21.8746608424881,21.9193930671669));
#30574=CARTESIAN_POINT('Ctrl Pts',(53.2109550429793,21.8822798433186,21.9188396239907));
#30575=CARTESIAN_POINT('Ctrl Pts',(53.2171132348228,21.8946343528937,21.9179440361739));
#30576=CARTESIAN_POINT('Ctrl Pts',(53.2195046628134,21.8993843442424,21.9176001518224));
#30577=CARTESIAN_POINT('Ctrl Pts',(53.2238123524297,21.9078560044096,21.9169877053446));
#30578=CARTESIAN_POINT('Ctrl Pts',(53.2257213543959,21.9115812486799,21.9167187027262));
#30579=CARTESIAN_POINT('Ctrl Pts',(53.229898511729,21.9196697585728,21.916135306161));
#30580=CARTESIAN_POINT('Ctrl Pts',(53.2321710756985,21.9240306484503,21.9158211930497));
#30581=CARTESIAN_POINT('Ctrl Pts',(53.2386320346689,21.9363176907273,21.9149372322428));
#30582=CARTESIAN_POINT('Ctrl Pts',(53.2428578310199,21.9442241960658,21.9143696801352));
#30583=CARTESIAN_POINT('Ctrl Pts',(53.2697529346133,21.9937392997632,21.9108215933723));
#30584=CARTESIAN_POINT('Ctrl Pts',(53.293847455087,22.0345612616061,21.9079242214424));
#30585=CARTESIAN_POINT('Ctrl Pts',(53.3560556881346,22.131862051641,21.9009908199185));
#30586=CARTESIAN_POINT('Ctrl Pts',(53.3956521505147,22.1873220642859,21.8970142636764));
#30587=CARTESIAN_POINT('Ctrl Pts',(53.5379302761178,22.3664514415244,21.8837203187678));
#30588=CARTESIAN_POINT('Ctrl Pts',(53.6526685959417,22.4797058327579,21.8744856673388));
#30589=CARTESIAN_POINT('Ctrl Pts',(53.797978593388,22.5920752502866,21.8631639699588));
#30590=CARTESIAN_POINT('Ctrl Pts',(53.8164585148788,22.6058606879556,21.8617314956129));
#30591=CARTESIAN_POINT('Ctrl Pts',(53.8428194620852,22.6248229121148,21.8596962395714));
#30592=CARTESIAN_POINT('Ctrl Pts',(53.8505050515846,22.6302691960999,21.859103810811));
#30593=CARTESIAN_POINT('Ctrl Pts',(53.8639655317667,22.6396652693003,21.858067741994));
#30594=CARTESIAN_POINT('Ctrl Pts',(53.869723207206,22.6436395219167,21.8576250416526));
#30595=CARTESIAN_POINT('Ctrl Pts',(53.8818217826867,22.6518969666933,21.8566957223432));
#30596=CARTESIAN_POINT('Ctrl Pts',(53.8881666485841,22.6561741183351,21.8562088850777));
#30597=CARTESIAN_POINT('Ctrl Pts',(53.9033389067207,22.6662754428282,21.8550458902131));
#30598=CARTESIAN_POINT('Ctrl Pts',(53.9121882440023,22.6720660816087,21.8543684921998));
#30599=CARTESIAN_POINT('Ctrl Pts',(53.9423761163796,22.6914786925323,21.8520605289971));
#30600=CARTESIAN_POINT('Ctrl Pts',(53.9639270377739,22.7047642551455,21.8504176463531));
#30601=CARTESIAN_POINT('Ctrl Pts',(54.0162044869587,22.7356344545864,21.8464419214565));
#30602=CARTESIAN_POINT('Ctrl Pts',(54.0471568385134,22.7528177958132,21.8440955683627));
#30603=CARTESIAN_POINT('Ctrl Pts',(54.170933374695,22.8172854435037,21.8347414178948));
#30604=CARTESIAN_POINT('Ctrl Pts',(54.2669353382658,22.8580875989863,21.8275372586523));
#30605=CARTESIAN_POINT('Ctrl Pts',(54.4826811196101,22.9304507287261,21.8116734126673));
#30606=CARTESIAN_POINT('Ctrl Pts',(54.6030897518693,22.9587563664343,21.8030216820526));
#30607=CARTESIAN_POINT('Ctrl Pts',(54.7408746869787,22.977909824288,21.7938092423701));
#30608=CARTESIAN_POINT('Ctrl Pts',(54.7564237520758,22.9798848069889,21.7927795874487));
#30609=CARTESIAN_POINT('Ctrl Pts',(54.7782915916966,22.9824008463221,21.7913469835604));
#30610=CARTESIAN_POINT('Ctrl Pts',(54.7845916573608,22.9830953034037,21.7909360542432));
#30611=CARTESIAN_POINT('Ctrl Pts',(54.7947842764362,22.9841696912345,21.7902742537754));
#30612=CARTESIAN_POINT('Ctrl Pts',(54.7986747621842,22.9845682165339,21.790022358841));
#30613=CARTESIAN_POINT('Ctrl Pts',(54.8069050110589,22.9853868381767,21.7894910209665));
#30614=CARTESIAN_POINT('Ctrl Pts',(54.811245027185,22.9858041526986,21.7892117406183));
#30615=CARTESIAN_POINT('Ctrl Pts',(54.8219804263145,22.986800903384,21.788523083483));
#30616=CARTESIAN_POINT('Ctrl Pts',(54.8283773714245,22.9873636995753,21.7881146303464));
#30617=CARTESIAN_POINT('Ctrl Pts',(54.8521603123513,22.9893404070899,21.7866027453845));
#30618=CARTESIAN_POINT('Ctrl Pts',(54.8695625026795,22.9905571925582,21.7855097541409));
#30619=CARTESIAN_POINT('Ctrl Pts',(54.9794427604105,22.996792934718,21.7786794598602));
#30620=CARTESIAN_POINT('Ctrl Pts',(55.0721571717986,22.9955943612478,21.7732303855258));
#30621=CARTESIAN_POINT('Ctrl Pts',(55.1644483608155,22.9879598333782,21.7678366528264));
#30622=CARTESIAN_POINT('',(53.0052506709088,21.0016360287739,21.82180160064));
#30623=CARTESIAN_POINT('Ctrl Pts',(55.1644483516286,22.9879598341382,21.6085614209934));
#30624=CARTESIAN_POINT('Ctrl Pts',(55.1617779762643,22.9881807333834,21.6087317139713));
#30625=CARTESIAN_POINT('Ctrl Pts',(55.1591071650582,22.9883962512936,21.6089021757682));
#30626=CARTESIAN_POINT('Ctrl Pts',(55.1473710419759,22.9893194864748,21.6096518482129));
#30627=CARTESIAN_POINT('Ctrl Pts',(55.1383015064477,22.9899705857306,21.6102328283703));
#30628=CARTESIAN_POINT('Ctrl Pts',(55.1119122403895,22.9916837878414,21.6119282176947));
#30629=CARTESIAN_POINT('Ctrl Pts',(55.0945830631652,22.9925819112099,21.6130477215589));
#30630=CARTESIAN_POINT('Ctrl Pts',(54.9313800541841,22.9989065380806,21.6236519036185));
#30631=CARTESIAN_POINT('Ctrl Pts',(54.7853644296207,22.9885300440164,21.6336466817665));
#30632=CARTESIAN_POINT('Ctrl Pts',(54.5143004666532,22.9390527483187,21.6528438923881));
#30633=CARTESIAN_POINT('Ctrl Pts',(54.389346787241,22.9034016554108,21.6619515336031));
#30634=CARTESIAN_POINT('Ctrl Pts',(54.2544282853142,22.8502396124984,21.6715509014633));
#30635=CARTESIAN_POINT('Ctrl Pts',(54.2401932448406,22.8444396262404,21.6725603604724));
#30636=CARTESIAN_POINT('Ctrl Pts',(54.2202322199938,22.8360362989407,21.6739697043924));
#30637=CARTESIAN_POINT('Ctrl Pts',(54.2144497503709,22.833569712244,21.6743772386554));
#30638=CARTESIAN_POINT('Ctrl Pts',(54.2047423042156,22.8293745245944,21.6750600375736));
#30639=CARTESIAN_POINT('Ctrl Pts',(54.2008111009197,22.82766054252,21.6753361725057));
#30640=CARTESIAN_POINT('Ctrl Pts',(54.1933092774923,22.8243609575302,21.6758623518518));
#30641=CARTESIAN_POINT('Ctrl Pts',(54.1897377540319,22.8227775285375,21.6761125300098));
#30642=CARTESIAN_POINT('Ctrl Pts',(54.1807435781754,22.818758316895,21.6767417797376));
#30643=CARTESIAN_POINT('Ctrl Pts',(54.1753270735485,22.816308747576,21.677120016706));
#30644=CARTESIAN_POINT('Ctrl Pts',(54.1556958856566,22.807324784326,21.6784885678753));
#30645=CARTESIAN_POINT('Ctrl Pts',(54.1415468114881,22.8006472371079,21.679470542339));
#30646=CARTESIAN_POINT('Ctrl Pts',(54.1066583769887,22.7836771789033,21.6818844714766));
#30647=CARTESIAN_POINT('Ctrl Pts',(54.0860164315846,22.7731885591763,21.6833061211108));
#30648=CARTESIAN_POINT('Ctrl Pts',(54.0013731152529,22.728308504735,21.689127423286));
#30649=CARTESIAN_POINT('Ctrl Pts',(53.9390874315507,22.6907903806595,21.6933925329391));
#30650=CARTESIAN_POINT('Ctrl Pts',(53.7369129211323,22.553428459473,21.7076252250684));
#30651=CARTESIAN_POINT('Ctrl Pts',(53.607919748892,22.4389704164121,21.7174451561569));
#30652=CARTESIAN_POINT('Ctrl Pts',(53.4804501043683,22.292478005863,21.7294275417452));
#30653=CARTESIAN_POINT('Ctrl Pts',(53.4660047413569,22.2752998722027,21.7308234141959));
#30654=CARTESIAN_POINT('Ctrl Pts',(53.4455662760572,22.2501450886237,21.7328563263371));
#30655=CARTESIAN_POINT('Ctrl Pts',(53.4393380030701,22.2423610869161,21.7334838947135));
#30656=CARTESIAN_POINT('Ctrl Pts',(53.42847953215,22.2285798231934,21.7345925226408));
#30657=CARTESIAN_POINT('Ctrl Pts',(53.4238246312341,22.2226022113269,21.7350725873166));
#30658=CARTESIAN_POINT('Ctrl Pts',(53.4142820003185,22.2102029227855,21.73606681098));
#30659=CARTESIAN_POINT('Ctrl Pts',(53.4093989683717,22.2037778216362,21.7365811427809));
#30660=CARTESIAN_POINT('Ctrl Pts',(53.3969790068595,22.1872281033464,21.7379038696963));
#30661=CARTESIAN_POINT('Ctrl Pts',(53.3894990325579,22.1770613813856,21.7387144613357));
#30662=CARTESIAN_POINT('Ctrl Pts',(53.3584890218798,22.1340638335243,21.7421349462034));
#30663=CARTESIAN_POINT('Ctrl Pts',(53.3358639131521,22.1005951851126,21.7447790126629));
#30664=CARTESIAN_POINT('Ctrl Pts',(53.2638327535743,21.9867377216486,21.7537201551066));
#30665=CARTESIAN_POINT('Ctrl Pts',(53.2191196504964,21.9035426213686,21.7601743499628));
#30666=CARTESIAN_POINT('Ctrl Pts',(53.1476539198563,21.7444802559619,21.7722784450761));
#30667=CARTESIAN_POINT('Ctrl Pts',(53.1192701499859,21.6695461037394,21.7778895909982));
#30668=CARTESIAN_POINT('Ctrl Pts',(53.0908231470972,21.5781999293943,21.7845184947134));
#30669=CARTESIAN_POINT('Ctrl Pts',(53.0863552031951,21.5632362026823,21.7855976629879));
#30670=CARTESIAN_POINT('Ctrl Pts',(53.0784285025961,21.5355048681868,21.7875836493999));
#30671=CARTESIAN_POINT('Ctrl Pts',(53.0749201365852,21.5227523452241,21.7884915170118));
#30672=CARTESIAN_POINT('Ctrl Pts',(53.0588699559472,21.4620577684243,21.7927842349298));
#30673=CARTESIAN_POINT('Ctrl Pts',(53.0479895199753,21.4136897705801,21.7961222885044));
#30674=CARTESIAN_POINT('Ctrl Pts',(53.0373468883347,21.3565029711685,21.799935196117));
#30675=CARTESIAN_POINT('Ctrl Pts',(53.0358272605837,21.3480331324557,21.800496499402));
#30676=CARTESIAN_POINT('Ctrl Pts',(53.0334512578881,21.3342787182565,21.801402185719));
#30677=CARTESIAN_POINT('Ctrl Pts',(53.0325612827175,21.3290001701196,21.8017483727361));
#30678=CARTESIAN_POINT('Ctrl Pts',(53.0310129992354,21.319586119525,21.8023632297214));
#30679=CARTESIAN_POINT('Ctrl Pts',(53.0303464547553,21.3154520720876,21.8026323555845));
#30680=CARTESIAN_POINT('Ctrl Pts',(53.0290754110196,21.3074076804958,21.8031543239326));
#30681=CARTESIAN_POINT('Ctrl Pts',(53.0284695309719,21.3034976570394,21.8034072467288));
#30682=CARTESIAN_POINT('Ctrl Pts',(53.0271487012991,21.2948028500444,21.8039679891812));
#30683=CARTESIAN_POINT('Ctrl Pts',(53.0264395136366,21.2900171977745,21.8042754892173));
#30684=CARTESIAN_POINT('Ctrl Pts',(53.0247126304538,21.2780643332706,21.8050407911548));
#30685=CARTESIAN_POINT('Ctrl Pts',(53.0237165164829,21.2708940054424,21.8054974412499));
#30686=CARTESIAN_POINT('Ctrl Pts',(53.0111727514092,21.1768465231527,21.8114568477455));
#30687=CARTESIAN_POINT('Ctrl Pts',(53.0053225665444,21.0892957162249,21.8166699893501));
#30688=CARTESIAN_POINT('Ctrl Pts',(53.0052506709088,21.0016360287739,21.82180160064));
#30689=CARTESIAN_POINT('Ctrl Pts',(53.0052506727303,21.0016382481781,21.8218014707158));
#30690=CARTESIAN_POINT('Ctrl Pts',(53.0050980911781,20.8158532415753,21.8326773561794));
#30691=CARTESIAN_POINT('Ctrl Pts',(53.0308982462845,20.6309633578212,21.8431993114979));
#30692=CARTESIAN_POINT('Ctrl Pts',(53.0885150928867,20.429183853493,21.8561264103871));
#30693=CARTESIAN_POINT('Ctrl Pts',(53.0955337411309,20.4061870542386,21.8576200319245));
#30694=CARTESIAN_POINT('Ctrl Pts',(53.1061686196015,20.3734718070132,21.8597765417519));
#30695=CARTESIAN_POINT('Ctrl Pts',(53.1094477852777,20.3636453890307,21.8604284050087));
#30696=CARTESIAN_POINT('Ctrl Pts',(53.115269011805,20.3466435840098,21.8615636445917));
#30697=CARTESIAN_POINT('Ctrl Pts',(53.1177759042922,20.3394563185554,21.8620458524304));
#30698=CARTESIAN_POINT('Ctrl Pts',(53.1226808407823,20.3256485208664,21.8629767601612));
#30699=CARTESIAN_POINT('Ctrl Pts',(53.1250729275634,20.3190259814591,21.863425256261));
#30700=CARTESIAN_POINT('Ctrl Pts',(53.1308111808933,20.3033989682237,21.8644883886614));
#30701=CARTESIAN_POINT('Ctrl Pts',(53.1341874034381,20.2944057907627,21.865104019444));
#30702=CARTESIAN_POINT('Ctrl Pts',(53.146283442061,20.262879761762,21.8672757824595));
#30703=CARTESIAN_POINT('Ctrl Pts',(53.1553472739557,20.2404820225856,21.8688433631035));
#30704=CARTESIAN_POINT('Ctrl Pts',(53.2148410381555,20.1008174599471,21.8787782206856));
#30705=CARTESIAN_POINT('Ctrl Pts',(53.2760150411987,19.9884727899826,21.8875142622304));
#30706=CARTESIAN_POINT('Ctrl Pts',(53.3880049215924,19.8228285322391,21.9014301816578));
#30707=CARTESIAN_POINT('Ctrl Pts',(53.4317528180296,19.7651470709507,21.9064949832486));
#30708=CARTESIAN_POINT('Ctrl Pts',(53.5107039583615,19.6720320943453,21.9149388884185));
#30709=CARTESIAN_POINT('Ctrl Pts',(53.5442803056887,19.6353087153633,21.9183467338849));
#30710=CARTESIAN_POINT('Ctrl Pts',(53.598262208756,19.5805294849428,21.9235079226599));
#30711=CARTESIAN_POINT('Ctrl Pts',(53.6177222288231,19.5615724841883,21.9253094660529));
#30712=CARTESIAN_POINT('Ctrl Pts',(53.6430229066554,19.5379136217837,21.9275710145567));
#30713=CARTESIAN_POINT('Ctrl Pts',(53.6485100427259,19.5328400534064,21.9280567933379));
#30714=CARTESIAN_POINT('Ctrl Pts',(53.6569492292224,19.5251244523029,21.9287965860874));
#30715=CARTESIAN_POINT('Ctrl Pts',(53.6598807787989,19.5224602449637,21.9290522309805));
#30716=CARTESIAN_POINT('Ctrl Pts',(53.6659258925465,19.5169992062352,21.9295766097371));
#30717=CARTESIAN_POINT('Ctrl Pts',(53.6690402845746,19.5142034745889,21.9298452515595));
#30718=CARTESIAN_POINT('Ctrl Pts',(53.6761364345678,19.5078736094059,21.9304539477382));
#30719=CARTESIAN_POINT('Ctrl Pts',(53.6801235509547,19.504345606022,21.9307935454502));
#30720=CARTESIAN_POINT('Ctrl Pts',(53.6905191270377,19.4952210149287,21.9316728824456));
#30721=CARTESIAN_POINT('Ctrl Pts',(53.6969494317181,19.4896493211342,21.9322108380987));
#30722=CARTESIAN_POINT('Ctrl Pts',(53.7395565926629,19.4532059686567,21.935737745149));
#30723=CARTESIAN_POINT('Ctrl Pts',(53.7767951369329,19.4235926826868,21.9386431368235));
#30724=CARTESIAN_POINT('Ctrl Pts',(53.8301838638295,19.384168564838,21.9426244566304));
#30725=CARTESIAN_POINT('Ctrl Pts',(53.845465247139,19.3732146556651,21.9437439471052));
#30726=CARTESIAN_POINT('Ctrl Pts',(53.9898840980947,19.2727533511981,21.9541602202661));
#30727=CARTESIAN_POINT('Ctrl Pts',(54.1290172833517,19.1985817961632,21.9630325544292));
#30728=CARTESIAN_POINT('Ctrl Pts',(54.3367626858106,19.1175868952596,21.9763242863846));
#30729=CARTESIAN_POINT('Ctrl Pts',(54.3992488503363,19.0967240006669,21.9803203322845));
#30730=CARTESIAN_POINT('Ctrl Pts',(54.476875634755,19.0750099388456,21.9853390561586));
#30731=CARTESIAN_POINT('Ctrl Pts',(54.4911470622699,19.0711883175691,21.9862638429036));
#30732=CARTESIAN_POINT('Ctrl Pts',(54.5137354128136,19.0654077191829,21.9877314480522));
#30733=CARTESIAN_POINT('Ctrl Pts',(54.5220249119441,19.0633429954504,21.9882708506131));
#30734=CARTESIAN_POINT('Ctrl Pts',(54.5375822544979,19.0595739863298,21.9892848192234));
#30735=CARTESIAN_POINT('Ctrl Pts',(54.5448469207738,19.0578571221787,21.9897589710997));
#30736=CARTESIAN_POINT('Ctrl Pts',(54.5611288869914,19.0541055632396,21.9908232388005));
#30737=CARTESIAN_POINT('Ctrl Pts',(54.5701509919643,19.0520927028254,21.9914140433699));
#30738=CARTESIAN_POINT('Ctrl Pts',(54.5930854885562,19.0471430368258,21.9929187627052));
#30739=CARTESIAN_POINT('Ctrl Pts',(54.6070157058985,19.0442921830061,21.9938353942528));
#30740=CARTESIAN_POINT('Ctrl Pts',(54.6905828672312,19.0281188284701,21.9993512329737));
#30741=CARTESIAN_POINT('Ctrl Pts',(54.760851522398,19.0183692872041,22.0040624180753));
#30742=CARTESIAN_POINT('Ctrl Pts',(55.0086858164157,18.997357108006,22.0209323512635));
#30743=CARTESIAN_POINT('Ctrl Pts',(55.1870754480297,19.0060978318498,22.0336107361399));
#30744=CARTESIAN_POINT('Ctrl Pts',(55.3884195402434,19.0432467413716,22.0475121720839));
#30745=CARTESIAN_POINT('Ctrl Pts',(55.4148070987268,19.0486701271835,22.0493236396646));
#30746=CARTESIAN_POINT('Ctrl Pts',(55.4582723178746,19.0585250740111,22.0522816940782));
#30747=CARTESIAN_POINT('Ctrl Pts',(55.4754149244574,19.06265152676,22.0534416353026));
#30748=CARTESIAN_POINT('Ctrl Pts',(55.4987488004834,19.0685966858054,22.0550092454916));
#30749=CARTESIAN_POINT('Ctrl Pts',(55.5049886929585,19.0702187816143,22.0554273459321));
#30750=CARTESIAN_POINT('Ctrl Pts',(55.5154393183897,19.0729896421543,22.0561255998323));
#30751=CARTESIAN_POINT('Ctrl Pts',(55.5196542990744,19.0741220130227,22.056406678919));
#30752=CARTESIAN_POINT('Ctrl Pts',(55.527633393466,19.0762937301641,22.056937696563));
#30753=CARTESIAN_POINT('Ctrl Pts',(55.5313982174934,19.0773303077249,22.0571877969514));
#30754=CARTESIAN_POINT('Ctrl Pts',(55.541238748375,19.0800708355095,22.0578403846677));
#30755=CARTESIAN_POINT('Ctrl Pts',(55.5473095157265,19.0817925878596,22.0582418497776));
#30756=CARTESIAN_POINT('Ctrl Pts',(55.5682749531333,19.0878463053209,22.0596247413766));
#30757=CARTESIAN_POINT('Ctrl Pts',(55.5831276379326,19.0923233064311,22.060598184771));
#30758=CARTESIAN_POINT('Ctrl Pts',(55.7199499988913,19.1353126133284,22.0695205377821));
#30759=CARTESIAN_POINT('Ctrl Pts',(55.83802062457,19.1853050457379,22.0769004279614));
#30760=CARTESIAN_POINT('Ctrl Pts',(56.0802577085243,19.3165948273743,22.092885568502));
#30761=CARTESIAN_POINT('Ctrl Pts',(56.2017887384573,19.4010922930311,22.1014783269401));
#30762=CARTESIAN_POINT('Ctrl Pts',(56.3258980597828,19.5095904175426,22.1117094654506));
#30763=CARTESIAN_POINT('Ctrl Pts',(56.3387638254859,19.5211363218532,22.1127890035741));
#30764=CARTESIAN_POINT('Ctrl Pts',(56.3581554809446,19.5389990808885,22.1144462182574));
#30765=CARTESIAN_POINT('Ctrl Pts',(56.3647911966308,19.5451958959145,22.1150188160601));
#30766=CARTESIAN_POINT('Ctrl Pts',(56.376274176585,19.5560670738104,22.1160194659288));
#30767=CARTESIAN_POINT('Ctrl Pts',(56.3811405423169,19.5607211163156,22.1164466394684));
#30768=CARTESIAN_POINT('Ctrl Pts',(56.3920332459515,19.5712446773882,22.1174098950999));
#30769=CARTESIAN_POINT('Ctrl Pts',(56.3980461769483,19.5771278296098,22.1179465669647));
#30770=CARTESIAN_POINT('Ctrl Pts',(56.4140936310367,19.5930288516578,22.1193923213842));
#30771=CARTESIAN_POINT('Ctrl Pts',(56.4240587024888,19.6031158228955,22.1203044433582));
#30772=CARTESIAN_POINT('Ctrl Pts',(56.4689451736135,19.6495308816316,22.1244797993637));
#30773=CARTESIAN_POINT('Ctrl Pts',(56.5025871538981,19.6870651750828,22.1277972068187));
#30774=CARTESIAN_POINT('Ctrl Pts',(56.5516673711542,19.7461835383234,22.1329388458436));
#30775=CARTESIAN_POINT('Ctrl Pts',(56.5681576959389,19.7668703657113,22.1347232694608));
#30776=CARTESIAN_POINT('Ctrl Pts',(56.6906085573119,19.9269124462104,22.1484129697966));
#30777=CARTESIAN_POINT('Ctrl Pts',(56.7782076008204,20.079325106133,22.1608886736713));
#30778=CARTESIAN_POINT('Ctrl Pts',(56.8549747247496,20.2659610832714,22.1745882585467));
#30779=CARTESIAN_POINT('Ctrl Pts',(56.8646601625911,20.2909252622256,22.1763885421882));
#30780=CARTESIAN_POINT('Ctrl Pts',(56.8798584191307,20.3325661397942,22.179330319118));
#30781=CARTESIAN_POINT('Ctrl Pts',(56.8856586710146,20.3491336073491,22.1804849916147));
#30782=CARTESIAN_POINT('Ctrl Pts',(56.8932859935294,20.3718780928727,22.1820466944667));
#30783=CARTESIAN_POINT('Ctrl Pts',(56.8953027617215,20.3779900099763,22.1824640570668));
#30784=CARTESIAN_POINT('Ctrl Pts',(56.8986367459139,20.3882605972091,22.1831614234442));
#30785=CARTESIAN_POINT('Ctrl Pts',(56.8999699514307,20.3924139775989,22.1834423478833));
#30786=CARTESIAN_POINT('Ctrl Pts',(56.9024713724709,20.4002954874993,22.1839733301926));
#30787=CARTESIAN_POINT('Ctrl Pts',(56.9036422740737,20.4040227199068,22.1842235484473));
#30788=CARTESIAN_POINT('Ctrl Pts',(56.9066788170377,20.4137889454666,22.1848769160476));
#30789=CARTESIAN_POINT('Ctrl Pts',(56.9085267376512,20.4198334669496,22.1852790383876));
#30790=CARTESIAN_POINT('Ctrl Pts',(56.9148284310914,20.4408021778623,22.1866665286772));
#30791=CARTESIAN_POINT('Ctrl Pts',(56.9191362626855,20.4557701172069,22.1876438426298));
#30792=CARTESIAN_POINT('Ctrl Pts',(56.9564852226199,20.591504023708,22.1964012050979));
#30793=CARTESIAN_POINT('Ctrl Pts',(56.9782676272977,20.7150975577829,22.2036366071863));
#30794=CARTESIAN_POINT('Ctrl Pts',(57.0003820395373,20.9897963101217,22.2196247974323));
#30795=CARTESIAN_POINT('Ctrl Pts',(56.9954644111347,21.1405219317575,22.2283660367647));
#30796=CARTESIAN_POINT('Ctrl Pts',(56.971172018139,21.3062748612305,22.2387642985368));
#30797=CARTESIAN_POINT('Ctrl Pts',(56.9684578571297,21.3232600368203,22.2398385344605));
#30798=CARTESIAN_POINT('Ctrl Pts',(56.9639790185299,21.3491361995339,22.2414892758297));
#30799=CARTESIAN_POINT('Ctrl Pts',(56.9623727873206,21.3580540605275,22.2420607644256));
#30800=CARTESIAN_POINT('Ctrl Pts',(56.9593345936081,21.3742874246815,22.2431059023321));
#30801=CARTESIAN_POINT('Ctrl Pts',(56.9579222722598,21.381606471782,22.2435789191615));
#30802=CARTESIAN_POINT('Ctrl Pts',(56.9547757458389,21.3974352367301,22.2446058847258));
#30803=CARTESIAN_POINT('Ctrl Pts',(56.9530269290366,21.4059418609066,22.2451602909001));
#30804=CARTESIAN_POINT('Ctrl Pts',(56.9481026156856,21.4291261784821,22.2466782563411));
#30805=CARTESIAN_POINT('Ctrl Pts',(56.9448168810974,21.4437796264216,22.2476453167328));
#30806=CARTESIAN_POINT('Ctrl Pts',(56.9269837393075,21.519305565867,22.2526703123439));
#30807=CARTESIAN_POINT('Ctrl Pts',(56.9097441922972,21.5795000446673,22.2568138156584));
#30808=CARTESIAN_POINT('Ctrl Pts',(56.8341068292719,21.8032584937247,22.2727516274026));
#30809=CARTESIAN_POINT('Ctrl Pts',(56.7572835271216,21.9597465581341,22.2850865375878));
#30810=CARTESIAN_POINT('Ctrl Pts',(56.6319421699512,22.1482956386775,22.3005918544247));
#30811=CARTESIAN_POINT('Ctrl Pts',(56.6009586083271,22.1911132364786,22.3041547560605));
#30812=CARTESIAN_POINT('Ctrl Pts',(56.5626154137994,22.2398973797142,22.3082194092159));
#30813=CARTESIAN_POINT('Ctrl Pts',(56.5568719410436,22.2471015238296,22.3088197798853));
#30814=CARTESIAN_POINT('Ctrl Pts',(56.5479536706485,22.2581302378595,22.3097387385641));
#30815=CARTESIAN_POINT('Ctrl Pts',(56.5448142396232,22.2619830538696,22.3100597447509));
#30816=CARTESIAN_POINT('Ctrl Pts',(56.5390076146459,22.2690550028525,22.3106488472951));
#30817=CARTESIAN_POINT('Ctrl Pts',(56.5363447130036,22.2722774703801,22.3109172326787));
#30818=CARTESIAN_POINT('Ctrl Pts',(56.5303162798953,22.2795261551094,22.311520849531));
#30819=CARTESIAN_POINT('Ctrl Pts',(56.5269449863657,22.2835474701986,22.3118556565445));
#30820=CARTESIAN_POINT('Ctrl Pts',(56.5169631075879,22.2953589762317,22.3128390479792));
#30821=CARTESIAN_POINT('Ctrl Pts',(56.5103083770861,22.3031118768778,22.3134845163494));
#30822=CARTESIAN_POINT('Ctrl Pts',(56.4574515166504,22.3637423702608,22.3185353564067));
#30823=CARTESIAN_POINT('Ctrl Pts',(56.4085406773114,22.4142042331848,22.3227581299532));
#30824=CARTESIAN_POINT('Ctrl Pts',(56.2329790976124,22.5771663913761,22.3368967834419));
#30825=CARTESIAN_POINT('Ctrl Pts',(56.0947392657173,22.6760786430796,22.3464419036216));
#30826=CARTESIAN_POINT('Ctrl Pts',(55.9011792211822,22.7802966474929,22.359682374932));
#30827=CARTESIAN_POINT('Ctrl Pts',(55.8558038133251,22.8025480075239,22.3627726463147));
#30828=CARTESIAN_POINT('Ctrl Pts',(55.7971829979176,22.8285820949323,22.3667725602011));
#30829=CARTESIAN_POINT('Ctrl Pts',(55.784674454502,22.8339845135468,22.3676264433042));
#30830=CARTESIAN_POINT('Ctrl Pts',(55.7644676461298,22.8424672347026,22.369006888356));
#30831=CARTESIAN_POINT('Ctrl Pts',(55.756803667968,22.8456284831238,22.3695306986817));
#30832=CARTESIAN_POINT('Ctrl Pts',(55.7421638615069,22.8515606127669,22.370531842752));
#30833=CARTESIAN_POINT('Ctrl Pts',(55.7351916491895,22.8543400811375,22.3710088766293));
#30834=CARTESIAN_POINT('Ctrl Pts',(55.7192171121566,22.8606040660049,22.3721024681726));
#30835=CARTESIAN_POINT('Ctrl Pts',(55.7102049029022,22.8640626961907,22.3727198813044));
#30836=CARTESIAN_POINT('Ctrl Pts',(55.6865928764559,22.8729282338661,22.3743388514017));
#30837=CARTESIAN_POINT('Ctrl Pts',(55.6719544654871,22.8782297837889,22.3753438807442));
#30838=CARTESIAN_POINT('Ctrl Pts',(55.5437398241881,22.922974204115,22.3841601501546));
#30839=CARTESIAN_POINT('Ctrl Pts',(55.4268952292185,22.9522382108311,22.3923090568675));
#30840=CARTESIAN_POINT('Ctrl Pts',(55.2604470155227,22.978263322737,22.4039843683873));
#30841=CARTESIAN_POINT('Ctrl Pts',(55.2125158558117,22.9839835915043,22.4073508429909));
#30842=CARTESIAN_POINT('Ctrl Pts',(55.16444812056,22.9879598532527,22.4107149109706));
#30843=CARTESIAN_POINT('Origin',(55.,21.,6.22095488139522));
#30844=CARTESIAN_POINT('',(55.1644483538502,22.9879598339544,23.3702474674336));
#30845=CARTESIAN_POINT('',(55.164448305082,22.9879598379886,23.2119648302802));
#30846=CARTESIAN_POINT('',(55.1644483516311,22.987959834138,6.22095488139522));
#30847=CARTESIAN_POINT('',(53.0052508080785,20.9981768768052,22.7789686217093));
#30848=CARTESIAN_POINT('Ctrl Pts',(55.1644483538502,22.9879598339544,23.3702474674336));
#30849=CARTESIAN_POINT('Ctrl Pts',(55.1875526887303,22.9860485932075,23.368713924432));
#30850=CARTESIAN_POINT('Ctrl Pts',(55.2106221949796,22.9837346957845,23.3671685994482));
#30851=CARTESIAN_POINT('Ctrl Pts',(55.4530047006759,22.9551474869474,23.3507848761386));
#30852=CARTESIAN_POINT('Ctrl Pts',(55.6664930236811,22.89303334915,23.3348455322072));
#30853=CARTESIAN_POINT('Ctrl Pts',(55.8724179696231,22.793871326211,23.3196409044909));
#30854=CARTESIAN_POINT('Ctrl Pts',(55.879370829335,22.7904732327871,23.3191280144358));
#30855=CARTESIAN_POINT('Ctrl Pts',(55.8983085803995,22.7810808008894,23.3177326958174));
#30856=CARTESIAN_POINT('Ctrl Pts',(55.9102534002626,22.7750058860545,23.316854435342));
#30857=CARTESIAN_POINT('Ctrl Pts',(55.9268929575256,22.7663311639797,23.3156344907239));
#30858=CARTESIAN_POINT('Ctrl Pts',(55.9316394855505,22.7638322499974,23.3152868977275));
#30859=CARTESIAN_POINT('Ctrl Pts',(55.9398384892587,22.7594733741743,23.3146872511578));
#30860=CARTESIAN_POINT('Ctrl Pts',(55.943295637845,22.7576223373053,23.3144346470344));
#30861=CARTESIAN_POINT('Ctrl Pts',(55.9505742040902,22.7536975645942,23.3139033649992));
#30862=CARTESIAN_POINT('Ctrl Pts',(55.9543943387017,22.7516215094611,23.3136248424149));
#30863=CARTESIAN_POINT('Ctrl Pts',(55.9637875055941,22.7464769337867,23.3129407077181));
#30864=CARTESIAN_POINT('Ctrl Pts',(55.9693527633204,22.7433941777708,23.3125359922492));
#30865=CARTESIAN_POINT('Ctrl Pts',(55.9897621089433,22.731960912501,23.311053717938));
#30866=CARTESIAN_POINT('Ctrl Pts',(56.0045143225361,22.7234467373072,23.3099860759078));
#30867=CARTESIAN_POINT('Ctrl Pts',(56.1038199009942,22.6644245848771,23.3028123112672));
#30868=CARTESIAN_POINT('Ctrl Pts',(56.1846516218118,22.6078970473494,23.297034617931));
#30869=CARTESIAN_POINT('Ctrl Pts',(56.3899988695879,22.4403660473972,23.2816186118194));
#30870=CARTESIAN_POINT('Ctrl Pts',(56.505313221539,22.3193852197528,23.2720748873674));
#30871=CARTESIAN_POINT('Ctrl Pts',(56.6179305488844,22.1669865721406,23.2603889902156));
#30872=CARTESIAN_POINT('Ctrl Pts',(56.6312825688485,22.148248245368,23.2589586210355));
#30873=CARTESIAN_POINT('Ctrl Pts',(56.6494947927601,22.1217301194484,23.2569412544159));
#30874=CARTESIAN_POINT('Ctrl Pts',(56.6546303235663,22.1141409336612,23.2563646807037));
#30875=CARTESIAN_POINT('Ctrl Pts',(56.6639447352404,22.100169836249,23.2553045218374));
#30876=CARTESIAN_POINT('Ctrl Pts',(56.6681396669139,22.0937987929973,23.254821550069));
#30877=CARTESIAN_POINT('Ctrl Pts',(56.6765711178769,22.0808322241151,23.2538394727112));
#30878=CARTESIAN_POINT('Ctrl Pts',(56.6808055044786,22.0742354784745,23.2533402990355));
#30879=CARTESIAN_POINT('Ctrl Pts',(56.6911721142027,22.0578739978053,23.2521032644886));
#30880=CARTESIAN_POINT('Ctrl Pts',(56.6972587007716,22.0480808215462,23.25136373718));
#30881=CARTESIAN_POINT('Ctrl Pts',(56.7197103299989,22.0112481789389,23.2485853046421));
#30882=CARTESIAN_POINT('Ctrl Pts',(56.7355161604466,21.9838749746554,23.2465262670731));
#30883=CARTESIAN_POINT('Ctrl Pts',(56.7734379174398,21.9144412823184,23.2413148138363));
#30884=CARTESIAN_POINT('Ctrl Pts',(56.794712857841,21.8719461405824,23.2381351250671));
#30885=CARTESIAN_POINT('Ctrl Pts',(56.8547713207095,21.7404528777584,23.2283307252892));
#30886=CARTESIAN_POINT('Ctrl Pts',(56.888593445687,21.6493527394525,23.2215775941274));
#30887=CARTESIAN_POINT('Ctrl Pts',(56.9461673353621,21.4510445581725,23.2071740806812));
#30888=CARTESIAN_POINT('Ctrl Pts',(56.9679846630149,21.3435834236867,23.1995425786452));
#30889=CARTESIAN_POINT('Ctrl Pts',(56.9827530321108,21.2190260423238,23.1912328516155));
#30890=CARTESIAN_POINT('Ctrl Pts',(56.9844411331688,21.2031635328648,23.190184635181));
#30891=CARTESIAN_POINT('Ctrl Pts',(56.9865382697136,21.1809254785505,23.1887307203448));
#30892=CARTESIAN_POINT('Ctrl Pts',(56.9871071937269,21.174566116905,23.1883167315292));
#30893=CARTESIAN_POINT('Ctrl Pts',(56.9879760761829,21.1642986435778,23.1876513239162));
#30894=CARTESIAN_POINT('Ctrl Pts',(56.9882950611097,21.1603922516021,23.1873988602531));
#30895=CARTESIAN_POINT('Ctrl Pts',(56.9889437931303,21.1521481966832,23.1868675716016));
#30896=CARTESIAN_POINT('Ctrl Pts',(56.9892708681074,21.1478103511436,23.1865889033597));
#30897=CARTESIAN_POINT('Ctrl Pts',(56.9900421585445,21.137114515127,23.1859038948312));
#30898=CARTESIAN_POINT('Ctrl Pts',(56.9904701024633,21.1307553322432,23.1854984563951));
#30899=CARTESIAN_POINT('Ctrl Pts',(56.9919345925874,21.1073168748699,23.1840104928581));
#30900=CARTESIAN_POINT('Ctrl Pts',(56.9927818892099,21.0902259453287,23.1829379840885));
#30901=CARTESIAN_POINT('Ctrl Pts',(56.9970556815977,20.9737219898884,23.1756991873359));
#30902=CARTESIAN_POINT('Ctrl Pts',(56.9932621818815,20.8741718490033,23.1698676922224));
#30903=CARTESIAN_POINT('Ctrl Pts',(56.9634431679508,20.6111298883732,23.1544720798639));
#30904=CARTESIAN_POINT('Ctrl Pts',(56.9245085192051,20.4499181991109,23.1449954484879));
#30905=CARTESIAN_POINT('Ctrl Pts',(56.8587879331676,20.2758667397828,23.1335236801344));
#30906=CARTESIAN_POINT('Ctrl Pts',(56.8511242032126,20.2564943222127,23.1322296933896));
#30907=CARTESIAN_POINT('Ctrl Pts',(56.8388991535796,20.2269530711962,23.1302282851751));
#30908=CARTESIAN_POINT('Ctrl Pts',(56.8345535452792,20.2166961428536,23.1295281000388));
#30909=CARTESIAN_POINT('Ctrl Pts',(56.8273441564334,20.2000689599384,23.1283841970194));
#30910=CARTESIAN_POINT('Ctrl Pts',(56.8245323880571,20.1936763070465,23.1279422539157));
#30911=CARTESIAN_POINT('Ctrl Pts',(56.8185650475588,20.1803003885954,23.1270129595154));
#30912=CARTESIAN_POINT('Ctrl Pts',(56.8154026939068,20.173320290921,23.1265253818259));
#30913=CARTESIAN_POINT('Ctrl Pts',(56.8077549562634,20.1566953571391,23.1253576939694));
#30914=CARTESIAN_POINT('Ctrl Pts',(56.803232529486,20.1470679160023,23.1246763170244));
#30915=CARTESIAN_POINT('Ctrl Pts',(56.7875263593158,20.1143155713807,23.1223402741277));
#30916=CARTESIAN_POINT('Ctrl Pts',(56.775973426261,20.091371539409,23.1206728810155));
#30917=CARTESIAN_POINT('Ctrl Pts',(56.7471370084489,20.0367547738245,23.1166269036083));
#30918=CARTESIAN_POINT('Ctrl Pts',(56.7294314637788,20.0053163145938,23.1142341702073));
#30919=CARTESIAN_POINT('Ctrl Pts',(56.6060345425788,19.7994728560723,23.0981363340667));
#30920=CARTESIAN_POINT('Ctrl Pts',(56.4750119054561,19.6417183174487,23.0835243630705));
#30921=CARTESIAN_POINT('Ctrl Pts',(56.2968842411621,19.483992552103,23.0674458212872));
#30922=CARTESIAN_POINT('Ctrl Pts',(56.2708119507939,19.4620713174149,23.0651746187066));
#30923=CARTESIAN_POINT('Ctrl Pts',(56.2375992622489,19.4355682462377,23.0623949479387));
#30924=CARTESIAN_POINT('Ctrl Pts',(56.2309757686384,19.4303512146974,23.0618460732412));
#30925=CARTESIAN_POINT('Ctrl Pts',(56.2204894198042,19.4221987858299,23.0609859245855));
#30926=CARTESIAN_POINT('Ctrl Pts',(56.2166486852783,19.4192352885015,23.060672733008));
#30927=CARTESIAN_POINT('Ctrl Pts',(56.2094992228896,19.4137602808129,23.0600932109083));
#30928=CARTESIAN_POINT('Ctrl Pts',(56.2061934902591,19.4112451160129,23.0598266314776));
#30929=CARTESIAN_POINT('Ctrl Pts',(56.1985804044716,19.4054901616888,23.0592158272106));
#30930=CARTESIAN_POINT('Ctrl Pts',(56.1942677642927,19.4022574928147,23.0588720995644));
#30931=CARTESIAN_POINT('Ctrl Pts',(56.1808993120217,19.3923211384713,23.0578134421759));
#30932=CARTESIAN_POINT('Ctrl Pts',(56.1717995791893,19.3856765296031,23.0571024701889));
#30933=CARTESIAN_POINT('Ctrl Pts',(56.0844921031683,19.3230520181378,23.0503672868372));
#30934=CARTESIAN_POINT('Ctrl Pts',(56.0023772651679,19.272712385282,23.044684660013));
#30935=CARTESIAN_POINT('Ctrl Pts',(55.7671423967155,19.1509539468919,23.0292345071162));
#30936=CARTESIAN_POINT('Ctrl Pts',(55.6081307236582,19.0927370793039,23.0196200082326));
#30937=CARTESIAN_POINT('Ctrl Pts',(55.4160055260398,19.0489045509081,23.0075386372113));
#30938=CARTESIAN_POINT('Ctrl Pts',(55.388187660709,19.0431800635657,23.0057805614262));
#30939=CARTESIAN_POINT('Ctrl Pts',(55.3490479363299,19.0359931247797,23.0032905010244));
#30940=CARTESIAN_POINT('Ctrl Pts',(55.3378205130788,19.0340308343984,23.0025743410944));
#30941=CARTESIAN_POINT('Ctrl Pts',(55.3196413489024,19.031013865025,23.0014114799522));
#30942=CARTESIAN_POINT('Ctrl Pts',(55.3126996613352,19.029899517437,23.0009666743903));
#30943=CARTESIAN_POINT('Ctrl Pts',(55.2982186206325,19.0276533421696,23.0000370993482));
#30944=CARTESIAN_POINT('Ctrl Pts',(55.2906783920566,19.0265279951092,22.9995521330404));
#30945=CARTESIAN_POINT('Ctrl Pts',(55.2728200808145,19.0239672857812,22.9984012292588));
#30946=CARTESIAN_POINT('Ctrl Pts',(55.2624969200019,19.0225694843224,22.9977341190151));
#30947=CARTESIAN_POINT('Ctrl Pts',(55.227985896426,19.018171541122,22.9954975915836));
#30948=CARTESIAN_POINT('Ctrl Pts',(55.2037548481514,19.0155339549619,22.9939168674208));
#30949=CARTESIAN_POINT('Ctrl Pts',(55.1459242496455,19.0103093159642,22.9901179446026));
#30950=CARTESIAN_POINT('Ctrl Pts',(55.1122964086017,19.0081284680849,22.9878877677947));
#30951=CARTESIAN_POINT('Ctrl Pts',(54.9082050587891,19.000077133985,22.9742230755));
#30952=CARTESIAN_POINT('Ctrl Pts',(54.7376340198427,19.0152416919135,22.9621705096904));
#30953=CARTESIAN_POINT('Ctrl Pts',(54.543452890987,19.0579921827243,22.9484378914524));
#30954=CARTESIAN_POINT('Ctrl Pts',(54.5159263518666,19.0646699399603,22.9464932075839));
#30955=CARTESIAN_POINT('Ctrl Pts',(54.4478441283461,19.082729790655,22.9417018142102));
#30956=CARTESIAN_POINT('Ctrl Pts',(54.4074864741428,19.0948151077224,22.9388779976395));
#30957=CARTESIAN_POINT('Ctrl Pts',(54.3597364574703,19.110778510702,22.9355804087703));
#30958=CARTESIAN_POINT('Ctrl Pts',(54.351950357403,19.113435157266,22.9350441128625));
#30959=CARTESIAN_POINT('Ctrl Pts',(54.3392328362932,19.1178624474355,22.9341707116321));
#30960=CARTESIAN_POINT('Ctrl Pts',(54.33429165259,19.1196044540795,22.9338320026674));
#30961=CARTESIAN_POINT('Ctrl Pts',(54.3254195784695,19.1227716443559,22.9332250580764));
#30962=CARTESIAN_POINT('Ctrl Pts',(54.3214862740021,19.1241897300222,22.9329564157882));
#30963=CARTESIAN_POINT('Ctrl Pts',(54.3128782687993,19.1273238173764,22.9323694575363));
#30964=CARTESIAN_POINT('Ctrl Pts',(54.3082055328977,19.1290449564336,22.9320514501441));
#30965=CARTESIAN_POINT('Ctrl Pts',(54.2953864046925,19.13382130009,22.9311805957229));
#30966=CARTESIAN_POINT('Ctrl Pts',(54.2872533642442,19.1369123749882,22.9306298253768));
#30967=CARTESIAN_POINT('Ctrl Pts',(54.2361825597691,19.1567059173028,22.9271807199228));
#30968=CARTESIAN_POINT('Ctrl Pts',(54.1938103249119,19.1748399761501,22.9243610336628));
#30969=CARTESIAN_POINT('Ctrl Pts',(54.0408900316513,19.2466515318523,22.9142073197606));
#30970=CARTESIAN_POINT('Ctrl Pts',(53.9347345236412,19.3090426621499,22.9071894004573));
#30971=CARTESIAN_POINT('Ctrl Pts',(53.740106018739,19.4490783099857,22.893220266618));
#30972=CARTESIAN_POINT('Ctrl Pts',(53.6514202282217,19.5255448017021,22.8863070178739));
#30973=CARTESIAN_POINT('Ctrl Pts',(53.5591075622195,19.6204717614227,22.8780888329795));
#30974=CARTESIAN_POINT('Ctrl Pts',(53.5484016902059,19.6317414338212,22.8771186945713));
#30975=CARTESIAN_POINT('Ctrl Pts',(53.5312666604669,19.6502063090987,22.875537305142));
#30976=CARTESIAN_POINT('Ctrl Pts',(53.5247559517101,19.657325198205,22.8749295368323));
#30977=CARTESIAN_POINT('Ctrl Pts',(53.513271201472,19.6700671456049,22.8738449305129));
#30978=CARTESIAN_POINT('Ctrl Pts',(53.5082767490647,19.6756716201505,22.8733689638534));
#30979=CARTESIAN_POINT('Ctrl Pts',(53.4978287371467,19.6875298445927,22.8723640980562));
#30980=CARTESIAN_POINT('Ctrl Pts',(53.4923823366013,19.6937896841029,22.8718349142052));
#30981=CARTESIAN_POINT('Ctrl Pts',(53.4813976287212,19.7065752222454,22.8707565580318));
#30982=CARTESIAN_POINT('Ctrl Pts',(53.4758619542447,19.7131029444985,22.8702072929601));
#30983=CARTESIAN_POINT('Ctrl Pts',(53.4521583508878,19.741421943914,22.8678298146206));
#30984=CARTESIAN_POINT('Ctrl Pts',(53.4344152195748,19.7635629203708,22.8659845635901));
#30985=CARTESIAN_POINT('Ctrl Pts',(53.3662683598414,19.8524202091886,22.8586280152659));
#30986=CARTESIAN_POINT('Ctrl Pts',(53.3196136778135,19.921891847168,22.8529774307393));
#30987=CARTESIAN_POINT('Ctrl Pts',(53.2412710452091,20.0560457482043,22.8422826071459));
#30988=CARTESIAN_POINT('Ctrl Pts',(53.2084547445226,20.1199193115414,22.8372745521671));
#30989=CARTESIAN_POINT('Ctrl Pts',(53.1337834691278,20.2868333937937,22.8245228509604));
#30990=CARTESIAN_POINT('Ctrl Pts',(53.0969608216442,20.3918730263889,22.8168002976119));
#30991=CARTESIAN_POINT('Ctrl Pts',(53.0664944665588,20.5093986504415,22.8088293104622));
#30992=CARTESIAN_POINT('Ctrl Pts',(53.063990684449,20.5193740820848,22.8081579587824));
#30993=CARTESIAN_POINT('Ctrl Pts',(53.0603224230704,20.5344829141993,22.8071494561963));
#30994=CARTESIAN_POINT('Ctrl Pts',(53.0591009702892,20.5396021094467,22.8068091940248));
#30995=CARTESIAN_POINT('Ctrl Pts',(53.0569452083263,20.5487981258443,22.8062006102182));
#30996=CARTESIAN_POINT('Ctrl Pts',(53.0560034515358,20.5528730882056,22.8059318717448));
#30997=CARTESIAN_POINT('Ctrl Pts',(53.0539727828272,20.5617874527811,22.8053460364319));
#30998=CARTESIAN_POINT('Ctrl Pts',(53.0528891044388,20.5666279563752,22.8050292395965));
#30999=CARTESIAN_POINT('Ctrl Pts',(53.0506862507167,20.5766425950012,22.8043764255838));
#31000=CARTESIAN_POINT('Ctrl Pts',(53.0495695923727,20.5818172504558,22.8040405500336));
#31001=CARTESIAN_POINT('Ctrl Pts',(53.0467457866064,20.5951603088361,22.8031780426417));
#31002=CARTESIAN_POINT('Ctrl Pts',(53.0450692530142,20.6033351821776,22.8026530432196));
#31003=CARTESIAN_POINT('Ctrl Pts',(53.0402915204004,20.627397973566,22.8011171366485));
#31004=CARTESIAN_POINT('Ctrl Pts',(53.0373322815782,20.643313782092,22.8001133014111));
#31005=CARTESIAN_POINT('Ctrl Pts',(53.015163999816,20.7711849833125,22.7921319427207));
#31006=CARTESIAN_POINT('Ctrl Pts',(53.0053546549519,20.8845682234732,22.7855596182985));
#31007=CARTESIAN_POINT('Ctrl Pts',(53.005250832938,20.9981770887742,22.7789685690919));
#31008=CARTESIAN_POINT('Ctrl Pts',(53.0052508331338,20.9981768744968,22.7789685815233));
#31009=CARTESIAN_POINT('Ctrl Pts',(53.0051453360732,21.1136051175367,22.7722719806175));
#31010=CARTESIAN_POINT('Ctrl Pts',(53.015058653874,21.2288184959203,22.7655756215079));
#31011=CARTESIAN_POINT('Ctrl Pts',(53.041379234816,21.3798229821317,22.7562946358845));
#31012=CARTESIAN_POINT('Ctrl Pts',(53.0489400926171,21.4169241618426,22.7539745442792));
#31013=CARTESIAN_POINT('Ctrl Pts',(53.0601601337043,21.4649519739355,22.7509086422972));
#31014=CARTESIAN_POINT('Ctrl Pts',(53.062864854609,21.4760950166121,22.7501929020584));
#31015=CARTESIAN_POINT('Ctrl Pts',(53.0681980994851,21.4972690408415,22.7488240992638));
#31016=CARTESIAN_POINT('Ctrl Pts',(53.070809070488,21.5073040831553,22.7481716136797));
#31017=CARTESIAN_POINT('Ctrl Pts',(53.0754731027712,21.5246730208645,22.747035532366));
#31018=CARTESIAN_POINT('Ctrl Pts',(53.0774901615593,21.5320164240476,22.7465531087708));
#31019=CARTESIAN_POINT('Ctrl Pts',(53.081453191364,21.546127542573,22.7456219568207));
#31020=CARTESIAN_POINT('Ctrl Pts',(53.0833930499127,21.552896867841,22.7451734333469));
#31021=CARTESIAN_POINT('Ctrl Pts',(53.0880628139187,21.5688725404339,22.7441105039795));
#31022=CARTESIAN_POINT('Ctrl Pts',(53.0908234151917,21.5780696614237,22.7434951053604));
#31023=CARTESIAN_POINT('Ctrl Pts',(53.1007541000729,21.6103071679826,22.741325581283));
#31024=CARTESIAN_POINT('Ctrl Pts',(53.1082755110909,21.6332362916083,22.7397600405652));
#31025=CARTESIAN_POINT('Ctrl Pts',(53.1605709874856,21.7834043917928,22.7293539544039));
#31026=CARTESIAN_POINT('Ctrl Pts',(53.2177291450206,21.9059360388466,22.7200974280056));
#31027=CARTESIAN_POINT('Ctrl Pts',(53.3374097423015,22.1066096699775,22.7038185989115));
#31028=CARTESIAN_POINT('Ctrl Pts',(53.3942606071647,22.1876001092131,22.6968923946849));
#31029=CARTESIAN_POINT('Ctrl Pts',(53.4830875165198,22.296037913884,22.6873674253064));
#31030=CARTESIAN_POINT('Ctrl Pts',(53.5102840777869,22.327209400868,22.6845977280595));
#31031=CARTESIAN_POINT('Ctrl Pts',(53.5440408153854,22.3635535681865,22.6813519937749));
#31032=CARTESIAN_POINT('Ctrl Pts',(53.5496868286309,22.3695572975213,22.6808152743485));
#31033=CARTESIAN_POINT('Ctrl Pts',(53.5587989233984,22.379127167919,22.6799591092306));
#31034=CARTESIAN_POINT('Ctrl Pts',(53.5622413410306,22.3827155630702,22.6796379283695));
#31035=CARTESIAN_POINT('Ctrl Pts',(53.5686032623531,22.3892978181851,22.679048574456));
#31036=CARTESIAN_POINT('Ctrl Pts',(53.5715187483275,22.3922953574548,22.678780111681));
#31037=CARTESIAN_POINT('Ctrl Pts',(53.5781143711546,22.3990340808006,22.6781764009049));
#31038=CARTESIAN_POINT('Ctrl Pts',(53.5817998509754,22.4027699168376,22.6778415770493));
#31039=CARTESIAN_POINT('Ctrl Pts',(53.5927018127565,22.4137339554812,22.67685836163));
#31040=CARTESIAN_POINT('Ctrl Pts',(53.5999592466746,22.4209214560237,22.6762130835218));
#31041=CARTESIAN_POINT('Ctrl Pts',(53.6574291114675,22.4769697260454,22.6711722602938));
#31042=CARTESIAN_POINT('Ctrl Pts',(53.7101348254793,22.5232157620165,22.6669584868662));
#31043=CARTESIAN_POINT('Ctrl Pts',(53.8980658465668,22.6713475138432,22.6528330328157));
#31044=CARTESIAN_POINT('Ctrl Pts',(54.0437450344656,22.7587610030584,22.6432931665649));
#31045=CARTESIAN_POINT('Ctrl Pts',(54.2450715908759,22.8470715021673,22.6300541719681));
#31046=CARTESIAN_POINT('Ctrl Pts',(54.2921826708261,22.8656323343491,22.626958370829));
#31047=CARTESIAN_POINT('Ctrl Pts',(54.3522090215923,22.8866804943506,22.6229920844478));
#31048=CARTESIAN_POINT('Ctrl Pts',(54.3645137219724,22.8908605493942,22.6221779582407));
#31049=CARTESIAN_POINT('Ctrl Pts',(54.3849181851159,22.8975705290688,22.6208257403055));
#31050=CARTESIAN_POINT('Ctrl Pts',(54.3929949356308,22.9001695713855,22.6202899286777));
#31051=CARTESIAN_POINT('Ctrl Pts',(54.4082171215991,22.9049610097096,22.6192789294699));
#31052=CARTESIAN_POINT('Ctrl Pts',(54.4153587962142,22.9071649336191,22.6188041295629));
#31053=CARTESIAN_POINT('Ctrl Pts',(54.4314469558668,22.9120308897033,22.6177333902377));
#31054=CARTESIAN_POINT('Ctrl Pts',(54.4404000311366,22.9146703520779,22.6171367260849));
#31055=CARTESIAN_POINT('Ctrl Pts',(54.4633159294062,22.9212517446198,22.615607348649));
#31056=CARTESIAN_POINT('Ctrl Pts',(54.4773036437228,22.9251042980848,22.6146717639242));
#31057=CARTESIAN_POINT('Ctrl Pts',(54.5651231268361,22.9482642348591,22.6087838967931));
#31058=CARTESIAN_POINT('Ctrl Pts',(54.63996122882,22.963471665927,22.6037011733299));
#31059=CARTESIAN_POINT('Ctrl Pts',(54.864227588018,22.995790348985,22.5882850481216));
#31060=CARTESIAN_POINT('Ctrl Pts',(55.0148363468645,23.0003360640307,22.5776559059377));
#31061=CARTESIAN_POINT('Ctrl Pts',(55.1644483539992,22.9879598339421,22.5673314474746));
#31062=CARTESIAN_POINT('Ctrl Pts',(55.16444812056,22.9879598532527,22.4107149109706));
#31063=CARTESIAN_POINT('Ctrl Pts',(55.092998751669,22.9938702917407,22.4157153656997));
#31064=CARTESIAN_POINT('Ctrl Pts',(55.0212477053551,22.9959274312002,22.4207116381971));
#31065=CARTESIAN_POINT('Ctrl Pts',(54.9038934735875,22.9929558220811,22.4287132587244));
#31066=CARTESIAN_POINT('Ctrl Pts',(54.8583300774655,22.9902361026577,22.431777235822));
#31067=CARTESIAN_POINT('Ctrl Pts',(54.8040622238466,22.9851233423472,22.4353455123856));
#31068=CARTESIAN_POINT('Ctrl Pts',(54.7952335802668,22.9842320975303,22.4359234413858));
#31069=CARTESIAN_POINT('Ctrl Pts',(54.7815423324367,22.9827576222653,22.4368153674359));
#31070=CARTESIAN_POINT('Ctrl Pts',(54.7766755663477,22.9822153615976,22.4371315695007));
#31071=CARTESIAN_POINT('Ctrl Pts',(54.7676516610276,22.9811762515095,22.4377162346869));
#31072=CARTESIAN_POINT('Ctrl Pts',(54.7634941200175,22.980684240208,22.4379849538012));
#31073=CARTESIAN_POINT('Ctrl Pts',(54.7540349013644,22.9795346097989,22.438594886404));
#31074=CARTESIAN_POINT('Ctrl Pts',(54.7487343032689,22.9788687809919,22.4389356355363));
#31075=CARTESIAN_POINT('Ctrl Pts',(54.7349385837194,22.9770795217114,22.439819947821));
#31076=CARTESIAN_POINT('Ctrl Pts',(54.72644780779,22.9759226184039,22.4403616939125));
#31077=CARTESIAN_POINT('Ctrl Pts',(54.6696468990648,22.967810105479,22.4439705446231));
#31078=CARTESIAN_POINT('Ctrl Pts',(54.6215942770523,22.9591375037917,22.4469495944768));
#31079=CARTESIAN_POINT('Ctrl Pts',(54.5617114703128,22.9460438061985,22.4506228932857));
#31080=CARTESIAN_POINT('Ctrl Pts',(54.549543907413,22.9432634019586,22.4513672063442));
#31081=CARTESIAN_POINT('Ctrl Pts',(54.5235250428917,22.9370603304564,22.4529558992286));
#31082=CARTESIAN_POINT('Ctrl Pts',(54.5096827213903,22.9336028772246,22.4537993111489));
#31083=CARTESIAN_POINT('Ctrl Pts',(54.3674794708185,22.8964589275022,22.4624558035776));
#31084=CARTESIAN_POINT('Ctrl Pts',(54.2427479200608,22.8501917243545,22.4700054792398));
#31085=CARTESIAN_POINT('Ctrl Pts',(54.0762814461305,22.7687674941564,22.4809656359055));
#31086=CARTESIAN_POINT('Ctrl Pts',(54.0299658303962,22.7437968678231,22.4841158779019));
#31087=CARTESIAN_POINT('Ctrl Pts',(53.9650633857615,22.7054189632111,22.4887172557206));
#31088=CARTESIAN_POINT('Ctrl Pts',(53.9456344926247,22.6934759961514,22.4901196612445));
#31089=CARTESIAN_POINT('Ctrl Pts',(53.9112895465205,22.6715439544146,22.4926467932075));
#31090=CARTESIAN_POINT('Ctrl Pts',(53.8962953435343,22.6616815704203,22.4937669141107));
#31091=CARTESIAN_POINT('Ctrl Pts',(53.873806610768,22.6464510111782,22.4954736112511));
#31092=CARTESIAN_POINT('Ctrl Pts',(53.8662126013602,22.6412308223551,22.4960546231608));
#31093=CARTESIAN_POINT('Ctrl Pts',(53.852534691493,22.631688273234,22.4971097817043));
#31094=CARTESIAN_POINT('Ctrl Pts',(53.8464383258529,22.627384010214,22.4975832328444));
#31095=CARTESIAN_POINT('Ctrl Pts',(53.8333983799302,22.6180672296986,22.4986028155109));
#31096=CARTESIAN_POINT('Ctrl Pts',(53.826462659292,22.6130440186073,22.4991493525739));
#31097=CARTESIAN_POINT('Ctrl Pts',(53.8078793435547,22.5994017180392,22.5006253150456));
#31098=CARTESIAN_POINT('Ctrl Pts',(53.7962931392008,22.5907002514828,22.5015579271549));
#31099=CARTESIAN_POINT('Ctrl Pts',(53.7406877386876,22.5479841211556,22.5060951104498));
#31100=CARTESIAN_POINT('Ctrl Pts',(53.698013422705,22.5122672239427,22.5097665166));
#31101=CARTESIAN_POINT('Ctrl Pts',(53.6469821174682,22.4657932221256,22.5144024445763));
#31102=CARTESIAN_POINT('Ctrl Pts',(53.637165154185,22.4566702890569,22.5153061259929));
#31103=CARTESIAN_POINT('Ctrl Pts',(53.5050658413079,22.3314057298249,22.5276277863977));
#31104=CARTESIAN_POINT('Ctrl Pts',(53.3979186834733,22.2003307151686,22.5396048900806));
#31105=CARTESIAN_POINT('Ctrl Pts',(53.2808000484889,22.012974888698,22.554731808105));
#31106=CARTESIAN_POINT('Ctrl Pts',(53.2548129746005,21.9675173933419,22.5582606418134));
#31107=CARTESIAN_POINT('Ctrl Pts',(53.2263974495058,21.9129326649336,22.5622916535438));
#31108=CARTESIAN_POINT('Ctrl Pts',(53.222209244717,21.904749742239,22.5628906396545));
#31109=CARTESIAN_POINT('Ctrl Pts',(53.2158459801481,21.8921023768893,22.5638079327298));
#31110=CARTESIAN_POINT('Ctrl Pts',(53.2136308402978,21.8876584050031,22.5641286444772));
#31111=CARTESIAN_POINT('Ctrl Pts',(53.2095812260238,21.8794575910284,22.5647174693087));
#31112=CARTESIAN_POINT('Ctrl Pts',(53.2077419766136,21.8757032709956,22.5649858694102));
#31113=CARTESIAN_POINT('Ctrl Pts',(53.2036183348874,21.867218582008,22.5655898474871));
#31114=CARTESIAN_POINT('Ctrl Pts',(53.2013408205431,21.8624849641657,22.5659249986879));
#31115=CARTESIAN_POINT('Ctrl Pts',(53.1946777302972,21.8484951229244,22.5669103473822));
#31116=CARTESIAN_POINT('Ctrl Pts',(53.1903446376154,21.8392138887377,22.5675574102831));
#31117=CARTESIAN_POINT('Ctrl Pts',(53.1564510500299,21.7651324442052,22.5726727390936));
#31118=CARTESIAN_POINT('Ctrl Pts',(53.1303054894104,21.6988169916693,22.576953090349));
#31119=CARTESIAN_POINT('Ctrl Pts',(53.0696741379118,21.5170645829692,22.5882555807318));
#31120=CARTESIAN_POINT('Ctrl Pts',(53.0419975719998,21.3996771463598,22.5951219070059));
#31121=CARTESIAN_POINT('Ctrl Pts',(53.0118886056539,21.1876937219276,22.6076992535515));
#31122=CARTESIAN_POINT('Ctrl Pts',(53.0052664294991,21.094076959173,22.6133111086405));
#31123=CARTESIAN_POINT('Ctrl Pts',(53.0052474901953,20.9858297683454,22.6200389753441));
#31124=CARTESIAN_POINT('Ctrl Pts',(53.0054034722093,20.9713112447033,22.6209461139882));
#31125=CARTESIAN_POINT('Ctrl Pts',(53.0059201341663,20.9474622962105,22.622444642487));
#31126=CARTESIAN_POINT('Ctrl Pts',(53.0061878598199,20.9381302453841,22.6230331300854));
#31127=CARTESIAN_POINT('Ctrl Pts',(53.006787789477,20.9213331068914,22.6240963265487));
#31128=CARTESIAN_POINT('Ctrl Pts',(53.0070964514545,20.9138673118923,22.6245702906203));
#31129=CARTESIAN_POINT('Ctrl Pts',(53.0078448955458,20.8979338674464,22.6255849025647));
#31130=CARTESIAN_POINT('Ctrl Pts',(53.0082967342974,20.8894669581286,22.6261259187958));
#31131=CARTESIAN_POINT('Ctrl Pts',(53.0096664959496,20.866546442037,22.6275956496375));
#31132=CARTESIAN_POINT('Ctrl Pts',(53.0106878553721,20.852099755385,22.6285275804372));
#31133=CARTESIAN_POINT('Ctrl Pts',(53.0168683571946,20.7764061442851,22.6334406213628));
#31134=CARTESIAN_POINT('Ctrl Pts',(53.0246984402708,20.7154165809302,22.6375045289539));
#31135=CARTESIAN_POINT('Ctrl Pts',(53.0614780789679,20.5060340644227,22.6518293972231));
#31136=CARTESIAN_POINT('Ctrl Pts',(53.1044576441259,20.3606420484767,22.6624788716272));
#31137=CARTESIAN_POINT('Ctrl Pts',(53.1721614539167,20.200916347281,22.6744936219287));
#31138=CARTESIAN_POINT('Ctrl Pts',(53.181241984156,20.1804588108251,22.6760376266282));
#31139=CARTESIAN_POINT('Ctrl Pts',(53.2135241773388,20.1109108505455,22.6812957272146));
#31140=CARTESIAN_POINT('Ctrl Pts',(53.2383867657655,20.0626124866743,22.6849633921613));
#31141=CARTESIAN_POINT('Ctrl Pts',(53.2695471785789,20.0077104969352,22.6891032952618));
#31142=CARTESIAN_POINT('Ctrl Pts',(53.2739536927457,20.0000652135611,22.6896790987014));
#31143=CARTESIAN_POINT('Ctrl Pts',(53.2811478492163,19.9877726501253,22.6906034806767));
#31144=CARTESIAN_POINT('Ctrl Pts',(53.2839038913492,19.9831071483973,22.6909539836961));
#31145=CARTESIAN_POINT('Ctrl Pts',(53.2888263915764,19.9748512167794,22.6915735468317));
#31146=CARTESIAN_POINT('Ctrl Pts',(53.2909851938514,19.9712563295747,22.6918430908454));
#31147=CARTESIAN_POINT('Ctrl Pts',(53.2956621558542,19.9635234986922,22.6924223793507));
#31148=CARTESIAN_POINT('Ctrl Pts',(53.2981840531741,19.959387916135,22.6927318761022));
#31149=CARTESIAN_POINT('Ctrl Pts',(53.3052404852789,19.9479105494786,22.6935900643626));
#31150=CARTESIAN_POINT('Ctrl Pts',(53.3098076981883,19.9405888362109,22.6941366682079));
#31151=CARTESIAN_POINT('Ctrl Pts',(53.336487942343,19.8984293827333,22.6972805159877));
#31152=CARTESIAN_POINT('Ctrl Pts',(53.3596319114187,19.8642521062456,22.6998149872042));
#31153=CARTESIAN_POINT('Ctrl Pts',(53.4414075294469,19.7512126928967,22.7082374947068));
#31154=CARTESIAN_POINT('Ctrl Pts',(53.504800665623,19.6759674455647,22.7139171681438));
#31155=CARTESIAN_POINT('Ctrl Pts',(53.6682640022487,19.5087278705629,22.727484953272));
#31156=CARTESIAN_POINT('Ctrl Pts',(53.7726698597119,19.4216881707559,22.7353760782752));
#31157=CARTESIAN_POINT('Ctrl Pts',(53.9050916654885,19.3324313619997,22.7452079054729));
#31158=CARTESIAN_POINT('Ctrl Pts',(53.9253361341334,19.319313556683,22.7467055485507));
#31159=CARTESIAN_POINT('Ctrl Pts',(53.9539622803344,19.3014933613065,22.7488181931838));
#31160=CARTESIAN_POINT('Ctrl Pts',(53.9621481169816,19.2964791822796,22.7494217465351));
#31161=CARTESIAN_POINT('Ctrl Pts',(53.9763990973267,19.2878906835243,22.7504716627808));
#31162=CARTESIAN_POINT('Ctrl Pts',(53.982447609913,19.2842889955243,22.7509170201939));
#31163=CARTESIAN_POINT('Ctrl Pts',(53.9950767950381,19.2768590090452,22.7518464532058));
#31164=CARTESIAN_POINT('Ctrl Pts',(54.0016605624012,19.2730362229406,22.7523307188288));
#31165=CARTESIAN_POINT('Ctrl Pts',(54.017260190871,19.2640975006701,22.7534776134172));
#31166=CARTESIAN_POINT('Ctrl Pts',(54.0262942971588,19.2590140100602,22.7541413940337));
#31167=CARTESIAN_POINT('Ctrl Pts',(54.0564480298625,19.2423546217517,22.7563558312849));
#31168=CARTESIAN_POINT('Ctrl Pts',(54.0777369716226,19.2310911786521,22.7579174941703));
#31169=CARTESIAN_POINT('Ctrl Pts',(54.1288284968502,19.2052329650925,22.7616627450694));
#31170=CARTESIAN_POINT('Ctrl Pts',(54.1588008315016,19.1909913642154,22.7638578690015));
#31171=CARTESIAN_POINT('Ctrl Pts',(54.344011353497,19.108585232087,22.7774121086704));
#31172=CARTESIAN_POINT('Ctrl Pts',(54.5070516976254,19.0597019322775,22.7893840708762));
#31173=CARTESIAN_POINT('Ctrl Pts',(54.7436880304318,19.0205346662645,22.8059629132606));
#31174=CARTESIAN_POINT('Ctrl Pts',(54.8136763738419,19.0127243385667,22.8107589765102));
#31175=CARTESIAN_POINT('Ctrl Pts',(54.8941420691767,19.0080346050364,22.8160501696307));
#31176=CARTESIAN_POINT('Ctrl Pts',(54.9043506757875,19.0075183178579,22.8167173389075));
#31177=CARTESIAN_POINT('Ctrl Pts',(54.9198066150873,19.0068557179785,22.8177207563291));
#31178=CARTESIAN_POINT('Ctrl Pts',(54.9250511135593,19.0066516175314,22.8180600712668));
#31179=CARTESIAN_POINT('Ctrl Pts',(54.9344742892906,19.0063221374573,22.8186675790737));
#31180=CARTESIAN_POINT('Ctrl Pts',(54.9386525905587,19.0061891928523,22.8189361830087));
#31181=CARTESIAN_POINT('Ctrl Pts',(54.9477984462798,19.0059269692235,22.8195224410402));
#31182=CARTESIAN_POINT('Ctrl Pts',(54.9527660677098,19.0058031162346,22.8198397907198));
#31183=CARTESIAN_POINT('Ctrl Pts',(54.9669416105508,19.0055026897701,22.8207424276101));
#31184=CARTESIAN_POINT('Ctrl Pts',(54.9761505076584,19.0053713159823,22.8213252614499));
#31185=CARTESIAN_POINT('Ctrl Pts',(55.0381002170351,19.0049166443926,22.8252241886409));
#31186=CARTESIAN_POINT('Ctrl Pts',(55.0908400959626,19.0066213661855,22.8284369355605));
#31187=CARTESIAN_POINT('Ctrl Pts',(55.315718667367,19.0228358003474,22.8419130058105));
#31188=CARTESIAN_POINT('Ctrl Pts',(55.4856438255221,19.0575752077836,22.8515991916908));
#31189=CARTESIAN_POINT('Ctrl Pts',(55.7089713365105,19.1344136649463,22.8656898030499));
#31190=CARTESIAN_POINT('Ctrl Pts',(55.7679396950883,19.1579033322196,22.869541782155));
#31191=CARTESIAN_POINT('Ctrl Pts',(55.8394092345565,19.1904014240051,22.8744269267669));
#31192=CARTESIAN_POINT('Ctrl Pts',(55.8530621899135,19.1967973630842,22.875370146346));
#31193=CARTESIAN_POINT('Ctrl Pts',(55.8744753674274,19.2071263146197,22.8768659379682));
#31194=CARTESIAN_POINT('Ctrl Pts',(55.8822847881621,19.2109564654072,22.8774149465477));
#31195=CARTESIAN_POINT('Ctrl Pts',(55.8966752344161,19.2181314354871,22.8784331966886));
#31196=CARTESIAN_POINT('Ctrl Pts',(55.9032632490416,19.2214619605569,22.8789019324261));
#31197=CARTESIAN_POINT('Ctrl Pts',(55.9178539138087,19.228940147919,22.8799458677329));
#31198=CARTESIAN_POINT('Ctrl Pts',(55.9258472057564,19.2331056189077,22.8805216864939));
#31199=CARTESIAN_POINT('Ctrl Pts',(55.9488086334058,19.2452698890248,22.8821872527772));
#31200=CARTESIAN_POINT('Ctrl Pts',(55.963702980361,19.2534055647389,22.8832818237977));
#31201=CARTESIAN_POINT('Ctrl Pts',(56.0902572475387,19.3246443597481,22.8927066239594));
#31202=CARTESIAN_POINT('Ctrl Pts',(56.195674020134,19.3981791792827,22.9014235100781));
#31203=CARTESIAN_POINT('Ctrl Pts',(56.401201805401,19.5732024639533,22.9201683169168));
#31204=CARTESIAN_POINT('Ctrl Pts',(56.499016900732,19.6763421392218,22.9301858881024));
#31205=CARTESIAN_POINT('Ctrl Pts',(56.5878029038941,19.7925524134654,22.939926341211));
#31206=CARTESIAN_POINT('Ctrl Pts',(56.5905176511349,19.7961306806596,22.9402248516379));
#31207=CARTESIAN_POINT('Ctrl Pts',(56.6032256570252,19.8129989292799,22.9416253219826));
#31208=CARTESIAN_POINT('Ctrl Pts',(56.6130649462209,19.8264048517742,22.9427187658543));
#31209=CARTESIAN_POINT('Ctrl Pts',(56.6265134541318,19.8452170161086,22.9442244336797));
#31210=CARTESIAN_POINT('Ctrl Pts',(56.6302653132038,19.8505197836554,22.9446457263116));
#31211=CARTESIAN_POINT('Ctrl Pts',(56.6362507938172,19.8590677406693,22.9453197153147));
#31212=CARTESIAN_POINT('Ctrl Pts',(56.6385007830842,19.8623013293754,22.945573507638));
#31213=CARTESIAN_POINT('Ctrl Pts',(56.6432018901952,19.8691004329026,22.9461046583597));
#31214=CARTESIAN_POINT('Ctrl Pts',(56.6456510070594,19.8726672867907,22.9463818739079));
#31215=CARTESIAN_POINT('Ctrl Pts',(56.651616021782,19.8814154987903,22.9470583658351));
#31216=CARTESIAN_POINT('Ctrl Pts',(56.6551192039271,19.8866055536877,22.9474567902047));
#31217=CARTESIAN_POINT('Ctrl Pts',(56.6676886802169,19.9054179839502,22.9488907850934));
#31218=CARTESIAN_POINT('Ctrl Pts',(56.676611999672,19.9191357312973,22.9499172602975));
#31219=CARTESIAN_POINT('Ctrl Pts',(56.6984047254779,19.9535569273485,22.9524496949407));
#31220=CARTESIAN_POINT('Ctrl Pts',(56.7110656381577,19.9743898363287,22.9539441833923));
#31221=CARTESIAN_POINT('Ctrl Pts',(56.7632228016893,20.0638673946306,22.9602253631319));
#31222=CARTESIAN_POINT('Ctrl Pts',(56.7989971744072,20.134604110048,22.9648545623867));
#31223=CARTESIAN_POINT('Ctrl Pts',(56.8947068459724,20.3556092483932,22.9788526518921));
#31224=CARTESIAN_POINT('Ctrl Pts',(56.9406684338658,20.5111714294437,22.9881392547273));
#31225=CARTESIAN_POINT('Ctrl Pts',(56.9711531759364,20.6932257036802,22.9995173723624));
#31226=CARTESIAN_POINT('Ctrl Pts',(56.9745553031364,20.715946133555,23.000944868142));
#31227=CARTESIAN_POINT('Ctrl Pts',(56.9787959564025,20.7480425414306,23.0029740937289));
#31228=CARTESIAN_POINT('Ctrl Pts',(56.9799617716072,20.7573739994876,23.0035655512563));
#31229=CARTESIAN_POINT('Ctrl Pts',(56.9818791305782,20.7736561318084,23.0046003187129));
#31230=CARTESIAN_POINT('Ctrl Pts',(56.9826602037335,20.7806032147077,23.0050426941229));
#31231=CARTESIAN_POINT('Ctrl Pts',(56.9842197339272,20.7951630667022,23.0059717251293));
#31232=CARTESIAN_POINT('Ctrl Pts',(56.9849909328174,20.802776482892,23.0064586009335));
#31233=CARTESIAN_POINT('Ctrl Pts',(56.9867246823767,20.8209338162315,23.0076224191841));
#31234=CARTESIAN_POINT('Ctrl Pts',(56.9876471224384,20.8314812436545,23.0083006078862));
#31235=CARTESIAN_POINT('Ctrl Pts',(56.9904969979849,20.8673559553041,23.010614852929));
#31236=CARTESIAN_POINT('Ctrl Pts',(56.9920245610702,20.8927116461319,23.0122633205069));
#31237=CARTESIAN_POINT('Ctrl Pts',(56.9945275141777,20.953613520845,23.0162551983083));
#31238=CARTESIAN_POINT('Ctrl Pts',(56.995037378894,20.9891691149874,23.0186122673949));
#31239=CARTESIAN_POINT('Ctrl Pts',(56.9921803729877,21.2197163889459,23.0340688063671));
#31240=CARTESIAN_POINT('Ctrl Pts',(56.9611858366273,21.4132635714133,23.0479904204564));
#31241=CARTESIAN_POINT('Ctrl Pts',(56.889781330413,21.6399850368595,23.0641670603674));
#31242=CARTESIAN_POINT('Ctrl Pts',(56.8756340981315,21.6803320278049,23.0670339867784));
#31243=CARTESIAN_POINT('Ctrl Pts',(56.8572203117068,21.7278931206529,23.0703745713239));
#31244=CARTESIAN_POINT('Ctrl Pts',(56.8541926487967,21.735571416047,23.070912639284));
#31245=CARTESIAN_POINT('Ctrl Pts',(56.8491625288446,21.7480996127196,23.0717882834729));
#31246=CARTESIAN_POINT('Ctrl Pts',(56.8471884757789,21.7529607062207,23.0721274775284));
#31247=CARTESIAN_POINT('Ctrl Pts',(56.8436071185636,21.7616809239717,23.0727348578246));
#31248=CARTESIAN_POINT('Ctrl Pts',(56.84200684963,21.7655428168709,23.0730034543396));
#31249=CARTESIAN_POINT('Ctrl Pts',(56.8384771859602,21.7739857272321,23.0735898000635));
#31250=CARTESIAN_POINT('Ctrl Pts',(56.8365428085651,21.7785645656347,23.0739072441875));
#31251=CARTESIAN_POINT('Ctrl Pts',(56.8309728978997,21.7916127555847,23.0748104203925));
#31252=CARTESIAN_POINT('Ctrl Pts',(56.8272956978076,21.8000643400396,23.0753936944983));
#31253=CARTESIAN_POINT('Ctrl Pts',(56.8021160772697,21.8568572867254,23.0793034594482));
#31254=CARTESIAN_POINT('Ctrl Pts',(56.7787542471611,21.9043567777965,23.0825259438379));
#31255=CARTESIAN_POINT('Ctrl Pts',(56.6703689274799,22.1042323985453,23.0961143165011));
#31256=CARTESIAN_POINT('Ctrl Pts',(56.5674498107945,22.246021747285,23.1058931437571));
#31257=CARTESIAN_POINT('Ctrl Pts',(56.4049029290755,22.4174229264766,23.1200016429794));
#31258=CARTESIAN_POINT('Ctrl Pts',(56.3603616887444,22.4602242753475,23.1237536432254));
#31259=CARTESIAN_POINT('Ctrl Pts',(56.302655397468,22.5107416186355,23.1285264816614));
#31260=CARTESIAN_POINT('Ctrl Pts',(56.2912900158755,22.5204674934109,23.1294624231846));
#31261=CARTESIAN_POINT('Ctrl Pts',(56.2731653721166,22.535627782729,23.1309491977405));
#31262=CARTESIAN_POINT('Ctrl Pts',(56.2664780629372,22.5411476451347,23.1314965393039));
#31263=CARTESIAN_POINT('Ctrl Pts',(56.2539750022494,22.551331631308,23.1325177427869));
#31264=CARTESIAN_POINT('Ctrl Pts',(56.2481686622943,22.5560071094177,23.1329911350777));
#31265=CARTESIAN_POINT('Ctrl Pts',(56.2352343130173,22.5663033405105,23.1340438816937));
#31266=CARTESIAN_POINT('Ctrl Pts',(56.2280939029292,22.5719081791372,23.134623856791));
#31267=CARTESIAN_POINT('Ctrl Pts',(56.2072522369521,22.588039079482,23.1363134200241));
#31268=CARTESIAN_POINT('Ctrl Pts',(56.1934524442461,22.5984358960355,23.1374280493145));
#31269=CARTESIAN_POINT('Ctrl Pts',(56.0594988603445,22.6966553380409,23.1482116843996));
#31270=CARTESIAN_POINT('Ctrl Pts',(55.9300303282188,22.7709330836322,23.158412810211));
#31271=CARTESIAN_POINT('Ctrl Pts',(55.7879970687086,22.8325186641314,23.1692019539959));
#31272=CARTESIAN_POINT('Ctrl Pts',(55.7824454118992,22.8348959675945,23.1696229774918));
#31273=CARTESIAN_POINT('Ctrl Pts',(55.6660635245657,22.8841082213906,23.1784339184179));
#31274=CARTESIAN_POINT('Ctrl Pts',(55.5512214303481,22.9208499758922,23.1868586738788));
#31275=CARTESIAN_POINT('Ctrl Pts',(55.4183870749249,22.9504429886334,23.1958721356301));
#31276=CARTESIAN_POINT('Ctrl Pts',(55.4029742360403,22.9536855935929,23.1969068777261));
#31277=CARTESIAN_POINT('Ctrl Pts',(55.3812952865156,22.9579790055342,23.1983452503405));
#31278=CARTESIAN_POINT('Ctrl Pts',(55.3750605707958,22.9591828532656,23.1987569463429));
#31279=CARTESIAN_POINT('Ctrl Pts',(55.3649754571175,22.9610802591352,23.1994195975235));
#31280=CARTESIAN_POINT('Ctrl Pts',(55.3611286432068,22.9617922853275,23.1996715820059));
#31281=CARTESIAN_POINT('Ctrl Pts',(55.3529944451729,22.9632731486945,23.2002027400198));
#31282=CARTESIAN_POINT('Ctrl Pts',(55.3487065915121,22.9640392685493,23.2004817527859));
#31283=CARTESIAN_POINT('Ctrl Pts',(55.3381072579373,22.9658972686173,23.2011691097553));
#31284=CARTESIAN_POINT('Ctrl Pts',(55.3317928972795,22.9669728174655,23.2015765374078));
#31285=CARTESIAN_POINT('Ctrl Pts',(55.308368200945,22.9708468241331,23.2030807559671));
#31286=CARTESIAN_POINT('Ctrl Pts',(55.291226198336,22.9734526853042,23.204167241347));
#31287=CARTESIAN_POINT('Ctrl Pts',(55.2376252711634,22.9808872269974,23.2075261601569));
#31288=CARTESIAN_POINT('Ctrl Pts',(55.2010767496228,22.9849298544309,23.2097613072402));
#31289=CARTESIAN_POINT('Ctrl Pts',(55.164448305082,22.9879598379886,23.2119648302802));
#31290=CARTESIAN_POINT('Origin',(55.,21.,6.22095488139522));
#31291=CARTESIAN_POINT('',(55.1644484328881,22.9879598274162,24.1690565717028));
#31292=CARTESIAN_POINT('',(55.1644483449248,22.9879598346927,24.0089660407953));
#31293=CARTESIAN_POINT('',(55.1644483516311,22.987959834138,6.22095488139522));
#31294=CARTESIAN_POINT('Ctrl Pts',(55.1644484328881,22.9879598274162,24.1690565717028));
#31295=CARTESIAN_POINT('Ctrl Pts',(55.2278574488935,22.9827144933962,24.1653421584155));
#31296=CARTESIAN_POINT('Ctrl Pts',(55.2909969668646,22.9744369095191,24.1615920607638));
#31297=CARTESIAN_POINT('Ctrl Pts',(55.4047925019397,22.9539373158229,24.1546351819034));
#31298=CARTESIAN_POINT('Ctrl Pts',(55.4555517072851,22.9427300215604,24.1514590663388));
#31299=CARTESIAN_POINT('Ctrl Pts',(55.5191158365712,22.9260673540089,24.1473619840124));
#31300=CARTESIAN_POINT('Ctrl Pts',(55.5323825226982,22.9224425969265,24.1465002201414));
#31301=CARTESIAN_POINT('Ctrl Pts',(55.5536131967499,22.9164052844999,24.1451099885801));
#31302=CARTESIAN_POINT('Ctrl Pts',(55.5616015682748,22.9140795336627,24.1445843427756));
#31303=CARTESIAN_POINT('Ctrl Pts',(55.5767647130944,22.9095618104466,24.1435816273379));
#31304=CARTESIAN_POINT('Ctrl Pts',(55.5839421437628,22.9073791999503,24.1431048705318));
#31305=CARTESIAN_POINT('Ctrl Pts',(55.6002810082798,22.9023097901571,24.1420146380049));
#31306=CARTESIAN_POINT('Ctrl Pts',(55.6094341896089,22.8993972174951,24.1414003269731));
#31307=CARTESIAN_POINT('Ctrl Pts',(55.6332111148614,22.8916417603352,24.1397951139723));
#31308=CARTESIAN_POINT('Ctrl Pts',(55.6478002023449,22.8866954553319,24.1388008364628));
#31309=CARTESIAN_POINT('Ctrl Pts',(55.7890109192969,22.8369882496432,24.1290838788807));
#31310=CARTESIAN_POINT('Ctrl Pts',(55.9108401786786,22.7797251554187,24.1199333572215));
#31311=CARTESIAN_POINT('Ctrl Pts',(56.1181386276991,22.6553982213338,24.1031256116387));
#31312=CARTESIAN_POINT('Ctrl Pts',(56.2056874100779,22.5927637794189,24.0955716211202));
#31313=CARTESIAN_POINT('Ctrl Pts',(56.3217829935932,22.4946241422552,24.0852177535661));
#31314=CARTESIAN_POINT('Ctrl Pts',(56.3548303306389,22.4647344728215,24.0822285996259));
#31315=CARTESIAN_POINT('Ctrl Pts',(56.393189304029,22.4276305092686,24.0787353713917));
#31316=CARTESIAN_POINT('Ctrl Pts',(56.3994863396319,22.4214581597692,24.078161131154));
#31317=CARTESIAN_POINT('Ctrl Pts',(56.4092086264832,22.4118011469382,24.0772735983961));
#31318=CARTESIAN_POINT('Ctrl Pts',(56.4126622584889,22.4083454037042,24.0769581354393));
#31319=CARTESIAN_POINT('Ctrl Pts',(56.4190536744635,22.4019029145152,24.0763740425799));
#31320=CARTESIAN_POINT('Ctrl Pts',(56.4219947229854,22.3989196263637,24.076105162339));
#31321=CARTESIAN_POINT('Ctrl Pts',(56.4286784537155,22.3920970456884,24.0754938430999));
#31322=CARTESIAN_POINT('Ctrl Pts',(56.4324150654822,22.3882519189691,24.0751518762033));
#31323=CARTESIAN_POINT('Ctrl Pts',(56.4421260254281,22.378177992106,24.0742624676531));
#31324=CARTESIAN_POINT('Ctrl Pts',(56.4480756069747,22.3719253237596,24.0737168768965));
#31325=CARTESIAN_POINT('Ctrl Pts',(56.4882447178267,22.3291574504627,24.0700269729553));
#31326=CARTESIAN_POINT('Ctrl Pts',(56.5211233532755,22.2914009990119,24.0669752642144));
#31327=CARTESIAN_POINT('Ctrl Pts',(56.588221216425,22.2082254351498,24.0605778682594));
#31328=CARTESIAN_POINT('Ctrl Pts',(56.6219891695425,22.1625003741782,24.0572509093319));
#31329=CARTESIAN_POINT('Ctrl Pts',(56.7230902544962,22.0126009001958,24.046727412675));
#31330=CARTESIAN_POINT('Ctrl Pts',(56.782681589181,21.9035736458635,24.0396123859671));
#31331=CARTESIAN_POINT('Ctrl Pts',(56.8551336483146,21.7355206141634,24.0286553069179));
#31332=CARTESIAN_POINT('Ctrl Pts',(56.8760822205523,21.6803131041616,24.0250608104729));
#31333=CARTESIAN_POINT('Ctrl Pts',(56.8990300652018,21.6106694565227,24.0204924714197));
#31334=CARTESIAN_POINT('Ctrl Pts',(56.9033622962385,21.5970295855748,24.0195962418077));
#31335=CARTESIAN_POINT('Ctrl Pts',(56.9100163492697,21.575270711226,24.0181636376955));
#31336=CARTESIAN_POINT('Ctrl Pts',(56.9124340849827,21.5671813755035,24.0176304036652));
#31337=CARTESIAN_POINT('Ctrl Pts',(56.9168967570228,21.5518970309113,24.0166215907342));
#31338=CARTESIAN_POINT('Ctrl Pts',(56.9189527253857,21.5447053745374,24.0161463808844));
#31339=CARTESIAN_POINT('Ctrl Pts',(56.9235004777551,21.5284522610685,24.0150711156692));
#31340=CARTESIAN_POINT('Ctrl Pts',(56.925968756619,21.5193844661557,24.0144703096416));
#31341=CARTESIAN_POINT('Ctrl Pts',(56.9321378560755,21.4960720402998,24.0129232270118));
#31342=CARTESIAN_POINT('Ctrl Pts',(56.935745218384,21.4818034809731,24.0119739646326));
#31343=CARTESIAN_POINT('Ctrl Pts',(56.9583753609548,21.3879327638859,24.0057123054994));
#31344=CARTESIAN_POINT('Ctrl Pts',(56.9726391616497,21.3072743624777,24.00024903561));
#31345=CARTESIAN_POINT('Ctrl Pts',(56.9994110161194,21.0724741815147,23.9841229920169));
#31346=CARTESIAN_POINT('Ctrl Pts',(56.9990199022874,20.9174741845069,23.9731661659592));
#31347=CARTESIAN_POINT('Ctrl Pts',(56.9747462668238,20.7136761379846,23.9591287047738));
#31348=CARTESIAN_POINT('Ctrl Pts',(56.9668204613882,20.6635145995775,23.9557093049161));
#31349=CARTESIAN_POINT('Ctrl Pts',(56.9552215515261,20.6047538676348,23.9517864683638));
#31350=CARTESIAN_POINT('Ctrl Pts',(56.9533930810636,20.5958140289205,23.9511919427236));
#31351=CARTESIAN_POINT('Ctrl Pts',(56.9504777681279,20.5820423957456,23.9502799599097));
#31352=CARTESIAN_POINT('Ctrl Pts',(56.9494341984007,20.5772017143913,23.9499601412401));
#31353=CARTESIAN_POINT('Ctrl Pts',(56.947475845707,20.5682791521837,23.9493720669486));
#31354=CARTESIAN_POINT('Ctrl Pts',(56.9465662542278,20.564196284397,23.949103530915));
#31355=CARTESIAN_POINT('Ctrl Pts',(56.9444809133073,20.5549726428453,23.9484981256949));
#31356=CARTESIAN_POINT('Ctrl Pts',(56.9432976198474,20.5498336606666,23.9481616914997));
#31357=CARTESIAN_POINT('Ctrl Pts',(56.9401905925549,20.5365805738803,23.9472961538754));
#31358=CARTESIAN_POINT('Ctrl Pts',(56.9382363098146,20.5284736348841,23.9467687421765));
#31359=CARTESIAN_POINT('Ctrl Pts',(56.9255891212297,20.4774168997053,23.9434586574634));
#31360=CARTESIAN_POINT('Ctrl Pts',(56.9135191599593,20.4348171534066,23.9407482383574));
#31361=CARTESIAN_POINT('Ctrl Pts',(56.8411417775347,20.2083905910536,23.9264467006547));
#31362=CARTESIAN_POINT('Ctrl Pts',(56.7557530889236,20.0336707725478,23.9156868751425));
#31363=CARTESIAN_POINT('Ctrl Pts',(56.6162152604842,19.8296322137838,23.9008328584788));
#31364=CARTESIAN_POINT('Ctrl Pts',(56.58411905745,19.7865427252884,23.8975529917815));
#31365=CARTESIAN_POINT('Ctrl Pts',(56.5415794881433,19.734001016379,23.8933388227023));
#31366=CARTESIAN_POINT('Ctrl Pts',(56.5327210561125,19.7232905994466,23.8924680364628));
#31367=CARTESIAN_POINT('Ctrl Pts',(56.5183614046713,19.7062937089394,23.8910667131691));
#31368=CARTESIAN_POINT('Ctrl Pts',(56.5129312641996,19.6999475744826,23.8905390800347));
#31369=CARTESIAN_POINT('Ctrl Pts',(56.5025527829702,19.6879714648255,23.8895348209119));
#31370=CARTESIAN_POINT('Ctrl Pts',(56.4976122401817,19.6823348990479,23.889058522703));
#31371=CARTESIAN_POINT('Ctrl Pts',(56.486306265171,19.6695818664444,23.8879724688984));
#31372=CARTESIAN_POINT('Ctrl Pts',(56.4799213074308,19.6624830309295,23.887361901486));
#31373=CARTESIAN_POINT('Ctrl Pts',(56.4632312175164,19.6441927101101,23.8857728661002));
#31374=CARTESIAN_POINT('Ctrl Pts',(56.4528487337648,19.6330729577827,23.8847911332849));
#31375=CARTESIAN_POINT('Ctrl Pts',(56.3753215541541,19.5519216336571,23.8775082774481));
#31376=CARTESIAN_POINT('Ctrl Pts',(56.3032845171955,19.4867634763132,23.8709921160163));
#31377=CARTESIAN_POINT('Ctrl Pts',(56.1161180437961,19.3407795540519,23.8546778573428));
#31378=CARTESIAN_POINT('Ctrl Pts',(55.9966356774817,19.2663774826738,23.8447423161791));
#31379=CARTESIAN_POINT('Ctrl Pts',(55.8263437290236,19.1838023112513,23.8318135817867));
#31380=CARTESIAN_POINT('Ctrl Pts',(55.781577161115,19.1640925862992,23.8285237373053));
#31381=CARTESIAN_POINT('Ctrl Pts',(55.7277274570382,19.1427111163859,23.8247296097404));
#31382=CARTESIAN_POINT('Ctrl Pts',(55.7193045762337,19.1394328329818,23.8241407984635));
#31383=CARTESIAN_POINT('Ctrl Pts',(55.7062501622968,19.1344538044945,23.8232356970498));
#31384=CARTESIAN_POINT('Ctrl Pts',(55.7016342434948,19.1327128531093,23.8229170999324));
#31385=CARTESIAN_POINT('Ctrl Pts',(55.6930911279522,19.129526861767,23.822330159734));
#31386=CARTESIAN_POINT('Ctrl Pts',(55.6891658669211,19.1280770633056,23.8220615446272));
#31387=CARTESIAN_POINT('Ctrl Pts',(55.6802611863933,19.1248199179019,23.8214545596043));
#31388=CARTESIAN_POINT('Ctrl Pts',(55.6752791197591,19.1230200496571,23.8211166346995));
#31389=CARTESIAN_POINT('Ctrl Pts',(55.6604516622494,19.1177300207326,23.8201157222406));
#31390=CARTESIAN_POINT('Ctrl Pts',(55.6505857806225,19.1142972593132,23.8194560176971));
#31391=CARTESIAN_POINT('Ctrl Pts',(55.5527629968044,19.081119671006,23.812972578089));
#31392=CARTESIAN_POINT('Ctrl Pts',(55.4628453582455,19.0574687940955,23.8074703932382));
#31393=CARTESIAN_POINT('Ctrl Pts',(55.2401361014388,19.0152417635003,23.7942293860894));
#31394=CARTESIAN_POINT('Ctrl Pts',(55.1065074718338,19.0036067714459,23.7865885659887));
#31395=CARTESIAN_POINT('Ctrl Pts',(54.9114044695047,19.0062751445912,23.774923801163));
#31396=CARTESIAN_POINT('Ctrl Pts',(54.8501646632438,19.0099406494272,23.7711936969204));
#31397=CARTESIAN_POINT('Ctrl Pts',(54.7748004241117,19.0179499861071,23.7664730489652));
#31398=CARTESIAN_POINT('Ctrl Pts',(54.7604232368745,19.0196363809469,23.7655666746434));
#31399=CARTESIAN_POINT('Ctrl Pts',(54.7376559337581,19.0225584592186,23.7641215996191));
#31400=CARTESIAN_POINT('Ctrl Pts',(54.729252971863,19.0236914462918,23.7635861358629));
#31401=CARTESIAN_POINT('Ctrl Pts',(54.7134563790515,19.0259239660321,23.7625754347905));
#31402=CARTESIAN_POINT('Ctrl Pts',(54.7060611874405,19.0270115543746,23.7621005826464));
#31403=CARTESIAN_POINT('Ctrl Pts',(54.689437101637,19.0295519467769,23.7610292473917));
#31404=CARTESIAN_POINT('Ctrl Pts',(54.6802119996413,19.0310280666782,23.7604320361217));
#31405=CARTESIAN_POINT('Ctrl Pts',(54.6566608028872,19.0349663988157,23.758900323075));
#31406=CARTESIAN_POINT('Ctrl Pts',(54.6423508304461,19.0375204686403,23.7579629348897));
#31407=CARTESIAN_POINT('Ctrl Pts',(54.5523804517107,19.0545952589935,23.7520259440463));
#31408=CARTESIAN_POINT('Ctrl Pts',(54.4775957104705,19.0733308455812,23.7468933019434));
#31409=CARTESIAN_POINT('Ctrl Pts',(54.2522767857922,19.143863454152,23.7308232857337));
#31410=CARTESIAN_POINT('Ctrl Pts',(54.1067121862988,19.2093681438856,23.7195359005349));
#31411=CARTESIAN_POINT('Ctrl Pts',(53.9409992303602,19.3092221894913,23.7062986631718));
#31412=CARTESIAN_POINT('Ctrl Pts',(53.9119815592086,19.327747511516,23.7039675298469));
#31413=CARTESIAN_POINT('Ctrl Pts',(53.8659769094769,19.3588223373338,23.700266963215));
#31414=CARTESIAN_POINT('Ctrl Pts',(53.8486850809592,19.3709062231818,23.6988749161295));
#31415=CARTESIAN_POINT('Ctrl Pts',(53.8259913050678,19.3873069669499,23.6970499228626));
#31416=CARTESIAN_POINT('Ctrl Pts',(53.8204161690311,19.391380335896,23.696601738528));
#31417=CARTESIAN_POINT('Ctrl Pts',(53.8112719332227,19.3981345037371,23.695867048822));
#31418=CARTESIAN_POINT('Ctrl Pts',(53.8076905369639,19.4007984397911,23.6955794085762));
#31419=CARTESIAN_POINT('Ctrl Pts',(53.800686911998,19.4060445245249,23.6950171684617));
#31420=CARTESIAN_POINT('Ctrl Pts',(53.7972640259651,19.408625713999,23.6947425086883));
#31421=CARTESIAN_POINT('Ctrl Pts',(53.7888524726667,19.4150114857118,23.6940677826427));
#31422=CARTESIAN_POINT('Ctrl Pts',(53.7838733285206,19.4188286478513,23.693668589046));
#31423=CARTESIAN_POINT('Ctrl Pts',(53.7668232401048,19.4320279439866,23.6923020152519));
#31424=CARTESIAN_POINT('Ctrl Pts',(53.7548418393424,19.4415255927732,23.6913423672132));
#31425=CARTESIAN_POINT('Ctrl Pts',(53.6411844700034,19.5337692810685,23.6822325650844));
#31426=CARTESIAN_POINT('Ctrl Pts',(53.5477744287519,19.6262231051083,23.6746820892311));
#31427=CARTESIAN_POINT('Ctrl Pts',(53.4010029422945,19.80333143732,23.6613359711608));
#31428=CARTESIAN_POINT('Ctrl Pts',(53.3436546888174,19.8840585072693,23.6555854122675));
#31429=CARTESIAN_POINT('Ctrl Pts',(53.2656466113675,20.0132122387942,23.6465075020604));
#31430=CARTESIAN_POINT('Ctrl Pts',(53.2405141277928,20.0587558673,23.6433292366863));
#31431=CARTESIAN_POINT('Ctrl Pts',(53.2110205619976,20.1175209015712,23.6392297264973));
#31432=CARTESIAN_POINT('Ctrl Pts',(53.2049775993265,20.129878540189,23.6383677722817));
#31433=CARTESIAN_POINT('Ctrl Pts',(53.1954852936865,20.1498097436006,23.6369773067224));
#31434=CARTESIAN_POINT('Ctrl Pts',(53.1919546220124,20.1573442546834,23.6364516189851));
#31435=CARTESIAN_POINT('Ctrl Pts',(53.1853306042956,20.1717133199875,23.6354488713851));
#31436=CARTESIAN_POINT('Ctrl Pts',(53.1822284648573,20.1785436813219,23.6349721246668));
#31437=CARTESIAN_POINT('Ctrl Pts',(53.1752428417722,20.1941581319422,23.6338819823226));
#31438=CARTESIAN_POINT('Ctrl Pts',(53.1713841449312,20.2029530427416,23.6332677518921));
#31439=CARTESIAN_POINT('Ctrl Pts',(53.1615036610038,20.2259225170042,23.6316628877564));
#31440=CARTESIAN_POINT('Ctrl Pts',(53.1555823418622,20.2401393427404,23.630668880916));
#31441=CARTESIAN_POINT('Ctrl Pts',(53.1108661960963,20.3511039136503,23.6229036393757));
#31442=CARTESIAN_POINT('Ctrl Pts',(53.0795501588148,20.4506741312491,23.6158825461797));
#31443=CARTESIAN_POINT('Ctrl Pts',(53.0222733386474,20.6993170214271,23.5982938948018));
#31444=CARTESIAN_POINT('Ctrl Pts',(53.0051951726877,20.8497790334131,23.5875816050759));
#31445=CARTESIAN_POINT('Ctrl Pts',(53.005261785231,21.0327320230545,23.5752406874897));
#31446=CARTESIAN_POINT('Ctrl Pts',(53.006043736852,21.0647350499803,23.5731092580746));
#31447=CARTESIAN_POINT('Ctrl Pts',(53.0079957634069,21.1049514524451,23.5704762816586));
#31448=CARTESIAN_POINT('Ctrl Pts',(53.0084470821659,21.1131930525887,23.5699391113804));
#31449=CARTESIAN_POINT('Ctrl Pts',(53.009242377354,21.1262330720561,23.5690932542597));
#31450=CARTESIAN_POINT('Ctrl Pts',(53.0095525719062,21.1310333460878,23.5687827508951));
#31451=CARTESIAN_POINT('Ctrl Pts',(53.0101374746282,21.1396029183349,23.5682300468477));
#31452=CARTESIAN_POINT('Ctrl Pts',(53.0104055281421,21.1433725307798,23.5679874849649));
#31453=CARTESIAN_POINT('Ctrl Pts',(53.0110713778308,21.1523746519575,23.5674095525719));
#31454=CARTESIAN_POINT('Ctrl Pts',(53.0114791093999,21.1576063698247,23.5670747413607));
#31455=CARTESIAN_POINT('Ctrl Pts',(53.0127685049821,21.1733487731796,23.5660703202624));
#31456=CARTESIAN_POINT('Ctrl Pts',(53.0137129091456,21.1838543340842,23.5654041048098));
#31457=CARTESIAN_POINT('Ctrl Pts',(53.0160838316053,21.2080727197732,23.5638766749151));
#31458=CARTESIAN_POINT('Ctrl Pts',(53.0175692827296,21.2217793815065,23.5630184267433));
#31459=CARTESIAN_POINT('Ctrl Pts',(53.0230946135337,21.2682591687343,23.5601258665221));
#31460=CARTESIAN_POINT('Ctrl Pts',(53.0278062533681,21.3009484349768,23.5581215919491));
#31461=CARTESIAN_POINT('Ctrl Pts',(53.0572521287678,21.4745889248671,23.5475650709058));
#31462=CARTESIAN_POINT('Ctrl Pts',(53.0962890070089,21.6126940982866,23.5394588729822));
#31463=CARTESIAN_POINT('Ctrl Pts',(53.1849082253035,21.8326523066063,23.5255368170095));
#31464=CARTESIAN_POINT('Ctrl Pts',(53.2261626605271,21.9172599176625,23.5199133766742));
#31465=CARTESIAN_POINT('Ctrl Pts',(53.280798575232,22.0117326111282,23.5131361117721));
#31466=CARTESIAN_POINT('Ctrl Pts',(53.2885206459475,22.0247413411533,23.5121915451495));
#31467=CARTESIAN_POINT('Ctrl Pts',(53.3013431448295,22.0457930588591,23.5106437142266));
#31468=CARTESIAN_POINT('Ctrl Pts',(53.3063546173168,22.0538897220427,23.5100436910415));
#31469=CARTESIAN_POINT('Ctrl Pts',(53.3154125996122,22.0682925584727,23.508967720244));
#31470=CARTESIAN_POINT('Ctrl Pts',(53.3194370575568,22.0746124389834,23.5084925927916));
#31471=CARTESIAN_POINT('Ctrl Pts',(53.3280309105786,22.0879416043895,23.5074840631513));
#31472=CARTESIAN_POINT('Ctrl Pts',(53.3326089827357,22.094945095688,23.5069503439587));
#31473=CARTESIAN_POINT('Ctrl Pts',(53.3449460588823,22.1135614364283,23.5055213031828));
#31474=CARTESIAN_POINT('Ctrl Pts',(53.3527830799339,22.1251217811847,23.5046230642647));
#31475=CARTESIAN_POINT('Ctrl Pts',(53.3918170533879,22.1814185269128,23.5001944631864));
#31476=CARTESIAN_POINT('Ctrl Pts',(53.4247157217733,22.2249410664469,23.496599630525));
#31477=CARTESIAN_POINT('Ctrl Pts',(53.5879716613595,22.4234479175594,23.4793616150222));
#31478=CARTESIAN_POINT('Ctrl Pts',(53.7396201366567,22.5593100336184,23.4648613802283));
#31479=CARTESIAN_POINT('Ctrl Pts',(53.9387495259889,22.6893873506059,23.4487685603017));
#31480=CARTESIAN_POINT('Ctrl Pts',(53.9689168893588,22.7079666787367,23.4464040526565));
#31481=CARTESIAN_POINT('Ctrl Pts',(54.0069558825313,22.7300184746869,23.4435270539493));
#31482=CARTESIAN_POINT('Ctrl Pts',(54.0143741946855,22.7342555521636,23.442970808694));
#31483=CARTESIAN_POINT('Ctrl Pts',(54.0260697310895,22.740836343767,23.4421016689838));
#31484=CARTESIAN_POINT('Ctrl Pts',(54.0303286156587,22.7432121936547,23.4417867920909));
#31485=CARTESIAN_POINT('Ctrl Pts',(54.0382631453654,22.7476004532246,23.4412032210433));
#31486=CARTESIAN_POINT('Ctrl Pts',(54.0419363883678,22.7496168832681,23.4409342806353));
#31487=CARTESIAN_POINT('Ctrl Pts',(54.0503352261351,22.7541930514267,23.440322103096));
#31488=CARTESIAN_POINT('Ctrl Pts',(54.055064824387,22.756745274623,23.4399793433694));
#31489=CARTESIAN_POINT('Ctrl Pts',(54.0696717109687,22.7645515010465,23.438926651256));
#31490=CARTESIAN_POINT('Ctrl Pts',(54.0795831320692,22.7697416557472,23.4382206125345));
#31491=CARTESIAN_POINT('Ctrl Pts',(54.1832465969071,22.8229189610767,23.4309163007775));
#31492=CARTESIAN_POINT('Ctrl Pts',(54.2806292909887,22.8634998689112,23.4247290155489));
#31493=CARTESIAN_POINT('Ctrl Pts',(54.5407342649076,22.9484400449457,23.4088071670829));
#31494=CARTESIAN_POINT('Ctrl Pts',(54.7066419119843,22.9802219036377,23.3991702876915));
#31495=CARTESIAN_POINT('Ctrl Pts',(54.8950816066056,22.9920949487837,23.3875241719794));
#31496=CARTESIAN_POINT('Ctrl Pts',(54.9156160984686,22.993070360752,23.3862470066826));
#31497=CARTESIAN_POINT('Ctrl Pts',(54.947221891206,22.9940823686731,23.3842671893001));
#31498=CARTESIAN_POINT('Ctrl Pts',(54.9582849293128,22.9943444704469,23.3835715464159));
#31499=CARTESIAN_POINT('Ctrl Pts',(54.9763192271522,22.9946216115993,23.3824330168959));
#31500=CARTESIAN_POINT('Ctrl Pts',(54.983289494628,22.9946921841389,23.3819918711408));
#31501=CARTESIAN_POINT('Ctrl Pts',(54.9979353102157,22.9947636984397,23.3810625599421));
#31502=CARTESIAN_POINT('Ctrl Pts',(55.005610765536,22.9947568754515,23.3805741593405));
#31503=CARTESIAN_POINT('Ctrl Pts',(55.0239895699,22.9946344619003,23.3794013085571));
#31504=CARTESIAN_POINT('Ctrl Pts',(55.0346923124084,22.9944770171974,23.3787155625139));
#31505=CARTESIAN_POINT('Ctrl Pts',(55.0714859441515,22.9936395139523,23.3763483885824));
#31506=CARTESIAN_POINT('Ctrl Pts',(55.0975635324336,22.9925335635314,23.3746537710115));
#31507=CARTESIAN_POINT('Ctrl Pts',(55.1372340497878,22.9900705221096,23.3720489315753));
#31508=CARTESIAN_POINT('Ctrl Pts',(55.1508472364672,22.9890849479159,23.371150237346));
#31509=CARTESIAN_POINT('Ctrl Pts',(55.1644483538502,22.9879598339544,23.3702474674336));
#31510=CARTESIAN_POINT('',(53.0052508822312,20.9981658358939,23.4208211887813));
#31511=CARTESIAN_POINT('Ctrl Pts',(55.164448305082,22.9879598379886,23.2119648302802));
#31512=CARTESIAN_POINT('Ctrl Pts',(55.0991263259238,22.9933634123224,23.2158945217506));
#31513=CARTESIAN_POINT('Ctrl Pts',(55.033550205288,22.9955463711911,23.2197243986835));
#31514=CARTESIAN_POINT('Ctrl Pts',(54.8064007976559,22.9918972263633,23.2329283338445));
#31515=CARTESIAN_POINT('Ctrl Pts',(54.6457766981688,22.9696839662503,23.2422120601349));
#31516=CARTESIAN_POINT('Ctrl Pts',(54.4673973487199,22.9224695711337,23.2535861794245));
#31517=CARTESIAN_POINT('Ctrl Pts',(54.4453031849839,22.9162114214996,23.255013042448));
#31518=CARTESIAN_POINT('Ctrl Pts',(54.4143219137268,22.9068553022161,23.2570415141568));
#31519=CARTESIAN_POINT('Ctrl Pts',(54.4053406240195,22.9040735768447,23.2576328608777));
#31520=CARTESIAN_POINT('Ctrl Pts',(54.3897167567491,22.8991131592788,23.2586674900303));
#31521=CARTESIAN_POINT('Ctrl Pts',(54.3830652918374,22.896962833737,23.2591098385876));
#31522=CARTESIAN_POINT('Ctrl Pts',(54.3691560836983,22.8923852887287,23.2600388683995));
#31523=CARTESIAN_POINT('Ctrl Pts',(54.3619007440387,22.8899511804784,23.2605257701469));
#31524=CARTESIAN_POINT('Ctrl Pts',(54.3448392418368,22.8841177400253,23.2616762730441));
#31525=CARTESIAN_POINT('Ctrl Pts',(54.3350453223651,22.8806835319282,23.2623410176298));
#31526=CARTESIAN_POINT('Ctrl Pts',(54.3023860367182,22.8689446505354,23.2645724311521));
#31527=CARTESIAN_POINT('Ctrl Pts',(54.2796465986697,22.8602984273747,23.2661503723539));
#31528=CARTESIAN_POINT('Ctrl Pts',(54.2255913825251,22.8386053073891,23.2699615121339));
#31529=CARTESIAN_POINT('Ctrl Pts',(54.1944400246391,22.8251715215852,23.2722070828989));
#31530=CARTESIAN_POINT('Ctrl Pts',(54.0064537875455,22.7383537477567,23.2860635705158));
#31531=CARTESIAN_POINT('Ctrl Pts',(53.8593935104238,22.645602571587,23.2983126821385));
#31532=CARTESIAN_POINT('Ctrl Pts',(53.7108572168926,22.522345275487,23.3116270570718));
#31533=CARTESIAN_POINT('Ctrl Pts',(53.6957209447134,22.5093973756668,23.3129950026004));
#31534=CARTESIAN_POINT('Ctrl Pts',(53.6454872049498,22.4651063562734,23.3175666527756));
#31535=CARTESIAN_POINT('Ctrl Pts',(53.6113024340647,22.4327461086395,23.3207313592904));
#31536=CARTESIAN_POINT('Ctrl Pts',(53.5723411889971,22.3931582258712,23.3243713105746));
#31537=CARTESIAN_POINT('Ctrl Pts',(53.5664293799758,22.3870741892434,23.3249245546237));
#31538=CARTESIAN_POINT('Ctrl Pts',(53.5568760678426,22.3771162408892,23.3258198323081));
#31539=CARTESIAN_POINT('Ctrl Pts',(53.5532109955784,22.373265233944,23.3261636043928));
#31540=CARTESIAN_POINT('Ctrl Pts',(53.5466885654262,22.366356815639,23.3267758573086));
#31541=CARTESIAN_POINT('Ctrl Pts',(53.543825398956,22.3633050303755,23.3270447783194));
#31542=CARTESIAN_POINT('Ctrl Pts',(53.5376195220838,22.3566484684455,23.3276279994759));
#31543=CARTESIAN_POINT('Ctrl Pts',(53.5342805319479,22.3530403435809,23.3279420189467));
#31544=CARTESIAN_POINT('Ctrl Pts',(53.5274159744056,22.345567247119,23.3285881636097));
#31545=CARTESIAN_POINT('Ctrl Pts',(53.523892199814,22.341700671773,23.3289201560256));
#31546=CARTESIAN_POINT('Ctrl Pts',(53.5071018741299,22.3231307322401,23.3305037943368));
#31547=CARTESIAN_POINT('Ctrl Pts',(53.4940390116084,22.3082436013264,23.3317410915564));
#31548=CARTESIAN_POINT('Ctrl Pts',(53.4286731284674,22.2314723959766,23.3379744079782));
#31549=CARTESIAN_POINT('Ctrl Pts',(53.3799484704837,22.1666311447625,23.3427627309584));
#31550=CARTESIAN_POINT('Ctrl Pts',(53.2937774319601,22.0361042220352,23.3518940304228));
#31551=CARTESIAN_POINT('Ctrl Pts',(53.2558531578978,21.970906465801,23.3562377114781));
#31552=CARTESIAN_POINT('Ctrl Pts',(53.1703758829508,21.8027087107385,23.3672401135191));
#31553=CARTESIAN_POINT('Ctrl Pts',(53.1277492439044,21.6975225571349,23.3739531089497));
#31554=CARTESIAN_POINT('Ctrl Pts',(53.0896975623514,21.5744676285229,23.3819476488903));
#31555=CARTESIAN_POINT('Ctrl Pts',(53.085285662596,21.5595868515015,23.3829163660343));
#31556=CARTESIAN_POINT('Ctrl Pts',(53.078416135962,21.5353839016736,23.3844957994014));
#31557=CARTESIAN_POINT('Ctrl Pts',(53.0758515948601,21.5260925569232,23.385103045895));
#31558=CARTESIAN_POINT('Ctrl Pts',(53.0714104344116,21.5095352404554,23.3861869462143));
#31559=CARTESIAN_POINT('Ctrl Pts',(53.0695072758501,21.5022765306617,23.3866627314725));
#31560=CARTESIAN_POINT('Ctrl Pts',(53.065585955783,21.4869689153054,23.3876674457245));
#31561=CARTESIAN_POINT('Ctrl Pts',(53.063576975258,21.4789178267269,23.3881966606351));
#31562=CARTESIAN_POINT('Ctrl Pts',(53.0595976188397,21.4625358849382,23.3892751560575));
#31563=CARTESIAN_POINT('Ctrl Pts',(53.0576305228776,21.4542044211841,23.3898245298029));
#31564=CARTESIAN_POINT('Ctrl Pts',(53.0528834004297,21.4335034497103,23.3911918184686));
#31565=CARTESIAN_POINT('Ctrl Pts',(53.0501675871054,21.4211197484581,23.3920117646553));
#31566=CARTESIAN_POINT('Ctrl Pts',(53.0193000797086,21.2736644283603,23.4018000996712));
#31567=CARTESIAN_POINT('Ctrl Pts',(53.0051240058792,21.1360799458073,23.4112224742061));
#31568=CARTESIAN_POINT('Ctrl Pts',(53.0052508435975,20.9981654614968,23.4208211472388));
#31569=CARTESIAN_POINT('Ctrl Pts',(53.0052508432575,20.9981658311762,23.4208211215096));
#31570=CARTESIAN_POINT('Ctrl Pts',(53.005371052201,20.867432669888,23.429919983384));
#31571=CARTESIAN_POINT('Ctrl Pts',(53.0183428780867,20.7370158548825,23.4391245158));
#31572=CARTESIAN_POINT('Ctrl Pts',(53.0466488227188,20.5954867718677,23.4487342893852));
#31573=CARTESIAN_POINT('Ctrl Pts',(53.049446452778,20.5822050079215,23.4496321051015));
#31574=CARTESIAN_POINT('Ctrl Pts',(53.0539722639705,20.5617558432602,23.4510071637296));
#31575=CARTESIAN_POINT('Ctrl Pts',(53.0556049194828,20.554568001693,23.4514891040053));
#31576=CARTESIAN_POINT('Ctrl Pts',(53.0587334361215,20.5411395979358,23.4523866575698));
#31577=CARTESIAN_POINT('Ctrl Pts',(53.0602196369505,20.5348969076754,23.4528027775369));
#31578=CARTESIAN_POINT('Ctrl Pts',(53.0627657417058,20.5244266783544,23.4534986499897));
#31579=CARTESIAN_POINT('Ctrl Pts',(53.0638094117212,20.5201952868669,23.4537793147855));
#31580=CARTESIAN_POINT('Ctrl Pts',(53.0658157386696,20.5121741150133,23.4543102414826));
#31581=CARTESIAN_POINT('Ctrl Pts',(53.0667756814197,20.508383700906,23.4545606613191));
#31582=CARTESIAN_POINT('Ctrl Pts',(53.0693209400191,20.4984562778836,23.4552153582743));
#31583=CARTESIAN_POINT('Ctrl Pts',(53.0709243878838,20.4923238993149,23.4556186002173));
#31584=CARTESIAN_POINT('Ctrl Pts',(53.0765961963292,20.4710470028298,23.4570139235789));
#31585=CARTESIAN_POINT('Ctrl Pts',(53.0808140084591,20.4559424377483,23.4579978295762));
#31586=CARTESIAN_POINT('Ctrl Pts',(53.1195845986196,20.3231646828597,23.4666009701352));
#31587=CARTESIAN_POINT('Ctrl Pts',(53.1647481064187,20.2088445237748,23.4736985692407));
#31588=CARTESIAN_POINT('Ctrl Pts',(53.2674181349835,20.0059399127586,23.4868916015663));
#31589=CARTESIAN_POINT('Ctrl Pts',(53.3219852286993,19.9163673527866,23.4929621066318));
#31590=CARTESIAN_POINT('Ctrl Pts',(53.4147887694859,19.7879697122599,23.5024816549071));
#31591=CARTESIAN_POINT('Ctrl Pts',(53.4479927339966,19.7457333883856,23.5057610696224));
#31592=CARTESIAN_POINT('Ctrl Pts',(53.4916360087646,19.694607944774,23.5099510742376));
#31593=CARTESIAN_POINT('Ctrl Pts',(53.5005180065553,19.6844149267343,23.5107979351905));
#31594=CARTESIAN_POINT('Ctrl Pts',(53.5151292380655,19.6679872155712,23.5121820733801));
#31595=CARTESIAN_POINT('Ctrl Pts',(53.5207958575069,19.6616972170761,23.512716736701));
#31596=CARTESIAN_POINT('Ctrl Pts',(53.5315400455793,19.6499226747893,23.5137265888208));
#31597=CARTESIAN_POINT('Ctrl Pts',(53.5366087460332,19.6444302094296,23.5142013972969));
#31598=CARTESIAN_POINT('Ctrl Pts',(53.5480913277272,19.6321270923832,23.5152735186442));
#31599=CARTESIAN_POINT('Ctrl Pts',(53.5545224612008,19.6253328534108,23.515871565598));
#31600=CARTESIAN_POINT('Ctrl Pts',(53.5711000115471,19.6080642820284,23.5174071497393));
#31601=CARTESIAN_POINT('Ctrl Pts',(53.5813137887221,19.5976556645577,23.5183475994617));
#31602=CARTESIAN_POINT('Ctrl Pts',(53.6471344163324,19.5320344761336,23.5243736180764));
#31603=CARTESIAN_POINT('Ctrl Pts',(53.7058330721819,19.4800337815536,23.5295970182413));
#31604=CARTESIAN_POINT('Ctrl Pts',(53.8835586632631,19.340361215746,23.5449932789214));
#31605=CARTESIAN_POINT('Ctrl Pts',(54.009461454125,19.2622804117087,23.5554417793021));
#31606=CARTESIAN_POINT('Ctrl Pts',(54.196287797516,19.1733686297209,23.5696734898399));
#31607=CARTESIAN_POINT('Ctrl Pts',(54.2508807079937,19.1503088936273,23.5736876174422));
#31608=CARTESIAN_POINT('Ctrl Pts',(54.3159176450354,19.1261906675119,23.5782411913554));
#31609=CARTESIAN_POINT('Ctrl Pts',(54.3254380311283,19.122742360948,23.5789021393181));
#31610=CARTESIAN_POINT('Ctrl Pts',(54.3399674139916,19.1176045893399,23.5799018568847));
#31611=CARTESIAN_POINT('Ctrl Pts',(54.3449573827806,19.1158623543236,23.5802435969681));
#31612=CARTESIAN_POINT('Ctrl Pts',(54.3539085058441,19.1127769508369,23.5808536763409));
#31613=CARTESIAN_POINT('Ctrl Pts',(54.3578670000827,19.1114263933958,23.5811224425567));
#31614=CARTESIAN_POINT('Ctrl Pts',(54.366509826161,19.1085079535311,23.5817070019089));
#31615=CARTESIAN_POINT('Ctrl Pts',(54.3711957356444,19.1069450191265,23.582022503755));
#31616=CARTESIAN_POINT('Ctrl Pts',(54.3842672039095,19.1026390627224,23.5828987500165));
#31617=CARTESIAN_POINT('Ctrl Pts',(54.3926653501125,19.0999342031445,23.5834573121264));
#31618=CARTESIAN_POINT('Ctrl Pts',(54.4385349907675,19.0854957903425,23.5864855465748));
#31619=CARTESIAN_POINT('Ctrl Pts',(54.476331523129,19.0748140009854,23.5888990327003));
#31620=CARTESIAN_POINT('Ctrl Pts',(54.7069281786897,19.0169393383591,23.6032698149354));
#31621=CARTESIAN_POINT('Ctrl Pts',(54.9055766203397,18.997621295714,23.6142784303345));
#31622=CARTESIAN_POINT('Ctrl Pts',(55.1579398194784,19.0107742513284,23.629458874477));
#31623=CARTESIAN_POINT('Ctrl Pts',(55.2119142849729,19.0157984969555,23.6327671060513));
#31624=CARTESIAN_POINT('Ctrl Pts',(55.2794252266827,19.0248687892531,23.6370130942451));
#31625=CARTESIAN_POINT('Ctrl Pts',(55.2932163898071,19.0268690134407,23.6378861250292));
#31626=CARTESIAN_POINT('Ctrl Pts',(55.3152443075999,19.030299906895,23.6392901085783));
#31627=CARTESIAN_POINT('Ctrl Pts',(55.3234951524013,19.0316381650779,23.639818136255));
#31628=CARTESIAN_POINT('Ctrl Pts',(55.3391242880388,19.0342740780151,23.6408225307277));
#31629=CARTESIAN_POINT('Ctrl Pts',(55.3465041732239,19.0355615208083,23.6412985658234));
#31630=CARTESIAN_POINT('Ctrl Pts',(55.3632547980467,19.0385810432972,23.6423831653956));
#31631=CARTESIAN_POINT('Ctrl Pts',(55.372620674372,19.0403387538053,23.6429925348494));
#31632=CARTESIAN_POINT('Ctrl Pts',(55.3968498090622,19.0450658525299,23.6445767121868));
#31633=CARTESIAN_POINT('Ctrl Pts',(55.4116922382151,19.048137614523,23.6455547533047));
#31634=CARTESIAN_POINT('Ctrl Pts',(55.5194257096349,19.0717174066035,23.6527106456975));
#31635=CARTESIAN_POINT('Ctrl Pts',(55.6107655960914,19.0986748134007,23.6590948769539));
#31636=CARTESIAN_POINT('Ctrl Pts',(55.8329023582963,19.1818974140789,23.6753852741072));
#31637=CARTESIAN_POINT('Ctrl Pts',(55.9602640737285,19.2458296468731,23.6854467049082));
#31638=CARTESIAN_POINT('Ctrl Pts',(56.1210638884837,19.3493462861587,23.698512928518));
#31639=CARTESIAN_POINT('Ctrl Pts',(56.1613863401268,19.3774635310095,23.7018196737397));
#31640=CARTESIAN_POINT('Ctrl Pts',(56.2078578281129,19.4124897192678,23.7056304951447));
#31641=CARTESIAN_POINT('Ctrl Pts',(56.2150461634527,19.4179847495933,23.7062199470105));
#31642=CARTESIAN_POINT('Ctrl Pts',(56.2260967556087,19.4265519846505,23.7071257625892));
#31643=CARTESIAN_POINT('Ctrl Pts',(56.229985307592,19.4295898448149,23.7074444397174));
#31644=CARTESIAN_POINT('Ctrl Pts',(56.2371493546468,19.4352295585967,23.7080313654027));
#31645=CARTESIAN_POINT('Ctrl Pts',(56.2404279189602,19.4378272699812,23.7082998870417));
#31646=CARTESIAN_POINT('Ctrl Pts',(56.2478358076809,19.4437348027416,23.7089064506153));
#31647=CARTESIAN_POINT('Ctrl Pts',(56.2519601409186,19.4470507496263,23.7092440493147));
#31648=CARTESIAN_POINT('Ctrl Pts',(56.2641702926548,19.4569479191527,23.710243369011));
#31649=CARTESIAN_POINT('Ctrl Pts',(56.2722179154558,19.4635762824884,23.7109018214867));
#31650=CARTESIAN_POINT('Ctrl Pts',(56.3470576451503,19.5262086915572,23.7170273620546));
#31651=CARTESIAN_POINT('Ctrl Pts',(56.4101725284991,19.5864786758345,23.7222115284933));
#31652=CARTESIAN_POINT('Ctrl Pts',(56.5729915112007,19.7637586484671,23.7363018894857));
#31653=CARTESIAN_POINT('Ctrl Pts',(56.6634305585103,19.8884277457925,23.7450290716835));
#31654=CARTESIAN_POINT('Ctrl Pts',(56.7546244847892,20.0505902900363,23.7562453171472));
#31655=CARTESIAN_POINT('Ctrl Pts',(56.769873829009,20.0793304943032,23.7582263709569));
#31656=CARTESIAN_POINT('Ctrl Pts',(56.7950144539179,20.1296476191352,23.7616925939171));
#31657=CARTESIAN_POINT('Ctrl Pts',(56.8052362314239,20.1510522802272,23.7631664351786));
#31658=CARTESIAN_POINT('Ctrl Pts',(56.8193470948104,20.1820086379003,23.7652993706655));
#31659=CARTESIAN_POINT('Ctrl Pts',(56.823547836053,20.1914166690451,23.7659477745376));
#31660=CARTESIAN_POINT('Ctrl Pts',(56.8307211482963,20.2078223453816,23.7670789572054));
#31661=CARTESIAN_POINT('Ctrl Pts',(56.8337269736865,20.2148052836009,23.7675605912004));
#31662=CARTESIAN_POINT('Ctrl Pts',(56.839445028349,20.2283010164013,23.7684918066029));
#31663=CARTESIAN_POINT('Ctrl Pts',(56.8421627724346,20.2348113622403,23.7689411920937));
#31664=CARTESIAN_POINT('Ctrl Pts',(56.8485195897429,20.250269255431,23.7700086545812));
#31665=CARTESIAN_POINT('Ctrl Pts',(56.8521282942499,20.2592290237748,23.7706277455539));
#31666=CARTESIAN_POINT('Ctrl Pts',(56.8646507435292,20.2909836236564,23.7728233843142));
#31667=CARTESIAN_POINT('Ctrl Pts',(56.8732095814058,20.3139151707046,23.7744117117489));
#31668=CARTESIAN_POINT('Ctrl Pts',(56.9388318215794,20.5001256640484,23.7873367104232));
#31669=CARTESIAN_POINT('Ctrl Pts',(56.974848418882,20.6700102735432,23.7993922282362));
#31670=CARTESIAN_POINT('Ctrl Pts',(56.9962064607337,20.9394302046381,23.8182155831398));
#31671=CARTESIAN_POINT('Ctrl Pts',(56.9967845640676,21.0369432146682,23.8249461261145));
#31672=CARTESIAN_POINT('Ctrl Pts',(56.989476557572,21.1453898907522,23.8320931520076));
#31673=CARTESIAN_POINT('Ctrl Pts',(56.9886212060638,21.1566553749929,23.8328314151003));
#31674=CARTESIAN_POINT('Ctrl Pts',(56.9872160641331,21.1732887136987,23.8339146870059));
#31675=CARTESIAN_POINT('Ctrl Pts',(56.9867401520251,21.1786623458717,23.8342636085846));
#31676=CARTESIAN_POINT('Ctrl Pts',(56.9858592710022,21.1881695169784,23.834879001847));
#31677=CARTESIAN_POINT('Ctrl Pts',(56.985463186857,21.1923037860004,23.8351459607402));
#31678=CARTESIAN_POINT('Ctrl Pts',(56.9845770513471,21.201258452546,23.835722761078));
#31679=CARTESIAN_POINT('Ctrl Pts',(56.9840823497504,21.2060783056769,23.8360323399815));
#31680=CARTESIAN_POINT('Ctrl Pts',(56.9826810465643,21.2192581583034,23.8368765789452));
#31681=CARTESIAN_POINT('Ctrl Pts',(56.9817391239669,21.2276144171214,23.837409305451));
#31682=CARTESIAN_POINT('Ctrl Pts',(56.9767449314093,21.2695368788017,23.840070322094));
#31683=CARTESIAN_POINT('Ctrl Pts',(56.9718923212409,21.3030043614319,23.8421572543967));
#31684=CARTESIAN_POINT('Ctrl Pts',(56.9317712792969,21.537549487808,23.8566204574773));
#31685=CARTESIAN_POINT('Ctrl Pts',(56.8666686542478,21.7323026767777,23.8679069450745));
#31686=CARTESIAN_POINT('Ctrl Pts',(56.756598022282,21.9458823394283,23.8823356726027));
#31687=CARTESIAN_POINT('Ctrl Pts',(56.7391985440534,21.9775061173452,23.8845262736268));
#31688=CARTESIAN_POINT('Ctrl Pts',(56.7079601487604,22.0308054180066,23.8883257641648));
#31689=CARTESIAN_POINT('Ctrl Pts',(56.6945421407528,22.0527176823218,23.889920062393));
#31690=CARTESIAN_POINT('Ctrl Pts',(56.6749767388604,22.0833252542758,23.8921961650324));
#31691=CARTESIAN_POINT('Ctrl Pts',(56.6691768653315,22.0922404806152,23.8928651610198));
#31692=CARTESIAN_POINT('Ctrl Pts',(56.6590770596141,22.1074969826515,23.8940206306559));
#31693=CARTESIAN_POINT('Ctrl Pts',(56.654811338603,22.1138607126937,23.8945058171669));
#31694=CARTESIAN_POINT('Ctrl Pts',(56.6465886625499,22.1259760546985,23.8954357786244));
#31695=CARTESIAN_POINT('Ctrl Pts',(56.6426379574153,22.1317317872237,23.8958803123192));
#31696=CARTESIAN_POINT('Ctrl Pts',(56.6323084312514,22.1466127094163,23.897036791697));
#31697=CARTESIAN_POINT('Ctrl Pts',(56.6258833495972,22.1557053453652,23.8977504938186));
#31698=CARTESIAN_POINT('Ctrl Pts',(56.6072276848336,22.1816429505268,23.8998070503394));
#31699=CARTESIAN_POINT('Ctrl Pts',(56.5948093863116,22.1983504747478,23.9011570940068));
#31700=CARTESIAN_POINT('Ctrl Pts',(56.4813874369299,22.3460617449723,23.9133257239011));
#31701=CARTESIAN_POINT('Ctrl Pts',(56.3647317478751,22.464198368296,23.9248023326573));
#31702=CARTESIAN_POINT('Ctrl Pts',(56.1568487420871,22.6280659729732,23.9432593176487));
#31703=CARTESIAN_POINT('Ctrl Pts',(56.0743316354838,22.6836606898815,23.9501604704387));
#31704=CARTESIAN_POINT('Ctrl Pts',(55.9731537402961,22.7413476753729,23.957885145782));
#31705=CARTESIAN_POINT('Ctrl Pts',(55.9581908557786,22.7496257485308,23.9590095189039));
#31706=CARTESIAN_POINT('Ctrl Pts',(55.9375092430206,22.7607227396348,23.9605371875023));
#31707=CARTESIAN_POINT('Ctrl Pts',(55.9318812107387,22.763707900526,23.9609502531802));
#31708=CARTESIAN_POINT('Ctrl Pts',(55.9223875183622,22.768685313645,23.9616424581039));
#31709=CARTESIAN_POINT('Ctrl Pts',(55.9185295051924,22.7706919613483,23.9619224891895));
#31710=CARTESIAN_POINT('Ctrl Pts',(55.9111827990654,22.7744826914593,23.9624533006095));
#31711=CARTESIAN_POINT('Ctrl Pts',(55.9076953747581,22.7762691301973,23.9627042327872));
#31712=CARTESIAN_POINT('Ctrl Pts',(55.8985127412093,22.7809388435023,23.9633622845547));
#31713=CARTESIAN_POINT('Ctrl Pts',(55.892808859721,22.7838051051317,23.9637683482897));
#31714=CARTESIAN_POINT('Ctrl Pts',(55.8728050835645,22.7937372317536,23.9651833815061));
#31715=CARTESIAN_POINT('Ctrl Pts',(55.8584338480649,22.8006591395237,23.9661838665021));
#31716=CARTESIAN_POINT('Ctrl Pts',(55.7449974119872,22.8536289960962,23.9739672550977));
#31717=CARTESIAN_POINT('Ctrl Pts',(55.642370758999,22.8916468216948,23.9803390609347));
#31718=CARTESIAN_POINT('Ctrl Pts',(55.4281711025293,22.951537451725,23.9932553584661));
#31719=CARTESIAN_POINT('Ctrl Pts',(55.3168195425044,22.9726764531659,23.9997798618336));
#31720=CARTESIAN_POINT('Ctrl Pts',(55.1910139235846,22.9856281348028,24.0073582988248));
#31721=CARTESIAN_POINT('Ctrl Pts',(55.1777361368094,22.9868606397568,24.0081604816638));
#31722=CARTESIAN_POINT('Ctrl Pts',(55.1644483449248,22.9879598346927,24.0089660407953));
#31723=CARTESIAN_POINT('Origin',(55.,21.,6.22095488139522));
#31724=CARTESIAN_POINT('',(55.1644483516314,22.9879598341379,24.9666501649259));
#31725=CARTESIAN_POINT('',(55.1644480328175,22.9879598605109,24.8095189920889));
#31726=CARTESIAN_POINT('',(55.1644483516311,22.987959834138,6.22095488139522));
#31727=CARTESIAN_POINT('',(53.0052508816068,21.0013916490052,24.380394655106));
#31728=CARTESIAN_POINT('Ctrl Pts',(55.1644483516314,22.9879598341379,24.9666501649259));
#31729=CARTESIAN_POINT('Ctrl Pts',(55.1676348043784,22.9876962438517,24.9664433125484));
#31730=CARTESIAN_POINT('Ctrl Pts',(55.1708206486967,22.9874249902382,24.966236876594));
#31731=CARTESIAN_POINT('Ctrl Pts',(55.1781715296382,22.9867813051299,24.9657614465516));
#31732=CARTESIAN_POINT('Ctrl Pts',(55.1823360370128,22.9864034381216,24.965492766225));
#31733=CARTESIAN_POINT('Ctrl Pts',(55.191449129187,22.985547659663,24.9649062812653));
#31734=CARTESIAN_POINT('Ctrl Pts',(55.1963971175177,22.9850643443955,24.9645887816202));
#31735=CARTESIAN_POINT('Ctrl Pts',(55.2105127152994,22.9836322498315,24.9636855562457));
#31736=CARTESIAN_POINT('Ctrl Pts',(55.2196757710823,22.9826384111216,24.9631022880781));
#31737=CARTESIAN_POINT('Ctrl Pts',(55.2813430105057,22.9755171145529,24.9591955069159));
#31738=CARTESIAN_POINT('Ctrl Pts',(55.3335976495527,22.9673676455074,24.9559758082724));
#31739=CARTESIAN_POINT('Ctrl Pts',(55.5561161877095,22.923541406835,24.9424214907378));
#31740=CARTESIAN_POINT('Ctrl Pts',(55.7216365943301,22.8677593283082,24.9326708509641));
#31741=CARTESIAN_POINT('Ctrl Pts',(55.933732027601,22.7638161272085,24.9185683953547));
#31742=CARTESIAN_POINT('Ctrl Pts',(55.9883137784462,22.7338216591524,24.9147865747066));
#31743=CARTESIAN_POINT('Ctrl Pts',(56.0541911542102,22.6934974092091,24.9099800788978));
#31744=CARTESIAN_POINT('Ctrl Pts',(56.0668929202699,22.6855242335651,24.9090417877736));
#31745=CARTESIAN_POINT('Ctrl Pts',(56.0868036314119,22.6727106135166,24.9075520043549));
#31746=CARTESIAN_POINT('Ctrl Pts',(56.0940731091583,22.6679649150338,24.9070040260844));
#31747=CARTESIAN_POINT('Ctrl Pts',(56.1075284161863,22.6590551440066,24.9059820746544));
#31748=CARTESIAN_POINT('Ctrl Pts',(56.1137223445617,22.6549035320121,24.9055085746815));
#31749=CARTESIAN_POINT('Ctrl Pts',(56.1273992548265,22.6456247337835,24.9044561431834));
#31750=CARTESIAN_POINT('Ctrl Pts',(56.1348707988371,22.6404810604455,24.9038765942969));
#31751=CARTESIAN_POINT('Ctrl Pts',(56.1564389863986,22.6254149011974,24.9021899908399));
#31752=CARTESIAN_POINT('Ctrl Pts',(56.1704421296306,22.6153606162459,24.9010779238478));
#31753=CARTESIAN_POINT('Ctrl Pts',(56.3064204573832,22.5150315177791,24.8901077597363));
#31754=CARTESIAN_POINT('Ctrl Pts',(56.4178242737187,22.4113155304903,24.879694506376));
#31755=CARTESIAN_POINT('Ctrl Pts',(56.5967024995637,22.2020206124041,24.8605012772838));
#31756=CARTESIAN_POINT('Ctrl Pts',(56.6681227782446,22.1007652961101,24.8518336237985));
#31757=CARTESIAN_POINT('Ctrl Pts',(56.737515795382,21.9799550505251,24.8426072261192));
#31758=CARTESIAN_POINT('Ctrl Pts',(56.745159503831,21.9662770736392,24.8415779132199));
#31759=CARTESIAN_POINT('Ctrl Pts',(56.7556676119914,21.9469418984802,24.8401457023311));
#31760=CARTESIAN_POINT('Ctrl Pts',(56.7586671881259,21.9413593612169,24.8397348296448));
#31761=CARTESIAN_POINT('Ctrl Pts',(56.763474685549,21.9323089021253,24.8390730961121));
#31762=CARTESIAN_POINT('Ctrl Pts',(56.7652990727238,21.9288498479524,24.8388212118687));
#31763=CARTESIAN_POINT('Ctrl Pts',(56.7691360241086,21.9215228167533,24.8382898729361));
#31764=CARTESIAN_POINT('Ctrl Pts',(56.7711461010435,21.9176535637337,24.8380105809474));
#31765=CARTESIAN_POINT('Ctrl Pts',(56.7760855451718,21.9080688003199,24.8373218552407));
#31766=CARTESIAN_POINT('Ctrl Pts',(56.7790000571311,21.9023456152373,24.8369133455825));
#31767=CARTESIAN_POINT('Ctrl Pts',(56.7897301942436,21.8810209300242,24.8354010100674));
#31768=CARTESIAN_POINT('Ctrl Pts',(56.7973689117648,21.8653306254997,24.8343076328615));
#31769=CARTESIAN_POINT('Ctrl Pts',(56.8489967611899,21.7556502868303,24.8267843833106));
#31770=CARTESIAN_POINT('Ctrl Pts',(56.8858041596834,21.658440945814,24.8207178442405));
#31771=CARTESIAN_POINT('Ctrl Pts',(56.9596389112881,21.405424924289,24.8054029108501));
#31772=CARTESIAN_POINT('Ctrl Pts',(56.9858034823534,21.2472496426684,24.7962151320123));
#31773=CARTESIAN_POINT('Ctrl Pts',(56.9938393398452,21.0645519298029,24.7849445058906));
#31774=CARTESIAN_POINT('Ctrl Pts',(56.9944536332143,21.0414355005556,24.7835077985283));
#31775=CARTESIAN_POINT('Ctrl Pts',(56.9947525182008,21.0088830974136,24.7814675007012));
#31776=CARTESIAN_POINT('Ctrl Pts',(56.9947722207145,20.9994514944123,24.7808743325751));
#31777=CARTESIAN_POINT('Ctrl Pts',(56.9946900188627,20.9830212396635,24.779837339938));
#31778=CARTESIAN_POINT('Ctrl Pts',(56.9946181663626,20.9760225514705,24.7793944594499));
#31779=CARTESIAN_POINT('Ctrl Pts',(56.994390699841,20.9613760236692,24.7784651277143));
#31780=CARTESIAN_POINT('Ctrl Pts',(56.9942279242369,20.9537284247535,24.7779784600591));
#31781=CARTESIAN_POINT('Ctrl Pts',(56.9937356932732,20.9355244919542,24.7768165491122));
#31782=CARTESIAN_POINT('Ctrl Pts',(56.9933663814113,20.9249695520094,24.776140071492));
#31783=CARTESIAN_POINT('Ctrl Pts',(56.9918308067822,20.8892111623983,24.773838569783));
#31784=CARTESIAN_POINT('Ctrl Pts',(56.9902702405538,20.8640279362705,24.7722013215391));
#31785=CARTESIAN_POINT('Ctrl Pts',(56.985385956164,20.8037547607055,24.7682417035525));
#31786=CARTESIAN_POINT('Ctrl Pts',(56.981609132341,20.7687110400051,24.7659059669717));
#31787=CARTESIAN_POINT('Ctrl Pts',(56.9631106953068,20.6313408203308,24.7566169735997));
#31788=CARTESIAN_POINT('Ctrl Pts',(56.9413741142413,20.5301326881196,24.749470357777));
#31789=CARTESIAN_POINT('Ctrl Pts',(56.8763739140957,20.3116964289198,24.7335840601125));
#31790=CARTESIAN_POINT('Ctrl Pts',(56.8297442418331,20.1958965663062,24.7248489019185));
#31791=CARTESIAN_POINT('Ctrl Pts',(56.7654482993205,20.0713106110895,24.7155649980124));
#31792=CARTESIAN_POINT('Ctrl Pts',(56.7581197842988,20.0575104568143,24.7145385891349));
#31793=CARTESIAN_POINT('Ctrl Pts',(56.7475952794788,20.0382420418461,24.7131097115398));
#31794=CARTESIAN_POINT('Ctrl Pts',(56.7445344746864,20.0327011319146,24.7126993161964));
#31795=CARTESIAN_POINT('Ctrl Pts',(56.7395407506309,20.0237619029437,24.7120381444399));
#31796=CARTESIAN_POINT('Ctrl Pts',(56.7376241565473,20.0203545863536,24.711786347912));
#31797=CARTESIAN_POINT('Ctrl Pts',(56.7335479878515,20.0131575803304,24.7112549972677));
#31798=CARTESIAN_POINT('Ctrl Pts',(56.7313859763516,20.009369297354,24.7109756067746));
#31799=CARTESIAN_POINT('Ctrl Pts',(56.7260060383929,20.0000139680418,24.7102862971545));
#31800=CARTESIAN_POINT('Ctrl Pts',(56.7227735534764,19.9944552745603,24.7098773055863));
#31801=CARTESIAN_POINT('Ctrl Pts',(56.7106422770758,19.9738241263041,24.7083611145125));
#31802=CARTESIAN_POINT('Ctrl Pts',(56.7015717976799,19.9588528486678,24.7072644329522));
#31803=CARTESIAN_POINT('Ctrl Pts',(56.6781857806741,19.9213752335779,24.7045230780892));
#31804=CARTESIAN_POINT('Ctrl Pts',(56.6636134050195,19.8990324800545,24.7028924565857));
#31805=CARTESIAN_POINT('Ctrl Pts',(56.5510297122465,19.7337581679719,24.690805346767));
#31806=CARTESIAN_POINT('Ctrl Pts',(56.4352079441073,19.6038442236217,24.6811003423006));
#31807=CARTESIAN_POINT('Ctrl Pts',(56.2796151644102,19.4694267423815,24.668919959998));
#31808=CARTESIAN_POINT('Ctrl Pts',(56.2546815550972,19.4489218184005,24.666992528749));
#31809=CARTESIAN_POINT('Ctrl Pts',(56.1921830057454,19.4000175245283,24.6622037697784));
#31810=CARTESIAN_POINT('Ctrl Pts',(56.1540907306473,19.3723273389756,24.6593208863156));
#31811=CARTESIAN_POINT('Ctrl Pts',(56.1035759886274,19.3382721901914,24.6555229418699));
#31812=CARTESIAN_POINT('Ctrl Pts',(56.0920151840305,19.3306521934883,24.6546554227062));
#31813=CARTESIAN_POINT('Ctrl Pts',(56.0733648532688,19.3186359644834,24.6532581159843));
#31814=CARTESIAN_POINT('Ctrl Pts',(56.0663253165551,19.3141626875614,24.6527312025308));
#31815=CARTESIAN_POINT('Ctrl Pts',(56.0529048076852,19.3057523074876,24.6517275071888));
#31816=CARTESIAN_POINT('Ctrl Pts',(56.04652927229,19.3018067667803,24.651251047686));
#31817=CARTESIAN_POINT('Ctrl Pts',(56.0319670690531,19.2929080032148,24.6501635037004));
#31818=CARTESIAN_POINT('Ctrl Pts',(56.0237667498073,19.2879775837296,24.6495515990114));
#31819=CARTESIAN_POINT('Ctrl Pts',(55.9985667089958,19.2730719233735,24.6476725632003));
#31820=CARTESIAN_POINT('Ctrl Pts',(55.9814547591628,19.2632897295159,24.6463985090654));
#31821=CARTESIAN_POINT('Ctrl Pts',(55.8590042680371,19.1956775410622,24.6372920576926));
#31822=CARTESIAN_POINT('Ctrl Pts',(55.7487924046716,19.1472267404228,24.6291275942133));
#31823=CARTESIAN_POINT('Ctrl Pts',(55.5080612006935,19.0664008089282,24.6115109037598));
#31824=CARTESIAN_POINT('Ctrl Pts',(55.3772469249719,19.0366816068826,24.602060054858));
#31825=CARTESIAN_POINT('Ctrl Pts',(55.2152280364035,19.0166768406861,24.5910750875196));
#31826=CARTESIAN_POINT('Ctrl Pts',(55.1859387422817,19.0137168213038,24.5891186642995));
#31827=CARTESIAN_POINT('Ctrl Pts',(55.1485108481939,19.0107695420505,24.5866648266484));
#31828=CARTESIAN_POINT('Ctrl Pts',(55.140424838047,19.0101823809317,24.5861374395999));
#31829=CARTESIAN_POINT('Ctrl Pts',(55.1276158022245,19.0093307302018,24.5853065894854));
#31830=CARTESIAN_POINT('Ctrl Pts',(55.1228951358004,19.0090337216756,24.5850013711377));
#31831=CARTESIAN_POINT('Ctrl Pts',(55.1139636607921,19.0085036703964,24.5844258187784));
#31832=CARTESIAN_POINT('Ctrl Pts',(55.1097532181249,19.0082671920576,24.5841553074799));
#31833=CARTESIAN_POINT('Ctrl Pts',(55.0999349189261,19.0077469785543,24.5835263565206));
#31834=CARTESIAN_POINT('Ctrl Pts',(55.0943265830782,19.0074735667869,24.5831684950534));
#31835=CARTESIAN_POINT('Ctrl Pts',(55.0762663218059,19.0066695358208,24.5820203927195));
#31836=CARTESIAN_POINT('Ctrl Pts',(55.0638102625817,19.0062319191309,24.5812351347766));
#31837=CARTESIAN_POINT('Ctrl Pts',(54.9527820074298,19.0033727879327,24.5742877963379));
#31838=CARTESIAN_POINT('Ctrl Pts',(54.8541468867826,19.0081461230351,24.568478537762));
#31839=CARTESIAN_POINT('Ctrl Pts',(54.5835310230122,19.0414627817128,24.5525939473954));
#31840=CARTESIAN_POINT('Ctrl Pts',(54.4143493830394,19.0852357066642,24.542655088259));
#31841=CARTESIAN_POINT('Ctrl Pts',(54.2324333538452,19.1587067533168,24.5305455533129));
#31842=CARTESIAN_POINT('Ctrl Pts',(54.2120108156771,19.1673537273201,24.5291660051294));
#31843=CARTESIAN_POINT('Ctrl Pts',(54.182665118346,19.180360001092,24.5271525069361));
#31844=CARTESIAN_POINT('Ctrl Pts',(54.1736232014417,19.1844484541934,24.5265277712401));
#31845=CARTESIAN_POINT('Ctrl Pts',(54.157737640267,19.1917746288857,24.5254223334259));
#31846=CARTESIAN_POINT('Ctrl Pts',(54.1508811679711,19.194984187914,24.524942606874));
#31847=CARTESIAN_POINT('Ctrl Pts',(54.1436601887791,19.1984146231634,24.5244345822891));
#31848=CARTESIAN_POINT('Ctrl Pts',(54.1432772273929,19.1985967044526,24.5244076311092));
#31849=CARTESIAN_POINT('Ctrl Pts',(54.1426809112851,19.198880459691,24.5243656519631));
#31850=CARTESIAN_POINT('Ctrl Pts',(54.1424675163437,19.1989820495527,24.5243506269103));
#31851=CARTESIAN_POINT('Ctrl Pts',(54.1421208330106,19.199147168937,24.5243262128666));
#31852=CARTESIAN_POINT('Ctrl Pts',(54.141987534679,19.199210674828,24.524316824755));
#31853=CARTESIAN_POINT('Ctrl Pts',(54.1417018581962,19.1993468155217,24.5242967025858));
#31854=CARTESIAN_POINT('Ctrl Pts',(54.1415494786931,19.199419456547,24.5242859681222));
#31855=CARTESIAN_POINT('Ctrl Pts',(54.1412586991956,19.1995581197091,24.5242654814664));
#31856=CARTESIAN_POINT('Ctrl Pts',(54.1411202949939,19.1996241397018,24.5242557292091));
#31857=CARTESIAN_POINT('Ctrl Pts',(54.1408561603809,19.1997501715726,24.5242371156331));
#31858=CARTESIAN_POINT('Ctrl Pts',(54.1407304331086,19.1998101785305,24.5242282547265));
#31859=CARTESIAN_POINT('Ctrl Pts',(54.1404904830244,19.1999247324763,24.5242113419952));
#31860=CARTESIAN_POINT('Ctrl Pts',(54.140376259191,19.1999792771305,24.5242032902558));
#31861=CARTESIAN_POINT('Ctrl Pts',(54.1401582501536,19.2000834072238,24.5241879211847));
#31862=CARTESIAN_POINT('Ctrl Pts',(54.1400544640929,19.2001329907453,24.5241806039222));
#31863=CARTESIAN_POINT('Ctrl Pts',(54.139856364504,19.2002276533565,24.5241666360689));
#31864=CARTESIAN_POINT('Ctrl Pts',(54.139762050177,19.2002727309085,24.5241599855287));
#31865=CARTESIAN_POINT('Ctrl Pts',(54.1395820181777,19.2003587946248,24.5241472896687));
#31866=CARTESIAN_POINT('Ctrl Pts',(54.1394962999072,19.2003997794916,24.524141244395));
#31867=CARTESIAN_POINT('Ctrl Pts',(54.1393326664959,19.2004780326435,24.5241297033616));
#31868=CARTESIAN_POINT('Ctrl Pts',(54.1392547507871,19.2005152998936,24.5241242076346));
#31869=CARTESIAN_POINT('Ctrl Pts',(54.1391060031611,19.2005864580724,24.5241137151684));
#31870=CARTESIAN_POINT('Ctrl Pts',(54.1390351708357,19.2006203481178,24.5241087184605));
#31871=CARTESIAN_POINT('Ctrl Pts',(54.1388999382049,19.2006850605928,24.5240991782298));
#31872=CARTESIAN_POINT('Ctrl Pts',(54.1388355375489,19.2007158822997,24.5240946347319));
#31873=CARTESIAN_POINT('Ctrl Pts',(54.1387125771048,19.2007747384283,24.5240859593593));
#31874=CARTESIAN_POINT('Ctrl Pts',(54.1386540171968,19.200802772172,24.5240818275173));
#31875=CARTESIAN_POINT('Ctrl Pts',(54.1385422028668,19.2008563065322,24.5240739378007));
#31876=CARTESIAN_POINT('Ctrl Pts',(54.1384889481523,19.2008818066812,24.5240701799395));
#31877=CARTESIAN_POINT('Ctrl Pts',(54.138356359029,19.2009453020512,24.5240608235276));
#31878=CARTESIAN_POINT('Ctrl Pts',(54.1382770258726,19.2009833002168,24.5240552248676));
#31879=CARTESIAN_POINT('Ctrl Pts',(54.1381200143869,19.2010585167052,24.5240441436185));
#31880=CARTESIAN_POINT('Ctrl Pts',(54.138042336046,19.2010957347679,24.5240386610433));
#31881=CARTESIAN_POINT('Ctrl Pts',(54.1378885930604,19.2011694099667,24.5240278091049));
#31882=CARTESIAN_POINT('Ctrl Pts',(54.1378125281441,19.2012058669793,24.5240224397366));
#31883=CARTESIAN_POINT('Ctrl Pts',(54.137661971134,19.2012780389131,24.5240118113688));
#31884=CARTESIAN_POINT('Ctrl Pts',(54.1375874790808,19.2013137535728,24.5240065523855));
#31885=CARTESIAN_POINT('Ctrl Pts',(54.1374400285605,19.2013844588914,24.5239961420579));
#31886=CARTESIAN_POINT('Ctrl Pts',(54.1373670700523,19.2014194493387,24.5239909907236));
#31887=CARTESIAN_POINT('Ctrl Pts',(54.1372226485801,19.2014887237887,24.523980793046));
#31888=CARTESIAN_POINT('Ctrl Pts',(54.1371511854602,19.2015230076452,24.5239757467042));
#31889=CARTESIAN_POINT('Ctrl Pts',(54.129139970632,19.2053669108682,24.5234100049145));
#31890=CARTESIAN_POINT('Ctrl Pts',(54.1212256391666,19.2092290112937,24.5228474909823));
#31891=CARTESIAN_POINT('Ctrl Pts',(54.0987980336851,19.2203578964112,24.5212429899138));
#31892=CARTESIAN_POINT('Ctrl Pts',(54.0843477890384,19.227749452343,24.5201966661263));
#31893=CARTESIAN_POINT('Ctrl Pts',(54.052012585362,19.2447905080663,24.5178263664843));
#31894=CARTESIAN_POINT('Ctrl Pts',(54.0341818652593,19.2545385196946,24.5164990160639));
#31895=CARTESIAN_POINT('Ctrl Pts',(53.977745987031,19.2865214054872,24.512231668133));
#31896=CARTESIAN_POINT('Ctrl Pts',(53.9397375655378,19.309776571731,24.5092568699223));
#31897=CARTESIAN_POINT('Ctrl Pts',(53.7622871645128,19.4266898488615,24.4948827916702));
#31898=CARTESIAN_POINT('Ctrl Pts',(53.6342863563278,19.5364246014618,24.4829603438867));
#31899=CARTESIAN_POINT('Ctrl Pts',(53.4858322569959,19.7003249974754,24.4678051562642));
#31900=CARTESIAN_POINT('Ctrl Pts',(53.4516989011861,19.7411815575075,24.464212847805));
#31901=CARTESIAN_POINT('Ctrl Pts',(53.4138815496365,19.7903170097563,24.460147068855));
#31902=CARTESIAN_POINT('Ctrl Pts',(53.4085714737221,19.7973113753004,24.4595740827152));
#31903=CARTESIAN_POINT('Ctrl Pts',(53.4000668303537,19.8086685398365,24.4586532766773));
#31904=CARTESIAN_POINT('Ctrl Pts',(53.3968435780148,19.8130095688568,24.4583035563238));
#31905=CARTESIAN_POINT('Ctrl Pts',(53.3911519094315,19.820740500493,24.4576847805924));
#31906=CARTESIAN_POINT('Ctrl Pts',(53.3886764929846,19.824125133102,24.4574152467923));
#31907=CARTESIAN_POINT('Ctrl Pts',(53.3833583866539,19.8314449002278,24.4568353008663));
#31908=CARTESIAN_POINT('Ctrl Pts',(53.3805193859416,19.8353826082748,24.4565251408301));
#31909=CARTESIAN_POINT('Ctrl Pts',(53.3726479290097,19.8463847996819,24.4556634875886));
#31910=CARTESIAN_POINT('Ctrl Pts',(53.3676470595739,19.8534719027567,24.4551141087919));
#31911=CARTESIAN_POINT('Ctrl Pts',(53.338710218839,19.8950535738245,24.4519222368892));
#31912=CARTESIAN_POINT('Ctrl Pts',(53.315819971952,19.9302670635964,24.4493447741032));
#31913=CARTESIAN_POINT('Ctrl Pts',(53.2044242995398,20.114084992578,24.436378115828));
#31914=CARTESIAN_POINT('Ctrl Pts',(53.1344013522111,20.2730269760886,24.426690984179));
#31915=CARTESIAN_POINT('Ctrl Pts',(53.0719163302744,20.4862464912673,24.413516415007));
#31916=CARTESIAN_POINT('Ctrl Pts',(53.0598299291023,20.5339647139773,24.4105622547277));
#31917=CARTESIAN_POINT('Ctrl Pts',(53.0428007465075,20.6134415502945,24.4055961776215));
#31918=CARTESIAN_POINT('Ctrl Pts',(53.036838485273,20.6449605074253,24.4036151909408));
#31919=CARTESIAN_POINT('Ctrl Pts',(53.0296972914166,20.688426197937,24.4008615200558));
#31920=CARTESIAN_POINT('Ctrl Pts',(53.0278621601364,20.7002612334259,24.4001095449652));
#31921=CARTESIAN_POINT('Ctrl Pts',(53.0251033542933,20.7191766150367,24.3989039156715));
#31922=CARTESIAN_POINT('Ctrl Pts',(53.024110909842,20.7262467607354,24.3984524378235));
#31923=CARTESIAN_POINT('Ctrl Pts',(53.022195379038,20.740446300345,24.3975439456216));
#31924=CARTESIAN_POINT('Ctrl Pts',(53.0212728355989,20.7475756581781,24.3970869214274));
#31925=CARTESIAN_POINT('Ctrl Pts',(53.0194871914024,20.7619866730898,24.3961612614836));
#31926=CARTESIAN_POINT('Ctrl Pts',(53.0186256639307,20.7692684096212,24.3956925836446));
#31927=CARTESIAN_POINT('Ctrl Pts',(53.0167383165913,20.7860111692049,24.3946127106645));
#31928=CARTESIAN_POINT('Ctrl Pts',(53.0157400204477,20.7954750555062,24.3940006604504));
#31929=CARTESIAN_POINT('Ctrl Pts',(53.0124488889824,20.8289709548609,24.3918283909596));
#31930=CARTESIAN_POINT('Ctrl Pts',(53.0105247093562,20.8530362748832,24.3902567394274));
#31931=CARTESIAN_POINT('Ctrl Pts',(53.0064843855035,20.9185047798876,24.3859498910358));
#31932=CARTESIAN_POINT('Ctrl Pts',(53.0052215183626,20.9599462506629,24.3831895681168));
#31933=CARTESIAN_POINT('Ctrl Pts',(53.0052504872089,21.001394173412,24.3803951722837));
#31934=CARTESIAN_POINT('Ctrl Pts',(53.0052504854785,21.0013916954035,24.3803953393496));
#31935=CARTESIAN_POINT('Ctrl Pts',(53.0053744414124,21.1790606296367,24.3684170045932));
#31936=CARTESIAN_POINT('Ctrl Pts',(53.0292322017107,21.3558945387234,24.3557807860037));
#31937=CARTESIAN_POINT('Ctrl Pts',(53.0895213675535,21.575885919755,24.3401825258644));
#31938=CARTESIAN_POINT('Ctrl Pts',(53.104699482229,21.6240273304911,24.3367843651265));
#31939=CARTESIAN_POINT('Ctrl Pts',(53.1247556485663,21.6801243933373,24.3328825920221));
#31940=CARTESIAN_POINT('Ctrl Pts',(53.1278816459156,21.6886823969914,24.3322889815137));
#31941=CARTESIAN_POINT('Ctrl Pts',(53.1327959925183,21.7018555748569,24.3313781003643));
#31942=CARTESIAN_POINT('Ctrl Pts',(53.1345430171888,21.7064858810228,24.3310584769951));
#31943=CARTESIAN_POINT('Ctrl Pts',(53.1377985616489,21.7150180871364,24.3304705848655));
#31944=CARTESIAN_POINT('Ctrl Pts',(53.1393021148868,21.7189217223319,24.3302020370318));
#31945=CARTESIAN_POINT('Ctrl Pts',(53.1427302050711,21.7277391835431,24.3295963830438));
#31946=CARTESIAN_POINT('Ctrl Pts',(53.1446619645514,21.7326501117046,24.329259713464));
#31947=CARTESIAN_POINT('Ctrl Pts',(53.1504406494992,21.7471712820239,24.3282659829877));
#31948=CARTESIAN_POINT('Ctrl Pts',(53.1543429876387,21.7567594857693,24.3276121357559));
#31949=CARTESIAN_POINT('Ctrl Pts',(53.1891104480686,21.8403156779393,24.3219307536087));
#31950=CARTESIAN_POINT('Ctrl Pts',(53.2243369692337,21.9124009079606,24.317141991972));
#31951=CARTESIAN_POINT('Ctrl Pts',(53.3271700845343,22.094178252436,24.3048786505637));
#31952=CARTESIAN_POINT('Ctrl Pts',(53.4012172397528,22.1997834794396,24.2975450830677));
#31953=CARTESIAN_POINT('Ctrl Pts',(53.5182633119268,22.3364547943455,24.2868913638562));
#31954=CARTESIAN_POINT('Ctrl Pts',(53.5530917736207,22.3740855300647,24.2838183989105));
#31955=CARTESIAN_POINT('Ctrl Pts',(53.6051688545557,22.4261751522309,24.2793209128481));
#31956=CARTESIAN_POINT('Ctrl Pts',(53.6212740665945,22.441750404861,24.2779425824143));
#31957=CARTESIAN_POINT('Ctrl Pts',(53.6504332651493,22.4690146540765,24.2754662147029));
#31958=CARTESIAN_POINT('Ctrl Pts',(53.6633855149432,22.4808092765275,24.2743727118282));
#31959=CARTESIAN_POINT('Ctrl Pts',(53.6832977336752,22.4984677074687,24.2727003881602));
#31960=CARTESIAN_POINT('Ctrl Pts',(53.6901454809844,22.5044571988141,24.2721268239649));
#31961=CARTESIAN_POINT('Ctrl Pts',(53.6971155062008,22.5104699831316,24.2715444946886));
#31962=CARTESIAN_POINT('Ctrl Pts',(53.6971971478378,22.5105404008242,24.271537673925));
#31963=CARTESIAN_POINT('Ctrl Pts',(53.6973638001637,22.510684118529,24.2715237513458));
#31964=CARTESIAN_POINT('Ctrl Pts',(53.6974488114816,22.5107574181148,24.2715166494947));
#31965=CARTESIAN_POINT('Ctrl Pts',(53.6976224265456,22.5109070892501,24.2715021461315));
#31966=CARTESIAN_POINT('Ctrl Pts',(53.6977110307563,22.5109834601244,24.2714947445996));
#31967=CARTESIAN_POINT('Ctrl Pts',(53.6978920745766,22.5111394799748,24.271479621636));
#31968=CARTESIAN_POINT('Ctrl Pts',(53.6979845148122,22.5112191282935,24.2714719001731));
#31969=CARTESIAN_POINT('Ctrl Pts',(53.698173496219,22.5113819281663,24.2714561152316));
#31970=CARTESIAN_POINT('Ctrl Pts',(53.6982700380402,22.5114650789451,24.2714480517222));
#31971=CARTESIAN_POINT('Ctrl Pts',(53.6984675130052,22.5116351297639,24.2714315585051));
#31972=CARTESIAN_POINT('Ctrl Pts',(53.6985684468999,22.5117220289573,24.271423128761));
#31973=CARTESIAN_POINT('Ctrl Pts',(53.6987750242842,22.5118998460546,24.2714058765732));
#31974=CARTESIAN_POINT('Ctrl Pts',(53.6988806686358,22.5119907630264,24.2713970540869));
#31975=CARTESIAN_POINT('Ctrl Pts',(53.6990970164859,22.5121769113792,24.271378987313));
#31976=CARTESIAN_POINT('Ctrl Pts',(53.699207720944,22.5122721417036,24.2713697429782));
#31977=CARTESIAN_POINT('Ctrl Pts',(53.6994345737779,22.5124672419858,24.2713508004779));
#31978=CARTESIAN_POINT('Ctrl Pts',(53.6995507231692,22.5125671106945,24.2713411022649));
#31979=CARTESIAN_POINT('Ctrl Pts',(53.6997888900893,22.5127718459999,24.2713212167001));
#31980=CARTESIAN_POINT('Ctrl Pts',(53.6999109087731,22.512876711189,24.2713110292941));
#31981=CARTESIAN_POINT('Ctrl Pts',(53.7001612832108,22.5130918351072,24.2712901263204));
#31982=CARTESIAN_POINT('Ctrl Pts',(53.7002896402545,22.5132020922211,24.2712794106928));
#31983=CARTESIAN_POINT('Ctrl Pts',(53.7004997078298,22.5133824912249,24.2712618744412));
#31984=CARTESIAN_POINT('Ctrl Pts',(53.7005814100934,22.5134526429002,24.2712550542114));
#31985=CARTESIAN_POINT('Ctrl Pts',(53.70076751334,22.5136124097792,24.2712395193977));
#31986=CARTESIAN_POINT('Ctrl Pts',(53.700871917902,22.5137020207871,24.2712308046424));
#31987=CARTESIAN_POINT('Ctrl Pts',(53.7011103999963,22.5139066684285,24.2712108990488));
#31988=CARTESIAN_POINT('Ctrl Pts',(53.701244483496,22.5140216980151,24.2711997079253));
#31989=CARTESIAN_POINT('Ctrl Pts',(53.7070512557002,22.5190019608301,24.2707150758491));
#31990=CARTESIAN_POINT('Ctrl Pts',(53.712751161316,22.5238352395217,24.2702403301013));
#31991=CARTESIAN_POINT('Ctrl Pts',(53.7256242359562,22.5346272949989,24.2691702151703));
#31992=CARTESIAN_POINT('Ctrl Pts',(53.7328122628395,22.5405679979953,24.2685741248451));
#31993=CARTESIAN_POINT('Ctrl Pts',(53.7512670760165,22.5556038394103,24.2670471959981));
#31994=CARTESIAN_POINT('Ctrl Pts',(53.7625915668127,22.5646269752729,24.2661135016873));
#31995=CARTESIAN_POINT('Ctrl Pts',(53.8344515100184,22.6206154765686,24.2602080822056));
#31996=CARTESIAN_POINT('Ctrl Pts',(53.8975452624156,22.664178116476,24.2551047954707));
#31997=CARTESIAN_POINT('Ctrl Pts',(54.0992766138642,22.7869475617343,24.2390355902647));
#31998=CARTESIAN_POINT('Ctrl Pts',(54.2450143737752,22.8532332362195,24.2277139411983));
#31999=CARTESIAN_POINT('Ctrl Pts',(54.4299260009135,22.911865703729,24.2144412050943));
#32000=CARTESIAN_POINT('Ctrl Pts',(54.4630375121495,22.9214282185605,24.2121074398105));
#32001=CARTESIAN_POINT('Ctrl Pts',(54.5168080274741,22.9354582685018,24.2084031773435));
#32002=CARTESIAN_POINT('Ctrl Pts',(54.5373184057796,22.9404636096017,24.2070100140868));
#32003=CARTESIAN_POINT('Ctrl Pts',(54.564640113532,22.9466733243871,24.2051837964063));
#32004=CARTESIAN_POINT('Ctrl Pts',(54.5713829081274,22.9481690518494,24.2047354786657));
#32005=CARTESIAN_POINT('Ctrl Pts',(54.5824963742723,22.9505738159128,24.2040006271888));
#32006=CARTESIAN_POINT('Ctrl Pts',(54.5868625033272,22.9515032407408,24.2037129576162));
#32007=CARTESIAN_POINT('Ctrl Pts',(54.5954274801637,22.9532964481474,24.2031507079015));
#32008=CARTESIAN_POINT('Ctrl Pts',(54.599626040789,22.9541613626998,24.2028760675952));
#32009=CARTESIAN_POINT('Ctrl Pts',(54.6099746599695,22.9562584536195,24.2022014625306));
#32010=CARTESIAN_POINT('Ctrl Pts',(54.6161278707485,22.9574751835347,24.2018023697279));
#32011=CARTESIAN_POINT('Ctrl Pts',(54.6372889189158,22.9615559300947,24.2004365018136));
#32012=CARTESIAN_POINT('Ctrl Pts',(54.6523243013168,22.964276619309,24.1994774481572));
#32013=CARTESIAN_POINT('Ctrl Pts',(54.7968129741785,22.9887111235441,24.1903574965546));
#32014=CARTESIAN_POINT('Ctrl Pts',(54.9280997295243,22.9977730564976,24.1827979213669));
#32015=CARTESIAN_POINT('Ctrl Pts',(55.0944337379504,22.9928227445012,24.1731426277646));
#32016=CARTESIAN_POINT('Ctrl Pts',(55.1294820511752,22.9908523238325,24.1711048544396));
#32017=CARTESIAN_POINT('Ctrl Pts',(55.1644484328881,22.9879598274162,24.1690565717028));
#32018=CARTESIAN_POINT('Ctrl Pts',(55.1644483449248,22.9879598346927,24.0089660407953));
#32019=CARTESIAN_POINT('Ctrl Pts',(55.1201504546627,22.9916242521574,24.0116515562158));
#32020=CARTESIAN_POINT('Ctrl Pts',(55.075741393938,22.9938071064991,24.014374972811));
#32021=CARTESIAN_POINT('Ctrl Pts',(55.0170795277407,22.9947275452425,24.0180305829984));
#32022=CARTESIAN_POINT('Ctrl Pts',(55.0028624442198,22.9947986063458,24.0189210070507));
#32023=CARTESIAN_POINT('Ctrl Pts',(54.9802255455821,22.994669757504,24.0203463745895));
#32024=CARTESIAN_POINT('Ctrl Pts',(54.9718054848462,22.9945685088112,24.0208782316466));
#32025=CARTESIAN_POINT('Ctrl Pts',(54.9559071143158,22.9942766455062,24.0218857287375));
#32026=CARTESIAN_POINT('Ctrl Pts',(54.9484287242451,22.9940972700442,24.0223610088173));
#32027=CARTESIAN_POINT('Ctrl Pts',(54.931529604813,22.9935968046183,24.0234381795587));
#32028=CARTESIAN_POINT('Ctrl Pts',(54.9221098397583,22.9932509958099,24.0240408331336));
#32029=CARTESIAN_POINT('Ctrl Pts',(54.8978916526339,22.9921899880803,24.0255961357955));
#32030=CARTESIAN_POINT('Ctrl Pts',(54.8830983204186,22.9913766697587,24.0265518256977));
#32031=CARTESIAN_POINT('Ctrl Pts',(54.7839848515052,22.9848193485508,24.0329939884227));
#32032=CARTESIAN_POINT('Ctrl Pts',(54.7001052303843,22.9738870615148,24.0386417614492));
#32033=CARTESIAN_POINT('Ctrl Pts',(54.468031614072,22.9285054502434,24.0547998883235));
#32034=CARTESIAN_POINT('Ctrl Pts',(54.3227183528229,22.8823942503079,24.0655744578728));
#32035=CARTESIAN_POINT('Ctrl Pts',(54.1531881242769,22.8064001350005,24.0782787290817));
#32036=CARTESIAN_POINT('Ctrl Pts',(54.1226759940034,22.7917797451871,24.0805685456348));
#32037=CARTESIAN_POINT('Ctrl Pts',(54.0739988975599,22.7669135280702,24.0842109271548));
#32038=CARTESIAN_POINT('Ctrl Pts',(54.0555976420066,22.7571470418782,24.0855852944508));
#32039=CARTESIAN_POINT('Ctrl Pts',(54.0313340174825,22.7437777916207,24.0873907948999));
#32040=CARTESIAN_POINT('Ctrl Pts',(54.02533320286,22.7404308116502,24.0878367711843));
#32041=CARTESIAN_POINT('Ctrl Pts',(54.0154700277099,22.7348625724343,24.0885687269228));
#32042=CARTESIAN_POINT('Ctrl Pts',(54.0115976609762,22.7326592938996,24.0888558256824));
#32043=CARTESIAN_POINT('Ctrl Pts',(54.0040105454273,22.7283087045995,24.0894177505274));
#32044=CARTESIAN_POINT('Ctrl Pts',(54.0002952983333,22.7261623568016,24.0896926324532));
#32045=CARTESIAN_POINT('Ctrl Pts',(53.9911447006593,22.7208364823964,24.0903690409796));
#32046=CARTESIAN_POINT('Ctrl Pts',(53.9857173669071,22.7176431401592,24.0907696842096));
#32047=CARTESIAN_POINT('Ctrl Pts',(53.9670408126773,22.7065348116988,24.0921468241187));
#32048=CARTESIAN_POINT('Ctrl Pts',(53.953867992275,22.6984915669489,24.0931154259836));
#32049=CARTESIAN_POINT('Ctrl Pts',(53.8318463418225,22.6220276629111,24.1020751439746));
#32050=CARTESIAN_POINT('Ctrl Pts',(53.7297423064452,22.5433766629365,24.1094906789742));
#32051=CARTESIAN_POINT('Ctrl Pts',(53.5625076910332,22.3866377073119,24.1227884230327));
#32052=CARTESIAN_POINT('Ctrl Pts',(53.4944186815043,22.312391369064,24.1286328948172));
#32053=CARTESIAN_POINT('Ctrl Pts',(53.399743874035,22.192043435566,24.1378421023001));
#32054=CARTESIAN_POINT('Ctrl Pts',(53.3689097527057,22.1494916681885,24.1410519184223));
#32055=CARTESIAN_POINT('Ctrl Pts',(53.332143639312,22.094291147485,24.1451868901259));
#32056=CARTESIAN_POINT('Ctrl Pts',(53.3246141777311,22.0827281684426,24.1460514580284));
#32057=CARTESIAN_POINT('Ctrl Pts',(53.3127334098542,22.0640622069451,24.1474450373972));
#32058=CARTESIAN_POINT('Ctrl Pts',(53.3083054923293,22.05700833288,24.1479712009774));
#32059=CARTESIAN_POINT('Ctrl Pts',(53.2999757072047,22.0435521920616,24.1489741358482));
#32060=CARTESIAN_POINT('Ctrl Pts',(53.2960654985755,22.0371552371698,24.1494505894083));
#32061=CARTESIAN_POINT('Ctrl Pts',(53.2872398690975,22.0225322120775,24.1505390518519));
#32062=CARTESIAN_POINT('Ctrl Pts',(53.2823475057463,22.0142925093043,24.1511518874507));
#32063=CARTESIAN_POINT('Ctrl Pts',(53.2697813902583,21.9927770409265,24.1527510288973));
#32064=CARTESIAN_POINT('Ctrl Pts',(53.2622011283673,21.9794476762148,24.1537406698523));
#32065=CARTESIAN_POINT('Ctrl Pts',(53.2055781965782,21.8771532657491,24.1613289756606));
#32066=CARTESIAN_POINT('Ctrl Pts',(53.1632499850094,21.7846598743356,24.1681643887401));
#32067=CARTESIAN_POINT('Ctrl Pts',(53.1196806768405,21.666354097067,24.1768459592815));
#32068=CARTESIAN_POINT('Ctrl Pts',(53.1116336426709,21.6431959226837,24.1785419117466));
#32069=CARTESIAN_POINT('Ctrl Pts',(53.0807085948919,21.5486100075613,24.1854484365023));
#32070=CARTESIAN_POINT('Ctrl Pts',(53.0614407213508,21.4760674420471,24.1907015752486));
#32071=CARTESIAN_POINT('Ctrl Pts',(53.0310087615182,21.3283949953725,24.2011662044374));
#32072=CARTESIAN_POINT('Ctrl Pts',(53.0199540427219,21.2533577871977,24.2063680862179));
#32073=CARTESIAN_POINT('Ctrl Pts',(53.0118574211865,21.1629169455024,24.212373208555));
#32074=CARTESIAN_POINT('Ctrl Pts',(53.0106877976602,21.1479521507097,24.2133581532773));
#32075=CARTESIAN_POINT('Ctrl Pts',(53.009283810642,21.126937882553,24.214727757282));
#32076=CARTESIAN_POINT('Ctrl Pts',(53.0089079248541,21.1208988139083,24.2151197907483));
#32077=CARTESIAN_POINT('Ctrl Pts',(53.0083127110249,21.1105788312556,24.2157869493336));
#32078=CARTESIAN_POINT('Ctrl Pts',(53.008079693714,21.1062987758672,24.2160628272749));
#32079=CARTESIAN_POINT('Ctrl Pts',(53.0076282017065,21.0974823332571,24.2166293846024));
#32080=CARTESIAN_POINT('Ctrl Pts',(53.0074114209899,21.0929459183311,24.2169199693291));
#32081=CARTESIAN_POINT('Ctrl Pts',(53.0068882495684,21.0811532989728,24.2176730277907));
#32082=CARTESIAN_POINT('Ctrl Pts',(53.0066059870503,21.0738960125848,24.2181341749747));
#32083=CARTESIAN_POINT('Ctrl Pts',(53.0056294460151,21.0446800850045,24.21998199044));
#32084=CARTESIAN_POINT('Ctrl Pts',(53.0052582849255,21.0227112526261,24.2213518101054));
#32085=CARTESIAN_POINT('Ctrl Pts',(53.0051869685036,20.8303971244324,24.2332061857491));
#32086=CARTESIAN_POINT('Ctrl Pts',(53.0269430638565,20.6607262184238,24.2427735846008));
#32087=CARTESIAN_POINT('Ctrl Pts',(53.0946009687021,20.4017082946576,24.2584692867371));
#32088=CARTESIAN_POINT('Ctrl Pts',(53.1260505416986,20.3094869824277,24.2642804424908));
#32089=CARTESIAN_POINT('Ctrl Pts',(53.1700519439094,20.2059286616253,24.2712670480698));
#32090=CARTESIAN_POINT('Ctrl Pts',(53.1761634107087,20.1919905607599,24.2722172114739));
#32091=CARTESIAN_POINT('Ctrl Pts',(53.1863676500479,20.1694240381615,24.2737722998942));
#32092=CARTESIAN_POINT('Ctrl Pts',(53.1903640222102,20.1607525085169,24.2743739309471));
#32093=CARTESIAN_POINT('Ctrl Pts',(53.1976076149501,20.1453273113667,24.2754515629388));
#32094=CARTESIAN_POINT('Ctrl Pts',(53.2008309476769,20.1385625774085,24.2759267324222));
#32095=CARTESIAN_POINT('Ctrl Pts',(53.2077256015357,20.1243004331026,24.2769340675041));
#32096=CARTESIAN_POINT('Ctrl Pts',(53.211406016372,20.1168076035813,24.2774665422779));
#32097=CARTESIAN_POINT('Ctrl Pts',(53.2213337221065,20.0969126995134,24.2788891833555));
#32098=CARTESIAN_POINT('Ctrl Pts',(53.2276635825834,20.0845525641883,24.2797822226333));
#32099=CARTESIAN_POINT('Ctrl Pts',(53.2590477756434,20.0248153019157,24.2841440429888));
#32100=CARTESIAN_POINT('Ctrl Pts',(53.2858734333657,19.9783987803166,24.2876749726932));
#32101=CARTESIAN_POINT('Ctrl Pts',(53.3702046389756,19.845171328773,24.2982431385995));
#32102=CARTESIAN_POINT('Ctrl Pts',(53.432668764797,19.7617227869511,24.3054418134468));
#32103=CARTESIAN_POINT('Ctrl Pts',(53.5828752659126,19.5907289870585,24.3213082969186));
#32104=CARTESIAN_POINT('Ctrl Pts',(53.6728526841473,19.5056865407901,24.3299684805561));
#32105=CARTESIAN_POINT('Ctrl Pts',(53.7824634150558,19.4198488194517,24.3391882590102));
#32106=CARTESIAN_POINT('Ctrl Pts',(53.794913901926,19.4103331726723,24.3402176745465));
#32107=CARTESIAN_POINT('Ctrl Pts',(53.8125550764452,19.3971767826822,24.3416499322326));
#32108=CARTESIAN_POINT('Ctrl Pts',(53.817652576768,19.3934128452296,24.3420607514116));
#32109=CARTESIAN_POINT('Ctrl Pts',(53.8259242133656,19.3873658520242,24.3427223694111));
#32110=CARTESIAN_POINT('Ctrl Pts',(53.8290872275258,19.3850677636875,24.342974191508));
#32111=CARTESIAN_POINT('Ctrl Pts',(53.8357906859715,19.3802274132129,24.3435053672755));
#32112=CARTESIAN_POINT('Ctrl Pts',(53.8393327448244,19.3776874273995,24.3437845584957));
#32113=CARTESIAN_POINT('Ctrl Pts',(53.8481118863605,19.371435435325,24.3444729754754));
#32114=CARTESIAN_POINT('Ctrl Pts',(53.8533586698706,19.3677370216715,24.3448812783426));
#32115=CARTESIAN_POINT('Ctrl Pts',(53.8729217829715,19.3540880276946,24.3463924737536));
#32116=CARTESIAN_POINT('Ctrl Pts',(53.8873510154334,19.3442996001751,24.3474849361285));
#32117=CARTESIAN_POINT('Ctrl Pts',(53.9884010859737,19.2776675062381,24.3549970223303));
#32118=CARTESIAN_POINT('Ctrl Pts',(54.079218351292,19.2274515108908,24.3610544309121));
#32119=CARTESIAN_POINT('Ctrl Pts',(54.3191469521964,19.1182287589057,24.3763727757744));
#32120=CARTESIAN_POINT('Ctrl Pts',(54.4721846627788,19.0697076193825,24.3855721550808));
#32121=CARTESIAN_POINT('Ctrl Pts',(54.6520710515779,19.0356917618733,24.3968553359351));
#32122=CARTESIAN_POINT('Ctrl Pts',(54.6748459090992,19.0317936704078,24.3982909124424));
#32123=CARTESIAN_POINT('Ctrl Pts',(54.7070005718512,19.0268634707939,24.4003297633327));
#32124=CARTESIAN_POINT('Ctrl Pts',(54.7163283966702,19.0255008624061,24.4009226332413));
#32125=CARTESIAN_POINT('Ctrl Pts',(54.7325954193293,19.0232422243168,24.4019591643541));
#32126=CARTESIAN_POINT('Ctrl Pts',(54.7395303771718,19.0223164846107,24.4024018828136));
#32127=CARTESIAN_POINT('Ctrl Pts',(54.7540554412726,19.020455274477,24.4033309331839));
#32128=CARTESIAN_POINT('Ctrl Pts',(54.7616463305098,19.0195269323018,24.4038174816814));
#32129=CARTESIAN_POINT('Ctrl Pts',(54.7797318788632,19.0174206090636,24.4049792154059));
#32130=CARTESIAN_POINT('Ctrl Pts',(54.7902308382829,19.0162822836284,24.4056556351956));
#32131=CARTESIAN_POINT('Ctrl Pts',(54.8258480083624,19.0127064874755,24.4079574508394));
#32132=CARTESIAN_POINT('Ctrl Pts',(54.8510024075139,19.0106624113426,24.4095950781105));
#32133=CARTESIAN_POINT('Ctrl Pts',(54.9113754114096,19.0069078809627,24.4135559498465));
#32134=CARTESIAN_POINT('Ctrl Pts',(54.9466128382667,19.0056529713029,24.415892575055));
#32135=CARTESIAN_POINT('Ctrl Pts',(55.0853077001173,19.0043918750168,24.4251877403351));
#32136=CARTESIAN_POINT('Ctrl Pts',(55.1886572786616,19.0114997699508,24.4323399416086));
#32137=CARTESIAN_POINT('Ctrl Pts',(55.4140974886809,19.0447407386672,24.4482246769193));
#32138=CARTESIAN_POINT('Ctrl Pts',(55.5352584213596,19.074378183792,24.4569523608459));
#32139=CARTESIAN_POINT('Ctrl Pts',(55.6676432703045,19.1202329160133,24.4662298844263));
#32140=CARTESIAN_POINT('Ctrl Pts',(55.682351326863,19.1255217980751,24.4672566075729));
#32141=CARTESIAN_POINT('Ctrl Pts',(55.7029269232083,19.1331948768822,24.4686857742312));
#32142=CARTESIAN_POINT('Ctrl Pts',(55.7088471473249,19.1354348090135,24.4690961502209));
#32143=CARTESIAN_POINT('Ctrl Pts',(55.7184056169918,19.1391033860441,24.4697572461807));
#32144=CARTESIAN_POINT('Ctrl Pts',(55.7220504428948,19.1405145881404,24.4700089863843));
#32145=CARTESIAN_POINT('Ctrl Pts',(55.7297524269464,19.1435226993168,24.4705401722585));
#32146=CARTESIAN_POINT('Ctrl Pts',(55.7338085422907,19.1451222152031,24.4708194546238));
#32147=CARTESIAN_POINT('Ctrl Pts',(55.7438298504644,19.1491121015627,24.4715084118892));
#32148=CARTESIAN_POINT('Ctrl Pts',(55.7497888599526,19.151518047898,24.4719171606612));
#32149=CARTESIAN_POINT('Ctrl Pts',(55.7719170798269,19.1605769156864,24.473431921239));
#32150=CARTESIAN_POINT('Ctrl Pts',(55.7880107871393,19.1674137646631,24.4745274388747));
#32151=CARTESIAN_POINT('Ctrl Pts',(55.8283880728196,19.1851969399015,24.4772654219345));
#32152=CARTESIAN_POINT('Ctrl Pts',(55.8525467468859,19.1964199130238,24.4788938772922));
#32153=CARTESIAN_POINT('Ctrl Pts',(56.0316276992867,19.2840151981439,24.4909441445611));
#32154=CARTESIAN_POINT('Ctrl Pts',(56.1762777001333,19.3797402981935,24.5006186912474));
#32155=CARTESIAN_POINT('Ctrl Pts',(56.3326308301585,19.5153142183306,24.5128740032492));
#32156=CARTESIAN_POINT('Ctrl Pts',(56.3578841520877,19.5383751275753,24.5149160073336));
#32157=CARTESIAN_POINT('Ctrl Pts',(56.4157110278066,19.593974244281,24.5197606758156));
#32158=CARTESIAN_POINT('Ctrl Pts',(56.4477742930153,19.6270122962901,24.522580664548));
#32159=CARTESIAN_POINT('Ctrl Pts',(56.4878816687065,19.6713073041469,24.5263064439513));
#32160=CARTESIAN_POINT('Ctrl Pts',(56.4969932466944,19.6815814987274,24.5271669406076));
#32161=CARTESIAN_POINT('Ctrl Pts',(56.5114497059954,19.6982256451391,24.528555515134));
#32162=CARTESIAN_POINT('Ctrl Pts',(56.5168622077254,19.704536482911,24.5290807819553));
#32163=CARTESIAN_POINT('Ctrl Pts',(56.527082284277,19.7166046917551,24.5300830273523));
#32164=CARTESIAN_POINT('Ctrl Pts',(56.531897157794,19.7223557163277,24.5305596949737));
#32165=CARTESIAN_POINT('Ctrl Pts',(56.5428062621453,19.7355361867768,24.531650077597));
#32166=CARTESIAN_POINT('Ctrl Pts',(56.5488794362536,19.742982743128,24.5322646300916));
#32167=CARTESIAN_POINT('Ctrl Pts',(56.5673820186913,19.7660071614647,24.5341604733343));
#32168=CARTESIAN_POINT('Ctrl Pts',(56.5796316632102,19.7817272559743,24.5354488705616));
#32169=CARTESIAN_POINT('Ctrl Pts',(56.6811813476548,19.9161539162316,24.54641962589));
#32170=CARTESIAN_POINT('Ctrl Pts',(56.7571826535879,20.044287776389,24.5566264820719));
#32171=CARTESIAN_POINT('Ctrl Pts',(56.8686209598344,20.2912798885625,24.5755180412968));
#32172=CARTESIAN_POINT('Ctrl Pts',(56.9086066661541,20.4073327590701,24.584100975454));
#32173=CARTESIAN_POINT('Ctrl Pts',(56.9414193521452,20.5415630888679,24.5932521286237));
#32174=CARTESIAN_POINT('Ctrl Pts',(56.944963652324,20.556840965103,24.5942824240086));
#32175=CARTESIAN_POINT('Ctrl Pts',(56.9496870534991,20.5783506981071,24.5957156917872));
#32176=CARTESIAN_POINT('Ctrl Pts',(56.9510170823219,20.5845483331275,24.5961266557924));
#32177=CARTESIAN_POINT('Ctrl Pts',(56.953119766704,20.594579196344,24.5967884444127));
#32178=CARTESIAN_POINT('Ctrl Pts',(56.9539107201787,20.5984084794924,24.597040293299));
#32179=CARTESIAN_POINT('Ctrl Pts',(56.9555594390969,20.6065106916597,24.5975714659817));
#32180=CARTESIAN_POINT('Ctrl Pts',(56.9564144705416,20.6107841527528,24.5978506276065));
#32181=CARTESIAN_POINT('Ctrl Pts',(56.958493790088,20.6213566161494,24.5985388688223));
#32182=CARTESIAN_POINT('Ctrl Pts',(56.9597017150029,20.6276588541642,24.5989470265737));
#32183=CARTESIAN_POINT('Ctrl Pts',(56.9640754850284,20.6510896180521,24.6004570629606));
#32184=CARTESIAN_POINT('Ctrl Pts',(56.9670474576904,20.6682541431399,24.601548532192));
#32185=CARTESIAN_POINT('Ctrl Pts',(56.9860985927904,20.7875596366002,24.6090468857285));
#32186=CARTESIAN_POINT('Ctrl Pts',(56.9944415430899,20.8907899121634,24.6150929570007));
#32187=CARTESIAN_POINT('Ctrl Pts',(56.9952065330458,21.1544603789626,24.6304148984246));
#32188=CARTESIAN_POINT('Ctrl Pts',(56.9763613361714,21.3141605022672,24.6396280555755));
#32189=CARTESIAN_POINT('Ctrl Pts',(56.9331801189221,21.4923160557855,24.6509262513412));
#32190=CARTESIAN_POINT('Ctrl Pts',(56.9273534283053,21.5146544128928,24.6523605894061));
#32191=CARTESIAN_POINT('Ctrl Pts',(56.9186042750282,21.545961535097,24.6543979654552));
#32192=CARTESIAN_POINT('Ctrl Pts',(56.9160037429072,21.5550189314289,24.6549906192823));
#32193=CARTESIAN_POINT('Ctrl Pts',(56.9113610036103,21.5707675668143,24.656026880526));
#32194=CARTESIAN_POINT('Ctrl Pts',(56.909347575784,21.5774671715941,24.6564695464577));
#32195=CARTESIAN_POINT('Ctrl Pts',(56.9050592124056,21.5914688960616,24.657398593521));
#32196=CARTESIAN_POINT('Ctrl Pts',(56.9027774422238,21.5987687871518,24.6578851917919));
#32197=CARTESIAN_POINT('Ctrl Pts',(56.8972439708907,21.6161205149528,24.6590472428152));
#32198=CARTESIAN_POINT('Ctrl Pts',(56.8939543100859,21.6261599142584,24.6597239319087));
#32199=CARTESIAN_POINT('Ctrl Pts',(56.8825287762426,21.6601144508086,24.662027636207));
#32200=CARTESIAN_POINT('Ctrl Pts',(56.8740187063137,21.6839001920939,24.6636669100598));
#32201=CARTESIAN_POINT('Ctrl Pts',(56.8525387016752,21.7405228395673,24.6676324875115));
#32202=CARTESIAN_POINT('Ctrl Pts',(56.8391445797303,21.7731886433931,24.6699722138506));
#32203=CARTESIAN_POINT('Ctrl Pts',(56.7830255071102,21.9003316902037,24.6792863832323));
#32204=CARTESIAN_POINT('Ctrl Pts',(56.7338327749072,21.9917643565053,24.686455361212));
#32205=CARTESIAN_POINT('Ctrl Pts',(56.610624479092,22.1833528612105,24.7023341584585));
#32206=CARTESIAN_POINT('Ctrl Pts',(56.5338803441178,22.2812695787954,24.7110381176753));
#32207=CARTESIAN_POINT('Ctrl Pts',(56.4377750938679,22.3827779463659,24.7202948658823));
#32208=CARTESIAN_POINT('Ctrl Pts',(56.426891045618,22.3940064740992,24.7213221078798));
#32209=CARTESIAN_POINT('Ctrl Pts',(56.4114161461479,22.4095999808155,24.7227518702476));
#32210=CARTESIAN_POINT('Ctrl Pts',(56.4069351640366,22.4140725194842,24.7231623316721));
#32211=CARTESIAN_POINT('Ctrl Pts',(56.3996533229827,22.4212717599659,24.7238235282743));
#32212=CARTESIAN_POINT('Ctrl Pts',(56.396865654455,22.4240116517299,24.7240752842722));
#32213=CARTESIAN_POINT('Ctrl Pts',(56.3909515979916,22.4297902720865,24.7246064681429));
#32214=CARTESIAN_POINT('Ctrl Pts',(56.3878232667474,22.4328269787615,24.7248857328756));
#32215=CARTESIAN_POINT('Ctrl Pts',(56.3800602550646,22.4403133456851,24.7255745857494));
#32216=CARTESIAN_POINT('Ctrl Pts',(56.3754139374104,22.444750962926,24.725983248388));
#32217=CARTESIAN_POINT('Ctrl Pts',(56.3580510251904,22.4611743013001,24.7274973198924));
#32218=CARTESIAN_POINT('Ctrl Pts',(56.3451981077814,22.4730156231024,24.7285922469728));
#32219=CARTESIAN_POINT('Ctrl Pts',(56.3123815466474,22.5024615056038,24.73132845339));
#32220=CARTESIAN_POINT('Ctrl Pts',(56.2922176330935,22.5198386848212,24.7329557458309));
#32221=CARTESIAN_POINT('Ctrl Pts',(56.1388915735912,22.6467162438117,24.7449856958899));
#32222=CARTESIAN_POINT('Ctrl Pts',(55.9923762343565,22.7389505321152,24.7546434375773));
#32223=CARTESIAN_POINT('Ctrl Pts',(55.7665585067778,22.8431584765607,24.76936898023));
#32224=CARTESIAN_POINT('Ctrl Pts',(55.6955352478824,22.8711156685095,24.7739701783918));
#32225=CARTESIAN_POINT('Ctrl Pts',(55.6093184682002,22.8994653899005,24.7796112167173));
#32226=CARTESIAN_POINT('Ctrl Pts',(55.5954969675613,22.9038437717777,24.7805170669479));
#32227=CARTESIAN_POINT('Ctrl Pts',(55.5727051384031,22.9107913090369,24.7820138994928));
#32228=CARTESIAN_POINT('Ctrl Pts',(55.563762179779,22.9134489285392,24.7826019909393));
#32229=CARTESIAN_POINT('Ctrl Pts',(55.5476241899227,22.9181217726163,24.7836647579728));
#32230=CARTESIAN_POINT('Ctrl Pts',(55.5404358141173,22.9201595028303,24.7841386913768));
#32231=CARTESIAN_POINT('Ctrl Pts',(55.5250616953261,22.9244245229243,24.7851535501004));
#32232=CARTESIAN_POINT('Ctrl Pts',(55.5168728748607,22.9266400691092,24.7856948456783));
#32233=CARTESIAN_POINT('Ctrl Pts',(55.4946475188633,22.9325014122606,24.7871661207754));
#32234=CARTESIAN_POINT('Ctrl Pts',(55.480585169007,22.9360464233084,24.7880993280154));
#32235=CARTESIAN_POINT('Ctrl Pts',(55.4064525763073,22.9538772592639,24.7930319914985));
#32236=CARTESIAN_POINT('Ctrl Pts',(55.3457874409596,22.9655202155769,24.797115040149));
#32237=CARTESIAN_POINT('Ctrl Pts',(55.2447304996243,22.9800919459253,24.8039962631807));
#32238=CARTESIAN_POINT('Ctrl Pts',(55.2046327693612,22.9846356983861,24.8067466482639));
#32239=CARTESIAN_POINT('Ctrl Pts',(55.1644480328175,22.9879598605109,24.8095189920889));
#32240=CARTESIAN_POINT('Origin',(55.,21.,6.22095488139522));
#32241=CARTESIAN_POINT('',(55.1644486115703,22.9879598126352,25.7694502499567));
#32242=CARTESIAN_POINT('',(55.1644483516311,22.987959834138,25.6104387285779));
#32243=CARTESIAN_POINT('',(55.1644483516311,22.987959834138,6.22095488139522));
#32244=CARTESIAN_POINT('Ctrl Pts',(55.1644486115703,22.9879598126352,25.7694502499567));
#32245=CARTESIAN_POINT('Ctrl Pts',(55.1987137427014,22.9851253221169,25.7670853474462));
#32246=CARTESIAN_POINT('Ctrl Pts',(55.2329147190426,22.9814041745798,25.7647034036361));
#32247=CARTESIAN_POINT('Ctrl Pts',(55.3633286894365,22.963788417207,25.7555552787918));
#32248=CARTESIAN_POINT('Ctrl Pts',(55.4585615134211,22.9437578732887,25.7487310203176));
#32249=CARTESIAN_POINT('Ctrl Pts',(55.6050887325483,22.9015657588654,25.7382731815912));
#32250=CARTESIAN_POINT('Ctrl Pts',(55.6575678444106,22.8840622241677,25.7345385385399));
#32251=CARTESIAN_POINT('Ctrl Pts',(55.717963738037,22.8610863550257,25.7303047097285));
#32252=CARTESIAN_POINT('Ctrl Pts',(55.7266478402137,22.8577129149717,25.7296975411362));
#32253=CARTESIAN_POINT('Ctrl Pts',(55.7399491257513,22.8524383333742,25.7287703605073));
#32254=CARTESIAN_POINT('Ctrl Pts',(55.7445831968322,22.8505805445787,25.728447864191));
#32255=CARTESIAN_POINT('Ctrl Pts',(55.7530843413423,22.8471353524798,25.7278572826226));
#32256=CARTESIAN_POINT('Ctrl Pts',(55.7569533865524,22.8455531980367,25.7275888985259));
#32257=CARTESIAN_POINT('Ctrl Pts',(55.7656455325285,22.8419668180063,25.7269868381286));
#32258=CARTESIAN_POINT('Ctrl Pts',(55.7704657422825,22.8399558096826,25.7266535755869));
#32259=CARTESIAN_POINT('Ctrl Pts',(55.7845835491554,22.8340006043129,25.7256791212905));
#32260=CARTESIAN_POINT('Ctrl Pts',(55.7938593205844,22.8300046315442,25.7250409613763));
#32261=CARTESIAN_POINT('Ctrl Pts',(55.8634704866508,22.799387470929,25.7202646175037));
#32262=CARTESIAN_POINT('Ctrl Pts',(55.9224895619041,22.7698563481475,25.7162873093644));
#32263=CARTESIAN_POINT('Ctrl Pts',(56.1304996229599,22.6525362883027,25.7021549861658));
#32264=CARTESIAN_POINT('Ctrl Pts',(56.2693784417955,22.5484145214144,25.6924300500915));
#32265=CARTESIAN_POINT('Ctrl Pts',(56.4298277762251,22.3918524716028,25.6789358331926));
#32266=CARTESIAN_POINT('Ctrl Pts',(56.4651557658104,22.3546138452156,25.675798456889));
#32267=CARTESIAN_POINT('Ctrl Pts',(56.5080429290298,22.3057647825805,25.6717451898777));
#32268=CARTESIAN_POINT('Ctrl Pts',(56.5169725906122,22.2953799781264,25.6708869403508));
#32269=CARTESIAN_POINT('Ctrl Pts',(56.531145310657,22.2785501968891,25.6695010653625));
#32270=CARTESIAN_POINT('Ctrl Pts',(56.5364563791508,22.2721628668902,25.6689762306133));
#32271=CARTESIAN_POINT('Ctrl Pts',(56.5464887966712,22.2599429637516,25.6679742004703));
#32272=CARTESIAN_POINT('Ctrl Pts',(56.5512174436157,22.2541165457146,25.6674973121549));
#32273=CARTESIAN_POINT('Ctrl Pts',(56.5619372666742,22.2407546949579,25.6664055664006));
#32274=CARTESIAN_POINT('Ctrl Pts',(56.5679069560941,22.2332023393362,25.6657898645808));
#32275=CARTESIAN_POINT('Ctrl Pts',(56.583331447765,22.2133955043724,25.6641785133988));
#32276=CARTESIAN_POINT('Ctrl Pts',(56.5926985545834,22.2010738592288,25.6631794451923));
#32277=CARTESIAN_POINT('Ctrl Pts',(56.6808603046209,22.0822594111258,25.6535753605125));
#32278=CARTESIAN_POINT('Ctrl Pts',(56.7489906850262,21.9682955440858,25.6445549407022));
#32279=CARTESIAN_POINT('Ctrl Pts',(56.8458512198371,21.7621958737475,25.6287258172756));
#32280=CARTESIAN_POINT('Ctrl Pts',(56.8801527438242,21.67315338539,25.6220354076973));
#32281=CARTESIAN_POINT('Ctrl Pts',(56.9247054453855,21.5270969724586,25.6115500348712));
#32282=CARTESIAN_POINT('Ctrl Pts',(56.9390768902927,21.471491709778,25.6076682751786));
#32283=CARTESIAN_POINT('Ctrl Pts',(56.9529873697942,21.4061479941851,25.6032903264984));
#32284=CARTESIAN_POINT('Ctrl Pts',(56.9548789845702,21.3969433508574,25.6026778295513));
#32285=CARTESIAN_POINT('Ctrl Pts',(56.9576792288291,21.3828115646912,25.6017442603133));
#32286=CARTESIAN_POINT('Ctrl Pts',(56.9586344287251,21.3778939441162,25.6014206511083));
#32287=CARTESIAN_POINT('Ctrl Pts',(56.9603525654504,21.3688669805552,25.6008289916017));
#32288=CARTESIAN_POINT('Ctrl Pts',(56.9611211109768,21.3647588504085,25.6005606350281));
#32289=CARTESIAN_POINT('Ctrl Pts',(56.9628175290375,21.3555305690075,25.5999598280195));
#32290=CARTESIAN_POINT('Ctrl Pts',(56.9637382805708,21.3504091960823,25.59962778303));
#32291=CARTESIAN_POINT('Ctrl Pts',(56.9660426973824,21.3372972523279,25.5987810653452));
#32292=CARTESIAN_POINT('Ctrl Pts',(56.9673977110284,21.3293016493912,25.5982679634477));
#32293=CARTESIAN_POINT('Ctrl Pts',(56.9751916531498,21.2815454477942,25.5952213143963));
#32294=CARTESIAN_POINT('Ctrl Pts',(56.9804743545328,21.2416024641927,25.592747454608));
#32295=CARTESIAN_POINT('Ctrl Pts',(57.0025758128941,21.0239542000424,25.5795369209107));
#32296=CARTESIAN_POINT('Ctrl Pts',(56.9966960605877,20.8447574200326,25.5695615310469));
#32297=CARTESIAN_POINT('Ctrl Pts',(56.9592821020438,20.6226031753363,25.5561728113888));
#32298=CARTESIAN_POINT('Ctrl Pts',(56.9498962616782,20.5767756674893,25.5533593531232));
#32299=CARTESIAN_POINT('Ctrl Pts',(56.9315693366514,20.5009575520206,25.548587276673));
#32300=CARTESIAN_POINT('Ctrl Pts',(56.9235174912562,20.4707705961186,25.5466557194962));
#32301=CARTESIAN_POINT('Ctrl Pts',(56.9115422466572,20.4297670794274,25.54398315837));
#32302=CARTESIAN_POINT('Ctrl Pts',(56.9082290077694,20.4187759557905,25.5432619206835));
#32303=CARTESIAN_POINT('Ctrl Pts',(56.9024970348965,20.4003385270025,25.5420436159648));
#32304=CARTESIAN_POINT('Ctrl Pts',(56.9001289704138,20.3928766657925,25.5415482128943));
#32305=CARTESIAN_POINT('Ctrl Pts',(56.8953641778733,20.3781635919909,25.5405666753345));
#32306=CARTESIAN_POINT('Ctrl Pts',(56.8929696090625,20.3709118173179,25.540080618982));
#32307=CARTESIAN_POINT('Ctrl Pts',(56.8875997098284,20.3549577699148,25.5390061791335));
#32308=CARTESIAN_POINT('Ctrl Pts',(56.8846057331062,20.346262002641,25.53841718838));
#32309=CARTESIAN_POINT('Ctrl Pts',(56.8738423888088,20.315689231853,25.5363343199171));
#32310=CARTESIAN_POINT('Ctrl Pts',(56.8657515919242,20.2939281571805,25.5348298505742));
#32311=CARTESIAN_POINT('Ctrl Pts',(56.7973254741935,20.1192832269913,25.5225725790334));
#32312=CARTESIAN_POINT('Ctrl Pts',(56.7186950303505,19.9742771673024,25.5111737305711));
#32313=CARTESIAN_POINT('Ctrl Pts',(56.5649908452727,19.7590884269826,25.4927338148515));
#32314=CARTESIAN_POINT('Ctrl Pts',(56.5007184611168,19.6820827106578,25.4857743850951));
#32315=CARTESIAN_POINT('Ctrl Pts',(56.4189681743203,19.5979117277289,25.4779914188751));
#32316=CARTESIAN_POINT('Ctrl Pts',(56.4068500416963,19.5857527758847,25.4768626104906));
#32317=CARTESIAN_POINT('Ctrl Pts',(56.3900130935428,19.5692897261254,25.4753298587012));
#32318=CARTESIAN_POINT('Ctrl Pts',(56.3854287439169,19.564850012639,25.474916065421));
#32319=CARTESIAN_POINT('Ctrl Pts',(56.3776823586011,19.5574197349651,25.4742229149952));
#32320=CARTESIAN_POINT('Ctrl Pts',(56.3745317290066,19.5544174083192,25.4739426615991));
#32321=CARTESIAN_POINT('Ctrl Pts',(56.3685260029905,19.5487317640814,25.4734116438554));
#32322=CARTESIAN_POINT('Ctrl Pts',(56.3656727959931,19.5460465178075,25.4731607263745));
#32323=CARTESIAN_POINT('Ctrl Pts',(56.3581548400927,19.5390127785168,25.472503081986));
#32324=CARTESIAN_POINT('Ctrl Pts',(56.3534770713746,19.5346781749595,25.4720974077733));
#32325=CARTESIAN_POINT('Ctrl Pts',(56.3370595480313,19.5196107480058,25.4706855223959));
#32326=CARTESIAN_POINT('Ctrl Pts',(56.3252119162404,19.5089956448969,25.4696877441147));
#32327=CARTESIAN_POINT('Ctrl Pts',(56.2277076935532,19.4237154408265,25.4616338473089));
#32328=CARTESIAN_POINT('Ctrl Pts',(56.1359294820986,19.3563423914512,25.45502332415));
#32329=CARTESIAN_POINT('Ctrl Pts',(55.945094257375,19.239914863322,25.4420474701758));
#32330=CARTESIAN_POINT('Ctrl Pts',(55.8467243269586,19.1905363247235,25.435699930808));
#32331=CARTESIAN_POINT('Ctrl Pts',(55.6920528987658,19.1282835835363,25.4257026965543));
#32332=CARTESIAN_POINT('Ctrl Pts',(55.6384346344294,19.1093229080778,25.4222367430073));
#32333=CARTESIAN_POINT('Ctrl Pts',(55.5705552912544,19.0885360601271,25.4178129543353));
#32334=CARTESIAN_POINT('Ctrl Pts',(55.5569838004522,19.0845374544169,25.4169267859392));
#32335=CARTESIAN_POINT('Ctrl Pts',(55.5352820159186,19.0783935352728,25.4155065511723));
#32336=CARTESIAN_POINT('Ctrl Pts',(55.5271785438499,19.0761546264718,25.4149755307995));
#32337=CARTESIAN_POINT('Ctrl Pts',(55.511833707776,19.0720192299842,25.4139685514591));
#32338=CARTESIAN_POINT('Ctrl Pts',(55.5045953311176,19.0701121423055,25.4134929453715));
#32339=CARTESIAN_POINT('Ctrl Pts',(55.4881900153905,19.0658884547582,25.4124135802196));
#32340=CARTESIAN_POINT('Ctrl Pts',(55.4790170467408,19.0635962134906,25.4118090471561));
#32341=CARTESIAN_POINT('Ctrl Pts',(55.455341513841,19.0578584345586,25.4102459849503));
#32342=CARTESIAN_POINT('Ctrl Pts',(55.4408162099327,19.0545101379141,25.4092843650881));
#32343=CARTESIAN_POINT('Ctrl Pts',(55.3413278626324,19.0327479598299,25.4026785576816));
#32344=CARTESIAN_POINT('Ctrl Pts',(55.2552889208056,19.0197451693043,25.3968633144754));
#32345=CARTESIAN_POINT('Ctrl Pts',(55.0195324630175,18.9997367425953,25.3806764698064));
#32346=CARTESIAN_POINT('Ctrl Pts',(54.8694411485365,19.0039076819948,25.3700669397672));
#32347=CARTESIAN_POINT('Ctrl Pts',(54.6715682255119,19.0318343432153,25.3564043538794));
#32348=CARTESIAN_POINT('Ctrl Pts',(54.6221786573854,19.0407155730788,25.3530266801714));
#32349=CARTESIAN_POINT('Ctrl Pts',(54.564285719063,19.0533969622904,25.3491452445288));
#32350=CARTESIAN_POINT('Ctrl Pts',(54.5554124616931,19.0554043480942,25.3485525293237));
#32351=CARTESIAN_POINT('Ctrl Pts',(54.5417366368638,19.0585967151658,25.3476427285455));
#32352=CARTESIAN_POINT('Ctrl Pts',(54.5369243614921,19.0597389405891,25.3473232987571));
#32353=CARTESIAN_POINT('Ctrl Pts',(54.5280496332209,19.0618803146879,25.3467355908434));
#32354=CARTESIAN_POINT('Ctrl Pts',(54.5239860976243,19.0628743384554,25.3464670349452));
#32355=CARTESIAN_POINT('Ctrl Pts',(54.5148001264134,19.0651520651995,25.3458611472473));
#32356=CARTESIAN_POINT('Ctrl Pts',(54.5096796513578,19.0664433275995,25.3455242535553));
#32357=CARTESIAN_POINT('Ctrl Pts',(54.4964631959368,19.0698320819651,25.344656732413));
#32358=CARTESIAN_POINT('Ctrl Pts',(54.4883750737319,19.0719602064619,25.3441278097276));
#32359=CARTESIAN_POINT('Ctrl Pts',(54.4371322928298,19.0857882318441,25.3407879589516));
#32360=CARTESIAN_POINT('Ctrl Pts',(54.3943642813671,19.0988864291551,25.3380507863272));
#32361=CARTESIAN_POINT('Ctrl Pts',(54.3294702529646,19.1211736710106,25.3339244024836));
#32362=CARTESIAN_POINT('Ctrl Pts',(54.3070118619256,19.1293407513215,25.3325014201927));
#32363=CARTESIAN_POINT('Ctrl Pts',(54.221587247276,19.1621553775841,25.327089607174));
#32364=CARTESIAN_POINT('Ctrl Pts',(54.1597407705482,19.1895955265956,25.3231719037584));
#32365=CARTESIAN_POINT('Ctrl Pts',(53.9663797051667,19.2874337849833,25.3105997711783));
#32366=CARTESIAN_POINT('Ctrl Pts',(53.841338140746,19.3694329476286,25.3019263243817));
#32367=CARTESIAN_POINT('Ctrl Pts',(53.71334315765,19.4755858480685,25.2916052019623));
#32368=CARTESIAN_POINT('Ctrl Pts',(53.7002263401399,19.4867542365627,25.2905293215721));
#32369=CARTESIAN_POINT('Ctrl Pts',(53.680428187019,19.5040588145211,25.2888764750155));
#32370=CARTESIAN_POINT('Ctrl Pts',(53.6736411084337,19.5100731942793,25.2883045442814));
#32371=CARTESIAN_POINT('Ctrl Pts',(53.6613486404189,19.5211167395031,25.2872588180134));
#32372=CARTESIAN_POINT('Ctrl Pts',(53.6558299623056,19.5261309189819,25.2867856571914));
#32373=CARTESIAN_POINT('Ctrl Pts',(53.6439457020634,19.5370510252227,25.285758631805));
#32374=CARTESIAN_POINT('Ctrl Pts',(53.6375903322752,19.5429677920137,25.2852043111359));
#32375=CARTESIAN_POINT('Ctrl Pts',(53.6203584925594,19.5592217292458,25.2836872151279));
#32376=CARTESIAN_POINT('Ctrl Pts',(53.609559883736,19.5696402630136,25.2827209465972));
#32377=CARTESIAN_POINT('Ctrl Pts',(53.5544839065643,19.6239908258312,25.2777105893766));
#32378=CARTESIAN_POINT('Ctrl Pts',(53.5121715471467,19.6698559806677,25.2735815415471));
#32379=CARTESIAN_POINT('Ctrl Pts',(53.3603285933521,19.850773098871,25.2576460762852));
#32380=CARTESIAN_POINT('Ctrl Pts',(53.2664787650186,19.9979343331679,25.2452961260464));
#32381=CARTESIAN_POINT('Ctrl Pts',(53.1705139197744,20.2032558780712,25.2297746884592));
#32382=CARTESIAN_POINT('Ctrl Pts',(53.1500459799559,20.2520082043859,25.2262102003987));
#32383=CARTESIAN_POINT('Ctrl Pts',(53.1283100090884,20.3101528623972,25.2221438568295));
#32384=CARTESIAN_POINT('Ctrl Pts',(53.1251427658284,20.3188077696421,25.2215433009778));
#32385=CARTESIAN_POINT('Ctrl Pts',(53.1203595096896,20.3321647632041,25.2206240643528));
#32386=CARTESIAN_POINT('Ctrl Pts',(53.1187009518077,20.3368513221767,25.2203029639187));
#32387=CARTESIAN_POINT('Ctrl Pts',(53.1156795724806,20.3454913483539,25.2197136871885));
#32388=CARTESIAN_POINT('Ctrl Pts',(53.1143116678404,20.3494428824373,25.2194452217143));
#32389=CARTESIAN_POINT('Ctrl Pts',(53.1112546477196,20.358364503779,25.218841417915));
#32390=CARTESIAN_POINT('Ctrl Pts',(53.1095727210666,20.3633369648263,25.2185065043475));
#32391=CARTESIAN_POINT('Ctrl Pts',(53.1052949474696,20.3761502256042,25.217647497414));
#32392=CARTESIAN_POINT('Ctrl Pts',(53.102728103208,20.384000704284,25.2171250533664));
#32393=CARTESIAN_POINT('Ctrl Pts',(53.0871510780936,20.4326628863885,25.2139091086782));
#32394=CARTESIAN_POINT('Ctrl Pts',(53.075408468489,20.4738722174298,25.2112832282967));
#32395=CARTESIAN_POINT('Ctrl Pts',(53.0634629608103,20.5215734599231,25.2083209097801));
#32396=CARTESIAN_POINT('Ctrl Pts',(53.0619539879243,20.5277232644443,25.2079404568527));
#32397=CARTESIAN_POINT('Ctrl Pts',(53.0577687344165,20.5451381152892,25.2068669610492));
#32398=CARTESIAN_POINT('Ctrl Pts',(53.0551611882988,20.5564195364914,25.2061761029616));
#32399=CARTESIAN_POINT('Ctrl Pts',(53.0429075624966,20.6116204474346,25.2028151583015));
#32400=CARTESIAN_POINT('Ctrl Pts',(53.0346498716367,20.655836300039,25.2001828725965));
#32401=CARTESIAN_POINT('Ctrl Pts',(53.0128925837776,20.7990026686966,25.1917507212868));
#32402=CARTESIAN_POINT('Ctrl Pts',(53.0053239422665,20.898694736625,25.1860104863481));
#32403=CARTESIAN_POINT('Ctrl Pts',(53.0051907103367,21.0799090277027,25.1753093433157));
#32404=CARTESIAN_POINT('Ctrl Pts',(53.0101103656949,21.1612031272879,25.170412390646));
#32405=CARTESIAN_POINT('Ctrl Pts',(53.0217625348664,21.2565544136016,25.1644434531611));
#32406=CARTESIAN_POINT('Ctrl Pts',(53.0237067659709,21.2711248247565,25.1635252310404));
#32407=CARTESIAN_POINT('Ctrl Pts',(53.0271569043668,21.294967622256,25.1620120252493));
#32408=CARTESIAN_POINT('Ctrl Pts',(53.0285676134974,21.3042533791974,25.1614200419647));
#32409=CARTESIAN_POINT('Ctrl Pts',(53.0312194072802,21.3209150676238,25.1603529121146));
#32410=CARTESIAN_POINT('Ctrl Pts',(53.0324365059465,21.3282946805478,25.1598785326594));
#32411=CARTESIAN_POINT('Ctrl Pts',(53.0351164056717,21.3439932658364,25.1588656081408));
#32412=CARTESIAN_POINT('Ctrl Pts',(53.0365905973743,21.3523101194445,25.158326710118));
#32413=CARTESIAN_POINT('Ctrl Pts',(53.0407076951347,21.3747085536115,25.1568691401507));
#32414=CARTESIAN_POINT('Ctrl Pts',(53.043449526565,21.3887712221637,25.1559473436282));
#32415=CARTESIAN_POINT('Ctrl Pts',(53.0583059357758,21.4608271560232,25.1511888790892));
#32416=CARTESIAN_POINT('Ctrl Pts',(53.07284720207,21.5182840795158,25.1472755411651));
#32417=CARTESIAN_POINT('Ctrl Pts',(53.125923392249,21.6945952213958,25.1348865795288));
#32418=CARTESIAN_POINT('Ctrl Pts',(53.1730731901187,21.8105290853614,25.1261688925054));
#32419=CARTESIAN_POINT('Ctrl Pts',(53.2539703931561,21.9658869139979,25.1139607142313));
#32420=CARTESIAN_POINT('Ctrl Pts',(53.2788777314909,22.0096016120363,25.1104654592546));
#32421=CARTESIAN_POINT('Ctrl Pts',(53.3344303282074,22.0990591336827,25.1032411605051));
#32422=CARTESIAN_POINT('Ctrl Pts',(53.3653726540244,22.1445732597396,25.0995237832423));
#32423=CARTESIAN_POINT('Ctrl Pts',(53.4034361443054,22.1958636218789,25.0953349161264));
#32424=CARTESIAN_POINT('Ctrl Pts',(53.4087597193454,22.2029382043951,25.0947571572306));
#32425=CARTESIAN_POINT('Ctrl Pts',(53.4174230406902,22.2142928793373,25.0938302017551));
#32426=CARTESIAN_POINT('Ctrl Pts',(53.4207333938952,22.2185950998905,25.0934790645787));
#32427=CARTESIAN_POINT('Ctrl Pts',(53.4266332646917,22.2261983034915,25.0928587328654));
#32428=CARTESIAN_POINT('Ctrl Pts',(53.4292156757261,22.2295046852513,25.0925890507336));
#32429=CARTESIAN_POINT('Ctrl Pts',(53.4347998581858,22.2366080643972,25.0920098571577));
#32430=CARTESIAN_POINT('Ctrl Pts',(53.4378050199245,22.2404022872835,25.0917005911911));
#32431=CARTESIAN_POINT('Ctrl Pts',(53.446193135112,22.2509140212713,25.0908439607375));
#32432=CARTESIAN_POINT('Ctrl Pts',(53.4516058827614,22.2576077791068,25.0902986707892));
#32433=CARTESIAN_POINT('Ctrl Pts',(53.4829738471706,22.2958899211716,25.0871799037485));
#32434=CARTESIAN_POINT('Ctrl Pts',(53.5098540068613,22.326711911013,25.0846680261461));
#32435=CARTESIAN_POINT('Ctrl Pts',(53.6033336616256,22.4274709490318,25.0763677402079));
#32436=CARTESIAN_POINT('Ctrl Pts',(53.6740605271425,22.4933980095581,25.0707809079501));
#32437=CARTESIAN_POINT('Ctrl Pts',(53.856592186776,22.6403105570128,25.0571873701118));
#32438=CARTESIAN_POINT('Ctrl Pts',(53.9725373406965,22.7153176723617,25.0491798743587));
#32439=CARTESIAN_POINT('Ctrl Pts',(54.1167541340739,22.7887104366737,25.0392170930963));
#32440=CARTESIAN_POINT('Ctrl Pts',(54.1384267072222,22.7992497517744,25.0377208913161));
#32441=CARTESIAN_POINT('Ctrl Pts',(54.1689895627996,22.8134335723434,25.0356098561294));
#32442=CARTESIAN_POINT('Ctrl Pts',(54.1777238551143,22.8174106867839,25.0350064454044));
#32443=CARTESIAN_POINT('Ctrl Pts',(54.1929147417576,22.8241958547521,25.033956621114));
#32444=CARTESIAN_POINT('Ctrl Pts',(54.1993581850637,22.8270330628305,25.0335112117328));
#32445=CARTESIAN_POINT('Ctrl Pts',(54.2128031623955,22.8328684379433,25.0325815182322));
#32446=CARTESIAN_POINT('Ctrl Pts',(54.219807106966,22.8358607297286,25.0320970431942));
#32447=CARTESIAN_POINT('Ctrl Pts',(54.2363917697655,22.8428341410072,25.0309493763775));
#32448=CARTESIAN_POINT('Ctrl Pts',(54.2459866761908,22.8467807399175,25.0302850298756));
#32449=CARTESIAN_POINT('Ctrl Pts',(54.2779932371539,22.8596547451663,25.0280674125708));
#32450=CARTESIAN_POINT('Ctrl Pts',(54.3005352996268,22.8682501398506,25.0265030946542));
#32451=CARTESIAN_POINT('Ctrl Pts',(54.3545044763139,22.8877151893424,25.0227505152921));
#32452=CARTESIAN_POINT('Ctrl Pts',(54.3860575962214,22.8982116896339,25.0205506601696));
#32453=CARTESIAN_POINT('Ctrl Pts',(54.5799959784933,22.9573862062563,25.006992035006));
#32454=CARTESIAN_POINT('Ctrl Pts',(54.7477669732928,22.9859824683103,24.9950210163085));
#32455=CARTESIAN_POINT('Ctrl Pts',(54.9872897546912,22.9959464872326,24.9784515668118));
#32456=CARTESIAN_POINT('Ctrl Pts',(55.0576018867768,22.9951561742846,24.9736629886231));
#32457=CARTESIAN_POINT('Ctrl Pts',(55.1379314968794,22.9900017360129,24.968378859988));
#32458=CARTESIAN_POINT('Ctrl Pts',(55.148125421962,22.9892689303293,24.9677117846586));
#32459=CARTESIAN_POINT('Ctrl Pts',(55.1603587101088,22.9882949619975,24.9669158040825));
#32460=CARTESIAN_POINT('Ctrl Pts',(55.1624036561328,22.9881289757869,24.966782898771));
#32461=CARTESIAN_POINT('Ctrl Pts',(55.1644483516314,22.9879598341379,24.9666501649259));
#32462=CARTESIAN_POINT('',(53.0052505171966,21.0014364385374,25.0209548813952));
#32463=CARTESIAN_POINT('Ctrl Pts',(55.1644480328175,22.9879598605109,24.8095189920889));
#32464=CARTESIAN_POINT('Ctrl Pts',(55.0694986482504,22.9958142643243,24.8160695474148));
#32465=CARTESIAN_POINT('Ctrl Pts',(54.9740639845202,22.9968597274719,24.8227495899263));
#32466=CARTESIAN_POINT('Ctrl Pts',(54.7885947631868,22.9855771526695,24.8356719559787));
#32467=CARTESIAN_POINT('Ctrl Pts',(54.6987781032876,22.973949870372,24.8418996449565));
#32468=CARTESIAN_POINT('Ctrl Pts',(54.599810923806,22.9542224305118,24.8485268780842));
#32469=CARTESIAN_POINT('Ctrl Pts',(54.5895859910395,22.9521006524244,24.8492086813215));
#32470=CARTESIAN_POINT('Ctrl Pts',(54.5742014826202,22.948781985647,24.8502296723462));
#32471=CARTESIAN_POINT('Ctrl Pts',(54.5690294295359,22.9476447247763,24.8505720851651));
#32472=CARTESIAN_POINT('Ctrl Pts',(54.5597799131597,22.9455722388945,24.8511828822077));
#32473=CARTESIAN_POINT('Ctrl Pts',(54.5557008192255,22.9446447749193,24.8514516977496));
#32474=CARTESIAN_POINT('Ctrl Pts',(54.5468190821993,22.9425959280332,24.85203580544));
#32475=CARTESIAN_POINT('Ctrl Pts',(54.5420176780389,22.9414695665684,24.8523508098508));
#32476=CARTESIAN_POINT('Ctrl Pts',(54.5284320347866,22.9382293069453,24.8532400930335));
#32477=CARTESIAN_POINT('Ctrl Pts',(54.5196577760865,22.9360734870835,24.8538120311549));
#32478=CARTESIAN_POINT('Ctrl Pts',(54.4635245733565,22.92187655774,24.8574573507342));
#32479=CARTESIAN_POINT('Ctrl Pts',(54.4166026810043,22.9081571823331,24.8604422002779));
#32480=CARTESIAN_POINT('Ctrl Pts',(54.2372081337404,22.8484667656616,24.8717785910531));
#32481=CARTESIAN_POINT('Ctrl Pts',(54.1092171139349,22.790305046343,24.8797290338978));
#32482=CARTESIAN_POINT('Ctrl Pts',(53.9046806401534,22.6699501066238,24.8936436136888));
#32483=CARTESIAN_POINT('Ctrl Pts',(53.8247038376438,22.61466193902,24.8994424917228));
#32484=CARTESIAN_POINT('Ctrl Pts',(53.7371820630214,22.5441993382042,24.9064188352943));
#32485=CARTESIAN_POINT('Ctrl Pts',(53.7253983161695,22.534487297231,24.9073721427187));
#32486=CARTESIAN_POINT('Ctrl Pts',(53.7064178262241,22.5184742945385,24.9089313584512));
#32487=CARTESIAN_POINT('Ctrl Pts',(53.6991527158156,22.5122550583766,24.9095339433015));
#32488=CARTESIAN_POINT('Ctrl Pts',(53.6862740296592,22.5010688909484,24.9106126359956));
#32489=CARTESIAN_POINT('Ctrl Pts',(53.6806431615453,22.4961220775187,24.9110879060852));
#32490=CARTESIAN_POINT('Ctrl Pts',(53.6748282058459,22.4909551834413,24.9115825483667));
#32491=CARTESIAN_POINT('Ctrl Pts',(53.6746160832492,22.4907666203233,24.9116005976465));
#32492=CARTESIAN_POINT('Ctrl Pts',(53.6742405962284,22.4904326934249,24.9116325568571));
#32493=CARTESIAN_POINT('Ctrl Pts',(53.6740772154313,22.4902873480239,24.9116464660165));
#32494=CARTESIAN_POINT('Ctrl Pts',(53.6737870509912,22.4900291289757,24.911671174316));
#32495=CARTESIAN_POINT('Ctrl Pts',(53.6736602577595,22.4899162659251,24.9116819730149));
#32496=CARTESIAN_POINT('Ctrl Pts',(53.6734344933636,22.4897152535529,24.9117012042656));
#32497=CARTESIAN_POINT('Ctrl Pts',(53.6733355166616,22.4896271106267,24.9117096365444));
#32498=CARTESIAN_POINT('Ctrl Pts',(53.6731589276725,22.489469819127,24.911724683045));
#32499=CARTESIAN_POINT('Ctrl Pts',(53.6730813119391,22.4894006742915,24.9117312971128));
#32500=CARTESIAN_POINT('Ctrl Pts',(53.6728778291622,22.4892193708762,24.9117486388872));
#32501=CARTESIAN_POINT('Ctrl Pts',(53.6727519710279,22.4891072024914,24.9117593670015));
#32502=CARTESIAN_POINT('Ctrl Pts',(53.6725064295371,22.4888883130017,24.9117803005684));
#32503=CARTESIAN_POINT('Ctrl Pts',(53.6723867447892,22.488781593385,24.9117905059603));
#32504=CARTESIAN_POINT('Ctrl Pts',(53.6721531002008,22.4885732083161,24.9118104319152));
#32505=CARTESIAN_POINT('Ctrl Pts',(53.6720391391556,22.4884715441983,24.9118201524226));
#32506=CARTESIAN_POINT('Ctrl Pts',(53.6718165342088,22.4882729134487,24.9118391429239));
#32507=CARTESIAN_POINT('Ctrl Pts',(53.6717078892287,22.4881759479876,24.9118484128694));
#32508=CARTESIAN_POINT('Ctrl Pts',(53.6714955459617,22.4879863902022,24.9118665334425));
#32509=CARTESIAN_POINT('Ctrl Pts',(53.6713918467396,22.4878937989375,24.9118753840251));
#32510=CARTESIAN_POINT('Ctrl Pts',(53.6711890577208,22.4877126939811,24.9118926942909));
#32511=CARTESIAN_POINT('Ctrl Pts',(53.6710899671371,22.4876241812735,24.9119011539303));
#32512=CARTESIAN_POINT('Ctrl Pts',(53.6708960880452,22.4874509638594,24.9119177082222));
#32513=CARTESIAN_POINT('Ctrl Pts',(53.6708012987304,22.4873662599383,24.9119258028445));
#32514=CARTESIAN_POINT('Ctrl Pts',(53.6706157412565,22.4872004135045,24.9119416507998));
#32515=CARTESIAN_POINT('Ctrl Pts',(53.6705249723595,22.4871192716804,24.911949404107));
#32516=CARTESIAN_POINT('Ctrl Pts',(53.6703471985066,22.4869603234802,24.9119645911416));
#32517=CARTESIAN_POINT('Ctrl Pts',(53.670260192947,22.4868825177742,24.9119720248409));
#32518=CARTESIAN_POINT('Ctrl Pts',(53.6700897096876,22.4867300342585,24.9119865925954));
#32519=CARTESIAN_POINT('Ctrl Pts',(53.670006231586,22.4866553571777,24.9119937266134));
#32520=CARTESIAN_POINT('Ctrl Pts',(53.6698425869416,22.4865089406253,24.9120077132792));
#32521=CARTESIAN_POINT('Ctrl Pts',(53.6697624198444,22.4864372016385,24.9120145659098));
#32522=CARTESIAN_POINT('Ctrl Pts',(53.6628926127019,22.4802886287659,24.9126018584426));
#32523=CARTESIAN_POINT('Ctrl Pts',(53.6561447796106,22.4741654356619,24.9131842453037));
#32524=CARTESIAN_POINT('Ctrl Pts',(53.6365165287981,22.4561073891668,24.9148947291948));
#32525=CARTESIAN_POINT('Ctrl Pts',(53.623751736778,22.4440486800239,24.9160280814115));
#32526=CARTESIAN_POINT('Ctrl Pts',(53.5950020375112,22.4161618084909,24.9186298075048));
#32527=CARTESIAN_POINT('Ctrl Pts',(53.5791225752763,22.4002288450258,24.9201026320038));
#32528=CARTESIAN_POINT('Ctrl Pts',(53.5277394391093,22.3468983816586,24.9249893124848));
#32529=CARTESIAN_POINT('Ctrl Pts',(53.493418431436,22.3083950639374,24.9284503096402));
#32530=CARTESIAN_POINT('Ctrl Pts',(53.3771548011107,22.1673169959474,24.9408916577074));
#32531=CARTESIAN_POINT('Ctrl Pts',(53.303885422737,22.0580386044249,24.9501299119466));
#32532=CARTESIAN_POINT('Ctrl Pts',(53.2054529529215,21.8744003200238,24.9645672612726));
#32533=CARTESIAN_POINT('Ctrl Pts',(53.1729875878152,21.8043652286845,24.9698421783664));
#32534=CARTESIAN_POINT('Ctrl Pts',(53.1408593093562,21.7230009508422,24.975585963564));
#32535=CARTESIAN_POINT('Ctrl Pts',(53.1371363652526,21.7133537494606,24.9762610072975));
#32536=CARTESIAN_POINT('Ctrl Pts',(53.1316281004472,21.6987430289135,24.9772738854839));
#32537=CARTESIAN_POINT('Ctrl Pts',(53.1297872393542,21.6938008409931,24.9776148714347));
#32538=CARTESIAN_POINT('Ctrl Pts',(53.1265218522209,21.6849267698452,24.9782241486304));
#32539=CARTESIAN_POINT('Ctrl Pts',(53.1250900755792,21.6809976700276,24.9784928618732));
#32540=CARTESIAN_POINT('Ctrl Pts',(53.1219909440572,21.6724091293542,24.9790779379945));
#32541=CARTESIAN_POINT('Ctrl Pts',(53.1203285708724,21.6677479848315,24.9793940055533));
#32542=CARTESIAN_POINT('Ctrl Pts',(53.1156539637337,21.6544850198008,24.980289331709));
#32543=CARTESIAN_POINT('Ctrl Pts',(53.1126832644326,21.6458685413581,24.9808661989606));
#32544=CARTESIAN_POINT('Ctrl Pts',(53.0936183491421,21.5893160550945,24.9846228963687));
#32545=CARTESIAN_POINT('Ctrl Pts',(53.079291264784,21.5407987876339,24.9877078373612));
#32546=CARTESIAN_POINT('Ctrl Pts',(53.0260467787715,21.3314979314074,25.0006390514469));
#32547=CARTESIAN_POINT('Ctrl Pts',(53.0053636459116,21.1667638399575,25.0099340749681));
#32548=CARTESIAN_POINT('Ctrl Pts',(53.0052504670078,21.0013649643292,25.019750596888));
#32549=CARTESIAN_POINT('Ctrl Pts',(53.0052505171966,21.0014364385374,25.0209548813952));
#32550=CARTESIAN_POINT('Ctrl Pts',(53.0052001533975,20.9314973777562,25.0254037518945));
#32551=CARTESIAN_POINT('Ctrl Pts',(53.0088323744059,20.8615259841515,25.0298526223938));
#32552=CARTESIAN_POINT('Ctrl Pts',(53.016130795315,20.7919362088143,25.0343014928931));
#32553=CARTESIAN_POINT('Ctrl Pts',(53.0234288322359,20.7223500947698,25.0387501293261));
#32554=CARTESIAN_POINT('Ctrl Pts',(53.0343926343225,20.6531460421601,25.0431987657592));
#32555=CARTESIAN_POINT('Ctrl Pts',(53.048953970378,20.5847326730935,25.0476474021923));
#32556=CARTESIAN_POINT('Ctrl Pts',(53.0642055004891,20.5130765726949,25.0523068999371));
#32557=CARTESIAN_POINT('Ctrl Pts',(53.0834039916007,20.4422885516444,25.056966397682));
#32558=CARTESIAN_POINT('Ctrl Pts',(53.1064115872689,20.3728234015283,25.0616258954268));
#32559=CARTESIAN_POINT('Ctrl Pts',(53.1284128967115,20.3063964577825,25.0660816001084));
#32560=CARTESIAN_POINT('Ctrl Pts',(53.1538968136819,20.2411795245564,25.0705373047901));
#32561=CARTESIAN_POINT('Ctrl Pts',(53.1826932359489,20.1775501912979,25.0749930094717));
#32562=CARTESIAN_POINT('Ctrl Pts',(53.2115124075885,20.1138705904264,25.0794522341908));
#32563=CARTESIAN_POINT('Ctrl Pts',(53.2436490666211,20.0517815147258,25.0839114589099));
#32564=CARTESIAN_POINT('Ctrl Pts',(53.2788875824894,19.9916351807055,25.088370683629));
#32565=CARTESIAN_POINT('Ctrl Pts',(53.3141870948961,19.9313847356555,25.0928376270975));
#32566=CARTESIAN_POINT('Ctrl Pts',(53.3525989041981,19.8730841418326,25.097304570566));
#32567=CARTESIAN_POINT('Ctrl Pts',(53.3938652082761,19.8170551182265,25.1017715140344));
#32568=CARTESIAN_POINT('Ctrl Pts',(53.3993768780767,19.8095716887248,25.1023681343998));
#32569=CARTESIAN_POINT('Ctrl Pts',(53.4049394140699,19.8021287303179,25.1029647547651));
#32570=CARTESIAN_POINT('Ctrl Pts',(53.4105521515587,19.7947269605664,25.1035613751305));
#32571=CARTESIAN_POINT('Ctrl Pts',(53.4524588730015,19.739462679318,25.1080159578556));
#32572=CARTESIAN_POINT('Ctrl Pts',(53.4973340371494,19.6862774989079,25.1124705405806));
#32573=CARTESIAN_POINT('Ctrl Pts',(53.5449437481546,19.6355078356892,25.1169251233057));
#32574=CARTESIAN_POINT('Ctrl Pts',(53.5924820341012,19.5848143381537,25.121373023175));
#32575=CARTESIAN_POINT('Ctrl Pts',(53.6427463924562,19.5365295194779,25.1258209230443));
#32576=CARTESIAN_POINT('Ctrl Pts',(53.6954616143976,19.4909581970701,25.1302688229135));
#32577=CARTESIAN_POINT('Ctrl Pts',(53.748114857069,19.4454404545809,25.1347114932196));
#32578=CARTESIAN_POINT('Ctrl Pts',(53.8032128716403,19.402630190384,25.1391541635256));
#32579=CARTESIAN_POINT('Ctrl Pts',(53.8604436771806,19.362795385536,25.1435968338317));
#32580=CARTESIAN_POINT('Ctrl Pts',(53.9176384992424,19.3229856265497,25.1480367108391));
#32581=CARTESIAN_POINT('Ctrl Pts',(53.9769630512782,19.2861478945724,25.1524765878465));
#32582=CARTESIAN_POINT('Ctrl Pts',(54.0380735607145,19.2525089162163,25.1569164648539));
#32583=CARTESIAN_POINT('Ctrl Pts',(54.0991663979844,19.2188796657061,25.161355057921));
#32584=CARTESIAN_POINT('Ctrl Pts',(54.1620437388259,19.1884475683449,25.1657936509881));
#32585=CARTESIAN_POINT('Ctrl Pts',(54.2263357484426,19.1613942270399,25.1702322440552));
#32586=CARTESIAN_POINT('Ctrl Pts',(54.2906309961562,19.1343395231808,25.1746710606741));
#32587=CARTESIAN_POINT('Ctrl Pts',(54.3563406020663,19.1106641008342,25.179109877293));
#32588=CARTESIAN_POINT('Ctrl Pts',(54.4230748723272,19.0905013852951,25.1835486939119));
#32589=CARTESIAN_POINT('Ctrl Pts',(54.4898797455656,19.0703173381712,25.1879922066737));
#32590=CARTESIAN_POINT('Ctrl Pts',(54.5577109774409,19.0536535572182,25.1924357194355));
#32591=CARTESIAN_POINT('Ctrl Pts',(54.6261647640543,19.0405932584414,25.1968792321974));
#32592=CARTESIAN_POINT('Ctrl Pts',(54.6946585840436,19.0275253216963,25.2013253436294));
#32593=CARTESIAN_POINT('Ctrl Pts',(54.7637751984106,19.0180651280658,25.2057714550614));
#32594=CARTESIAN_POINT('Ctrl Pts',(54.8331044622872,19.0122441191153,25.2102175664935));
#32595=CARTESIAN_POINT('Ctrl Pts',(54.9025542274361,19.0064129926626,25.2146714057168));
#32596=CARTESIAN_POINT('Ctrl Pts',(54.9722168907849,19.0042336923204,25.2191252449402));
#32597=CARTESIAN_POINT('Ctrl Pts',(55.0416818868452,19.0056855356266,25.2235790841636));
#32598=CARTESIAN_POINT('Ctrl Pts',(55.078155111173,19.006447839083,25.2259176127222));
#32599=CARTESIAN_POINT('Ctrl Pts',(55.1145739153244,19.0082103327259,25.2282561412809));
#32600=CARTESIAN_POINT('Ctrl Pts',(55.1508797507476,19.0109643383503,25.2305946698395));
#32601=CARTESIAN_POINT('Ctrl Pts',(55.2200375291387,19.0162103520679,25.2350492551131));
#32602=CARTESIAN_POINT('Ctrl Pts',(55.2890579270999,19.0250778938475,25.2395038403867));
#32603=CARTESIAN_POINT('Ctrl Pts',(55.3575314519216,19.0375528482563,25.2439584256602));
#32604=CARTESIAN_POINT('Ctrl Pts',(55.4259022511927,19.0500090874527,25.2484063280629));
#32605=CARTESIAN_POINT('Ctrl Pts',(55.4937273281079,19.0660619108251,25.2528542304656));
#32606=CARTESIAN_POINT('Ctrl Pts',(55.5606013397307,19.0856453566823,25.2573021328683));
#32607=CARTESIAN_POINT('Ctrl Pts',(55.6273967245928,19.105205777408,25.2617448056735));
#32608=CARTESIAN_POINT('Ctrl Pts',(55.6932427976504,19.1282884390331,25.2661874784788));
#32609=CARTESIAN_POINT('Ctrl Pts',(55.7577452285476,19.1547765091693,25.2706301512841));
#32610=CARTESIAN_POINT('Ctrl Pts',(55.8222071036778,19.1812479249875,25.2750700307682));
#32611=CARTESIAN_POINT('Ctrl Pts',(55.885326560898,19.2111203162352,25.2795099102524));
#32612=CARTESIAN_POINT('Ctrl Pts',(55.9467266951757,19.2442277690026,25.2839497897365));
#32613=CARTESIAN_POINT('Ctrl Pts',(56.0081090731831,19.2773256474444,25.2883883852544));
#32614=CARTESIAN_POINT('Ctrl Pts',(56.0677726847449,19.3136564979985,25.2928269807723));
#32615=CARTESIAN_POINT('Ctrl Pts',(56.1253644078508,19.3530080412939,25.2972655762902));
#32616=CARTESIAN_POINT('Ctrl Pts',(56.1829590312068,19.3923615662858,25.3017043953304));
#32617=CARTESIAN_POINT('Ctrl Pts',(56.2384811562253,19.4347358079341,25.3061432143706));
#32618=CARTESIAN_POINT('Ctrl Pts',(56.2916073734096,19.4798756776323,25.3105820334109));
#32619=CARTESIAN_POINT('Ctrl Pts',(56.3447897958764,19.5250633033963,25.3150255485332));
#32620=CARTESIAN_POINT('Ctrl Pts',(56.3955708776067,19.5730220795878,25.3194690636556));
#32621=CARTESIAN_POINT('Ctrl Pts',(56.4436617459362,19.6234578372529,25.3239125787779));
#32622=CARTESIAN_POINT('Ctrl Pts',(56.4917807385802,19.6739230905616,25.3283586925395));
#32623=CARTESIAN_POINT('Ctrl Pts',(56.5372060676061,19.7268678370387,25.332804806301));
#32624=CARTESIAN_POINT('Ctrl Pts',(56.5796889248339,19.7819645065693,25.3372509200626));
#32625=CARTESIAN_POINT('Ctrl Pts',(56.6222456208304,19.8371569387321,25.3417047615427));
#32626=CARTESIAN_POINT('Ctrl Pts',(56.6618493581873,19.8945083572998,25.3461586030229));
#32627=CARTESIAN_POINT('Ctrl Pts',(56.6982948970917,19.9536625759287,25.350612444503));
#32628=CARTESIAN_POINT('Ctrl Pts',(56.7174307681436,19.9847217270316,25.3529509511848));
#32629=CARTESIAN_POINT('Ctrl Pts',(56.7356967523851,20.0162774680169,25.3552894578666));
#32630=CARTESIAN_POINT('Ctrl Pts',(56.7530683958959,20.048275900373,25.3576279645484));
#32631=CARTESIAN_POINT('Ctrl Pts',(56.7861594011771,20.1092292749587,25.3620825538283));
#32632=CARTESIAN_POINT('Ctrl Pts',(56.8161329725906,20.1720308909635,25.3665371431082));
#32633=CARTESIAN_POINT('Ctrl Pts',(56.842778934709,20.2363290235365,25.3709917323881));
#32634=CARTESIAN_POINT('Ctrl Pts',(56.8693849222466,20.3005306953068,25.3754396388416));
#32635=CARTESIAN_POINT('Ctrl Pts',(56.8926730228657,20.3662239791824,25.3798875452951));
#32636=CARTESIAN_POINT('Ctrl Pts',(56.9124788743392,20.4330325250015,25.3843354517486));
#32637=CARTESIAN_POINT('Ctrl Pts',(56.9322614394135,20.499762521788,25.3887781286503));
#32638=CARTESIAN_POINT('Ctrl Pts',(56.9485697485646,20.5676047092078,25.393220805552));
#32639=CARTESIAN_POINT('Ctrl Pts',(56.9612881542128,20.6361644071224,25.3976634824538));
#32640=CARTESIAN_POINT('Ctrl Pts',(56.9739985632717,20.7046809987109,25.4021033660602));
#32641=CARTESIAN_POINT('Ctrl Pts',(56.9831234574383,20.7739137257499,25.4065432496667));
#32642=CARTESIAN_POINT('Ctrl Pts',(56.9885978775687,20.8434559364608,25.4109831332731));
#32643=CARTESIAN_POINT('Ctrl Pts',(56.9940707145801,20.9129780366231,25.4154217329329));
#32644=CARTESIAN_POINT('Ctrl Pts',(56.9958951348644,20.9828089551278,25.4198603325926));
#32645=CARTESIAN_POINT('Ctrl Pts',(56.9940580328572,21.0525368832141,25.4242989322523));
#32646=CARTESIAN_POINT('Ctrl Pts',(56.9922208383303,21.1222683229188,25.4287377554475));
#32647=CARTESIAN_POINT('Ctrl Pts',(56.9867217707048,21.1918962727284,25.4331765786427));
#32648=CARTESIAN_POINT('Ctrl Pts',(56.9775998050228,21.2610106773175,25.437615401838));
#32649=CARTESIAN_POINT('Ctrl Pts',(56.9684681887157,21.3301982018052,25.4420589211064));
#32650=CARTESIAN_POINT('Ctrl Pts',(56.9557060884259,21.3988706105079,25.4465024403748));
#32651=CARTESIAN_POINT('Ctrl Pts',(56.9394040425061,21.4666256769734,25.4509459596432));
#32652=CARTESIAN_POINT('Ctrl Pts',(56.9230924628923,21.5344203676728,25.4553920775519));
#32653=CARTESIAN_POINT('Ctrl Pts',(56.9032369564458,21.6012961790338,25.4598381954606));
#32654=CARTESIAN_POINT('Ctrl Pts',(56.8799778501924,21.6668664373665,25.4642843133693));
#32655=CARTESIAN_POINT('Ctrl Pts',(56.8566783179238,21.7325506615686,25.4687381589537));
#32656=CARTESIAN_POINT('Ctrl Pts',(56.8299635648336,21.7969243512478,25.4731920045381));
#32657=CARTESIAN_POINT('Ctrl Pts',(56.8000215860336,21.8596219240533,25.4776458501225));
#32658=CARTESIAN_POINT('Ctrl Pts',(56.7843006973762,21.892540976189,25.4799843198342));
#32659=CARTESIAN_POINT('Ctrl Pts',(56.7676909130401,21.9249983947807,25.4823227895458));
#32660=CARTESIAN_POINT('Ctrl Pts',(56.7502242594158,21.9569444102206,25.4846612592574));
#32661=CARTESIAN_POINT('Ctrl Pts',(56.7169516615478,22.0177990506161,25.4891158596643));
#32662=CARTESIAN_POINT('Ctrl Pts',(56.6804357450355,22.0770364677886,25.4935704600712));
#32663=CARTESIAN_POINT('Ctrl Pts',(56.6408580806643,22.1342893465156,25.498025060478));
#32664=CARTESIAN_POINT('Ctrl Pts',(56.6013398682158,22.1914562223474,25.5024729693693));
#32665=CARTESIAN_POINT('Ctrl Pts',(56.5587693124784,22.2466440772406,25.5069208782606));
#32666=CARTESIAN_POINT('Ctrl Pts',(56.5133735161578,22.2995107398911,25.5113687871518));
#32667=CARTESIAN_POINT('Ctrl Pts',(56.468031430981,22.35231485206,25.5158114333911));
#32668=CARTESIAN_POINT('Ctrl Pts',(56.4198710620093,22.4028028573868,25.5202540796305));
#32669=CARTESIAN_POINT('Ctrl Pts',(56.3691613222879,22.4506635847263,25.5246967258698));
#32670=CARTESIAN_POINT('Ctrl Pts',(56.3184836056079,22.4984940881667,25.529136566592));
#32671=CARTESIAN_POINT('Ctrl Pts',(56.2652600671528,22.5437002699515,25.5335764073142));
#32672=CARTESIAN_POINT('Ctrl Pts',(56.2097971603903,22.5860070596349,25.5380162480364));
#32673=CARTESIAN_POINT('Ctrl Pts',(56.1543504450653,22.6283014985818,25.5424547926238));
#32674=CARTESIAN_POINT('Ctrl Pts',(56.0966660482703,22.6676979292194,25.5468933372112));
#32675=CARTESIAN_POINT('Ctrl Pts',(56.0370828691747,22.7039620550248,25.5513318817986));
#32676=CARTESIAN_POINT('Ctrl Pts',(55.9774968527151,22.7402279077358,25.5557706377505));
#32677=CARTESIAN_POINT('Ctrl Pts',(55.9160122938274,22.7733609072408,25.5602093937023));
#32678=CARTESIAN_POINT('Ctrl Pts',(55.8529948537301,22.8031714677229,25.5646481496542));
#32679=CARTESIAN_POINT('Ctrl Pts',(55.7899127541798,22.8330126155239,25.5690914600204));
#32680=CARTESIAN_POINT('Ctrl Pts',(55.7252950778109,22.8595243114278,25.5735347703865));
#32681=CARTESIAN_POINT('Ctrl Pts',(55.6595288283531,22.8825645505722,25.5779780807527));
#32682=CARTESIAN_POINT('Ctrl Pts',(55.5937241886818,22.9056182391639,25.582423984845));
#32683=CARTESIAN_POINT('Ctrl Pts',(55.526770111227,22.9251963003124,25.5868698889372));
#32684=CARTESIAN_POINT('Ctrl Pts',(55.4590675248692,22.9412069879615,25.5913157930294));
#32685=CARTESIAN_POINT('Ctrl Pts',(55.3912521515552,22.9572443481031,25.5957691036332));
#32686=CARTESIAN_POINT('Ctrl Pts',(55.3226862619325,22.9697023868234,25.600222414237));
#32687=CARTESIAN_POINT('Ctrl Pts',(55.2537788206309,22.9785408443343,25.6046757248408));
#32688=CARTESIAN_POINT('Ctrl Pts',(55.2240545789698,22.9823534434093,25.6065967260865));
#32689=CARTESIAN_POINT('Ctrl Pts',(55.1942668153676,22.9854931861074,25.6085177273322));
#32690=CARTESIAN_POINT('Ctrl Pts',(55.1644483516311,22.987959834138,25.6104387285779));
#32691=CARTESIAN_POINT('Origin',(55.,21.,6.22095488139522));
#32692=CARTESIAN_POINT('',(55.1644483516311,22.987959834138,26.5685072087751));
#32693=CARTESIAN_POINT('',(55.1643728891593,22.9868942741083,26.4105573801158));
#32694=CARTESIAN_POINT('',(55.1644483516311,22.987959834138,6.22095488139522));
#32695=CARTESIAN_POINT('',(53.005250049757,20.9995544605957,25.9790451186048));
#32696=CARTESIAN_POINT('Ctrl Pts',(53.005250049757,20.9995544605957,25.9790451186048));
#32697=CARTESIAN_POINT('Ctrl Pts',(53.0052554859099,20.9752159494636,25.9806079598459));
#32698=CARTESIAN_POINT('Ctrl Pts',(53.0057063467274,20.9508829793038,25.982170801087));
#32699=CARTESIAN_POINT('Ctrl Pts',(53.0066021269694,20.9265664770214,25.9837336423282));
#32700=CARTESIAN_POINT('Ctrl Pts',(53.0091549439874,20.8572686984656,25.9881874665249));
#32701=CARTESIAN_POINT('Ctrl Pts',(53.0153306838428,20.78796709998,25.9926412907217));
#32702=CARTESIAN_POINT('Ctrl Pts',(53.0251312383553,20.7190712959132,25.9970951149184));
#32703=CARTESIAN_POINT('Ctrl Pts',(53.0349170842458,20.6502788903161,26.0015422548387));
#32704=CARTESIAN_POINT('Ctrl Pts',(53.0483168791449,20.5818915511762,26.0059893947589));
#32705=CARTESIAN_POINT('Ctrl Pts',(53.0652805461648,20.5143167725238,26.0104365346791));
#32706=CARTESIAN_POINT('Ctrl Pts',(53.0822242708594,20.4468214341374,26.014878446584));
#32707=CARTESIAN_POINT('Ctrl Pts',(53.1027234278885,20.3801372316042,26.0193203584889));
#32708=CARTESIAN_POINT('Ctrl Pts',(53.1266766784958,20.3146626410238,26.0237622703938));
#32709=CARTESIAN_POINT('Ctrl Pts',(53.1506148735093,20.2492292038907,26.0282013903761));
#32710=CARTESIAN_POINT('Ctrl Pts',(53.178002687431,20.1850043292041,26.0326405103585));
#32711=CARTESIAN_POINT('Ctrl Pts',(53.2086890578424,20.1223709946644,26.0370796303408));
#32712=CARTESIAN_POINT('Ctrl Pts',(53.2393665699213,20.059755740689,26.0415174688682));
#32713=CARTESIAN_POINT('Ctrl Pts',(53.2733405328967,19.9987315542473,26.0459553073956));
#32714=CARTESIAN_POINT('Ctrl Pts',(53.3104126278366,19.9396594536065,26.050393145923));
#32715=CARTESIAN_POINT('Ctrl Pts',(53.347486620293,19.88058432939,26.054831211599));
#32716=CARTESIAN_POINT('Ctrl Pts',(53.3876587972494,19.8234619027611,26.0592692772749));
#32717=CARTESIAN_POINT('Ctrl Pts',(53.430686907246,19.7686251669736,26.0637073429508));
#32718=CARTESIAN_POINT('Ctrl Pts',(53.4737606498378,19.7137302751906,26.0681501153279));
#32719=CARTESIAN_POINT('Ctrl Pts',(53.5196960678683,19.6611262983735,26.072592887705));
#32720=CARTESIAN_POINT('Ctrl Pts',(53.5682105163276,19.6111132382569,26.0770356600821));
#32721=CARTESIAN_POINT('Ctrl Pts',(53.6167533952926,19.5610708694161,26.081481036019));
#32722=CARTESIAN_POINT('Ctrl Pts',(53.6678779538738,19.5136227724311,26.0859264119558));
#32723=CARTESIAN_POINT('Ctrl Pts',(53.7212666166781,19.4690302103313,26.0903717878927));
#32724=CARTESIAN_POINT('Ctrl Pts',(53.7747482750312,19.4243599742542,26.0948249070497));
#32725=CARTESIAN_POINT('Ctrl Pts',(53.8305015182019,19.3825554953541,26.0992780262068));
#32726=CARTESIAN_POINT('Ctrl Pts',(53.8881784858555,19.3438356110623,26.1037311453639));
#32727=CARTESIAN_POINT('Ctrl Pts',(53.9185544324252,19.3234435345665,26.106076409255));
#32728=CARTESIAN_POINT('Ctrl Pts',(53.9494635164362,19.3039062662285,26.1084216731461));
#32729=CARTESIAN_POINT('Ctrl Pts',(53.9808523549507,19.2852505605511,26.1107669370371));
#32730=CARTESIAN_POINT('Ctrl Pts',(54.0404847602063,19.2498085163744,26.1152224611471));
#32731=CARTESIAN_POINT('Ctrl Pts',(54.1020857201306,19.2174109949132,26.119677985257));
#32732=CARTESIAN_POINT('Ctrl Pts',(54.1653117999386,19.1882817075554,26.1241335093669));
#32733=CARTESIAN_POINT('Ctrl Pts',(54.2284429897427,19.1591961375719,26.1285823466049));
#32734=CARTESIAN_POINT('Ctrl Pts',(54.2931940178165,19.1333692693402,26.1330311838428));
#32735=CARTESIAN_POINT('Ctrl Pts',(54.3591950686674,19.110979988862,26.1374800210808));
#32736=CARTESIAN_POINT('Ctrl Pts',(54.4251183823711,19.0886170788547,26.1419236184034));
#32737=CARTESIAN_POINT('Ctrl Pts',(54.4922883335603,19.0696838712695,26.1463672157261));
#32738=CARTESIAN_POINT('Ctrl Pts',(54.5603149029982,19.0543112844099,26.1508108130488));
#32739=CARTESIAN_POINT('Ctrl Pts',(54.6282986042985,19.038948384856,26.1552516101606));
#32740=CARTESIAN_POINT('Ctrl Pts',(54.6971373768873,19.0271417623195,26.1596924072723));
#32741=CARTESIAN_POINT('Ctrl Pts',(54.7664272707845,19.0189721499517,26.1641332043841));
#32742=CARTESIAN_POINT('Ctrl Pts',(54.8356970030509,19.0108049147374,26.1685727093346));
#32743=CARTESIAN_POINT('Ctrl Pts',(54.9054171104519,19.0062726460233,26.1730122142852));
#32744=CARTESIAN_POINT('Ctrl Pts',(54.9751764736149,19.0054044632964,26.1774517192358));
#32745=CARTESIAN_POINT('Ctrl Pts',(55.0449391996525,19.0045362387172,26.1818914382006));
#32746=CARTESIAN_POINT('Ctrl Pts',(55.114740696023,19.0073324544971,26.1863311571655));
#32747=CARTESIAN_POINT('Ctrl Pts',(55.184169567371,19.0137701208182,26.1907708761303));
#32748=CARTESIAN_POINT('Ctrl Pts',(55.2536715568894,19.0202145668893,26.1952152707311));
#32749=CARTESIAN_POINT('Ctrl Pts',(55.3227996500613,19.0303080725577,26.1996596653319));
#32750=CARTESIAN_POINT('Ctrl Pts',(55.3911482661161,19.043975819062,26.2041040599327));
#32751=CARTESIAN_POINT('Ctrl Pts',(55.4595366871907,19.057651525419,26.20855104287));
#32752=CARTESIAN_POINT('Ctrl Pts',(55.5271442534278,19.0749054948847,26.2129980258072));
#32753=CARTESIAN_POINT('Ctrl Pts',(55.5935789799403,19.0956125506943,26.2174450087445));
#32754=CARTESIAN_POINT('Ctrl Pts',(55.6601287766886,19.1163554727733,26.2218996942103));
#32755=CARTESIAN_POINT('Ctrl Pts',(55.7255012199284,19.1405632503944,26.2263543796761));
#32756=CARTESIAN_POINT('Ctrl Pts',(55.7893235384156,19.1680622515481,26.2308090651418));
#32757=CARTESIAN_POINT('Ctrl Pts',(55.8227110405595,19.1824478611865,26.2331394540099));
#32758=CARTESIAN_POINT('Ctrl Pts',(55.8556747182556,19.197733397104,26.235469842878));
#32759=CARTESIAN_POINT('Ctrl Pts',(55.8881641213877,19.2138891255077,26.2378002317461));
#32760=CARTESIAN_POINT('Ctrl Pts',(55.9502810579926,19.2447774847976,26.2422557342678));
#32761=CARTESIAN_POINT('Ctrl Pts',(56.010906875813,19.2789708724776,26.2467112367896));
#32762=CARTESIAN_POINT('Ctrl Pts',(56.0696674020691,19.3163019239036,26.2511667393113));
#32763=CARTESIAN_POINT('Ctrl Pts',(56.128339977417,19.3535770993855,26.2556155729769));
#32764=CARTESIAN_POINT('Ctrl Pts',(56.1851523930307,19.3939803570567,26.2600644066425));
#32765=CARTESIAN_POINT('Ctrl Pts',(56.239753849348,19.4372978673059,26.2645132403082));
#32766=CARTESIAN_POINT('Ctrl Pts',(56.2942913182649,19.4805646138015,26.2689568603894));
#32767=CARTESIAN_POINT('Ctrl Pts',(56.3466225926864,19.5267385271277,26.2734004804706));
#32768=CARTESIAN_POINT('Ctrl Pts',(56.3964262326221,19.5755627990871,26.2778441005518));
#32769=CARTESIAN_POINT('Ctrl Pts',(56.4461986700604,19.6243564821331,26.2822849366589));
#32770=CARTESIAN_POINT('Ctrl Pts',(56.4934462660713,19.6757968880417,26.286725772766));
#32771=CARTESIAN_POINT('Ctrl Pts',(56.5378822056027,19.7295883013013,26.2911666088731));
#32772=CARTESIAN_POINT('Ctrl Pts',(56.5823053758943,19.7833642569052,26.2956061688487));
#32773=CARTESIAN_POINT('Ctrl Pts',(56.6239181823223,19.8394895017036,26.3000457288243));
#32774=CARTESIAN_POINT('Ctrl Pts',(56.6624732994973,19.8976343206729,26.3044852888));
#32775=CARTESIAN_POINT('Ctrl Pts',(56.701030412825,19.9557821500321,26.3089250786294));
#32776=CARTESIAN_POINT('Ctrl Pts',(56.7365292542682,20.0159493521424,26.3133648684588));
#32777=CARTESIAN_POINT('Ctrl Pts',(56.7687661404784,20.07777773677,26.3178046582882));
#32778=CARTESIAN_POINT('Ctrl Pts',(56.8010371446848,20.1396715576366,26.3222491469812));
#32779=CARTESIAN_POINT('Ctrl Pts',(56.8300390765395,20.2032296354737,26.3266936356742));
#32780=CARTESIAN_POINT('Ctrl Pts',(56.8556149590916,20.2680705730089,26.3311381243673));
#32781=CARTESIAN_POINT('Ctrl Pts',(56.8812058129006,20.3329494662366,26.3355852147137));
#32782=CARTESIAN_POINT('Ctrl Pts',(56.9033664702261,20.3991122498787,26.3400323050602));
#32783=CARTESIAN_POINT('Ctrl Pts',(56.9219896428977,20.4661616582768,26.3444793954066));
#32784=CARTESIAN_POINT('Ctrl Pts',(56.9406451526124,20.5333274904253,26.3489342076249));
#32785=CARTESIAN_POINT('Ctrl Pts',(56.9557508104675,20.601382542975,26.3533890198431));
#32786=CARTESIAN_POINT('Ctrl Pts',(56.9672504622757,20.6699194322955,26.3578438320614));
#32787=CARTESIAN_POINT('Ctrl Pts',(56.9732648610753,20.7057647075902,26.3601737301926));
#32788=CARTESIAN_POINT('Ctrl Pts',(56.9782937493876,20.7417416945414,26.3625036283239));
#32789=CARTESIAN_POINT('Ctrl Pts',(56.9823347679958,20.7777919216255,26.3648335264551));
#32790=CARTESIAN_POINT('Ctrl Pts',(56.9900512974037,20.84663165349,26.3692825847718));
#32791=CARTESIAN_POINT('Ctrl Pts',(56.9941931550845,20.9160117809082,26.3737316430885));
#32792=CARTESIAN_POINT('Ctrl Pts',(56.9946975038501,20.9855282815713,26.3781807014052));
#32793=CARTESIAN_POINT('Ctrl Pts',(56.9952010934743,21.0549401466075,26.3826230630384));
#32794=CARTESIAN_POINT('Ctrl Pts',(56.9920780367055,21.1244874908298,26.3870654246715));
#32795=CARTESIAN_POINT('Ctrl Pts',(56.9853171987077,21.1937606332963,26.3915077863047));
#32796=CARTESIAN_POINT('Ctrl Pts',(56.9785643105686,21.262952319633,26.3959449243032));
#32797=CARTESIAN_POINT('Ctrl Pts',(56.9681821837198,21.3318699584875,26.4003820623017));
#32798=CARTESIAN_POINT('Ctrl Pts',(56.9542117163663,21.4001051488253,26.4048192003002));
#32799=CARTESIAN_POINT('Ctrl Pts',(56.9402500230965,21.4682974843858,26.4092535515759));
#32800=CARTESIAN_POINT('Ctrl Pts',(56.9227045578704,21.5358077419548,26.4136879028516));
#32801=CARTESIAN_POINT('Ctrl Pts',(56.9016676942168,21.6022354550108,26.4181222541273));
#32802=CARTESIAN_POINT('Ctrl Pts',(56.8806368525617,21.6686441525142,26.4225553360286));
#32803=CARTESIAN_POINT('Ctrl Pts',(56.8561167444901,21.7339704530156,26.4269884179299));
#32804=CARTESIAN_POINT('Ctrl Pts',(56.8282497352792,21.7978285955966,26.4314214998312));
#32805=CARTESIAN_POINT('Ctrl Pts',(56.8003811789297,21.8616902834951,26.4358548278512));
#32806=CARTESIAN_POINT('Ctrl Pts',(56.7691655510603,21.924083202831,26.4402881558712));
#32807=CARTESIAN_POINT('Ctrl Pts',(56.734792814888,21.9846428042255,26.4447214838912));
#32808=CARTESIAN_POINT('Ctrl Pts',(56.7003831145663,22.0452675309024,26.4491595794746));
#32809=CARTESIAN_POINT('Ctrl Pts',(56.6628097724314,22.1040545770526,26.453597675058));
#32810=CARTESIAN_POINT('Ctrl Pts',(56.6223075820728,22.1606660465651,26.4580357706414));
#32811=CARTESIAN_POINT('Ctrl Pts',(56.5817813814332,22.217311076171,26.4624764971916));
#32812=CARTESIAN_POINT('Ctrl Pts',(56.5383231833967,22.2717775788078,26.4669172237419));
#32813=CARTESIAN_POINT('Ctrl Pts',(56.492208042573,22.3237608243866,26.4713579502922));
#32814=CARTESIAN_POINT('Ctrl Pts',(56.4460115334723,22.3758357922726,26.4758065123226));
#32815=CARTESIAN_POINT('Ctrl Pts',(56.3971490682769,22.4254184076707,26.480255074353));
#32816=CARTESIAN_POINT('Ctrl Pts',(56.3459319110476,22.4722414385296,26.4847036363833));
#32817=CARTESIAN_POINT('Ctrl Pts',(56.3184415326082,22.4973733065915,26.4870913646436));
#32818=CARTESIAN_POINT('Ctrl Pts',(56.2902733482307,22.5217108604893,26.4894790929038));
#32819=CARTESIAN_POINT('Ctrl Pts',(56.2614790088167,22.5452178722804,26.4918668211641));
#32820=CARTESIAN_POINT('Ctrl Pts',(56.2076670278864,22.5891486897944,26.4963291005642));
#32821=CARTESIAN_POINT('Ctrl Pts',(56.1514529776905,22.6303505042149,26.5007913799643));
#32822=CARTESIAN_POINT('Ctrl Pts',(56.0931444860463,22.6685510765711,26.5052536593645));
#32823=CARTESIAN_POINT('Ctrl Pts',(56.0349188706141,22.7066973529124,26.5097095963469));
#32824=CARTESIAN_POINT('Ctrl Pts',(55.974605124732,22.7418505863297,26.5141655333292));
#32825=CARTESIAN_POINT('Ctrl Pts',(55.9125436069833,22.7737789399624,26.5186214703116));
#32826=CARTESIAN_POINT('Ctrl Pts',(55.8505532127707,22.8056707031683,26.5230723007157));
#32827=CARTESIAN_POINT('Ctrl Pts',(55.7868194557606,22.8343447041128,26.5275231311199));
#32828=CARTESIAN_POINT('Ctrl Pts',(55.7217097632358,22.8596135566698,26.531973961524));
#32829=CARTESIAN_POINT('Ctrl Pts',(55.6566446468541,22.8848651093757,26.5364217447497));
#32830=CARTESIAN_POINT('Ctrl Pts',(55.5902059183537,22.9067159657897,26.5408695279754));
#32831=CARTESIAN_POINT('Ctrl Pts',(55.5227821248716,22.9250263407067,26.5453173112011));
#32832=CARTESIAN_POINT('Ctrl Pts',(55.4553656706266,22.9433347224968,26.5497646102752));
#32833=CARTESIAN_POINT('Ctrl Pts',(55.3869648314726,22.9581032488662,26.5542119093493));
#32834=CARTESIAN_POINT('Ctrl Pts',(55.3179831069597,22.9692420638886,26.5586592084234));
#32835=CARTESIAN_POINT('Ctrl Pts',(55.2670659071085,22.9774639121333,26.5619418752073));
#32836=CARTESIAN_POINT('Ctrl Pts',(55.2158325719834,22.9837092199195,26.5652245419912));
#32837=CARTESIAN_POINT('Ctrl Pts',(55.1644483516311,22.987959834138,26.5685072087751));
#32838=CARTESIAN_POINT('Ctrl Pts',(53.0052500783576,20.9994408866902,25.9772229232566));
#32839=CARTESIAN_POINT('Ctrl Pts',(53.0052168943837,21.1178314313542,25.969843828915));
#32840=CARTESIAN_POINT('Ctrl Pts',(53.0157237467158,21.2360116493196,25.9629670122793));
#32841=CARTESIAN_POINT('Ctrl Pts',(53.0553516448135,21.4566802688221,25.9499560771908));
#32842=CARTESIAN_POINT('Ctrl Pts',(53.0822955029543,21.5591258510858,25.9438400738149));
#32843=CARTESIAN_POINT('Ctrl Pts',(53.1364684850564,21.7139110708629,25.9340161240978));
#32844=CARTESIAN_POINT('Ctrl Pts',(53.1581014789727,21.7680023374757,25.9304683168702));
#32845=CARTESIAN_POINT('Ctrl Pts',(53.1879357837986,21.8340587940084,25.9259522809833));
#32846=CARTESIAN_POINT('Ctrl Pts',(53.1939427273713,21.8469875481996,25.9250594539539));
#32847=CARTESIAN_POINT('Ctrl Pts',(53.2037225485487,21.8674595027399,25.9236309183512));
#32848=CARTESIAN_POINT('Ctrl Pts',(53.2074056508731,21.8750452373608,25.9230983165377));
#32849=CARTESIAN_POINT('Ctrl Pts',(53.2144482759667,21.8893191886766,25.9220898341636));
#32850=CARTESIAN_POINT('Ctrl Pts',(53.2177975671835,21.8960123126986,25.921614316845));
#32851=CARTESIAN_POINT('Ctrl Pts',(53.2254481267374,21.9110883516037,25.9205371818387));
#32852=CARTESIAN_POINT('Ctrl Pts',(53.2297712575822,21.9194599120203,25.9199348046992));
#32853=CARTESIAN_POINT('Ctrl Pts',(53.2410333087816,21.9408945370596,25.9183813406902));
#32854=CARTESIAN_POINT('Ctrl Pts',(53.2480584153073,21.953911429301,25.9174272288736));
#32855=CARTESIAN_POINT('Ctrl Pts',(53.2958130772659,22.0400893611099,25.9110375353348));
#32856=CARTESIAN_POINT('Ctrl Pts',(53.3409644880603,22.110692046266,25.9054438100963));
#32857=CARTESIAN_POINT('Ctrl Pts',(53.4720711051744,22.2897958207562,25.8902834373139));
#32858=CARTESIAN_POINT('Ctrl Pts',(53.565104899898,22.3925557241909,25.8805199323808));
#32859=CARTESIAN_POINT('Ctrl Pts',(53.7002336413577,22.5137733837179,25.8680133646231));
#32860=CARTESIAN_POINT('Ctrl Pts',(53.7334004786974,22.5416317930085,25.8650600155022));
#32861=CARTESIAN_POINT('Ctrl Pts',(53.7804983565995,22.5786445834628,25.8610505370502));
#32862=CARTESIAN_POINT('Ctrl Pts',(53.7936747974107,22.5887361405098,25.8599479137013));
#32863=CARTESIAN_POINT('Ctrl Pts',(53.8137836131362,22.6037426216574,25.8582956442951));
#32864=CARTESIAN_POINT('Ctrl Pts',(53.8206236377335,22.6087793866882,25.8577388534942));
#32865=CARTESIAN_POINT('Ctrl Pts',(53.8318289221935,22.6169207103406,25.8568354870571));
#32866=CARTESIAN_POINT('Ctrl Pts',(53.8361748006287,22.6200515909781,25.856487250934));
#32867=CARTESIAN_POINT('Ctrl Pts',(53.8445488857416,22.6260334061561,25.8558203920828));
#32868=CARTESIAN_POINT('Ctrl Pts',(53.848575158784,22.6288869671294,25.855501597135));
#32869=CARTESIAN_POINT('Ctrl Pts',(53.8526311622533,22.6317390456855,25.8551823180915));
#32870=CARTESIAN_POINT('Ctrl Pts',(53.8526502916636,22.6317524964979,25.8551808123111));
#32871=CARTESIAN_POINT('Ctrl Pts',(53.8526886932853,22.631779497524,25.8551777895932));
#32872=CARTESIAN_POINT('Ctrl Pts',(53.8527079662335,22.6317930482481,25.8551762725984));
#32873=CARTESIAN_POINT('Ctrl Pts',(53.8527466579178,22.631820251175,25.8551732272186));
#32874=CARTESIAN_POINT('Ctrl Pts',(53.8527660765872,22.631833903323,25.8551716988395));
#32875=CARTESIAN_POINT('Ctrl Pts',(53.8528050628986,22.6318613113132,25.8551686304424));
#32876=CARTESIAN_POINT('Ctrl Pts',(53.8528246305032,22.6318750671212,25.855167090428));
#32877=CARTESIAN_POINT('Ctrl Pts',(53.8528639174295,22.6319026843368,25.8551639985463));
#32878=CARTESIAN_POINT('Ctrl Pts',(53.85288363709,22.6319165459744,25.855162446653));
#32879=CARTESIAN_POINT('Ctrl Pts',(53.8529232313168,22.631944377066,25.8551593307646));
#32880=CARTESIAN_POINT('Ctrl Pts',(53.852943105864,22.6319583464983,25.8551577667717));
#32881=CARTESIAN_POINT('Ctrl Pts',(53.8529830131672,22.6319863954753,25.8551546264264));
#32882=CARTESIAN_POINT('Ctrl Pts',(53.853003045852,22.6320004749616,25.8551530500802));
#32883=CARTESIAN_POINT('Ctrl Pts',(53.8530432727706,22.6320287463683,25.8551498847675));
#32884=CARTESIAN_POINT('Ctrl Pts',(53.8530634667852,22.6320429381259,25.8551482958191));
#32885=CARTESIAN_POINT('Ctrl Pts',(53.8564102213836,22.6343948457042,25.8548849670434));
#32886=CARTESIAN_POINT('Ctrl Pts',(53.8597438809084,22.6367223579057,25.8546239353481));
#32887=CARTESIAN_POINT('Ctrl Pts',(53.8673711701042,22.6420130054644,25.8540295736486));
#32888=CARTESIAN_POINT('Ctrl Pts',(53.8716693145569,22.6449694958284,25.8536966943792));
#32889=CARTESIAN_POINT('Ctrl Pts',(53.8842961897082,22.6535821503281,25.8527246308436));
#32890=CARTESIAN_POINT('Ctrl Pts',(53.8926563477196,22.6591922631115,25.8520884545075));
#32891=CARTESIAN_POINT('Ctrl Pts',(53.9556345587976,22.7007659572642,25.8473485004364));
#32892=CARTESIAN_POINT('Ctrl Pts',(54.0119551749834,22.734091500109,25.843402885128));
#32893=CARTESIAN_POINT('Ctrl Pts',(54.2231724667732,22.8454320255768,25.8292679487586));
#32894=CARTESIAN_POINT('Ctrl Pts',(54.3864080176575,22.9059352033324,25.819517022989));
#32895=CARTESIAN_POINT('Ctrl Pts',(54.6055034078439,22.9560265693039,25.8059888965488));
#32896=CARTESIAN_POINT('Ctrl Pts',(54.6560113960928,22.965537751984,25.8028475902073));
#32897=CARTESIAN_POINT('Ctrl Pts',(54.7203812286329,22.9751021933107,25.7987898157386));
#32898=CARTESIAN_POINT('Ctrl Pts',(54.7339554159447,22.9769763771404,25.7979311357743));
#32899=CARTESIAN_POINT('Ctrl Pts',(54.755789988905,22.9797621261863,25.7965446833748));
#32900=CARTESIAN_POINT('Ctrl Pts',(54.7640387927685,22.9807622045808,25.7960197047885));
#32901=CARTESIAN_POINT('Ctrl Pts',(54.7797491121106,22.9825673831855,25.7950174766231));
#32902=CARTESIAN_POINT('Ctrl Pts',(54.7872094100477,22.9833819714796,25.7945405346773));
#32903=CARTESIAN_POINT('Ctrl Pts',(54.8042491035216,22.9851452875238,25.7934487733241));
#32904=CARTESIAN_POINT('Ctrl Pts',(54.8138310678165,22.9860668038534,25.7928331102182));
#32905=CARTESIAN_POINT('Ctrl Pts',(54.8388317759815,22.9882886586392,25.7912220810086));
#32906=CARTESIAN_POINT('Ctrl Pts',(54.8542594048445,22.9894789878342,25.7902232993738));
#32907=CARTESIAN_POINT('Ctrl Pts',(54.9679368844923,22.9969205199647,25.7828282501797));
#32908=CARTESIAN_POINT('Ctrl Pts',(55.0664554171434,22.9960660352381,25.7762135204845));
#32909=CARTESIAN_POINT('Ctrl Pts',(55.1644486115703,22.9879598126352,25.7694502499567));
#32910=CARTESIAN_POINT('',(53.0052505021471,20.9985846147351,25.8209548813952));
#32911=CARTESIAN_POINT('Ctrl Pts',(55.1644483516311,22.987959834138,25.6104387285779));
#32912=CARTESIAN_POINT('Ctrl Pts',(55.1579505623676,22.9884973453669,25.6108573370408));
#32913=CARTESIAN_POINT('Ctrl Pts',(55.1514513148831,22.9890029011531,25.6112759455036));
#32914=CARTESIAN_POINT('Ctrl Pts',(55.1449509479891,22.9894765103356,25.6116945539665));
#32915=CARTESIAN_POINT('Ctrl Pts',(55.0757777214915,22.9945163912813,25.6161491483744));
#32916=CARTESIAN_POINT('Ctrl Pts',(55.0062047534237,22.9959542399979,25.6206037427823));
#32917=CARTESIAN_POINT('Ctrl Pts',(54.9366391221284,22.9937434543229,25.6250583371902));
#32918=CARTESIAN_POINT('Ctrl Pts',(54.8671778558954,22.9915359853544,25.6295062486426));
#32919=CARTESIAN_POINT('Ctrl Pts',(54.7977243897905,22.9856907617156,25.6339541600949));
#32920=CARTESIAN_POINT('Ctrl Pts',(54.7286893658636,22.9762130710793,25.6384020715472));
#32921=CARTESIAN_POINT('Ctrl Pts',(54.6597355119215,22.9667465241198,25.6428447532353));
#32922=CARTESIAN_POINT('Ctrl Pts',(54.5911996055224,22.9536560591925,25.6472874349233));
#32923=CARTESIAN_POINT('Ctrl Pts',(54.5234889208121,22.936998903952,25.6517301166113));
#32924=CARTESIAN_POINT('Ctrl Pts',(54.4558208106123,22.9203522222465,25.6561700048702));
#32925=CARTESIAN_POINT('Ctrl Pts',(54.3889773669066,22.9001434157983,25.6606098931291));
#32926=CARTESIAN_POINT('Ctrl Pts',(54.3233558891505,22.8764808311711,25.665049781388));
#32927=CARTESIAN_POINT('Ctrl Pts',(54.2577533901692,22.8528250901396,25.6694883855606));
#32928=CARTESIAN_POINT('Ctrl Pts',(54.1933726157074,22.8257177198506,25.6739269897332));
#32929=CARTESIAN_POINT('Ctrl Pts',(54.1305942010773,22.7953164398789,25.6783655939059));
#32930=CARTESIAN_POINT('Ctrl Pts',(54.0678126268779,22.7649136298439,25.6828044214686));
#32931=CARTESIAN_POINT('Ctrl Pts',(54.0066340120517,22.7312167964684,25.6872432490314));
#32932=CARTESIAN_POINT('Ctrl Pts',(53.9474159375527,22.6944303921914,25.6916820765941));
#32933=CARTESIAN_POINT('Ctrl Pts',(53.8881352163903,22.6576050716627,25.6961255999822));
#32934=CARTESIAN_POINT('Ctrl Pts',(53.8308195917504,22.6176839154238,25.7005691233703));
#32935=CARTESIAN_POINT('Ctrl Pts',(53.7757982674691,22.5749151344019,25.7050126467584));
#32936=CARTESIAN_POINT('Ctrl Pts',(53.7207447675428,22.5321213428386,25.7094587686524));
#32937=CARTESIAN_POINT('Ctrl Pts',(53.667988608646,22.4864769323068,25.7139048905463));
#32938=CARTESIAN_POINT('Ctrl Pts',(53.6178243107435,22.4382690730626,25.7183510124402));
#32939=CARTESIAN_POINT('Ctrl Pts',(53.5675728265466,22.3899774278434,25.72280486176));
#32940=CARTESIAN_POINT('Ctrl Pts',(53.5199225298912,22.339113797589,25.7272587110798));
#32941=CARTESIAN_POINT('Ctrl Pts',(53.4751290838272,22.2860000977879,25.7317125603996));
#32942=CARTESIAN_POINT('Ctrl Pts',(53.451610930245,22.2581135148387,25.7340509898248));
#32943=CARTESIAN_POINT('Ctrl Pts',(53.4288796015844,22.2296071906273,25.7363894192501));
#32944=CARTESIAN_POINT('Ctrl Pts',(53.4069672511891,22.200530809149,25.7387278486753));
#32945=CARTESIAN_POINT('Ctrl Pts',(53.3650931932104,22.1449664328104,25.7431965399643));
#32946=CARTESIAN_POINT('Ctrl Pts',(53.3260457686232,22.087097308453,25.7476652312533));
#32947=CARTESIAN_POINT('Ctrl Pts',(53.2900869513704,22.0272414169154,25.7521339225422));
#32948=CARTESIAN_POINT('Ctrl Pts',(53.2541821620369,21.9674754585159,25.7565958996478));
#32949=CARTESIAN_POINT('Ctrl Pts',(53.2213570194895,21.9057290678154,25.7610578767534));
#32950=CARTESIAN_POINT('Ctrl Pts',(53.1918320278417,21.8423515578194,25.765519853859));
#32951=CARTESIAN_POINT('Ctrl Pts',(53.1612641374524,21.7767353909527,25.770139439487));
#32952=CARTESIAN_POINT('Ctrl Pts',(53.1342342429006,21.7093711268831,25.7747590251151));
#32953=CARTESIAN_POINT('Ctrl Pts',(53.1109365293977,21.6406768034945,25.7793786107431));
#32954=CARTESIAN_POINT('Ctrl Pts',(53.0884794010214,21.5744609819775,25.7838315210032));
#32955=CARTESIAN_POINT('Ctrl Pts',(53.0694899032742,21.5070099421813,25.7882844312633));
#32956=CARTESIAN_POINT('Ctrl Pts',(53.0540931529504,21.438718708406,25.7927373415233));
#32957=CARTESIAN_POINT('Ctrl Pts',(53.0387034612457,21.3704587826533,25.7971882103528));
#32958=CARTESIAN_POINT('Ctrl Pts',(53.0269033496652,21.3013599010742,25.8016390791823));
#32959=CARTESIAN_POINT('Ctrl Pts',(53.0187674350936,21.2318298648886,25.8060899480117));
#32960=CARTESIAN_POINT('Ctrl Pts',(53.0106315145687,21.1622997778266,25.810540820098));
#32961=CARTESIAN_POINT('Ctrl Pts',(53.0061598545227,21.0923390168737,25.8149916921842));
#32962=CARTESIAN_POINT('Ctrl Pts',(53.0053753430082,21.02236157911,25.8194425642705));
#32963=CARTESIAN_POINT('Ctrl Pts',(53.0052864892454,21.014435935519,25.8199466699787));
#32964=CARTESIAN_POINT('Ctrl Pts',(53.0052448785904,21.0065100799959,25.820450775687));
#32965=CARTESIAN_POINT('Ctrl Pts',(53.0052505021471,20.9985846147351,25.8209548813952));
#32966=CARTESIAN_POINT('Ctrl Pts',(53.0073840846254,20.9985711856803,25.8209558328711));
#32967=CARTESIAN_POINT('Ctrl Pts',(53.005850056014,20.7640139712392,25.8358909363755));
#32968=CARTESIAN_POINT('Ctrl Pts',(53.1526219523583,19.8662942493302,25.8931704714496));
#32969=CARTESIAN_POINT('Ctrl Pts',(54.4827630389435,18.6996030104917,25.9927944380933));
#32970=CARTESIAN_POINT('Ctrl Pts',(56.6523991680059,19.3180745080547,26.1198277328024));
#32971=CARTESIAN_POINT('Ctrl Pts',(57.3092165337547,21.4764259740402,26.2468610275113));
#32972=CARTESIAN_POINT('Ctrl Pts',(56.1973412839694,22.7902337162283,26.3437709099491));
#32973=CARTESIAN_POINT('Ctrl Pts',(55.355531775765,22.972868043151,26.3983363608173));
#32974=CARTESIAN_POINT('Ctrl Pts',(55.164372889159,22.9868942741083,26.4105573801159));
#32975=CARTESIAN_POINT('Origin',(55.,21.,7.5));
#32976=CARTESIAN_POINT('',(52.5495004857877,21.0015429988506,7.95782749621206));
#32977=CARTESIAN_POINT('',(56.0772665381941,23.205491718641,7.70002485738492));
#32978=CARTESIAN_POINT('Ctrl Pts',(52.5465050492984,21.0015448849783,7.95782749621206));
#32979=CARTESIAN_POINT('Ctrl Pts',(52.5459443844546,21.0835112770769,7.95355359535896));
#32980=CARTESIAN_POINT('Ctrl Pts',(52.5868459923412,21.9769760028613,7.9069352629362));
#32981=CARTESIAN_POINT('Ctrl Pts',(53.6445503233722,23.5238918290192,7.82100104999381));
#32982=CARTESIAN_POINT('Ctrl Pts',(55.3982288713416,23.5326747575202,7.73934073790454));
#32983=CARTESIAN_POINT('Ctrl Pts',(56.0772665381941,23.205491718641,7.70002485738492));
#32984=CARTESIAN_POINT('',(53.9249115396487,23.2020751695661,7.7));
#32985=CARTESIAN_POINT('Origin',(55.,21.,7.7));
#32986=CARTESIAN_POINT('',(52.5493075430995,21.0024481883259,7.84217250378794));
#32987=CARTESIAN_POINT('Ctrl Pts',(53.9249115396487,23.2020751695661,7.7));
#32988=CARTESIAN_POINT('Ctrl Pts',(53.1925621422827,22.8445304331579,7.74234443156966));
#32989=CARTESIAN_POINT('Ctrl Pts',(52.5954013728997,22.0066433600949,7.78973526616564));
#32990=CARTESIAN_POINT('Ctrl Pts',(52.5465178413277,21.0991960387036,7.83712610076162));
#32991=CARTESIAN_POINT('Ctrl Pts',(52.5472668131576,21.0024502269706,7.84217250378794));
#32992=CARTESIAN_POINT('',(52.5495002427347,21.0010907074207,8.64217250373997));
#32993=CARTESIAN_POINT('Ctrl Pts',(52.5495012227464,21.0024479948441,7.84217250378794));
#32994=CARTESIAN_POINT('Ctrl Pts',(52.549422118682,20.9232630187398,7.84630671022257));
#32995=CARTESIAN_POINT('Ctrl Pts',(52.5531853006392,20.8439028055671,7.85044091665719));
#32996=CARTESIAN_POINT('Ctrl Pts',(52.5608151121287,20.7647823714506,7.85457512309182));
#32997=CARTESIAN_POINT('Ctrl Pts',(52.5684657252199,20.6854462266639,7.85872060085541));
#32998=CARTESIAN_POINT('Ctrl Pts',(52.5800041470203,20.6063516605387,7.862866078619));
#32999=CARTESIAN_POINT('Ctrl Pts',(52.5954022533773,20.5279195757744,7.86701155638259));
#33000=CARTESIAN_POINT('Ctrl Pts',(52.6107230540881,20.4498812565067,7.87113622192226));
#33001=CARTESIAN_POINT('Ctrl Pts',(52.6298648063395,20.3724992676908,7.87526088746194));
#33002=CARTESIAN_POINT('Ctrl Pts',(52.6527479093513,20.2961833527507,7.87938555300161));
#33003=CARTESIAN_POINT('Ctrl Pts',(52.6756198352345,20.2199047139087,7.8835082038706));
#33004=CARTESIAN_POINT('Ctrl Pts',(52.702229348838,20.144691581996,7.88763085473958));
#33005=CARTESIAN_POINT('Ctrl Pts',(52.7324463126037,20.0709410541977,7.89175350560856));
#33006=CARTESIAN_POINT('Ctrl Pts',(52.7626586529099,19.9972018108742,7.89587552567596));
#33007=CARTESIAN_POINT('Ctrl Pts',(52.796477162552,19.9249251776549,7.89999754574336));
#33008=CARTESIAN_POINT('Ctrl Pts',(52.8337232570441,19.8544890559543,7.90411956581076));
#33009=CARTESIAN_POINT('Ctrl Pts',(52.8713328823099,19.7833654608913,7.90828181777803));
#33010=CARTESIAN_POINT('Ctrl Pts',(52.9124371517035,19.7141189594769,7.91244406974529));
#33011=CARTESIAN_POINT('Ctrl Pts',(52.9568052803081,19.6471121305064,7.91660632171256));
#33012=CARTESIAN_POINT('Ctrl Pts',(53.0008010424648,19.5806676668117,7.92073364133022));
#33013=CARTESIAN_POINT('Ctrl Pts',(53.0480057411504,19.5164257812278,7.92486096094788));
#33014=CARTESIAN_POINT('Ctrl Pts',(53.0981527312477,19.4547080481865,7.92898828056554));
#33015=CARTESIAN_POINT('Ctrl Pts',(53.148936364137,19.3922067755989,7.93316799870761));
#33016=CARTESIAN_POINT('Ctrl Pts',(53.2027371757151,19.3322945787699,7.93734771684968));
#33017=CARTESIAN_POINT('Ctrl Pts',(53.2592401587572,19.2752665640406,7.94152743499175));
#33018=CARTESIAN_POINT('Ctrl Pts',(53.3157431417993,19.2182385493112,7.94570715313382));
#33019=CARTESIAN_POINT('Ctrl Pts',(53.3749478683294,19.1640950033771,7.94988687127589));
#33020=CARTESIAN_POINT('Ctrl Pts',(53.4365070735543,19.1130871459036,7.95406658941796));
#33021=CARTESIAN_POINT('Ctrl Pts',(53.4988934139118,19.0613939256025,7.95830246799464));
#33022=CARTESIAN_POINT('Ctrl Pts',(53.5639619311142,19.0127020952609,7.96253834657133));
#33023=CARTESIAN_POINT('Ctrl Pts',(53.6313921892293,18.9673015692687,7.96677422514801));
#33024=CARTESIAN_POINT('Ctrl Pts',(53.6987256512506,18.9219662157035,7.97100402312361));
#33025=CARTESIAN_POINT('Ctrl Pts',(53.7684137389447,18.8799130391827,7.97523382109922));
#33026=CARTESIAN_POINT('Ctrl Pts',(53.8401027657429,18.8413919633331,7.97946361907482));
#33027=CARTESIAN_POINT('Ctrl Pts',(53.911877321831,18.8028249295399,7.98369846345199));
#33028=CARTESIAN_POINT('Ctrl Pts',(53.985657222653,18.7677987134624,7.98793330782917));
#33029=CARTESIAN_POINT('Ctrl Pts',(54.0610580981629,18.7365207412095,7.99216815220634));
#33030=CARTESIAN_POINT('Ctrl Pts',(54.1362325494697,18.7053366947883,7.99639027960567));
#33031=CARTESIAN_POINT('Ctrl Pts',(54.2130178316279,18.6778786080508,8.000612407005));
#33032=CARTESIAN_POINT('Ctrl Pts',(54.2910097948158,18.6543054037337,8.00483453440433));
#33033=CARTESIAN_POINT('Ctrl Pts',(54.3689753494903,18.630740181435,8.00905523216779));
#33034=CARTESIAN_POINT('Ctrl Pts',(54.4481463301967,18.6110573631241,8.01327592993125));
#33035=CARTESIAN_POINT('Ctrl Pts',(54.5281021875988,18.5953664094813,8.01749662769471));
#33036=CARTESIAN_POINT('Ctrl Pts',(54.6080553125754,18.5796759920639,8.02171718121931));
#33037=CARTESIAN_POINT('Ctrl Pts',(54.6887928056727,18.5679772563439,8.02593773474391));
#33038=CARTESIAN_POINT('Ctrl Pts',(54.7698840529587,18.5603285260271,8.03015828826851));
#33039=CARTESIAN_POINT('Ctrl Pts',(54.8514475556846,18.5526352513899,8.03440342125671));
#33040=CARTESIAN_POINT('Ctrl Pts',(54.9333684758368,18.5490393671079,8.03864855424491));
#33041=CARTESIAN_POINT('Ctrl Pts',(55.0152053631808,18.5495471751265,8.04289368723312));
#33042=CARTESIAN_POINT('Ctrl Pts',(55.0966835794971,18.550052757547,8.04712021484346));
#33043=CARTESIAN_POINT('Ctrl Pts',(55.1780780341992,18.554626057633,8.0513467424538));
#33044=CARTESIAN_POINT('Ctrl Pts',(55.2589568338114,18.563221058811,8.05557327006414));
#33045=CARTESIAN_POINT('Ctrl Pts',(55.3403696819735,18.5718728134019,8.05982770574128));
#33046=CARTESIAN_POINT('Ctrl Pts',(55.4212595698563,18.5845994999149,8.06408214141841));
#33047=CARTESIAN_POINT('Ctrl Pts',(55.5011968970607,18.6013020364421,8.06833657709554));
#33048=CARTESIAN_POINT('Ctrl Pts',(55.581134224265,18.6180045729694,8.07259101277268));
#33049=CARTESIAN_POINT('Ctrl Pts',(55.660118549111,18.6386827804699,8.07684544844981));
#33050=CARTESIAN_POINT('Ctrl Pts',(55.7377380125337,18.66318745406,8.08109988412694));
#33051=CARTESIAN_POINT('Ctrl Pts',(55.8150631561192,18.687599210085,8.08533818770575));
#33052=CARTESIAN_POINT('Ctrl Pts',(55.8913147918291,18.7158971420639,8.08957649128455));
#33053=CARTESIAN_POINT('Ctrl Pts',(55.9660753525726,18.7479678814121,8.09381479486336));
#33054=CARTESIAN_POINT('Ctrl Pts',(56.0407314205827,18.7799937955317,8.09804717457105));
#33055=CARTESIAN_POINT('Ctrl Pts',(56.1139001310483,18.8157818615719,8.10227955427875));
#33056=CARTESIAN_POINT('Ctrl Pts',(56.1851796564499,18.8551691367529,8.10651193398644));
#33057=CARTESIAN_POINT('Ctrl Pts',(56.2564901504259,18.8945735243902,8.11074615252184));
#33058=CARTESIAN_POINT('Ctrl Pts',(56.3259093825185,18.9375800833776,8.11498037105723));
#33059=CARTESIAN_POINT('Ctrl Pts',(56.393055648912,18.9839776268518,8.11921458959263));
#33060=CARTESIAN_POINT('Ctrl Pts',(56.4600568949614,19.0302749624053,8.12343966319916));
#33061=CARTESIAN_POINT('Ctrl Pts',(56.5247945892955,19.0799484052375,8.12766473680569));
#33062=CARTESIAN_POINT('Ctrl Pts',(56.5869162490708,19.1327434379724,8.13188981041223));
#33063=CARTESIAN_POINT('Ctrl Pts',(56.6490188187896,19.1855222467338,8.13611358564884));
#33064=CARTESIAN_POINT('Ctrl Pts',(56.7085065979807,19.2414204405044,8.14033736088546));
#33065=CARTESIAN_POINT('Ctrl Pts',(56.7650598860866,19.3001429917408,8.14456113612207));
#33066=CARTESIAN_POINT('Ctrl Pts',(56.8216129508396,19.358865311057,8.14878489467721));
#33067=CARTESIAN_POINT('Ctrl Pts',(56.875231227228,19.4204116312256,8.15300865323234));
#33068=CARTESIAN_POINT('Ctrl Pts',(56.925632619831,19.4844508376688,8.15723241178748));
#33069=CARTESIAN_POINT('Ctrl Pts',(56.9762484696386,19.5487625300193,8.16147414237485));
#33070=CARTESIAN_POINT('Ctrl Pts',(57.0236196989971,19.6155880078858,8.16571587296222));
#33071=CARTESIAN_POINT('Ctrl Pts',(57.0675032574135,19.6845607081342,8.16995760354959));
#33072=CARTESIAN_POINT('Ctrl Pts',(57.1112656105149,19.7533429074715,8.17418761858083));
#33073=CARTESIAN_POINT('Ctrl Pts',(57.1515593395479,19.8242600576247,8.17841763361206));
#33074=CARTESIAN_POINT('Ctrl Pts',(57.188189379129,19.8969236241008,8.1826476486433));
#33075=CARTESIAN_POINT('Ctrl Pts',(57.2249715959299,19.9698890668417,8.18689523700874));
#33076=CARTESIAN_POINT('Ctrl Pts',(57.2580594326714,20.0446150352548,8.19114282537418));
#33077=CARTESIAN_POINT('Ctrl Pts',(57.2873047354194,20.1206893055762,8.19539041373961));
#33078=CARTESIAN_POINT('Ctrl Pts',(57.3165500381673,20.1967635758976,8.19963800210505));
#33079=CARTESIAN_POINT('Ctrl Pts',(57.3419527204521,20.2741856860223,8.20388559047049));
#33080=CARTESIAN_POINT('Ctrl Pts',(57.3634158799239,20.3525313686954,8.20813317883593));
#33081=CARTESIAN_POINT('Ctrl Pts',(57.384771145699,20.4304832134837,8.21235941489247));
#33082=CARTESIAN_POINT('Ctrl Pts',(57.4023066169024,20.5096422156924,8.216585650949));
#33083=CARTESIAN_POINT('Ctrl Pts',(57.4158893440379,20.5895990651033,8.22081188700554));
#33084=CARTESIAN_POINT('Ctrl Pts',(57.4294523479186,20.6694398104875,8.22503198621417));
#33085=CARTESIAN_POINT('Ctrl Pts',(57.4390739289214,20.7500756467217,8.22925208542279));
#33086=CARTESIAN_POINT('Ctrl Pts',(57.444671222262,20.8310832600236,8.23347218463142));
#33087=CARTESIAN_POINT('Ctrl Pts',(57.450291279378,20.9124203252604,8.23770944666948));
#33088=CARTESIAN_POINT('Ctrl Pts',(57.451854115726,20.9941317396832,8.24194670870754));
#33089=CARTESIAN_POINT('Ctrl Pts',(57.449328003338,21.0757798262361,8.24618397074561));
#33090=CARTESIAN_POINT('Ctrl Pts',(57.4468167335279,21.1569481763784,8.25039633607185));
#33091=CARTESIAN_POINT('Ctrl Pts',(57.4402644461553,21.2380534699362,8.2546087013981));
#33092=CARTESIAN_POINT('Ctrl Pts',(57.4296921086673,21.3186636268545,8.25882106672435));
#33093=CARTESIAN_POINT('Ctrl Pts',(57.4191233632417,21.3992463956271,8.26303200085533));
#33094=CARTESIAN_POINT('Ctrl Pts',(57.4045373404319,21.4793338999595,8.26724293498631));
#33095=CARTESIAN_POINT('Ctrl Pts',(57.3860068412155,21.5584994213718,8.27145386911729));
#33096=CARTESIAN_POINT('Ctrl Pts',(57.3674769238625,21.6376624569624,8.27566467102364));
#33097=CARTESIAN_POINT('Ctrl Pts',(57.3450028836156,21.7159031135083,8.27987547292999));
#33098=CARTESIAN_POINT('Ctrl Pts',(57.3187082729761,21.7928065305181,8.28408627483635));
#33099=CARTESIAN_POINT('Ctrl Pts',(57.2921271536252,21.8705478948629,8.28834295806206));
#33100=CARTESIAN_POINT('Ctrl Pts',(57.2616418377762,21.946922234669,8.29259964128777));
#33101=CARTESIAN_POINT('Ctrl Pts',(57.2274305212793,22.021520201892,8.29685632451349));
#33102=CARTESIAN_POINT('Ctrl Pts',(57.1935388937509,22.0954210855287,8.30107323099837));
#33103=CARTESIAN_POINT('Ctrl Pts',(57.1559908843481,22.16757826781,8.30529013748324));
#33104=CARTESIAN_POINT('Ctrl Pts',(57.1150058694171,22.2376188518002,8.30950704396812));
#33105=CARTESIAN_POINT('Ctrl Pts',(57.0734409565243,22.3086504416974,8.31378361556425));
#33106=CARTESIAN_POINT('Ctrl Pts',(57.0283412900334,22.3775046540551,8.31806018716038));
#33107=CARTESIAN_POINT('Ctrl Pts',(56.979979776086,22.4438248980712,8.32233675875652));
#33108=CARTESIAN_POINT('Ctrl Pts',(56.9316182621387,22.5101451420873,8.32661333035265));
#33109=CARTESIAN_POINT('Ctrl Pts',(56.8799952623039,22.573931076411,8.33088990194878));
#33110=CARTESIAN_POINT('Ctrl Pts',(56.8254230573828,22.6348641875016,8.33516647354491));
#33111=CARTESIAN_POINT('Ctrl Pts',(56.7714178366747,22.6951642270115,8.33939861320753));
#33112=CARTESIAN_POINT('Ctrl Pts',(56.7143205495057,22.7528981716161,8.34363075287014));
#33113=CARTESIAN_POINT('Ctrl Pts',(56.6544045728723,22.8077322144774,8.34786289253276));
#33114=CARTESIAN_POINT('Ctrl Pts',(56.5945744576463,22.8624876784961,8.35208896741119));
#33115=CARTESIAN_POINT('Ctrl Pts',(56.5319340152705,22.9143511832187,8.35631504228962));
#33116=CARTESIAN_POINT('Ctrl Pts',(56.4667954483278,22.9630235257798,8.36054111716805));
#33117=CARTESIAN_POINT('Ctrl Pts',(56.4015073358401,23.011807610621,8.36477689429662));
#33118=CARTESIAN_POINT('Ctrl Pts',(56.3337099361628,23.0573855189617,8.3690126714252));
#33119=CARTESIAN_POINT('Ctrl Pts',(56.2637532666214,23.0994946847048,8.37324844855378));
#33120=CARTESIAN_POINT('Ctrl Pts',(56.1940823883991,23.141431823476,8.37746692142328));
#33121=CARTESIAN_POINT('Ctrl Pts',(56.1222702433406,23.1799282560506,8.38168539429279));
#33122=CARTESIAN_POINT('Ctrl Pts',(56.048692467878,23.2147673371747,8.38590386716229));
#33123=CARTESIAN_POINT('Ctrl Pts',(55.9751390238809,23.2495948973484,8.39012094502323));
#33124=CARTESIAN_POINT('Ctrl Pts',(55.8998215286527,23.2807673092017,8.39433802288417));
#33125=CARTESIAN_POINT('Ctrl Pts',(55.8231391481475,23.3081144236773,8.3985551007451));
#33126=CARTESIAN_POINT('Ctrl Pts',(55.7464586626518,23.3354608623386,8.40277207439171));
#33127=CARTESIAN_POINT('Ctrl Pts',(55.6684137970017,23.3589820365267,8.40698904803832));
#33128=CARTESIAN_POINT('Ctrl Pts',(55.5894212164372,23.3785568901361,8.41120602168493));
#33129=CARTESIAN_POINT('Ctrl Pts',(55.5098197460523,23.3982826304364,8.41545550056567));
#33130=CARTESIAN_POINT('Ctrl Pts',(55.4292563476232,23.4140008172801,8.41970497944642));
#33131=CARTESIAN_POINT('Ctrl Pts',(55.3481684974395,23.4256399047243,8.42395445832717));
#33132=CARTESIAN_POINT('Ctrl Pts',(55.2675842978785,23.4372066997889,8.42817754296168));
#33133=CARTESIAN_POINT('Ctrl Pts',(55.186482615642,23.4447449399005,8.43240062759619));
#33134=CARTESIAN_POINT('Ctrl Pts',(55.105296749555,23.4482366806608,8.43662371223071));
#33135=CARTESIAN_POINT('Ctrl Pts',(55.0233497669174,23.4517611564502,8.44088638823457));
#33136=CARTESIAN_POINT('Ctrl Pts',(54.9413174975649,23.4511628672211,8.44514906423844));
#33137=CARTESIAN_POINT('Ctrl Pts',(54.8596423428699,23.4464770544775,8.4494117402423));
#33138=CARTESIAN_POINT('Ctrl Pts',(54.7779671881749,23.4417912417339,8.45367441624616));
#33139=CARTESIAN_POINT('Ctrl Pts',(54.6966496184479,23.4330180203266,8.45793709225003));
#33140=CARTESIAN_POINT('Ctrl Pts',(54.6161216682733,23.4202453752524,8.46219976825389));
#33141=CARTESIAN_POINT('Ctrl Pts',(54.536172916678,23.4075645976338,8.4664317848919));
#33142=CARTESIAN_POINT('Ctrl Pts',(54.4567039432331,23.3908944354196,8.47066380152991));
#33143=CARTESIAN_POINT('Ctrl Pts',(54.3781434386056,23.3702836680555,8.47489581816792));
#33144=CARTESIAN_POINT('Ctrl Pts',(54.2996952454205,23.3497023661974,8.4791217846425));
#33145=CARTESIAN_POINT('Ctrl Pts',(54.2221533873162,23.3251917649516,8.48334775111707));
#33146=CARTESIAN_POINT('Ctrl Pts',(54.1459385201734,23.2968520280324,8.48757371759165));
#33147=CARTESIAN_POINT('Ctrl Pts',(54.0695461971795,23.2684463059278,8.49180952364878));
#33148=CARTESIAN_POINT('Ctrl Pts',(53.9944875157402,23.236193678747,8.49604532970592));
#33149=CARTESIAN_POINT('Ctrl Pts',(53.9211728758895,23.2002459604061,8.50028113576305));
#33150=CARTESIAN_POINT('Ctrl Pts',(53.8481594848187,23.1644459507127,8.50449953695521));
#33151=CARTESIAN_POINT('Ctrl Pts',(53.7768762549463,23.1249813533276,8.50871793814738));
#33152=CARTESIAN_POINT('Ctrl Pts',(53.7077088482683,23.082050390638,8.51293633933954));
#33153=CARTESIAN_POINT('Ctrl Pts',(53.6385640843698,23.0391334819136,8.51715335958751));
#33154=CARTESIAN_POINT('Ctrl Pts',(53.571534162698,22.9927527062658,8.52137037983549));
#33155=CARTESIAN_POINT('Ctrl Pts',(53.5069784244422,22.9431512614614,8.52558740008347));
#33156=CARTESIAN_POINT('Ctrl Pts',(53.4424240640287,22.8935508753231,8.52980433032567));
#33157=CARTESIAN_POINT('Ctrl Pts',(53.38034414985,22.8407302407367,8.53402126056788));
#33158=CARTESIAN_POINT('Ctrl Pts',(53.3210662513842,22.7849738703295,8.53823819081009));
#33159=CARTESIAN_POINT('Ctrl Pts',(53.2613294942306,22.7287859006985,8.54248776348949));
#33160=CARTESIAN_POINT('Ctrl Pts',(53.204438681225,22.6696168635082,8.54673733616889));
#33161=CARTESIAN_POINT('Ctrl Pts',(53.1506910796216,22.6077956235196,8.55098690884829));
#33162=CARTESIAN_POINT('Ctrl Pts',(53.097278590771,22.5463598348871,8.55520998572217));
#33163=CARTESIAN_POINT('Ctrl Pts',(53.0469704719098,22.482305228034,8.55943306259605));
#33164=CARTESIAN_POINT('Ctrl Pts',(53.0000166551467,22.4159861829514,8.56365613946993));
#33165=CARTESIAN_POINT('Ctrl Pts',(52.9526209523248,22.3490430041248,8.56791896005209));
#33166=CARTESIAN_POINT('Ctrl Pts',(52.9086432780434,22.2797929500265,8.57218178063425));
#33167=CARTESIAN_POINT('Ctrl Pts',(52.8682938210179,22.2086269136873,8.57644460121641));
#33168=CARTESIAN_POINT('Ctrl Pts',(52.8279443639923,22.1374608773482,8.58070742179856));
#33169=CARTESIAN_POINT('Ctrl Pts',(52.7912232825414,22.0643793163929,8.58497024238072));
#33170=CARTESIAN_POINT('Ctrl Pts',(52.7582908137182,21.9897929956006,8.58923306296287));
#33171=CARTESIAN_POINT('Ctrl Pts',(52.7223976386163,21.9085011894265,8.59387912112526));
#33172=CARTESIAN_POINT('Ctrl Pts',(52.690888228178,21.8251600641242,8.59852517928764));
#33173=CARTESIAN_POINT('Ctrl Pts',(52.6639779262701,21.7402372059325,8.60317123745003));
#33174=CARTESIAN_POINT('Ctrl Pts',(52.6371426068781,21.6555509756903,8.60780434989627));
#33175=CARTESIAN_POINT('Ctrl Pts',(52.6148809649752,21.5692920834761,8.61243746234251));
#33176=CARTESIAN_POINT('Ctrl Pts',(52.5973604478986,21.481947541417,8.61707057478874));
#33177=CARTESIAN_POINT('Ctrl Pts',(52.5799228403308,21.3950163258056,8.62168176270639));
#33178=CARTESIAN_POINT('Ctrl Pts',(52.5671817197313,21.3070099981626,8.62629295062405));
#33179=CARTESIAN_POINT('Ctrl Pts',(52.5592542932496,21.2184276653249,8.6309041385417));
#33180=CARTESIAN_POINT('Ctrl Pts',(52.5527968728571,21.1462714159045,8.63466026027446));
#33181=CARTESIAN_POINT('Ctrl Pts',(52.5495325756989,21.0737333974149,8.63841638200722));
#33182=CARTESIAN_POINT('Ctrl Pts',(52.5495002427347,21.0010907074207,8.64217250373998));
#33183=CARTESIAN_POINT('',(52.5495009513656,20.9978406848801,9.44217250382341));
#33184=CARTESIAN_POINT('Ctrl Pts',(52.5495002427343,21.0010907064931,8.64217250378794));
#33185=CARTESIAN_POINT('Ctrl Pts',(52.5494633039605,20.9181000424275,8.64646368624462));
#33186=CARTESIAN_POINT('Ctrl Pts',(52.5536466572638,20.8351255123515,8.6507548687013));
#33187=CARTESIAN_POINT('Ctrl Pts',(52.562019055815,20.752615348514,8.65504605115798));
#33188=CARTESIAN_POINT('Ctrl Pts',(52.5703955399197,20.6700649214614,8.65933932762095));
#33189=CARTESIAN_POINT('Ctrl Pts',(52.5829650897535,20.587979750338,8.66363260408392));
#33190=CARTESIAN_POINT('Ctrl Pts',(52.5996448073063,20.5068010554466,8.6679258805469));
#33191=CARTESIAN_POINT('Ctrl Pts',(52.6163507093547,20.4254949229552,8.67222589676899));
#33192=CARTESIAN_POINT('Ctrl Pts',(52.6371795746486,20.3450985416839,8.67652591299108));
#33193=CARTESIAN_POINT('Ctrl Pts',(52.6619977589626,20.2660410291411,8.68082592921317));
#33194=CARTESIAN_POINT('Ctrl Pts',(52.6868364033699,20.1869183416418,8.68512949036554));
#33195=CARTESIAN_POINT('Ctrl Pts',(52.7156707645301,20.1091371353627,8.6894330515179));
#33196=CARTESIAN_POINT('Ctrl Pts',(52.7483187471438,20.0331071488858,8.69373661267027));
#33197=CARTESIAN_POINT('Ctrl Pts',(52.7810346800022,19.9569189212014,8.69804913082428));
#33198=CARTESIAN_POINT('Ctrl Pts',(52.8175798980594,19.8824895922892,8.70236164897828));
#33199=CARTESIAN_POINT('Ctrl Pts',(52.8577259346309,19.8102050265499,8.70667416713229));
#33200=CARTESIAN_POINT('Ctrl Pts',(52.8874910987764,19.756611642292,8.70987156397881));
#33201=CARTESIAN_POINT('Ctrl Pts',(52.9192346953156,19.7041967242502,8.71306896082534));
#33202=CARTESIAN_POINT('Ctrl Pts',(52.9528488415688,19.6531063945012,8.71626635767186));
#33203=CARTESIAN_POINT('Ctrl Pts',(52.9973333307875,19.5854941694044,8.72049774776804));
#33204=CARTESIAN_POINT('Ctrl Pts',(53.0452543647997,19.5199614369122,8.72472913786422));
#33205=CARTESIAN_POINT('Ctrl Pts',(53.0963910874101,19.456878696308,8.7289605279604));
#33206=CARTESIAN_POINT('Ctrl Pts',(53.1474545003025,19.3938863912592,8.73318585192644));
#33207=CARTESIAN_POINT('Ctrl Pts',(53.2017241556532,19.3333374604473,8.73741117589249));
#33208=CARTESIAN_POINT('Ctrl Pts',(53.2589356744407,19.2755739319226,8.74163649985853));
#33209=CARTESIAN_POINT('Ctrl Pts',(53.3162912702017,19.2176649362868,8.74587246454696));
#33210=CARTESIAN_POINT('Ctrl Pts',(53.3766033000059,19.1625557800068,8.75010842923539));
#33211=CARTESIAN_POINT('Ctrl Pts',(53.4395643536709,19.1105580602555,8.75434439392382));
#33212=CARTESIAN_POINT('Ctrl Pts',(53.5022542940963,19.0587842451155,8.75856211835035));
#33213=CARTESIAN_POINT('Ctrl Pts',(53.567570136524,19.0100954301877,8.76277984277687));
#33214=CARTESIAN_POINT('Ctrl Pts',(53.6351725367441,18.9647613787218,8.76699756720339));
#33215=CARTESIAN_POINT('Ctrl Pts',(53.7027526198979,18.9194422930416,8.77121389926462));
#33216=CARTESIAN_POINT('Ctrl Pts',(53.7726173760282,18.8774760302271,8.77543023132585));
#33217=CARTESIAN_POINT('Ctrl Pts',(53.8443973110694,18.8390898502398,8.77964656338708));
#33218=CARTESIAN_POINT('Ctrl Pts',(53.9161755347366,18.8007045854542,8.78386279492271));
#33219=CARTESIAN_POINT('Ctrl Pts',(53.9898684360633,18.7658994520344,8.78807902645834));
#33220=CARTESIAN_POINT('Ctrl Pts',(54.0650819530737,18.7348557450945,8.79229525799397));
#33221=CARTESIAN_POINT('Ctrl Pts',(54.1409043996592,18.7035607079147,8.79654562419287));
#33222=CARTESIAN_POINT('Ctrl Pts',(54.2182717590573,18.6760884781144,8.80079599039178));
#33223=CARTESIAN_POINT('Ctrl Pts',(54.2967615807266,18.6525746070092,8.80504635659068));
#33224=CARTESIAN_POINT('Ctrl Pts',(54.37473421048,18.6292156755356,8.80926871590933));
#33225=CARTESIAN_POINT('Ctrl Pts',(54.4538140839922,18.6097631464843,8.81349107522797));
#33226=CARTESIAN_POINT('Ctrl Pts',(54.5335754404777,18.5942987757674,8.81771343454661));
#33227=CARTESIAN_POINT('Ctrl Pts',(54.614130381755,18.5786805424539,8.82197780418565));
#33228=CARTESIAN_POINT('Ctrl Pts',(54.6953799615533,18.5671303369363,8.82624217382469));
#33229=CARTESIAN_POINT('Ctrl Pts',(54.7768808099841,18.5596786938916,8.83050654346373));
#33230=CARTESIAN_POINT('Ctrl Pts',(54.8583816584149,18.5522270508469,8.83477091310277));
#33231=CARTESIAN_POINT('Ctrl Pts',(54.9401332918113,18.5488739258957,8.8390352827418));
#33232=CARTESIAN_POINT('Ctrl Pts',(55.0216948174201,18.5495960363856,8.84329965238084));
#33233=CARTESIAN_POINT('Ctrl Pts',(55.1026239270472,18.5503125477378,8.84753095672971));
#33234=CARTESIAN_POINT('Ctrl Pts',(55.1836691614056,18.5550439596971,8.85176226107857));
#33235=CARTESIAN_POINT('Ctrl Pts',(55.2643994752335,18.5638055973514,8.85599356542743));
#33236=CARTESIAN_POINT('Ctrl Pts',(55.3450140680852,18.5725546758416,8.86021880451225));
#33237=CARTESIAN_POINT('Ctrl Pts',(55.425314178663,18.5853224566516,8.86444404359707));
#33238=CARTESIAN_POINT('Ctrl Pts',(55.5048690847785,18.6020722577119,8.86866928268188));
#33239=CARTESIAN_POINT('Ctrl Pts',(55.5846263394862,18.6188646620361,8.87290526869888));
#33240=CARTESIAN_POINT('Ctrl Pts',(55.6636341222117,18.639659358033,8.87714125471588));
#33241=CARTESIAN_POINT('Ctrl Pts',(55.7414639155221,18.6643669997239,8.88137724073288));
#33242=CARTESIAN_POINT('Ctrl Pts',(55.8189566713769,18.6889676463897,8.8855948830554));
#33243=CARTESIAN_POINT('Ctrl Pts',(55.8952811706885,18.7174472858186,8.88981252537793));
#33244=CARTESIAN_POINT('Ctrl Pts',(55.970026763108,18.7496670626651,8.89403016770045));
#33245=CARTESIAN_POINT('Ctrl Pts',(56.0447477017894,18.7818762122905,8.89824641889548));
#33246=CARTESIAN_POINT('Ctrl Pts',(56.1178903411844,18.817822865629,8.90246267009049));
#33247=CARTESIAN_POINT('Ctrl Pts',(56.1890633963501,18.8573197883351,8.90667892128552));
#33248=CARTESIAN_POINT('Ctrl Pts',(56.2602347774529,18.8968157820332,8.91089507331002));
#33249=CARTESIAN_POINT('Ctrl Pts',(56.3294362604733,18.9398616525109,8.91511122533452));
#33250=CARTESIAN_POINT('Ctrl Pts',(56.396301861268,18.9862245998574,8.91932737735901));
#33251=CARTESIAN_POINT('Ctrl Pts',(56.4637116313637,19.0329648606857,8.92357784150325));
#33252=CARTESIAN_POINT('Ctrl Pts',(56.528746921495,19.0830761764581,8.92782830564748));
#33253=CARTESIAN_POINT('Ctrl Pts',(56.5910647494884,19.1362770557469,8.93207876979172));
#33254=CARTESIAN_POINT('Ctrl Pts',(56.6529694163975,19.1891252184266,8.93630105377578));
#33255=CARTESIAN_POINT('Ctrl Pts',(56.7121922461191,19.2450217344356,8.94052333775984));
#33256=CARTESIAN_POINT('Ctrl Pts',(56.7684337064739,19.3036531970712,8.9447456217439));
#33257=CARTESIAN_POINT('Ctrl Pts',(56.8252382128131,19.3628716325446,8.94901017596822));
#33258=CARTESIAN_POINT('Ctrl Pts',(56.8790010037236,19.4248797141324,8.95327473019254));
#33259=CARTESIAN_POINT('Ctrl Pts',(56.9294559916372,19.4893214020397,8.95753928441686));
#33260=CARTESIAN_POINT('Ctrl Pts',(56.9799109795508,19.5537630899469,8.96180383864118));
#33261=CARTESIAN_POINT('Ctrl Pts',(57.0270579394572,19.6206379535486,8.9660683928655));
#33262=CARTESIAN_POINT('Ctrl Pts',(57.0706773591257,19.689562849884,8.97033294708982));
#33263=CARTESIAN_POINT('Ctrl Pts',(57.113954896683,19.7579475237852,8.97456407641275));
#33264=CARTESIAN_POINT('Ctrl Pts',(57.1539223370878,19.8286066506894,8.97879520573567));
#33265=CARTESIAN_POINT('Ctrl Pts',(57.1903330678364,19.90118641165,8.98302633505859));
#33266=CARTESIAN_POINT('Ctrl Pts',(57.2266915748675,19.9736620718456,8.98725139569523));
#33267=CARTESIAN_POINT('Ctrl Pts',(57.2595032972075,20.0480524828814,8.99147645633188));
#33268=CARTESIAN_POINT('Ctrl Pts',(57.2885654926829,20.1239758931964,8.99570151696852));
#33269=CARTESIAN_POINT('Ctrl Pts',(57.3177031426095,20.2000964241749,8.99993754716978));
#33270=CARTESIAN_POINT('Ctrl Pts',(57.3430715233589,20.2777575227887,9.00417357737104));
#33271=CARTESIAN_POINT('Ctrl Pts',(57.3645133119766,20.3565506643989,9.0084096075723));
#33272=CARTESIAN_POINT('Ctrl Pts',(57.3858610866042,20.4349983284111,9.01262706441161));
#33273=CARTESIAN_POINT('Ctrl Pts',(57.4033164994337,20.5145676796993,9.01684452125091));
#33274=CARTESIAN_POINT('Ctrl Pts',(57.416773540449,20.5948384221257,9.02106197809021));
#33275=CARTESIAN_POINT('Ctrl Pts',(57.4302261355124,20.6750826446162,9.0252780415615));
#33276=CARTESIAN_POINT('Ctrl Pts',(57.4396829052383,20.7560273398839,9.02949410503279));
#33277=CARTESIAN_POINT('Ctrl Pts',(57.4450889889884,20.8372422477182,9.03371016850408));
#33278=CARTESIAN_POINT('Ctrl Pts',(57.4504949430223,20.9184552068436,9.03792613081315));
#33279=CARTESIAN_POINT('Ctrl Pts',(57.4518503745512,20.9999379016525,9.04214209312222));
#33280=CARTESIAN_POINT('Ctrl Pts',(57.449152427175,21.0812566210407,9.04635805543129));
#33281=CARTESIAN_POINT('Ctrl Pts',(57.4464322612815,21.1632450278314,9.05060873762859));
#33282=CARTESIAN_POINT('Ctrl Pts',(57.4395916443802,21.2450662657673,9.05485941982588));
#33283=CARTESIAN_POINT('Ctrl Pts',(57.4286811215174,21.3262794201067,9.05911010202317));
#33284=CARTESIAN_POINT('Ctrl Pts',(57.4178439849383,21.4069463190864,9.06333219331112));
#33285=CARTESIAN_POINT('Ctrl Pts',(57.402991671001,21.4870128391883,9.06755428459908));
#33286=CARTESIAN_POINT('Ctrl Pts',(57.3842250890649,21.5660573952115,9.07177637588703));
#33287=CARTESIAN_POINT('Ctrl Pts',(57.3652678834759,21.6459048551444,9.07604135353899));
#33288=CARTESIAN_POINT('Ctrl Pts',(57.3423165757122,21.7247090052469,9.08030633119095));
#33289=CARTESIAN_POINT('Ctrl Pts',(57.3155261021999,21.8020530655954,9.08457130884292));
#33290=CARTESIAN_POINT('Ctrl Pts',(57.2887356286876,21.8793971259439,9.08883628649488));
#33291=CARTESIAN_POINT('Ctrl Pts',(57.2581062294484,21.9552806736383,9.09310126414684));
#33292=CARTESIAN_POINT('Ctrl Pts',(57.2238408955478,22.0293113820847,9.0973662417988));
#33293=CARTESIAN_POINT('Ctrl Pts',(57.1898465433513,22.1027566309648,9.10159749058312));
#33294=CARTESIAN_POINT('Ctrl Pts',(57.1521461140952,22.1746536964031,9.10582873936745));
#33295=CARTESIAN_POINT('Ctrl Pts',(57.1109032105033,22.2446035054936,9.11005998815177));
#33296=CARTESIAN_POINT('Ctrl Pts',(57.069719443434,22.3144530163967,9.11428516992049));
#33297=CARTESIAN_POINT('Ctrl Pts',(57.0250035242599,22.3823604191509,9.1185103516892));
#33298=CARTESIAN_POINT('Ctrl Pts',(56.9769663118386,22.4479483595264,9.12273553345791));
#33299=CARTESIAN_POINT('Ctrl Pts',(56.9288061026312,22.513704234415,9.12697153358499));
#33300=CARTESIAN_POINT('Ctrl Pts',(56.8773077746333,22.5771283284492,9.13120753371207));
#33301=CARTESIAN_POINT('Ctrl Pts',(56.8227292797739,22.6378669734307,9.13544353383915));
#33302=CARTESIAN_POINT('Ctrl Pts',(56.7683881032024,22.6983415145509,9.13966111498454));
#33303=CARTESIAN_POINT('Ctrl Pts',(56.7109937969682,22.756153558255,9.14387869612993));
#33304=CARTESIAN_POINT('Ctrl Pts',(56.6508420524642,22.8109861313151,9.14809627727531));
#33305=CARTESIAN_POINT('Ctrl Pts',(56.5907101672733,22.8658006012057,9.15231246597124));
#33306=CARTESIAN_POINT('Ctrl Pts',(56.5278229950112,22.9176372409537,9.15652865466716));
#33307=CARTESIAN_POINT('Ctrl Pts',(56.4625123322713,22.9662166533611,9.16074484336308));
#33308=CARTESIAN_POINT('Ctrl Pts',(56.3972032249617,23.0147949088074,9.1649609316468));
#33309=CARTESIAN_POINT('Ctrl Pts',(56.3294711156287,23.0601158145682,9.16917701993052));
#33310=CARTESIAN_POINT('Ctrl Pts',(56.2596788971637,23.1019417989184,9.17339310821423));
#33311=CARTESIAN_POINT('Ctrl Pts',(56.1893164437269,23.1441095210659,9.17764364390536));
#33312=CARTESIAN_POINT('Ctrl Pts',(56.1168604651603,23.1827246880677,9.18189417959649));
#33313=CARTESIAN_POINT('Ctrl Pts',(56.0427087845393,23.2175907288417,9.18614471528762));
#33314=CARTESIAN_POINT('Ctrl Pts',(55.9690511163499,23.2522244854997,9.19036693311118));
#33315=CARTESIAN_POINT('Ctrl Pts',(55.8937207293832,23.2831587976864,9.19458915093473));
#33316=CARTESIAN_POINT('Ctrl Pts',(55.8171265895045,23.3102498537441,9.19881136875829));
#33317=CARTESIAN_POINT('Ctrl Pts',(55.739761889176,23.3376134541032,9.2030760633832));
#33318=CARTESIAN_POINT('Ctrl Pts',(55.6611083311514,23.3610558966466,9.20734075800812));
#33319=CARTESIAN_POINT('Ctrl Pts',(55.5816000133454,23.3804813955326,9.21160545263304));
#33320=CARTESIAN_POINT('Ctrl Pts',(55.5020916955393,23.3999068944186,9.21587014725795));
#33321=CARTESIAN_POINT('Ctrl Pts',(55.421729103167,23.4153154220188,9.22013484188287));
#33322=CARTESIAN_POINT('Ctrl Pts',(55.3409518431461,23.4266648080555,9.22439953650778));
#33323=CARTESIAN_POINT('Ctrl Pts',(55.260808466249,23.437925132093,9.22863076480876));
#33324=CARTESIAN_POINT('Ctrl Pts',(55.1799564086001,23.4452320607928,9.23286199310974));
#33325=CARTESIAN_POINT('Ctrl Pts',(55.098819690326,23.4485066711781,9.23709322141072));
#33326=CARTESIAN_POINT('Ctrl Pts',(55.0177993118685,23.4517765861853,9.24131838266418));
#33327=CARTESIAN_POINT('Ctrl Pts',(54.9364955440597,23.4510256474488,9.24554354391765));
#33328=CARTESIAN_POINT('Ctrl Pts',(54.8553397818511,23.4462264145588,9.24976870517112));
#33329=CARTESIAN_POINT('Ctrl Pts',(54.7739757310339,23.4414148642989,9.25400471042302));
#33330=CARTESIAN_POINT('Ctrl Pts',(54.6927609148197,23.4325341538951,9.25824071567493));
#33331=CARTESIAN_POINT('Ctrl Pts',(54.6121323693784,23.419609255875,9.26247672092683));
#33332=CARTESIAN_POINT('Ctrl Pts',(54.5318548992027,23.406740635839,9.26669428163579));
#33333=CARTESIAN_POINT('Ctrl Pts',(54.4521590681906,23.3898630393969,9.27091184234475));
#33334=CARTESIAN_POINT('Ctrl Pts',(54.373471535494,23.3690530456627,9.27512940305371));
#33335=CARTESIAN_POINT('Ctrl Pts',(54.2948099804698,23.3482499220791,9.27934557138949));
#33336=CARTESIAN_POINT('Ctrl Pts',(54.217156511829,23.3235170980812,9.28356173972527));
#33337=CARTESIAN_POINT('Ctrl Pts',(54.1409257931169,23.2949818642134,9.28777790806105));
#33338=CARTESIAN_POINT('Ctrl Pts',(54.064696888021,23.2664473092315,9.29199397608936));
#33339=CARTESIAN_POINT('Ctrl Pts',(53.9898911005788,23.2341106882708,9.29621004411767));
#33340=CARTESIAN_POINT('Ctrl Pts',(53.9169048121914,23.1981480987745,9.30042611214597));
#33341=CARTESIAN_POINT('Ctrl Pts',(53.8433214187941,23.1618912972716,9.30467667206854));
#33342=CARTESIAN_POINT('Ctrl Pts',(53.7715878700404,23.1219491226593,9.3089272319911));
#33343=CARTESIAN_POINT('Ctrl Pts',(53.7020850487283,23.0785492607262,9.31317779191367));
#33344=CARTESIAN_POINT('Ctrl Pts',(53.6330459854035,23.0354389846292,9.31739998994994));
#33345=CARTESIAN_POINT('Ctrl Pts',(53.5662083210735,22.9889173426043,9.32162218798621));
#33346=CARTESIAN_POINT('Ctrl Pts',(53.5019146379084,22.9392499833407,9.32584438602249));
#33347=CARTESIAN_POINT('Ctrl Pts',(53.43697313217,22.8890821762118,9.3301091268882));
#33348=CARTESIAN_POINT('Ctrl Pts',(53.3746275312274,22.8357052187734,9.33437386775391));
#33349=CARTESIAN_POINT('Ctrl Pts',(53.3151937054493,22.7794319317811,9.33863860861962));
#33350=CARTESIAN_POINT('Ctrl Pts',(53.2557598796711,22.7231586447889,9.34290334948534));
#33351=CARTESIAN_POINT('Ctrl Pts',(53.1992381153865,22.663989420995,9.34716809035105));
#33352=CARTESIAN_POINT('Ctrl Pts',(53.1459022174421,22.6022707832055,9.35143283121676));
#33353=CARTESIAN_POINT('Ctrl Pts',(53.0934104411699,22.5415289366906,9.35563007607454));
#33354=CARTESIAN_POINT('Ctrl Pts',(53.0437996775331,22.4780807482771,9.35982732093232));
#33355=CARTESIAN_POINT('Ctrl Pts',(52.9973646295413,22.4122329209403,9.36402456579009));
#33356=CARTESIAN_POINT('Ctrl Pts',(52.9509918326174,22.346473369545,9.36821618379948));
#33357=CARTESIAN_POINT('Ctrl Pts',(52.9077865744021,22.2783209440572,9.37240780180887));
#33358=CARTESIAN_POINT('Ctrl Pts',(52.8680047304671,22.2081168903254,9.37659941981826));
#33359=CARTESIAN_POINT('Ctrl Pts',(52.8282635509888,22.1379845982169,9.38078675321307));
#33360=CARTESIAN_POINT('Ctrl Pts',(52.7919390721948,22.065805249046,9.38497408660787));
#33361=CARTESIAN_POINT('Ctrl Pts',(52.759244187876,21.9919494142508,9.38916142000267));
#33362=CARTESIAN_POINT('Ctrl Pts',(52.7265723169706,21.9181455654128,9.39334580599953));
#33363=CARTESIAN_POINT('Ctrl Pts',(52.6975251579487,21.842668005412,9.3975301919964));
#33364=CARTESIAN_POINT('Ctrl Pts',(52.6722691891804,21.7659109101985,9.40171457799326));
#33365=CARTESIAN_POINT('Ctrl Pts',(52.6470180173743,21.689168393752,9.40589816923378));
#33366=CARTESIAN_POINT('Ctrl Pts',(52.6255567618322,21.6111472707469,9.4100817604743));
#33367=CARTESIAN_POINT('Ctrl Pts',(52.6080028976971,21.5322594410385,9.41426535171482));
#33368=CARTESIAN_POINT('Ctrl Pts',(52.5904506362686,21.4533788139631,9.41844856098422));
#33369=CARTESIAN_POINT('Ctrl Pts',(52.5768051527144,21.3736321005787,9.42263177025363));
#33370=CARTESIAN_POINT('Ctrl Pts',(52.5671329872607,21.2934422401849,9.42681497952303));
#33371=CARTESIAN_POINT('Ctrl Pts',(52.5574557755994,21.2132105427607,9.43100037127602));
#33372=CARTESIAN_POINT('Ctrl Pts',(52.5517560652642,21.1325357075258,9.435185763029));
#33373=CARTESIAN_POINT('Ctrl Pts',(52.5500485115664,21.0518454850662,9.43937115478199));
#33374=CARTESIAN_POINT('Ctrl Pts',(52.5496675473193,21.0338430703327,9.44030493778397));
#33375=CARTESIAN_POINT('Ctrl Pts',(52.5494850909459,21.0158398899857,9.44123872078596));
#33376=CARTESIAN_POINT('Ctrl Pts',(52.549500951365,20.9978406855638,9.44217250378794));
#33377=CARTESIAN_POINT('',(52.5495000065655,21.0001793810522,10.2421725038327));
#33378=CARTESIAN_POINT('Ctrl Pts',(52.5495009513656,20.9978406848801,9.44217250382341));
#33379=CARTESIAN_POINT('Ctrl Pts',(52.5495886065576,20.8983651786185,9.44733320619029));
#33380=CARTESIAN_POINT('Ctrl Pts',(52.5557371744544,20.7991567821712,9.45249390855717));
#33381=CARTESIAN_POINT('Ctrl Pts',(52.5678270520411,20.7008595627187,9.45765461092406));
#33382=CARTESIAN_POINT('Ctrl Pts',(52.580109737472,20.6009947115979,9.46289761552193));
#33383=CARTESIAN_POINT('Ctrl Pts',(52.5985246902829,20.5020702618922,9.46814062011981));
#33384=CARTESIAN_POINT('Ctrl Pts',(52.6228978721534,20.4047389448427,9.47338362471768));
#33385=CARTESIAN_POINT('Ctrl Pts',(52.6307735551381,20.3732883693027,9.47507779178704));
#33386=CARTESIAN_POINT('Ctrl Pts',(52.6392709797487,20.3420039670236,9.47677195885639));
#33387=CARTESIAN_POINT('Ctrl Pts',(52.6483832195965,20.3109072862634,9.47846612592574));
#33388=CARTESIAN_POINT('Ctrl Pts',(52.6711412674524,20.2332425451333,9.4826973507271));
#33389=CARTESIAN_POINT('Ctrl Pts',(52.6977935641045,20.1565608183473,9.48692857552846));
#33390=CARTESIAN_POINT('Ctrl Pts',(52.7282373323909,20.0812809830761,9.49115980032983));
#33391=CARTESIAN_POINT('Ctrl Pts',(52.7586374468349,20.0061090928542,9.49538495790524));
#33392=CARTESIAN_POINT('Ctrl Pts',(52.7928180624719,19.9323355291198,9.49961011548066));
#33393=CARTESIAN_POINT('Ctrl Pts',(52.830626453431,19.8603646787473,9.50383527305608));
#33394=CARTESIAN_POINT('Ctrl Pts',(52.8685319217436,19.7882090350127,9.50807127920519));
#33395=CARTESIAN_POINT('Ctrl Pts',(52.9100836797597,19.7178658249795,9.5123072853543));
#33396=CARTESIAN_POINT('Ctrl Pts',(52.9550789186719,19.6497229835549,9.51654329150341));
#33397=CARTESIAN_POINT('Ctrl Pts',(52.999878185035,19.5818769318943,9.52076084812446));
#33398=CARTESIAN_POINT('Ctrl Pts',(53.0480907483382,19.5162125167468,9.52497840474551));
#33399=CARTESIAN_POINT('Ctrl Pts',(53.0994710522777,19.4530869549747,9.52919596136656));
#33400=CARTESIAN_POINT('Ctrl Pts',(53.150834391881,19.3899822354937,9.53341212546864));
#33401=CARTESIAN_POINT('Ctrl Pts',(53.2053631018543,19.3294150650192,9.53762828957072));
#33402=CARTESIAN_POINT('Ctrl Pts',(53.262770360231,19.2717108376466,9.54184445367279));
#33403=CARTESIAN_POINT('Ctrl Pts',(53.3201762509071,19.2140079850499,9.54606051732676));
#33404=CARTESIAN_POINT('Ctrl Pts',(53.3804602249465,19.159168268753,9.55027658098073));
#33405=CARTESIAN_POINT('Ctrl Pts',(53.4432985200949,19.107480316493,9.5544926446347));
#33406=CARTESIAN_POINT('Ctrl Pts',(53.5066510353778,19.0553693899034,9.55874320930137));
#33407=CARTESIAN_POINT('Ctrl Pts',(53.5725995095767,19.0064623657227,9.56299377396804));
#33408=CARTESIAN_POINT('Ctrl Pts',(53.6407795565335,18.9610124973255,9.56724433863471));
#33409=CARTESIAN_POINT('Ctrl Pts',(53.7085045211023,18.9158659938505,9.57146653199327));
#33410=CARTESIAN_POINT('Ctrl Pts',(53.7784309240605,18.8741308231446,9.57568872535183));
#33411=CARTESIAN_POINT('Ctrl Pts',(53.8501755696681,18.8360096974774,9.5799109187104));
#33412=CARTESIAN_POINT('Ctrl Pts',(53.9226433546275,18.7975043356644,9.58417566903112));
#33413=CARTESIAN_POINT('Ctrl Pts',(53.9969658019666,18.7626864893385,9.58844041935184));
#33414=CARTESIAN_POINT('Ctrl Pts',(54.0727277340705,18.7317150983975,9.59270516967257));
#33415=CARTESIAN_POINT('Ctrl Pts',(54.1484896661744,18.7007437074564,9.59696991999329));
#33416=CARTESIAN_POINT('Ctrl Pts',(54.2256906071985,18.6736188709929,9.60123467031401));
#33417=CARTESIAN_POINT('Ctrl Pts',(54.3039020009561,18.6504473136941,9.60549942063474));
#33418=CARTESIAN_POINT('Ctrl Pts',(54.3814984979045,18.6274579308327,9.60973064155215));
#33419=CARTESIAN_POINT('Ctrl Pts',(54.4603805779328,18.608273637356,9.61396186246957));
#33420=CARTESIAN_POINT('Ctrl Pts',(54.5401405584574,18.5930352009171,9.61819308338698));
#33421=CARTESIAN_POINT('Ctrl Pts',(54.6197861692198,18.5778186152402,9.62241823705454));
#33422=CARTESIAN_POINT('Ctrl Pts',(54.7003067275132,18.5665367357808,9.6266433907221));
#33423=CARTESIAN_POINT('Ctrl Pts',(54.7812796426594,18.5592805045879,9.63086854438966));
#33424=CARTESIAN_POINT('Ctrl Pts',(54.8624605587454,18.552005633793,9.63510455151275));
#33425=CARTESIAN_POINT('Ctrl Pts',(54.9440957042696,18.5487772476019,9.63934055863584));
#33426=CARTESIAN_POINT('Ctrl Pts',(55.0257491544411,18.5496352861165,9.64357656575892));
#33427=CARTESIAN_POINT('Ctrl Pts',(55.1070468760822,18.5504895865308,9.64779411844333));
#33428=CARTESIAN_POINT('Ctrl Pts',(55.188362275281,18.5553947836171,9.65201167112774));
#33429=CARTESIAN_POINT('Ctrl Pts',(55.2692620604703,18.5643382433533,9.65622922381215));
#33430=CARTESIAN_POINT('Ctrl Pts',(55.3501351347561,18.573278750203,9.66044538397565));
#33431=CARTESIAN_POINT('Ctrl Pts',(55.4305924057973,18.5862548208621,9.66466154413915));
#33432=CARTESIAN_POINT('Ctrl Pts',(55.5102049454675,18.6032018934377,9.66887770430264));
#33433=CARTESIAN_POINT('Ctrl Pts',(55.5898155884708,18.620148562271,9.67309376402152));
#33434=CARTESIAN_POINT('Ctrl Pts',(55.6685810856139,18.6410659470403,9.67730982374039));
#33435=CARTESIAN_POINT('Ctrl Pts',(55.7460833713172,18.6658385117897,9.68152588345927));
#33436=CARTESIAN_POINT('Ctrl Pts',(55.8242200344799,18.6908138467742,9.68577645278297));
#33437=CARTESIAN_POINT('Ctrl Pts',(55.9010722494636,18.7197076336754,9.69002702210667));
#33438=CARTESIAN_POINT('Ctrl Pts',(55.9762296438501,18.7523510210737,9.69427759143038));
#33439=CARTESIAN_POINT('Ctrl Pts',(56.0508852335377,18.7847764577925,9.69849978090301));
#33440=CARTESIAN_POINT('Ctrl Pts',(56.1238681720284,18.8209013137562,9.70272197037564));
#33441=CARTESIAN_POINT('Ctrl Pts',(56.194800356877,18.8605135295575,9.70694415984827));
#33442=CARTESIAN_POINT('Ctrl Pts',(56.2664477079404,18.9005251313145,9.71120891909751));
#33443=CARTESIAN_POINT('Ctrl Pts',(56.3360023079129,18.9440945526786,9.71547367834675));
#33444=CARTESIAN_POINT('Ctrl Pts',(56.4031054890392,18.9909591251973,9.71973843759599));
#33445=CARTESIAN_POINT('Ctrl Pts',(56.4702086701655,19.037823697716,9.72400319684523));
#33446=CARTESIAN_POINT('Ctrl Pts',(56.5348600911658,19.0879830752915,9.72826795609447));
#33447=CARTESIAN_POINT('Ctrl Pts',(56.5967377036965,19.1411350356752,9.73253271534371));
#33448=CARTESIAN_POINT('Ctrl Pts',(56.6581286759659,19.1938689792217,9.73676393413348));
#33449=CARTESIAN_POINT('Ctrl Pts',(56.7170195532931,19.2497463153063,9.74099515292325));
#33450=CARTESIAN_POINT('Ctrl Pts',(56.7730710033144,19.308500822582,9.74522637171302));
#33451=CARTESIAN_POINT('Ctrl Pts',(56.8290420791093,19.3671710796186,9.74945152320325));
#33452=CARTESIAN_POINT('Ctrl Pts',(56.8821814958066,19.4287099803759,9.75367667469348));
#33453=CARTESIAN_POINT('Ctrl Pts',(56.9321837027249,19.4928117606204,9.75790182618371));
#33454=CARTESIAN_POINT('Ctrl Pts',(56.9823143861035,19.5570782449916,9.76213783384492));
#33455=CARTESIAN_POINT('Ctrl Pts',(57.0292913635986,19.6239204834868,9.76637384150613));
#33456=CARTESIAN_POINT('Ctrl Pts',(57.0728447075579,19.6929938529796,9.77060984916733));
#33457=CARTESIAN_POINT('Ctrl Pts',(57.1162082795827,19.7617662539184,9.77482739956911));
#33458=CARTESIAN_POINT('Ctrl Pts',(57.1561777345011,19.8327499918985,9.77904494997088));
#33459=CARTESIAN_POINT('Ctrl Pts',(57.1925287476046,19.9055741501008,9.78326250037265));
#33460=CARTESIAN_POINT('Ctrl Pts',(57.2288677582892,19.97837426314,9.78747865821884));
#33461=CARTESIAN_POINT('Ctrl Pts',(57.2615904922698,20.0530131739984,9.79169481606503));
#33462=CARTESIAN_POINT('Ctrl Pts',(57.2905186224002,20.1290954757048,9.79591097391123));
#33463=CARTESIAN_POINT('Ctrl Pts',(57.3194460631376,20.2051759642761,9.80012703128118));
#33464=CARTESIAN_POINT('Ctrl Pts',(57.3445789156268,20.2826993403403,9.80434308865113));
#33465=CARTESIAN_POINT('Ctrl Pts',(57.3657875728272,20.361251684733,9.80855914602108));
#33466=CARTESIAN_POINT('Ctrl Pts',(57.3871698540912,20.440447095639,9.81280971802372));
#33467=CARTESIAN_POINT('Ctrl Pts',(57.4045632523075,20.5206879409317,9.81706029002635));
#33468=CARTESIAN_POINT('Ctrl Pts',(57.417887129105,20.6015378551122,9.82131086202899));
#33469=CARTESIAN_POINT('Ctrl Pts',(57.4311220302655,20.6818478609222,9.82553304909854));
#33470=CARTESIAN_POINT('Ctrl Pts',(57.4403416045215,20.7627583522951,9.82975523616809));
#33471=CARTESIAN_POINT('Ctrl Pts',(57.4455190161863,20.8438366513195,9.83397742323764));
#33472=CARTESIAN_POINT('Ctrl Pts',(57.4507486379313,20.925732560526,9.83824218770682));
#33473=CARTESIAN_POINT('Ctrl Pts',(57.4518541076335,21.0077991950925,9.84250695217599));
#33474=CARTESIAN_POINT('Ctrl Pts',(57.4488616512167,21.0895927631027,9.84677171664517));
#33475=CARTESIAN_POINT('Ctrl Pts',(57.4458691947999,21.1713863311129,9.85103648111434));
#33476=CARTESIAN_POINT('Ctrl Pts',(57.4387789180195,21.2529063581448,9.85530124558352));
#33477=CARTESIAN_POINT('Ctrl Pts',(57.4276701375239,21.3337183743441,9.85956601005269));
#33478=CARTESIAN_POINT('Ctrl Pts',(57.4166487304825,21.4138947829709,9.86379723103763));
#33479=CARTESIAN_POINT('Ctrl Pts',(57.4016305233529,21.4936749372697,9.86802845202257));
#33480=CARTESIAN_POINT('Ctrl Pts',(57.3826552117956,21.5726293667839,9.8722596730075));
#33481=CARTESIAN_POINT('Ctrl Pts',(57.3637071094665,21.6514705813405,9.8764848267267));
#33482=CARTESIAN_POINT('Ctrl Pts',(57.3408132798271,21.7294879744486,9.8807099804459));
#33483=CARTESIAN_POINT('Ctrl Pts',(57.3140649610287,21.8062590192608,9.8849351341651));
#33484=CARTESIAN_POINT('Ctrl Pts',(57.2872479323257,21.8832272701554,9.88917114127329));
#33485=CARTESIAN_POINT('Ctrl Pts',(57.2565566572777,21.9589422946898,9.89340714838148));
#33486=CARTESIAN_POINT('Ctrl Pts',(57.2221343399255,22.0329904284763,9.89764315548967));
#33487=CARTESIAN_POINT('Ctrl Pts',(57.1878619854026,22.1067159672578,9.90186070818633));
#33488=CARTESIAN_POINT('Ctrl Pts',(57.1498912195992,22.1787886810994,9.90607826088299));
#33489=CARTESIAN_POINT('Ctrl Pts',(57.1084120666089,22.2488189650138,9.91029581357964));
#33490=CARTESIAN_POINT('Ctrl Pts',(57.0669466090509,22.3188261265896,9.91451197374045));
#33491=CARTESIAN_POINT('Ctrl Pts',(57.0219753014447,22.3867917977215,9.91872813390126));
#33492=CARTESIAN_POINT('Ctrl Pts',(56.973733686242,22.4523517431372,9.92294429406206));
#33493=CARTESIAN_POINT('Ctrl Pts',(56.9254932205056,22.5179101264378,9.92716035376325));
#33494=CARTESIAN_POINT('Ctrl Pts',(56.8739828785433,22.5810625241831,9.93137641346443));
#33495=CARTESIAN_POINT('Ctrl Pts',(56.8194801744949,22.6414755997639,9.93559247316562));
#33496=CARTESIAN_POINT('Ctrl Pts',(56.7645313509494,22.7023831728445,9.93984304246529));
#33497=CARTESIAN_POINT('Ctrl Pts',(56.7065412620411,22.7605060056448,9.94409361176496));
#33498=CARTESIAN_POINT('Ctrl Pts',(56.6458328328143,22.8155397369462,9.94834418106463));
#33499=CARTESIAN_POINT('Ctrl Pts',(56.585529737066,22.8702060231657,9.9525663704826));
#33500=CARTESIAN_POINT('Ctrl Pts',(56.5225448920022,22.9218240826417,9.95678855990056));
#33501=CARTESIAN_POINT('Ctrl Pts',(56.4572272983366,22.9701367594618,9.96101074931852));
#33502=CARTESIAN_POINT('Ctrl Pts',(56.3912511462556,23.0189365442432,9.96527550855905));
#33503=CARTESIAN_POINT('Ctrl Pts',(56.3228953459908,23.0643636499391,9.96954026779957));
#33504=CARTESIAN_POINT('Ctrl Pts',(56.2525470057195,23.1061994797414,9.9738050270401));
#33505=CARTESIAN_POINT('Ctrl Pts',(56.1821986654482,23.1480353095437,9.97806978628062));
#33506=CARTESIAN_POINT('Ctrl Pts',(56.1098582411348,23.1862796950713,9.98233454552115));
#33507=CARTESIAN_POINT('Ctrl Pts',(56.0359337950515,23.220763702484,9.98659930476167));
#33508=CARTESIAN_POINT('Ctrl Pts',(55.9625907055436,23.2549765207904,9.99083052508566));
#33509=CARTESIAN_POINT('Ctrl Pts',(55.8874134108726,23.2856162299238,9.99506174540966));
#33510=CARTESIAN_POINT('Ctrl Pts',(55.8107842910035,23.3124833152829,9.99929296573365));
#33511=CARTESIAN_POINT('Ctrl Pts',(55.7342650518872,23.3393118751367,10.0035181187862));
#33512=CARTESIAN_POINT('Ctrl Pts',(55.6562985572485,23.3623784027111,10.0077432718387));
#33513=CARTESIAN_POINT('Ctrl Pts',(55.5772893002634,23.3815304561986,10.0119684248912));
#33514=CARTESIAN_POINT('Ctrl Pts',(55.4980770721725,23.4007317104206,10.0162044321653));
#33515=CARTESIAN_POINT('Ctrl Pts',(55.4178171477371,23.4159981588874,10.0204404394394));
#33516=CARTESIAN_POINT('Ctrl Pts',(55.3369347508858,23.4272258287282,10.0246764467136));
#33517=CARTESIAN_POINT('Ctrl Pts',(55.2564047389614,23.4384045823429,10.0288939987345));
#33518=CARTESIAN_POINT('Ctrl Pts',(55.1752581295352,23.4455796034614,10.0331115507555));
#33519=CARTESIAN_POINT('Ctrl Pts',(55.09392531759,23.448699304675,10.0373291027764));
#33520=CARTESIAN_POINT('Ctrl Pts',(55.0126193598504,23.4518179758356,10.0415452622596));
#33521=CARTESIAN_POINT('Ctrl Pts',(54.9311277858973,23.4508839682967,10.0457614217428));
#33522=CARTESIAN_POINT('Ctrl Pts',(54.8498843552359,23.445897696797,10.0499775812261));
#33523=CARTESIAN_POINT('Ctrl Pts',(54.7686428604029,23.4409115441078,10.0541936402487));
#33524=CARTESIAN_POINT('Ctrl Pts',(54.6876499610865,23.4318733490222,10.0584096992714));
#33525=CARTESIAN_POINT('Ctrl Pts',(54.6073362126123,23.4188355463062,10.062625758294));
#33526=CARTESIAN_POINT('Ctrl Pts',(54.5263650459627,23.4056910210348,10.0668763283921));
#33527=CARTESIAN_POINT('Ctrl Pts',(54.4460846761135,23.3884811683558,10.0711268984901));
#33528=CARTESIAN_POINT('Ctrl Pts',(54.3669259354745,23.367312290093,10.0753774685882));
#33529=CARTESIAN_POINT('Ctrl Pts',(54.2882957432863,23.3462847579117,10.0795996573322));
#33530=CARTESIAN_POINT('Ctrl Pts',(54.2107726755594,23.3213511111254,10.0838218460763));
#33531=CARTESIAN_POINT('Ctrl Pts',(54.1347620394814,23.2926651569031,10.0880440348203));
#33532=CARTESIAN_POINT('Ctrl Pts',(54.0579849935265,23.2636899642298,10.0923087955954));
#33533=CARTESIAN_POINT('Ctrl Pts',(53.9827514956785,23.230886563881,10.0965735563704));
#33534=CARTESIAN_POINT('Ctrl Pts',(53.9094551176978,23.1944616901839,10.1008383171455));
#33535=CARTESIAN_POINT('Ctrl Pts',(53.8361587397172,23.1580368164868,10.1051030779206));
#33536=CARTESIAN_POINT('Ctrl Pts',(53.7647998703185,23.1179907612598,10.1093678386956));
#33537=CARTESIAN_POINT('Ctrl Pts',(53.6957417143754,23.0745747936335,10.1136325994707));
#33538=CARTESIAN_POINT('Ctrl Pts',(53.6272266735438,23.0315002754389,10.1178638195872));
#33539=CARTESIAN_POINT('Ctrl Pts',(53.5607193389105,22.984947175665,10.1220950397038));
#33540=CARTESIAN_POINT('Ctrl Pts',(53.4965946844597,22.9351286022394,10.1263262598204));
#33541=CARTESIAN_POINT('Ctrl Pts',(53.4325619803304,22.8853814652042,10.1305514126598));
#33542=CARTESIAN_POINT('Ctrl Pts',(53.3709055348076,22.8323784370686,10.1347765654993));
#33543=CARTESIAN_POINT('Ctrl Pts',(53.3119727599222,22.7763767299633,10.1390017183387));
#33544=CARTESIAN_POINT('Ctrl Pts',(53.2528885857669,22.7202311535497,10.1432377256654));
#33545=CARTESIAN_POINT('Ctrl Pts',(53.1965424906567,22.6610717277937,10.1474737329921));
#33546=CARTESIAN_POINT('Ctrl Pts',(53.1432524020399,22.5991993645163,10.1517097403188));
#33547=CARTESIAN_POINT('Ctrl Pts',(53.090194488868,22.5375965681292,10.1559272921145));
#33548=CARTESIAN_POINT('Ctrl Pts',(53.0401663202996,22.4733047736645,10.1601448439101));
#33549=CARTESIAN_POINT('Ctrl Pts',(52.9934446114649,22.4066576423355,10.1643623957058));
#33550=CARTESIAN_POINT('Ctrl Pts',(52.9467383290998,22.3400325164075,10.1685785549596));
#33551=CARTESIAN_POINT('Ctrl Pts',(52.9033366051359,22.2710539783736,10.1727947142134));
#33552=CARTESIAN_POINT('Ctrl Pts',(52.8634742849804,22.200086713142,10.1770108734672));
#33553=CARTESIAN_POINT('Ctrl Pts',(52.8236129146808,22.1291211389477,10.1812269322566));
#33554=CARTESIAN_POINT('Ctrl Pts',(52.7872910072233,22.0561673376716,10.185442991046));
#33555=CARTESIAN_POINT('Ctrl Pts',(52.7546979615751,21.9816155083559,10.1896590498354));
#33556=CARTESIAN_POINT('Ctrl Pts',(52.7218381176401,21.906453416945,10.1939096201974));
#33557=CARTESIAN_POINT('Ctrl Pts',(52.692768671173,21.8296674477605,10.1981601905594));
#33558=CARTESIAN_POINT('Ctrl Pts',(52.6676339104245,21.751677240708,10.2024107609215));
#33559=CARTESIAN_POINT('Ctrl Pts',(52.6426669792038,21.6742077889456,10.2066329494252));
#33560=CARTESIAN_POINT('Ctrl Pts',(52.6215824103021,21.5955506016873,10.210855137929));
#33561=CARTESIAN_POINT('Ctrl Pts',(52.6044707359118,21.5161296299351,10.2150773264328));
#33562=CARTESIAN_POINT('Ctrl Pts',(52.5871865226414,21.4359078478586,10.2193420877239));
#33563=CARTESIAN_POINT('Ctrl Pts',(52.5739558514078,21.3549072713918,10.2236068490151));
#33564=CARTESIAN_POINT('Ctrl Pts',(52.5648184199452,21.273570689515,10.2278716103062));
#33565=CARTESIAN_POINT('Ctrl Pts',(52.5556809884825,21.1922341076383,10.2321363715974));
#33566=CARTESIAN_POINT('Ctrl Pts',(52.5506367623642,21.1105620051941,10.2364011328885));
#33567=CARTESIAN_POINT('Ctrl Pts',(52.5496715539799,21.0289958035729,10.2406658941797));
#33568=CARTESIAN_POINT('Ctrl Pts',(52.5495578944551,21.0193908562159,10.2411680973824));
#33569=CARTESIAN_POINT('Ctrl Pts',(52.5495007097351,21.0097852392485,10.2416703005852));
#33570=CARTESIAN_POINT('Ctrl Pts',(52.5495000065656,21.0001793819091,10.2421725037879));
#33571=CARTESIAN_POINT('',(52.5495008566119,21.0020489641339,11.0421724789485));
#33572=CARTESIAN_POINT('Ctrl Pts',(52.5495000065655,21.0001793810522,10.2421725038327));
#33573=CARTESIAN_POINT('Ctrl Pts',(52.5494940944825,20.9194152249059,10.246394929427));
#33574=CARTESIAN_POINT('Ctrl Pts',(52.5534852447008,20.8384964272295,10.2506173550213));
#33575=CARTESIAN_POINT('Ctrl Pts',(52.5614933360761,20.7578523177923,10.2548397806156));
#33576=CARTESIAN_POINT('Ctrl Pts',(52.5694899518793,20.6773237711335,10.2590561554861));
#33577=CARTESIAN_POINT('Ctrl Pts',(52.5814920319619,20.597069591859,10.2632725303566));
#33578=CARTESIAN_POINT('Ctrl Pts',(52.5974674466584,20.5175193473994,10.2674889052271));
#33579=CARTESIAN_POINT('Ctrl Pts',(52.6134244530256,20.4380607679841,10.271700421606));
#33580=CARTESIAN_POINT('Ctrl Pts',(52.6333456042126,20.3593049670456,10.275911937985));
#33581=CARTESIAN_POINT('Ctrl Pts',(52.657147118386,20.2816751256477,10.280123454364));
#33582=CARTESIAN_POINT('Ctrl Pts',(52.6809336462747,20.2040941627753,10.2843323190215));
#33583=CARTESIAN_POINT('Ctrl Pts',(52.7085955512577,20.127638197695,10.2885411836791));
#33584=CARTESIAN_POINT('Ctrl Pts',(52.7399985197093,20.052717803881,10.2927500483367));
#33585=CARTESIAN_POINT('Ctrl Pts',(52.7713914438852,19.9778213734416,10.296957566784));
#33586=CARTESIAN_POINT('Ctrl Pts',(52.8065228750273,19.9044599694482,10.3011650852314));
#33587=CARTESIAN_POINT('Ctrl Pts',(52.8452099382239,19.8330252617683,10.3053726036787));
#33588=CARTESIAN_POINT('Ctrl Pts',(52.883896611826,19.761591273465,10.3095800797546));
#33589=CARTESIAN_POINT('Ctrl Pts',(52.9261386226279,19.6920843529753,10.3137875558306));
#33590=CARTESIAN_POINT('Ctrl Pts',(52.9717073065553,19.6248712788546,10.3179950319065));
#33591=CARTESIAN_POINT('Ctrl Pts',(53.0173211902005,19.5575915358789,10.3222066813909));
#33592=CARTESIAN_POINT('Ctrl Pts',(53.0662680755153,19.4926105716875,10.3264183308752));
#33593=CARTESIAN_POINT('Ctrl Pts',(53.1182764588268,19.4302653840235,10.3306299803596));
#33594=CARTESIAN_POINT('Ctrl Pts',(53.1703098516973,19.3678902160844,10.3348436551232));
#33595=CARTESIAN_POINT('Ctrl Pts',(53.2254073578391,19.3081536930189,10.3390573298867));
#33596=CARTESIAN_POINT('Ctrl Pts',(53.2832594495177,19.2513570597947,10.3432710046503));
#33597=CARTESIAN_POINT('Ctrl Pts',(53.3412157186426,19.1944581497464,10.34749226721));
#33598=CARTESIAN_POINT('Ctrl Pts',(53.4019361342735,19.1405100181646,10.3517135297697));
#33599=CARTESIAN_POINT('Ctrl Pts',(53.4650769767002,19.0897744733817,10.3559347923293));
#33600=CARTESIAN_POINT('Ctrl Pts',(53.5237335120291,19.0426422027211,10.3598562578491));
#33601=CARTESIAN_POINT('Ctrl Pts',(53.5844782987549,18.9982821328772,10.3637777233688));
#33602=CARTESIAN_POINT('Ctrl Pts',(53.6470151067306,18.9568695272732,10.3676991888886));
#33603=CARTESIAN_POINT('Ctrl Pts',(53.7144916687481,18.9121857587728,10.3719304091876));
#33604=CARTESIAN_POINT('Ctrl Pts',(53.7843107156218,18.870764532508,10.3761616294866));
#33605=CARTESIAN_POINT('Ctrl Pts',(53.8561235800349,18.8328597216959,10.3803928497857));
#33606=CARTESIAN_POINT('Ctrl Pts',(53.9278334698295,18.7950092637281,10.3846180028111));
#33607=CARTESIAN_POINT('Ctrl Pts',(54.0015310912931,18.7606654220311,10.3888431558365));
#33608=CARTESIAN_POINT('Ctrl Pts',(54.0768389451719,18.7300387851665,10.3930683088619));
#33609=CARTESIAN_POINT('Ctrl Pts',(54.1523402620237,18.6993334696525,10.3973043161426));
#33610=CARTESIAN_POINT('Ctrl Pts',(54.2294596980397,18.6723647373858,10.4015403234232));
#33611=CARTESIAN_POINT('Ctrl Pts',(54.3077920827892,18.649298307026,10.4057763307039));
#33612=CARTESIAN_POINT('Ctrl Pts',(54.3857831916818,18.6263323717018,10.4099938826928));
#33613=CARTESIAN_POINT('Ctrl Pts',(54.4649762557747,18.6072349463723,10.4142114346817));
#33614=CARTESIAN_POINT('Ctrl Pts',(54.5449532428255,18.5921207051048,10.4184289866706));
#33615=CARTESIAN_POINT('Ctrl Pts',(54.6249038232982,18.5770114542153,10.42264514612));
#33616=CARTESIAN_POINT('Ctrl Pts',(54.7056373562451,18.5658828619374,10.4268613055693));
#33617=CARTESIAN_POINT('Ctrl Pts',(54.7867247909581,18.5587986696693,10.4310774650187));
#33618=CARTESIAN_POINT('Ctrl Pts',(54.8678102935257,18.5517146462029,10.4352935240057));
#33619=CARTESIAN_POINT('Ctrl Pts',(54.9492492178389,18.5486748704977,10.4395095829928));
#33620=CARTESIAN_POINT('Ctrl Pts',(55.0306079885442,18.5496911621109,10.4437256419798));
#33621=CARTESIAN_POINT('Ctrl Pts',(55.1126327329865,18.550715772723,10.4479762121146));
#33622=CARTESIAN_POINT('Ctrl Pts',(55.1945755256662,18.5558631702371,10.4522267822494));
#33623=CARTESIAN_POINT('Ctrl Pts',(55.2759945504124,18.5650919405155,10.4564773523842));
#33624=CARTESIAN_POINT('Ctrl Pts',(55.3568699331744,18.5742590894835,10.4606995410887));
#33625=CARTESIAN_POINT('Ctrl Pts',(55.4372280679039,18.5874531367582,10.4649217297931));
#33626=CARTESIAN_POINT('Ctrl Pts',(55.5166453570889,18.604581910188,10.4691439184976));
#33627=CARTESIAN_POINT('Ctrl Pts',(55.5968634073559,18.6218833922973,10.4734086793476));
#33628=CARTESIAN_POINT('Ctrl Pts',(55.6761210631514,18.6431992683482,10.4776734401976));
#33629=CARTESIAN_POINT('Ctrl Pts',(55.7539985055505,18.6683832854374,10.4819382010476));
#33630=CARTESIAN_POINT('Ctrl Pts',(55.8318759479495,18.6935673025266,10.4862029618976));
#33631=CARTESIAN_POINT('Ctrl Pts',(55.9083727493533,18.7226192295344,10.4904677227476));
#33632=CARTESIAN_POINT('Ctrl Pts',(55.9830925372282,18.7553442773454,10.4947324835976));
#33633=CARTESIAN_POINT('Ctrl Pts',(56.0572246850924,18.7878119562854,10.4989637038798));
#33634=CARTESIAN_POINT('Ctrl Pts',(56.1298856760451,18.8240168954734,10.503194924162));
#33635=CARTESIAN_POINT('Ctrl Pts',(56.2006731417975,18.8638037879057,10.5074261444442));
#33636=CARTESIAN_POINT('Ctrl Pts',(56.2713591032709,18.9035336287146,10.5116512974522));
#33637=CARTESIAN_POINT('Ctrl Pts',(56.3401764732719,18.9468349958729,10.5158764504602));
#33638=CARTESIAN_POINT('Ctrl Pts',(56.4067436195039,18.9935048868774,10.5201016034682));
#33639=CARTESIAN_POINT('Ctrl Pts',(56.4734817745108,19.0402946712727,10.5243376107531));
#33640=CARTESIAN_POINT('Ctrl Pts',(56.5379576996635,19.0904701136743,10.528573618038));
#33641=CARTESIAN_POINT('Ctrl Pts',(56.5998124600216,19.1437806318327,10.532809625323));
#33642=CARTESIAN_POINT('Ctrl Pts',(56.6613977333373,19.1968588882575,10.5370271772931));
#33643=CARTESIAN_POINT('Ctrl Pts',(56.7203842741128,19.2530446605368,10.5412447292632));
#33644=CARTESIAN_POINT('Ctrl Pts',(56.7764490629299,19.3120488819828,10.5454622812334));
#33645=CARTESIAN_POINT('Ctrl Pts',(56.8324953404255,19.3710336215733,10.5496784406635));
#33646=CARTESIAN_POINT('Ctrl Pts',(56.8856214617184,19.4328346255407,10.5538946000936));
#33647=CARTESIAN_POINT('Ctrl Pts',(56.9355412283676,19.497125952287,10.5581107595237));
#33648=CARTESIAN_POINT('Ctrl Pts',(56.9854598055269,19.5614157470974,10.5623268184911));
#33649=CARTESIAN_POINT('Ctrl Pts',(57.0321718956901,19.6281953788033,10.5665428774584));
#33650=CARTESIAN_POINT('Ctrl Pts',(57.0754324736214,19.6971069508829,10.5707589364258));
#33651=CARTESIAN_POINT('Ctrl Pts',(57.1190471675672,19.7665826090756,10.5750095065825));
#33652=CARTESIAN_POINT('Ctrl Pts',(57.1591533140597,19.8382248736267,10.5792600767392));
#33653=CARTESIAN_POINT('Ctrl Pts',(57.1955461483394,19.911640059304,10.583510646896));
#33654=CARTESIAN_POINT('Ctrl Pts',(57.2316959841033,19.9845650446023,10.5877328355798));
#33655=CARTESIAN_POINT('Ctrl Pts',(57.2641818143274,20.0592388920022,10.5919550242637));
#33656=CARTESIAN_POINT('Ctrl Pts',(57.2928514014913,20.1352557021412,10.5961772129475));
#33657=CARTESIAN_POINT('Ctrl Pts',(57.3218100632935,20.2120389876313,10.6004419738407));
#33658=CARTESIAN_POINT('Ctrl Pts',(57.346874942372,20.2901920078152,10.6047067347339));
#33659=CARTESIAN_POINT('Ctrl Pts',(57.3679412905953,20.3692827144483,10.608971495627));
#33660=CARTESIAN_POINT('Ctrl Pts',(57.3890076388186,20.4483734210814,10.6132362565202));
#33661=CARTESIAN_POINT('Ctrl Pts',(57.4060754185282,20.5284013295618,10.6175010174134));
#33662=CARTESIAN_POINT('Ctrl Pts',(57.4190933765831,20.6089277747377,10.6217657783066));
#33663=CARTESIAN_POINT('Ctrl Pts',(57.4320089538018,20.6888209128491,10.6259969986256));
#33664=CARTESIAN_POINT('Ctrl Pts',(57.4409866592818,20.7695043569888,10.6302282189447));
#33665=CARTESIAN_POINT('Ctrl Pts',(57.4459388145949,20.8505558122309,10.6344594392638));
#33666=CARTESIAN_POINT('Ctrl Pts',(57.4508838688641,20.9314910453629,10.6386845923093));
#33667=CARTESIAN_POINT('Ctrl Pts',(57.4518148091863,21.0127927813999,10.6429097453547));
#33668=CARTESIAN_POINT('Ctrl Pts',(57.4486952760865,21.09403028699,10.6471348984002));
#33669=CARTESIAN_POINT('Ctrl Pts',(57.4455677290451,21.1754764881169,10.6513709056759));
#33670=CARTESIAN_POINT('Ctrl Pts',(57.4383688019827,21.2568576613764,10.6556069129515));
#33671=CARTESIAN_POINT('Ctrl Pts',(57.4271144206118,21.3377363457759,10.6598429202271));
#33672=CARTESIAN_POINT('Ctrl Pts',(57.4159090718788,21.4182626611637,10.664060472236));
#33673=CARTESIAN_POINT('Ctrl Pts',(57.4006835888085,21.498290392473,10.6682780242449));
#33674=CARTESIAN_POINT('Ctrl Pts',(57.3815057072802,21.5773913890871,10.6724955762537));
#33675=CARTESIAN_POINT('Ctrl Pts',(57.3623341578516,21.6564662683536,10.676711735723));
#33676=CARTESIAN_POINT('Ctrl Pts',(57.3392129109556,21.7346145690944,10.6809278951922));
#33677=CARTESIAN_POINT('Ctrl Pts',(57.3122606512133,21.8114190845986,10.6851440546614));
#33678=CARTESIAN_POINT('Ctrl Pts',(57.2853090336881,21.8882217700085,10.6893601136682));
#33679=CARTESIAN_POINT('Ctrl Pts',(57.254526739808,21.9636802955179,10.693576172675));
#33680=CARTESIAN_POINT('Ctrl Pts',(57.220081628862,22.0373947229428,10.6977922316818));
#33681=CARTESIAN_POINT('Ctrl Pts',(57.1853545629394,22.1117125494883,10.702042801793));
#33682=CARTESIAN_POINT('Ctrl Pts',(57.1469046267709,22.1842571516632,10.7062933719041));
#33683=CARTESIAN_POINT('Ctrl Pts',(57.1049515806814,22.2546430141626,10.7105439420153));
#33684=CARTESIAN_POINT('Ctrl Pts',(57.0632786583457,22.32455890478,10.7147661307389));
#33685=CARTESIAN_POINT('Ctrl Pts',(57.0181495763465,22.3923444395174,10.7189883194626));
#33686=CARTESIAN_POINT('Ctrl Pts',(56.9698228391822,22.4576516155228,10.7232105081863));
#33687=CARTESIAN_POINT('Ctrl Pts',(56.9210088263624,22.5236172799522,10.7274752689912));
#33688=CARTESIAN_POINT('Ctrl Pts',(56.8689326201312,22.5870539505716,10.7317400297961));
#33689=CARTESIAN_POINT('Ctrl Pts',(56.8139004459577,22.6476393483267,10.736004790601));
#33690=CARTESIAN_POINT('Ctrl Pts',(56.7588682717842,22.7082247460818,10.7402695514058));
#33691=CARTESIAN_POINT('Ctrl Pts',(56.7008805164288,22.7659585765689,10.7445343122107));
#33692=CARTESIAN_POINT('Ctrl Pts',(56.6402779712684,22.8205599212802,10.7487990730156));
#33693=CARTESIAN_POINT('Ctrl Pts',(56.5801520389524,22.8747318499968,10.7530302933186));
#33694=CARTESIAN_POINT('Ctrl Pts',(56.5172268635239,22.9260235608084,10.7572615136216));
#33695=CARTESIAN_POINT('Ctrl Pts',(56.4518097309541,22.9741324056676,10.7614927339246));
#33696=CARTESIAN_POINT('Ctrl Pts',(56.3864864019737,23.0221722658106,10.7657178869539));
#33697=CARTESIAN_POINT('Ctrl Pts',(56.3186785840612,23.0670380513405,10.7699430399832));
#33698=CARTESIAN_POINT('Ctrl Pts',(56.2487284797095,23.1084656587107,10.7741681930124));
#33699=CARTESIAN_POINT('Ctrl Pts',(56.1785986763164,23.1499996919598,10.7784042002921));
#33700=CARTESIAN_POINT('Ctrl Pts',(56.1063159204699,23.1880775481734,10.7826402075718));
#33701=CARTESIAN_POINT('Ctrl Pts',(56.0322564176405,23.222475407792,10.7868762148514));
#33702=CARTESIAN_POINT('Ctrl Pts',(55.9585195746456,23.2567234040268,10.7910937668437));
#33703=CARTESIAN_POINT('Ctrl Pts',(55.8830218550091,23.2873231980491,10.795311318836));
#33704=CARTESIAN_POINT('Ctrl Pts',(55.8061597338934,23.3140995513264,10.7995288708283));
#33705=CARTESIAN_POINT('Ctrl Pts',(55.7293229909011,23.3408670636611,10.8037450302809));
#33706=CARTESIAN_POINT('Ctrl Pts',(55.6511231797466,23.3638134893972,10.8079611897335));
#33707=CARTESIAN_POINT('Ctrl Pts',(55.5719752056556,23.3828123329619,10.8121773491861));
#33708=CARTESIAN_POINT('Ctrl Pts',(55.4928291175002,23.4018107238227,10.8163934081761));
#33709=CARTESIAN_POINT('Ctrl Pts',(55.4127353636673,23.4168616120932,10.8206094671662));
#33710=CARTESIAN_POINT('Ctrl Pts',(55.3321210033346,23.4278891838682,10.8248255261562));
#33711=CARTESIAN_POINT('Ctrl Pts',(55.2508467628784,23.4390070233746,10.8290760962869));
#33712=CARTESIAN_POINT('Ctrl Pts',(55.1690438267035,23.4460352946014,10.8333266664176));
#33713=CARTESIAN_POINT('Ctrl Pts',(55.0871552772608,23.4489496131292,10.8375772365483));
#33714=CARTESIAN_POINT('Ctrl Pts',(55.0058135047322,23.4518444725006,10.8417994252553));
#33715=CARTESIAN_POINT('Ctrl Pts',(54.9243877273233,23.4506802188239,10.8460216139623));
#33716=CARTESIAN_POINT('Ctrl Pts',(54.8433105161209,23.4454853619766,10.8502438026693));
#33717=CARTESIAN_POINT('Ctrl Pts',(54.7614158071071,23.4402381256253,10.8545085635118));
#33718=CARTESIAN_POINT('Ctrl Pts',(54.679877215646,23.4308786032364,10.8587733243544));
#33719=CARTESIAN_POINT('Ctrl Pts',(54.5991315741485,23.4174893495433,10.8630380851969));
#33720=CARTESIAN_POINT('Ctrl Pts',(54.5183859326511,23.4041000958502,10.8673028460395));
#33721=CARTESIAN_POINT('Ctrl Pts',(54.4384336981956,23.3866812761905,10.871567606882));
#33722=CARTESIAN_POINT('Ctrl Pts',(54.3596956929881,23.3653669153901,10.8758323677246));
#33723=CARTESIAN_POINT('Ctrl Pts',(54.2815769288897,23.3442201830226,10.8800635880269));
#33724=CARTESIAN_POINT('Ctrl Pts',(54.204360415008,23.319159710537,10.8842948083291));
#33725=CARTESIAN_POINT('Ctrl Pts',(54.1284670641012,23.2902795880948,10.8885260286314));
#33726=CARTESIAN_POINT('Ctrl Pts',(54.0526825389488,23.2614408777272,10.8927511816599));
#33727=CARTESIAN_POINT('Ctrl Pts',(53.9782178394031,23.2287935593128,10.8969763346883));
#33728=CARTESIAN_POINT('Ctrl Pts',(53.90548042427,23.1924819607796,10.9012014877168));
#33729=CARTESIAN_POINT('Ctrl Pts',(53.8325561495876,23.1560770791826,10.9054374949967));
#33730=CARTESIAN_POINT('Ctrl Pts',(53.7613684992649,23.1159891961191,10.9096735022765));
#33731=CARTESIAN_POINT('Ctrl Pts',(53.6923095212342,23.0724130528795,10.9139095095564));
#33732=CARTESIAN_POINT('Ctrl Pts',(53.6235514169462,23.0290267606582,10.9181270615477));
#33733=CARTESIAN_POINT('Ctrl Pts',(53.55690387543,22.9821827826933,10.9223446135391));
#33734=CARTESIAN_POINT('Ctrl Pts',(53.4927291157899,22.9321192332805,10.9265621655304));
#33735=CARTESIAN_POINT('Ctrl Pts',(53.428575545196,22.8820722137133,10.930778324982));
#33736=CARTESIAN_POINT('Ctrl Pts',(53.3668935013947,22.8288080194679,10.9349944844336));
#33737=CARTESIAN_POINT('Ctrl Pts',(53.3080142411145,22.7726066799289,10.9392106438852));
#33738=CARTESIAN_POINT('Ctrl Pts',(53.2491363838083,22.7164066795545,10.9434267028742));
#33739=CARTESIAN_POINT('Ctrl Pts',(53.1930615127808,22.6572699948515,10.9476427618633));
#33740=CARTESIAN_POINT('Ctrl Pts',(53.140084890369,22.5955143480916,10.9518588208523));
#33741=CARTESIAN_POINT('Ctrl Pts',(53.0866746203768,22.5332531918152,10.956109390984));
#33742=CARTESIAN_POINT('Ctrl Pts',(53.0364138799446,22.4683303534671,10.9603599611158));
#33743=CARTESIAN_POINT('Ctrl Pts',(52.9895634067052,22.401104904831,10.9646105312476));
#33744=CARTESIAN_POINT('Ctrl Pts',(52.9430257581448,22.3343283263541,10.9688327199534));
#33745=CARTESIAN_POINT('Ctrl Pts',(52.8998531706619,22.2652802242718,10.9730549086592));
#33746=CARTESIAN_POINT('Ctrl Pts',(52.8602562387386,22.1943395187897,10.9772770973651));
#33747=CARTESIAN_POINT('Ctrl Pts',(52.8202600527306,22.1226835213632,10.9815418582098));
#33748=CARTESIAN_POINT('Ctrl Pts',(52.7839122496268,22.0490969752077,10.9858066190546));
#33749=CARTESIAN_POINT('Ctrl Pts',(52.7513803240931,21.9739916853465,10.9900713798993));
#33750=CARTESIAN_POINT('Ctrl Pts',(52.7188483985593,21.8988863954853,10.9943361407441));
#33751=CARTESIAN_POINT('Ctrl Pts',(52.6901324595109,21.8222628356214,10.9986009015888));
#33752=CARTESIAN_POINT('Ctrl Pts',(52.6653480735384,21.7445472666455,11.0028656624336));
#33753=CARTESIAN_POINT('Ctrl Pts',(52.6357253635559,21.6516603271242,11.0079629754672));
#33754=CARTESIAN_POINT('Ctrl Pts',(52.6116270588092,21.5569317973583,11.0130602885009));
#33755=CARTESIAN_POINT('Ctrl Pts',(52.5932460894767,21.4609618901612,11.0181576015345));
#33756=CARTESIAN_POINT('Ctrl Pts',(52.5750889287308,21.3661605224948,11.0231928491567));
#33757=CARTESIAN_POINT('Ctrl Pts',(52.5625107684555,21.2701478592151,11.0282280967789));
#33758=CARTESIAN_POINT('Ctrl Pts',(52.5556514284901,21.1735232288698,11.0332633444011));
#33759=CARTESIAN_POINT('Ctrl Pts',(52.5516058953972,21.1165355096989,11.0362330559169));
#33760=CARTESIAN_POINT('Ctrl Pts',(52.549548756107,21.0593353118622,11.0392027674327));
#33761=CARTESIAN_POINT('Ctrl Pts',(52.5495008566119,21.0020489641339,11.0421724789485));
#33762=CARTESIAN_POINT('',(52.5495290836882,20.9986540030259,11.8421725323987));
#33763=CARTESIAN_POINT('Ctrl Pts',(52.5512711617411,21.0020470050971,11.0421725037879));
#33764=CARTESIAN_POINT('Ctrl Pts',(52.5557259539615,20.4383632669047,11.0714146549061));
#33765=CARTESIAN_POINT('Ctrl Pts',(53.0293753351344,19.0516701821435,11.143001237594));
#33766=CARTESIAN_POINT('Ctrl Pts',(55.3350226443368,18.1229073326861,11.2569322518514));
#33767=CARTESIAN_POINT('Ctrl Pts',(57.5990916197438,19.7214754048292,11.3839655465605));
#33768=CARTESIAN_POINT('Ctrl Pts',(57.4835458207409,22.4906047579764,11.5109988412695));
#33769=CARTESIAN_POINT('Ctrl Pts',(55.094173934607,23.8950014953986,11.6380321359785));
#33770=CARTESIAN_POINT('Ctrl Pts',(52.942897126316,22.812112652436,11.748423356818));
#33771=CARTESIAN_POINT('Ctrl Pts',(52.5552276006745,21.4948623786468,11.8164701460878));
#33772=CARTESIAN_POINT('Ctrl Pts',(52.5527567710893,20.9986563282935,11.8421725037879));
#33773=CARTESIAN_POINT('',(52.5495003638158,20.9986646869211,12.6421725037591));
#33774=CARTESIAN_POINT('Ctrl Pts',(52.5495003696722,20.9986539823399,11.8421725326532));
#33775=CARTESIAN_POINT('Ctrl Pts',(52.5495501121537,20.9080950425036,11.846857062966));
#33776=CARTESIAN_POINT('Ctrl Pts',(52.5546239307066,20.8177144413065,11.8515415932788));
#33777=CARTESIAN_POINT('Ctrl Pts',(52.5646380792273,20.7280394057033,11.8562261235917));
#33778=CARTESIAN_POINT('Ctrl Pts',(52.5746897537974,20.6380283305641,11.8609282082593));
#33779=CARTESIAN_POINT('Ctrl Pts',(52.5897187232734,20.5487283771237,11.865630292927));
#33780=CARTESIAN_POINT('Ctrl Pts',(52.6095903921718,20.4606558085949,11.8703323775946));
#33781=CARTESIAN_POINT('Ctrl Pts',(52.6295615247038,20.3721424105744,11.8750579975994));
#33782=CARTESIAN_POINT('Ctrl Pts',(52.6544238258674,20.2848689666113,11.8797836176042));
#33783=CARTESIAN_POINT('Ctrl Pts',(52.683992309623,20.199338630809,11.884509237609));
#33784=CARTESIAN_POINT('Ctrl Pts',(52.6998216008856,20.153550533983,11.8870390668714));
#33785=CARTESIAN_POINT('Ctrl Pts',(52.7169988381724,20.108261620341,11.8895688961339));
#33786=CARTESIAN_POINT('Ctrl Pts',(52.7354901934547,20.0635462712658,11.8920987253964));
#33787=CARTESIAN_POINT('Ctrl Pts',(52.7664175762218,19.9887584206568,11.8963299457013));
#33788=CARTESIAN_POINT('Ctrl Pts',(52.8011118491665,19.9153641107187,11.9005611660062));
#33789=CARTESIAN_POINT('Ctrl Pts',(52.8394260610957,19.8437688360335,11.9047923863112));
#33790=CARTESIAN_POINT('Ctrl Pts',(52.8776853331266,19.7722762239611,11.9090175393423));
#33791=CARTESIAN_POINT('Ctrl Pts',(52.919554017429,19.7025779301395,11.9132426923735));
#33792=CARTESIAN_POINT('Ctrl Pts',(52.9648370486113,19.635059704128,11.9174678454046));
#33793=CARTESIAN_POINT('Ctrl Pts',(53.0102364100779,19.567368026512,11.9217038526838));
#33794=CARTESIAN_POINT('Ctrl Pts',(53.0590674972057,19.5018680657897,11.925939859963));
#33795=CARTESIAN_POINT('Ctrl Pts',(53.1110872055688,19.4389238631527,11.9301758672422));
#33796=CARTESIAN_POINT('Ctrl Pts',(53.1628802763265,19.376253893567,11.9343934192363));
#33797=CARTESIAN_POINT('Ctrl Pts',(53.217833950369,19.3161178246963,11.9386109712305));
#33798=CARTESIAN_POINT('Ctrl Pts',(53.2756659041834,19.2588445859131,11.9428285232246));
#33799=CARTESIAN_POINT('Ctrl Pts',(53.3334787632022,19.2015902574503,11.9470446826791));
#33800=CARTESIAN_POINT('Ctrl Pts',(53.3941676846644,19.1471972088512,11.9512608421335));
#33801=CARTESIAN_POINT('Ctrl Pts',(53.4574127164301,19.0959583191095,11.9554770015879));
#33802=CARTESIAN_POINT('Ctrl Pts',(53.5206562411948,19.0447206502867,11.9596930605798));
#33803=CARTESIAN_POINT('Ctrl Pts',(53.5864553932218,18.9966372826957,11.9639091195717));
#33804=CARTESIAN_POINT('Ctrl Pts',(53.6544574206571,18.9519605918891,11.9681251785636));
#33805=CARTESIAN_POINT('Ctrl Pts',(53.723016088135,18.9069181938233,11.9723757486921));
#33806=CARTESIAN_POINT('Ctrl Pts',(53.7938134692512,18.8653387784438,11.9766263188205));
#33807=CARTESIAN_POINT('Ctrl Pts',(53.8664601983647,18.8274352096868,11.980876888949));
#33808=CARTESIAN_POINT('Ctrl Pts',(53.9386218590641,18.7897847262952,11.9850990776578));
#33809=CARTESIAN_POINT('Ctrl Pts',(54.0126077940697,18.7557612911305,11.9893212663665));
#33810=CARTESIAN_POINT('Ctrl Pts',(54.0880153397349,18.7255255047723,11.9935434550753));
#33811=CARTESIAN_POINT('Ctrl Pts',(54.1641832161262,18.6949848524064,11.9978082159136));
#33812=CARTESIAN_POINT('Ctrl Pts',(54.2418010731814,18.6683088180263,12.002072976752));
#33813=CARTESIAN_POINT('Ctrl Pts',(54.3204391217192,18.6456110638405,12.0063377375903));
#33814=CARTESIAN_POINT('Ctrl Pts',(54.399077170257,18.6229133096547,12.0106024984287));
#33815=CARTESIAN_POINT('Ctrl Pts',(54.4787349265582,18.6041938833373,12.014867259267));
#33816=CARTESIAN_POINT('Ctrl Pts',(54.5589748794589,18.589513100419,12.0191320201054));
#33817=CARTESIAN_POINT('Ctrl Pts',(54.6385837791951,18.5749477756257,12.0233632404103));
#33818=CARTESIAN_POINT('Ctrl Pts',(54.7190642668798,18.5643031333827,12.0275944607152));
#33819=CARTESIAN_POINT('Ctrl Pts',(54.7999959514765,18.5576755681167,12.0318256810201));
#33820=CARTESIAN_POINT('Ctrl Pts',(54.8808115857021,18.5510575063153,12.0360508340513));
#33821=CARTESIAN_POINT('Ctrl Pts',(54.962076672418,18.5484451189129,12.0402759870824));
#33822=CARTESIAN_POINT('Ctrl Pts',(55.0433613224848,18.5498836669023,12.0445011401136));
#33823=CARTESIAN_POINT('Ctrl Pts',(55.1248547895454,18.5513259104635,12.0487371473928));
#33824=CARTESIAN_POINT('Ctrl Pts',(55.2063674551396,18.5568400080709,12.052973154672));
#33825=CARTESIAN_POINT('Ctrl Pts',(55.2874616224533,18.5664190858703,12.0572091619512));
#33826=CARTESIAN_POINT('Ctrl Pts',(55.3682024815986,18.575956429886,12.0614267139453));
#33827=CARTESIAN_POINT('Ctrl Pts',(55.4485280158544,18.5895233608773,12.0656442659395));
#33828=CARTESIAN_POINT('Ctrl Pts',(55.5280087651534,18.6070610133308,12.0698618179336));
#33829=CARTESIAN_POINT('Ctrl Pts',(55.6074632717172,18.6245928752506,12.0740779773881));
#33830=CARTESIAN_POINT('Ctrl Pts',(55.6860730935931,18.6460927549896,12.0782941368425));
#33831=CARTESIAN_POINT('Ctrl Pts',(55.7634186584541,18.6714506228288,12.0825102962969));
#33832=CARTESIAN_POINT('Ctrl Pts',(55.8407623803269,18.6968078864415,12.0867263552888));
#33833=CARTESIAN_POINT('Ctrl Pts',(55.9168414636413,18.7260228094845,12.0909424142807));
#33834=CARTESIAN_POINT('Ctrl Pts',(55.9912525837727,18.7589358409086,12.0951584732726));
#33835=CARTESIAN_POINT('Ctrl Pts',(56.0662728064653,18.7921182865238,12.0994090434011));
#33836=CARTESIAN_POINT('Ctrl Pts',(56.1395971880355,18.8290594833582,12.1036596135296));
#33837=CARTESIAN_POINT('Ctrl Pts',(56.2108357501217,18.8695476921021,12.1079101836581));
#33838=CARTESIAN_POINT('Ctrl Pts',(56.2815986462453,18.9097655576188,12.1121323723668));
#33839=CARTESIAN_POINT('Ctrl Pts',(56.3503031295201,18.9534829076873,12.1163545610756));
#33840=CARTESIAN_POINT('Ctrl Pts',(56.4165959246362,19.0004484912101,12.1205767497843));
#33841=CARTESIAN_POINT('Ctrl Pts',(56.4835571468785,19.0478876264962,12.1248415106226));
#33842=CARTESIAN_POINT('Ctrl Pts',(56.5480573915711,19.0986405670876,12.129106271461));
#33843=CARTESIAN_POINT('Ctrl Pts',(56.6097681146265,19.1524078190434,12.1333710322993));
#33844=CARTESIAN_POINT('Ctrl Pts',(56.6714788376818,19.2061750709992,12.1376357931377));
#33845=CARTESIAN_POINT('Ctrl Pts',(56.7303997367595,19.2629562537313,12.141900553976));
#33846=CARTESIAN_POINT('Ctrl Pts',(56.7862429045101,19.3224164592822,12.1461653148144));
#33847=CARTESIAN_POINT('Ctrl Pts',(56.8416468894543,19.3814090355599,12.1503965351193));
#33848=CARTESIAN_POINT('Ctrl Pts',(56.8942291722578,19.443259830556,12.1546277554242));
#33849=CARTESIAN_POINT('Ctrl Pts',(56.9436808137138,19.5076678840148,12.1588589757292));
#33850=CARTESIAN_POINT('Ctrl Pts',(56.9930615449771,19.5719835808329,12.1630841287603));
#33851=CARTESIAN_POINT('Ctrl Pts',(57.0393202698788,19.6388488876622,12.1673092817915));
#33852=CARTESIAN_POINT('Ctrl Pts',(57.0821858632528,19.7079271379406,12.1715344348226));
#33853=CARTESIAN_POINT('Ctrl Pts',(57.1251615766104,19.7771828474629,12.1757704421018));
#33854=CARTESIAN_POINT('Ctrl Pts',(57.164726384035,19.8486625364532,12.180006449381));
#33855=CARTESIAN_POINT('Ctrl Pts',(57.2006487324116,19.9219947094122,12.1842424566602));
#33856=CARTESIAN_POINT('Ctrl Pts',(57.2364145755853,19.9950073913825,12.1884600086544));
#33857=CARTESIAN_POINT('Ctrl Pts',(57.2685694190252,20.0698560327421,12.1926775606486));
#33858=CARTESIAN_POINT('Ctrl Pts',(57.296929860991,20.1461478677852,12.1968951126427));
#33859=CARTESIAN_POINT('Ctrl Pts',(57.3252809389841,20.222414513,12.2011112720972));
#33860=CARTESIAN_POINT('Ctrl Pts',(57.3498399415676,20.3001229701735,12.2053274315516));
#33861=CARTESIAN_POINT('Ctrl Pts',(57.3704718183253,20.3788610392792,12.209543591006));
#33862=CARTESIAN_POINT('Ctrl Pts',(57.3911032034673,20.4575972322162,12.2137596499979));
#33863=CARTESIAN_POINT('Ctrl Pts',(57.4078075320624,20.537362538287,12.2179757089898));
#33864=CARTESIAN_POINT('Ctrl Pts',(57.420500173127,20.617731557813,12.2221917679817));
#33865=CARTESIAN_POINT('Ctrl Pts',(57.4332967115683,20.698758449113,12.2264423381102));
#33866=CARTESIAN_POINT('Ctrl Pts',(57.442015492194,20.7803985117083,12.2306929082387));
#33867=CARTESIAN_POINT('Ctrl Pts',(57.446622971078,20.8622092623081,12.2349434783671));
#33868=CARTESIAN_POINT('Ctrl Pts',(57.451199685432,20.9434737555402,12.2391656670759));
#33869=CARTESIAN_POINT('Ctrl Pts',(57.4517198926874,21.0249061944298,12.2433878557847));
#33870=CARTESIAN_POINT('Ctrl Pts',(57.448203149316,21.106073510734,12.2476100444934));
#33871=CARTESIAN_POINT('Ctrl Pts',(57.444650946787,21.1880592332594,12.2518748053317));
#33872=CARTESIAN_POINT('Ctrl Pts',(57.4369799720587,21.2697739729991,12.2561395661701));
#33873=CARTESIAN_POINT('Ctrl Pts',(57.4252637267549,21.3507792834349,12.2604043270084));
#33874=CARTESIAN_POINT('Ctrl Pts',(57.413547481451,21.4317845938708,12.2646690878467));
#33875=CARTESIAN_POINT('Ctrl Pts',(57.3977861214198,21.5120800146024,12.268933848685));
#33876=CARTESIAN_POINT('Ctrl Pts',(57.3781049385212,21.5912420412833,12.2731986095234));
#33877=CARTESIAN_POINT('Ctrl Pts',(57.3585785397706,21.6697814922325,12.2774298298283));
#33878=CARTESIAN_POINT('Ctrl Pts',(57.3351205760353,21.7474998378392,12.2816610501332));
#33879=CARTESIAN_POINT('Ctrl Pts',(57.3078164111831,21.8239743092317,12.2858922704381));
#33880=CARTESIAN_POINT('Ctrl Pts',(57.2805513985923,21.9003391215847,12.2901174234693));
#33881=CARTESIAN_POINT('Ctrl Pts',(57.2494512934621,21.9754631679865,12.2943425765005));
#33882=CARTESIAN_POINT('Ctrl Pts',(57.2146519649609,22.0489360915208,12.2985677295316));
#33883=CARTESIAN_POINT('Ctrl Pts',(57.1797632383856,22.1225977640378,12.3028037368108));
#33884=CARTESIAN_POINT('Ctrl Pts',(57.1411563779152,22.1945993629736,12.30703974409));
#33885=CARTESIAN_POINT('Ctrl Pts',(57.0990179740528,22.2645448962386,12.3112757513692));
#33886=CARTESIAN_POINT('Ctrl Pts',(57.0570631572817,22.3341856933054,12.3154933033634));
#33887=CARTESIAN_POINT('Ctrl Pts',(57.0116077395819,22.4017878979421,12.3197108553575));
#33888=CARTESIAN_POINT('Ctrl Pts',(56.9628822921637,22.466984443377,12.3239284073517));
#33889=CARTESIAN_POINT('Ctrl Pts',(56.9141729327799,22.5321594623956,12.3281445668061));
#33890=CARTESIAN_POINT('Ctrl Pts',(56.8621959658948,22.5949300274527,12.3323607262605));
#33891=CARTESIAN_POINT('Ctrl Pts',(56.807224509266,22.654959160556,12.336576885715));
#33892=CARTESIAN_POINT('Ctrl Pts',(56.7522543624956,22.7149868632868,12.3407929447069));
#33893=CARTESIAN_POINT('Ctrl Pts',(56.6942901826542,22.7722729218149,12.3450090036988));
#33894=CARTESIAN_POINT('Ctrl Pts',(56.6336435168314,22.8265155651991,12.3492250626907));
#33895=CARTESIAN_POINT('Ctrl Pts',(56.5725004193003,22.8812022192763,12.3534756328191));
#33896=CARTESIAN_POINT('Ctrl Pts',(56.5086310642246,22.9327950718666,12.3577262029476));
#33897=CARTESIAN_POINT('Ctrl Pts',(56.4423890534673,22.981026014074,12.3619767730761));
#33898=CARTESIAN_POINT('Ctrl Pts',(56.3765893462725,23.0289349141615,12.3661989617848));
#33899=CARTESIAN_POINT('Ctrl Pts',(56.308448998465,23.0735264573031,12.3704211504936));
#33900=CARTESIAN_POINT('Ctrl Pts',(56.2383424932468,23.1145822564798,12.3746433392023));
#33901=CARTESIAN_POINT('Ctrl Pts',(56.1675291074434,23.156052019343,12.3789081000407));
#33902=CARTESIAN_POINT('Ctrl Pts',(56.0947101227336,23.1939141113333,12.383172860879));
#33903=CARTESIAN_POINT('Ctrl Pts',(56.0202937915758,23.2279925558385,12.3874376217173));
#33904=CARTESIAN_POINT('Ctrl Pts',(55.9458774604181,23.2620710003437,12.3917023825557));
#33905=CARTESIAN_POINT('Ctrl Pts',(55.8698642541614,23.2923656786736,12.395967143394));
#33906=CARTESIAN_POINT('Ctrl Pts',(55.7926779521201,23.3187522321763,12.4002319042323));
#33907=CARTESIAN_POINT('Ctrl Pts',(55.7160986875752,23.344931266638,12.4044631245373));
#33908=CARTESIAN_POINT('Ctrl Pts',(55.6380775643946,23.3673616398872,12.4086943448422));
#33909=CARTESIAN_POINT('Ctrl Pts',(55.5590160940915,23.3858858431507,12.4129255651471));
#33910=CARTESIAN_POINT('Ctrl Pts',(55.4800679924032,23.4043834840032,12.4171507181783));
#33911=CARTESIAN_POINT('Ctrl Pts',(55.4000829552331,23.4189859740579,12.4213758712094));
#33912=CARTESIAN_POINT('Ctrl Pts',(55.3194794502073,23.4295849709148,12.4256010242406));
#33913=CARTESIAN_POINT('Ctrl Pts',(55.2386688780221,23.440211196168,12.4298370315198));
#33914=CARTESIAN_POINT('Ctrl Pts',(55.1572371049882,23.4468131856598,12.434073038799));
#33915=CARTESIAN_POINT('Ctrl Pts',(55.0756180311116,23.4493330037728,12.4383090460782));
#33916=CARTESIAN_POINT('Ctrl Pts',(54.9943545522976,23.4518418436324,12.4425265980723));
#33917=CARTESIAN_POINT('Ctrl Pts',(54.9129058686852,23.450303985438,12.4467441500665));
#33918=CARTESIAN_POINT('Ctrl Pts',(54.8317054235051,23.4447141316568,12.4509617020606));
#33919=CARTESIAN_POINT('Ctrl Pts',(54.7505317888649,23.4391261235182,12.4551778615151));
#33920=CARTESIAN_POINT('Ctrl Pts',(54.6696066933503,23.4294888085328,12.4593940209695));
#33921=CARTESIAN_POINT('Ctrl Pts',(54.5893613682022,23.4158489530753,12.4636101804239));
#33922=CARTESIAN_POINT('Ctrl Pts',(54.5091179551376,23.402209422628,12.4678262394158));
#33923=CARTESIAN_POINT('Ctrl Pts',(54.4295547383962,23.3845676203351,12.4720422984077));
#33924=CARTESIAN_POINT('Ctrl Pts',(54.3510942042322,23.363021692287,12.4762583573996));
#33925=CARTESIAN_POINT('Ctrl Pts',(54.2719914204661,23.3412993970517,12.4805089275281));
#33926=CARTESIAN_POINT('Ctrl Pts',(54.1940099217676,23.3156088770702,12.4847594976566));
#33927=CARTESIAN_POINT('Ctrl Pts',(54.1175667133664,23.286101866637,12.489010067785));
#33928=CARTESIAN_POINT('Ctrl Pts',(54.0416339227954,23.2567918770321,12.4932322564938));
#33929=CARTESIAN_POINT('Ctrl Pts',(53.9672193464176,23.2237164550153,12.4974544452025));
#33930=CARTESIAN_POINT('Ctrl Pts',(53.8947095337005,23.1870718404084,12.5016766339113));
#33931=CARTESIAN_POINT('Ctrl Pts',(53.8214686079623,23.150057739881,12.5059413947496));
#33932=CARTESIAN_POINT('Ctrl Pts',(53.7501714953767,23.1094023062835,12.5102061555879));
#33933=CARTESIAN_POINT('Ctrl Pts',(53.6811874211161,23.06535314941,12.5144709164263));
#33934=CARTESIAN_POINT('Ctrl Pts',(53.6122033468556,23.0213039925365,12.5187356772646));
#33935=CARTESIAN_POINT('Ctrl Pts',(53.5455326662232,22.9738614440747,12.5230004381029));
#33936=CARTESIAN_POINT('Ctrl Pts',(53.4815096521556,22.9233141484176,12.5272651989413));
#33937=CARTESIAN_POINT('Ctrl Pts',(53.4187616329917,22.8737734836619,12.5314450286277));
#33938=CARTESIAN_POINT('Ctrl Pts',(53.3583090111805,22.8210547669303,12.5356248583141));
#33939=CARTESIAN_POINT('Ctrl Pts',(53.3004973656926,22.765401100595,12.5398046880005));
#33940=CARTESIAN_POINT('Ctrl Pts',(53.2415032168275,22.7086090710834,12.5440700136571));
#33941=CARTESIAN_POINT('Ctrl Pts',(53.1852597290091,22.648760927074,12.5483353393137));
#33942=CARTESIAN_POINT('Ctrl Pts',(53.132101510513,22.5861606107114,12.5526006649703));
#33943=CARTESIAN_POINT('Ctrl Pts',(53.0801443795852,22.5249747221433,12.5567696173894));
#33944=CARTESIAN_POINT('Ctrl Pts',(53.0311349011389,22.4611600990071,12.5609385698084));
#33945=CARTESIAN_POINT('Ctrl Pts',(52.9853493218512,22.3950386715194,12.5651075222274));
#33946=CARTESIAN_POINT('Ctrl Pts',(52.9395912881483,22.3289570240981,12.5692739665154));
#33947=CARTESIAN_POINT('Ctrl Pts',(52.8970535765444,22.260571717223,12.5734404108034));
#33948=CARTESIAN_POINT('Ctrl Pts',(52.8579712424293,22.1902365528499,12.5776068550914));
#33949=CARTESIAN_POINT('Ctrl Pts',(52.8188997481619,22.1199208965868,12.5817721437774));
#33950=CARTESIAN_POINT('Ctrl Pts',(52.783281960016,22.0476568737207,12.5859374324635));
#33951=CARTESIAN_POINT('Ctrl Pts',(52.7513079523275,21.9738245862241,12.5901027211495));
#33952=CARTESIAN_POINT('Ctrl Pts',(52.7179993440694,21.8969105263733,12.5944418697003));
#33953=CARTESIAN_POINT('Ctrl Pts',(52.6886456301591,21.8182949040314,12.5987810182511));
#33954=CARTESIAN_POINT('Ctrl Pts',(52.663406240258,21.7384306683331,12.6031201668019));
#33955=CARTESIAN_POINT('Ctrl Pts',(52.6391545882402,21.6616919016508,12.6072895037439));
#33956=CARTESIAN_POINT('Ctrl Pts',(52.6187013072694,21.5838009235815,12.6114588406859));
#33957=CARTESIAN_POINT('Ctrl Pts',(52.6021362891922,21.5051731132901,12.6156281776278));
#33958=CARTESIAN_POINT('Ctrl Pts',(52.5855617474506,21.426500097803,12.6197999116312));
#33959=CARTESIAN_POINT('Ctrl Pts',(52.5728799892526,21.3470898783097,12.6239716456347));
#33960=CARTESIAN_POINT('Ctrl Pts',(52.5641292380657,21.2673646969099,12.6281433796381));
#33961=CARTESIAN_POINT('Ctrl Pts',(52.5553661774599,21.1875273684912,12.6323209818945));
#33962=CARTESIAN_POINT('Ctrl Pts',(52.550545175321,21.1073746695339,12.6364985841508));
#33963=CARTESIAN_POINT('Ctrl Pts',(52.5496524038118,21.0273296149722,12.6406761864072));
#33964=CARTESIAN_POINT('Ctrl Pts',(52.5495458140011,21.0177728727134,12.6411749588579));
#33965=CARTESIAN_POINT('Ctrl Pts',(52.5494951582618,21.0082176587128,12.6416737313085));
#33966=CARTESIAN_POINT('Ctrl Pts',(52.5495003638158,20.9986646869211,12.6421725037591));
#33967=CARTESIAN_POINT('',(52.5495009651831,21.0021749394239,13.4421725037879));
#33968=CARTESIAN_POINT('Ctrl Pts',(52.5495003638161,20.9986646863694,12.6421725037879));
#33969=CARTESIAN_POINT('Ctrl Pts',(52.5495425490658,20.9212484624948,12.6462145004087));
#33970=CARTESIAN_POINT('Ctrl Pts',(52.5532530208526,20.843934384163,12.6502564970295));
#33971=CARTESIAN_POINT('Ctrl Pts',(52.5606047961666,20.7669736291435,12.6542984936503));
#33972=CARTESIAN_POINT('Ctrl Pts',(52.5683007404991,20.6864100018396,12.6585297139552));
#33973=CARTESIAN_POINT('Ctrl Pts',(52.5800064524164,20.6060769848732,12.6627609342602));
#33974=CARTESIAN_POINT('Ctrl Pts',(52.5957000328985,20.5264053228807,12.6669921545651));
#33975=CARTESIAN_POINT('Ctrl Pts',(52.6113711098846,20.4468479044752,12.6712173075962));
#33976=CARTESIAN_POINT('Ctrl Pts',(52.6310186093195,20.3679504098838,12.6754424606274));
#33977=CARTESIAN_POINT('Ctrl Pts',(52.6545688466119,20.2901387778469,12.6796676136585));
#33978=CARTESIAN_POINT('Ctrl Pts',(52.678179583516,20.2121272508595,12.6839036209377));
#33979=CARTESIAN_POINT('Ctrl Pts',(52.7057130846198,20.1352076419053,12.6881396282169));
#33980=CARTESIAN_POINT('Ctrl Pts',(52.7370433772792,20.0597991843845,12.6923756354961));
#33981=CARTESIAN_POINT('Ctrl Pts',(52.7682371712398,19.9847192637351,12.6965931874903));
#33982=CARTESIAN_POINT('Ctrl Pts',(52.8031945703391,19.9111377897203,12.7008107394844));
#33983=CARTESIAN_POINT('Ctrl Pts',(52.8417418269329,19.8394518931172,12.7050282914786));
#33984=CARTESIAN_POINT('Ctrl Pts',(52.8802763560995,19.7677896655664,12.709244450933));
#33985=CARTESIAN_POINT('Ctrl Pts',(52.9223981689301,19.6980221816789,12.7134606103874));
#33986=CARTESIAN_POINT('Ctrl Pts',(52.9678869890961,19.6305231068341,12.7176767698418));
#33987=CARTESIAN_POINT('Ctrl Pts',(53.0133747253557,19.5630256403556,12.7218928288337));
#33988=CARTESIAN_POINT('Ctrl Pts',(53.062229048691,19.4977968603748,12.7261088878256));
#33989=CARTESIAN_POINT('Ctrl Pts',(53.1141864690518,19.4351812959667,12.7303249468175));
#33990=CARTESIAN_POINT('Ctrl Pts',(53.1665691940953,19.3720531831569,12.7345755169459));
#33991=CARTESIAN_POINT('Ctrl Pts',(53.2221057583337,19.3115816444894,12.7388260870744));
#33992=CARTESIAN_POINT('Ctrl Pts',(53.2804861009244,19.2540841369396,12.7430766572029));
#33993=CARTESIAN_POINT('Ctrl Pts',(53.3384766329819,19.1969705451581,12.7472988459116));
#33994=CARTESIAN_POINT('Ctrl Pts',(53.3992726910952,19.1427916559399,12.7515210346204));
#33995=CARTESIAN_POINT('Ctrl Pts',(53.4625362090209,19.091818839463,12.7557432233291));
#33996=CARTESIAN_POINT('Ctrl Pts',(53.5264376100142,19.0403320664816,12.7600079841674));
#33997=CARTESIAN_POINT('Ctrl Pts',(53.5928561163172,18.9921166688931,12.7642727450058));
#33998=CARTESIAN_POINT('Ctrl Pts',(53.6614139914404,18.9474070672224,12.7685375058442));
#33999=CARTESIAN_POINT('Ctrl Pts',(53.7299718665635,18.9026974655518,12.7728022666825));
#34000=CARTESIAN_POINT('Ctrl Pts',(53.8006686618954,18.8614938468948,12.7770670275209));
#34001=CARTESIAN_POINT('Ctrl Pts',(53.8731036507204,18.8239818778374,12.7813317883592));
#34002=CARTESIAN_POINT('Ctrl Pts',(53.9449689691098,18.7867649244912,12.7855630086642));
#34003=CARTESIAN_POINT('Ctrl Pts',(54.0188147040824,18.7530421616621,12.7897942289691));
#34004=CARTESIAN_POINT('Ctrl Pts',(54.0942670546318,18.7230287481669,12.794025449274));
#34005=CARTESIAN_POINT('Ctrl Pts',(54.1696112117913,18.6930583718059,12.7982506023052));
#34006=CARTESIAN_POINT('Ctrl Pts',(54.2465569807047,18.6667869513411,12.8024757553363));
#34007=CARTESIAN_POINT('Ctrl Pts',(54.3247065191816,18.644383527659,12.8067009083675));
#34008=CARTESIAN_POINT('Ctrl Pts',(54.4030568206766,18.6219225504834,12.8109369156467));
#34009=CARTESIAN_POINT('Ctrl Pts',(54.4826166624278,18.6033496803442,12.8151729229259));
#34010=CARTESIAN_POINT('Ctrl Pts',(54.562965484585,18.5887863880743,12.8194089302051));
#34011=CARTESIAN_POINT('Ctrl Pts',(54.642964245867,18.5742865446353,12.8236264821992));
#34012=CARTESIAN_POINT('Ctrl Pts',(54.7237446681765,18.5637615058452,12.8278440341934));
#34013=CARTESIAN_POINT('Ctrl Pts',(54.8048788584204,18.5572806157668,12.8320615861876));
#34014=CARTESIAN_POINT('Ctrl Pts',(54.8859862600005,18.5508018655309,12.836277745642));
#34015=CARTESIAN_POINT('Ctrl Pts',(54.9674467344728,18.5483646493068,12.8404939050965));
#34016=CARTESIAN_POINT('Ctrl Pts',(55.048826876333,18.5499864926602,12.8447100645509));
#34017=CARTESIAN_POINT('Ctrl Pts',(55.1302050790693,18.5516082973683,12.8489261235428));
#34018=CARTESIAN_POINT('Ctrl Pts',(55.2115024881918,18.5572889589791,12.8531421825347));
#34019=CARTESIAN_POINT('Ctrl Pts',(55.2922867481265,18.5669938950201,12.8573582415266));
#34020=CARTESIAN_POINT('Ctrl Pts',(55.3737322788434,18.5767782721632,12.8616088116551));
#34021=CARTESIAN_POINT('Ctrl Pts',(55.4546557424809,18.5906530690653,12.8658593817836));
#34022=CARTESIAN_POINT('Ctrl Pts',(55.5346222786994,18.6085298937435,12.870109951912));
#34023=CARTESIAN_POINT('Ctrl Pts',(55.6140548715271,18.6262873533369,12.8743321406208));
#34024=CARTESIAN_POINT('Ctrl Pts',(55.6925428409481,18.6479933749729,12.8785543293296));
#34025=CARTESIAN_POINT('Ctrl Pts',(55.7696748652404,18.6735110462723,12.8827765180383));
#34026=CARTESIAN_POINT('Ctrl Pts',(55.8475846080949,18.6992860110476,12.8870412788767));
#34027=CARTESIAN_POINT('Ctrl Pts',(55.9241104550958,18.7289497479128,12.891306039715));
#34028=CARTESIAN_POINT('Ctrl Pts',(55.9988506208529,18.762311977236,12.8955708005533));
#34029=CARTESIAN_POINT('Ctrl Pts',(56.0735907866101,18.7956742065591,12.8998355613916));
#34030=CARTESIAN_POINT('Ctrl Pts',(56.1465448706722,18.8327346528485,12.90410032223));
#34031=CARTESIAN_POINT('Ctrl Pts',(56.2173395866305,18.8732572838206,12.9083650830683));
#34032=CARTESIAN_POINT('Ctrl Pts',(56.2875775322036,18.9134612215039,12.9125963033732));
#34033=CARTESIAN_POINT('Ctrl Pts',(56.3559533604273,18.9572238016516,12.9168275236782));
#34034=CARTESIAN_POINT('Ctrl Pts',(56.4220836041848,19.004347607245,12.9210587439831));
#34035=CARTESIAN_POINT('Ctrl Pts',(56.4881190218013,19.0514038405995,12.9252838970142));
#34036=CARTESIAN_POINT('Ctrl Pts',(56.5519148747036,19.1018114594618,12.9295090500454));
#34037=CARTESIAN_POINT('Ctrl Pts',(56.6131134100363,19.1553278404114,12.9337342030766));
#34038=CARTESIAN_POINT('Ctrl Pts',(56.6744691619425,19.2089817027893,12.9379702103558));
#34039=CARTESIAN_POINT('Ctrl Pts',(56.7332138279284,19.2657600802133,12.9422062176349));
#34040=CARTESIAN_POINT('Ctrl Pts',(56.7890173071687,19.3253754675597,12.9464422249141));
#34041=CARTESIAN_POINT('Ctrl Pts',(56.8445776638061,19.3847311247183,12.9506597769083));
#34042=CARTESIAN_POINT('Ctrl Pts',(56.8972220826611,19.4468987869988,12.9548773289025));
#34043=CARTESIAN_POINT('Ctrl Pts',(56.9466602854203,19.5115565233549,12.9590948808966));
#34044=CARTESIAN_POINT('Ctrl Pts',(56.9960821648095,19.5761929111972,12.963311040351));
#34045=CARTESIAN_POINT('Ctrl Pts',(57.0422996481992,19.6433173713685,12.9675271998055));
#34046=CARTESIAN_POINT('Ctrl Pts',(57.0850630080604,19.7125752439781,12.9717433592599));
#34047=CARTESIAN_POINT('Ctrl Pts',(57.1278253489575,19.781831466313,12.9759594182518));
#34048=CARTESIAN_POINT('Ctrl Pts',(57.1671334866555,19.8532206038417,12.9801754772437));
#34049=CARTESIAN_POINT('Ctrl Pts',(57.2027820459374,19.9263606247459,12.9843915362356));
#34050=CARTESIAN_POINT('Ctrl Pts',(57.2387224114536,20.0000993434519,12.9886421063641));
#34051=CARTESIAN_POINT('Ctrl Pts',(57.2709427854333,20.0756173178473,12.9928926764925));
#34052=CARTESIAN_POINT('Ctrl Pts',(57.2992816471748,20.1525012348298,12.997143246621));
#34053=CARTESIAN_POINT('Ctrl Pts',(57.3274312879166,20.2288717913333,13.0013654353298));
#34054=CARTESIAN_POINT('Ctrl Pts',(57.3517510117247,20.3065896384019,13.0055876240385));
#34055=CARTESIAN_POINT('Ctrl Pts',(57.3721328296035,20.385234932094,13.0098098127473));
#34056=CARTESIAN_POINT('Ctrl Pts',(57.3927201563904,20.4646732025724,13.0140745735856));
#34057=CARTESIAN_POINT('Ctrl Pts',(57.4092896207638,20.5450572519506,13.0183393344239));
#34058=CARTESIAN_POINT('Ctrl Pts',(57.4217832455885,20.6259463121602,13.0226040952622));
#34059=CARTESIAN_POINT('Ctrl Pts',(57.4342768704133,20.7068353723697,13.0268688561006));
#34060=CARTESIAN_POINT('Ctrl Pts',(57.442694670034,20.7882289575597,13.0311336169389));
#34061=CARTESIAN_POINT('Ctrl Pts',(57.4470325630816,20.8696854374275,13.0353983777772));
#34062=CARTESIAN_POINT('Ctrl Pts',(57.451336340442,20.9505012966632,13.0396295980822));
#34063=CARTESIAN_POINT('Ctrl Pts',(57.4516403398395,21.0316821126902,13.0438608183871));
#34064=CARTESIAN_POINT('Ctrl Pts',(57.4479025137916,21.1127986390549,13.048092038692));
#34065=CARTESIAN_POINT('Ctrl Pts',(57.4441700475247,21.1937988499981,13.0523171917231));
#34066=CARTESIAN_POINT('Ctrl Pts',(57.4364072877171,21.2747344938583,13.0565423447543));
#34067=CARTESIAN_POINT('Ctrl Pts',(57.4246241137385,21.3551734183153,13.0607674977855));
#34068=CARTESIAN_POINT('Ctrl Pts',(57.4128106692603,21.435818987131,13.0650035050646));
#34069=CARTESIAN_POINT('Ctrl Pts',(57.3969561089172,21.5159648094864,13.0692395123438));
#34070=CARTESIAN_POINT('Ctrl Pts',(57.377123016808,21.5951776314357,13.073475519623));
#34071=CARTESIAN_POINT('Ctrl Pts',(57.3573763328054,21.6740453417949,13.0776930716172));
#34072=CARTESIAN_POINT('Ctrl Pts',(57.3336858174935,21.7519877086711,13.0819106236113));
#34073=CARTESIAN_POINT('Ctrl Pts',(57.3061645734845,21.8285862719143,13.0861281756055));
#34074=CARTESIAN_POINT('Ctrl Pts',(57.2786524163643,21.9051595440545,13.0903443350599));
#34075=CARTESIAN_POINT('Ctrl Pts',(57.2473121993811,21.9803894564804,13.0945604945144));
#34076=CARTESIAN_POINT('Ctrl Pts',(57.2123065126005,22.0538738749516,13.0987766539688));
#34077=CARTESIAN_POINT('Ctrl Pts',(57.1773016599345,22.127356542438,13.1029927129607));
#34078=CARTESIAN_POINT('Ctrl Pts',(57.1386317120743,22.1990933794108,13.1072087719526));
#34079=CARTESIAN_POINT('Ctrl Pts',(57.0965063067393,22.2687046763539,13.1114248309445));
#34080=CARTESIAN_POINT('Ctrl Pts',(57.0540360780468,22.3388857862387,13.1156754010729));
#34081=CARTESIAN_POINT('Ctrl Pts',(57.0080537951447,22.4069059789412,13.1199259712014));
#34082=CARTESIAN_POINT('Ctrl Pts',(56.9588191582693,22.4724054316652,13.1241765413299));
#34083=CARTESIAN_POINT('Ctrl Pts',(56.9099132652687,22.53746753895,13.1283987300386));
#34084=CARTESIAN_POINT('Ctrl Pts',(56.8577986664844,22.6000421449226,13.1326209187474));
#34085=CARTESIAN_POINT('Ctrl Pts',(56.8027695756549,22.6598108648557,13.1368431074561));
#34086=CARTESIAN_POINT('Ctrl Pts',(56.7471856290984,22.7201822299724,13.1411078682945));
#34087=CARTESIAN_POINT('Ctrl Pts',(56.6886284329182,22.7776904669439,13.1453726291328));
#34088=CARTESIAN_POINT('Ctrl Pts',(56.627436899567,22.8320478672589,13.1496373899712));
#34089=CARTESIAN_POINT('Ctrl Pts',(56.5662453662158,22.8864052675738,13.1539021508095));
#34090=CARTESIAN_POINT('Ctrl Pts',(56.5024199117009,22.937611579846,13.1581669116478));
#34091=CARTESIAN_POINT('Ctrl Pts',(56.4363293964162,22.9854239131708,13.1624316724862));
#34092=CARTESIAN_POINT('Ctrl Pts',(56.3707586549759,23.0328602227926,13.1666628927911));
#34093=CARTESIAN_POINT('Ctrl Pts',(56.3027124969757,23.0771336650337,13.170894113096));
#34094=CARTESIAN_POINT('Ctrl Pts',(56.232528791406,23.1179761633114,13.175125333401));
#34095=CARTESIAN_POINT('Ctrl Pts',(56.162445724358,23.1587600963051,13.1793504864321));
#34096=CARTESIAN_POINT('Ctrl Pts',(56.0902315956899,23.1961226244261,13.1835756394633));
#34097=CARTESIAN_POINT('Ctrl Pts',(56.0162548718767,23.2298377262453,13.1878007924944));
#34098=CARTESIAN_POINT('Ctrl Pts',(55.9420881048381,23.2636394408038,13.1920367997736));
#34099=CARTESIAN_POINT('Ctrl Pts',(55.8661500611846,23.2937746934287,13.1962728070528));
#34100=CARTESIAN_POINT('Ctrl Pts',(55.7888387106711,23.320061149743,13.200508814332));
#34101=CARTESIAN_POINT('Ctrl Pts',(55.711864187485,23.3462330821644,13.2047263663262));
#34102=CARTESIAN_POINT('Ctrl Pts',(55.6335287391667,23.3685895265775,13.2089439183203));
#34103=CARTESIAN_POINT('Ctrl Pts',(55.5542452974421,23.3869986175663,13.2131614703145));
#34104=CARTESIAN_POINT('Ctrl Pts',(55.4749880333063,23.405401630292,13.2173776297689));
#34105=CARTESIAN_POINT('Ctrl Pts',(55.3947838498681,23.4198597727448,13.2215937892234));
#34106=CARTESIAN_POINT('Ctrl Pts',(55.3140587944245,23.430291612882,13.2258099486778));
#34107=CARTESIAN_POINT('Ctrl Pts',(55.2333356624953,23.4407232044496,13.2300260076697));
#34108=CARTESIAN_POINT('Ctrl Pts',(55.1520921444674,23.4471286259672,13.2342420666616));
#34109=CARTESIAN_POINT('Ctrl Pts',(55.0707609558563,23.4494781356702,13.2384581256535));
#34110=CARTESIAN_POINT('Ctrl Pts',(54.9887640195022,23.4518468776113,13.242708695782));
#34111=CARTESIAN_POINT('Ctrl Pts',(54.9066784497142,23.4500929708947,13.2469592659104));
#34112=CARTESIAN_POINT('Ctrl Pts',(54.8249473974727,23.4442395210675,13.2512098360389));
#34113=CARTESIAN_POINT('Ctrl Pts',(54.7437620704464,23.4384251552247,13.2554320247477));
#34114=CARTESIAN_POINT('Ctrl Pts',(54.6629269996648,23.4285659437547,13.2596542134564));
#34115=CARTESIAN_POINT('Ctrl Pts',(54.5828692323513,23.4147364602956,13.2638764021652));
#34116=CARTESIAN_POINT('Ctrl Pts',(54.5020042463466,23.4007675348072,13.2681411630035));
#34117=CARTESIAN_POINT('Ctrl Pts',(54.4219328010098,23.3827479292142,13.2724059238418));
#34118=CARTESIAN_POINT('Ctrl Pts',(54.3430804049416,23.3608064079099,13.2766706846802));
#34119=CARTESIAN_POINT('Ctrl Pts',(54.2642280088733,23.3388648866055,13.2809354455185));
#34120=CARTESIAN_POINT('Ctrl Pts',(54.1865950988654,23.3130016628266,13.2852002063568));
#34121=CARTESIAN_POINT('Ctrl Pts',(54.1105857646076,23.2833949653709,13.2894649671952));
#34122=CARTESIAN_POINT('Ctrl Pts',(54.0351742114943,23.2540211120213,13.2936961875001));
#34123=CARTESIAN_POINT('Ctrl Pts',(53.9610779865151,23.2208523503577,13.297927407805));
#34124=CARTESIAN_POINT('Ctrl Pts',(53.8887055370419,23.1840272128796,13.30215862811));
#34125=CARTESIAN_POINT('Ctrl Pts',(53.8164368645958,23.1472548800712,13.3063837811411));
#34126=CARTESIAN_POINT('Ctrl Pts',(53.7458874693976,23.1068367934756,13.3106089341723));
#34127=CARTESIAN_POINT('Ctrl Pts',(53.6774470532155,23.0629599979039,13.3148340872034));
#34128=CARTESIAN_POINT('Ctrl Pts',(53.6088308163596,23.0189704846107,13.3190700944826));
#34129=CARTESIAN_POINT('Ctrl Pts',(53.5423348456485,22.9715046463281,13.3233061017618));
#34130=CARTESIAN_POINT('Ctrl Pts',(53.4783281327667,22.92079800564,13.327542109041));
#34131=CARTESIAN_POINT('Ctrl Pts',(53.4146002820429,22.870312281831,13.3317596610352));
#34132=CARTESIAN_POINT('Ctrl Pts',(53.3533404159781,22.8166142196711,13.3359772130293));
#34133=CARTESIAN_POINT('Ctrl Pts',(53.2948832331578,22.7599792786943,13.3401947650235));
#34134=CARTESIAN_POINT('Ctrl Pts',(53.2364453515694,22.7033630372866,13.3444109244779));
#34135=CARTESIAN_POINT('Ctrl Pts',(53.1808086491966,22.643812165981,13.3486270839323));
#34136=CARTESIAN_POINT('Ctrl Pts',(53.12827256027,22.5816404905546,13.3528432433868));
#34137=CARTESIAN_POINT('Ctrl Pts',(53.075737723172,22.5194702965533,13.3570593023787));
#34138=CARTESIAN_POINT('Ctrl Pts',(53.0263036518553,22.4546797784244,13.3612753613706));
#34139=CARTESIAN_POINT('Ctrl Pts',(52.980229964204,22.3876163924157,13.3654914203625));
#34140=CARTESIAN_POINT('Ctrl Pts',(52.9337791339819,22.3200040497443,13.3697419904909));
#34141=CARTESIAN_POINT('Ctrl Pts',(52.8907442400028,22.2500818439982,13.3739925606194));
#34142=CARTESIAN_POINT('Ctrl Pts',(52.8513461543074,22.1782346546382,13.3782431307479));
#34143=CARTESIAN_POINT('Ctrl Pts',(52.8122111329946,22.106867195097,13.3824653194566));
#34144=CARTESIAN_POINT('Ctrl Pts',(52.7766646506345,22.0336008296154,13.3866875081654));
#34145=CARTESIAN_POINT('Ctrl Pts',(52.7448756021483,21.9588348138308,13.3909096968741));
#34146=CARTESIAN_POINT('Ctrl Pts',(52.7127660261858,21.8833149358359,13.3951744577125));
#34147=CARTESIAN_POINT('Ctrl Pts',(52.6844902500044,21.8062654515716,13.3994392185508));
#34148=CARTESIAN_POINT('Ctrl Pts',(52.6601708012614,21.7281137072808,13.4037039793891));
#34149=CARTESIAN_POINT('Ctrl Pts',(52.6358513525184,21.6499619629899,13.4079687402275));
#34150=CARTESIAN_POINT('Ctrl Pts',(52.6154882888828,21.5707084413021,13.4122335010658));
#34151=CARTESIAN_POINT('Ctrl Pts',(52.5991509624684,21.4907893122141,13.4164982619042));
#34152=CARTESIAN_POINT('Ctrl Pts',(52.5760578947605,21.3778223669276,13.4225265683907));
#34153=CARTESIAN_POINT('Ctrl Pts',(52.5609317705013,21.263175741453,13.4285548748773));
#34154=CARTESIAN_POINT('Ctrl Pts',(52.5539600038609,21.1477788458736,13.4345831813639));
#34155=CARTESIAN_POINT('Ctrl Pts',(52.5510343073978,21.0993526281496,13.4371129555053));
#34156=CARTESIAN_POINT('Ctrl Pts',(52.5495441175164,21.0507945698908,13.4396427296466));
#34157=CARTESIAN_POINT('Ctrl Pts',(52.5495009651831,21.0021749394239,13.4421725037879));
#34158=CARTESIAN_POINT('',(52.5499009846874,21.000004473486,14.2421725034846));
#34159=CARTESIAN_POINT('Ctrl Pts',(52.5487175127731,21.0021682154797,13.4421728897047));
#34160=CARTESIAN_POINT('Ctrl Pts',(52.5547032669598,20.3526186542018,13.4759591120076));
#34161=CARTESIAN_POINT('Ctrl Pts',(53.1534784602604,18.8792388521044,13.55208976588));
#34162=CARTESIAN_POINT('Ctrl Pts',(55.640566724473,18.1751855530352,13.6705648513222));
#34163=CARTESIAN_POINT('Ctrl Pts',(57.720838282277,20.0065507411148,13.7975981460311));
#34164=CARTESIAN_POINT('Ctrl Pts',(57.3100291386536,22.7474746827509,13.92463144074));
#34165=CARTESIAN_POINT('Ctrl Pts',(54.7842582038357,23.8884871240272,14.0516647354491));
#34166=CARTESIAN_POINT('Ctrl Pts',(52.844309899764,22.6356866765821,14.1575117554562));
#34167=CARTESIAN_POINT('Ctrl Pts',(52.5534943172644,21.4087914667217,14.2210143438937));
#34168=CARTESIAN_POINT('Ctrl Pts',(52.5535009435967,21.0000045195322,14.2421725007616));
#34169=CARTESIAN_POINT('',(52.5495009672036,20.9978227852975,15.042172503748));
#34170=CARTESIAN_POINT('Ctrl Pts',(52.5495000000041,21.0000044683571,14.2421725037879));
#34171=CARTESIAN_POINT('Ctrl Pts',(52.5494998442032,20.9145614302854,14.2465876779589));
#34172=CARTESIAN_POINT('Ctrl Pts',(52.5539727787239,20.8292041264636,14.2510028521299));
#34173=CARTESIAN_POINT('Ctrl Pts',(52.5628662413919,20.7444040441387,14.2554180263009));
#34174=CARTESIAN_POINT('Ctrl Pts',(52.5717838644767,20.6593735897509,14.2598451949506));
#34175=CARTESIAN_POINT('Ctrl Pts',(52.5851459765392,20.5749037787846,14.2642723636003));
#34176=CARTESIAN_POINT('Ctrl Pts',(52.6028484141931,20.4914584336917,14.26869953225));
#34177=CARTESIAN_POINT('Ctrl Pts',(52.6205754493165,20.4078971416102,14.2731328524336));
#34178=CARTESIAN_POINT('Ctrl Pts',(52.6426547332348,20.3253635372867,14.2775661726172));
#34179=CARTESIAN_POINT('Ctrl Pts',(52.6689322213934,20.244306105925,14.2819994928009));
#34180=CARTESIAN_POINT('Ctrl Pts',(52.6952815016257,20.1630272195658,14.2864449251486));
#34181=CARTESIAN_POINT('Ctrl Pts',(52.7258517765444,20.0832329417358,14.2908903574964));
#34182=CARTESIAN_POINT('Ctrl Pts',(52.7604405008871,20.0053525750633,14.2953357898441));
#34183=CARTESIAN_POINT('Ctrl Pts',(52.7874021300513,19.9446454629827,14.2988009681851));
#34184=CARTESIAN_POINT('Ctrl Pts',(52.8168044190187,19.8851008470814,14.302266146526));
#34185=CARTESIAN_POINT('Ctrl Pts',(52.8485328046591,19.8269104222729,14.305731324867));
#34186=CARTESIAN_POINT('Ctrl Pts',(52.8872753386224,19.7558559244161,14.3099625451719));
#34187=CARTESIAN_POINT('Ctrl Pts',(52.9296142697847,19.6865895385243,14.3141937654769));
#34188=CARTESIAN_POINT('Ctrl Pts',(52.975360155001,19.6194987330529,14.3184249857818));
#34189=CARTESIAN_POINT('Ctrl Pts',(53.0210404438198,19.5525041311008,14.322650138813));
#34190=CARTESIAN_POINT('Ctrl Pts',(53.0701177243472,19.4876792946342,14.3268752918441));
#34191=CARTESIAN_POINT('Ctrl Pts',(53.1223568248339,19.425386918398,14.3311004448753));
#34192=CARTESIAN_POINT('Ctrl Pts',(53.1747301254667,19.3629345155549,14.3353364521545));
#34193=CARTESIAN_POINT('Ctrl Pts',(53.2302812804322,19.3030280125131,14.3395724594337));
#34194=CARTESIAN_POINT('Ctrl Pts',(53.2887296739244,19.2460033862367,14.3438084667129));
#34195=CARTESIAN_POINT('Ctrl Pts',(53.3469234215458,19.1892272028129,14.348026018707));
#34196=CARTESIAN_POINT('Ctrl Pts',(53.4079888859932,19.1353081697927,14.3522435707012));
#34197=CARTESIAN_POINT('Ctrl Pts',(53.4716102092135,19.0845431622144,14.3564611226953));
#34198=CARTESIAN_POINT('Ctrl Pts',(53.5352105261203,19.0337949160866,14.3606772821498));
#34199=CARTESIAN_POINT('Ctrl Pts',(53.6013646628347,18.9861989170979,14.3648934416042));
#34200=CARTESIAN_POINT('Ctrl Pts',(53.6697232007087,18.9420121751411,14.3691096010587));
#34201=CARTESIAN_POINT('Ctrl Pts',(53.7380801097372,18.8978264860649,14.3733256600506));
#34202=CARTESIAN_POINT('Ctrl Pts',(53.8086409244351,18.8570501439591,14.3775417190424));
#34203=CARTESIAN_POINT('Ctrl Pts',(53.8810279426985,18.8198963820546,14.3817577780343));
#34204=CARTESIAN_POINT('Ctrl Pts',(53.9540074949562,18.7824384928706,14.3860083481628));
#34205=CARTESIAN_POINT('Ctrl Pts',(54.0288428666092,18.7486629972304,14.3902589182913));
#34206=CARTESIAN_POINT('Ctrl Pts',(54.1051241738747,18.7187399302542,14.3945094884198));
#34207=CARTESIAN_POINT('Ctrl Pts',(54.1808961443376,18.6890166621515,14.3987316771285));
#34208=CARTESIAN_POINT('Ctrl Pts',(54.2580943351833,18.6630946242449,14.4029538658373));
#34209=CARTESIAN_POINT('Ctrl Pts',(54.3363012259363,18.6410904664853,14.4071760545461));
#34210=CARTESIAN_POINT('Ctrl Pts',(54.4152966730796,18.618864441841,14.4114408153844));
#34211=CARTESIAN_POINT('Ctrl Pts',(54.4953208023052,18.600635857537,14.4157055762227));
#34212=CARTESIAN_POINT('Ctrl Pts',(54.5759341390416,18.5864717951576,14.4199703370611));
#34213=CARTESIAN_POINT('Ctrl Pts',(54.656547475778,18.5723077327782,14.4242350978994));
#34214=CARTESIAN_POINT('Ctrl Pts',(54.7377495339812,18.5622081880313,14.4284998587377));
#34215=CARTESIAN_POINT('Ctrl Pts',(54.819098862249,18.5561863760998,14.4327646195761));
#34216=CARTESIAN_POINT('Ctrl Pts',(54.8998084125864,18.5502119231625,14.436995839881));
#34217=CARTESIAN_POINT('Ctrl Pts',(54.9809655730983,18.5482288437161,14.4412270601859));
#34218=CARTESIAN_POINT('Ctrl Pts',(55.0621420588733,18.5502880547871,14.4454582804909));
#34219=CARTESIAN_POINT('Ctrl Pts',(55.1432021432495,18.5523443130934,14.449683433522));
#34220=CARTESIAN_POINT('Ctrl Pts',(55.2242810370014,18.5584313382175,14.4539085865532));
#34221=CARTESIAN_POINT('Ctrl Pts',(55.3049464759174,18.5685481915478,14.4581337395843));
#34222=CARTESIAN_POINT('Ctrl Pts',(55.3858191410986,18.578691034667,14.4623697468635));
#34223=CARTESIAN_POINT('Ctrl Pts',(55.4662757532284,18.5928844658689,14.4666057541427));
#34224=CARTESIAN_POINT('Ctrl Pts',(55.5458818565599,18.6110748758744,14.4708417614219));
#34225=CARTESIAN_POINT('Ctrl Pts',(55.625141134867,18.6291860345519,14.4750593134161));
#34226=CARTESIAN_POINT('Ctrl Pts',(55.703556841916,18.6512593206239,14.4792768654102));
#34227=CARTESIAN_POINT('Ctrl Pts',(55.7807082676652,18.6771903111104,14.4834944174044));
#34228=CARTESIAN_POINT('Ctrl Pts',(55.8578342197686,18.7031127397738,14.4877105768588));
#34229=CARTESIAN_POINT('Ctrl Pts',(55.9336962791937,18.7328901954063,14.4919267363133));
#34230=CARTESIAN_POINT('Ctrl Pts',(56.0078890347163,18.7663684404767,14.4961428957677));
#34231=CARTESIAN_POINT('Ctrl Pts',(56.0820800223759,18.7998458878283,14.5003589547596));
#34232=CARTESIAN_POINT('Ctrl Pts',(56.1546013618978,18.8370237570559,14.5045750137515));
#34233=CARTESIAN_POINT('Ctrl Pts',(56.2250690888506,18.8777003092064,14.5087910727434));
#34234=CARTESIAN_POINT('Ctrl Pts',(56.2961136391718,18.9187098249253,14.5130416428718));
#34235=CARTESIAN_POINT('Ctrl Pts',(56.3650703779875,18.9632753399351,14.5172922130003));
#34236=CARTESIAN_POINT('Ctrl Pts',(56.4315741878375,19.0111446521385,14.5215427831288));
#34237=CARTESIAN_POINT('Ctrl Pts',(56.4976339460701,19.0586943368565,14.5257649718375));
#34238=CARTESIAN_POINT('Ctrl Pts',(56.5612731040727,19.1095034924075,14.5299871605463));
#34239=CARTESIAN_POINT('Ctrl Pts',(56.6221672597112,19.1632845534702,14.534209349255));
#34240=CARTESIAN_POINT('Ctrl Pts',(56.6836754082485,19.2176078864346,14.5384741100934));
#34241=CARTESIAN_POINT('Ctrl Pts',(56.7423825399049,19.2749630539153,14.5427388709317));
#34242=CARTESIAN_POINT('Ctrl Pts',(56.7979939976509,19.335017166932,14.54700363177));
#34243=CARTESIAN_POINT('Ctrl Pts',(56.853605455397,19.3950712799487,14.5512683926084));
#34244=CARTESIAN_POINT('Ctrl Pts',(56.9061209792954,19.457823927783,14.5555331534467));
#34245=CARTESIAN_POINT('Ctrl Pts',(56.9552901008918,19.5229113529125,14.559797914285));
#34246=CARTESIAN_POINT('Ctrl Pts',(57.0040725282214,19.5874868930761,14.56402913459));
#34247=CARTESIAN_POINT('Ctrl Pts',(57.0497439663743,19.6546027410072,14.5682603548949));
#34248=CARTESIAN_POINT('Ctrl Pts',(57.0920294076324,19.723926644898,14.5724915751998));
#34249=CARTESIAN_POINT('Ctrl Pts',(57.1342542145273,19.7931511431626,14.576716728231));
#34250=CARTESIAN_POINT('Ctrl Pts',(57.1731024274221,19.8645770155185,14.5809418812621));
#34251=CARTESIAN_POINT('Ctrl Pts',(57.2083404518764,19.9378405493494,14.5851670342933));
#34252=CARTESIAN_POINT('Ctrl Pts',(57.2436690013968,20.0112922942491,14.5894030415725));
#34253=CARTESIAN_POINT('Ctrl Pts',(57.275368510485,20.0865907739699,14.5936390488517));
#34254=CARTESIAN_POINT('Ctrl Pts',(57.3032484521605,20.1633418753037,14.5978750561309));
#34255=CARTESIAN_POINT('Ctrl Pts',(57.331006927503,20.2397585901838,14.602092608125));
#34256=CARTESIAN_POINT('Ctrl Pts',(57.3549788805052,20.3176148586486,14.6063101601192));
#34257=CARTESIAN_POINT('Ctrl Pts',(57.3750239328768,20.39650056482,14.6105277121133));
#34258=CARTESIAN_POINT('Ctrl Pts',(57.395062366828,20.4753602247257,14.6147438715678));
#34259=CARTESIAN_POINT('Ctrl Pts',(57.4111763605519,20.5552481971022,14.6189600310222));
#34260=CARTESIAN_POINT('Ctrl Pts',(57.4232756870592,20.6357402101413,14.6231761904766));
#34261=CARTESIAN_POINT('Ctrl Pts',(57.435374725264,20.7162303052188,14.6273922494685));
#34262=CARTESIAN_POINT('Ctrl Pts',(57.4434592184389,20.7973239524205,14.6316083084604));
#34263=CARTESIAN_POINT('Ctrl Pts',(57.4474904808888,20.8785891439837,14.6358243674523));
#34264=CARTESIAN_POINT('Ctrl Pts',(57.4515547417975,20.9605195430618,14.6400749375808));
#34265=CARTESIAN_POINT('Ctrl Pts',(57.4514990693311,21.0426238295319,14.6443255077092));
#34266=CARTESIAN_POINT('Ctrl Pts',(57.4473373979528,21.1244584693046,14.6485760778377));
#34267=CARTESIAN_POINT('Ctrl Pts',(57.4432035144096,21.2057466921993,14.6527982665465));
#34268=CARTESIAN_POINT('Ctrl Pts',(57.4350184058769,21.2867683974232,14.6570204552552));
#34269=CARTESIAN_POINT('Ctrl Pts',(57.4228477969882,21.367095086632,14.661242643964));
#34270=CARTESIAN_POINT('Ctrl Pts',(57.4105544724242,21.4482317060588,14.6655074048023));
#34271=CARTESIAN_POINT('Ctrl Pts',(57.3941949207406,21.5286587389069,14.6697721656406));
#34272=CARTESIAN_POINT('Ctrl Pts',(57.3738890775575,21.6079481042435,14.674036926479));
#34273=CARTESIAN_POINT('Ctrl Pts',(57.3535832343744,21.6872374695801,14.6783016873173));
#34274=CARTESIAN_POINT('Ctrl Pts',(57.3293313038483,21.7653887262961,14.6825664481556));
#34275=CARTESIAN_POINT('Ctrl Pts',(57.3013031184507,21.8419941846647,14.686831208994));
#34276=CARTESIAN_POINT('Ctrl Pts',(57.273495362832,21.9179971736258,14.6910624292989));
#34277=CARTESIAN_POINT('Ctrl Pts',(57.2418663045063,21.9927636097845,14.6952936496038));
#34278=CARTESIAN_POINT('Ctrl Pts',(57.2065459980047,22.0658822677432,14.6995248699087));
#34279=CARTESIAN_POINT('Ctrl Pts',(57.1712763383506,22.138896078664,14.7037500229399));
#34280=CARTESIAN_POINT('Ctrl Pts',(57.1323261433176,22.2102663889744,14.7079751759711));
#34281=CARTESIAN_POINT('Ctrl Pts',(57.0898743571043,22.2795997114401,14.7122003290022));
#34282=CARTESIAN_POINT('Ctrl Pts',(57.0473135139614,22.34911114842,14.7164363362814));
#34283=CARTESIAN_POINT('Ctrl Pts',(57.0012332339305,22.4165746772112,14.7206723435606));
#34284=CARTESIAN_POINT('Ctrl Pts',(56.9518613569798,22.4816165135179,14.7249083508398));
#34285=CARTESIAN_POINT('Ctrl Pts',(56.9027045816571,22.5463749778781,14.729125902834));
#34286=CARTESIAN_POINT('Ctrl Pts',(56.8502851073941,22.6087324296222,14.7333434548281));
#34287=CARTESIAN_POINT('Ctrl Pts',(56.7948714118838,22.6683485441605,14.7375610068223));
#34288=CARTESIAN_POINT('Ctrl Pts',(56.7394760127151,22.7279449748139,14.7417771662767));
#34289=CARTESIAN_POINT('Ctrl Pts',(56.6810886718463,22.7848015254518,14.7459933257312));
#34290=CARTESIAN_POINT('Ctrl Pts',(56.6200169544138,22.8386123347274,14.7502094851856));
#34291=CARTESIAN_POINT('Ctrl Pts',(56.5589466921968,22.8924218618003,14.7544255441775));
#34292=CARTESIAN_POINT('Ctrl Pts',(56.4951925301558,22.9431854852801,14.7586416031694));
#34293=CARTESIAN_POINT('Ctrl Pts',(56.4290964802649,22.9906364560347,14.7628576621613));
#34294=CARTESIAN_POINT('Ctrl Pts',(56.3624593919755,23.0384758433024,14.7671082322898));
#34295=CARTESIAN_POINT('Ctrl Pts',(56.2934422795059,23.0829478023613,14.7713588024182));
#34296=CARTESIAN_POINT('Ctrl Pts',(56.2224253714566,23.1238235475715,14.7756093725467));
#34297=CARTESIAN_POINT('Ctrl Pts',(56.1518826493667,23.1644263619404,14.7798315612555));
#34298=CARTESIAN_POINT('Ctrl Pts',(56.079367202195,23.2014806820742,14.7840537499642));
#34299=CARTESIAN_POINT('Ctrl Pts',(56.0052747067387,23.2348093909753,14.788275938673));
#34300=CARTESIAN_POINT('Ctrl Pts',(55.9304351401459,23.2684741516761,14.7925406995113));
#34301=CARTESIAN_POINT('Ctrl Pts',(55.8539869961572,23.2983375711843,14.7968054603496));
#34302=CARTESIAN_POINT('Ctrl Pts',(55.7763549952266,23.3242683088204,14.801070221188));
#34303=CARTESIAN_POINT('Ctrl Pts',(55.6987229942959,23.3501990464565,14.8053349820263));
#34304=CARTESIAN_POINT('Ctrl Pts',(55.6199076177568,23.3721970345811,14.8095997428646));
#34305=CARTESIAN_POINT('Ctrl Pts',(55.540343507813,23.3901839141715,14.813864503703));
#34306=CARTESIAN_POINT('Ctrl Pts',(55.4614051358154,23.4080293345902,14.8180957240079));
#34307=CARTESIAN_POINT('Ctrl Pts',(55.3814337654475,23.4219934753772,14.8223269443128));
#34308=CARTESIAN_POINT('Ctrl Pts',(55.300845441241,23.4319626375593,14.8265581646177));
#34309=CARTESIAN_POINT('Ctrl Pts',(55.2203726750507,23.4419175046607,14.8307833176489));
#34310=CARTESIAN_POINT('Ctrl Pts',(55.1392851695522,23.4478887138307,14.8350084706801));
#34311=CARTESIAN_POINT('Ctrl Pts',(55.0580105740899,23.4498132629435,14.8392336237112));
#34312=CARTESIAN_POINT('Ctrl Pts',(54.976527187464,23.4517427561454,14.8434696309904));
#34313=CARTESIAN_POINT('Ctrl Pts',(54.8948562102012,23.4496046734464,14.8477056382696));
#34314=CARTESIAN_POINT('Ctrl Pts',(54.8134352488942,23.4433877800392,14.8519416455488));
#34315=CARTESIAN_POINT('Ctrl Pts',(54.73236901952,23.4371979721709,14.856159197543));
#34316=CARTESIAN_POINT('Ctrl Pts',(54.6515510992603,23.4269648477751,14.8603767495371));
#34317=CARTESIAN_POINT('Ctrl Pts',(54.5714130153411,23.4127294598817,14.8645943015313));
#34318=CARTESIAN_POINT('Ctrl Pts',(54.491301391194,23.3984987721895,14.8688104609857));
#34319=CARTESIAN_POINT('Ctrl Pts',(54.4118696150248,23.3802685264764,14.8730266204402));
#34320=CARTESIAN_POINT('Ctrl Pts',(54.3335414508891,23.3581313051476,14.8772427798946));
#34321=CARTESIAN_POINT('Ctrl Pts',(54.2552151531549,23.3359946113039,14.8814588388865));
#34322=CARTESIAN_POINT('Ctrl Pts',(54.1779928622648,23.309951254453,14.8856748978784));
#34323=CARTESIAN_POINT('Ctrl Pts',(54.1022841566359,23.2801439679488,14.8898909568703));
#34324=CARTESIAN_POINT('Ctrl Pts',(54.0259557268796,23.25009268976,14.8941415269988));
#34325=CARTESIAN_POINT('Ctrl Pts',(53.9511662283322,23.2162157379607,14.8983920971272));
#34326=CARTESIAN_POINT('Ctrl Pts',(53.8783140630311,23.1787085415002,14.9026426672557));
#34327=CARTESIAN_POINT('Ctrl Pts',(53.8059483378588,23.1414517837935,14.9068648559645));
#34328=CARTESIAN_POINT('Ctrl Pts',(53.7354945284408,23.1006134016322,14.9110870446732));
#34329=CARTESIAN_POINT('Ctrl Pts',(53.6673159993428,23.0564298199531,14.915309233382));
#34330=CARTESIAN_POINT('Ctrl Pts',(53.5984500293521,23.0118007373042,14.9195739942203));
#34331=CARTESIAN_POINT('Ctrl Pts',(53.5319058748999,22.963758900825,14.9238387550586));
#34332=CARTESIAN_POINT('Ctrl Pts',(53.4680241857756,22.9125899598794,14.928103515897));
#34333=CARTESIAN_POINT('Ctrl Pts',(53.4041424966514,22.8614210189338,14.9323682767353));
#34334=CARTESIAN_POINT('Ctrl Pts',(53.3429235906776,22.8071253412798,14.9366330375736));
#34335=CARTESIAN_POINT('Ctrl Pts',(53.284668980371,22.7500256406975,14.940897798412));
#34336=CARTESIAN_POINT('Ctrl Pts',(53.227028795328,22.6935281842705,14.945117577801));
#34337=CARTESIAN_POINT('Ctrl Pts',(53.1720584083385,22.6340576330772,14.94933735719));
#34338=CARTESIAN_POINT('Ctrl Pts',(53.1200859364908,22.5719011940387,14.953557136579));
#34339=CARTESIAN_POINT('Ctrl Pts',(53.0688039783508,22.5105705743552,14.9577208513744));
#34340=CARTESIAN_POINT('Ctrl Pts',(53.0204411034233,22.4466253580654,14.9618845661698));
#34341=CARTESIAN_POINT('Ctrl Pts',(52.9752778230292,22.3803805113383,14.9660482809652));
#34342=CARTESIAN_POINT('Ctrl Pts',(52.9301575445797,22.3141987392418,14.9702080313048));
#34343=CARTESIAN_POINT('Ctrl Pts',(52.8882310864795,22.2457220735526,14.9743677816443));
#34344=CARTESIAN_POINT('Ctrl Pts',(52.84973859012,22.1752983107198,14.9785275319838));
#34345=CARTESIAN_POINT('Ctrl Pts',(52.8112701534318,22.1049185661438,14.9826846822783));
#34346=CARTESIAN_POINT('Ctrl Pts',(52.7762316482358,22.0325945592949,14.9868418325727));
#34347=CARTESIAN_POINT('Ctrl Pts',(52.7448188932777,21.9587014268702,14.9909989828672));
#34348=CARTESIAN_POINT('Ctrl Pts',(52.712595271367,21.8829008686501,14.9952634429406));
#34349=CARTESIAN_POINT('Ctrl Pts',(52.6841874401857,21.8054495065769,14.999527903014));
#34350=CARTESIAN_POINT('Ctrl Pts',(52.6597549449292,21.7267759848928,15.0037923630874));
#34351=CARTESIAN_POINT('Ctrl Pts',(52.6359347509933,21.6500740956888,15.0079499517788));
#34352=CARTESIAN_POINT('Ctrl Pts',(52.6158930621347,21.5722110794703,15.0121075404701));
#34353=CARTESIAN_POINT('Ctrl Pts',(52.5997270895804,21.4935992357224,15.0162651291615));
#34354=CARTESIAN_POINT('Ctrl Pts',(52.5829377942457,21.4119562997928,15.0205830249259));
#34355=CARTESIAN_POINT('Ctrl Pts',(52.5703292912183,21.3295061650706,15.0249009206903));
#34356=CARTESIAN_POINT('Ctrl Pts',(52.5619516542964,21.2467195047255,15.0292188164548));
#34357=CARTESIAN_POINT('Ctrl Pts',(52.5535740173746,21.1639328443803,15.0335367122192));
#34358=CARTESIAN_POINT('Ctrl Pts',(52.5494272346723,21.0808102355086,15.0378546079836));
#34359=CARTESIAN_POINT('Ctrl Pts',(52.5495009672036,20.9978227852975,15.042172503748));
#34360=CARTESIAN_POINT('',(52.5495003595367,21.0013274370615,15.8421725038163));
#34361=CARTESIAN_POINT('Ctrl Pts',(52.5495009672043,20.9978227845304,15.0421725037879));
#34362=CARTESIAN_POINT('Ctrl Pts',(52.5496037390909,20.8821509953396,15.0481909888401));
#34363=CARTESIAN_POINT('Ctrl Pts',(52.5579001031268,20.7668303186539,15.0542094738923));
#34364=CARTESIAN_POINT('Ctrl Pts',(52.5742215619191,20.6527980136261,15.0602279589445));
#34365=CARTESIAN_POINT('Ctrl Pts',(52.5811849082287,20.6041475565505,15.0627956703366));
#34366=CARTESIAN_POINT('Ctrl Pts',(52.5896084284055,20.5557312073288,15.0653633817288));
#34367=CARTESIAN_POINT('Ctrl Pts',(52.5994766191758,20.5076203211785,15.0679310931209));
#34368=CARTESIAN_POINT('Ctrl Pts',(52.6157379830066,20.4283404772714,15.0721623134258));
#34369=CARTESIAN_POINT('Ctrl Pts',(52.6359615079926,20.3497184298317,15.0763935337307));
#34370=CARTESIAN_POINT('Ctrl Pts',(52.6600793886806,20.2721801165656,15.0806247540357));
#34371=CARTESIAN_POINT('Ctrl Pts',(52.6841626860156,20.1947529878137,15.0848499070668));
#34372=CARTESIAN_POINT('Ctrl Pts',(52.7121291114251,20.1184069470735,15.089075060098));
#34373=CARTESIAN_POINT('Ctrl Pts',(52.7438598840222,20.0435576195735,15.0933002131291));
#34374=CARTESIAN_POINT('Ctrl Pts',(52.7756721716968,19.9685160071644,15.0975362204083));
#34375=CARTESIAN_POINT('Ctrl Pts',(52.8112680710964,19.8949792689268,15.1017722276875));
#34376=CARTESIAN_POINT('Ctrl Pts',(52.8504775292819,19.8233507753465,15.1060082349667));
#34377=CARTESIAN_POINT('Ctrl Pts',(52.889516161102,19.7520343502256,15.1102257869609));
#34378=CARTESIAN_POINT('Ctrl Pts',(52.9321367130421,19.6826099912273,15.114443338955));
#34379=CARTESIAN_POINT('Ctrl Pts',(52.9781239927611,19.6154539872754,15.1186608909492));
#34380=CARTESIAN_POINT('Ctrl Pts',(53.0240960885265,19.5483201567083,15.1228770504036));
#34381=CARTESIAN_POINT('Ctrl Pts',(53.0734324420786,19.4834535771597,15.1270932098581));
#34382=CARTESIAN_POINT('Ctrl Pts',(53.1258741064872,19.4212022342096,15.1313093693125));
#34383=CARTESIAN_POINT('Ctrl Pts',(53.1783145213172,19.3589523745828,15.1355254283044));
#34384=CARTESIAN_POINT('Ctrl Pts',(53.2338597995003,19.2993179825095,15.1397414872963));
#34385=CARTESIAN_POINT('Ctrl Pts',(53.2922111415219,19.2426134560496,15.1439575462882));
#34386=CARTESIAN_POINT('Ctrl Pts',(53.3510401265597,19.185444766811,15.1482081164167));
#34387=CARTESIAN_POINT('Ctrl Pts',(53.4127209934834,19.1312544760597,15.1524586865452));
#34388=CARTESIAN_POINT('Ctrl Pts',(53.4769115317551,19.0803250879643,15.1567092566737));
#34389=CARTESIAN_POINT('Ctrl Pts',(53.5406734643213,19.0297357597422,15.1609314453824));
#34390=CARTESIAN_POINT('Ctrl Pts',(53.6069112378669,18.9823641429786,15.1651536340912));
#34391=CARTESIAN_POINT('Ctrl Pts',(53.6752597219263,18.9384439261448,15.1693758228));
#34392=CARTESIAN_POINT('Ctrl Pts',(53.7442973605264,18.8940808638365,15.1736405836383));
#34393=CARTESIAN_POINT('Ctrl Pts',(53.8154880922254,18.8532394355534,15.1779053444766));
#34394=CARTESIAN_POINT('Ctrl Pts',(53.8884312921365,18.8161123523178,15.182170105315));
#34395=CARTESIAN_POINT('Ctrl Pts',(53.9613744920476,18.7789852690823,15.1864348661533));
#34396=CARTESIAN_POINT('Ctrl Pts',(54.0360696941342,18.7455726689773,15.1906996269916));
#34397=CARTESIAN_POINT('Ctrl Pts',(54.1120986250629,18.7160163314102,15.19496438783));
#34398=CARTESIAN_POINT('Ctrl Pts',(54.1875296207276,18.6866924418901,15.1991956081349));
#34399=CARTESIAN_POINT('Ctrl Pts',(54.2645562828332,18.6610543719289,15.2034268284398));
#34400=CARTESIAN_POINT('Ctrl Pts',(54.3427839578555,18.639276101712,15.2076580487448));
#34401=CARTESIAN_POINT('Ctrl Pts',(54.4208994598669,18.6175290600104,15.2118832017759));
#34402=CARTESIAN_POINT('Ctrl Pts',(54.5002121103291,18.5996309493965,15.2161083548071));
#34403=CARTESIAN_POINT('Ctrl Pts',(54.580308280633,18.5857073270428,15.2203335078382));
#34404=CARTESIAN_POINT('Ctrl Pts',(54.660610214774,18.5717479354638,15.2245695151174));
#34405=CARTESIAN_POINT('Ctrl Pts',(54.7416992573065,18.5617836439258,15.2288055223966));
#34406=CARTESIAN_POINT('Ctrl Pts',(54.8231442756635,18.5558902842202,15.2330415296758));
#34407=CARTESIAN_POINT('Ctrl Pts',(54.9042344572768,18.5500226004934,15.2372590816699));
#34408=CARTESIAN_POINT('Ctrl Pts',(54.9856770533162,18.5481904923178,15.2414766336641));
#34409=CARTESIAN_POINT('Ctrl Pts',(55.0670392105314,18.5504171795485,15.2456941856582));
#34410=CARTESIAN_POINT('Ctrl Pts',(55.1483745038132,18.5526431315777,15.2499103451127));
#34411=CARTESIAN_POINT('Ctrl Pts',(55.2296289466304,18.5589252050102,15.2541265045671));
#34412=CARTESIAN_POINT('Ctrl Pts',(55.3103697425097,18.5692345088564,15.2583426640215));
#34413=CARTESIAN_POINT('Ctrl Pts',(55.3911086144995,18.5795435670528,15.2625587230134));
#34414=CARTESIAN_POINT('Ctrl Pts',(55.4713334028487,18.5938796048835,15.2667747820053));
#34415=CARTESIAN_POINT('Ctrl Pts',(55.5506179235651,18.6121620339209,15.2709908409972));
#34416=CARTESIAN_POINT('Ctrl Pts',(55.6305514387403,18.6305941163211,15.2752414111256));
#34417=CARTESIAN_POINT('Ctrl Pts',(55.7095287507911,18.6530374034561,15.2794919812541));
#34418=CARTESIAN_POINT('Ctrl Pts',(55.7871269356959,18.6793575378568,15.2837425513826));
#34419=CARTESIAN_POINT('Ctrl Pts',(55.8642069908936,18.7055019304726,15.2879647400913));
#34420=CARTESIAN_POINT('Ctrl Pts',(55.9399258661526,18.7354713256712,15.2921869288001));
#34421=CARTESIAN_POINT('Ctrl Pts',(56.0138892264417,18.7690856389127,15.2964091175088));
#34422=CARTESIAN_POINT('Ctrl Pts',(56.0885983558037,18.803038883689,15.3006738783472));
#34423=CARTESIAN_POINT('Ctrl Pts',(56.1615159377876,18.8407107403156,15.3049386391855));
#34424=CARTESIAN_POINT('Ctrl Pts',(56.2322628222139,18.8818690817163,15.3092034000238));
#34425=CARTESIAN_POINT('Ctrl Pts',(56.3030097066402,18.9230274231169,15.3134681608622));
#34426=CARTESIAN_POINT('Ctrl Pts',(56.3715855247913,18.9676719325829,15.3177329217005));
#34427=CARTESIAN_POINT('Ctrl Pts',(56.4376443516593,19.0155280379551,15.3219976825388));
#34428=CARTESIAN_POINT('Ctrl Pts',(56.5031836538988,19.0630077753757,15.3262289028438));
#34429=CARTESIAN_POINT('Ctrl Pts',(56.5664912053607,19.113826780033,15.3304601231487));
#34430=CARTESIAN_POINT('Ctrl Pts',(56.6272068319805,19.1677477859323,15.3346913434536));
#34431=CARTESIAN_POINT('Ctrl Pts',(56.6878353966413,19.2215914728832,15.3389164964848));
#34432=CARTESIAN_POINT('Ctrl Pts',(56.7458790732919,19.278528020792,15.3431416495159));
#34433=CARTESIAN_POINT('Ctrl Pts',(56.8010080858906,19.3382779641117,15.3473668025471));
#34434=CARTESIAN_POINT('Ctrl Pts',(56.8562787227033,19.3981814026304,15.3516028098263));
#34435=CARTESIAN_POINT('Ctrl Pts',(56.9086193225069,19.460912427944,15.3558388171055));
#34436=CARTESIAN_POINT('Ctrl Pts',(56.9577323992554,19.5261499048731,15.3600748243847));
#34437=CARTESIAN_POINT('Ctrl Pts',(57.0066315019075,19.5911031574955,15.3642923763788));
#34438=CARTESIAN_POINT('Ctrl Pts',(57.0523308580345,19.6585406983729,15.368509928373));
#34439=CARTESIAN_POINT('Ctrl Pts',(57.0945762550086,19.728111419206,15.3727274803671));
#34440=CARTESIAN_POINT('Ctrl Pts',(57.1368077035136,19.7976591693698,15.3769436398216));
#34441=CARTESIAN_POINT('Ctrl Pts',(57.1755872164572,19.8693383037118,15.381159799276));
#34442=CARTESIAN_POINT('Ctrl Pts',(57.2107043973718,19.9427695060011,15.3853759587305));
#34443=CARTESIAN_POINT('Ctrl Pts',(57.2458207415151,20.0161989585736,15.3895920177224));
#34444=CARTESIAN_POINT('Ctrl Pts',(57.2772747275535,20.0913799761822,15.3938080767143));
#34445=CARTESIAN_POINT('Ctrl Pts',(57.3049029824672,20.1679107671566,15.3980241357062));
#34446=CARTESIAN_POINT('Ctrl Pts',(57.3327573922996,20.2450680115523,15.4022747058346));
#34447=CARTESIAN_POINT('Ctrl Pts',(57.3567229718169,20.3235967830605,15.4065252759631));
#34448=CARTESIAN_POINT('Ctrl Pts',(57.3766832942771,20.403068874405,15.4107758460916));
#34449=CARTESIAN_POINT('Ctrl Pts',(57.3965103399598,20.4820103238091,15.4149980348003));
#34450=CARTESIAN_POINT('Ctrl Pts',(57.4123854216895,20.5618820616089,15.4192202235091));
#34451=CARTESIAN_POINT('Ctrl Pts',(57.4242460358015,20.6422551077925,15.4234424122179));
#34452=CARTESIAN_POINT('Ctrl Pts',(57.4362262399262,20.7234385516095,15.4277071730562));
#34453=CARTESIAN_POINT('Ctrl Pts',(57.444110518731,20.8051329864981,15.4319719338945));
#34454=CARTESIAN_POINT('Ctrl Pts',(57.4478883300894,20.8868939726969,15.4362366947329));
#34455=CARTESIAN_POINT('Ctrl Pts',(57.4516661414477,20.9686549588957,15.4405014555712));
#34456=CARTESIAN_POINT('Ctrl Pts',(57.4513375515427,21.0504820148687,15.4447662164095));
#34457=CARTESIAN_POINT('Ctrl Pts',(57.446945697521,21.1319356031678,15.4490309772479));
#34458=CARTESIAN_POINT('Ctrl Pts',(57.4425883835667,21.2127485935758,15.4532621975528));
#34459=CARTESIAN_POINT('Ctrl Pts',(57.4342151951589,21.2934970116553,15.4574934178577));
#34460=CARTESIAN_POINT('Ctrl Pts',(57.421830197336,21.3737495756141,15.4617246381627));
#34461=CARTESIAN_POINT('Ctrl Pts',(57.4094629587331,21.4538870630131,15.4659497911938));
#34462=CARTESIAN_POINT('Ctrl Pts',(57.3930954062288,21.5335296528248,15.470174944225));
#34463=CARTESIAN_POINT('Ctrl Pts',(57.37278354489,21.612248723232,15.4744000972561));
#34464=CARTESIAN_POINT('Ctrl Pts',(57.3524195031971,21.691170019762,15.4786361045353));
#34465=CARTESIAN_POINT('Ctrl Pts',(57.3280908930137,21.7691625748633,15.4828721118145));
#34466=CARTESIAN_POINT('Ctrl Pts',(57.2999062400462,21.8458023037308,15.4871081190937));
#34467=CARTESIAN_POINT('Ctrl Pts',(57.271844380967,21.9221081313682,15.4913256710879));
#34468=CARTESIAN_POINT('Ctrl Pts',(57.2399601625843,21.9970724541366,15.495543223082));
#34469=CARTESIAN_POINT('Ctrl Pts',(57.2044107588722,22.0702912950073,15.4997607750762));
#34470=CARTESIAN_POINT('Ctrl Pts',(57.1688730927645,22.1434859606825,15.5039769345306));
#34471=CARTESIAN_POINT('Ctrl Pts',(57.1296728474387,22.2149358710432,15.5081930939851));
#34472=CARTESIAN_POINT('Ctrl Pts',(57.08701465625,22.284258569992,15.5124092534395));
#34473=CARTESIAN_POINT('Ctrl Pts',(57.0443574815196,22.3535796171212,15.5166253124314));
#34474=CARTESIAN_POINT('Ctrl Pts',(56.998242769351,22.4207731582393,15.5208413714233));
#34475=CARTESIAN_POINT('Ctrl Pts',(56.9489195348987,22.4854840613384,15.5250574304152));
#34476=CARTESIAN_POINT('Ctrl Pts',(56.8991925582587,22.5507246645245,15.5293080005437));
#34477=CARTESIAN_POINT('Ctrl Pts',(56.8462045673086,22.6134414068766,15.5335585706721));
#34478=CARTESIAN_POINT('Ctrl Pts',(56.7902522278264,22.6733042791921,15.5378091408006));
#34479=CARTESIAN_POINT('Ctrl Pts',(56.7346734868929,22.7327674419971,15.5420313295094));
#34480=CARTESIAN_POINT('Ctrl Pts',(56.6761702435895,22.7894144475848,15.5462535182181));
#34481=CARTESIAN_POINT('Ctrl Pts',(56.6150690512437,22.8429601758353,15.5504757069269));
#34482=CARTESIAN_POINT('Ctrl Pts',(56.5533517784577,22.8970458031379,15.5547404677652));
#34483=CARTESIAN_POINT('Ctrl Pts',(56.4889842527477,22.9479669596254,15.5590052286035));
#34484=CARTESIAN_POINT('Ctrl Pts',(56.4223341919505,22.9954738024861,15.5632699894419));
#34485=CARTESIAN_POINT('Ctrl Pts',(56.3556841311534,23.0429806453468,15.5675347502802));
#34486=CARTESIAN_POINT('Ctrl Pts',(56.2867519757585,23.087072969091,15.5717995111185));
#34487=CARTESIAN_POINT('Ctrl Pts',(56.2159304305799,23.1275486922724,15.5760642719569));
#34488=CARTESIAN_POINT('Ctrl Pts',(56.145665866787,23.1677060910748,15.5802954922618));
#34489=CARTESIAN_POINT('Ctrl Pts',(56.0732780641252,23.2044541975874,15.5845267125667));
#34490=CARTESIAN_POINT('Ctrl Pts',(55.999131604964,23.2375625769936,15.5887579328716));
#34491=CARTESIAN_POINT('Ctrl Pts',(55.9250914666357,23.2706234813009,15.5929830859028));
#34492=CARTESIAN_POINT('Ctrl Pts',(55.8492981012134,23.3000548360924,15.597208238934));
#34493=CARTESIAN_POINT('Ctrl Pts',(55.7721420190791,23.325671290697,15.6014333919651));
#34494=CARTESIAN_POINT('Ctrl Pts',(55.6947877260761,23.3513535529422,15.6056693992443));
#34495=CARTESIAN_POINT('Ctrl Pts',(55.6160641188624,23.3732010606255,15.6099054065235));
#34496=CARTESIAN_POINT('Ctrl Pts',(55.5363863735001,23.391075052842,15.6141414138027));
#34497=CARTESIAN_POINT('Ctrl Pts',(55.4570557652895,23.4088711722884,15.6183589657969));
#34498=CARTESIAN_POINT('Ctrl Pts',(55.3767797702377,23.4227282170112,15.622576517791));
#34499=CARTESIAN_POINT('Ctrl Pts',(55.2959830472944,23.4325592049762,15.6267940697852));
#34500=CARTESIAN_POINT('Ctrl Pts',(55.215213001591,23.4423869469725,15.6310102292396));
#34501=CARTESIAN_POINT('Ctrl Pts',(55.1339230305855,23.4481912159273,15.6352263886941));
#34502=CARTESIAN_POINT('Ctrl Pts',(55.0525454440931,23.449936575976,15.6394425481485));
#34503=CARTESIAN_POINT('Ctrl Pts',(54.9711697966636,23.4516818944363,15.6436586071404));
#34504=CARTESIAN_POINT('Ctrl Pts',(54.8897070027367,23.4493684874252,15.6478746661323));
#34505=CARTESIAN_POINT('Ctrl Pts',(54.8085904782411,23.4430130259538,15.6520907251242));
#34506=CARTESIAN_POINT('Ctrl Pts',(54.7268099631656,23.4366055409697,15.6563412952527));
#34507=CARTESIAN_POINT('Ctrl Pts',(54.6453818920659,23.4260895439576,15.6605918653811));
#34508=CARTESIAN_POINT('Ctrl Pts',(54.5647444090101,23.4115353658016,15.6648424355096));
#34509=CARTESIAN_POINT('Ctrl Pts',(54.4846453493145,23.397078367136,15.6690646242184));
#34510=CARTESIAN_POINT('Ctrl Pts',(54.4053267954773,23.3786371161955,15.6732868129271));
#34511=CARTESIAN_POINT('Ctrl Pts',(54.3272053798535,23.3563313962815,15.6775090016359));
#34512=CARTESIAN_POINT('Ctrl Pts',(54.2482962696811,23.3338007688459,15.6817737624742));
#34513=CARTESIAN_POINT('Ctrl Pts',(54.1706090348107,23.3073274599816,15.6860385233125));
#34514=CARTESIAN_POINT('Ctrl Pts',(54.0945529866508,23.2770849689937,15.6903032841509));
#34515=CARTESIAN_POINT('Ctrl Pts',(54.018496938491,23.2468424780058,15.6945680449892));
#34516=CARTESIAN_POINT('Ctrl Pts',(53.9440724885446,23.212831063588,15.6988328058275));
#34517=CARTESIAN_POINT('Ctrl Pts',(53.8716623659161,23.1752711172426,15.7030975666659));
#34518=CARTESIAN_POINT('Ctrl Pts',(53.7998217181607,23.1380065639293,15.7073287869708));
#34519=CARTESIAN_POINT('Ctrl Pts',(53.7296944118989,23.0971093974879,15.7115600072757));
#34520=CARTESIAN_POINT('Ctrl Pts',(53.6616717511369,23.0527610061317,15.7157912275807));
#34521=CARTESIAN_POINT('Ctrl Pts',(53.5937466301093,23.0084762072647,15.7200163806118));
#34522=CARTESIAN_POINT('Ctrl Pts',(53.527920546952,22.9607502639732,15.724241533643));
#34523=CARTESIAN_POINT('Ctrl Pts',(53.4645609831116,22.9098107957116,15.7284666866741));
#34524=CARTESIAN_POINT('Ctrl Pts',(53.4010386511023,22.8587404660069,15.7327026939533));
#34525=CARTESIAN_POINT('Ctrl Pts',(53.3399959434504,22.8044403024048,15.7369387012325));
#34526=CARTESIAN_POINT('Ctrl Pts',(53.281774569503,22.7471839113251,15.7411747085117));
#34527=CARTESIAN_POINT('Ctrl Pts',(53.2238068523557,22.6901769728428,15.7453922605059));
#34528=CARTESIAN_POINT('Ctrl Pts',(53.1686362757324,22.630239834564,15.7496098125));
#34529=CARTESIAN_POINT('Ctrl Pts',(53.1165661843707,22.5676821464009,15.7538273644942));
#34530=CARTESIAN_POINT('Ctrl Pts',(53.0645132853686,22.5051451133632,15.7580435239486));
#34531=CARTESIAN_POINT('Ctrl Pts',(53.0155591358799,22.4399896057526,15.7622596834031));
#34532=CARTESIAN_POINT('Ctrl Pts',(52.9699679181935,22.3725596514674,15.7664758428575));
#34533=CARTESIAN_POINT('Ctrl Pts',(52.9243777868535,22.3051313039015,15.7706919018494));
#34534=CARTESIAN_POINT('Ctrl Pts',(52.8821506874837,22.235429003185,15.7749079608413));
#34535=CARTESIAN_POINT('Ctrl Pts',(52.843507620092,22.1638259600982,15.7791240198332));
#34536=CARTESIAN_POINT('Ctrl Pts',(52.8045482345037,22.0916368003549,15.7833745899616));
#34537=CARTESIAN_POINT('Ctrl Pts',(52.7692320688656,22.0175160515675,15.7876251600901));
#34538=CARTESIAN_POINT('Ctrl Pts',(52.7377375999625,21.9418699928209,15.7918757302186));
#34539=CARTESIAN_POINT('Ctrl Pts',(52.7064534223177,21.8667290292682,15.7960979189273));
#34540=CARTESIAN_POINT('Ctrl Pts',(52.6789401616835,21.7900835257579,15.8003201076361));
#34541=CARTESIAN_POINT('Ctrl Pts',(52.6553230790539,21.7123485006532,15.8045422963448));
#34542=CARTESIAN_POINT('Ctrl Pts',(52.6314678664943,21.6338296769573,15.8088070571832));
#34543=CARTESIAN_POINT('Ctrl Pts',(52.6115879618003,21.5541997081427,15.8130718180215));
#34544=CARTESIAN_POINT('Ctrl Pts',(52.5957595223028,21.4738965872448,15.8173365788598));
#34545=CARTESIAN_POINT('Ctrl Pts',(52.5799310828053,21.3935934663469,15.8216013396982));
#34546=CARTESIAN_POINT('Ctrl Pts',(52.5681541142666,21.3126176793944,15.8258661005365));
#34547=CARTESIAN_POINT('Ctrl Pts',(52.5604509600289,21.2314103100038,15.8301308613749));
#34548=CARTESIAN_POINT('Ctrl Pts',(52.5532009537332,21.1549800684201,15.8341447421792));
#34549=CARTESIAN_POINT('Ctrl Pts',(52.549542003553,21.0782038541672,15.8381586229836));
#34550=CARTESIAN_POINT('Ctrl Pts',(52.549500359537,21.0013274376061,15.8421725037879));
#34551=CARTESIAN_POINT('',(52.5495245738618,21.0013531866909,16.6421724750583));
#34552=CARTESIAN_POINT('Ctrl Pts',(52.5495003595367,21.0013274370615,15.8421725038163));
#34553=CARTESIAN_POINT('Ctrl Pts',(52.549457014999,20.921311761013,15.8463502920186));
#34554=CARTESIAN_POINT('Ctrl Pts',(52.5533370002312,20.8411382049865,15.8505280802208));
#34555=CARTESIAN_POINT('Ctrl Pts',(52.5611603672117,20.7612291987261,15.854705868423));
#34556=CARTESIAN_POINT('Ctrl Pts',(52.569154716791,20.6795737513753,15.8589749637422));
#34557=CARTESIAN_POINT('Ctrl Pts',(52.5812669392635,20.5981950523709,15.8632440590614));
#34558=CARTESIAN_POINT('Ctrl Pts',(52.5974621330943,20.5175458072683,15.8675131543806));
#34559=CARTESIAN_POINT('Ctrl Pts',(52.6132746688864,20.4388021325641,15.8716813800431));
#34560=CARTESIAN_POINT('Ctrl Pts',(52.6329792633433,20.3607543185169,15.8758496057055));
#34561=CARTESIAN_POINT('Ctrl Pts',(52.6564910916385,20.2838182867246,15.880017831368));
#34562=CARTESIAN_POINT('Ctrl Pts',(52.6799915393678,20.2069194947233,15.8841840394602));
#34563=CARTESIAN_POINT('Ctrl Pts',(52.707295425388,20.1311318729757,15.8883502475524));
#34564=CARTESIAN_POINT('Ctrl Pts',(52.7382674978157,20.056858261679,15.8925164556445));
#34565=CARTESIAN_POINT('Ctrl Pts',(52.7692346193451,19.9825965230491,15.8966819977667));
#34566=CARTESIAN_POINT('Ctrl Pts',(52.8038685787417,19.909848754533,15.9008475398888));
#34567=CARTESIAN_POINT('Ctrl Pts',(52.8419857912841,19.8389983096565,15.9050130820109));
#34568=CARTESIAN_POINT('Ctrl Pts',(52.8817535957394,19.7650798237683,15.9093590048503));
#34569=CARTESIAN_POINT('Ctrl Pts',(52.9253129412092,19.6932272251965,15.9137049276897));
#34570=CARTESIAN_POINT('Ctrl Pts',(52.9724028570058,19.6238459113451,15.9180508505291));
#34571=CARTESIAN_POINT('Ctrl Pts',(53.0175954337311,19.5572600978753,15.9222216681668));
#34572=CARTESIAN_POINT('Ctrl Pts',(53.0660391913371,19.4929506050044,15.9263924858045));
#34573=CARTESIAN_POINT('Ctrl Pts',(53.1174612432284,19.4312431420858,15.9305633034422));
#34574=CARTESIAN_POINT('Ctrl Pts',(53.1689180539389,19.3694939679078,15.9347369403509));
#34575=CARTESIAN_POINT('Ctrl Pts',(53.2233568382817,19.3103506702542,15.9389105772595));
#34576=CARTESIAN_POINT('Ctrl Pts',(53.28046768838,19.2541022712384,15.9430842141681));
#34577=CARTESIAN_POINT('Ctrl Pts',(53.3376669344287,19.1977668111707,15.9472643110157));
#34578=CARTESIAN_POINT('Ctrl Pts',(53.3975461352792,19.1443354966691,15.9514444078632));
#34579=CARTESIAN_POINT('Ctrl Pts',(53.4597629127033,19.0940566732151,15.9556245047107));
#34580=CARTESIAN_POINT('Ctrl Pts',(53.4674016628953,19.0878836216973,15.9561377218351));
#34581=CARTESIAN_POINT('Ctrl Pts',(53.4750756158463,19.0817580361128,15.9566509389594));
#34582=CARTESIAN_POINT('Ctrl Pts',(53.4827841103334,19.0756803295338,15.9571641560838));
#34583=CARTESIAN_POINT('Ctrl Pts',(53.5463368190137,19.0255726572375,15.9613953763887));
#34584=CARTESIAN_POINT('Ctrl Pts',(53.6124936397374,18.978522764802,15.9656265966936));
#34585=CARTESIAN_POINT('Ctrl Pts',(53.6809280800406,18.934812473412,15.9698578169986));
#34586=CARTESIAN_POINT('Ctrl Pts',(53.7492643901463,18.8911648595205,15.9740829700297));
#34587=CARTESIAN_POINT('Ctrl Pts',(53.8198714449031,18.8508475839993,15.9783081230609));
#34588=CARTESIAN_POINT('Ctrl Pts',(53.8923904411771,18.8141017143508,15.982533276092));
#34589=CARTESIAN_POINT('Ctrl Pts',(53.9650957358331,18.7772614460425,15.9867692833712));
#34590=CARTESIAN_POINT('Ctrl Pts',(54.0397224333459,18.7440112438922,15.9910052906504));
#34591=CARTESIAN_POINT('Ctrl Pts',(54.1158804456856,18.7145497459627,15.9952412979296));
#34592=CARTESIAN_POINT('Ctrl Pts',(54.1917066555205,18.6852166048339,15.9994588499238));
#34593=CARTESIAN_POINT('Ctrl Pts',(54.269050431445,18.6596394002223,16.0036764019179));
#34594=CARTESIAN_POINT('Ctrl Pts',(54.3475046489063,18.6379669632283,16.0078939539121));
#34595=CARTESIAN_POINT('Ctrl Pts',(54.4259329625698,18.6163016819799,16.0121101133665));
#34596=CARTESIAN_POINT('Ctrl Pts',(54.505470541884,18.5985387317467,16.0163262728209));
#34597=CARTESIAN_POINT('Ctrl Pts',(54.5856950720646,18.5847770958588,16.0205424322754));
#34598=CARTESIAN_POINT('Ctrl Pts',(54.6659176906573,18.5710157878827,16.0247584912673));
#34599=CARTESIAN_POINT('Ctrl Pts',(54.746826769155,18.5612556821962,16.0289745502592));
#34600=CARTESIAN_POINT('Ctrl Pts',(54.8279911923932,18.5555443918726,16.033190609251));
#34601=CARTESIAN_POINT('Ctrl Pts',(54.9098199982933,18.5497863509885,16.0374411793795));
#34602=CARTESIAN_POINT('Ctrl Pts',(54.9919078711413,18.5481437653839,16.041691749508));
#34603=CARTESIAN_POINT('Ctrl Pts',(55.0738110835159,18.5506118776416,16.0459423196365));
#34604=CARTESIAN_POINT('Ctrl Pts',(55.1551674211474,18.5530635101031,16.0501645083452));
#34605=CARTESIAN_POINT('Ctrl Pts',(55.2363410937179,18.5595710135019,16.054386697054));
#34606=CARTESIAN_POINT('Ctrl Pts',(55.3169023351057,18.5700775403308,16.0586088857627));
#34607=CARTESIAN_POINT('Ctrl Pts',(55.3982758716903,18.5806900039742,16.0628736466011));
#34608=CARTESIAN_POINT('Ctrl Pts',(55.4790240793993,18.5953825019187,16.0671384074394));
#34609=CARTESIAN_POINT('Ctrl Pts',(55.5587164881322,18.6140439786347,16.0714031682777));
#34610=CARTESIAN_POINT('Ctrl Pts',(55.6384088968652,18.6327054553507,16.0756679291161));
#34611=CARTESIAN_POINT('Ctrl Pts',(55.7170450613846,18.6553357158492,16.0799326899544));
#34612=CARTESIAN_POINT('Ctrl Pts',(55.7942138663665,18.6817733966518,16.0841974507928));
#34613=CARTESIAN_POINT('Ctrl Pts',(55.870775771459,18.708003156319,16.0884286710977));
#34614=CARTESIAN_POINT('Ctrl Pts',(55.9461804281699,18.7380789780496,16.0926598914026));
#34615=CARTESIAN_POINT('Ctrl Pts',(56.0200140090283,18.7718793409274,16.0968911117075));
#34616=CARTESIAN_POINT('Ctrl Pts',(56.0937417176992,18.8056312364505,16.1011162647387));
#34617=CARTESIAN_POINT('Ctrl Pts',(56.1659024056086,18.8430968741381,16.1053414177699));
#34618=CARTESIAN_POINT('Ctrl Pts',(56.2360989684194,18.8841054869695,16.109566570801));
#34619=CARTESIAN_POINT('Ctrl Pts',(56.3064758633741,18.9252194492764,16.1138025780802));
#34620=CARTESIAN_POINT('Ctrl Pts',(56.3748780843435,18.9698944544936,16.1180385853594));
#34621=CARTESIAN_POINT('Ctrl Pts',(56.4409272143529,19.0179104427556,16.1222745926386));
#34622=CARTESIAN_POINT('Ctrl Pts',(56.5066885838746,19.065717236677,16.1264921446328));
#34623=CARTESIAN_POINT('Ctrl Pts',(56.5701169401544,19.1168356941034,16.1307096966269));
#34624=CARTESIAN_POINT('Ctrl Pts',(56.6308664782144,19.1710044340577,16.1349272486211));
#34625=CARTESIAN_POINT('Ctrl Pts',(56.6915959581589,19.2251552887263,16.1391434080755));
#34626=CARTESIAN_POINT('Ctrl Pts',(56.749648029612,19.2823541167226,16.1433595675299));
#34627=CARTESIAN_POINT('Ctrl Pts',(56.8047105349806,19.3422997451499,16.1475757269844));
#34628=CARTESIAN_POINT('Ctrl Pts',(56.8597717283214,19.4022439451945,16.1517917859763));
#34629=CARTESIAN_POINT('Ctrl Pts',(56.9118431835207,19.4649344723882,16.1560078449682));
#34630=CARTESIAN_POINT('Ctrl Pts',(56.9606511343337,19.5300349053682,16.1602239039601));
#34631=CARTESIAN_POINT('Ctrl Pts',(57.0098586094086,19.5956682269862,16.1644744740885));
#34632=CARTESIAN_POINT('Ctrl Pts',(57.0557486051443,19.663750715539,16.168725044217));
#34633=CARTESIAN_POINT('Ctrl Pts',(57.0980845201935,19.7339069559766,16.1729756143455));
#34634=CARTESIAN_POINT('Ctrl Pts',(57.1401377547226,19.8035947572058,16.1771978030542));
#34635=CARTESIAN_POINT('Ctrl Pts',(57.1786840580431,19.8753282585799,16.181419991763));
#34636=CARTESIAN_POINT('Ctrl Pts',(57.2135381668652,19.9487155314421,16.1856421804717));
#34637=CARTESIAN_POINT('Ctrl Pts',(57.2487437080225,20.0228427647149,16.1899069413101));
#34638=CARTESIAN_POINT('Ctrl Pts',(57.2801819930715,20.0986568582413,16.1941717021484));
#34639=CARTESIAN_POINT('Ctrl Pts',(57.3077129245077,20.1757358990832,16.1984364629868));
#34640=CARTESIAN_POINT('Ctrl Pts',(57.3352438559439,20.2528149399252,16.2027012238251));
#34641=CARTESIAN_POINT('Ctrl Pts',(57.3588673561866,20.3311584482512,16.2069659846634));
#34642=CARTESIAN_POINT('Ctrl Pts',(57.3784960928316,20.4103334956227,16.2112307455018));
#34643=CARTESIAN_POINT('Ctrl Pts',(57.3979704577963,20.48888586486,16.2154619658067));
#34644=CARTESIAN_POINT('Ctrl Pts',(57.413585740031,20.5685512919107,16.2196931861116));
#34645=CARTESIAN_POINT('Ctrl Pts',(57.4252196594165,20.6489161730017,16.2239244064165));
#34646=CARTESIAN_POINT('Ctrl Pts',(57.4368368965758,20.7291658164779,16.2281495594477));
#34647=CARTESIAN_POINT('Ctrl Pts',(57.444484043332,20.8101124657808,16.2323747124788));
#34648=CARTESIAN_POINT('Ctrl Pts',(57.4480892655331,20.8913298661928,16.23659986551));
#34649=CARTESIAN_POINT('Ctrl Pts',(57.4517037494048,20.9727559108369,16.2408358727892));
#34650=CARTESIAN_POINT('Ctrl Pts',(57.4512554077082,21.0544536397797,16.2450718800684));
#34651=CARTESIAN_POINT('Ctrl Pts',(57.4467239565788,21.1359857724297,16.2493078873476));
#34652=CARTESIAN_POINT('Ctrl Pts',(57.4422122479137,21.2171626887996,16.2535254393418));
#34653=CARTESIAN_POINT('Ctrl Pts',(57.4336529517075,21.2981749811907,16.2577429913359));
#34654=CARTESIAN_POINT('Ctrl Pts',(57.4210781864923,21.3785903655553,16.2619605433301));
#34655=CARTESIAN_POINT('Ctrl Pts',(57.4085075731784,21.4589791985895,16.2661767027845));
#34656=CARTESIAN_POINT('Ctrl Pts',(57.3919241955128,21.5387710560022,16.2703928622389));
#34657=CARTESIAN_POINT('Ctrl Pts',(57.3714118509523,21.6175403494209,16.2746090216934));
#34658=CARTESIAN_POINT('Ctrl Pts',(57.3508999951595,21.6963077659269,16.2788250806853));
#34659=CARTESIAN_POINT('Ctrl Pts',(57.3264594768472,21.7740522172467,16.2830411396772));
#34660=CARTESIAN_POINT('Ctrl Pts',(57.2982245271079,21.8503612602887,16.2872571986691));
#34661=CARTESIAN_POINT('Ctrl Pts',(57.2697584562651,21.9272949416033,16.2915077687976));
#34662=CARTESIAN_POINT('Ctrl Pts',(57.2374356989915,22.0027691512276,16.295758338926));
#34663=CARTESIAN_POINT('Ctrl Pts',(57.201443401874,22.0763815301023,16.3000089090545));
#34664=CARTESIAN_POINT('Ctrl Pts',(57.1656914283979,22.1495023928372,16.3042310977633));
#34665=CARTESIAN_POINT('Ctrl Pts',(57.1263190506184,22.2207858312159,16.308453286472));
#34666=CARTESIAN_POINT('Ctrl Pts',(57.0835551270548,22.2898636681928,16.3126754751808));
#34667=CARTESIAN_POINT('Ctrl Pts',(57.0403600168672,22.3596380137413,16.3169402360191));
#34668=CARTESIAN_POINT('Ctrl Pts',(56.9937048585003,22.4271616299197,16.3212049968574));
#34669=CARTESIAN_POINT('Ctrl Pts',(56.9438681942022,22.4920880314409,16.3254697576958));
#34670=CARTESIAN_POINT('Ctrl Pts',(56.8940315299041,22.557014432962,16.3297345185341));
#34671=CARTESIAN_POINT('Ctrl Pts',(56.8410137207801,22.6193432944647,16.3339992793724));
#34672=CARTESIAN_POINT('Ctrl Pts',(56.7851311750811,22.6787664929208,16.3382640402108));
#34673=CARTESIAN_POINT('Ctrl Pts',(56.7296881218793,22.7377223531489,16.3424952605157));
#34674=CARTESIAN_POINT('Ctrl Pts',(56.6712173592052,22.7940391998182,16.3467264808206));
#34675=CARTESIAN_POINT('Ctrl Pts',(56.6100001086279,22.8473900238494,16.3509577011256));
#34676=CARTESIAN_POINT('Ctrl Pts',(56.5488706393034,22.9006643465329,16.3551828541567));
#34677=CARTESIAN_POINT('Ctrl Pts',(56.4850028513178,22.9509807906114,16.3594080071879));
#34678=CARTESIAN_POINT('Ctrl Pts',(56.4187159489162,22.9980478738736,16.363633160219));
#34679=CARTESIAN_POINT('Ctrl Pts',(56.3522587581308,23.0452358705779,16.3678691674982));
#34680=CARTESIAN_POINT('Ctrl Pts',(56.2833703358447,23.089157450691,16.3721051747774));
#34681=CARTESIAN_POINT('Ctrl Pts',(56.2124071023241,23.1295584679069,16.3763411820566));
#34682=CARTESIAN_POINT('Ctrl Pts',(56.1417530388818,23.1697834674157,16.3805587340508));
#34683=CARTESIAN_POINT('Ctrl Pts',(56.0690426079775,23.2065182779872,16.3847762860449));
#34684=CARTESIAN_POINT('Ctrl Pts',(55.9946564453281,23.2395554928975,16.3889938380391));
#34685=CARTESIAN_POINT('Ctrl Pts',(55.9202948432973,23.272581799671,16.3932099974935));
#34686=CARTESIAN_POINT('Ctrl Pts',(55.8442590328413,23.3019127466807,16.397426156948));
#34687=CARTESIAN_POINT('Ctrl Pts',(55.7669520451756,23.3273879802046,16.4016423164024));
#34688=CARTESIAN_POINT('Ctrl Pts',(55.689646899579,23.3528626067053,16.4058583753943));
#34689=CARTESIAN_POINT('Ctrl Pts',(55.6110710789075,23.3744815579321,16.4100744343862));
#34690=CARTESIAN_POINT('Ctrl Pts',(55.5316439154648,23.392133983946,16.4142904933781));
#34691=CARTESIAN_POINT('Ctrl Pts',(55.4515665899416,23.4099309063453,16.4185410635065));
#34692=CARTESIAN_POINT('Ctrl Pts',(55.370624384555,23.4236959469679,16.422791633635));
#34693=CARTESIAN_POINT('Ctrl Pts',(55.2892568505849,23.4333681851273,16.4270422037635));
#34694=CARTESIAN_POINT('Ctrl Pts',(55.2084326145874,23.4429758409265,16.4312643924722));
#34695=CARTESIAN_POINT('Ctrl Pts',(55.1271891852546,23.4485452133612,16.435486581181));
#34696=CARTESIAN_POINT('Ctrl Pts',(55.0459600100496,23.4500689638205,16.4397087698897));
#34697=CARTESIAN_POINT('Ctrl Pts',(54.9639118049027,23.4516080781837,16.4439735307281));
#34698=CARTESIAN_POINT('Ctrl Pts',(54.8818786285043,23.4490195430659,16.4482382915664));
#34699=CARTESIAN_POINT('Ctrl Pts',(54.8003026417379,23.4423495276277,16.4525030524048));
#34700=CARTESIAN_POINT('Ctrl Pts',(54.7187266549715,23.4356795121894,16.4567678132431));
#34701=CARTESIAN_POINT('Ctrl Pts',(54.6376083270162,23.4249281434262,16.4610325740814));
#34702=CARTESIAN_POINT('Ctrl Pts',(54.5573781172022,23.4101942077079,16.4652973349198));
#34703=CARTESIAN_POINT('Ctrl Pts',(54.477778883927,23.3955761481387,16.4695285552247));
#34704=CARTESIAN_POINT('Ctrl Pts',(54.3987553529978,23.3769831691967,16.4737597755296));
#34705=CARTESIAN_POINT('Ctrl Pts',(54.3207347734857,23.3544742517277,16.4779909958345));
#34706=CARTESIAN_POINT('Ctrl Pts',(54.2428260700237,23.3319976104708,16.4822161488657));
#34707=CARTESIAN_POINT('Ctrl Pts',(54.1659179046154,23.3056163106458,16.4864413018969));
#34708=CARTESIAN_POINT('Ctrl Pts',(54.0904282704373,23.2754405109298,16.490666454928));
#34709=CARTESIAN_POINT('Ctrl Pts',(54.0147447064282,23.2451871907992,16.4949024622072));
#34710=CARTESIAN_POINT('Ctrl Pts',(53.9404874343666,23.211119941561,16.4991384694864));
#34711=CARTESIAN_POINT('Ctrl Pts',(53.8680632558197,23.1734004364531,16.5033744767656));
#34712=CARTESIAN_POINT('Ctrl Pts',(53.7959546123441,23.1358452663362,16.5075920287598));
#34713=CARTESIAN_POINT('Ctrl Pts',(53.7256635417241,23.094669806884,16.5118095807539));
#34714=CARTESIAN_POINT('Ctrl Pts',(53.6575707034229,23.0500814212347,16.5160271327481));
#34715=CARTESIAN_POINT('Ctrl Pts',(53.5895003478277,23.0055077576558,16.5202432922025));
#34716=CARTESIAN_POINT('Ctrl Pts',(53.5236271718488,22.9575236601793,16.524459451657));
#34717=CARTESIAN_POINT('Ctrl Pts',(53.460304442681,22.9063808225987,16.5286756111114));
#34718=CARTESIAN_POINT('Ctrl Pts',(53.3969832223658,22.8552392036485,16.5328916701033));
#34719=CARTESIAN_POINT('Ctrl Pts',(53.3362126890234,22.8009392872248,16.5371077290952));
#34720=CARTESIAN_POINT('Ctrl Pts',(53.2783133538254,22.7437733059042,16.5413237880871));
#34721=CARTESIAN_POINT('Ctrl Pts',(53.2199400755756,22.6861393845018,16.5455743582156));
#34722=CARTESIAN_POINT('Ctrl Pts',(53.1644855702601,22.6255925861026,16.549824928344));
#34723=CARTESIAN_POINT('Ctrl Pts',(53.1122393598967,22.5624692047131,16.5540754984725));
#34724=CARTESIAN_POINT('Ctrl Pts',(53.0603420019414,22.4997673035314,16.5582976871813));
#34725=CARTESIAN_POINT('Ctrl Pts',(53.0116104567288,22.4345235358576,16.56251987589));
#34726=CARTESIAN_POINT('Ctrl Pts',(52.9662859150989,22.367098120427,16.5667420645988));
#34727=CARTESIAN_POINT('Ctrl Pts',(52.9205043682539,22.2989928577131,16.5710068254371));
#34728=CARTESIAN_POINT('Ctrl Pts',(52.8781991674195,22.2286621210014,16.5752715862754));
#34729=CARTESIAN_POINT('Ctrl Pts',(52.8395712689205,22.1565024634328,16.5795363471138));
#34730=CARTESIAN_POINT('Ctrl Pts',(52.8009433704215,22.0843428058643,16.5838011079521));
#34731=CARTESIAN_POINT('Ctrl Pts',(52.765992921951,22.0103546905198,16.5880658687904));
#34732=CARTESIAN_POINT('Ctrl Pts',(52.7348703241554,21.9349533686812,16.5923306296288));
#34733=CARTESIAN_POINT('Ctrl Pts',(52.700383049492,21.8514003788787,16.5970564555181));
#34734=CARTESIAN_POINT('Ctrl Pts',(52.6704856308601,21.7658477178848,16.6017822814074));
#34735=CARTESIAN_POINT('Ctrl Pts',(52.6453875193758,21.6787859132958,16.6065081072968));
#34736=CARTESIAN_POINT('Ctrl Pts',(52.620372265052,21.5920115284962,16.6112183316731));
#34737=CARTESIAN_POINT('Ctrl Pts',(52.6001248278688,21.5037381827685,16.6159285560493));
#34738=CARTESIAN_POINT('Ctrl Pts',(52.5848061128296,21.4144740490969,16.6206387804256));
#34739=CARTESIAN_POINT('Ctrl Pts',(52.5695741644158,21.3257155157731,16.6253223256533));
#34740=CARTESIAN_POINT('Ctrl Pts',(52.5592153803563,21.2359776385129,16.630005870881));
#34741=CARTESIAN_POINT('Ctrl Pts',(52.553839980721,21.1457786338287,16.6346894161087));
#34742=CARTESIAN_POINT('Ctrl Pts',(52.5509771614083,21.0977406329148,16.63718376902));
#34743=CARTESIAN_POINT('Ctrl Pts',(52.5495270008763,21.049572131945,16.6396781219313));
#34744=CARTESIAN_POINT('Ctrl Pts',(52.5495003736302,21.001353204219,16.6421724748426));
#34745=CARTESIAN_POINT('',(52.5495008534978,20.9979547636087,17.4421725287708));
#34746=CARTESIAN_POINT('Ctrl Pts',(52.5527477474802,21.0013508521608,16.6421725037879));
#34747=CARTESIAN_POINT('Ctrl Pts',(52.5552350469976,20.504606588975,16.6679029773045));
#34748=CARTESIAN_POINT('Ctrl Pts',(52.9435499391095,19.1868004307352,16.7359778823908));
#34749=CARTESIAN_POINT('Ctrl Pts',(55.0960917460929,18.1050615266267,16.8463972190466));
#34750=CARTESIAN_POINT('Ctrl Pts',(57.4845327466849,19.5110408269755,16.9734305137557));
#34751=CARTESIAN_POINT('Ctrl Pts',(57.5982440738356,22.2802461173785,17.1004638084647));
#34752=CARTESIAN_POINT('Ctrl Pts',(55.3331166026311,23.8773139761478,17.2274971031737));
#34753=CARTESIAN_POINT('Ctrl Pts',(53.0286539046507,22.9472535002863,17.3414000016147));
#34754=CARTESIAN_POINT('Ctrl Pts',(52.5557259094851,21.5611067451181,17.4129584684862));
#34755=CARTESIAN_POINT('Ctrl Pts',(52.5512853518551,20.9979567345713,17.4421725037879));
#34756=CARTESIAN_POINT('',(52.5495000073192,20.9998106024674,18.2421725037368));
#34757=CARTESIAN_POINT('Ctrl Pts',(52.5495008534978,20.9979547636087,17.4421725287708));
#34758=CARTESIAN_POINT('Ctrl Pts',(52.5495817226398,20.9010614341234,17.44719535461));
#34759=CARTESIAN_POINT('Ctrl Pts',(52.5554132275324,20.8044154643906,17.4522181804492));
#34760=CARTESIAN_POINT('Ctrl Pts',(52.5668846255356,20.7086242553934,17.4572410062884));
#34761=CARTESIAN_POINT('Ctrl Pts',(52.5785010996755,20.6116215969704,17.4623273546527));
#34762=CARTESIAN_POINT('Ctrl Pts',(52.5959009390986,20.5154955018815,17.467413703017));
#34763=CARTESIAN_POINT('Ctrl Pts',(52.6189200695926,20.4208552728281,17.4725000513813));
#34764=CARTESIAN_POINT('Ctrl Pts',(52.6325930837622,20.3646404130529,17.4755212651181));
#34765=CARTESIAN_POINT('Ctrl Pts',(52.6482477619896,20.308949382765,17.4785424788548));
#34766=CARTESIAN_POINT('Ctrl Pts',(52.6658418210588,20.2539062755377,17.4815636925916));
#34767=CARTESIAN_POINT('Ctrl Pts',(52.6904823617375,20.1768182131765,17.4857949128965));
#34768=CARTESIAN_POINT('Ctrl Pts',(52.7189920782052,20.1008075996192,17.4900261332014));
#34769=CARTESIAN_POINT('Ctrl Pts',(52.7512580351567,20.0262906873441,17.4942573535064));
#34770=CARTESIAN_POINT('Ctrl Pts',(52.7834777249843,19.9518806271057,17.4984825065375));
#34771=CARTESIAN_POINT('Ctrl Pts',(52.8194427747475,19.8789604372923,17.5027076595687));
#34772=CARTESIAN_POINT('Ctrl Pts',(52.8589906676706,19.807930669433,17.5069328125998));
#34773=CARTESIAN_POINT('Ctrl Pts',(52.8986401575386,19.7367184289595,17.511168819879));
#34774=CARTESIAN_POINT('Ctrl Pts',(52.9418907726608,19.6674067833562,17.5154048271582));
#34775=CARTESIAN_POINT('Ctrl Pts',(52.9885303274327,19.6003786203612,17.5196408344374));
#34776=CARTESIAN_POINT('Ctrl Pts',(53.03496668466,19.5336424832702,17.5238583864316));
#34777=CARTESIAN_POINT('Ctrl Pts',(53.0847622529817,19.4691703618106,17.5280759384257));
#34778=CARTESIAN_POINT('Ctrl Pts',(53.1376628599747,19.4073133933876,17.5322934904199));
#34779=CARTESIAN_POINT('Ctrl Pts',(53.1905460003907,19.3454768487285,17.5365096498743));
#34780=CARTESIAN_POINT('Ctrl Pts',(53.2465318416129,19.2862540954425,17.5407258093287));
#34781=CARTESIAN_POINT('Ctrl Pts',(53.3053257318486,19.2299634538051,17.5449419687831));
#34782=CARTESIAN_POINT('Ctrl Pts',(53.364118221145,19.1736741534597,17.549158027775));
#34783=CARTESIAN_POINT('Ctrl Pts',(53.4257182898329,19.1203171465723,17.5533740867669));
#34784=CARTESIAN_POINT('Ctrl Pts',(53.4897952511075,19.0701730993629,17.5575901457588));
#34785=CARTESIAN_POINT('Ctrl Pts',(53.5543967232505,19.0196185910888,17.5618407158872));
#34786=CARTESIAN_POINT('Ctrl Pts',(53.6215154571478,18.9723301938202,17.5660912860157));
#34787=CARTESIAN_POINT('Ctrl Pts',(53.69078101193,18.9285522233769,17.5703418561442));
#34788=CARTESIAN_POINT('Ctrl Pts',(53.7595840746877,18.8850665621807,17.574564044853));
#34789=CARTESIAN_POINT('Ctrl Pts',(53.8305049373513,18.8450447686413,17.5787862335617));
#34790=CARTESIAN_POINT('Ctrl Pts',(53.9031555871003,18.8086801730713,17.5830084222704));
#34791=CARTESIAN_POINT('Ctrl Pts',(53.9765387699242,18.7719489149993,17.5872731831088));
#34792=CARTESIAN_POINT('Ctrl Pts',(54.0516863740956,18.7389492160398,17.5915379439471));
#34793=CARTESIAN_POINT('Ctrl Pts',(54.1281794747178,18.709829870578,17.5958027047855));
#34794=CARTESIAN_POINT('Ctrl Pts',(54.20467257534,18.6807105251162,17.6000674656238));
#34795=CARTESIAN_POINT('Ctrl Pts',(54.2825106942889,18.6554716206412,17.6043322264622));
#34796=CARTESIAN_POINT('Ctrl Pts',(54.36126280213,18.634209425571,17.6085969873006));
#34797=CARTESIAN_POINT('Ctrl Pts',(54.4393955580764,18.6131144486383,17.6128282076055));
#34798=CARTESIAN_POINT('Ctrl Pts',(54.5187209550309,18.5958547063319,17.6170594279104));
#34799=CARTESIAN_POINT('Ctrl Pts',(54.5988280069488,18.5825610075968,17.6212906482153));
#34800=CARTESIAN_POINT('Ctrl Pts',(54.6788201909611,18.5692863710953,17.6255158012465));
#34801=CARTESIAN_POINT('Ctrl Pts',(54.7595913490877,18.5599665587695,17.6297409542777));
#34802=CARTESIAN_POINT('Ctrl Pts',(54.8407168036213,18.5546822060617,17.6339661073088));
#34803=CARTESIAN_POINT('Ctrl Pts',(54.9220506661816,18.5493842780645,17.638202114588));
#34804=CARTESIAN_POINT('Ctrl Pts',(55.0037401904558,18.548142686925,17.6424381218672));
#34805=CARTESIAN_POINT('Ctrl Pts',(55.0853486089544,18.5509867568856,17.6466741291464));
#34806=CARTESIAN_POINT('Ctrl Pts',(55.1666014788135,18.5538184359039,17.6508916811406));
#34807=CARTESIAN_POINT('Ctrl Pts',(55.247773480268,18.5607002416188,17.6551092331347));
#34808=CARTESIAN_POINT('Ctrl Pts',(55.3284317574115,18.5716090037386,17.6593267851289));
#34809=CARTESIAN_POINT('Ctrl Pts',(55.4090634030268,18.5825141640333,17.6635429445833));
#34810=CARTESIAN_POINT('Ctrl Pts',(55.4891812008074,18.5974435780524,17.6677591040378));
#34811=CARTESIAN_POINT('Ctrl Pts',(55.5683579201622,18.6163222691419,17.6719752634922));
#34812=CARTESIAN_POINT('Ctrl Pts',(55.6475327528962,18.6352005103904,17.6761913224841));
#34813=CARTESIAN_POINT('Ctrl Pts',(55.7257660998022,18.6580277326974,17.680407381476));
#34814=CARTESIAN_POINT('Ctrl Pts',(55.802642829588,18.6846782646658,17.6846234404679));
#34815=CARTESIAN_POINT('Ctrl Pts',(55.8801488445251,18.7115469482659,17.6888740105964));
#34816=CARTESIAN_POINT('Ctrl Pts',(55.9562754717608,18.7423016809405,17.6931245807249));
#34817=CARTESIAN_POINT('Ctrl Pts',(56.0306165673728,18.7767636785405,17.6973751508533));
#34818=CARTESIAN_POINT('Ctrl Pts',(56.1044612811412,18.8109955704397,17.7015973395621));
#34819=CARTESIAN_POINT('Ctrl Pts',(56.1765438481376,18.8488850974135,17.7058195282708));
#34820=CARTESIAN_POINT('Ctrl Pts',(56.2464914363706,18.8902110652829,17.7100417169796));
#34821=CARTESIAN_POINT('Ctrl Pts',(56.3171443028361,18.9319537209368,17.7143064778179));
#34822=CARTESIAN_POINT('Ctrl Pts',(56.3856184891288,18.9772022386538,17.7185712386563));
#34823=CARTESIAN_POINT('Ctrl Pts',(56.4515618227161,19.0256853024826,17.7228359994946));
#34824=CARTESIAN_POINT('Ctrl Pts',(56.5175051563034,19.0741683663115,17.7271007603329));
#34825=CARTESIAN_POINT('Ctrl Pts',(56.5809173044246,19.1258856219538,17.7313655211712));
#34826=CARTESIAN_POINT('Ctrl Pts',(56.6414836653779,19.1805271020711,17.7356302820096));
#34827=CARTESIAN_POINT('Ctrl Pts',(56.7015736976156,19.2347388501453,17.7398615023145));
#34828=CARTESIAN_POINT('Ctrl Pts',(56.7590879060606,19.2920322453441,17.7440927226194));
#34829=CARTESIAN_POINT('Ctrl Pts',(56.8136935348023,19.3521328901224,17.7483239429244));
#34830=CARTESIAN_POINT('Ctrl Pts',(56.8682208628942,19.4121473547825,17.7525490959555));
#34831=CARTESIAN_POINT('Ctrl Pts',(56.919847584601,19.4749607330765,17.7567742489867));
#34832=CARTESIAN_POINT('Ctrl Pts',(56.9682756776452,19.5402599180709,17.7609994020178));
#34833=CARTESIAN_POINT('Ctrl Pts',(57.0168281805107,19.6057268540427,17.765235409297));
#34834=CARTESIAN_POINT('Ctrl Pts',(57.0621652532177,19.6736920639891,17.7694714165762));
#34835=CARTESIAN_POINT('Ctrl Pts',(57.1040254316298,19.7438044606611,17.7737074238554));
#34836=CARTESIAN_POINT('Ctrl Pts',(57.1457032351135,19.8136113941503,17.7779249758496));
#34837=CARTESIAN_POINT('Ctrl Pts',(57.1839341302728,19.885546446283,17.7821425278437));
#34838=CARTESIAN_POINT('Ctrl Pts',(57.2185028816817,19.9592333527778,17.7863600798379));
#34839=CARTESIAN_POINT('Ctrl Pts',(57.2530602192752,20.0328959295324,17.7905762392923));
#34840=CARTESIAN_POINT('Ctrl Pts',(57.2839576170289,20.1083087914076,17.7947923987468));
#34841=CARTESIAN_POINT('Ctrl Pts',(57.3110264192234,20.18507231017,17.7990085582012));
#34842=CARTESIAN_POINT('Ctrl Pts',(57.3380945764232,20.2618339998133,17.8032246171931));
#34843=CARTESIAN_POINT('Ctrl Pts',(57.3613341658813,20.339945843526,17.807440676185));
#34844=CARTESIAN_POINT('Ctrl Pts',(57.3806256878986,20.4189908915367,17.8116567351769));
#34845=CARTESIAN_POINT('Ctrl Pts',(57.4000751233494,20.4986829737688,17.8159073053054));
#34846=CARTESIAN_POINT('Ctrl Pts',(57.4155114287791,20.5793231463309,17.8201578754338));
#34847=CARTESIAN_POINT('Ctrl Pts',(57.42686460485,20.660473212064,17.8244084455623));
#34848=CARTESIAN_POINT('Ctrl Pts',(57.4381419747948,20.7410814318785,17.8286306342711));
#34849=CARTESIAN_POINT('Ctrl Pts',(57.4453905959142,20.8221922832546,17.8328528229798));
#34850=CARTESIAN_POINT('Ctrl Pts',(57.4485941657342,20.9033725632514,17.8370750116886));
#34851=CARTESIAN_POINT('Ctrl Pts',(57.4518300369975,20.985371380182,17.8413397725269));
#34852=CARTESIAN_POINT('Ctrl Pts',(57.4509388309823,21.0674405479362,17.8456045333652));
#34853=CARTESIAN_POINT('Ctrl Pts',(57.4459575613102,21.149137045262,17.8498692942036));
#34854=CARTESIAN_POINT('Ctrl Pts',(57.4409762916381,21.2308335425878,17.8541340550419));
#34855=CARTESIAN_POINT('Ctrl Pts',(57.4319050755729,21.3121568977794,17.8583988158802));
#34856=CARTESIAN_POINT('Ctrl Pts',(57.4188337747238,21.3926747002994,17.8626635767186));
#34857=CARTESIAN_POINT('Ctrl Pts',(57.4058652741066,21.4725592644862,17.8668947970235));
#34858=CARTESIAN_POINT('Ctrl Pts',(57.3889107966641,21.5519504667765,17.8711260173284));
#34859=CARTESIAN_POINT('Ctrl Pts',(57.3680204733985,21.6304199295433,17.8753572376333));
#34860=CARTESIAN_POINT('Ctrl Pts',(57.3471601053945,21.7087768725925,17.8795823906645));
#34861=CARTESIAN_POINT('Ctrl Pts',(57.322375219031,21.7862142556502,17.8838075436957));
#34862=CARTESIAN_POINT('Ctrl Pts',(57.2937673036419,21.8623118964409,17.8880326967268));
#34863=CARTESIAN_POINT('Ctrl Pts',(57.2650858956698,21.9386050290072,17.892268704006));
#34864=CARTESIAN_POINT('Ctrl Pts',(57.2325618730893,22.0135510621235,17.8965047112852));
#34865=CARTESIAN_POINT('Ctrl Pts',(57.1963484602612,22.0867399372012,17.9007407185644));
#34866=CARTESIAN_POINT('Ctrl Pts',(57.1602928207353,22.159609945605,17.9049582705586));
#34867=CARTESIAN_POINT('Ctrl Pts',(57.1205800716868,22.2307376521125,17.9091758225527));
#34868=CARTESIAN_POINT('Ctrl Pts',(57.077409658326,22.2997381895959,17.9133933745469));
#34869=CARTESIAN_POINT('Ctrl Pts',(57.0342534988536,22.3687159446714,17.9176095340013));
#34870=CARTESIAN_POINT('Ctrl Pts',(56.9876421886092,22.4355675316493,17.9218256934557));
#34871=CARTESIAN_POINT('Ctrl Pts',(56.9378200605565,22.4999345528739,17.9260418529102));
#34872=CARTESIAN_POINT('Ctrl Pts',(56.8879991196641,22.5643000403627,17.9302579119021));
#34873=CARTESIAN_POINT('Ctrl Pts',(56.8349677985317,22.6261807128325,17.934473970894));
#34874=CARTESIAN_POINT('Ctrl Pts',(56.779011637759,22.6852500831384,17.9386900298859));
#34875=CARTESIAN_POINT('Ctrl Pts',(56.7225974400589,22.7448029739809,17.9429406000143));
#34876=CARTESIAN_POINT('Ctrl Pts',(56.6632106165959,22.8014979663097,17.9471911701428));
#34877=CARTESIAN_POINT('Ctrl Pts',(56.6011814009535,22.8550386441367,17.9514417402713));
#34878=CARTESIAN_POINT('Ctrl Pts',(56.5395663596809,22.9082218262858,17.95566392898));
#34879=CARTESIAN_POINT('Ctrl Pts',(56.4753445140025,22.9582924489776,17.9598861176888));
#34880=CARTESIAN_POINT('Ctrl Pts',(56.4088710167949,23.0050019222024,17.9641083063975));
#34881=CARTESIAN_POINT('Ctrl Pts',(56.3417272704506,23.0521823648424,17.9683730672359));
#34882=CARTESIAN_POINT('Ctrl Pts',(56.2722866214324,23.095933236925,17.9726378280742));
#34883=CARTESIAN_POINT('Ctrl Pts',(56.2009413814607,23.1360454228072,17.9769025889125));
#34884=CARTESIAN_POINT('Ctrl Pts',(56.1295961414889,23.1761576086893,17.9811673497509));
#34885=CARTESIAN_POINT('Ctrl Pts',(56.0563467704904,23.212630951131,17.9854321105892));
#34886=CARTESIAN_POINT('Ctrl Pts',(55.9816053200206,23.245306492599,17.9896968714275));
#34887=CARTESIAN_POINT('Ctrl Pts',(55.9074516793276,23.2777250548056,17.9939280917325));
#34888=CARTESIAN_POINT('Ctrl Pts',(55.8315512950746,23.3065269466999,17.9981593120374));
#34889=CARTESIAN_POINT('Ctrl Pts',(55.7542912874203,23.3315220144193,18.0023905323423));
#34890=CARTESIAN_POINT('Ctrl Pts',(55.6771420652096,23.356481240961,18.0066156853735));
#34891=CARTESIAN_POINT('Ctrl Pts',(55.5986375302757,23.3776443428533,18.0108408384046));
#34892=CARTESIAN_POINT('Ctrl Pts',(55.5191857643622,23.3948687630189,18.0150659914358));
#34893=CARTESIAN_POINT('Ctrl Pts',(55.4395298900606,23.4121374320265,18.019301998715));
#34894=CARTESIAN_POINT('Ctrl Pts',(55.358922346814,23.4254469735827,18.0235380059942));
#34895=CARTESIAN_POINT('Ctrl Pts',(55.2777907619473,23.4347037894941,18.0277740132734));
#34896=CARTESIAN_POINT('Ctrl Pts',(55.1970126482685,23.4439202756409,18.0319915652675));
#34897=CARTESIAN_POINT('Ctrl Pts',(55.1157155136274,23.4491192148747,18.0362091172617));
#34898=CARTESIAN_POINT('Ctrl Pts',(55.0343308805465,23.4502595047547,18.0404266692558));
#34899=CARTESIAN_POINT('Ctrl Pts',(54.9529731188199,23.4513994181369,18.0446428287102));
#34900=CARTESIAN_POINT('Ctrl Pts',(54.871528380536,23.4484833368552,18.0488589881647));
#34901=CARTESIAN_POINT('Ctrl Pts',(54.7904302867506,23.4415222270724,18.0530751476191));
#34902=CARTESIAN_POINT('Ctrl Pts',(54.7093341253685,23.4345612831588,18.057291206611));
#34903=CARTESIAN_POINT('Ctrl Pts',(54.6285850551857,23.4235555432474,18.0615072656029));
#34904=CARTESIAN_POINT('Ctrl Pts',(54.5486122285985,23.4085679001907,18.0657233245948));
#34905=CARTESIAN_POINT('Ctrl Pts',(54.4679847733293,23.3934575736997,18.0699738947233));
#34906=CARTESIAN_POINT('Ctrl Pts',(54.3881468028777,23.3742999269146,18.0742244648517));
#34907=CARTESIAN_POINT('Ctrl Pts',(54.3095264363016,23.3512117105513,18.0784750349802));
#34908=CARTESIAN_POINT('Ctrl Pts',(54.231431024627,23.3282776561803,18.082697223689));
#34909=CARTESIAN_POINT('Ctrl Pts',(54.1545374292306,23.3014655748344,18.0869194123977));
#34910=CARTESIAN_POINT('Ctrl Pts',(54.0792470958768,23.270939087591,18.0911416011065));
#34911=CARTESIAN_POINT('Ctrl Pts',(54.0031976136433,23.2401048032167,18.0954063619448));
#34912=CARTESIAN_POINT('Ctrl Pts',(53.928784347114,23.2054809919233,18.0996711227831));
#34913=CARTESIAN_POINT('Ctrl Pts',(53.8563957226305,23.1672839008266,18.1039358836215));
#34914=CARTESIAN_POINT('Ctrl Pts',(53.784007098147,23.1290868097299,18.1082006444598));
#34915=CARTESIAN_POINT('Ctrl Pts',(53.7136434972102,23.0873167400179,18.1124654052981));
#34916=CARTESIAN_POINT('Ctrl Pts',(53.6456619049135,23.0422337217365,18.1167301661365));
#34917=CARTESIAN_POINT('Ctrl Pts',(53.5783618985047,22.9976027074167,18.1209521683294));
#34918=CARTESIAN_POINT('Ctrl Pts',(53.5131415056379,22.94955588298,18.1251741705222));
#34919=CARTESIAN_POINT('Ctrl Pts',(53.4503694764712,22.8983138545951,18.1293961727151));
#34920=CARTESIAN_POINT('Ctrl Pts',(53.387687550532,22.8471453792275,18.1336121146288));
#34921=CARTESIAN_POINT('Ctrl Pts',(53.3274473680911,22.7927911007097,18.1378280565424));
#34922=CARTESIAN_POINT('Ctrl Pts',(53.269989142396,22.7355151058324,18.1420439984561));
#34923=CARTESIAN_POINT('Ctrl Pts',(53.2125973181063,22.6783053017659,18.1462550682307));
#34924=CARTESIAN_POINT('Ctrl Pts',(53.1579813909364,22.6181808191965,18.1504661380052));
#34925=CARTESIAN_POINT('Ctrl Pts',(53.1064477106784,22.5554452666696,18.1546772077798));
#34926=CARTESIAN_POINT('Ctrl Pts',(53.0549465744822,22.4927493323049,18.1588856182194));
#34927=CARTESIAN_POINT('Ctrl Pts',(53.0065241175869,22.4274459608158,18.1630940286591));
#34928=CARTESIAN_POINT('Ctrl Pts',(52.9614482602216,22.3598739111574,18.1673024390988));
#34929=CARTESIAN_POINT('Ctrl Pts',(52.9163868968525,22.2923235890729,18.1715094963376));
#34930=CARTESIAN_POINT('Ctrl Pts',(52.8746702553024,22.222506425746,18.1757165535765));
#34931=CARTESIAN_POINT('Ctrl Pts',(52.8365236665253,22.1507912080368,18.1799236108154));
#34932=CARTESIAN_POINT('Ctrl Pts',(52.7983775197472,22.0790768212816,18.1841306193077));
#34933=CARTESIAN_POINT('Ctrl Pts',(52.7638015616878,22.0054648370139,18.1883376278001));
#34934=CARTESIAN_POINT('Ctrl Pts',(52.732975074571,21.9303484494982,18.1925446362924));
#34935=CARTESIAN_POINT('Ctrl Pts',(52.7021181160096,21.8551578107442,18.1967558033392));
#34936=CARTESIAN_POINT('Ctrl Pts',(52.6750182095149,21.7784602315354,18.200966970386));
#34937=CARTESIAN_POINT('Ctrl Pts',(52.65180614198,21.7006681490955,18.2051781374328));
#34938=CARTESIAN_POINT('Ctrl Pts',(52.6285829340402,21.6228387311064,18.2093913255881));
#34939=CARTESIAN_POINT('Ctrl Pts',(52.6092513929158,21.5439142179396,18.2136045137433));
#34940=CARTESIAN_POINT('Ctrl Pts',(52.5938914951548,21.4643189775484,18.2178177018986));
#34941=CARTESIAN_POINT('Ctrl Pts',(52.5785040199944,21.3845808306238,18.2220384544774));
#34942=CARTESIAN_POINT('Ctrl Pts',(52.567102501311,21.3041700140185,18.2262592070563));
#34943=CARTESIAN_POINT('Ctrl Pts',(52.5597151524206,21.2235175891835,18.2304799596351));
#34944=CARTESIAN_POINT('Ctrl Pts',(52.5528935488415,21.1490417686845,18.2343774743357));
#34945=CARTESIAN_POINT('Ctrl Pts',(52.5494942454254,21.0743602572356,18.2382749890363));
#34946=CARTESIAN_POINT('Ctrl Pts',(52.5495000073192,20.9998106024675,18.2421725037368));
#34947=CARTESIAN_POINT('',(52.5495009535749,21.0021618208968,19.0421725037529));
#34948=CARTESIAN_POINT('Ctrl Pts',(52.5495000073193,20.9998106014887,18.242172503788));
#34949=CARTESIAN_POINT('Ctrl Pts',(52.5495007913209,20.9896669322961,18.2427028228071));
#34950=CARTESIAN_POINT('Ctrl Pts',(52.5495645584554,20.97952354572,18.2432331418263));
#34951=CARTESIAN_POINT('Ctrl Pts',(52.5496913003384,20.9693809477182,18.2437634608455));
#34952=CARTESIAN_POINT('Ctrl Pts',(52.5507025271837,20.8884568905792,18.2479946811504));
#34953=CARTESIAN_POINT('Ctrl Pts',(52.5557288629305,20.8074312572561,18.2522259014553));
#34954=CARTESIAN_POINT('Ctrl Pts',(52.5647840834785,20.7267351286385,18.2564571217602));
#34955=CARTESIAN_POINT('Ctrl Pts',(52.573826319474,20.6461547126213,18.2606822747914));
#34956=CARTESIAN_POINT('Ctrl Pts',(52.5868859150317,20.5659033210397,18.2649074278226));
#34957=CARTESIAN_POINT('Ctrl Pts',(52.6039246404514,20.4864115252813,18.2691325808537));
#34958=CARTESIAN_POINT('Ctrl Pts',(52.6210071376707,20.4067155182998,18.2733685881329));
#34959=CARTESIAN_POINT('Ctrl Pts',(52.6420892230513,20.3277834867746,18.2776045954121));
#34960=CARTESIAN_POINT('Ctrl Pts',(52.6670800035458,20.2500436411736,18.2818406026913));
#34961=CARTESIAN_POINT('Ctrl Pts',(52.6919619051015,20.1726424897521,18.2860581546855));
#34962=CARTESIAN_POINT('Ctrl Pts',(52.7207183788695,20.0964236056981,18.2902757066796));
#34963=CARTESIAN_POINT('Ctrl Pts',(52.7532090935203,20.021797120961,18.2944932586738));
#34964=CARTESIAN_POINT('Ctrl Pts',(52.7856890804763,19.9471952761915,18.2987094181282));
#34965=CARTESIAN_POINT('Ctrl Pts',(52.8219006743826,19.8741852125637,18.3029255775827));
#34966=CARTESIAN_POINT('Ctrl Pts',(52.8616552350494,19.8031575223913,18.3071417370371));
#34967=CARTESIAN_POINT('Ctrl Pts',(52.9014088484456,19.7321315246649,18.311357796029));
#34968=CARTESIAN_POINT('Ctrl Pts',(52.9447050327113,19.6630882116331,18.3155738550209));
#34969=CARTESIAN_POINT('Ctrl Pts',(52.9913096737311,19.5963927104942,18.3197899140128));
#34970=CARTESIAN_POINT('Ctrl Pts',(53.0382958035143,19.5291512640654,18.3240404841413));
#34971=CARTESIAN_POINT('Ctrl Pts',(53.0886445421045,19.4642966460451,18.3282910542697));
#34972=CARTESIAN_POINT('Ctrl Pts',(53.1420731264766,19.4021708531136,18.3325416243982));
#34973=CARTESIAN_POINT('Ctrl Pts',(53.1951449636285,19.3404598794067,18.336763813107));
#34974=CARTESIAN_POINT('Ctrl Pts',(53.2512552747237,19.2814416982429,18.3409860018157));
#34975=CARTESIAN_POINT('Ctrl Pts',(53.3100895781855,19.225414691754,18.3452081905245));
#34976=CARTESIAN_POINT('Ctrl Pts',(53.3695171051537,19.1688227676015,18.3494729513628));
#34977=CARTESIAN_POINT('Ctrl Pts',(53.4317234972464,19.1152829942843,18.3537377122011));
#34978=CARTESIAN_POINT('Ctrl Pts',(53.4963516845599,19.0650602093414,18.3580024730395));
#34979=CARTESIAN_POINT('Ctrl Pts',(53.5609798718733,19.0148374243984,18.3622672338778));
#34980=CARTESIAN_POINT('Ctrl Pts',(53.6280294227939,18.967931851362,18.3665319947161));
#34981=CARTESIAN_POINT('Ctrl Pts',(53.6971163264504,18.9245616407135,18.3707967555545));
#34982=CARTESIAN_POINT('Ctrl Pts',(53.7656598909403,18.8815325183591,18.3750279758594));
#34983=CARTESIAN_POINT('Ctrl Pts',(53.8364658830572,18.8418219556989,18.3792591961643));
#34984=CARTESIAN_POINT('Ctrl Pts',(53.9091795629834,18.8056752692031,18.3834904164693));
#34985=CARTESIAN_POINT('Ctrl Pts',(53.9817889765818,18.7695804145258,18.3877155695004));
#34986=CARTESIAN_POINT('Ctrl Pts',(54.0563002322929,18.7370394916865,18.3919407225316));
#34987=CARTESIAN_POINT('Ctrl Pts',(54.1323308198289,18.7082538439476,18.3961658755627));
#34988=CARTESIAN_POINT('Ctrl Pts',(54.2085567268834,18.6793942470384,18.4004018828419));
#34989=CARTESIAN_POINT('Ctrl Pts',(54.2863093787766,18.654309489749,18.4046378901211));
#34990=CARTESIAN_POINT('Ctrl Pts',(54.3651796937318,18.6331553855926,18.4088738974003));
#34991=CARTESIAN_POINT('Ctrl Pts',(54.443706389319,18.6120934448807,18.4130914493945));
#34992=CARTESIAN_POINT('Ctrl Pts',(54.523340579708,18.5949281079748,18.4173090013886));
#34993=CARTESIAN_POINT('Ctrl Pts',(54.6036615668166,18.5817638460271,18.4215265533828));
#34994=CARTESIAN_POINT('Ctrl Pts',(54.6839560337625,18.5686039306192,18.4257427128372));
#34995=CARTESIAN_POINT('Ctrl Pts',(54.764936388665,18.5594425418583,18.4299588722916));
#34996=CARTESIAN_POINT('Ctrl Pts',(54.846172157216,18.554332965266,18.4341750317461));
#34997=CARTESIAN_POINT('Ctrl Pts',(54.9274059900832,18.5492235104246,18.438391090738));
#34998=CARTESIAN_POINT('Ctrl Pts',(55.008894760424,18.5481657038711,18.4426071497299));
#34999=CARTESIAN_POINT('Ctrl Pts',(55.0902047336656,18.5511608145849,18.4468232087217));
#35000=CARTESIAN_POINT('Ctrl Pts',(55.1721802809889,18.5541804421936,18.4510737788502));
#35001=CARTESIAN_POINT('Ctrl Pts',(55.2539736105822,18.5613196431465,18.4553243489787));
#35002=CARTESIAN_POINT('Ctrl Pts',(55.3351440444507,18.5725262680166,18.4595749191072));
#35003=CARTESIAN_POINT('Ctrl Pts',(55.4157724964008,18.5836580652956,18.4637971078159));
#35004=CARTESIAN_POINT('Ctrl Pts',(55.4957858957313,18.5988029867764,18.4680192965247));
#35005=CARTESIAN_POINT('Ctrl Pts',(55.5747630124426,18.6178585832223,18.4722414852334));
#35006=CARTESIAN_POINT('Ctrl Pts',(55.6545364516964,18.6371063163482,18.4765062460718));
#35007=CARTESIAN_POINT('Ctrl Pts',(55.7332521272118,18.660343893077,18.4807710069101));
#35008=CARTESIAN_POINT('Ctrl Pts',(55.8104939020217,18.6874148913422,18.4850357677484));
#35009=CARTESIAN_POINT('Ctrl Pts',(55.8877356768317,18.7144858896075,18.4893005285868));
#35010=CARTESIAN_POINT('Ctrl Pts',(55.9635031290862,18.7453900679564,18.4935652894251));
#35011=CARTESIAN_POINT('Ctrl Pts',(56.0374047419543,18.7799230528266,18.4978300502635));
#35012=CARTESIAN_POINT('Ctrl Pts',(56.1107251500119,18.8141844504317,18.5020612705684));
#35013=CARTESIAN_POINT('Ctrl Pts',(56.182483924496,18.852146215288,18.5062924908733));
#35014=CARTESIAN_POINT('Ctrl Pts',(56.2522825941555,18.8936432984,18.5105237111783));
#35015=CARTESIAN_POINT('Ctrl Pts',(56.3219811774079,18.9350808775992,18.5147488642094));
#35016=CARTESIAN_POINT('Ctrl Pts',(56.3897248417463,18.9800434712623,18.5189740172406));
#35017=CARTESIAN_POINT('Ctrl Pts',(56.4551370060087,19.0283188534289,18.5231991702717));
#35018=CARTESIAN_POINT('Ctrl Pts',(56.5207172114877,19.0767182531087,18.5274351775509));
#35019=CARTESIAN_POINT('Ctrl Pts',(56.5839534975876,19.1284472782783,18.5316711848301));
#35020=CARTESIAN_POINT('Ctrl Pts',(56.6444931312107,19.1832466894482,18.5359071921093));
#35021=CARTESIAN_POINT('Ctrl Pts',(56.7047690079228,19.2378073525031,18.5401247441035));
#35022=CARTESIAN_POINT('Ctrl Pts',(56.7623713281544,19.2954113955379,18.5443422960976));
#35023=CARTESIAN_POINT('Ctrl Pts',(56.8169841998611,19.3557619796832,18.5485598480918));
#35024=CARTESIAN_POINT('Ctrl Pts',(56.87157903964,19.4160926374386,18.5527760075462));
#35025=CARTESIAN_POINT('Ctrl Pts',(56.923186079324,19.4791676909798,18.5569921670007));
#35026=CARTESIAN_POINT('Ctrl Pts',(56.9715271339629,19.5446543331401,18.5612083264551));
#35027=CARTESIAN_POINT('Ctrl Pts',(57.0198670367325,19.6101394148864,18.565424385447));
#35028=CARTESIAN_POINT('Ctrl Pts',(57.0649408339631,19.678035596293,18.5696404444389));
#35029=CARTESIAN_POINT('Ctrl Pts',(57.1065122790564,19.7479791262983,18.5738565034308));
#35030=CARTESIAN_POINT('Ctrl Pts',(57.1484240129886,19.8184951887851,18.5781070735593));
#35031=CARTESIAN_POINT('Ctrl Pts',(57.1867755332491,19.891091868116,18.5823576436877));
#35032=CARTESIAN_POINT('Ctrl Pts',(57.2213717123995,19.9653706144946,18.5866082138162));
#35033=CARTESIAN_POINT('Ctrl Pts',(57.2557368899074,20.0391533953407,18.590830402525));
#35034=CARTESIAN_POINT('Ctrl Pts',(57.2863966035495,20.1145953907973,18.5950525912337));
#35035=CARTESIAN_POINT('Ctrl Pts',(57.3132085346942,20.1912871183059,18.5992747799425));
#35036=CARTESIAN_POINT('Ctrl Pts',(57.3402908092758,20.2687521248852,18.6035395407808));
#35037=CARTESIAN_POINT('Ctrl Pts',(57.3634471335384,20.3474917412843,18.6078043016191));
#35038=CARTESIAN_POINT('Ctrl Pts',(57.3825833002841,20.4270714990442,18.6120690624575));
#35039=CARTESIAN_POINT('Ctrl Pts',(57.4017194670298,20.5066512568041,18.6163338232958));
#35040=CARTESIAN_POINT('Ctrl Pts',(57.4168354503997,20.5870706705503,18.6205985841341));
#35041=CARTESIAN_POINT('Ctrl Pts',(57.4278906833145,20.6678899581848,18.6248633449724));
#35042=CARTESIAN_POINT('Ctrl Pts',(57.4388589715159,20.7480736364335,18.6290945652774));
#35043=CARTESIAN_POINT('Ctrl Pts',(57.4458713284404,20.8289515948451,18.6333257855823));
#35044=CARTESIAN_POINT('Ctrl Pts',(57.4488503742784,20.9100995306101,18.6375570058872));
#35045=CARTESIAN_POINT('Ctrl Pts',(57.4518251483731,20.9911311059149,18.6417821589184));
#35046=CARTESIAN_POINT('Ctrl Pts',(57.4507780809056,21.0724314290177,18.6460073119495));
#35047=CARTESIAN_POINT('Ctrl Pts',(57.445683301105,21.1535690095559,18.6502324649807));
#35048=CARTESIAN_POINT('Ctrl Pts',(57.4405754330203,21.2349150292721,18.6544684722599));
#35049=CARTESIAN_POINT('Ctrl Pts',(57.4313989715538,21.3160970006676,18.6587044795391));
#35050=CARTESIAN_POINT('Ctrl Pts',(57.418180479306,21.3966779796048,18.6629404868183));
#35051=CARTESIAN_POINT('Ctrl Pts',(57.4050195769126,21.4769078862144,18.6671580388124));
#35052=CARTESIAN_POINT('Ctrl Pts',(57.387851858305,21.5565415631848,18.6713755908066));
#35053=CARTESIAN_POINT('Ctrl Pts',(57.3667554544363,21.6351526343296,18.6755931428007));
#35054=CARTESIAN_POINT('Ctrl Pts',(57.3456660161203,21.7137377498871,18.6798093022552));
#35055=CARTESIAN_POINT('Ctrl Pts',(57.3206505889357,21.7913004814464,18.6840254617096));
#35056=CARTESIAN_POINT('Ctrl Pts',(57.2918379712813,21.8674266328592,18.688241621164));
#35057=CARTESIAN_POINT('Ctrl Pts',(57.2630260401731,21.9435509703401,18.6924576801559));
#35058=CARTESIAN_POINT('Ctrl Pts',(57.230417264101,22.018238361307,18.6966737391478));
#35059=CARTESIAN_POINT('Ctrl Pts',(57.1941891815087,22.091093069243,18.7008897981397));
#35060=CARTESIAN_POINT('Ctrl Pts',(57.1576645489136,22.1645441395118,18.7051403682682));
#35061=CARTESIAN_POINT('Ctrl Pts',(57.1174612828544,22.236131948211,18.7093909383966));
#35062=CARTESIAN_POINT('Ctrl Pts',(57.0738084566093,22.305476439962,18.7136415085251));
#35063=CARTESIAN_POINT('Ctrl Pts',(57.0304471040127,22.3743579126199,18.7178636972338));
#35064=CARTESIAN_POINT('Ctrl Pts',(56.9836824371873,22.441025585864,18.7220858859426));
#35065=CARTESIAN_POINT('Ctrl Pts',(56.9337813495928,22.5051378481611,18.7263080746513));
#35066=CARTESIAN_POINT('Ctrl Pts',(56.8833771116861,22.5698965513746,18.7305728354897));
#35067=CARTESIAN_POINT('Ctrl Pts',(56.8297731655299,22.6320476535413,18.734837596328));
#35068=CARTESIAN_POINT('Ctrl Pts',(56.7732834856916,22.6912764201554,18.7391023571663));
#35069=CARTESIAN_POINT('Ctrl Pts',(56.7167938058533,22.7505051867694,18.7433671180047));
#35070=CARTESIAN_POINT('Ctrl Pts',(56.6574187861403,22.8068113329226,18.747631878843));
#35071=CARTESIAN_POINT('Ctrl Pts',(56.595505950671,22.8599223132629,18.7518966396814));
#35072=CARTESIAN_POINT('Ctrl Pts',(56.5340800333679,22.9126155982909,18.7561278599863));
#35073=CARTESIAN_POINT('Ctrl Pts',(56.4699257649903,22.9623614237981,18.7603590802912));
#35074=CARTESIAN_POINT('Ctrl Pts',(56.4033577027442,23.0088647062828,18.7645903005961));
#35075=CARTESIAN_POINT('Ctrl Pts',(56.3368850944403,23.0553013063151,18.7688154536273));
#35076=CARTESIAN_POINT('Ctrl Pts',(56.2680059444106,23.098504333733,18.7730406066584));
#35077=CARTESIAN_POINT('Ctrl Pts',(56.1970687784232,23.1382180875029,18.7772657596896));
#35078=CARTESIAN_POINT('Ctrl Pts',(56.1259493777121,23.1780338643074,18.7815017669688));
#35079=CARTESIAN_POINT('Ctrl Pts',(56.0527617360255,23.2143421144585,18.785737774248));
#35080=CARTESIAN_POINT('Ctrl Pts',(55.9778873921048,23.2469282361398,18.7899737815272));
#35081=CARTESIAN_POINT('Ctrl Pts',(55.9033392580483,23.2793723877715,18.7941913335214));
#35082=CARTESIAN_POINT('Ctrl Pts',(55.8271195139761,23.3081265819627,18.7984088855155));
#35083=CARTESIAN_POINT('Ctrl Pts',(55.7496287805504,23.3330252766249,18.8026264375097));
#35084=CARTESIAN_POINT('Ctrl Pts',(55.672163632802,23.3579157503045,18.8068425969641));
#35085=CARTESIAN_POINT('Ctrl Pts',(55.5934287713559,23.3789531103391,18.8110587564185));
#35086=CARTESIAN_POINT('Ctrl Pts',(55.5138420557708,23.3960209915026,18.815274915873));
#35087=CARTESIAN_POINT('Ctrl Pts',(55.4342572365759,23.4130884659731,18.8194909748649));
#35088=CARTESIAN_POINT('Ctrl Pts',(55.3538210584178,23.4261865532265,18.8237070338568));
#35089=CARTESIAN_POINT('Ctrl Pts',(55.2729622983371,23.4352498503617,18.8279230928487));
#35090=CARTESIAN_POINT('Ctrl Pts',(55.1914416576428,23.4443873363747,18.8321736629772));
#35091=CARTESIAN_POINT('Ctrl Pts',(55.1094919598312,23.4494236033213,18.8364242331056));
#35092=CARTESIAN_POINT('Ctrl Pts',(55.0275567494081,23.4503450523471,18.8406748032341));
#35093=CARTESIAN_POINT('Ctrl Pts',(54.9461686273817,23.4512603487791,18.8448969919429));
#35094=CARTESIAN_POINT('Ctrl Pts',(54.8647952666353,23.4481156898308,18.8491191806516));
#35095=CARTESIAN_POINT('Ctrl Pts',(54.7838684167242,23.4409500995946,18.8533413693604));
#35096=CARTESIAN_POINT('Ctrl Pts',(54.7021255852031,23.43371225905,18.8576061301987));
#35097=CARTESIAN_POINT('Ctrl Pts',(54.6208388006313,23.4223720122261,18.861870891037));
#35098=CARTESIAN_POINT('Ctrl Pts',(54.54044275794,23.4070225157381,18.8661356518754));
#35099=CARTESIAN_POINT('Ctrl Pts',(54.4600467152487,23.3916730192501,18.8704004127137));
#35100=CARTESIAN_POINT('Ctrl Pts',(54.3805418673589,23.3723144495057,18.874665173552));
#35101=CARTESIAN_POINT('Ctrl Pts',(54.3023456516815,23.3490910285198,18.8789299343904));
#35102=CARTESIAN_POINT('Ctrl Pts',(54.2247644160425,23.3260502498806,18.8831611546953));
#35103=CARTESIAN_POINT('Ctrl Pts',(54.1481803686174,23.299118837247,18.8873923750002));
#35104=CARTESIAN_POINT('Ctrl Pts',(54.0730120087879,23.2684010919916,18.8916235953052));
#35105=CARTESIAN_POINT('Ctrl Pts',(53.9979514351253,23.2377273938328,18.8958487483363));
#35106=CARTESIAN_POINT('Ctrl Pts',(53.9243029440742,23.20327832051,18.9000739013675));
#35107=CARTESIAN_POINT('Ctrl Pts',(53.85247036297,23.1652080690173,18.9042990543986));
#35108=CARTESIAN_POINT('Ctrl Pts',(53.7804532468567,23.1270400165812,18.9085350616778));
#35109=CARTESIAN_POINT('Ctrl Pts',(53.7102618332828,23.0852322973752,18.912771068957));
#35110=CARTESIAN_POINT('Ctrl Pts',(53.6422833169227,23.0399891319548,18.9170070762362));
#35111=CARTESIAN_POINT('Ctrl Pts',(53.5746009669319,22.9949430803396,18.9212246282304));
#35112=CARTESIAN_POINT('Ctrl Pts',(53.5091126662484,22.9464917073601,18.9254421802245));
#35113=CARTESIAN_POINT('Ctrl Pts',(53.4461747344618,22.8948818681319,18.9296597322187));
#35114=CARTESIAN_POINT('Ctrl Pts',(53.3832575833485,22.8432890692985,18.9338758916731));
#35115=CARTESIAN_POINT('Ctrl Pts',(53.3228894881164,22.7885401697459,18.9380920511276));
#35116=CARTESIAN_POINT('Ctrl Pts',(53.2653947955222,22.730923174089,18.942308210582));
#35117=CARTESIAN_POINT('Ctrl Pts',(53.2079014729099,22.6733075513284,18.9465242695739));
#35118=CARTESIAN_POINT('Ctrl Pts',(53.1532817444197,22.6128242982245,18.9507403285658));
#35119=CARTESIAN_POINT('Ctrl Pts',(53.1018230561569,22.5497982255322,18.9549563875577));
#35120=CARTESIAN_POINT('Ctrl Pts',(53.0499431456527,22.4862562441662,18.9592069576862));
#35121=CARTESIAN_POINT('Ctrl Pts',(53.0012765803358,22.4201299832977,18.9634575278146));
#35122=CARTESIAN_POINT('Ctrl Pts',(52.9560752859617,22.3517847511137,18.9677080979431));
#35123=CARTESIAN_POINT('Ctrl Pts',(52.9111758044901,22.2838958658812,18.9719302866519));
#35124=CARTESIAN_POINT('Ctrl Pts',(52.8696956450238,22.2138179871338,18.9761524753606));
#35125=CARTESIAN_POINT('Ctrl Pts',(52.8318361221775,22.1419350458348,18.9803746640694));
#35126=CARTESIAN_POINT('Ctrl Pts',(52.7935948635482,22.0693273122295,18.9846394249077));
#35127=CARTESIAN_POINT('Ctrl Pts',(52.7590478703977,21.9948783511333,18.988904185746));
#35128=CARTESIAN_POINT('Ctrl Pts',(52.7283525703267,21.9190039201541,18.9931689465844));
#35129=CARTESIAN_POINT('Ctrl Pts',(52.6976572702557,21.843129489175,18.9974337074227));
#35130=CARTESIAN_POINT('Ctrl Pts',(52.6708137606241,21.7658300645252,19.001698468261));
#35131=CARTESIAN_POINT('Ctrl Pts',(52.6479272046732,21.6875345922088,19.0059632290994));
#35132=CARTESIAN_POINT('Ctrl Pts',(52.6197371321448,21.5910956588898,19.0112162657558));
#35133=CARTESIAN_POINT('Ctrl Pts',(52.5974627565319,21.4928545750512,19.0164693024122));
#35134=CARTESIAN_POINT('Ctrl Pts',(52.5812939432754,21.3934606221259,19.0217223390686));
#35135=CARTESIAN_POINT('Ctrl Pts',(52.5653763691369,21.2956111022191,19.0268937514106));
#35136=CARTESIAN_POINT('Ctrl Pts',(52.5553761126385,21.1966441865217,19.0320651637527));
#35137=CARTESIAN_POINT('Ctrl Pts',(52.5514285146056,21.0972004676609,19.0372365760948));
#35138=CARTESIAN_POINT('Ctrl Pts',(52.5501725676789,21.065561979637,19.0388818853142));
#35139=CARTESIAN_POINT('Ctrl Pts',(52.549528931169,21.0338753951898,19.0405271945335));
#35140=CARTESIAN_POINT('Ctrl Pts',(52.5495009535749,21.0021618208968,19.0421725037529));
#35141=CARTESIAN_POINT('',(52.5495002327295,20.9989320078278,19.8421725038355));
#35142=CARTESIAN_POINT('Ctrl Pts',(52.5495009535743,21.0021618202204,19.042172503788));
#35143=CARTESIAN_POINT('Ctrl Pts',(52.5494297852942,20.9214900785257,19.0463577766029));
#35144=CARTESIAN_POINT('Ctrl Pts',(52.5533465260389,20.8407379080871,19.0505430494178));
#35145=CARTESIAN_POINT('Ctrl Pts',(52.561248273611,20.7603330080405,19.0547283222326));
#35146=CARTESIAN_POINT('Ctrl Pts',(52.5691465090023,20.6799638464871,19.0589117347711));
#35147=CARTESIAN_POINT('Ctrl Pts',(52.5810261897998,20.5999421189795,19.0630951473095));
#35148=CARTESIAN_POINT('Ctrl Pts',(52.5968324058427,20.5206924115017,19.0672785598479));
#35149=CARTESIAN_POINT('Ctrl Pts',(52.6126366275038,20.4414527035183,19.0714614445356));
#35150=CARTESIAN_POINT('Ctrl Pts',(52.632366307305,20.3629852857009,19.0756443292234));
#35151=CARTESIAN_POINT('Ctrl Pts',(52.655915337234,20.2857050022677,19.0798272139111));
#35152=CARTESIAN_POINT('Ctrl Pts',(52.6794688917087,20.2084098707424,19.084010902269));
#35153=CARTESIAN_POINT('Ctrl Pts',(52.7068431129201,20.132302777971,19.0881945906269));
#35154=CARTESIAN_POINT('Ctrl Pts',(52.7378823698768,20.0577823619324,19.0923782789848));
#35155=CARTESIAN_POINT('Ctrl Pts',(52.7689564606817,19.9831783152558,19.0965666624926));
#35156=CARTESIAN_POINT('Ctrl Pts',(52.8037036093297,19.9101649341082,19.1007550460004));
#35157=CARTESIAN_POINT('Ctrl Pts',(52.8419207859546,19.8391191465508,19.1049434295082));
#35158=CARTESIAN_POINT('Ctrl Pts',(52.880163830866,19.7680252698106,19.109134648032));
#35159=CARTESIAN_POINT('Ctrl Pts',(52.9218813306025,19.6989020392003,19.1133258665557));
#35160=CARTESIAN_POINT('Ctrl Pts',(52.9668265530173,19.6320979623948,19.1175170850795));
#35161=CARTESIAN_POINT('Ctrl Pts',(53.0118440847632,19.5651864090246,19.1217150465715));
#35162=CARTESIAN_POINT('Ctrl Pts',(53.0600994125051,19.5006018271536,19.1259130080635));
#35163=CARTESIAN_POINT('Ctrl Pts',(53.1113056482137,19.4386595837132,19.1301109695555));
#35164=CARTESIAN_POINT('Ctrl Pts',(53.1230381975715,19.4244671632308,19.1310728209731));
#35165=CARTESIAN_POINT('Ctrl Pts',(53.1349255128873,19.4104133028115,19.1320346723907));
#35166=CARTESIAN_POINT('Ctrl Pts',(53.1469638846957,19.3965015106406,19.1329965238083));
#35167=CARTESIAN_POINT('Ctrl Pts',(53.1999211318349,19.3353030173666,19.1372277441133));
#35168=CARTESIAN_POINT('Ctrl Pts',(53.2560126451939,19.2766160559906,19.1414589644182));
#35169=CARTESIAN_POINT('Ctrl Pts',(53.3149709686592,19.2207789868769,19.1456901847231));
#35170=CARTESIAN_POINT('Ctrl Pts',(53.3738447500152,19.1650219842123,19.1499153377543));
#35171=CARTESIAN_POINT('Ctrl Pts',(53.4355768423949,19.1121070746184,19.1541404907854));
#35172=CARTESIAN_POINT('Ctrl Pts',(53.4998603701468,19.0623386929229,19.1583656438166));
#35173=CARTESIAN_POINT('Ctrl Pts',(53.5643090396935,19.0124424582583,19.1626016510958));
#35174=CARTESIAN_POINT('Ctrl Pts',(53.6313219567419,18.9657092915203,19.166837658375));
#35175=CARTESIAN_POINT('Ctrl Pts',(53.700553517281,18.9224078628014,19.1710736656542));
#35176=CARTESIAN_POINT('Ctrl Pts',(53.7694834522328,18.8792950881989,19.1752912176483));
#35177=CARTESIAN_POINT('Ctrl Pts',(53.8406123464424,18.8395844664646,19.1795087696425));
#35178=CARTESIAN_POINT('Ctrl Pts',(53.9135684680578,18.8034989696334,19.1837263216366));
#35179=CARTESIAN_POINT('Ctrl Pts',(53.9865005012216,18.7674253874122,19.1879424810911));
#35180=CARTESIAN_POINT('Ctrl Pts',(54.0612581473,18.7349747591132,19.1921586405455));
#35181=CARTESIAN_POINT('Ctrl Pts',(54.1374453520316,18.7063239702896,19.1963748));
#35182=CARTESIAN_POINT('Ctrl Pts',(54.2136307413766,18.6776738641562,19.2005908589919));
#35183=CARTESIAN_POINT('Ctrl Pts',(54.2912451860894,18.6528235800871,19.2048069179838));
#35184=CARTESIAN_POINT('Ctrl Pts',(54.3698742973329,18.6319012164104,19.2090229769757));
#35185=CARTESIAN_POINT('Ctrl Pts',(54.4491470380896,18.6108075898194,19.2132735471042));
#35186=CARTESIAN_POINT('Ctrl Pts',(54.5294506739798,18.593706624379,19.2175241172326));
#35187=CARTESIAN_POINT('Ctrl Pts',(54.6103485494582,18.5806773681275,19.2217746873611));
#35188=CARTESIAN_POINT('Ctrl Pts',(54.6907062629137,18.5677351093325,19.2259968760699));
#35189=CARTESIAN_POINT('Ctrl Pts',(54.771649831094,18.5588103410262,19.2302190647786));
#35190=CARTESIAN_POINT('Ctrl Pts',(54.8527464809369,18.5539283225703,19.2344412534874));
#35191=CARTESIAN_POINT('Ctrl Pts',(54.9346608244747,18.5489970789527,19.2387060143257));
#35192=CARTESIAN_POINT('Ctrl Pts',(55.0167308683073,18.5481905745412,19.242970775164));
#35193=CARTESIAN_POINT('Ctrl Pts',(55.0985129203709,18.5514809670905,19.2472355360024));
#35194=CARTESIAN_POINT('Ctrl Pts',(55.1802949724344,18.5547713596398,19.2515002968407));
#35195=CARTESIAN_POINT('Ctrl Pts',(55.2617885586987,18.5621585416679,19.255765057679));
#35196=CARTESIAN_POINT('Ctrl Pts',(55.3425595024362,18.5735616147755,19.2600298185174));
#35197=CARTESIAN_POINT('Ctrl Pts',(55.4226952169922,18.5848750075544,19.2642610388223));
#35198=CARTESIAN_POINT('Ctrl Pts',(55.5024201211983,18.6001837291142,19.2684922591272));
#35199=CARTESIAN_POINT('Ctrl Pts',(55.5813048921626,18.6194465197463,19.2727234794322));
#35200=CARTESIAN_POINT('Ctrl Pts',(55.6600765478865,18.6386816888849,19.2769486324633));
#35201=CARTESIAN_POINT('Ctrl Pts',(55.7380100151372,18.661859556974,19.2811737854945));
#35202=CARTESIAN_POINT('Ctrl Pts',(55.8146831023249,18.6888873474479,19.2853989385256));
#35203=CARTESIAN_POINT('Ctrl Pts',(55.891553159587,18.7159845712276,19.2896349458048));
#35204=CARTESIAN_POINT('Ctrl Pts',(55.9671558862857,18.746951450961,19.293870953084));
#35205=CARTESIAN_POINT('Ctrl Pts',(56.0410781422642,18.7816432767249,19.2981069603632));
#35206=CARTESIAN_POINT('Ctrl Pts',(56.1146783364012,18.8161839583829,19.3023245123574));
#35207=CARTESIAN_POINT('Ctrl Pts',(56.1866122450872,18.8544170049677,19.3065420643515));
#35208=CARTESIAN_POINT('Ctrl Pts',(56.2564909582044,18.8961509745348,19.3107596163457));
#35209=CARTESIAN_POINT('Ctrl Pts',(56.3263465989601,18.9378711644946,19.3149757758001));
#35210=CARTESIAN_POINT('Ctrl Pts',(56.3941479928693,18.9830897437309,19.3191919352545));
#35211=CARTESIAN_POINT('Ctrl Pts',(56.4595317651643,19.0315698446538,19.323408094709));
#35212=CARTESIAN_POINT('Ctrl Pts',(56.5249139794966,19.0800487903942,19.3276241537009));
#35213=CARTESIAN_POINT('Ctrl Pts',(56.5878783139519,19.1317888255023,19.3318402126928));
#35214=CARTESIAN_POINT('Ctrl Pts',(56.6480924451072,19.1865112235305,19.3360562716847));
#35215=CARTESIAN_POINT('Ctrl Pts',(56.708799467398,19.2416815593499,19.3403068418131));
#35216=CARTESIAN_POINT('Ctrl Pts',(56.7667106884168,19.2998829977883,19.3445574119416));
#35217=CARTESIAN_POINT('Ctrl Pts',(56.8215229250338,19.3607915069839,19.3488079820701));
#35218=CARTESIAN_POINT('Ctrl Pts',(56.8759691756664,19.4212933248623,19.3530301707788));
#35219=CARTESIAN_POINT('Ctrl Pts',(56.9273574519107,19.4844657696759,19.3572523594876));
#35220=CARTESIAN_POINT('Ctrl Pts',(56.9754318709531,19.5499589063675,19.3614745481964));
#35221=CARTESIAN_POINT('Ctrl Pts',(57.0239910220948,19.6161124072669,19.3657393090347));
#35222=CARTESIAN_POINT('Ctrl Pts',(57.0691688455571,19.6846332567307,19.370004069873));
#35223=CARTESIAN_POINT('Ctrl Pts',(57.1107481558536,19.7551335523196,19.3742688307113));
#35224=CARTESIAN_POINT('Ctrl Pts',(57.1523274661502,19.8256338479085,19.3785335915497));
#35225=CARTESIAN_POINT('Ctrl Pts',(57.1903080965616,19.8981131330463,19.382798352388));
#35226=CARTESIAN_POINT('Ctrl Pts',(57.2245226006815,19.9721627322104,19.3870631132263));
#35227=CARTESIAN_POINT('Ctrl Pts',(57.2584680222521,20.0456299627146,19.3912943335313));
#35228=CARTESIAN_POINT('Ctrl Pts',(57.2888336769176,20.1209183703428,19.3955255538362));
#35229=CARTESIAN_POINT('Ctrl Pts',(57.3154214442977,20.1976448509006,19.3997567741411));
#35230=CARTESIAN_POINT('Ctrl Pts',(57.3419710866803,20.2742613110556,19.4039819271723));
#35231=CARTESIAN_POINT('Ctrl Pts',(57.3647534498519,20.3523113130751,19.4082070802034));
#35232=CARTESIAN_POINT('Ctrl Pts',(57.3836175664651,20.431389811172,19.4124322332346));
#35233=CARTESIAN_POINT('Ctrl Pts',(57.4025301442344,20.5106714587467,19.4166682405138));
#35234=CARTESIAN_POINT('Ctrl Pts',(57.4175041258897,20.5909864623144,19.420904247793));
#35235=CARTESIAN_POINT('Ctrl Pts',(57.4284370882124,20.6719092220216,19.4251402550722));
#35236=CARTESIAN_POINT('Ctrl Pts',(57.4393224181958,20.7524794203431,19.4293578070663));
#35237=CARTESIAN_POINT('Ctrl Pts',(57.4462017962051,20.8336516275832,19.4335753590605));
#35238=CARTESIAN_POINT('Ctrl Pts',(57.449025202975,20.9149952637015,19.4377929110547));
#35239=CARTESIAN_POINT('Ctrl Pts',(57.4518476775203,20.9963120420016,19.4420090705091));
#35240=CARTESIAN_POINT('Ctrl Pts',(57.4506168241535,21.0777996724995,19.4462252299635));
#35241=CARTESIAN_POINT('Ctrl Pts',(57.4453346376679,21.1590244000826,19.4504413894179));
#35242=CARTESIAN_POINT('Ctrl Pts',(57.4400525770461,21.2402471922451,19.4546574484098));
#35243=CARTESIAN_POINT('Ctrl Pts',(57.4307194065195,21.3212066300785,19.4588735074017));
#35244=CARTESIAN_POINT('Ctrl Pts',(57.4173891288913,21.4014723521216,19.4630895663936));
#35245=CARTESIAN_POINT('Ctrl Pts',(57.4039497344238,21.4823951003831,19.4673401365221));
#35246=CARTESIAN_POINT('Ctrl Pts',(57.3864475558196,21.5626122475542,19.4715907066506));
#35247=CARTESIAN_POINT('Ctrl Pts',(57.364990463597,21.6416933512942,19.475841276779));
#35248=CARTESIAN_POINT('Ctrl Pts',(57.3436766422115,21.7202464237515,19.4800634654878));
#35249=CARTESIAN_POINT('Ctrl Pts',(57.3184607651209,21.7976781502054,19.4842856541965));
#35250=CARTESIAN_POINT('Ctrl Pts',(57.2894981148884,21.8735837864353,19.4885078429053));
#35251=CARTESIAN_POINT('Ctrl Pts',(57.2602434356198,21.9502547756146,19.4927726037436));
#35252=CARTESIAN_POINT('Ctrl Pts',(57.227166196645,22.0253682817625,19.4970373645819));
#35253=CARTESIAN_POINT('Ctrl Pts',(57.1904745646009,22.0985314887779,19.5013021254203));
#35254=CARTESIAN_POINT('Ctrl Pts',(57.1537829325567,22.1716946957933,19.5055668862586));
#35255=CARTESIAN_POINT('Ctrl Pts',(57.1134772006757,22.2429072160272,19.5098316470969));
#35256=CARTESIAN_POINT('Ctrl Pts',(57.0698099594893,22.3118067622935,19.5140964079353));
#35257=CARTESIAN_POINT('Ctrl Pts',(57.026486142616,22.3801644428795,19.5183276282402));
#35258=CARTESIAN_POINT('Ctrl Pts',(56.9796910805182,22.4465017586957,19.5225588485451));
#35259=CARTESIAN_POINT('Ctrl Pts',(56.9296392456943,22.5104445145308,19.52679006885));
#35260=CARTESIAN_POINT('Ctrl Pts',(56.8796591816983,22.5742955809296,19.5310152218812));
#35261=CARTESIAN_POINT('Ctrl Pts',(56.8264319040669,22.6357585437843,19.5352403749124));
#35262=CARTESIAN_POINT('Ctrl Pts',(56.7702158888053,22.6944869303188,19.5394655279435));
#35263=CARTESIAN_POINT('Ctrl Pts',(56.7138554568637,22.7533661877139,19.5437015352227));
#35264=CARTESIAN_POINT('Ctrl Pts',(56.6544911698454,22.8094964055248,19.5479375425019));
#35265=CARTESIAN_POINT('Ctrl Pts',(56.5924250956956,22.8625607546061,19.5521735497811));
#35266=CARTESIAN_POINT('Ctrl Pts',(56.5306294287983,22.9153939148288,19.5563911017753));
#35267=CARTESIAN_POINT('Ctrl Pts',(56.4661558180753,22.965187554888,19.5606086537694));
#35268=CARTESIAN_POINT('Ctrl Pts',(56.3993389305689,23.0116661769276,19.5648262057636));
#35269=CARTESIAN_POINT('Ctrl Pts',(56.3325441044787,23.0581294527835,19.569042365218));
#35270=CARTESIAN_POINT('Ctrl Pts',(56.2634079194224,23.1012796189479,19.5732585246725));
#35271=CARTESIAN_POINT('Ctrl Pts',(56.1922959134083,23.1408831600229,19.5774746841269));
#35272=CARTESIAN_POINT('Ctrl Pts',(56.1211856018494,23.1804857574258,19.5816907431188));
#35273=CARTESIAN_POINT('Ctrl Pts',(56.0480999696586,23.2165416725246,19.5859068021107));
#35274=CARTESIAN_POINT('Ctrl Pts',(55.9734299032573,23.2488629290031,19.5901228611026));
#35275=CARTESIAN_POINT('Ctrl Pts',(55.8981486146541,23.2814487556167,19.594373431231));
#35276=CARTESIAN_POINT('Ctrl Pts',(55.8212572667672,23.3102382949725,19.5986240013595));
#35277=CARTESIAN_POINT('Ctrl Pts',(55.7431760222275,23.3350887884588,19.602874571488));
#35278=CARTESIAN_POINT('Ctrl Pts',(55.6656161328252,23.3597733530781,19.6070967601967));
#35279=CARTESIAN_POINT('Ctrl Pts',(55.5868826581863,23.3805712541825,19.6113189489055));
#35280=CARTESIAN_POINT('Ctrl Pts',(55.5073998763178,23.3973935045196,19.6155411376142));
#35281=CARTESIAN_POINT('Ctrl Pts',(55.4271156733091,23.4143853728132,19.6198058984526));
#35282=CARTESIAN_POINT('Ctrl Pts',(55.3460674472878,23.4273208899218,19.6240706592909));
#35283=CARTESIAN_POINT('Ctrl Pts',(55.2646981287331,23.4361619713486,19.6283354201293));
#35284=CARTESIAN_POINT('Ctrl Pts',(55.1833288101783,23.4450030527755,19.6326001809676));
#35285=CARTESIAN_POINT('Ctrl Pts',(55.1016388838035,23.4497497347133,19.6368649418059));
#35286=CARTESIAN_POINT('Ctrl Pts',(55.0200697162189,23.4504178126374,19.6411297026443));
#35287=CARTESIAN_POINT('Ctrl Pts',(54.9391420555075,23.4510806364124,19.6453609229492));
#35288=CARTESIAN_POINT('Ctrl Pts',(54.8580297917767,23.4477313112697,19.6495921432541));
#35289=CARTESIAN_POINT('Ctrl Pts',(54.777163628751,23.440347147774,19.6538233635591));
#35290=CARTESIAN_POINT('Ctrl Pts',(54.6964134221429,23.4329735726519,19.6580485165902));
#35291=CARTESIAN_POINT('Ctrl Pts',(54.6159090744608,23.4215766918839,19.6622736696214));
#35292=CARTESIAN_POINT('Ctrl Pts',(54.5360818557209,23.4061858210472,19.6664988226526));
#35293=CARTESIAN_POINT('Ctrl Pts',(54.45604956407,23.390755411683,19.6707348299318));
#35294=CARTESIAN_POINT('Ctrl Pts',(54.3766983568976,23.3713104677392,19.674970837211));
#35295=CARTESIAN_POINT('Ctrl Pts',(54.2984582330946,23.3479330057068,19.6792068444902));
#35296=CARTESIAN_POINT('Ctrl Pts',(54.2205589830653,23.324657393765,19.6834243964843));
#35297=CARTESIAN_POINT('Ctrl Pts',(54.1437616057692,23.2974835844915,19.6876419484785));
#35298=CARTESIAN_POINT('Ctrl Pts',(54.0684790480282,23.266543396019,19.6918595004726));
#35299=CARTESIAN_POINT('Ctrl Pts',(53.9932213468753,23.235613423293,19.6960756599271));
#35300=CARTESIAN_POINT('Ctrl Pts',(53.9194779017149,23.2009197175233,19.7002918193815));
#35301=CARTESIAN_POINT('Ctrl Pts',(53.8476431231349,23.162642799526,19.7045079788359));
#35302=CARTESIAN_POINT('Ctrl Pts',(53.775810056232,23.1243667935901,19.7087240378278));
#35303=CARTESIAN_POINT('Ctrl Pts',(53.7058859752706,23.0825079647952,19.7129400968197));
#35304=CARTESIAN_POINT('Ctrl Pts',(53.6382407717543,23.0372928248751,19.7171561558116));
#35305=CARTESIAN_POINT('Ctrl Pts',(53.5700418490274,22.991707570146,19.7214067259401));
#35306=CARTESIAN_POINT('Ctrl Pts',(53.5041596918322,22.9427110568059,19.7256572960685));
#35307=CARTESIAN_POINT('Ctrl Pts',(53.4409420723575,22.8905789135223,19.729907866197));
#35308=CARTESIAN_POINT('Ctrl Pts',(53.3781465623265,22.8387948610112,19.7341300549058));
#35309=CARTESIAN_POINT('Ctrl Pts',(53.3179804209147,22.7839172868419,19.7383522436145));
#35310=CARTESIAN_POINT('Ctrl Pts',(53.2607484711599,22.7262544335721,19.7425744323233));
#35311=CARTESIAN_POINT('Ctrl Pts',(53.2029394543555,22.6680101684728,19.7468391931616));
#35312=CARTESIAN_POINT('Ctrl Pts',(53.1481244573347,22.6069245020227,19.7511039539999));
#35313=CARTESIAN_POINT('Ctrl Pts',(53.0965756466165,22.5433489498317,19.7553687148383));
#35314=CARTESIAN_POINT('Ctrl Pts',(53.0450268358984,22.4797733976408,19.7596334756766));
#35315=CARTESIAN_POINT('Ctrl Pts',(52.9967444438948,22.4137083866067,19.7638982365149));
#35316=CARTESIAN_POINT('Ctrl Pts',(52.9519545173027,22.345533333219,19.7681629973533));
#35317=CARTESIAN_POINT('Ctrl Pts',(52.9066393874759,22.276558864398,19.7724777664492));
#35318=CARTESIAN_POINT('Ctrl Pts',(52.8647339880631,22.2051736964748,19.7767925355452));
#35319=CARTESIAN_POINT('Ctrl Pts',(52.8264977671134,22.1317412662075,19.7811073046411));
#35320=CARTESIAN_POINT('Ctrl Pts',(52.7883228181496,22.0584265084174,19.7854151594954));
#35321=CARTESIAN_POINT('Ctrl Pts',(52.7538055636304,21.983071395981,19.7897230143497));
#35322=CARTESIAN_POINT('Ctrl Pts',(52.7231620146361,21.9060678994446,19.794030869204));
#35323=CARTESIAN_POINT('Ctrl Pts',(52.6925687719447,21.8291908165042,19.7983316520233));
#35324=CARTESIAN_POINT('Ctrl Pts',(52.6658367414319,21.7506711416486,19.8026324348426));
#35325=CARTESIAN_POINT('Ctrl Pts',(52.6431351825498,21.6709236038963,19.8069332176618));
#35326=CARTESIAN_POINT('Ctrl Pts',(52.6204555946949,21.5912532474222,19.8112298380966));
#35327=CARTESIAN_POINT('Ctrl Pts',(52.6017988463954,21.5103578116504,19.8155264585314));
#35328=CARTESIAN_POINT('Ctrl Pts',(52.587285206786,21.4286695424289,19.8198230789662));
#35329=CARTESIAN_POINT('Ctrl Pts',(52.5727825748233,21.3470432284185,19.8241164406953));
#35330=CARTESIAN_POINT('Ctrl Pts',(52.5624168795559,21.2646257096145,19.8284098024244));
#35331=CARTESIAN_POINT('Ctrl Pts',(52.5562575955193,21.1818606899327,19.8327031641535));
#35332=CARTESIAN_POINT('Ctrl Pts',(52.5517293372353,21.1210124835883,19.8358596106983));
#35333=CARTESIAN_POINT('Ctrl Pts',(52.5494736278551,21.0599767387354,19.8390160572431));
#35334=CARTESIAN_POINT('Ctrl Pts',(52.5495002327291,20.9989320087486,19.8421725037879));
#35335=CARTESIAN_POINT('',(52.5495005252726,20.9983955185562,20.6421725037879));
#35336=CARTESIAN_POINT('Ctrl Pts',(52.5495002327295,20.9989320078278,19.8421725038355));
#35337=CARTESIAN_POINT('Ctrl Pts',(52.5495391024497,20.9097457359996,19.8467840681691));
#35338=CARTESIAN_POINT('Ctrl Pts',(52.5544510791458,20.8207169626876,19.8513956325027));
#35339=CARTESIAN_POINT('Ctrl Pts',(52.5641597639198,20.7323573384293,19.8560071968362));
#35340=CARTESIAN_POINT('Ctrl Pts',(52.5738970811663,20.6437371274313,19.8606323614145));
#35341=CARTESIAN_POINT('Ctrl Pts',(52.5884593140069,20.5557903160324,19.8652575259928));
#35342=CARTESIAN_POINT('Ctrl Pts',(52.6077191292299,20.4690174340456,19.8698826905711));
#35343=CARTESIAN_POINT('Ctrl Pts',(52.6270652852011,20.38185555375,19.8745285895212));
#35344=CARTESIAN_POINT('Ctrl Pts',(52.6511511000742,20.2958784425238,19.8791744884714));
#35345=CARTESIAN_POINT('Ctrl Pts',(52.6797988482953,20.2115731704032,19.8838203874215));
#35346=CARTESIAN_POINT('Ctrl Pts',(52.7031810509242,20.1427634705903,19.8876123556351));
#35347=CARTESIAN_POINT('Ctrl Pts',(52.7296013596882,20.0750671950961,19.8914043238486));
#35348=CARTESIAN_POINT('Ctrl Pts',(52.7589403160553,20.0087372986955,19.8951962920622));
#35349=CARTESIAN_POINT('Ctrl Pts',(52.7916778235747,19.934723913386,19.8994275123671));
#35350=CARTESIAN_POINT('Ctrl Pts',(52.8281472075493,19.8621952891128,19.9036587326721));
#35351=CARTESIAN_POINT('Ctrl Pts',(52.8681916962783,19.7915532257549,19.907889952977));
#35352=CARTESIAN_POINT('Ctrl Pts',(52.9081787640133,19.7210124581716,19.9121151060081));
#35353=CARTESIAN_POINT('Ctrl Pts',(52.9517305276497,19.6523532798264,19.9163402590393));
#35354=CARTESIAN_POINT('Ctrl Pts',(52.9986425958401,19.585956581001,19.9205654120705));
#35355=CARTESIAN_POINT('Ctrl Pts',(53.0456751792452,19.5193893117292,19.9248014193497));
#35356=CARTESIAN_POINT('Ctrl Pts',(53.0960851574693,19.4550965903672,19.9290374266289));
#35357=CARTESIAN_POINT('Ctrl Pts',(53.1496206424203,19.3934364366628,19.9332734339081));
#35358=CARTESIAN_POINT('Ctrl Pts',(53.2029228858847,19.3320449217112,19.9374909859022));
#35359=CARTESIAN_POINT('Ctrl Pts',(53.2593231581153,19.2732634419551,19.9417085378964));
#35360=CARTESIAN_POINT('Ctrl Pts',(53.3185312176626,19.2174139616768,19.9459260898905));
#35361=CARTESIAN_POINT('Ctrl Pts',(53.3777197280557,19.1615829216263,19.950142249345));
#35362=CARTESIAN_POINT('Ctrl Pts',(53.4397138468037,19.1086822773503,19.9543584087994));
#35363=CARTESIAN_POINT('Ctrl Pts',(53.5041865919209,19.0589970380727,19.9585745682538));
#35364=CARTESIAN_POINT('Ctrl Pts',(53.5686578007832,19.0093129826936,19.9627906272457));
#35365=CARTESIAN_POINT('Ctrl Pts',(53.6356071496528,18.9628444628948,19.9670066862376));
#35366=CARTESIAN_POINT('Ctrl Pts',(53.704675851816,18.9198351985645,19.9712227452295));
#35367=CARTESIAN_POINT('Ctrl Pts',(53.7743099254359,18.876473875926,19.975473315358));
#35368=CARTESIAN_POINT('Ctrl Pts',(53.8460978102861,18.8366289697907,19.9797238854865));
#35369=CARTESIAN_POINT('Ctrl Pts',(53.9196450778532,18.8005038094616,19.983974455615));
#35370=CARTESIAN_POINT('Ctrl Pts',(53.9927012640342,18.7646198599128,19.9881966443237));
#35371=CARTESIAN_POINT('Ctrl Pts',(54.0674929537223,18.7324062622766,19.9924188330325));
#35372=CARTESIAN_POINT('Ctrl Pts',(54.143613695683,18.7040137744798,19.9966410217412));
#35373=CARTESIAN_POINT('Ctrl Pts',(54.2205019594944,18.6753350065679,20.0009057825796));
#35374=CARTESIAN_POINT('Ctrl Pts',(54.2987457648483,18.6505549850221,20.0051705434179));
#35375=CARTESIAN_POINT('Ctrl Pts',(54.3779126848174,18.6297768834371,20.0094353042563));
#35376=CARTESIAN_POINT('Ctrl Pts',(54.4570796047866,18.6089987818522,20.0137000650946));
#35377=CARTESIAN_POINT('Ctrl Pts',(54.5371691546353,18.5922226361211,20.0179648259329));
#35378=CARTESIAN_POINT('Ctrl Pts',(54.6177424854411,18.5794981011031,20.0222295867713));
#35379=CARTESIAN_POINT('Ctrl Pts',(54.6976821412072,18.566873639151,20.0264608070762));
#35380=CARTESIAN_POINT('Ctrl Pts',(54.7783977531393,18.5581899016551,20.0306920273812));
#35381=CARTESIAN_POINT('Ctrl Pts',(54.8594667097273,18.5535330281557,20.0349232476861));
#35382=CARTESIAN_POINT('Ctrl Pts',(54.9404194191055,18.548882832287,20.0391484007172));
#35383=CARTESIAN_POINT('Ctrl Pts',(55.0217240066113,18.5482480587764,20.0433735537484));
#35384=CARTESIAN_POINT('Ctrl Pts',(55.1029496093053,18.5516634978125,20.0475987067796));
#35385=CARTESIAN_POINT('Ctrl Pts',(55.1843838773027,18.5550877109739,20.0518347140588));
#35386=CARTESIAN_POINT('Ctrl Pts',(55.2657382869153,18.5625830402717,20.056070721338));
#35387=CARTESIAN_POINT('Ctrl Pts',(55.346575438063,18.5741319665465,20.0603067286171));
#35388=CARTESIAN_POINT('Ctrl Pts',(55.4270604008013,18.5856305768723,20.0645242806113));
#35389=CARTESIAN_POINT('Ctrl Pts',(55.5070321384962,18.6011474786276,20.0687418326055));
#35390=CARTESIAN_POINT('Ctrl Pts',(55.5860627501174,18.620613376745,20.0729593845996));
#35391=CARTESIAN_POINT('Ctrl Pts',(55.6650672676286,18.6400728476657,20.0771755440541));
#35392=CARTESIAN_POINT('Ctrl Pts',(55.7431308250737,18.6634786145446,20.0813917035085));
#35393=CARTESIAN_POINT('Ctrl Pts',(55.8198366508486,18.6907104737765,20.0856078629629));
#35394=CARTESIAN_POINT('Ctrl Pts',(55.8965406488791,18.7179416841284,20.0898239219548));
#35395=CARTESIAN_POINT('Ctrl Pts',(55.9718865418039,18.7489986489792,20.0940399809467));
#35396=CARTESIAN_POINT('Ctrl Pts',(56.0454750055611,18.7837120532866,20.0982560399386));
#35397=CARTESIAN_POINT('Ctrl Pts',(56.1196658379113,18.8187096089873,20.1025066100671));
#35398=CARTESIAN_POINT('Ctrl Pts',(56.1920698962164,18.8574235508832,20.1067571801956));
#35399=CARTESIAN_POINT('Ctrl Pts',(56.2623024682511,18.8996327157739,20.111007750324));
#35400=CARTESIAN_POINT('Ctrl Pts',(56.3320660914049,18.9415600464663,20.1152299390328));
#35401=CARTESIAN_POINT('Ctrl Pts',(56.3996867829558,18.9869357535491,20.1194521277415));
#35402=CARTESIAN_POINT('Ctrl Pts',(56.464817484026,19.0355000665585,20.1236743164503));
#35403=CARTESIAN_POINT('Ctrl Pts',(56.5306048948826,19.0845540512449,20.1279390772886));
#35404=CARTESIAN_POINT('Ctrl Pts',(56.5938514453632,19.1368609952995,20.1322038381269));
#35405=CARTESIAN_POINT('Ctrl Pts',(56.6542359740413,19.1921135012984,20.1364685989653));
#35406=CARTESIAN_POINT('Ctrl Pts',(56.7146205027195,19.2473660072973,20.1407333598036));
#35407=CARTESIAN_POINT('Ctrl Pts',(56.7721427166022,19.3055636874104,20.1449981206419));
#35408=CARTESIAN_POINT('Ctrl Pts',(56.8265229404517,19.3663647291994,20.1492628814802));
#35409=CARTESIAN_POINT('Ctrl Pts',(56.8804754869275,19.4266875966076,20.1534941017852));
#35410=CARTESIAN_POINT('Ctrl Pts',(56.9315376377036,19.4897991966869,20.1577253220901));
#35411=CARTESIAN_POINT('Ctrl Pts',(56.979407866102,19.5553911430379,20.161956542395));
#35412=CARTESIAN_POINT('Ctrl Pts',(57.0272094519435,19.6208890351287,20.1661816954262));
#35413=CARTESIAN_POINT('Ctrl Pts',(57.0718279338929,19.688859837356,20.1704068484573));
#35414=CARTESIAN_POINT('Ctrl Pts',(57.1130004567089,19.758960387438,20.1746320014885));
#35415=CARTESIAN_POINT('Ctrl Pts',(57.1542787500784,19.8292410230109,20.1788680087677));
#35416=CARTESIAN_POINT('Ctrl Pts',(57.1920930467087,19.9016620068143,20.1831040160469));
#35417=CARTESIAN_POINT('Ctrl Pts',(57.2262208989421,19.9758463205586,20.1873400233261));
#35418=CARTESIAN_POINT('Ctrl Pts',(57.2602000641693,20.0497074307376,20.1915575753202));
#35419=CARTESIAN_POINT('Ctrl Pts',(57.2905246369787,20.1253161164419,20.1957751273144));
#35420=CARTESIAN_POINT('Ctrl Pts',(57.3170208242543,20.2022752667919,20.1999926793085));
#35421=CARTESIAN_POINT('Ctrl Pts',(57.3435082630916,20.2792090069812,20.2042088387629));
#35422=CARTESIAN_POINT('Ctrl Pts',(57.3661696753829,20.3574918870836,20.2084249982174));
#35423=CARTESIAN_POINT('Ctrl Pts',(57.3848800777843,20.4367085438358,20.2126411576718));
#35424=CARTESIAN_POINT('Ctrl Pts',(57.4035900343547,20.5159233130157,20.2168572166637));
#35425=CARTESIAN_POINT('Ctrl Pts',(57.4183490624273,20.5960713618798,20.2210732756556));
#35426=CARTESIAN_POINT('Ctrl Pts',(57.4290829042632,20.6767253579134,20.2252893346475));
#35427=CARTESIAN_POINT('Ctrl Pts',(57.4399046094526,20.7580395584361,20.229539904776));
#35428=CARTESIAN_POINT('Ctrl Pts',(57.4466348476017,20.8398675539549,20.2337904749044));
#35429=CARTESIAN_POINT('Ctrl Pts',(57.4492508484847,20.9217661761336,20.2380410450329));
#35430=CARTESIAN_POINT('Ctrl Pts',(57.4518493821065,21.0031179542183,20.2422632337417));
#35431=CARTESIAN_POINT('Ctrl Pts',(57.4503885236005,21.0845389503526,20.2464854224504));
#35432=CARTESIAN_POINT('Ctrl Pts',(57.4448983583969,21.1655967001733,20.2507076111592));
#35433=CARTESIAN_POINT('Ctrl Pts',(57.4393528361164,21.2474717514617,20.2549723719975));
#35434=CARTESIAN_POINT('Ctrl Pts',(57.4296963523323,21.3289757075925,20.2592371328358));
#35435=CARTESIAN_POINT('Ctrl Pts',(57.4160130524944,21.4096720397793,20.2635018936742));
#35436=CARTESIAN_POINT('Ctrl Pts',(57.4023297526564,21.490368371966,20.2677666545125));
#35437=CARTESIAN_POINT('Ctrl Pts',(57.3846198037662,21.5702566237358,20.2720314153508));
#35438=CARTESIAN_POINT('Ctrl Pts',(57.3630187627035,21.648916463893,20.2762961761892));
#35439=CARTESIAN_POINT('Ctrl Pts',(57.3415876046581,21.726957677802,20.2805273964941));
#35440=CARTESIAN_POINT('Ctrl Pts',(57.3162460191148,21.8040823907584,20.284758616799));
#35441=CARTESIAN_POINT('Ctrl Pts',(57.2870896288855,21.8798700355419,20.2889898371039));
#35442=CARTESIAN_POINT('Ctrl Pts',(57.2579750468791,21.9555490061471,20.2932149901351));
#35443=CARTESIAN_POINT('Ctrl Pts',(57.2250566898657,22.0298942861481,20.2974401431662));
#35444=CARTESIAN_POINT('Ctrl Pts',(57.1884803690812,22.1024989451906,20.3016652961974));
#35445=CARTESIAN_POINT('Ctrl Pts',(57.1518100852009,22.1752901226793,20.3059013034766));
#35446=CARTESIAN_POINT('Ctrl Pts',(57.1114631503549,22.2463312711302,20.3101373107558));
#35447=CARTESIAN_POINT('Ctrl Pts',(57.0676357326681,22.3152310546037,20.314373318035));
#35448=CARTESIAN_POINT('Ctrl Pts',(57.0239992607075,22.3838306579643,20.3185908700291));
#35449=CARTESIAN_POINT('Ctrl Pts',(56.9769128141619,22.4503071171187,20.3228084220233));
#35450=CARTESIAN_POINT('Ctrl Pts',(56.9266158252163,22.5142990827529,20.3270259740174));
#35451=CARTESIAN_POINT('Ctrl Pts',(56.8763354431922,22.5782699196958,20.3312421334719));
#35452=CARTESIAN_POINT('Ctrl Pts',(56.8228469109498,22.6397575269245,20.3354582929263));
#35453=CARTESIAN_POINT('Ctrl Pts',(56.7664314626968,22.6984316699811,20.3396744523807));
#35454=CARTESIAN_POINT('Ctrl Pts',(56.7100173587095,22.7571044149518,20.3438905113726));
#35455=CARTESIAN_POINT('Ctrl Pts',(56.6506768004122,22.8129634946732,20.3481065703645));
#35456=CARTESIAN_POINT('Ctrl Pts',(56.5887285835314,22.8657148061454,20.3523226293564));
#35457=CARTESIAN_POINT('Ctrl Pts',(56.5262732809154,22.918897920806,20.3565731994849));
#35458=CARTESIAN_POINT('Ctrl Pts',(56.4611677867953,22.9689218310047,20.3608237696134));
#35459=CARTESIAN_POINT('Ctrl Pts',(56.3937721203693,23.0155271088431,20.3650743397419));
#35460=CARTESIAN_POINT('Ctrl Pts',(56.3268264605633,23.0618211992614,20.3692965284506));
#35461=CARTESIAN_POINT('Ctrl Pts',(56.2576215502471,23.1047419763653,20.3735187171594));
#35462=CARTESIAN_POINT('Ctrl Pts',(56.1865370742528,23.1440802273757,20.3777409058681));
#35463=CARTESIAN_POINT('Ctrl Pts',(56.1147358568401,23.1838151241156,20.3820056667065));
#35464=CARTESIAN_POINT('Ctrl Pts',(56.0410173936067,23.2198946296911,20.3862704275448));
#35465=CARTESIAN_POINT('Ctrl Pts',(55.96579409698,23.2521527506452,20.3905351883831));
#35466=CARTESIAN_POINT('Ctrl Pts',(55.8905708003533,23.2844108715993,20.3947999492215));
#35467=CARTESIAN_POINT('Ctrl Pts',(55.8138431444299,23.312847500743,20.3990647100598));
#35468=CARTESIAN_POINT('Ctrl Pts',(55.7360378082485,23.3373486250084,20.4033294708982));
#35469=CARTESIAN_POINT('Ctrl Pts',(55.6588443780043,23.3616570583334,20.4075606912031));
#35470=CARTESIAN_POINT('Ctrl Pts',(55.5803007050971,23.3821828653269,20.411791911508));
#35471=CARTESIAN_POINT('Ctrl Pts',(55.5008120137583,23.3987783509269,20.416023131813));
#35472=CARTESIAN_POINT('Ctrl Pts',(55.4214373036394,23.415350039762,20.4202482848441));
#35473=CARTESIAN_POINT('Ctrl Pts',(55.341120717669,23.4280025061218,20.4244734378753));
#35474=CARTESIAN_POINT('Ctrl Pts',(55.2602832351607,23.4366376192397,20.4286985909065));
#35475=CARTESIAN_POINT('Ctrl Pts',(55.1792380844143,23.4452949156156,20.4329345981857));
#35476=CARTESIAN_POINT('Ctrl Pts',(55.097669809526,23.4499140558417,20.4371706054649));
#35477=CARTESIAN_POINT('Ctrl Pts',(55.0160135914354,23.4504476764235,20.4414066127441));
#35478=CARTESIAN_POINT('Ctrl Pts',(54.9347131302358,23.4509789721462,20.4456241647382));
#35479=CARTESIAN_POINT('Ctrl Pts',(54.8533259583399,23.4474602620402,20.4498417167324));
#35480=CARTESIAN_POINT('Ctrl Pts',(54.772285519582,23.4398967940075,20.4540592687265));
#35481=CARTESIAN_POINT('Ctrl Pts',(54.6912718385334,23.4323358232598,20.458275428181));
#35482=CARTESIAN_POINT('Ctrl Pts',(54.6106051258215,23.4207327898445,20.4624915876354));
#35483=CARTESIAN_POINT('Ctrl Pts',(54.5307153474474,23.4051449363559,20.4667077470899));
#35484=CARTESIAN_POINT('Ctrl Pts',(54.4508274726848,23.3895574542943,20.4709238060818));
#35485=CARTESIAN_POINT('Ctrl Pts',(54.3717169515563,23.3699854310681,20.4751398650737));
#35486=CARTESIAN_POINT('Ctrl Pts',(54.2938037578098,23.3465372610544,20.4793559240656));
#35487=CARTESIAN_POINT('Ctrl Pts',(54.2152527947924,23.3228971527876,20.483606494194));
#35488=CARTESIAN_POINT('Ctrl Pts',(54.1379193154039,23.2953172702312,20.4878570643225));
#35489=CARTESIAN_POINT('Ctrl Pts',(54.0622165104119,23.2639594467781,20.492107634451));
#35490=CARTESIAN_POINT('Ctrl Pts',(53.9870191795132,23.23281100219,20.4963298231597));
#35491=CARTESIAN_POINT('Ctrl Pts',(53.9134312108186,23.197935171268,20.5005520118685));
#35492=CARTESIAN_POINT('Ctrl Pts',(53.8418342657123,23.1595375389008,20.5047742005772));
#35493=CARTESIAN_POINT('Ctrl Pts',(53.769515411986,23.1207527450179,20.5090389614156));
#35494=CARTESIAN_POINT('Ctrl Pts',(53.6992283746618,23.0783749804686,20.5133037222539));
#35495=CARTESIAN_POINT('Ctrl Pts',(53.6313362463376,23.0326607634848,20.5175684830922));
#35496=CARTESIAN_POINT('Ctrl Pts',(53.5634441180134,22.9869465465011,20.5218332439305));
#35497=CARTESIAN_POINT('Ctrl Pts',(53.4979472458188,22.9378962173154,20.5260980047689));
#35498=CARTESIAN_POINT('Ctrl Pts',(53.4351727822584,22.8858064663732,20.5303627656072));
#35499=CARTESIAN_POINT('Ctrl Pts',(53.3737435940809,22.8348330142518,20.5345361313551));
#35500=CARTESIAN_POINT('Ctrl Pts',(53.3146772603322,22.7807463896056,20.5387094971031));
#35501=CARTESIAN_POINT('Ctrl Pts',(53.2583127972822,22.723796953788,20.542882862851));
#35502=CARTESIAN_POINT('Ctrl Pts',(53.2020418709362,22.6669420254356,20.5470493029076));
#35503=CARTESIAN_POINT('Ctrl Pts',(53.1484642415818,22.6072340609324,20.5512157429641));
#35504=CARTESIAN_POINT('Ctrl Pts',(53.0978860992566,22.5449637402214,20.5553821830207));
#35505=CARTESIAN_POINT('Ctrl Pts',(53.0473552090205,22.4827515948921,20.5595447306251));
#35506=CARTESIAN_POINT('Ctrl Pts',(52.9998185486412,22.4179822101817,20.5637072782296));
#35507=CARTESIAN_POINT('Ctrl Pts',(52.9555448532792,22.3509823844324,20.567869825834));
#35508=CARTESIAN_POINT('Ctrl Pts',(52.9112980752924,22.2840232930162,20.5720298427065));
#35509=CARTESIAN_POINT('Ctrl Pts',(52.8703105898291,22.2148368494016,20.576189859579));
#35510=CARTESIAN_POINT('Ctrl Pts',(52.8328092765498,22.1437808436022,20.5803498764515));
#35511=CARTESIAN_POINT('Ctrl Pts',(52.7953185310003,22.0727448611197,20.5845087210468));
#35512=CARTESIAN_POINT('Ctrl Pts',(52.7613122300788,21.999840785893,20.5886675656421));
#35513=CARTESIAN_POINT('Ctrl Pts',(52.7309717177786,21.9254517299565,20.5928264102373));
#35514=CARTESIAN_POINT('Ctrl Pts',(52.7006122507968,21.8510162008142,20.5969878529949));
#35515=CARTESIAN_POINT('Ctrl Pts',(52.6739233341779,21.7750942796353,20.6011492957525));
#35516=CARTESIAN_POINT('Ctrl Pts',(52.6510381008611,21.6980889960411,20.6053107385101));
#35517=CARTESIAN_POINT('Ctrl Pts',(52.6281465986378,21.6210626185426,20.6094733212034));
#35518=CARTESIAN_POINT('Ctrl Pts',(52.6090609727083,21.5429527524677,20.6136359038967));
#35519=CARTESIAN_POINT('Ctrl Pts',(52.5938637359314,21.4641751056811,20.6177984865901));
#35520=CARTESIAN_POINT('Ctrl Pts',(52.5786432827025,21.3852771121837,20.6219674283606));
#35521=CARTESIAN_POINT('Ctrl Pts',(52.5673231569836,21.3057097746646,20.6261363701311));
#35522=CARTESIAN_POINT('Ctrl Pts',(52.5599341697403,21.2258959804843,20.6303053119016));
#35523=CARTESIAN_POINT('Ctrl Pts',(52.5529230756155,21.1501640831302,20.6342610425303));
#35524=CARTESIAN_POINT('Ctrl Pts',(52.5494508847733,21.0742106786019,20.6382167731591));
#35525=CARTESIAN_POINT('Ctrl Pts',(52.5495005252726,20.9983955185562,20.6421725037879));
#35526=CARTESIAN_POINT('',(52.5495008698404,21.0020647244182,21.442172503788));
#35527=CARTESIAN_POINT('Ctrl Pts',(52.5468288761996,20.9983937692755,20.6421725037879));
#35528=CARTESIAN_POINT('Ctrl Pts',(52.5460903334207,20.9010294596174,20.6472470226307));
#35529=CARTESIAN_POINT('Ctrl Pts',(52.5955624235799,19.9919636142317,20.6946659730428));
#35530=CARTESIAN_POINT('Ctrl Pts',(53.7309516898259,18.396268298246,20.7844293550254));
#35531=CARTESIAN_POINT('Ctrl Pts',(56.4996417677023,18.5219005353188,20.9114626497339));
#35532=CARTESIAN_POINT('Ctrl Pts',(57.8953253383877,20.9163724138012,21.0384959444432));
#35533=CARTESIAN_POINT('Ctrl Pts',(56.6401754796155,23.3874100578551,21.165529239152));
#35534=CARTESIAN_POINT('Ctrl Pts',(53.8833525846904,23.6726393206288,21.2925625338611));
#35535=CARTESIAN_POINT('Ctrl Pts',(52.6242883163623,22.1034286881138,21.3847769554064));
#35536=CARTESIAN_POINT('Ctrl Pts',(52.5468214014796,21.1466563462855,21.434646945382));
#35537=CARTESIAN_POINT('Ctrl Pts',(52.5481225970323,21.0020658857137,21.442172503788));
#35538=CARTESIAN_POINT('',(52.5495000224195,21.0003314787029,22.2421725037548));
#35539=CARTESIAN_POINT('Ctrl Pts',(52.5495008698404,21.0020647244182,21.442172503788));
#35540=CARTESIAN_POINT('Ctrl Pts',(52.5494304515662,20.918489445297,21.4465248629335));
#35541=CARTESIAN_POINT('Ctrl Pts',(52.5536406367923,20.8347652266227,21.4508772220789));
#35542=CARTESIAN_POINT('Ctrl Pts',(52.5621453286912,20.7513740729974,21.4552295812244));
#35543=CARTESIAN_POINT('Ctrl Pts',(52.5702688987333,20.671719937914,21.4593868975371));
#35544=CARTESIAN_POINT('Ctrl Pts',(52.5823103019167,20.59237020044,21.4635442138498));
#35545=CARTESIAN_POINT('Ctrl Pts',(52.5982284637294,20.5137451927636,21.4677015301625));
#35546=CARTESIAN_POINT('Ctrl Pts',(52.6141376778356,20.4351643807365,21.4718565096196));
#35547=CARTESIAN_POINT('Ctrl Pts',(52.6339192331866,20.3573079598964,21.4760114890767));
#35548=CARTESIAN_POINT('Ctrl Pts',(52.6574805417972,20.2805885475327,21.4801664685337));
#35549=CARTESIAN_POINT('Ctrl Pts',(52.6810363253825,20.2038871255404,21.484320473666));
#35550=CARTESIAN_POINT('Ctrl Pts',(52.7083699617319,20.1283226413996,21.4884744787983));
#35551=CARTESIAN_POINT('Ctrl Pts',(52.7393387648728,20.0542933700172,21.4926284839306));
#35552=CARTESIAN_POINT('Ctrl Pts',(52.770310451467,19.980257205894,21.4967828758354));
#35553=CARTESIAN_POINT('Ctrl Pts',(52.8049177886942,19.9077569799207,21.5009372677401));
#35554=CARTESIAN_POINT('Ctrl Pts',(52.8429702805564,19.8371702448609,21.5050916596448));
#35555=CARTESIAN_POINT('Ctrl Pts',(52.8810619410912,19.7665108525694,21.5092503278008));
#35556=CARTESIAN_POINT('Ctrl Pts',(52.9226056021255,19.6977693032916,21.5134089959568));
#35557=CARTESIAN_POINT('Ctrl Pts',(52.9673656338089,19.6312970434097,21.5175676641128));
#35558=CARTESIAN_POINT('Ctrl Pts',(53.0121527784242,19.5647845186356,21.5217288513396));
#35559=CARTESIAN_POINT('Ctrl Pts',(53.0601598798022,19.5005443998092,21.5258900385663));
#35560=CARTESIAN_POINT('Ctrl Pts',(53.1111105325369,19.4388956377913,21.5300512257931));
#35561=CARTESIAN_POINT('Ctrl Pts',(53.1621424293653,19.3771485728562,21.5342190483005));
#35562=CARTESIAN_POINT('Ctrl Pts',(53.2161269149132,19.3180014579987,21.538386870808));
#35563=CARTESIAN_POINT('Ctrl Pts',(53.2727508194675,19.2617363495862,21.5425546933155));
#35564=CARTESIAN_POINT('Ctrl Pts',(53.2912025116041,19.2434015761962,21.5439128366367));
#35565=CARTESIAN_POINT('Ctrl Pts',(53.3099342199554,19.2253725119082,21.5452709799578));
#35566=CARTESIAN_POINT('Ctrl Pts',(53.3289343994194,19.2076579543636,21.546629123279));
#35567=CARTESIAN_POINT('Ctrl Pts',(53.3881284063353,19.1524692313414,21.5508603435839));
#35568=CARTESIAN_POINT('Ctrl Pts',(53.4501703342923,19.1001126034721,21.5550915638888));
#35569=CARTESIAN_POINT('Ctrl Pts',(53.5147580996481,19.0508959115945,21.5593227841938));
#35570=CARTESIAN_POINT('Ctrl Pts',(53.5792532506689,19.0017497930083,21.5635479372249));
#35571=CARTESIAN_POINT('Ctrl Pts',(53.6462866221427,18.9557349476237,21.5677730902561));
#35572=CARTESIAN_POINT('Ctrl Pts',(53.7155205621037,18.913121272421,21.5719982432872));
#35573=CARTESIAN_POINT('Ctrl Pts',(53.7849323612694,18.8703981244022,21.5762342505664));
#35574=CARTESIAN_POINT('Ctrl Pts',(53.8565557001205,18.8310939610539,21.5804702578456));
#35575=CARTESIAN_POINT('Ctrl Pts',(53.9300182421362,18.7954389806951,21.5847062651248));
#35576=CARTESIAN_POINT('Ctrl Pts',(54.0031607251758,18.7599393406797,21.588923817119));
#35577=CARTESIAN_POINT('Ctrl Pts',(54.078126001508,18.7280573643538,21.5931413691131));
#35578=CARTESIAN_POINT('Ctrl Pts',(54.154520639949,18.6999750214992,21.5973589211073));
#35579=CARTESIAN_POINT('Ctrl Pts',(54.2308900546184,18.6719019507953,21.6015750805617));
#35580=CARTESIAN_POINT('Ctrl Pts',(54.3086874581541,18.6476261824804,21.6057912400162));
#35581=CARTESIAN_POINT('Ctrl Pts',(54.3875001613117,18.6272812645392,21.6100073994706));
#35582=CARTESIAN_POINT('Ctrl Pts',(54.4663109865222,18.6069368313761,21.6142234584625));
#35583=CARTESIAN_POINT('Ctrl Pts',(54.5461366128117,18.5905231774913,21.6184395174544));
#35584=CARTESIAN_POINT('Ctrl Pts',(54.6265513350359,18.5781233836885,21.6226555764463));
#35585=CARTESIAN_POINT('Ctrl Pts',(54.7076243031402,18.5656220896509,21.6269061465748));
#35586=CARTESIAN_POINT('Ctrl Pts',(54.7892955842799,18.5572007599945,21.6311567167032));
#35587=CARTESIAN_POINT('Ctrl Pts',(54.8711225759084,18.5528913265734,21.6354072868317));
#35588=CARTESIAN_POINT('Ctrl Pts',(54.9524032017264,18.5486106676073,21.6396294755405));
#35589=CARTESIAN_POINT('Ctrl Pts',(55.0338369953068,18.5483871006073,21.6438516642492));
#35590=CARTESIAN_POINT('Ctrl Pts',(55.1149909625191,18.5521994916785,21.648073852958));
#35591=CARTESIAN_POINT('Ctrl Pts',(55.1969632013544,18.556050322909,21.6523386137963));
#35592=CARTESIAN_POINT('Ctrl Pts',(55.2786494556059,18.5640189118933,21.6566033746346));
#35593=CARTESIAN_POINT('Ctrl Pts',(55.3596115494113,18.5760301603506,21.660868135473));
#35594=CARTESIAN_POINT('Ctrl Pts',(55.4405736432166,18.5880414088078,21.6651328963113));
#35595=CARTESIAN_POINT('Ctrl Pts',(55.5208111167463,18.604095159214,21.6693976571496));
#35596=CARTESIAN_POINT('Ctrl Pts',(55.5999009248688,18.6240645778259,21.673662417988));
#35597=CARTESIAN_POINT('Ctrl Pts',(55.6783687252279,18.6438769454385,21.6778936382929));
#35598=CARTESIAN_POINT('Ctrl Pts',(55.7560011040426,18.6676178608814,21.6821248585978));
#35599=CARTESIAN_POINT('Ctrl Pts',(55.832375606204,18.6952004208182,21.6863560789028));
#35600=CARTESIAN_POINT('Ctrl Pts',(55.9086405926748,18.7227434292946,21.6905812319339));
#35601=CARTESIAN_POINT('Ctrl Pts',(55.9836508512003,18.7541169850837,21.6948063849651));
#35602=CARTESIAN_POINT('Ctrl Pts',(56.0569965225224,18.7891837250971,21.6990315379963));
#35603=CARTESIAN_POINT('Ctrl Pts',(56.1305306159211,18.8243405501538,21.7032675452755));
#35604=CARTESIAN_POINT('Ctrl Pts',(56.2023911025759,18.8632094372283,21.7075035525547));
#35605=CARTESIAN_POINT('Ctrl Pts',(56.2721826727244,18.9056023545611,21.7117395598339));
#35606=CARTESIAN_POINT('Ctrl Pts',(56.3416701774559,18.9478105759477,21.715957111828));
#35607=CARTESIAN_POINT('Ctrl Pts',(56.409106351521,18.993511948985,21.7201746638222));
#35608=CARTESIAN_POINT('Ctrl Pts',(56.4741249704932,19.0424745668655,21.7243922158164));
#35609=CARTESIAN_POINT('Ctrl Pts',(56.5391221217966,19.0914210184035,21.7286083752708));
#35610=CARTESIAN_POINT('Ctrl Pts',(56.6017029320628,19.143626296974,21.7328245347253));
#35611=CARTESIAN_POINT('Ctrl Pts',(56.6615314204312,19.19881605911,21.7370406941797));
#35612=CARTESIAN_POINT('Ctrl Pts',(56.7213584832078,19.2540045061857,21.7412567531716));
#35613=CARTESIAN_POINT('Ctrl Pts',(56.7784330135025,19.3121769793841,21.7454728121635));
#35614=CARTESIAN_POINT('Ctrl Pts',(56.83245437726,19.373020834411,21.7496888711554));
#35615=CARTESIAN_POINT('Ctrl Pts',(56.8869179403951,19.4343627352656,21.7539394412839));
#35616=CARTESIAN_POINT('Ctrl Pts',(56.9382777915358,19.4984196056773,21.7581900114123));
#35617=CARTESIAN_POINT('Ctrl Pts',(56.9862671116431,19.5648368694797,21.7624405815408));
#35618=CARTESIAN_POINT('Ctrl Pts',(57.0339360029623,19.6308106595403,21.7666627702496));
#35619=CARTESIAN_POINT('Ctrl Pts',(57.0782790330116,19.6991129904314,21.7708849589583));
#35620=CARTESIAN_POINT('Ctrl Pts',(57.1190791803643,19.7693685859095,21.7751071476671));
#35621=CARTESIAN_POINT('Ctrl Pts',(57.1602907136779,19.8403325652422,21.7793719085054));
#35622=CARTESIAN_POINT('Ctrl Pts',(57.1978872941892,19.9132889883853,21.7836366693437));
#35623=CARTESIAN_POINT('Ctrl Pts',(57.231694433609,19.9878289645527,21.787901430182));
#35624=CARTESIAN_POINT('Ctrl Pts',(57.2655015730289,20.0623689407201,21.7921661910204));
#35625=CARTESIAN_POINT('Ctrl Pts',(57.2955191543851,20.1384919981338,21.7964309518587));
#35626=CARTESIAN_POINT('Ctrl Pts',(57.3216243635664,20.2157739072852,21.800695712697));
#35627=CARTESIAN_POINT('Ctrl Pts',(57.3475242663604,20.292448027031,21.8049269330019));
#35628=CARTESIAN_POINT('Ctrl Pts',(57.3696702805044,20.3705503404663,21.8091581533068));
#35629=CARTESIAN_POINT('Ctrl Pts',(57.3879063608704,20.4496787649792,21.8133893736117));
#35630=CARTESIAN_POINT('Ctrl Pts',(57.4061162919734,20.5286937248694,21.8176145266429));
#35631=CARTESIAN_POINT('Ctrl Pts',(57.4204273208408,20.6087314243591,21.821839679674));
#35632=CARTESIAN_POINT('Ctrl Pts',(57.4307326301583,20.6893730039358,21.8260648327052));
#35633=CARTESIAN_POINT('Ctrl Pts',(57.4410644134005,20.7702217484844,21.8303008399844));
#35634=CARTESIAN_POINT('Ctrl Pts',(57.4473697247112,20.8516770305352,21.8345368472636));
#35635=CARTESIAN_POINT('Ctrl Pts',(57.44959220944,20.933304741917,21.8387728545428));
#35636=CARTESIAN_POINT('Ctrl Pts',(57.4518050113268,21.0145768206044,21.8429904065369));
#35637=CARTESIAN_POINT('Ctrl Pts',(57.4499704673567,21.0960193618123,21.847207958531));
#35638=CARTESIAN_POINT('Ctrl Pts',(57.4440848589507,21.1771989058883,21.8514255105252));
#35639=CARTESIAN_POINT('Ctrl Pts',(57.4382011938387,21.2583516463257,21.8556416699796));
#35640=CARTESIAN_POINT('Ctrl Pts',(57.4282691541085,21.3392410987342,21.8598578294341));
#35641=CARTESIAN_POINT('Ctrl Pts',(57.4143370766855,21.4194362050917,21.8640739888885));
#35642=CARTESIAN_POINT('Ctrl Pts',(57.4004053312357,21.4996294005622,21.8682900478804));
#35643=CARTESIAN_POINT('Ctrl Pts',(57.3824738182696,21.5791278250063,21.8725061068723));
#35644=CARTESIAN_POINT('Ctrl Pts',(57.3606422222319,21.6575093524931,21.8767221658641));
#35645=CARTESIAN_POINT('Ctrl Pts',(57.3386319206319,21.7365324828623,21.8809727359926));
#35646=CARTESIAN_POINT('Ctrl Pts',(57.3126575051584,21.8144198804118,21.8852233061211));
#35647=CARTESIAN_POINT('Ctrl Pts',(57.2828722281388,21.8907550954065,21.8894738762496));
#35648=CARTESIAN_POINT('Ctrl Pts',(57.2532858299575,21.9665806136517,21.8936960649583));
#35649=CARTESIAN_POINT('Ctrl Pts',(57.2199395547992,22.040874211304,21.8979182536671));
#35650=CARTESIAN_POINT('Ctrl Pts',(57.1830310492812,22.11325005631,21.9021404423758));
#35651=CARTESIAN_POINT('Ctrl Pts',(57.1457503970427,22.1863556635477,21.9064052032142));
#35652=CARTESIAN_POINT('Ctrl Pts',(57.1048355166899,22.2575042061177,21.9106699640525));
#35653=CARTESIAN_POINT('Ctrl Pts',(57.0605353613637,22.3263273632742,21.9149347248909));
#35654=CARTESIAN_POINT('Ctrl Pts',(57.0162352060374,22.3951505204308,21.9191994857292));
#35655=CARTESIAN_POINT('Ctrl Pts',(56.9685501087175,22.4616479380812,21.9234642465676));
#35656=CARTESIAN_POINT('Ctrl Pts',(56.9177699295494,22.525486396962,21.927729007406));
#35657=CARTESIAN_POINT('Ctrl Pts',(56.8673891149322,22.5888227934657,21.9319602277109));
#35658=CARTESIAN_POINT('Ctrl Pts',(56.81377284106,22.649779437751,21.9361914480158));
#35659=CARTESIAN_POINT('Ctrl Pts',(56.7571743408898,22.7080071972092,21.9404226683207));
#35660=CARTESIAN_POINT('Ctrl Pts',(56.7006569990074,22.7661514621358,21.9446478213519));
#35661=CARTESIAN_POINT('Ctrl Pts',(56.6411662452053,22.8215742832384,21.9488729743831));
#35662=CARTESIAN_POINT('Ctrl Pts',(56.578996101381,22.873958794057,21.9530981274142));
#35663=CARTESIAN_POINT('Ctrl Pts',(56.5166662449602,22.9264778785749,21.9573341346934));
#35664=CARTESIAN_POINT('Ctrl Pts',(56.4516435132685,22.9759426568323,21.9615701419726));
#35665=CARTESIAN_POINT('Ctrl Pts',(56.3842621026245,23.0220703947285,21.9658061492518));
#35666=CARTESIAN_POINT('Ctrl Pts',(56.3171742569011,23.0679971649457,21.970023701246));
#35667=CARTESIAN_POINT('Ctrl Pts',(56.2477486232329,23.1106156405142,21.9742412532401));
#35668=CARTESIAN_POINT('Ctrl Pts',(56.1763473934574,23.1496876656635,21.9784588052343));
#35669=CARTESIAN_POINT('Ctrl Pts',(56.1049697387436,23.1887467901191,21.9826749646887));
#35670=CARTESIAN_POINT('Ctrl Pts',(56.0316181908223,23.2242615665046,21.9868911241431));
#35671=CARTESIAN_POINT('Ctrl Pts',(55.9566811492274,23.2560388801421,21.9911072835976));
#35672=CARTESIAN_POINT('Ctrl Pts',(55.8817458932301,23.2878154365908,21.9953233425895));
#35673=CARTESIAN_POINT('Ctrl Pts',(55.8052256471341,23.3158545268721,21.9995394015814));
#35674=CARTESIAN_POINT('Ctrl Pts',(55.7275291471605,23.3400110234851,22.0037554605733));
#35675=CARTESIAN_POINT('Ctrl Pts',(55.6491966516928,23.3643652564569,22.0080060307018));
#35676=CARTESIAN_POINT('Ctrl Pts',(55.5696690100063,23.3847728815998,22.0122566008302));
#35677=CARTESIAN_POINT('Ctrl Pts',(55.4893792346574,23.4011368587996,22.0165071709587));
#35678=CARTESIAN_POINT('Ctrl Pts',(55.4096255609947,23.4173915723263,22.0207293596675));
#35679=CARTESIAN_POINT('Ctrl Pts',(55.3291203737993,23.4296564634265,22.0249515483762));
#35680=CARTESIAN_POINT('Ctrl Pts',(55.2482950311215,23.4378883952143,22.0291737370849));
#35681=CARTESIAN_POINT('Ctrl Pts',(55.1666547303261,23.4462033291819,22.0334384979233));
#35682=CARTESIAN_POINT('Ctrl Pts',(55.0846882666446,23.4504034929406,22.0377032587616));
#35683=CARTESIAN_POINT('Ctrl Pts',(55.0028401040249,23.4504983541739,22.0419680196));
#35684=CARTESIAN_POINT('Ctrl Pts',(54.9209919414053,23.4505932154072,22.0462327804383));
#35685=CARTESIAN_POINT('Ctrl Pts',(54.8392625579176,23.4465828618997,22.0504975412766));
#35686=CARTESIAN_POINT('Ctrl Pts',(54.7580891046741,23.4385301656372,22.054762302115));
#35687=CARTESIAN_POINT('Ctrl Pts',(54.6775540461783,23.4305408004121,22.0589935224199));
#35688=CARTESIAN_POINT('Ctrl Pts',(54.5972642030111,23.4185425342583,22.0632247427249));
#35689=CARTESIAN_POINT('Ctrl Pts',(54.5176502371787,23.4025588351394,22.0674559630298));
#35690=CARTESIAN_POINT('Ctrl Pts',(54.4381504322012,23.3865980555262,22.071681116061));
#35691=CARTESIAN_POINT('Ctrl Pts',(54.3593250317129,23.3666632837747,22.0759062690921));
#35692=CARTESIAN_POINT('Ctrl Pts',(54.2815997032149,23.3428297555689,22.0801314221233));
#35693=CARTESIAN_POINT('Ctrl Pts',(54.2036747014774,23.3189349999888,22.0843674294025));
#35694=CARTESIAN_POINT('Ctrl Pts',(54.1268559001192,23.2911214838037,22.0886034366817));
#35695=CARTESIAN_POINT('Ctrl Pts',(54.0515620708741,23.2595167059784,22.0928394439609));
#35696=CARTESIAN_POINT('Ctrl Pts',(53.9765962790917,23.2280496227188,22.097056995955));
#35697=CARTESIAN_POINT('Ctrl Pts',(53.9031426338185,23.1928244177353,22.1012745479492));
#35698=CARTESIAN_POINT('Ctrl Pts',(53.8315976302803,23.1540162841616,22.1054920999434));
#35699=CARTESIAN_POINT('Ctrl Pts',(53.7600762492746,23.1152209641508,22.1097082593978));
#35700=CARTESIAN_POINT('Ctrl Pts',(53.6904626668853,23.072845286326,22.1139244188523));
#35701=CARTESIAN_POINT('Ctrl Pts',(53.6231297436042,23.0271108867184,22.1181405783067));
#35702=CARTESIAN_POINT('Ctrl Pts',(53.5557984247301,22.981377576869,22.1223566372986));
#35703=CARTESIAN_POINT('Ctrl Pts',(53.4907480408866,22.9322859665042,22.1265726962905));
#35704=CARTESIAN_POINT('Ctrl Pts',(53.428322159038,22.8801007989544,22.1307887552824));
#35705=CARTESIAN_POINT('Ctrl Pts',(53.3653852814616,22.8274884624663,22.1350393254109));
#35706=CARTESIAN_POINT('Ctrl Pts',(53.3051164490023,22.7717319849042,22.1392898955393));
#35707=CARTESIAN_POINT('Ctrl Pts',(53.2478319870599,22.7131425814653,22.1435404656678));
#35708=CARTESIAN_POINT('Ctrl Pts',(53.1909300183614,22.654944384476,22.1477626543766));
#35709=CARTESIAN_POINT('Ctrl Pts',(53.1369729525433,22.5939513703889,22.1519848430853));
#35710=CARTESIAN_POINT('Ctrl Pts',(53.0862309264975,22.5305025917343,22.1562070317941));
#35711=CARTESIAN_POINT('Ctrl Pts',(53.0349772709971,22.466414062038,22.1604717926324));
#35712=CARTESIAN_POINT('Ctrl Pts',(52.9870041383326,22.3998203604865,22.1647365534707));
#35713=CARTESIAN_POINT('Ctrl Pts',(52.9425445714796,22.331100074995,22.169001314309));
#35714=CARTESIAN_POINT('Ctrl Pts',(52.8980850046265,22.2623797895035,22.1732660751474));
#35715=CARTESIAN_POINT('Ctrl Pts',(52.8571391890453,22.191533369362,22.1775308359857));
#35716=CARTESIAN_POINT('Ctrl Pts',(52.8198913303488,22.1189622149616,22.181795596824));
#35717=CARTESIAN_POINT('Ctrl Pts',(52.7805832678882,22.0423771018883,22.1862962444123));
#35718=CARTESIAN_POINT('Ctrl Pts',(52.7452605276227,21.9636134198769,22.1907968920006));
#35719=CARTESIAN_POINT('Ctrl Pts',(52.7141540642048,21.8830960354393,22.1952975395889));
#35720=CARTESIAN_POINT('Ctrl Pts',(52.68314566471,21.8028324841196,22.1997839987704));
#35721=CARTESIAN_POINT('Ctrl Pts',(52.6563271933403,21.7208265945311,22.2042704579518));
#35722=CARTESIAN_POINT('Ctrl Pts',(52.6338824286974,21.6375248142409,22.2087569171332));
#35723=CARTESIAN_POINT('Ctrl Pts',(52.6114813847721,21.5543852995692,22.2132346370288));
#35724=CARTESIAN_POINT('Ctrl Pts',(52.593437190479,21.4699552777701,22.2177123569243));
#35725=CARTESIAN_POINT('Ctrl Pts',(52.5798849594671,21.3846991559471,22.2221900768198));
#35726=CARTESIAN_POINT('Ctrl Pts',(52.5663684050419,21.2996674729948,22.2266560090059));
#35727=CARTESIAN_POINT('Ctrl Pts',(52.5573203157249,21.2138143915247,22.2311219411919));
#35728=CARTESIAN_POINT('Ctrl Pts',(52.5528252148071,21.127615910904,22.235587873378));
#35729=CARTESIAN_POINT('Ctrl Pts',(52.5506160024248,21.0852518451807,22.2377827501703));
#35730=CARTESIAN_POINT('Ctrl Pts',(52.5495057677445,21.0428045501252,22.2399776269625));
#35731=CARTESIAN_POINT('Ctrl Pts',(52.5495000224195,21.000331478703,22.2421725037548));
#35732=CARTESIAN_POINT('',(52.5495010182643,20.9977660545166,23.042172503788));
#35733=CARTESIAN_POINT('Ctrl Pts',(52.5495000224194,21.0003314780632,22.2421725037879));
#35734=CARTESIAN_POINT('Ctrl Pts',(52.5494885746931,20.9157024895623,22.2465458678182));
#35735=CARTESIAN_POINT('Ctrl Pts',(52.5538654945652,20.8311384562012,22.2509192318486));
#35736=CARTESIAN_POINT('Ctrl Pts',(52.5625847018229,20.7471029572889,22.2552925958789));
#35737=CARTESIAN_POINT('Ctrl Pts',(52.5714793432319,20.6613766284642,22.25975395385));
#35738=CARTESIAN_POINT('Ctrl Pts',(52.5848928388564,20.5762007824509,22.2642153118212));
#35739=CARTESIAN_POINT('Ctrl Pts',(52.6027216171688,20.4920564940763,22.2686766697924));
#35740=CARTESIAN_POINT('Ctrl Pts',(52.6202583231078,20.4092906636968,22.2730649414652));
#35741=CARTESIAN_POINT('Ctrl Pts',(52.6420665382094,20.3275232218687,22.277453213138));
#35742=CARTESIAN_POINT('Ctrl Pts',(52.6679975407064,20.2471953906567,22.2818414848108));
#35743=CARTESIAN_POINT('Ctrl Pts',(52.6945763612259,20.1648607794609,22.2863393859312));
#35744=CARTESIAN_POINT('Ctrl Pts',(52.7254865272691,20.0840391011955,22.2908372870515));
#35745=CARTESIAN_POINT('Ctrl Pts',(52.760516573242,20.0051813073348,22.2953351881719));
#35746=CARTESIAN_POINT('Ctrl Pts',(52.7955466192149,19.9263235134742,22.2998330892922));
#35747=CARTESIAN_POINT('Ctrl Pts',(52.8346962709619,19.8494299791551,22.3043309904125));
#35748=CARTESIAN_POINT('Ctrl Pts',(52.8777058399428,19.7749213297967,22.3088288915329));
#35749=CARTESIAN_POINT('Ctrl Pts',(52.918165369112,19.7048303025322,22.3130601118378));
#35750=CARTESIAN_POINT('Ctrl Pts',(52.9621767339345,19.6366143434541,22.3172913321427));
#35751=CARTESIAN_POINT('Ctrl Pts',(53.0095411218324,19.5706561979973,22.3215225524477));
#35752=CARTESIAN_POINT('Ctrl Pts',(53.0568375925131,19.5047926319045,22.3257477054788));
#35753=CARTESIAN_POINT('Ctrl Pts',(53.107477268325,19.4411808238766,22.32997285851));
#35754=CARTESIAN_POINT('Ctrl Pts',(53.1612162242584,19.3801776405823,22.3341980115412));
#35755=CARTESIAN_POINT('Ctrl Pts',(53.215093233406,19.3190177425662,22.3384340188204));
#35756=CARTESIAN_POINT('Ctrl Pts',(53.2720852253751,19.2604802949272,22.3426700260996));
#35757=CARTESIAN_POINT('Ctrl Pts',(53.3319034944793,19.2048943489952,22.3469060333788));
#35758=CARTESIAN_POINT('Ctrl Pts',(53.3914611494878,19.1495505779246,22.3511235853729));
#35759=CARTESIAN_POINT('Ctrl Pts',(53.4538201689723,19.0971329686796,22.3553411373671));
#35760=CARTESIAN_POINT('Ctrl Pts',(53.5186575666153,19.0479306249382,22.3595586893613));
#35761=CARTESIAN_POINT('Ctrl Pts',(53.5834735564246,18.9987445266915,22.3637748488157));
#35762=CARTESIAN_POINT('Ctrl Pts',(53.6507659292892,18.9527718665722,22.3679910082701));
#35763=CARTESIAN_POINT('Ctrl Pts',(53.7201791179804,18.9102610785204,22.3722071677246));
#35764=CARTESIAN_POINT('Ctrl Pts',(53.7895906526959,18.8677513034147,22.3764232267165));
#35765=CARTESIAN_POINT('Ctrl Pts',(53.8611225057065,18.8287034782351,22.3806392857084));
#35766=CARTESIAN_POINT('Ctrl Pts',(53.9343918996012,18.7933215851954,22.3848553447003));
#35767=CARTESIAN_POINT('Ctrl Pts',(54.0082610502981,18.7576500687551,22.3891059148288));
#35768=CARTESIAN_POINT('Ctrl Pts',(54.0838958939356,18.7257050005271,22.3933564849572));
#35769=CARTESIAN_POINT('Ctrl Pts',(54.1608825317766,18.6976463945514,22.3976070550857));
#35770=CARTESIAN_POINT('Ctrl Pts',(54.2373551232628,18.6697751382836,22.4018292437944));
#35771=CARTESIAN_POINT('Ctrl Pts',(54.3151610450022,18.6457386813615,22.4060514325032));
#35772=CARTESIAN_POINT('Ctrl Pts',(54.3938800624636,18.625643482684,22.410273621212));
#35773=CARTESIAN_POINT('Ctrl Pts',(54.4733928000644,18.6053456650663,22.4145383820503));
#35774=CARTESIAN_POINT('Ctrl Pts',(54.5538366742813,18.5890691284264,22.4188031428886));
#35775=CARTESIAN_POINT('Ctrl Pts',(54.6347707087752,18.5768702439136,22.4230679037269));
#35776=CARTESIAN_POINT('Ctrl Pts',(54.7157047432691,18.5646713594007,22.4273326645652));
#35777=CARTESIAN_POINT('Ctrl Pts',(54.7971284522444,18.5565501109006,22.4315974254036));
#35778=CARTESIAN_POINT('Ctrl Pts',(54.8786001934614,18.5525089710129,22.4358621862419));
#35779=CARTESIAN_POINT('Ctrl Pts',(54.9594311940223,18.5484996129747,22.4400934065468));
#35780=CARTESIAN_POINT('Ctrl Pts',(55.0406125788216,18.5484913358027,22.4443246268517));
#35781=CARTESIAN_POINT('Ctrl Pts',(55.1217149510855,18.5525246230693,22.4485558471566));
#35782=CARTESIAN_POINT('Ctrl Pts',(55.202701028224,18.5565521268842,22.4527810001878));
#35783=CARTESIAN_POINT('Ctrl Pts',(55.283607857416,18.5646096622987,22.4570061532189));
#35784=CARTESIAN_POINT('Ctrl Pts',(55.3640033251966,18.5766857757926,22.4612313062501));
#35785=CARTESIAN_POINT('Ctrl Pts',(55.4446053256976,18.5887929123359,22.4654673135293));
#35786=CARTESIAN_POINT('Ctrl Pts',(55.5246928623394,18.6049393174882,22.4697033208085));
#35787=CARTESIAN_POINT('Ctrl Pts',(55.6038329120281,18.6250608293365,22.4739393280877));
#35788=CARTESIAN_POINT('Ctrl Pts',(55.6826281671781,18.6450946765015,22.4781568800818));
#35789=CARTESIAN_POINT('Ctrl Pts',(55.7604837186519,18.6690689580281,22.482374432076));
#35790=CARTESIAN_POINT('Ctrl Pts',(55.8369815210786,18.6968690477151,22.4865919840701));
#35791=CARTESIAN_POINT('Ctrl Pts',(55.9134540656711,18.7246599584448,22.4908081435246));
#35792=CARTESIAN_POINT('Ctrl Pts',(55.9885693148541,18.7562740101354,22.495024302979));
#35793=CARTESIAN_POINT('Ctrl Pts',(56.0619257293278,18.7915471489317,22.4992404624334));
#35794=CARTESIAN_POINT('Ctrl Pts',(56.135280395867,18.8268194472407,22.5034565214253));
#35795=CARTESIAN_POINT('Ctrl Pts',(56.2068758925048,18.8657504568286,22.5076725804172));
#35796=CARTESIAN_POINT('Ctrl Pts',(56.2763332758992,18.9081291581858,22.5118886394091));
#35797=CARTESIAN_POINT('Ctrl Pts',(56.3463592123547,18.9508547562905,22.5161392095375));
#35798=CARTESIAN_POINT('Ctrl Pts',(56.414211452482,18.9970845136542,22.520389779666));
#35799=CARTESIAN_POINT('Ctrl Pts',(56.4795311218914,19.0465574210244,22.5246403497945));
#35800=CARTESIAN_POINT('Ctrl Pts',(56.5444146462899,19.0956999935673,22.5288625385033));
#35801=CARTESIAN_POINT('Ctrl Pts',(56.606798997415,19.1480421892964,22.533084727212));
#35802=CARTESIAN_POINT('Ctrl Pts',(56.6663668643945,19.2032886366342,22.5373069159208));
#35803=CARTESIAN_POINT('Ctrl Pts',(56.7265353513672,19.2590921312946,22.5415716767591));
#35804=CARTESIAN_POINT('Ctrl Pts',(56.7838298984299,19.3178584262345,22.5458364375975));
#35805=CARTESIAN_POINT('Ctrl Pts',(56.8379640335488,19.3792475632038,22.5501011984358));
#35806=CARTESIAN_POINT('Ctrl Pts',(56.8920981686677,19.440636700173,22.5543659592742));
#35807=CARTESIAN_POINT('Ctrl Pts',(56.9430716419734,19.5046482622515,22.5586307201125));
#35808=CARTESIAN_POINT('Ctrl Pts',(56.9906429078337,19.5709125067053,22.5628954809508));
#35809=CARTESIAN_POINT('Ctrl Pts',(57.0378400458841,19.6366556110084,22.5671267012558));
#35810=CARTESIAN_POINT('Ctrl Pts',(57.0818653202519,19.7048625939595,22.5713579215607));
#35811=CARTESIAN_POINT('Ctrl Pts',(57.1224518869003,19.7751946122778,22.5755891418656));
#35812=CARTESIAN_POINT('Ctrl Pts',(57.1629802552527,19.8454257794044,22.5798142948968));
#35813=CARTESIAN_POINT('Ctrl Pts',(57.2000794785399,19.9177755307403,22.5840394479279));
#35814=CARTESIAN_POINT('Ctrl Pts',(57.2335248790578,19.991874578919,22.5882646009591));
#35815=CARTESIAN_POINT('Ctrl Pts',(57.2670561994633,20.0661639845696,22.5925006082383));
#35816=CARTESIAN_POINT('Ctrl Pts',(57.2969146299699,20.1422112991335,22.5967366155175));
#35817=CARTESIAN_POINT('Ctrl Pts',(57.3229192871087,20.2196178913004,22.6009726227967));
#35818=CARTESIAN_POINT('Ctrl Pts',(57.3488106480872,20.2966872411944,22.6051901747908));
#35819=CARTESIAN_POINT('Ctrl Pts',(57.3708815888824,20.3751036083789,22.609407726785));
#35820=CARTESIAN_POINT('Ctrl Pts',(57.3890017491544,20.4544535835172,22.6136252787791));
#35821=CARTESIAN_POINT('Ctrl Pts',(57.4071159265617,20.5337773590989,22.6178414382336));
#35822=CARTESIAN_POINT('Ctrl Pts',(57.4212818104931,20.6140336775829,22.622057597688));
#35823=CARTESIAN_POINT('Ctrl Pts',(57.431419521424,20.6947961978637,22.6262737571424));
#35824=CARTESIAN_POINT('Ctrl Pts',(57.4415569907937,20.7755567937372,22.6304898161343));
#35825=CARTESIAN_POINT('Ctrl Pts',(57.4476664211974,20.8568231059859,22.6347058751262));
#35826=CARTESIAN_POINT('Ctrl Pts',(57.4497196473359,20.9381623136237,22.6389219341181));
#35827=CARTESIAN_POINT('Ctrl Pts',(57.4517896804423,21.0201673346456,22.6431725042466));
#35828=CARTESIAN_POINT('Ctrl Pts',(57.4497367693757,21.1022459707963,22.6474230743751));
#35829=CARTESIAN_POINT('Ctrl Pts',(57.4435856338116,21.1839551582031,22.6516736445035));
#35830=CARTESIAN_POINT('Ctrl Pts',(57.437475569905,21.2651187663879,22.6558958332123));
#35831=CARTESIAN_POINT('Ctrl Pts',(57.4273219630985,21.3459173863507,22.660118021921));
#35832=CARTESIAN_POINT('Ctrl Pts',(57.4132009421555,21.4259242453534,22.6643402106298));
#35833=CARTESIAN_POINT('Ctrl Pts',(57.3989375396244,21.5067378097416,22.6686049714681));
#35834=CARTESIAN_POINT('Ctrl Pts',(57.3806263745226,21.5867430831721,22.6728697323065));
#35835=CARTESIAN_POINT('Ctrl Pts',(57.358397760404,21.6655150289222,22.6771344931448));
#35836=CARTESIAN_POINT('Ctrl Pts',(57.3361691462854,21.7442869746723,22.6813992539832));
#35837=CARTESIAN_POINT('Ctrl Pts',(57.3100232979766,21.8218251567298,22.6856640148215));
#35838=CARTESIAN_POINT('Ctrl Pts',(57.2801399150844,21.8977261373262,22.6899287756598));
#35839=CARTESIAN_POINT('Ctrl Pts',(57.2504915523118,21.9730301889339,22.6941599959648));
#35840=CARTESIAN_POINT('Ctrl Pts',(57.2170530977956,22.0470050972885,22.6983912162697));
#35841=CARTESIAN_POINT('Ctrl Pts',(57.1799645709816,22.1192429223655,22.7026224365747));
#35842=CARTESIAN_POINT('Ctrl Pts',(57.1429292265191,22.1913771634574,22.7068475896058));
#35843=CARTESIAN_POINT('Ctrl Pts',(57.1022544153297,22.2617788581933,22.711072742637));
#35844=CARTESIAN_POINT('Ctrl Pts',(57.0581286005639,22.3300589887449,22.7152978956682));
#35845=CARTESIAN_POINT('Ctrl Pts',(57.0138894283566,22.3985145282026,22.7195339029474));
#35846=CARTESIAN_POINT('Ctrl Pts',(56.9661816777924,22.4648371522518,22.7237699102266));
#35847=CARTESIAN_POINT('Ctrl Pts',(56.9152422140318,22.5286587296027,22.7280059175058));
#35848=CARTESIAN_POINT('Ctrl Pts',(56.8645246815052,22.5922022513878,22.7322234694999));
#35849=CARTESIAN_POINT('Ctrl Pts',(56.8106038221552,22.6532661031908,22.7364410214941));
#35850=CARTESIAN_POINT('Ctrl Pts',(56.7537563129064,22.7115165920729,22.7406585734883));
#35851=CARTESIAN_POINT('Ctrl Pts',(56.696927573412,22.7697478479687,22.7448747329427));
#35852=CARTESIAN_POINT('Ctrl Pts',(56.6371744274441,22.8251672531546,22.7490908923972));
#35853=CARTESIAN_POINT('Ctrl Pts',(56.5748117894574,22.8774765185712,22.7533070518516));
#35854=CARTESIAN_POINT('Ctrl Pts',(56.5124506374458,22.9297845375639,22.7575231108435));
#35855=CARTESIAN_POINT('Ctrl Pts',(56.4474804739603,22.9789822662016,22.7617391698355));
#35856=CARTESIAN_POINT('Ctrl Pts',(56.3802496986626,23.0248113540135,22.7659552288274));
#35857=CARTESIAN_POINT('Ctrl Pts',(56.3124685965145,23.0710155821898,22.7702057989558));
#35858=CARTESIAN_POINT('Ctrl Pts',(56.2423900899683,23.1137954825678,22.7744563690843));
#35859=CARTESIAN_POINT('Ctrl Pts',(56.1703998605091,23.1529315865861,22.7787069392127));
#35860=CARTESIAN_POINT('Ctrl Pts',(56.098890315959,23.1918063754963,22.7829291279215));
#35861=CARTESIAN_POINT('Ctrl Pts',(56.025494950164,23.2270857320517,22.7871513166303));
#35862=CARTESIAN_POINT('Ctrl Pts',(55.9506136313523,23.2586022168339,22.791373505339));
#35863=CARTESIAN_POINT('Ctrl Pts',(55.8749772877364,23.2904364808451,22.7956382661773));
#35864=CARTESIAN_POINT('Ctrl Pts',(55.7978253135168,23.3184313985612,22.7999030270156));
#35865=CARTESIAN_POINT('Ctrl Pts',(55.7195854984368,23.3424659998471,22.8041677878539));
#35866=CARTESIAN_POINT('Ctrl Pts',(55.6413456833568,23.3665006011329,22.8084325486922));
#35867=CARTESIAN_POINT('Ctrl Pts',(55.5620185102528,23.386574830078,22.8126973095305));
#35868=CARTESIAN_POINT('Ctrl Pts',(55.482040398859,23.4026209238804,22.8169620703688));
#35869=CARTESIAN_POINT('Ctrl Pts',(55.4026912813566,23.4185408219674,22.8211932906737));
#35870=CARTESIAN_POINT('Ctrl Pts',(55.3224038865215,23.4305554604141,22.8254245109786));
#35871=CARTESIAN_POINT('Ctrl Pts',(55.2415969015931,23.438561294522,22.8296557312835));
#35872=CARTESIAN_POINT('Ctrl Pts',(55.1609057882251,23.4465556488241,22.8338808843147));
#35873=CARTESIAN_POINT('Ctrl Pts',(55.079697023254,23.4505525699812,22.8381060373458));
#35874=CARTESIAN_POINT('Ctrl Pts',(54.9983996620546,23.4504994774369,22.842331190377));
#35875=CARTESIAN_POINT('Ctrl Pts',(54.916893451207,23.4504462485,22.8465671976562));
#35876=CARTESIAN_POINT('Ctrl Pts',(54.8352986524015,23.446322084028,22.8508032049354));
#35877=CARTESIAN_POINT('Ctrl Pts',(54.7540530160318,23.4381263976826,22.8550392122146));
#35878=CARTESIAN_POINT('Ctrl Pts',(54.6731613477456,23.4299664180105,22.8592567642088));
#35879=CARTESIAN_POINT('Ctrl Pts',(54.5926162721334,23.4177703586222,22.8634743162029));
#35880=CARTESIAN_POINT('Ctrl Pts',(54.5128481900759,23.401589757658,22.8676918681971));
#35881=CARTESIAN_POINT('Ctrl Pts',(54.4331064456245,23.3854144991601,22.8719080276515));
#35882=CARTESIAN_POINT('Ctrl Pts',(54.3541416405487,23.3652574040454,22.8761241871059));
#35883=CARTESIAN_POINT('Ctrl Pts',(54.2763751613613,23.3412213357359,22.8803403465603));
#35884=CARTESIAN_POINT('Ctrl Pts',(54.1986105351915,23.3171858401572,22.8845564055522));
#35885=CARTESIAN_POINT('Ctrl Pts',(54.1220446219994,23.2892716935036,22.8887724645441));
#35886=CARTESIAN_POINT('Ctrl Pts',(54.0470834068934,23.2576315502274,22.892988523536));
#35887=CARTESIAN_POINT('Ctrl Pts',(53.971508586347,23.2257324121628,22.8972390936645));
#35888=CARTESIAN_POINT('Ctrl Pts',(53.8975653043072,23.1900461683508,22.901489663793));
#35889=CARTESIAN_POINT('Ctrl Pts',(53.8256470909457,23.1507778813712,22.9057402339214));
#35890=CARTESIAN_POINT('Ctrl Pts',(53.7542090816366,23.1117717920973,22.9099624226302));
#35891=CARTESIAN_POINT('Ctrl Pts',(53.6847695483082,23.0692316471731,22.9141846113389));
#35892=CARTESIAN_POINT('Ctrl Pts',(53.6176859967675,23.0234026407187,22.9184068000477));
#35893=CARTESIAN_POINT('Ctrl Pts',(53.5499260449404,22.9771115425537,22.922671560886));
#35894=CARTESIAN_POINT('Ctrl Pts',(53.4845702396638,22.9274651805442,22.9269363217244));
#35895=CARTESIAN_POINT('Ctrl Pts',(53.4219521812646,22.8747574061154,22.9312010825628));
#35896=CARTESIAN_POINT('Ctrl Pts',(53.3593341228654,22.8220496316865,22.9354658434011));
#35897=CARTESIAN_POINT('Ctrl Pts',(53.299454120126,22.7662808202186,22.9397306042395));
#35898=CARTESIAN_POINT('Ctrl Pts',(53.2426057460595,22.7077809245383,22.9439953650778));
#35899=CARTESIAN_POINT('Ctrl Pts',(53.1869656341608,22.6505243926645,22.9481694821773));
#35900=CARTESIAN_POINT('Ctrl Pts',(53.1340088995045,22.5904244190989,22.9523435992767));
#35901=CARTESIAN_POINT('Ctrl Pts',(53.0840457450709,22.527766193833,22.9565177163762));
#35902=CARTESIAN_POINT('Ctrl Pts',(53.0341473180934,22.4651891425358,22.9606864258911));
#35903=CARTESIAN_POINT('Ctrl Pts',(52.987235075695,22.4000607818049,22.964855135406));
#35904=CARTESIAN_POINT('Ctrl Pts',(52.9435826130974,22.3327031855761,22.9690238449209));
#35905=CARTESIAN_POINT('Ctrl Pts',(52.8999724782983,22.2654109029308,22.9731885122287));
#35906=CARTESIAN_POINT('Ctrl Pts',(52.8596161114748,22.1958940718837,22.9773531795364));
#35907=CARTESIAN_POINT('Ctrl Pts',(52.8227459819001,22.1245066432297,22.9815178468442));
#35908=CARTESIAN_POINT('Ctrl Pts',(52.7858995965409,22.0531651877935,22.9856798321229));
#35909=CARTESIAN_POINT('Ctrl Pts',(52.7525352111079,21.9799559496433,22.9898418174016));
#35910=CARTESIAN_POINT('Ctrl Pts',(52.7228403545881,21.9052591890214,22.9940038026803));
#35911=CARTESIAN_POINT('Ctrl Pts',(52.6931444373135,21.8305597600938,22.9981659366328));
#35912=CARTESIAN_POINT('Ctrl Pts',(52.6671185050231,21.7543731400044,23.0023280705853));
#35913=CARTESIAN_POINT('Ctrl Pts',(52.644902245445,21.6771003001696,23.0064902045377));
#35914=CARTESIAN_POINT('Ctrl Pts',(52.622686792589,21.5998302662847,23.0106521873538));
#35915=CARTESIAN_POINT('Ctrl Pts',(52.6042808618236,21.5214745534456,23.0148141701699));
#35916=CARTESIAN_POINT('Ctrl Pts',(52.5897738661255,21.4424480009992,23.018976152986));
#35917=CARTESIAN_POINT('Ctrl Pts',(52.5752530319411,21.3633460636921,23.0231421059929));
#35918=CARTESIAN_POINT('Ctrl Pts',(52.564638639425,21.2835724816293,23.0273080589998));
#35919=CARTESIAN_POINT('Ctrl Pts',(52.5579685557735,21.2035501790938,23.0314740120067));
#35920=CARTESIAN_POINT('Ctrl Pts',(52.5522587910044,21.1350490106478,23.0350401759338));
#35921=CARTESIAN_POINT('Ctrl Pts',(52.5494384806997,21.0663658657097,23.0386063398609));
#35922=CARTESIAN_POINT('Ctrl Pts',(52.5495010182643,20.9977660545166,23.042172503788));
#35923=CARTESIAN_POINT('',(52.5493390396331,21.0010204409205,23.842172503788));
#35924=CARTESIAN_POINT('Ctrl Pts',(52.5493375787181,20.9977659055204,23.042172503788));
#35925=CARTESIAN_POINT('Ctrl Pts',(52.5476321658041,20.8127232659271,23.0517912224542));
#35926=CARTESIAN_POINT('Ctrl Pts',(52.6512743420045,19.8149599677488,23.1037543726902));
#35927=CARTESIAN_POINT('Ctrl Pts',(54.016468625562,18.2755608973991,23.1980619544957));
#35928=CARTESIAN_POINT('Ctrl Pts',(56.7558779128847,18.6963517752573,23.3250952492048));
#35929=CARTESIAN_POINT('Ctrl Pts',(57.8876820693198,21.2262623582219,23.4521285439137));
#35930=CARTESIAN_POINT('Ctrl Pts',(56.3756506396827,23.5490170077549,23.5791618386227));
#35931=CARTESIAN_POINT('Ctrl Pts',(53.6041335644077,23.5380030107376,23.7061951333316));
#35932=CARTESIAN_POINT('Ctrl Pts',(52.5734000928234,21.9267438999263,23.7938653550534));
#35933=CARTESIAN_POINT('Ctrl Pts',(52.5456780645203,21.0581726905573,23.8391911452055));
#35934=CARTESIAN_POINT('Ctrl Pts',(52.5459788927558,21.0010218400661,23.842172503788));
#35935=CARTESIAN_POINT('',(52.5495005229243,21.0016008908874,24.6421725037586));
#35936=CARTESIAN_POINT('Ctrl Pts',(52.5495002124388,21.0010203738091,23.842172503788));
#35937=CARTESIAN_POINT('Ctrl Pts',(52.5494668326451,20.9208564408857,23.8463603929974));
#35938=CARTESIAN_POINT('Ctrl Pts',(52.5533713350428,20.8405326990059,23.8505482822069));
#35939=CARTESIAN_POINT('Ctrl Pts',(52.56123452562,20.7604729431319,23.8547361714163));
#35940=CARTESIAN_POINT('Ctrl Pts',(52.5694901515391,20.6764175728358,23.8591330693886));
#35941=CARTESIAN_POINT('Ctrl Pts',(52.5821100009684,20.5926537422153,23.8635299673608));
#35942=CARTESIAN_POINT('Ctrl Pts',(52.5990562459595,20.5096742512026,23.867926865333));
#35943=CARTESIAN_POINT('Ctrl Pts',(52.6151575944103,20.4308319059056,23.8721045451902));
#35944=CARTESIAN_POINT('Ctrl Pts',(52.6351641859981,20.3526981031234,23.8762822250473));
#35945=CARTESIAN_POINT('Ctrl Pts',(52.658990506447,20.2756901208084,23.8804599049045));
#35946=CARTESIAN_POINT('Ctrl Pts',(52.6828042394724,20.1987228217407,23.8846353776972));
#35947=CARTESIAN_POINT('Ctrl Pts',(52.7104335572416,20.1228806160397,23.8888108504898));
#35948=CARTESIAN_POINT('Ctrl Pts',(52.7417425205983,20.0485677077552,23.8929863232825));
#35949=CARTESIAN_POINT('Ctrl Pts',(52.7730450047718,19.9742701780362,23.8971609319887));
#35950=CARTESIAN_POINT('Ctrl Pts',(52.8080254378594,19.9015017549563,23.9013355406949));
#35951=CARTESIAN_POINT('Ctrl Pts',(52.8464995341962,19.8306471902019,23.905510149401));
#35952=CARTESIAN_POINT('Ctrl Pts',(52.8849780324974,19.7597845187132,23.9096852357397));
#35953=CARTESIAN_POINT('Ctrl Pts',(52.9269507585838,19.6908365565364,23.9138603220784));
#35954=CARTESIAN_POINT('Ctrl Pts',(52.9721879835204,19.6241625547249,23.9180354084171));
#35955=CARTESIAN_POINT('Ctrl Pts',(53.0174728968491,19.5574182661983,23.922214896068));
#35956=CARTESIAN_POINT('Ctrl Pts',(53.0660289078327,19.4929531144201,23.926394383719));
#35957=CARTESIAN_POINT('Ctrl Pts',(53.1175840045912,19.4310958377806,23.93057387137));
#35958=CARTESIAN_POINT('Ctrl Pts',(53.1691707310827,19.3692006108848,23.9347559231918));
#35959=CARTESIAN_POINT('Ctrl Pts',(53.2237598811306,19.3099167901632,23.9389379750137));
#35960=CARTESIAN_POINT('Ctrl Pts',(53.28104210512,19.253536715064,23.9431200268356));
#35961=CARTESIAN_POINT('Ctrl Pts',(53.3384170143248,19.1970654144667,23.9473088454054));
#35962=CARTESIAN_POINT('Ctrl Pts',(53.3984933359345,19.1435075469078,23.9514976639753));
#35963=CARTESIAN_POINT('Ctrl Pts',(53.4609287307505,19.0931151376733,23.9556864825451));
#35964=CARTESIAN_POINT('Ctrl Pts',(53.4836604329225,19.0747680888266,23.9572115626133));
#35965=CARTESIAN_POINT('Ctrl Pts',(53.5067045739923,19.0568402232667,23.9587366426815));
#35966=CARTESIAN_POINT('Ctrl Pts',(53.5300437569289,19.0393422293892,23.9602617227496));
#35967=CARTESIAN_POINT('Ctrl Pts',(53.5947965700661,18.9907953573373,23.9644929430516));
#35968=CARTESIAN_POINT('Ctrl Pts',(53.6620783416047,18.945368707485,23.9687241633536));
#35969=CARTESIAN_POINT('Ctrl Pts',(53.7315558201613,18.9033360754204,23.9729553836556));
#35970=CARTESIAN_POINT('Ctrl Pts',(53.8009336728765,18.8613637152083,23.9771805366839));
#35971=CARTESIAN_POINT('Ctrl Pts',(53.8725005850379,18.8227759456113,23.9814056897121));
#35972=CARTESIAN_POINT('Ctrl Pts',(53.9458919955203,18.7878050346111,23.9856308427403));
#35973=CARTESIAN_POINT('Ctrl Pts',(54.0194719456453,18.7527442847182,23.9898668500203));
#35974=CARTESIAN_POINT('Ctrl Pts',(54.0948853987074,18.7213192783467,23.9941028573002));
#35975=CARTESIAN_POINT('Ctrl Pts',(54.1717375500737,18.6937191055637,23.9983388645801));
#35976=CARTESIAN_POINT('Ctrl Pts',(54.2482548746696,18.6662391802499,24.0025564165714));
#35977=CARTESIAN_POINT('Ctrl Pts',(54.3261979500002,18.6425509960614,24.0067739685627));
#35978=CARTESIAN_POINT('Ctrl Pts',(54.4051561515476,18.6227934364136,24.010991520554));
#35979=CARTESIAN_POINT('Ctrl Pts',(54.4840882828935,18.6030424002623,24.0152076800056));
#35980=CARTESIAN_POINT('Ctrl Pts',(54.5640344241906,18.5872195241659,24.0194238394571));
#35981=CARTESIAN_POINT('Ctrl Pts',(54.6445699777732,18.5754134890048,24.0236399989087));
#35982=CARTESIAN_POINT('Ctrl Pts',(54.7251036123572,18.5636077351575,24.0278560578978));
#35983=CARTESIAN_POINT('Ctrl Pts',(54.8062261711365,18.5558186982803,24.0320721168868));
#35984=CARTESIAN_POINT('Ctrl Pts',(54.8875055082934,18.5520834901215,24.0362881758759));
#35985=CARTESIAN_POINT('Ctrl Pts',(54.969450168877,18.5483177068919,24.0405387460078));
#35986=CARTESIAN_POINT('Ctrl Pts',(55.0515537078735,18.5486724631353,24.0447893161397));
#35987=CARTESIAN_POINT('Ctrl Pts',(55.1333726448945,18.5531322088037,24.0490398862716));
#35988=CARTESIAN_POINT('Ctrl Pts',(55.214645269768,18.557562176363,24.0532620749776));
#35989=CARTESIAN_POINT('Ctrl Pts',(55.2956366211994,18.5660423711746,24.0574842636836));
#35990=CARTESIAN_POINT('Ctrl Pts',(55.3759184431055,18.5785055081349,24.0617064523897));
#35991=CARTESIAN_POINT('Ctrl Pts',(55.4570097430109,18.5910943103445,24.0659712132345));
#35992=CARTESIAN_POINT('Ctrl Pts',(55.5373766488547,18.6077467278717,24.0702359740793));
#35993=CARTESIAN_POINT('Ctrl Pts',(55.6165915194357,18.6283412665057,24.0745007349242));
#35994=CARTESIAN_POINT('Ctrl Pts',(55.6958063900168,18.6489358051396,24.078765495769));
#35995=CARTESIAN_POINT('Ctrl Pts',(55.7738687849726,18.6734722591182,24.0830302566138));
#35996=CARTESIAN_POINT('Ctrl Pts',(55.8503716359342,18.7017793119897,24.0872950174587));
#35997=CARTESIAN_POINT('Ctrl Pts',(55.9262728243055,18.7298637418538,24.0915262377619));
#35998=CARTESIAN_POINT('Ctrl Pts',(56.0009235480879,18.7617649446338,24.0957574580651));
#35999=CARTESIAN_POINT('Ctrl Pts',(56.0739130583664,18.7973513686767,24.0999886783683));
#36000=CARTESIAN_POINT('Ctrl Pts',(56.1467979067951,18.832886764278,24.1042138313977));
#36001=CARTESIAN_POINT('Ctrl Pts',(56.2180258583051,18.8720966839983,24.1084389844271));
#36002=CARTESIAN_POINT('Ctrl Pts',(56.2872040801193,18.914800751457,24.1126641374566));
#36003=CARTESIAN_POINT('Ctrl Pts',(56.356560018036,18.9576145239678,24.1169001447362));
#36004=CARTESIAN_POINT('Ctrl Pts',(56.4238552409761,19.0039402500301,24.1211361520158));
#36005=CARTESIAN_POINT('Ctrl Pts',(56.488716797084,19.0535487295902,24.1253721592954));
#36006=CARTESIAN_POINT('Ctrl Pts',(56.5532957666491,19.1029410766741,24.1295897112878));
#36007=CARTESIAN_POINT('Ctrl Pts',(56.6154618543834,19.1555873547957,24.1338072632801));
#36008=CARTESIAN_POINT('Ctrl Pts',(56.6748757159482,19.2112178483317,24.1380248152724));
#36009=CARTESIAN_POINT('Ctrl Pts',(56.7342699604073,19.266829973944,24.142240974725));
#36010=CARTESIAN_POINT('Ctrl Pts',(56.7909134441815,19.3254240407466,24.1464571341776));
#36011=CARTESIAN_POINT('Ctrl Pts',(56.8445014283317,19.3866913714721,24.1506732936302));
#36012=CARTESIAN_POINT('Ctrl Pts',(56.8980881355884,19.4479572423209,24.1548893526202));
#36013=CARTESIAN_POINT('Ctrl Pts',(56.948619182728,19.5118958997652,24.1591054116102));
#36014=CARTESIAN_POINT('Ctrl Pts',(56.9958290682475,19.5781643624039,24.1633214706002));
#36015=CARTESIAN_POINT('Ctrl Pts',(57.0434253968885,19.644975274813,24.1675720407308));
#36016=CARTESIAN_POINT('Ctrl Pts',(57.0876456498621,19.7141539289657,24.1718226108614));
#36017=CARTESIAN_POINT('Ctrl Pts',(57.128262428118,19.7853192653783,24.176073180992));
#36018=CARTESIAN_POINT('Ctrl Pts',(57.1686080046385,19.8560094246949,24.1802953696989));
#36019=CARTESIAN_POINT('Ctrl Pts',(57.2053979243557,19.9286593697791,24.1845175584057));
#36020=CARTESIAN_POINT('Ctrl Pts',(57.238456512793,20.0028727812688,24.1887397471126));
#36021=CARTESIAN_POINT('Ctrl Pts',(57.2718484294658,20.0778344831929,24.1930045079551));
#36022=CARTESIAN_POINT('Ctrl Pts',(57.3014331705383,20.154390904565,24.1972692687976));
#36023=CARTESIAN_POINT('Ctrl Pts',(57.3270809433459,20.2321168493083,24.2015340296401));
#36024=CARTESIAN_POINT('Ctrl Pts',(57.3527287161536,20.3098427940516,24.2057987904826));
#36025=CARTESIAN_POINT('Ctrl Pts',(57.3744394548109,20.3887377805894,24.2100635513251));
#36026=CARTESIAN_POINT('Ctrl Pts',(57.3921363841013,20.468366884159,24.2143283121676));
#36027=CARTESIAN_POINT('Ctrl Pts',(57.4096941346004,20.5473697388351,24.2185595324873));
#36028=CARTESIAN_POINT('Ctrl Pts',(57.423366868251,20.6273914465543,24.2227907528071));
#36029=CARTESIAN_POINT('Ctrl Pts',(57.4330424023754,20.708015551367,24.2270219731268));
#36030=CARTESIAN_POINT('Ctrl Pts',(57.4427040624612,20.7885240468576,24.2312471261729));
#36031=CARTESIAN_POINT('Ctrl Pts',(57.448379851686,20.8696327661643,24.2354722792189));
#36032=CARTESIAN_POINT('Ctrl Pts',(57.4500083261566,20.9509138332773,24.239697432265));
#36033=CARTESIAN_POINT('Ctrl Pts',(57.4516409841053,21.0324037078212,24.2439334395404));
#36034=CARTESIAN_POINT('Ctrl Pts',(57.4492054098064,21.1140663546487,24.2481694468159));
#36035=CARTESIAN_POINT('Ctrl Pts',(57.4426919626134,21.1954641291484,24.2524054540914));
#36036=CARTESIAN_POINT('Ctrl Pts',(57.4362068929457,21.2765072730917,24.2566230061005));
#36037=CARTESIAN_POINT('Ctrl Pts',(57.4256794380758,21.3572873808308,24.2608405581095));
#36038=CARTESIAN_POINT('Ctrl Pts',(57.4111522227015,21.4373730775457,24.2650581101185));
#36039=CARTESIAN_POINT('Ctrl Pts',(57.3966298038832,21.5174323317849,24.2692742695878));
#36040=CARTESIAN_POINT('Ctrl Pts',(57.3781103300617,21.596797173218,24.2734904290571));
#36041=CARTESIAN_POINT('Ctrl Pts',(57.355687926689,21.6750441778517,24.2777065885264));
#36042=CARTESIAN_POINT('Ctrl Pts',(57.3332660575971,21.7532893180169,24.2819226475331));
#36043=CARTESIAN_POINT('Ctrl Pts',(57.3069415729986,21.8304162277134,24.2861387065398));
#36044=CARTESIAN_POINT('Ctrl Pts',(57.2768586972871,21.9060158511793,24.2903547655465));
#36045=CARTESIAN_POINT('Ctrl Pts',(57.2465295742494,21.982234305282,24.2946053356573));
#36046=CARTESIAN_POINT('Ctrl Pts',(57.2123804089379,22.0568999024811,24.2988559057682));
#36047=CARTESIAN_POINT('Ctrl Pts',(57.1746080802747,22.1296149552853,24.303106475879));
#36048=CARTESIAN_POINT('Ctrl Pts',(57.1370879603909,22.2018444840201,24.3073286646023));
#36049=CARTESIAN_POINT('Ctrl Pts',(57.0959932043955,22.2721490627644,24.3115508533255));
#36050=CARTESIAN_POINT('Ctrl Pts',(57.051561559298,22.3401661905938,24.3157730420488));
#36051=CARTESIAN_POINT('Ctrl Pts',(57.0066819125277,22.4088691311359,24.3200378028534));
#36052=CARTESIAN_POINT('Ctrl Pts',(56.9583979923833,22.4752378398237,24.3243025636581));
#36053=CARTESIAN_POINT('Ctrl Pts',(56.9069966872212,22.5389327096815,24.3285673244627));
#36054=CARTESIAN_POINT('Ctrl Pts',(56.8555953820591,22.6026275795392,24.3328320852674));
#36055=CARTESIAN_POINT('Ctrl Pts',(56.8010770607924,22.6636482940861,24.337096846072));
#36056=CARTESIAN_POINT('Ctrl Pts',(56.74376553338,22.7216945183731,24.3413616068767));
#36057=CARTESIAN_POINT('Ctrl Pts',(56.686904736685,22.7792842338651,24.3455928271567));
#36058=CARTESIAN_POINT('Ctrl Pts',(56.6270813226942,22.8341620652118,24.3498240474367));
#36059=CARTESIAN_POINT('Ctrl Pts',(56.564584384522,22.8860079410517,24.3540552677167));
#36060=CARTESIAN_POINT('Ctrl Pts',(56.5021770625848,22.9377794735343,24.3582804207229));
#36061=CARTESIAN_POINT('Ctrl Pts',(56.4371041851804,22.9865273908568,24.3625055737292));
#36062=CARTESIAN_POINT('Ctrl Pts',(56.3696919526391,23.0319680619723,24.3667307267355));
#36063=CARTESIAN_POINT('Ctrl Pts',(56.3021065402889,23.0775254686779,24.3709667340209));
#36064=CARTESIAN_POINT('Ctrl Pts',(56.232170074164,23.1197582836417,24.3752027413063));
#36065=CARTESIAN_POINT('Ctrl Pts',(56.1602450513843,23.1584211059796,24.3794387485917));
#36066=CARTESIAN_POINT('Ctrl Pts',(56.0886333894946,23.1969154832347,24.3836563005613));
#36067=CARTESIAN_POINT('Ctrl Pts',(56.0150508704219,23.2318706815473,24.3878738525309));
#36068=CARTESIAN_POINT('Ctrl Pts',(55.939883062584,23.2630886148509,24.3920914045004));
#36069=CARTESIAN_POINT('Ctrl Pts',(55.8647400734435,23.2942962407042,24.3963075639304));
#36070=CARTESIAN_POINT('Ctrl Pts',(55.7880132640168,23.3217688738396,24.4005237233604));
#36071=CARTESIAN_POINT('Ctrl Pts',(55.7101094469895,23.3453560120579,24.4047398827904));
#36072=CARTESIAN_POINT('Ctrl Pts',(55.6322074862489,23.3689425882436,24.4089559417581));
#36073=CARTESIAN_POINT('Ctrl Pts',(55.5531290189643,23.3886437199271,24.4131720007257));
#36074=CARTESIAN_POINT('Ctrl Pts',(55.4732959498653,23.4043587905804,24.4173880596934));
#36075=CARTESIAN_POINT('Ctrl Pts',(55.3928093950728,23.4202024993276,24.4216386298511));
#36076=CARTESIAN_POINT('Ctrl Pts',(55.3115562952131,23.4319944804183,24.4258892000088));
#36077=CARTESIAN_POINT('Ctrl Pts',(55.2299775534543,23.4396845236438,24.4301397701664));
#36078=CARTESIAN_POINT('Ctrl Pts',(55.1489435209287,23.4473232196991,24.4343619588517));
#36079=CARTESIAN_POINT('Ctrl Pts',(55.0675886537223,23.4509146302014,24.4385841475369));
#36080=CARTESIAN_POINT('Ctrl Pts',(54.9863464495475,23.4504619626838,24.4428063362221));
#36081=CARTESIAN_POINT('Ctrl Pts',(54.904285082534,23.4500047309325,24.447071097116));
#36082=CARTESIAN_POINT('Ctrl Pts',(54.8223391483354,23.4454214366196,24.4513358580099));
#36083=CARTESIAN_POINT('Ctrl Pts',(54.7409495539087,23.4367689911807,24.4556006189038));
#36084=CARTESIAN_POINT('Ctrl Pts',(54.659559959482,23.4281165457418,24.4598653797978));
#36085=CARTESIAN_POINT('Ctrl Pts',(54.5787271707783,23.415395087548,24.4641301406917));
#36086=CARTESIAN_POINT('Ctrl Pts',(54.4988791167051,23.3987138450273,24.4683949015856));
#36087=CARTESIAN_POINT('Ctrl Pts',(54.4196590347824,23.3821637936279,24.4726261218866));
#36088=CARTESIAN_POINT('Ctrl Pts',(54.3411111780572,23.3616540035517,24.4768573421877));
#36089=CARTESIAN_POINT('Ctrl Pts',(54.2636612344112,23.337253831378,24.4810885624888));
#36090=CARTESIAN_POINT('Ctrl Pts',(54.1863223485687,23.312888647345,24.4853137155158));
#36091=CARTESIAN_POINT('Ctrl Pts',(54.1100786887618,23.2846442991288,24.4895388685429));
#36092=CARTESIAN_POINT('Ctrl Pts',(54.0353454447737,23.2526410808385,24.4937640215699));
#36093=CARTESIAN_POINT('Ctrl Pts',(53.9604202139999,23.2205556475299,24.4980000288501));
#36094=CARTESIAN_POINT('Ctrl Pts',(53.8870136301012,23.1846921094567,24.5022360361303));
#36095=CARTESIAN_POINT('Ctrl Pts',(53.8155284414307,23.1452219878,24.5064720434105));
#36096=CARTESIAN_POINT('Ctrl Pts',(53.7443546969706,23.1059238282112,24.5106895953999));
#36097=CARTESIAN_POINT('Ctrl Pts',(53.6750860540547,23.0630506645706,24.5149071473893));
#36098=CARTESIAN_POINT('Ctrl Pts',(53.6080980152219,23.0168190585104,24.5191246993788));
#36099=CARTESIAN_POINT('Ctrl Pts',(53.5411320943189,22.9706027170771,24.5233408588283));
#36100=CARTESIAN_POINT('Ctrl Pts',(53.4764456644804,22.9210303991786,24.5275570182777));
#36101=CARTESIAN_POINT('Ctrl Pts',(53.4143857657028,22.8683623176446,24.5317731777272));
#36102=CARTESIAN_POINT('Ctrl Pts',(53.3523273456901,22.8156954910869,24.535989236714));
#36103=CARTESIAN_POINT('Ctrl Pts',(53.2928956860611,22.7599333492358,24.5402052957007));
#36104=CARTESIAN_POINT('Ctrl Pts',(53.2364040943428,22.7013758348904,24.5444213546874));
#36105=CARTESIAN_POINT('Ctrl Pts',(53.1794500827098,22.6423389897284,24.5486719248214));
#36106=CARTESIAN_POINT('Ctrl Pts',(53.125484838457,22.580461131107,24.5529224949553));
#36107=CARTESIAN_POINT('Ctrl Pts',(53.0747896172992,22.5160854963824,24.5571730650892));
#36108=CARTESIAN_POINT('Ctrl Pts',(53.0244328925937,22.4521397034352,24.5613952537924));
#36109=CARTESIAN_POINT('Ctrl Pts',(52.97730287682,22.3857298072079,24.5656174424955));
#36110=CARTESIAN_POINT('Ctrl Pts',(52.933631926826,22.3172217870074,24.5698396311986));
#36111=CARTESIAN_POINT('Ctrl Pts',(52.8895206445309,22.2480230034006,24.574104392048));
#36112=CARTESIAN_POINT('Ctrl Pts',(52.8489388160609,22.1766839693441,24.5783691528973));
#36113=CARTESIAN_POINT('Ctrl Pts',(52.8120776917919,22.1036060090655,24.5826339137466));
#36114=CARTESIAN_POINT('Ctrl Pts',(52.775216567523,22.0305280487869,24.5868986745959));
#36115=CARTESIAN_POINT('Ctrl Pts',(52.7420762838396,21.9557116288227,24.5911634354452));
#36116=CARTESIAN_POINT('Ctrl Pts',(52.7127970955513,21.8795755362,24.5954281962945));
#36117=CARTESIAN_POINT('Ctrl Pts',(52.6797334709213,21.7935985903062,24.6002441922323));
#36118=CARTESIAN_POINT('Ctrl Pts',(52.6514890713543,21.7056709150828,24.6050601881701));
#36119=CARTESIAN_POINT('Ctrl Pts',(52.6282678414551,21.6163090281052,24.6098761841079));
#36120=CARTESIAN_POINT('Ctrl Pts',(52.6051398843363,21.5273060812737,24.6146728356211));
#36121=CARTESIAN_POINT('Ctrl Pts',(52.586994953676,21.4368806120397,24.6194694871343));
#36122=CARTESIAN_POINT('Ctrl Pts',(52.5739877880387,21.3455647514063,24.6242661386475));
#36123=CARTESIAN_POINT('Ctrl Pts',(52.5610695804394,21.2548734142115,24.6290299851116));
#36124=CARTESIAN_POINT('Ctrl Pts',(52.5532192128864,21.1633040306489,24.6337938315756));
#36125=CARTESIAN_POINT('Ctrl Pts',(52.5505403056274,21.0713964680082,24.6385576780397));
#36126=CARTESIAN_POINT('Ctrl Pts',(52.5498627171191,21.0481498595023,24.639762619946));
#36127=CARTESIAN_POINT('Ctrl Pts',(52.5495157320829,21.024881700089,24.6409675618523));
#36128=CARTESIAN_POINT('Ctrl Pts',(52.5495005229243,21.0016008908875,24.6421725037586));
#36129=CARTESIAN_POINT('',(52.5495007252096,20.9981147276813,25.442172503788));
#36130=CARTESIAN_POINT('Ctrl Pts',(52.5495005229239,21.0016008903187,24.642172503788));
#36131=CARTESIAN_POINT('Ctrl Pts',(52.5494469895352,20.919656774874,24.6464136750385));
#36132=CARTESIAN_POINT('Ctrl Pts',(52.5535080759981,20.8376904850347,24.6506548462889));
#36133=CARTESIAN_POINT('Ctrl Pts',(52.5616638957009,20.7561408347598,24.6548960175394));
#36134=CARTESIAN_POINT('Ctrl Pts',(52.5698203090628,20.6745852485174,24.659137497503));
#36135=CARTESIAN_POINT('Ctrl Pts',(52.5820720017549,20.5934468167741,24.6633789774667));
#36136=CARTESIAN_POINT('Ctrl Pts',(52.5983472524457,20.5131588244971,24.6676204574304));
#36137=CARTESIAN_POINT('Ctrl Pts',(52.6146284494122,20.4328414984462,24.6718634870481));
#36138=CARTESIAN_POINT('Ctrl Pts',(52.6349360333774,20.3533756766673,24.6761065166659));
#36139=CARTESIAN_POINT('Ctrl Pts',(52.6591475485383,20.2751827468349,24.6803495462836));
#36140=CARTESIAN_POINT('Ctrl Pts',(52.6833913128904,20.1968856657866,24.684598227521));
#36141=CARTESIAN_POINT('Ctrl Pts',(52.711549249218,20.1198652968742,24.6888469087583));
#36142=CARTESIAN_POINT('Ctrl Pts',(52.7434497051681,20.044525763354,24.6930955899957));
#36143=CARTESIAN_POINT('Ctrl Pts',(52.7753750807105,19.9691273770557,24.6973475901637));
#36144=CARTESIAN_POINT('Ctrl Pts',(52.8110485959233,19.8954128500759,24.7015995903318));
#36145=CARTESIAN_POINT('Ctrl Pts',(52.8502524249652,19.8237620930985,24.7058515904999));
#36146=CARTESIAN_POINT('Ctrl Pts',(52.8895250790829,19.7519855481841,24.710111055353));
#36147=CARTESIAN_POINT('Ctrl Pts',(52.9323401763454,19.6822803915989,24.7143705202061));
#36148=CARTESIAN_POINT('Ctrl Pts',(52.9784366254433,19.6149975550018,24.7186299850591));
#36149=CARTESIAN_POINT('Ctrl Pts',(52.9922583006089,19.5948233001543,24.7199071537073));
#36150=CARTESIAN_POINT('Ctrl Pts',(53.0063747167523,19.5748665941868,24.7211843223554));
#36151=CARTESIAN_POINT('Ctrl Pts',(53.0207781605817,19.5551362831154,24.7224614910035));
#36152=CARTESIAN_POINT('Ctrl Pts',(53.0684963230416,19.4897703747783,24.7266927111036));
#36153=CARTESIAN_POINT('Ctrl Pts',(53.1195456006491,19.426648366204,24.7309239312036));
#36154=CARTESIAN_POINT('Ctrl Pts',(53.173687417,19.3661295647525,24.7351551513036));
#36155=CARTESIAN_POINT('Ctrl Pts',(53.2277515977743,19.3056975430281,24.73938030413));
#36156=CARTESIAN_POINT('Ctrl Pts',(53.2848992027025,19.2478616583465,24.7436054569565));
#36157=CARTESIAN_POINT('Ctrl Pts',(53.3448495668384,19.1929506665271,24.7478306097829));
#36158=CARTESIAN_POINT('Ctrl Pts',(53.4049539446849,19.1378986072475,24.7520666171133));
#36159=CARTESIAN_POINT('Ctrl Pts',(53.4678752173697,19.0857868657356,24.7563026244437));
#36160=CARTESIAN_POINT('Ctrl Pts',(53.5332911681543,19.0369117562917,24.7605386317741));
#36161=CARTESIAN_POINT('Ctrl Pts',(53.598422113145,18.9882495871047,24.7647561835655));
#36162=CARTESIAN_POINT('Ctrl Pts',(53.6660256739054,18.9427961925174,24.7689737353569));
#36163=CARTESIAN_POINT('Ctrl Pts',(53.7357498184658,18.9008045044611,24.7731912871483));
#36164=CARTESIAN_POINT('Ctrl Pts',(53.8054509417181,18.8588266810939,24.7774074464011));
#36165=CARTESIAN_POINT('Ctrl Pts',(53.8772708603774,18.8203085341402,24.7816236056539));
#36166=CARTESIAN_POINT('Ctrl Pts',(53.9508294943397,18.7854590769073,24.7858397649068));
#36167=CARTESIAN_POINT('Ctrl Pts',(54.0243863755737,18.7506104500544,24.7900558236985));
#36168=CARTESIAN_POINT('Ctrl Pts',(54.0996814691092,18.7194305371688,24.7942718824902));
#36169=CARTESIAN_POINT('Ctrl Pts',(54.1763123908464,18.6920812465499,24.7984879412819));
#36170=CARTESIAN_POINT('Ctrl Pts',(54.2535705936829,18.6645080816424,24.8027385116512));
#36171=CARTESIAN_POINT('Ctrl Pts',(54.3321861487511,18.6408287178226,24.8069890820204));
#36172=CARTESIAN_POINT('Ctrl Pts',(54.4117304274016,18.6211580212307,24.8112396523896));
#36173=CARTESIAN_POINT('Ctrl Pts',(54.4907435739932,18.6016186695672,24.8154618409037));
#36174=CARTESIAN_POINT('Ctrl Pts',(54.5706726067556,18.5860346440911,24.8196840294178));
#36175=CARTESIAN_POINT('Ctrl Pts',(54.65108832087,18.57446688537,24.8239062179319));
#36176=CARTESIAN_POINT('Ctrl Pts',(54.7323148753122,18.5627824876888,24.8281709792287));
#36177=CARTESIAN_POINT('Ctrl Pts',(54.8140374971521,18.5551958504485,24.8324357405255));
#36178=CARTESIAN_POINT('Ctrl Pts',(54.8958117110061,18.5517158967071,24.8367005018222));
#36179=CARTESIAN_POINT('Ctrl Pts',(54.9775859248601,18.5482359429657,24.840965263119));
#36180=CARTESIAN_POINT('Ctrl Pts',(55.0594112494361,18.5488626047862,24.8452300244158));
#36181=CARTESIAN_POINT('Ctrl Pts',(55.1408483071797,18.5535511441347,24.8494947857125));
#36182=CARTESIAN_POINT('Ctrl Pts',(55.221644889089,18.5582028096541,24.853726006056));
#36183=CARTESIAN_POINT('Ctrl Pts',(55.3023622703535,18.5668700877868,24.8579572263995));
#36184=CARTESIAN_POINT('Ctrl Pts',(55.3825691868474,18.5795473424843,24.862188446743));
#36185=CARTESIAN_POINT('Ctrl Pts',(55.4626610922015,18.5922064188803,24.8664135998108));
#36186=CARTESIAN_POINT('Ctrl Pts',(55.5422435311876,18.6088639798844,24.8706387528786));
#36187=CARTESIAN_POINT('Ctrl Pts',(55.6208880888397,18.6294624594542,24.8748639059464));
#36188=CARTESIAN_POINT('Ctrl Pts',(55.6997346803356,18.6501138554638,24.8790999132162));
#36189=CARTESIAN_POINT('Ctrl Pts',(55.7776380947281,18.6747264104519,24.883335920486));
#36190=CARTESIAN_POINT('Ctrl Pts',(55.8541746453639,18.7031900546154,24.8875719277558));
#36191=CARTESIAN_POINT('Ctrl Pts',(55.9303777450363,18.7315296896684,24.8917894797817));
#36192=CARTESIAN_POINT('Ctrl Pts',(56.005225424915,18.7636867719553,24.8960070318077));
#36193=CARTESIAN_POINT('Ctrl Pts',(56.0783142831877,18.799502656972,24.9002245838336));
#36194=CARTESIAN_POINT('Ctrl Pts',(56.1513790091499,18.8353067163824,24.9044407433179));
#36195=CARTESIAN_POINT('Ctrl Pts',(56.2226856495796,18.8747669750721,24.9086569028023));
#36196=CARTESIAN_POINT('Ctrl Pts',(56.2918524963338,18.9176774078649,24.9128730622866));
#36197=CARTESIAN_POINT('Ctrl Pts',(56.361017694951,18.9605868181698,24.9170891213065));
#36198=CARTESIAN_POINT('Ctrl Pts',(56.428042806785,19.0069459930796,24.9213051803265));
#36199=CARTESIAN_POINT('Ctrl Pts',(56.4925736092709,19.0565046254472,24.9255212393464));
#36200=CARTESIAN_POINT('Ctrl Pts',(56.5576326365779,19.1064689260958,24.929771809436));
#36201=CARTESIAN_POINT('Ctrl Pts',(56.6201559408607,19.1596850256144,24.9340223795256));
#36202=CARTESIAN_POINT('Ctrl Pts',(56.6798145957848,19.2158550580773,24.9382729496151));
#36203=CARTESIAN_POINT('Ctrl Pts',(56.7390749056417,19.2716500392525,24.942495138347));
#36204=CARTESIAN_POINT('Ctrl Pts',(56.7955084237743,19.3303592449377,24.9467173270788));
#36205=CARTESIAN_POINT('Ctrl Pts',(56.8488312214888,19.39165508536,24.9509395158107));
#36206=CARTESIAN_POINT('Ctrl Pts',(56.9026916692801,19.4535689674965,24.9552042765792));
#36207=CARTESIAN_POINT('Ctrl Pts',(56.9533780132041,19.5181215575935,24.9594690373476));
#36208=CARTESIAN_POINT('Ctrl Pts',(57.0006417516066,19.5849442301702,24.9637337981161));
#36209=CARTESIAN_POINT('Ctrl Pts',(57.0479054900091,19.6517669027469,24.9679985588845));
#36210=CARTESIAN_POINT('Ctrl Pts',(57.0917464190062,19.7208592165682,24.972263319653));
#36211=CARTESIAN_POINT('Ctrl Pts',(57.1319638890079,19.7918277333235,24.9765280804214));
#36212=CARTESIAN_POINT('Ctrl Pts',(57.1718650729558,19.8622381256591,24.9807593014284));
#36213=CARTESIAN_POINT('Ctrl Pts',(57.208349251496,19.9347593240248,24.9849905224353));
#36214=CARTESIAN_POINT('Ctrl Pts',(57.2411873194301,20.009025908903,24.9892217434422));
#36215=CARTESIAN_POINT('Ctrl Pts',(57.2739782999067,20.0831860007721,24.9934468971786));
#36216=CARTESIAN_POINT('Ctrl Pts',(57.3031333670747,20.1590860868616,24.9976720509151));
#36217=CARTESIAN_POINT('Ctrl Pts',(57.3284685940376,20.2363349840535,25.0018972046515));
#36218=CARTESIAN_POINT('Ctrl Pts',(57.3538689008839,20.3137823144083,25.0061332117548));
#36219=CARTESIAN_POINT('Ctrl Pts',(57.3754294908446,20.3925849804311,25.0103692188581));
#36220=CARTESIAN_POINT('Ctrl Pts',(57.3930131164161,20.4723273034727,25.0146052259614));
#36221=CARTESIAN_POINT('Ctrl Pts',(57.410520137943,20.5517222246407,25.0188227786637));
#36222=CARTESIAN_POINT('Ctrl Pts',(57.4240846658178,20.6320481774305,25.023040331366));
#36223=CARTESIAN_POINT('Ctrl Pts',(57.4336212655173,20.7128801887332,25.0272578840683));
#36224=CARTESIAN_POINT('Ctrl Pts',(57.443154716448,20.7936855111397,25.0314740442304));
#36225=CARTESIAN_POINT('Ctrl Pts',(57.4486628258277,20.874996098887,25.0356902043925));
#36226=CARTESIAN_POINT('Ctrl Pts',(57.4501117328319,20.9563795158251,25.0399063645546));
#36227=CARTESIAN_POINT('Ctrl Pts',(57.451560605311,21.0377609935332,25.0441224242527));
#36228=CARTESIAN_POINT('Ctrl Pts',(57.4489504605594,21.1192148321139,25.0483384839508));
#36229=CARTESIAN_POINT('Ctrl Pts',(57.4422995483118,21.2003076791242,25.0525545436489));
#36230=CARTESIAN_POINT('Ctrl Pts',(57.4355941965437,21.2820642930798,25.0568051129391));
#36231=CARTESIAN_POINT('Ctrl Pts',(57.4247816456242,21.3634534991379,25.0610556822292));
#36232=CARTESIAN_POINT('Ctrl Pts',(57.4099338219404,21.4440374126894,25.0653062515193));
#36233=CARTESIAN_POINT('Ctrl Pts',(57.395185133105,21.5240832895412,25.0695284409236));
#36234=CARTESIAN_POINT('Ctrl Pts',(57.3764550603819,21.6033341518738,25.0737506303278));
#36235=CARTESIAN_POINT('Ctrl Pts',(57.353864903956,21.6813738063093,25.077972819732));
#36236=CARTESIAN_POINT('Ctrl Pts',(57.3310469843956,21.7602002882448,25.0822375789651));
#36237=CARTESIAN_POINT('Ctrl Pts',(57.3042908635483,21.8377905417839,25.0865023381982));
#36238=CARTESIAN_POINT('Ctrl Pts',(57.2737715302839,21.9137358907641,25.0907670974313));
#36239=CARTESIAN_POINT('Ctrl Pts',(57.2432521970195,21.9896812397442,25.0950318566643));
#36240=CARTESIAN_POINT('Ctrl Pts',(57.2089699115283,22.0639812736087,25.0992966158974));
#36241=CARTESIAN_POINT('Ctrl Pts',(57.1711464576412,22.1362540690674,25.1035613751305));
#36242=CARTESIAN_POINT('Ctrl Pts',(57.1336204695482,22.2079584689332,25.1077925937992));
#36243=CARTESIAN_POINT('Ctrl Pts',(57.0924681360465,22.2779363079199,25.1120238124678));
#36244=CARTESIAN_POINT('Ctrl Pts',(57.0478722692984,22.3457969455451,25.1162550311365));
#36245=CARTESIAN_POINT('Ctrl Pts',(57.0033403499239,22.4135602757322,25.1204801825316));
#36246=CARTESIAN_POINT('Ctrl Pts',(56.9553749572966,22.4792120488663,25.1247053339268));
#36247=CARTESIAN_POINT('Ctrl Pts',(56.9042050477441,22.5423856152551,25.1289304853219));
#36248=CARTESIAN_POINT('Ctrl Pts',(56.8529036599361,22.6057215026325,25.1331664930102));
#36249=CARTESIAN_POINT('Ctrl Pts',(56.7983814910119,22.6665660165,25.1374025006984));
#36250=CARTESIAN_POINT('Ctrl Pts',(56.7409133904935,22.7245784461138,25.1416385083866));
#36251=CARTESIAN_POINT('Ctrl Pts',(56.6836956924912,22.782338101437,25.1458560587572));
#36252=CARTESIAN_POINT('Ctrl Pts',(56.6235580050994,22.8372899630489,25.1500736091279));
#36253=CARTESIAN_POINT('Ctrl Pts',(56.5608110809614,22.8891318163506,25.1542911594985));
#36254=CARTESIAN_POINT('Ctrl Pts',(56.4980848743157,22.9409565527464,25.1585073173376));
#36255=CARTESIAN_POINT('Ctrl Pts',(56.4327514998883,22.9896730241156,25.1627234751768));
#36256=CARTESIAN_POINT('Ctrl Pts',(56.3651559454247,23.0350183032768,25.1669396330159));
#36257=CARTESIAN_POINT('Ctrl Pts',(56.2975620014607,23.0803625020629,25.1711556904029));
#36258=CARTESIAN_POINT('Ctrl Pts',(56.2277063713352,23.1223354102548,25.1753717477898));
#36259=CARTESIAN_POINT('Ctrl Pts',(56.1559630681782,23.1607173889725,25.1795878051768));
#36260=CARTESIAN_POINT('Ctrl Pts',(56.0836324399257,23.1994135809802,25.183838377232));
#36261=CARTESIAN_POINT('Ctrl Pts',(56.009383504594,23.2344595375161,25.1880889492872));
#36262=CARTESIAN_POINT('Ctrl Pts',(55.9336231895077,23.2656782626872,25.1923395213425));
#36263=CARTESIAN_POINT('Ctrl Pts',(55.8583687944921,23.2966885122253,25.1965617084878));
#36264=CARTESIAN_POINT('Ctrl Pts',(55.7816236070862,23.3239223917217,25.2007838956332));
#36265=CARTESIAN_POINT('Ctrl Pts',(55.7038030989693,23.3472561530181,25.2050060827786));
#36266=CARTESIAN_POINT('Ctrl Pts',(55.6251978335577,23.3708252165482,25.2092708472887));
#36267=CARTESIAN_POINT('Ctrl Pts',(55.5454959096208,23.3904149440204,25.2135356117989));
#36268=CARTESIAN_POINT('Ctrl Pts',(55.4651355960718,23.4059507740739,25.217800376309));
#36269=CARTESIAN_POINT('Ctrl Pts',(55.3847752825228,23.4214866041274,25.2220651408191));
#36270=CARTESIAN_POINT('Ctrl Pts',(55.3037570654115,23.432968532771,25.2263299053293));
#36271=CARTESIAN_POINT('Ctrl Pts',(55.222522108151,23.4403758237993,25.2305946698394));
#36272=CARTESIAN_POINT('Ctrl Pts',(55.1419260837726,23.4477248546651,25.2348258909297));
#36273=CARTESIAN_POINT('Ctrl Pts',(55.0608144934773,23.451090718721,25.23905711202));
#36274=CARTESIAN_POINT('Ctrl Pts',(54.9796146923591,23.4504152075174,25.2432883331102));
#36275=CARTESIAN_POINT('Ctrl Pts',(54.8985313263053,23.4497406649515,25.2475134869135));
#36276=CARTESIAN_POINT('Ctrl Pts',(54.8173604616272,23.4450362603868,25.2517386407167));
#36277=CARTESIAN_POINT('Ctrl Pts',(54.7365343158626,23.4362955656656,25.2559637945199));
#36278=CARTESIAN_POINT('Ctrl Pts',(54.6555005495152,23.4275324184557,25.2601998016045));
#36279=CARTESIAN_POINT('Ctrl Pts',(54.574813745973,23.4147121818007,25.264435808689));
#36280=CARTESIAN_POINT('Ctrl Pts',(54.4949092113116,23.3978810531763,25.2686718157735));
#36281=CARTESIAN_POINT('Ctrl Pts',(54.4153527843546,23.381123250122,25.2728893685024));
#36282=CARTESIAN_POINT('Ctrl Pts',(54.3365722840239,23.3603895179163,25.2771069212312));
#36283=CARTESIAN_POINT('Ctrl Pts',(54.2589901389481,23.3357770946355,25.2813244739601));
#36284=CARTESIAN_POINT('Ctrl Pts',(54.1814336100137,23.3111727979064,25.2855406341336));
#36285=CARTESIAN_POINT('Ctrl Pts',(54.105075093389,23.2826924938103,25.2897567943072));
#36286=CARTESIAN_POINT('Ctrl Pts',(54.0303225700522,23.2504834884642,25.2939729544807));
#36287=CARTESIAN_POINT('Ctrl Pts',(53.9555718282075,23.2182752507187,25.2981890141753));
#36288=CARTESIAN_POINT('Ctrl Pts',(53.8824274300873,23.1823386733941,25.3024050738699));
#36289=CARTESIAN_POINT('Ctrl Pts',(53.8112767225188,23.1428689226302,25.3066211335645));
#36290=CARTESIAN_POINT('Ctrl Pts',(53.7395436277525,23.103076101607,25.3108717028131));
#36291=CARTESIAN_POINT('Ctrl Pts',(53.6698374392182,23.0596922189523,25.3151222720618));
#36292=CARTESIAN_POINT('Ctrl Pts',(53.6025275191101,23.0129632175366,25.3193728413105));
#36293=CARTESIAN_POINT('Ctrl Pts',(53.5356670088646,22.9665462128381,25.3235950306749));
#36294=CARTESIAN_POINT('Ctrl Pts',(53.4711712001428,22.9168289578344,25.3278172200393));
#36295=CARTESIAN_POINT('Ctrl Pts',(53.4093693488068,22.8640934476267,25.3320394094037));
#36296=CARTESIAN_POINT('Ctrl Pts',(53.3469443861286,22.8108262366068,25.3363041685945));
#36297=CARTESIAN_POINT('Ctrl Pts',(53.2872683629448,22.7544798988007,25.3405689277853));
#36298=CARTESIAN_POINT('Ctrl Pts',(53.2306415662832,22.6953822527781,25.3448336869761));
#36299=CARTESIAN_POINT('Ctrl Pts',(53.1740147696215,22.6362846067556,25.3490984461669));
#36300=CARTESIAN_POINT('Ctrl Pts',(53.1204374663805,22.574436058744,25.3533632053577));
#36301=CARTESIAN_POINT('Ctrl Pts',(53.0701662876029,22.5101960443915,25.3576279645485));
#36302=CARTESIAN_POINT('Ctrl Pts',(53.0203123989143,22.4464892723848,25.3618573229035));
#36303=CARTESIAN_POINT('Ctrl Pts',(52.9735195039211,22.3801872905676,25.3660866812586));
#36304=CARTESIAN_POINT('Ctrl Pts',(52.930069306222,22.3116162445455,25.3703160396137));
#36305=CARTESIAN_POINT('Ctrl Pts',(52.8866800828081,22.2431414252551,25.3745394628495));
#36306=CARTESIAN_POINT('Ctrl Pts',(52.8466244911782,22.1724042513461,25.3787628860854));
#36307=CARTESIAN_POINT('Ctrl Pts',(52.8101436289925,22.0997633037877,25.3829863093213));
#36308=CARTESIAN_POINT('Ctrl Pts',(52.7737027894316,22.0272020495592,25.3872050991007));
#36309=CARTESIAN_POINT('Ctrl Pts',(52.7408290987219,21.9527415820618,25.3914238888802));
#36310=CARTESIAN_POINT('Ctrl Pts',(52.7117192342973,21.8767675788458,25.3956426786597));
#36311=CARTESIAN_POINT('Ctrl Pts',(52.6826311694021,21.8008504703471,25.3998583091105));
#36312=CARTESIAN_POINT('Ctrl Pts',(52.6573014986653,21.7234225098316,25.4040739395612));
#36313=CARTESIAN_POINT('Ctrl Pts',(52.6358794043523,21.6448907343375,25.408289570012));
#36314=CARTESIAN_POINT('Ctrl Pts',(52.6144670306404,21.5663945938309,25.4125032875563));
#36315=CARTESIAN_POINT('Ctrl Pts',(52.5969588308594,21.4867960817994,25.4167170051006));
#36316=CARTESIAN_POINT('Ctrl Pts',(52.5834541557757,21.4065174445975,25.4209307226449));
#36317=CARTESIAN_POINT('Ctrl Pts',(52.5699475313697,21.3262272196357,25.4251450484152));
#36318=CARTESIAN_POINT('Ctrl Pts',(52.5604456702665,21.2452571306903,25.4293593741854));
#36319=CARTESIAN_POINT('Ctrl Pts',(52.554996609532,21.1640386253292,25.4335736999556));
#36320=CARTESIAN_POINT('Ctrl Pts',(52.5512905675788,21.1087998965082,25.4364399678998));
#36321=CARTESIAN_POINT('Ctrl Pts',(52.5494581561907,21.053446442291,25.4393062358439));
#36322=CARTESIAN_POINT('Ctrl Pts',(52.5495007252096,20.9981147276813,25.442172503788));
#36323=CARTESIAN_POINT('',(52.5491673979362,20.9994536141197,26.2421724504355));
#36324=CARTESIAN_POINT('Ctrl Pts',(52.5517830077512,20.9980990070289,25.4421734099415));
#36325=CARTESIAN_POINT('Ctrl Pts',(52.5498278305076,20.7249505487043,25.4563360263802));
#36326=CARTESIAN_POINT('Ctrl Pts',(52.7180374006172,19.6374647203878,25.5128430743885));
#36327=CARTESIAN_POINT('Ctrl Pts',(54.3132510197648,18.1860561181197,25.6116945539665));
#36328=CARTESIAN_POINT('Ctrl Pts',(56.9920019014522,18.8971880273581,25.7387278486753));
#36329=CARTESIAN_POINT('Ctrl Pts',(57.8469697728126,21.5335586496174,25.8657611433844));
#36330=CARTESIAN_POINT('Ctrl Pts',(56.0953629013814,23.681434275856,25.9927944380933));
#36331=CARTESIAN_POINT('Ctrl Pts',(53.3748075180771,23.3780693189303,26.1182646831502));
#36332=CARTESIAN_POINT('Ctrl Pts',(52.5479892655699,21.7809080491335,26.2013904966373));
#36333=CARTESIAN_POINT('Ctrl Pts',(52.5456016115373,20.9994637759287,26.2421718785549));
#36334=CARTESIAN_POINT('',(52.682543123578,21.7964570772642,26.9999757050611));
#36335=CARTESIAN_POINT('Ctrl Pts',(52.5495000611252,20.9994526660932,26.242172503788));
#36336=CARTESIAN_POINT('Ctrl Pts',(52.5495067393017,20.9695534198073,26.2437353450291));
#36337=CARTESIAN_POINT('Ctrl Pts',(52.5500606104301,20.9396609804658,26.2452981862702));
#36338=CARTESIAN_POINT('Ctrl Pts',(52.5511610538356,20.9097887714958,26.2468610275113));
#36339=CARTESIAN_POINT('Ctrl Pts',(52.5541398745223,20.8289268629256,26.2510915256869));
#36340=CARTESIAN_POINT('Ctrl Pts',(52.5611337487646,20.7480607455217,26.2553220238625));
#36341=CARTESIAN_POINT('Ctrl Pts',(52.5721460426103,20.6676215837523,26.259552522038));
#36342=CARTESIAN_POINT('Ctrl Pts',(52.5831425394922,20.587297810706,26.26377695163));
#36343=CARTESIAN_POINT('Ctrl Pts',(52.598145945089,20.5074002338127,26.2680013812219));
#36344=CARTESIAN_POINT('Ctrl Pts',(52.6171076473889,20.4283582539146,26.2722258108139));
#36345=CARTESIAN_POINT('Ctrl Pts',(52.6361221281665,20.3490962665874,26.2764619987891));
#36346=CARTESIAN_POINT('Ctrl Pts',(52.6591169495656,20.2706951180793,26.2806981867644));
#36347=CARTESIAN_POINT('Ctrl Pts',(52.6859908382534,20.1935808476031,26.2849343747396));
#36348=CARTESIAN_POINT('Ctrl Pts',(52.712741926051,20.1168189526675,26.2891512053505));
#36349=CARTESIAN_POINT('Ctrl Pts',(52.7433365599026,20.0413326450863,26.2933680359615));
#36350=CARTESIAN_POINT('Ctrl Pts',(52.7776245398402,19.9675284197231,26.2975848665724));
#36351=CARTESIAN_POINT('Ctrl Pts',(52.8119012158823,19.8937485257802,26.301800306999));
#36352=CARTESIAN_POINT('Ctrl Pts',(52.8498686242415,19.8216500342973,26.3060157474256));
#36353=CARTESIAN_POINT('Ctrl Pts',(52.8913287446482,19.7516187333778,26.3102311878523));
#36354=CARTESIAN_POINT('Ctrl Pts',(52.9327879095229,19.6815890464709,26.3144465311256));
#36355=CARTESIAN_POINT('Ctrl Pts',(52.9777393885013,19.6136268550547,26.3186618743989));
#36356=CARTESIAN_POINT('Ctrl Pts',(53.0259403201985,19.5480913835292,26.3228772176722));
#36357=CARTESIAN_POINT('Ctrl Pts',(53.0745538377756,19.4819949475321,26.3271286430512));
#36358=CARTESIAN_POINT('Ctrl Pts',(53.1264724334857,19.418367372663,26.3313800684302));
#36359=CARTESIAN_POINT('Ctrl Pts',(53.1814048467678,19.3575439370746,26.3356314938092));
#36360=CARTESIAN_POINT('Ctrl Pts',(53.2359504452579,19.2971487987915,26.3398529821415));
#36361=CARTESIAN_POINT('Ctrl Pts',(53.2934671764026,19.239518722849,26.3440744704738));
#36362=CARTESIAN_POINT('Ctrl Pts',(53.3536334496469,19.184944234499,26.3482959588061));
#36363=CARTESIAN_POINT('Ctrl Pts',(53.4144397343252,19.1297892166487,26.3525623527085));
#36364=CARTESIAN_POINT('Ctrl Pts',(53.4779518868354,19.0777554876658,26.3568287466109));
#36365=CARTESIAN_POINT('Ctrl Pts',(53.543805961697,19.0290994005757,26.3610951405133));
#36366=CARTESIAN_POINT('Ctrl Pts',(53.6096600365586,18.9804433134857,26.3653615344157));
#36367=CARTESIAN_POINT('Ctrl Pts',(53.677855595404,18.93516508174,26.3696279283181));
#36368=CARTESIAN_POINT('Ctrl Pts',(53.7480028554,18.8934736175605,26.3738943222205));
#36369=CARTESIAN_POINT('Ctrl Pts',(53.8175864726838,18.8521171499291,26.3781264350714));
#36370=CARTESIAN_POINT('Ctrl Pts',(53.889351692782,18.8141347455355,26.3823585479223));
#36371=CARTESIAN_POINT('Ctrl Pts',(53.9629377574519,18.7797630407812,26.3865906607732));
#36372=CARTESIAN_POINT('Ctrl Pts',(54.0364182646889,18.7454406414074,26.3908167027604));
#36373=CARTESIAN_POINT('Ctrl Pts',(54.1117140113946,18.7147188497728,26.3950427447476));
#36374=CARTESIAN_POINT('Ctrl Pts',(54.1884375540172,18.6877896621911,26.3992687867348));
#36375=CARTESIAN_POINT('Ctrl Pts',(54.2653379730445,18.66079839278,26.4035045713262));
#36376=CARTESIAN_POINT('Ctrl Pts',(54.3436723692843,18.6376174674684,26.4077403559176));
#36377=CARTESIAN_POINT('Ctrl Pts',(54.4230281736965,18.6183926096747,26.4119761405091));
#36378=CARTESIAN_POINT('Ctrl Pts',(54.5020587700292,18.5992465372846,26.4161945664286));
#36379=CARTESIAN_POINT('Ctrl Pts',(54.5821019674695,18.5840242911116,26.4204129923482));
#36380=CARTESIAN_POINT('Ctrl Pts',(54.6627345151479,18.5728201049927,26.4246314182677));
#36381=CARTESIAN_POINT('Ctrl Pts',(54.7433403011021,18.5616196375129,26.4288484441031));
#36382=CARTESIAN_POINT('Ctrl Pts',(54.82453458892,18.5544346456498,26.4330654699385));
#36383=CARTESIAN_POINT('Ctrl Pts',(54.9058855980812,18.5513079553869,26.4372824957739));
#36384=CARTESIAN_POINT('Ctrl Pts',(54.9872345019779,18.5481813460389,26.4414994124778));
#36385=CARTESIAN_POINT('Ctrl Pts',(55.068739654742,18.5491128462283,26.4457163291817));
#36386=CARTESIAN_POINT('Ctrl Pts',(55.1499672776044,18.5540932017659,26.4499332458857));
#36387=CARTESIAN_POINT('Ctrl Pts',(55.2318231261238,18.5591120760612,26.454182776806));
#36388=CARTESIAN_POINT('Ctrl Pts',(55.3133966543977,18.568242694247,26.4584323077262));
#36389=CARTESIAN_POINT('Ctrl Pts',(55.3942490159461,18.5814223263609,26.4626818386465));
#36390=CARTESIAN_POINT('Ctrl Pts',(55.4745969115593,18.5945197261774,26.4669048552691));
#36391=CARTESIAN_POINT('Ctrl Pts',(55.5542321679018,18.611615600415,26.4711278718916));
#36392=CARTESIAN_POINT('Ctrl Pts',(55.6327360089674,18.6325973318939,26.4753508885141));
#36393=CARTESIAN_POINT('Ctrl Pts',(55.7119791820332,18.6537766647294,26.4796136765833));
#36394=CARTESIAN_POINT('Ctrl Pts',(55.7900690561176,18.6789152840031,26.4838764646525));
#36395=CARTESIAN_POINT('Ctrl Pts',(55.8665940424694,18.7078470784966,26.4881392527216));
#36396=CARTESIAN_POINT('Ctrl Pts',(55.9431190288212,18.7367788729901,26.4924020407908));
#36397=CARTESIAN_POINT('Ctrl Pts',(56.0180787129721,18.7695035922549,26.49666482886));
#36398=CARTESIAN_POINT('Ctrl Pts',(56.0910871936131,18.8058078967571,26.5009276169292));
#36399=CARTESIAN_POINT('Ctrl Pts',(56.1635699506814,18.8418507791821,26.5051597092743));
#36400=CARTESIAN_POINT('Ctrl Pts',(56.2344001739273,18.8815564034035,26.5093918016195));
#36401=CARTESIAN_POINT('Ctrl Pts',(56.3031834376743,18.9247498517597,26.5136238939646));
#36402=CARTESIAN_POINT('Ctrl Pts',(56.3718682972822,18.9678815058091,26.5178499317061));
#36403=CARTESIAN_POINT('Ctrl Pts',(56.4385116233919,19.0144908286332,26.5220759694475));
#36404=CARTESIAN_POINT('Ctrl Pts',(56.5027420427641,19.0643562820319,26.526302007189));
#36405=CARTESIAN_POINT('Ctrl Pts',(56.5671206489311,19.1143367806349,26.5305377948744));
#36406=CARTESIAN_POINT('Ctrl Pts',(56.6290747840083,19.1675882338332,26.5347735825597));
#36407=CARTESIAN_POINT('Ctrl Pts',(56.6882583461772,19.2238429105051,26.5390093702451));
#36408=CARTESIAN_POINT('Ctrl Pts',(56.7471998111796,19.2798674709534,26.5432278309539));
#36409=CARTESIAN_POINT('Ctrl Pts',(56.8033929800567,19.3388704181465,26.5474462916627));
#36410=CARTESIAN_POINT('Ctrl Pts',(56.8565292291881,19.4005471338079,26.5516647523715));
#36411=CARTESIAN_POINT('Ctrl Pts',(56.9096480251894,19.4622035911379,26.5558818274849));
#36412=CARTESIAN_POINT('Ctrl Pts',(56.95971159236,19.5265317210938,26.5600989025982));
#36413=CARTESIAN_POINT('Ctrl Pts',(57.0064498866016,19.5931918742925,26.5643159777116));
#36414=CARTESIAN_POINT('Ctrl Pts',(57.0531871300737,19.659850528839,26.5685329580168));
#36415=CARTESIAN_POINT('Ctrl Pts',(57.0965989834007,19.7288407212579,26.572749938322));
#36416=CARTESIAN_POINT('Ctrl Pts',(57.1364580866657,19.7997928954048,26.5769669186271));
#36417=CARTESIAN_POINT('Ctrl Pts',(57.1766245621654,19.8712922150352,26.5812164180447));
#36418=CARTESIAN_POINT('Ctrl Pts',(57.2131830074292,19.9447834979307,26.5854659174623));
#36419=CARTESIAN_POINT('Ctrl Pts',(57.2459482686662,20.0198639765444,26.5897154168799));
#36420=CARTESIAN_POINT('Ctrl Pts',(57.2785100903249,20.0944782803032,26.5939385311464));
#36421=CARTESIAN_POINT('Ctrl Pts',(57.3073255883373,20.1706616411086,26.5981616454129));
#36422=CARTESIAN_POINT('Ctrl Pts',(57.3322623959351,20.2480010860999,26.6023847596794));
#36423=CARTESIAN_POINT('Ctrl Pts',(57.3574329036161,20.3260653325581,26.6066474516726));
#36424=CARTESIAN_POINT('Ctrl Pts',(57.3786515154079,20.4053069781661,26.6109101436657));
#36425=CARTESIAN_POINT('Ctrl Pts',(57.3958347250919,20.4852901593674,26.6151728356589));
#36426=CARTESIAN_POINT('Ctrl Pts',(57.4130179347758,20.5652733405687,26.619435527652));
#36427=CARTESIAN_POINT('Ctrl Pts',(57.4261657282633,20.6459975734496,26.6236982196452));
#36428=CARTESIAN_POINT('Ctrl Pts',(57.4352482010145,20.727022987313,26.6279609116383));
#36429=CARTESIAN_POINT('Ctrl Pts',(57.4442524333069,20.8073504122328,26.6321868829072));
#36430=CARTESIAN_POINT('Ctrl Pts',(57.4492950829039,20.8882766980863,26.6364128541761));
#36431=CARTESIAN_POINT('Ctrl Pts',(57.4503086474803,20.9693767721592,26.640638825445));
#36432=CARTESIAN_POINT('Ctrl Pts',(57.4513207538296,21.0503601666194,26.6448587167602));
#36433=CARTESIAN_POINT('Ctrl Pts',(57.4483152812012,21.1315163906118,26.6490786080755));
#36434=CARTESIAN_POINT('Ctrl Pts',(57.4412763855329,21.2124143578939,26.6532984993907));
#36435=CARTESIAN_POINT('Ctrl Pts',(57.4342084164619,21.2936464655432,26.6575358205139));
#36436=CARTESIAN_POINT('Ctrl Pts',(57.4230735756371,21.3746177053289,26.6617731416371));
#36437=CARTESIAN_POINT('Ctrl Pts',(57.4079087777954,21.4548907207405,26.6660104627603));
#36438=CARTESIAN_POINT('Ctrl Pts',(57.3928335373729,21.5346896748314,26.670222759907));
#36439=CARTESIAN_POINT('Ctrl Pts',(57.3737758937374,21.6137981655812,26.6744350570538));
#36440=CARTESIAN_POINT('Ctrl Pts',(57.3508239366155,21.6917926488737,26.6786473542005));
#36441=CARTESIAN_POINT('Ctrl Pts',(57.3278794911986,21.7697616061708,26.6828582727487));
#36442=CARTESIAN_POINT('Ctrl Pts',(57.3010433946186,21.8466168330897,26.687069191297));
#36443=CARTESIAN_POINT('Ctrl Pts',(57.2704540986355,21.9219481742427,26.6912801098452));
#36444=CARTESIAN_POINT('Ctrl Pts',(57.2398653813777,21.997278090186,26.6954909487262));
#36445=CARTESIAN_POINT('Ctrl Pts',(57.2055237823416,22.0710837461625,26.6997017876071));
#36446=CARTESIAN_POINT('Ctrl Pts',(57.1676160316486,22.1429746232266,26.7039126264881));
#36447=CARTESIAN_POINT('Ctrl Pts',(57.1292945346533,22.21565015736,26.7081694248097));
#36448=CARTESIAN_POINT('Ctrl Pts',(57.0873287762015,22.286368421148,26.7124262231313));
#36449=CARTESIAN_POINT('Ctrl Pts',(57.0419586006651,22.3547528642412,26.7166830214529));
#36450=CARTESIAN_POINT('Ctrl Pts',(56.997011838929,22.4224991145881,26.7209000935197));
#36451=CARTESIAN_POINT('Ctrl Pts',(56.9487242697108,22.4879545818773,26.7251171655865));
#36452=CARTESIAN_POINT('Ctrl Pts',(56.897370724117,22.5507851512262,26.7293342376532));
#36453=CARTESIAN_POINT('Ctrl Pts',(56.8452915266946,22.6145035486114,26.7336108991022));
#36454=CARTESIAN_POINT('Ctrl Pts',(56.7900593633578,22.6755219190545,26.7378875605512));
#36455=CARTESIAN_POINT('Ctrl Pts',(56.7319993586573,22.7335306376325,26.7421642220002));
#36456=CARTESIAN_POINT('Ctrl Pts',(56.6739393539568,22.7915393562106,26.7464408834492));
#36457=CARTESIAN_POINT('Ctrl Pts',(56.6130519184716,22.8465381425506,26.7507175448982));
#36458=CARTESIAN_POINT('Ctrl Pts',(56.5496951052037,22.8982611334871,26.7549942063472));
#36459=CARTESIAN_POINT('Ctrl Pts',(56.4868952408543,22.9495294446129,26.7592332730713));
#36460=CARTESIAN_POINT('Ctrl Pts',(56.4214326579385,22.9977725913542,26.7634723397953));
#36461=CARTESIAN_POINT('Ctrl Pts',(56.3536303884841,23.0427028715338,26.7677114065194));
#36462=CARTESIAN_POINT('Ctrl Pts',(56.2859254991731,23.0875686211724,26.771944384938));
#36463=CARTESIAN_POINT('Ctrl Pts',(56.2158879807024,23.1291307013787,26.7761773633566));
#36464=CARTESIAN_POINT('Ctrl Pts',(56.1438738006428,23.1671416608526,26.7804103417752));
#36465=CARTESIAN_POINT('Ctrl Pts',(56.0718414190082,23.2051622275918,26.7846443900786));
#36466=CARTESIAN_POINT('Ctrl Pts',(55.9978317530468,23.2396296051631,26.788878438382));
#36467=CARTESIAN_POINT('Ctrl Pts',(55.9222300314476,23.2703396263767,26.7931124866853));
#36468=CARTESIAN_POINT('Ctrl Pts',(55.846785064203,23.3009859727233,26.7973377560152));
#36469=CARTESIAN_POINT('Ctrl Pts',(55.7697550562113,23.327890330548,26.8015630253451));
#36470=CARTESIAN_POINT('Ctrl Pts',(55.6915457231059,23.3508965870182,26.805788294675));
#36471=CARTESIAN_POINT('Ctrl Pts',(55.6133632373863,23.3738949459932,26.8100121135714));
#36472=CARTESIAN_POINT('Ctrl Pts',(55.5340026744714,23.3929977306962,26.8142359324678));
#36473=CARTESIAN_POINT('Ctrl Pts',(55.453885790929,23.408098407207,26.8184597513642));
#36474=CARTESIAN_POINT('Ctrl Pts',(55.3737721059884,23.4231984808355,26.8226834016281));
#36475=CARTESIAN_POINT('Ctrl Pts',(55.2929026156913,23.4342966792029,26.8269070518919));
#36476=CARTESIAN_POINT('Ctrl Pts',(55.2117087794886,23.4413376748593,26.8311307021558));
#36477=CARTESIAN_POINT('Ctrl Pts',(55.1301737309127,23.4484082598903,26.8353721020641));
#36478=CARTESIAN_POINT('Ctrl Pts',(55.0483120716804,23.4513874126894,26.8396135019725));
#36479=CARTESIAN_POINT('Ctrl Pts',(54.9665636225421,23.4502718744381,26.8438549018809));
#36480=CARTESIAN_POINT('Ctrl Pts',(54.8850438303021,23.4491594564358,26.8480844382572));
#36481=CARTESIAN_POINT('Ctrl Pts',(54.803637078279,23.4439752929518,26.8523139746335));
#36482=CARTESIAN_POINT('Ctrl Pts',(54.7227753986737,23.4347683196599,26.8565435110098));
#36483=CARTESIAN_POINT('Ctrl Pts',(54.6415735026559,23.4255226090645,26.8607908426842));
#36484=CARTESIAN_POINT('Ctrl Pts',(54.560921738975,23.4122202445618,26.8650381743587));
#36485=CARTESIAN_POINT('Ctrl Pts',(54.4812464891015,23.3949624307973,26.8692855060331));
#36486=CARTESIAN_POINT('Ctrl Pts',(54.401571239228,23.3777046170328,26.8735328377075));
#36487=CARTESIAN_POINT('Ctrl Pts',(54.3228729380817,23.3564915329934,26.8777801693819));
#36488=CARTESIAN_POINT('Ctrl Pts',(54.2455601136359,23.3314739346308,26.8820275010563));
#36489=CARTESIAN_POINT('Ctrl Pts',(54.169285408542,23.3067922605238,26.8862178016076));
#36490=CARTESIAN_POINT('Ctrl Pts',(54.0940686995614,23.2783134695851,26.890408102159));
#36491=CARTESIAN_POINT('Ctrl Pts',(54.0203200073828,23.2461472262667,26.8945984027103));
#36492=CARTESIAN_POINT('Ctrl Pts',(53.9430439450967,23.2124424845451,26.8989891236416));
#36493=CARTESIAN_POINT('Ctrl Pts',(53.867380360135,23.1746887917181,26.9033798445729));
#36494=CARTESIAN_POINT('Ctrl Pts',(53.7937845128205,23.1330715994753,26.9077705655042));
#36495=CARTESIAN_POINT('Ctrl Pts',(53.7237284891418,23.0934561169232,26.9119501009094));
#36496=CARTESIAN_POINT('Ctrl Pts',(53.655546373461,23.0503404512337,26.9161296363146));
#36497=CARTESIAN_POINT('Ctrl Pts',(53.5896096017808,23.0039334256934,26.9203091717198));
#36498=CARTESIAN_POINT('Ctrl Pts',(53.5237109517532,22.9575532305916,26.9244862907071));
#36499=CARTESIAN_POINT('Ctrl Pts',(53.4600554572414,22.9078857240475,26.9286634096944));
#36500=CARTESIAN_POINT('Ctrl Pts',(53.3989867597946,22.8551837792216,26.9328405286817));
#36501=CARTESIAN_POINT('Ctrl Pts',(53.3379337749728,22.8024953943033,26.9370165729203));
#36502=CARTESIAN_POINT('Ctrl Pts',(53.2794666247867,22.7467744315117,26.9411926171589));
#36503=CARTESIAN_POINT('Ctrl Pts',(53.2238957157063,22.688313898928,26.9453686613975));
#36504=CARTESIAN_POINT('Ctrl Pts',(53.1683212744554,22.629849650505,26.9495449710717));
#36505=CARTESIAN_POINT('Ctrl Pts',(53.1156437649222,22.5686458324901,26.9537212807459));
#36506=CARTESIAN_POINT('Ctrl Pts',(53.0661354820089,22.5050309884036,26.9578975904202));
#36507=CARTESIAN_POINT('Ctrl Pts',(53.0165789796522,22.4413541855458,26.962077967683));
#36508=CARTESIAN_POINT('Ctrl Pts',(52.9701981548031,22.3752620463761,26.9662583449458));
#36509=CARTESIAN_POINT('Ctrl Pts',(52.9272233588278,22.3071140905869,26.9704387222087));
#36510=CARTESIAN_POINT('Ctrl Pts',(52.8842240998105,22.2389273421457,26.9746214791162));
#36511=CARTESIAN_POINT('Ctrl Pts',(52.8446349593748,22.1686828624283,26.9788042360237));
#36512=CARTESIAN_POINT('Ctrl Pts',(52.8086402700108,22.0967646893393,26.9829869929312));
#36513=CARTESIAN_POINT('Ctrl Pts',(52.7725900071155,22.0247354791248,26.9871762077517));
#36514=CARTESIAN_POINT('Ctrl Pts',(52.7401454567778,21.9510278541624,26.9913654225722));
#36515=CARTESIAN_POINT('Ctrl Pts',(52.7114425093182,21.8760450113118,26.9955546373927));
#36516=CARTESIAN_POINT('Ctrl Pts',(52.7013453369014,21.8496674173858,26.9970283266155));
#36517=CARTESIAN_POINT('Ctrl Pts',(52.6917107340805,21.8231321393686,26.9985020158383));
#36518=CARTESIAN_POINT('Ctrl Pts',(52.682543123578,21.7964570772642,26.9999757050611));
#36519=CARTESIAN_POINT('',(54.2031000556071,23.3173046257725,27.));
#36520=CARTESIAN_POINT('Origin',(55.,21.,27.));
#36521=CARTESIAN_POINT('',(52.5485180219995,20.9992126141703,26.3578274962121));
#36522=CARTESIAN_POINT('Ctrl Pts',(54.203100055607,23.3173046257725,27.));
#36523=CARTESIAN_POINT('Ctrl Pts',(54.9737715883742,23.5823315431561,26.9576555684304));
#36524=CARTESIAN_POINT('Ctrl Pts',(56.7871288453655,23.2781442292576,26.872966705291));
#36525=CARTESIAN_POINT('Ctrl Pts',(57.8856565523512,20.7291287202087,26.745933410582));
#36526=CARTESIAN_POINT('Ctrl Pts',(56.3358056379254,18.430681285051,26.618900115873));
#36527=CARTESIAN_POINT('Ctrl Pts',(53.5661178804319,18.4833632214424,26.4918668211641));
#36528=CARTESIAN_POINT('Ctrl Pts',(52.5669730182605,20.0983171962907,26.4048426146105));
#36529=CARTESIAN_POINT('Ctrl Pts',(52.5455281581047,20.9544531196991,26.3601628396264));
#36530=CARTESIAN_POINT('Ctrl Pts',(52.5457196275622,20.9992117153605,26.3578274962121));
#36531=CARTESIAN_POINT('',(52.5495006168754,20.9982612343869,25.557827496241));
#36532=CARTESIAN_POINT('Ctrl Pts',(52.5495001263987,20.9992129296102,26.3578274962121));
#36533=CARTESIAN_POINT('Ctrl Pts',(52.5494743355874,21.0795111858266,26.3536313506362));
#36534=CARTESIAN_POINT('Ctrl Pts',(52.5533996345101,21.1599691050755,26.3494352050602));
#36535=CARTESIAN_POINT('Ctrl Pts',(52.5612969373346,21.2401616583602,26.3452390594843));
#36536=CARTESIAN_POINT('Ctrl Pts',(52.5691832420487,21.3202425321801,26.3410487576341));
#36537=CARTESIAN_POINT('Ctrl Pts',(52.581030522992,21.4000583066965,26.3368584557839));
#36538=CARTESIAN_POINT('Ctrl Pts',(52.596807678344,21.4791835923042,26.3326681539338));
#36539=CARTESIAN_POINT('Ctrl Pts',(52.6125678008879,21.5582234553005,26.328482375878));
#36540=CARTESIAN_POINT('Ctrl Pts',(52.6322492777825,21.6365738483382,26.3242965978223));
#36541=CARTESIAN_POINT('Ctrl Pts',(52.6557693381687,21.7138157003947,26.3201108197666));
#36542=CARTESIAN_POINT('Ctrl Pts',(52.679275888901,21.7910131856141,26.3159274459739));
#36543=CARTESIAN_POINT('Ctrl Pts',(52.7066165106108,21.8671029415645,26.3117440721813));
#36544=CARTESIAN_POINT('Ctrl Pts',(52.7376579070066,21.9416785567647,26.3075606983886));
#36545=CARTESIAN_POINT('Ctrl Pts',(52.768691371173,22.0162351151259,26.3033783936033));
#36546=CARTESIAN_POINT('Ctrl Pts',(52.8034235504787,22.0892778642556,26.299196088818));
#36547=CARTESIAN_POINT('Ctrl Pts',(52.8416726362047,22.1604194244723,26.2950137840327));
#36548=CARTESIAN_POINT('Ctrl Pts',(52.8799241435921,22.2315654888688,26.2908312144534));
#36549=CARTESIAN_POINT('Ctrl Pts',(52.9216927733975,22.3008097095626,26.2866486448742));
#36550=CARTESIAN_POINT('Ctrl Pts',(52.9667510390727,22.3677897911916,26.282466075295));
#36551=CARTESIAN_POINT('Ctrl Pts',(53.0118554409332,22.434838455253,26.2782792230874));
#36552=CARTESIAN_POINT('Ctrl Pts',(53.0602559369734,22.499617959663,26.2740923708799));
#36553=CARTESIAN_POINT('Ctrl Pts',(53.1116824370535,22.5617960915138,26.2699055186723));
#36554=CARTESIAN_POINT('Ctrl Pts',(53.1631379050008,22.6240092474837,26.2657163080663));
#36555=CARTESIAN_POINT('Ctrl Pts',(53.2176224490737,22.6836177662396,26.2615270974603));
#36556=CARTESIAN_POINT('Ctrl Pts',(53.2748282562834,22.7403254594132,26.2573378868542));
#36557=CARTESIAN_POINT('Ctrl Pts',(53.3321296921619,22.7971279485783,26.2531416733117));
#36558=CARTESIAN_POINT('Ctrl Pts',(53.3921611187412,22.8510196177861,26.2489454597692));
#36559=CARTESIAN_POINT('Ctrl Pts',(53.4545811722834,22.9017441723163,26.2447492462267));
#36560=CARTESIAN_POINT('Ctrl Pts',(53.4890374625839,22.9297444683282,26.2424329080665));
#36561=CARTESIAN_POINT('Ctrl Pts',(53.5242210620795,22.9567804653042,26.2401165699063));
#36562=CARTESIAN_POINT('Ctrl Pts',(53.5600710532226,22.9828148875355,26.2378002317461));
#36563=CARTESIAN_POINT('Ctrl Pts',(53.6255700198798,23.0303805270042,26.2335682151936));
#36564=CARTESIAN_POINT('Ctrl Pts',(53.6935506530067,23.0747859913906,26.2293361986411));
#36565=CARTESIAN_POINT('Ctrl Pts',(53.7636753302762,23.1157626428861,26.2251041820886));
#36566=CARTESIAN_POINT('Ctrl Pts',(53.8336997560659,23.1566807134353,26.2208782157019));
#36567=CARTESIAN_POINT('Ctrl Pts',(53.9058617403943,23.1941794742577,26.2166522493152));
#36568=CARTESIAN_POINT('Ctrl Pts',(53.979793008219,23.2280323031593,26.2124262829285));
#36569=CARTESIAN_POINT('Ctrl Pts',(54.0538964167674,23.2619639546028,26.2081904768497));
#36570=CARTESIAN_POINT('Ctrl Pts',(54.1297769710899,23.2922324063916,26.2039546707709));
#36571=CARTESIAN_POINT('Ctrl Pts',(54.207037125881,23.3186548105031,26.1997188646921));
#36572=CARTESIAN_POINT('Ctrl Pts',(54.2839798177425,23.3449686446299,26.1955004635927));
#36573=CARTESIAN_POINT('Ctrl Pts',(54.3622903557061,23.367467815414,26.1912820624934));
#36574=CARTESIAN_POINT('Ctrl Pts',(54.4415558711848,23.3860197830261,26.187063661394));
#36575=CARTESIAN_POINT('Ctrl Pts',(54.5207954381148,23.4045656774217,26.1828466412406));
#36576=CARTESIAN_POINT('Ctrl Pts',(54.6009889095858,23.4191668289195,26.1786296210871));
#36577=CARTESIAN_POINT('Ctrl Pts',(54.6817102262335,23.4297411117063,26.1744126009336));
#36578=CARTESIAN_POINT('Ctrl Pts',(54.7624298199797,23.4403151687975,26.1701956707875));
#36579=CARTESIAN_POINT('Ctrl Pts',(54.8436767755754,23.4468624688256,26.1659787406413));
#36580=CARTESIAN_POINT('Ctrl Pts',(54.9250182856289,23.4493525659876,26.1617618104952));
#36581=CARTESIAN_POINT('Ctrl Pts',(55.0069894484636,23.451861938629,26.157512237707));
#36582=CARTESIAN_POINT('Ctrl Pts',(55.0890561580517,23.4502509915335,26.1532626649189));
#36583=CARTESIAN_POINT('Ctrl Pts',(55.1707756721488,23.4445420675051,26.1490130921307));
#36584=CARTESIAN_POINT('Ctrl Pts',(55.251985666481,23.4388687385198,26.1447900153558));
#36585=CARTESIAN_POINT('Ctrl Pts',(55.3328523239207,23.4291485044898,26.1405669385809));
#36586=CARTESIAN_POINT('Ctrl Pts',(55.4129483312974,23.4154552212117,26.1363438618059));
#36587=CARTESIAN_POINT('Ctrl Pts',(55.4937981344202,23.4016330683553,26.1320810410111));
#36588=CARTESIAN_POINT('Ctrl Pts',(55.5738622334867,23.3837627967394,26.1278182202163));
#36589=CARTESIAN_POINT('Ctrl Pts',(55.6527155994374,23.3619721836319,26.1235553994216));
#36590=CARTESIAN_POINT('Ctrl Pts',(55.7315689653882,23.3401815705244,26.1192925786268));
#36591=CARTESIAN_POINT('Ctrl Pts',(55.8092111626853,23.3144708275666,26.115029757832));
#36592=CARTESIAN_POINT('Ctrl Pts',(55.8852384319867,23.2850171046479,26.1107669370372));
#36593=CARTESIAN_POINT('Ctrl Pts',(55.9606899593003,23.2557864299216,26.1065363978821));
#36594=CARTESIAN_POINT('Ctrl Pts',(56.0348340446258,23.2227596316656,26.1023058587271));
#36595=CARTESIAN_POINT('Ctrl Pts',(56.10726206758,23.1860743271212,26.098075319572));
#36596=CARTESIAN_POINT('Ctrl Pts',(56.1795860444293,23.149441722663,26.0938508577763));
#36597=CARTESIAN_POINT('Ctrl Pts',(56.2501984435353,23.1091612582058,26.0896263959806));
#36598=CARTESIAN_POINT('Ctrl Pts',(56.3187092839997,23.0654191037881,26.0854019341848));
#36599=CARTESIAN_POINT('Ctrl Pts',(56.3874101471757,23.0215556254641,26.0811657553575));
#36600=CARTESIAN_POINT('Ctrl Pts',(56.4539973385911,22.9742114027611,26.0769295765301));
#36601=CARTESIAN_POINT('Ctrl Pts',(56.5181012589417,22.9236212770708,26.0726933977028));
#36602=CARTESIAN_POINT('Ctrl Pts',(56.5819125540839,22.8732620880533,26.0684765564246));
#36603=CARTESIAN_POINT('Ctrl Pts',(56.6432628283119,22.8196868501988,26.0642597151464));
#36604=CARTESIAN_POINT('Ctrl Pts',(56.7018169237209,22.7631702720206,26.0600428738682));
#36605=CARTESIAN_POINT('Ctrl Pts',(56.7603516026685,22.7066724346657,26.0558274308891));
#36606=CARTESIAN_POINT('Ctrl Pts',(56.8160916097042,22.6472355166042,26.05161198791));
#36607=CARTESIAN_POINT('Ctrl Pts',(56.8687369733639,22.5851726639021,26.0473965449308));
#36608=CARTESIAN_POINT('Ctrl Pts',(56.9213810224365,22.5231113609478,26.0431812072139));
#36609=CARTESIAN_POINT('Ctrl Pts',(56.9709302817531,22.4584246091144,26.038965869497));
#36610=CARTESIAN_POINT('Ctrl Pts',(57.017124529458,22.3914592637439,26.0347505317801));
#36611=CARTESIAN_POINT('Ctrl Pts',(57.0637140513964,22.3239209103288,26.0304991243257));
#36612=CARTESIAN_POINT('Ctrl Pts',(57.1068905822333,22.2540651667685,26.0262477168714));
#36613=CARTESIAN_POINT('Ctrl Pts',(57.1464323385103,22.1822768145392,26.0219963094171));
#36614=CARTESIAN_POINT('Ctrl Pts',(57.185695585155,22.1109940986164,26.0177748464579));
#36615=CARTESIAN_POINT('Ctrl Pts',(57.2213749463101,22.0378063609927,26.0135533834986));
#36616=CARTESIAN_POINT('Ctrl Pts',(57.2533008416306,21.9631124374166,26.0093319205394));
#36617=CARTESIAN_POINT('Ctrl Pts',(57.2855664313269,21.887623763827,26.0050655408375));
#36618=CARTESIAN_POINT('Ctrl Pts',(57.313998038042,21.8105971193485,26.0007991611357));
#36619=CARTESIAN_POINT('Ctrl Pts',(57.3384722095208,21.7324602209669,25.9965327814338));
#36620=CARTESIAN_POINT('Ctrl Pts',(57.3629463809996,21.6543233225853,25.9922664017319));
#36621=CARTESIAN_POINT('Ctrl Pts',(57.383463058575,21.5750766543416,25.98800002203));
#36622=CARTESIAN_POINT('Ctrl Pts',(57.3999520678217,21.4951568662136,25.9837336423281));
#36623=CARTESIAN_POINT('Ctrl Pts',(57.4163058464752,21.4158925207623,25.9795022523002));
#36624=CARTESIAN_POINT('Ctrl Pts',(57.4287591978242,21.335668594493,25.9752708622723));
#36625=CARTESIAN_POINT('Ctrl Pts',(57.4372063082182,21.25490323886,25.9710394722444));
#36626=CARTESIAN_POINT('Ctrl Pts',(57.4456413088147,21.174253668633,25.9668141483473));
#36627=CARTESIAN_POINT('Ctrl Pts',(57.4500814272728,21.0930646690861,25.9625888244503));
#36628=CARTESIAN_POINT('Ctrl Pts',(57.450471757429,21.0117650347583,25.9583635005532));
#36629=CARTESIAN_POINT('Ctrl Pts',(57.4508630705698,20.930260660188,25.9541275358476));
#36630=CARTESIAN_POINT('Ctrl Pts',(57.4471840837195,20.8486455564067,25.949891571142));
#36631=CARTESIAN_POINT('Ctrl Pts',(57.4394318362206,20.7673574277278,25.9456556064364));
#36632=CARTESIAN_POINT('Ctrl Pts',(57.4317129704213,20.6864193312027,25.94143788208));
#36633=CARTESIAN_POINT('Ctrl Pts',(57.4199558870623,20.6058058660911,25.9372201577235));
#36634=CARTESIAN_POINT('Ctrl Pts',(57.4042097873049,20.525947736397,25.9330024333671));
#36635=CARTESIAN_POINT('Ctrl Pts',(57.3884688856889,20.4461159696657,25.9287861013763));
#36636=CARTESIAN_POINT('Ctrl Pts',(57.3687416726496,20.367039498909,25.9245697693854));
#36637=CARTESIAN_POINT('Ctrl Pts',(57.3451287228792,20.2891402929362,25.9203534373945));
#36638=CARTESIAN_POINT('Ctrl Pts',(57.3215163360887,20.2112429442359,25.9161372059294));
#36639=CARTESIAN_POINT('Ctrl Pts',(57.2940185326838,20.1345232490794,25.9119209744644));
#36640=CARTESIAN_POINT('Ctrl Pts',(57.2627857615478,20.0593880463568,25.9077047429993));
#36641=CARTESIAN_POINT('Ctrl Pts',(57.2313001283659,19.9836445453505,25.9034543767176));
#36642=CARTESIAN_POINT('Ctrl Pts',(57.1960189436645,19.9095117590793,25.8992040104359));
#36643=CARTESIAN_POINT('Ctrl Pts',(57.1571450758474,19.8373842544729,25.8949536441542));
#36644=CARTESIAN_POINT('Ctrl Pts',(57.118527360474,19.7657320212406,25.8907312849058));
#36645=CARTESIAN_POINT('Ctrl Pts',(57.0763644619894,19.6960590920095,25.8865089256575));
#36646=CARTESIAN_POINT('Ctrl Pts',(57.0308996285668,19.6287243352676,25.8822865664091));
#36647=CARTESIAN_POINT('Ctrl Pts',(56.9849824407749,19.5607196283879,25.8780221966108));
#36648=CARTESIAN_POINT('Ctrl Pts',(56.935697539068,19.4951002681144,25.8737578268124));
#36649=CARTESIAN_POINT('Ctrl Pts',(56.8833368420662,19.4322013556212,25.8694934570141));
#36650=CARTESIAN_POINT('Ctrl Pts',(56.8309761450644,19.369302443128,25.8652290872158));
#36651=CARTESIAN_POINT('Ctrl Pts',(56.7755400261528,19.3091242890382,25.8609647174175));
#36652=CARTESIAN_POINT('Ctrl Pts',(56.7173567069577,19.2519621883187,25.8567003476191));
#36653=CARTESIAN_POINT('Ctrl Pts',(56.6596245349327,19.1952433163516,25.8524690432835));
#36654=CARTESIAN_POINT('Ctrl Pts',(56.5989712868893,19.1412812952135,25.8482377389478));
#36655=CARTESIAN_POINT('Ctrl Pts',(56.5356909213767,19.0903917564063,25.8440064346121));
#36656=CARTESIAN_POINT('Ctrl Pts',(56.4725012636275,19.039575164021,25.8397811955408));
#36657=CARTESIAN_POINT('Ctrl Pts',(56.4066923267724,18.9918225958151,25.8355559564696));
#36658=CARTESIAN_POINT('Ctrl Pts',(56.3385946155272,18.9474126802297,25.8313307173984));
#36659=CARTESIAN_POINT('Ctrl Pts',(56.2703236968907,18.9028898074615,25.827094731378));
#36660=CARTESIAN_POINT('Ctrl Pts',(56.1997526873778,18.8617269389932,25.8228587453577));
#36661=CARTESIAN_POINT('Ctrl Pts',(56.1272477717193,18.8241639052645,25.8186227593374));
#36662=CARTESIAN_POINT('Ctrl Pts',(56.0550568347439,18.7867635362566,25.8144051170293));
#36663=CARTESIAN_POINT('Ctrl Pts',(55.9809491178069,18.7529321114306,25.8101874747213));
#36664=CARTESIAN_POINT('Ctrl Pts',(55.9053131801079,18.7228618188782,25.8059698324132));
#36665=CARTESIAN_POINT('Ctrl Pts',(55.82970218982,18.6928014445732,25.801753581233));
#36666=CARTESIAN_POINT('Ctrl Pts',(55.7525644114385,18.6664999105888,25.7975373300528));
#36667=CARTESIAN_POINT('Ctrl Pts',(55.6743089198722,18.6441015024877,25.7933210788725));
#36668=CARTESIAN_POINT('Ctrl Pts',(55.5960552689602,18.6217036212215,25.7891049268631));
#36669=CARTESIAN_POINT('Ctrl Pts',(55.5166844043928,18.603208810164,25.7848887748537));
#36670=CARTESIAN_POINT('Ctrl Pts',(55.4366197304326,18.5887112447911,25.7806726228443));
#36671=CARTESIAN_POINT('Ctrl Pts',(55.3559034691396,18.5740956944257,25.7764221586831));
#36672=CARTESIAN_POINT('Ctrl Pts',(55.2744825229026,18.5635428507918,25.7721716945219));
#36673=CARTESIAN_POINT('Ctrl Pts',(55.1927984612472,18.5570961944152,25.7679212303608));
#36674=CARTESIAN_POINT('Ctrl Pts',(55.1116559575289,18.5506922787871,25.7636989463923));
#36675=CARTESIAN_POINT('Ctrl Pts',(55.0302542877551,18.5483402197066,25.7594766624239));
#36676=CARTESIAN_POINT('Ctrl Pts',(54.9490268651635,18.5500302064056,25.7552543784555));
#36677=CARTESIAN_POINT('Ctrl Pts',(54.8669862555232,18.5517371119635,25.750989824198));
#36678=CARTESIAN_POINT('Ctrl Pts',(54.7851238857998,18.5575674128837,25.7467252699404));
#36679=CARTESIAN_POINT('Ctrl Pts',(54.7038796664837,18.5674575033356,25.7424607156829));
#36680=CARTESIAN_POINT('Ctrl Pts',(54.6226354471676,18.5773475937875,25.7381961614254));
#36681=CARTESIAN_POINT('Ctrl Pts',(54.5420098418629,18.5912973283797,25.7339316071678));
#36682=CARTESIAN_POINT('Ctrl Pts',(54.4624289921549,18.6091910027097,25.7296670529103));
#36683=CARTESIAN_POINT('Ctrl Pts',(54.3834718846294,18.6269444292348,25.7254359235582));
#36684=CARTESIAN_POINT('Ctrl Pts',(54.3052470881391,18.6486467291004,25.7212047942062));
#36685=CARTESIAN_POINT('Ctrl Pts',(54.2281791718382,18.6742220958966,25.7169736648541));
#36686=CARTESIAN_POINT('Ctrl Pts',(54.1512217936304,18.6997607800834,25.7127486041879));
#36687=CARTESIAN_POINT('Ctrl Pts',(54.0754184376643,18.7291613531296,25.7085235435216));
#36688=CARTESIAN_POINT('Ctrl Pts',(54.0011824034266,18.7622972362766,25.7042984828554));
#36689=CARTESIAN_POINT('Ctrl Pts',(53.9267536301263,18.7955191501379,25.7000624526614));
#36690=CARTESIAN_POINT('Ctrl Pts',(53.8539007868142,18.8324956855936,25.6958264224675));
#36691=CARTESIAN_POINT('Ctrl Pts',(53.7830239881532,18.8730492162277,25.6915903922736));
#36692=CARTESIAN_POINT('Ctrl Pts',(53.7124579563411,18.9134249356011,25.6873729354038));
#36693=CARTESIAN_POINT('Ctrl Pts',(53.6438510873143,18.9573461231155,25.683155478534));
#36694=CARTESIAN_POINT('Ctrl Pts',(53.5775755357257,19.0045905449172,25.6789380216642));
#36695=CARTESIAN_POINT('Ctrl Pts',(53.5113218803221,19.0518193580581,25.6747219581622));
#36696=CARTESIAN_POINT('Ctrl Pts',(53.4473983911052,19.1023689554765,25.6705058946601));
#36697=CARTESIAN_POINT('Ctrl Pts',(53.3861481003195,19.1559738895836,25.6662898311581));
#36698=CARTESIAN_POINT('Ctrl Pts',(53.324899279199,19.2095775374713,25.662073868818));
#36699=CARTESIAN_POINT('Ctrl Pts',(53.2663238781257,19.2662360692495,25.657857906478));
#36700=CARTESIAN_POINT('Ctrl Pts',(53.2107305969442,19.32564482463,25.653641944138));
#36701=CARTESIAN_POINT('Ctrl Pts',(53.1546794870073,19.3855428304371,25.6493912619766));
#36702=CARTESIAN_POINT('Ctrl Pts',(53.1016601821046,19.4482362287982,25.6451405798152));
#36703=CARTESIAN_POINT('Ctrl Pts',(53.0519487152839,19.5133775051762,25.6408898976538));
#36704=CARTESIAN_POINT('Ctrl Pts',(53.0025716166071,19.5780806297744,25.6366678063346));
#36705=CARTESIAN_POINT('Ctrl Pts',(52.9564582090912,19.6451983815589,25.6324457150154));
#36706=CARTESIAN_POINT('Ctrl Pts',(52.9138352448007,19.7143613010786,25.6282236236962));
#36707=CARTESIAN_POINT('Ctrl Pts',(52.8707793340077,19.7842267490267,25.6239586461137));
#36708=CARTESIAN_POINT('Ctrl Pts',(52.8312854112849,19.8561787221728,25.6196936685312));
#36709=CARTESIAN_POINT('Ctrl Pts',(52.7955386279351,19.9298129560334,25.6154286909487));
#36710=CARTESIAN_POINT('Ctrl Pts',(52.7597918445854,20.0034471898942,25.6111637133662));
#36711=CARTESIAN_POINT('Ctrl Pts',(52.727792329923,20.078763215713,25.6068987357837));
#36712=CARTESIAN_POINT('Ctrl Pts',(52.6996739643788,20.1553400803617,25.6026337582012));
#36713=CARTESIAN_POINT('Ctrl Pts',(52.667503705164,20.2429517725044,25.5977541917072));
#36714=CARTESIAN_POINT('Ctrl Pts',(52.6403127382136,20.3324844781953,25.5928746252133));
#36715=CARTESIAN_POINT('Ctrl Pts',(52.6183017873507,20.423403196451,25.5879950587193));
#36716=CARTESIAN_POINT('Ctrl Pts',(52.595621605406,20.5170862492664,25.5829671316396));
#36717=CARTESIAN_POINT('Ctrl Pts',(52.5784416541832,20.6122408387639,25.5779392045599));
#36718=CARTESIAN_POINT('Ctrl Pts',(52.5669285807952,20.7082574438846,25.5729112774802));
#36719=CARTESIAN_POINT('Ctrl Pts',(52.5554155074072,20.8042740490054,25.5678833504004));
#36720=CARTESIAN_POINT('Ctrl Pts',(52.5495695209335,20.9011524863519,25.5628554233207));
#36721=CARTESIAN_POINT('Ctrl Pts',(52.5495006168754,20.9982612343868,25.557827496241));
#36722=CARTESIAN_POINT('',(52.5495006353634,21.0017646290239,24.7578274961833));
#36723=CARTESIAN_POINT('Ctrl Pts',(52.549500616875,20.9982612349457,25.5578274962121));
#36724=CARTESIAN_POINT('Ctrl Pts',(52.5494426726785,21.0799239169191,25.5535993085524));
#36725=CARTESIAN_POINT('Ctrl Pts',(52.5534711553422,21.161620251567,25.5493711208926));
#36726=CARTESIAN_POINT('Ctrl Pts',(52.5615695457031,21.242913913882,25.5451429332329));
#36727=CARTESIAN_POINT('Ctrl Pts',(52.5696676334938,21.3242045389216,25.5409149035457));
#36728=CARTESIAN_POINT('Ctrl Pts',(52.581835280649,21.4050920630522,25.5366868738586));
#36729=CARTESIAN_POINT('Ctrl Pts',(52.5980040885974,21.4851452273341,25.5324588441714));
#36730=CARTESIAN_POINT('Ctrl Pts',(52.6141771330571,21.5652193669495,25.5282297066663));
#36731=CARTESIAN_POINT('Ctrl Pts',(52.6343533283592,21.644458261135,25.5240005691613));
#36732=CARTESIAN_POINT('Ctrl Pts',(52.6584134445613,21.7224421453576,25.5197714316562));
#36733=CARTESIAN_POINT('Ctrl Pts',(52.6825035509126,21.8005232339455,25.5155370226692));
#36734=CARTESIAN_POINT('Ctrl Pts',(52.7104871040229,21.8773457495278,25.5113026136823));
#36735=CARTESIAN_POINT('Ctrl Pts',(52.7421955433444,21.9525068427607,25.5070682046954));
#36736=CARTESIAN_POINT('Ctrl Pts',(52.773926246832,22.0277207105576,25.5028308225068));
#36737=CARTESIAN_POINT('Ctrl Pts',(52.8093868421525,22.1012704194946,25.4985934403183));
#36738=CARTESIAN_POINT('Ctrl Pts',(52.8483624271334,22.1727770483041,25.4943560581297));
#36739=CARTESIAN_POINT('Ctrl Pts',(52.8874072856409,22.2444107699167,25.4901111446005));
#36740=CARTESIAN_POINT('Ctrl Pts',(52.9299793642756,22.3139937704215,25.4858662310712));
#36741=CARTESIAN_POINT('Ctrl Pts',(52.9758202471203,22.3811757954843,25.481621317542));
#36742=CARTESIAN_POINT('Ctrl Pts',(52.9974933438922,22.4129387642616,25.4796143661921));
#36743=CARTESIAN_POINT('Ctrl Pts',(53.0198965302943,22.4441655212112,25.4776074148422));
#36744=CARTESIAN_POINT('Ctrl Pts',(53.0429994982016,22.4748217810844,25.4756004634922));
#36745=CARTESIAN_POINT('Ctrl Pts',(53.0917071719663,22.5394539578134,25.4713692351926));
#36746=CARTESIAN_POINT('Ctrl Pts',(53.1437114313465,22.6017917748592,25.467138006893));
#36747=CARTESIAN_POINT('Ctrl Pts',(53.1987682558081,22.6614795977428,25.4629067785934));
#36748=CARTESIAN_POINT('Ctrl Pts',(53.2537461357293,22.7210818358184,25.4586816173414));
#36749=CARTESIAN_POINT('Ctrl Pts',(53.3117675751297,22.7780412874812,25.4544564560894));
#36750=CARTESIAN_POINT('Ctrl Pts',(53.3725469350141,22.8320335071357,25.4502312948374));
#36751=CARTESIAN_POINT('Ctrl Pts',(53.4334822869078,22.8861642994052,25.4459952895851));
#36752=CARTESIAN_POINT('Ctrl Pts',(53.497189444735,22.9373122361443,25.4417592843329));
#36753=CARTESIAN_POINT('Ctrl Pts',(53.5633417190128,22.9851859443566,25.4375232790806));
#36754=CARTESIAN_POINT('Ctrl Pts',(53.6292059510151,23.0328511993902,25.4333057183733));
#36755=CARTESIAN_POINT('Ctrl Pts',(53.6974936764225,23.0772703990278,25.4290881576659));
#36756=CARTESIAN_POINT('Ctrl Pts',(53.7678490520451,23.1181959993008,25.4248705969585));
#36757=CARTESIAN_POINT('Ctrl Pts',(53.8381812007487,23.1591080885151,25.4206544286244));
#36758=CARTESIAN_POINT('Ctrl Pts',(53.9105792425456,23.1965286352039,25.4164382602902));
#36759=CARTESIAN_POINT('Ctrl Pts',(53.9846599580242,23.2302544359693,25.4122220919561));
#36760=CARTESIAN_POINT('Ctrl Pts',(54.0587389110369,23.2639794343589,25.4080060239294));
#36761=CARTESIAN_POINT('Ctrl Pts',(54.1345000345426,23.294009669972,25.4037899559028));
#36762=CARTESIAN_POINT('Ctrl Pts',(54.211538524869,23.320189378528,25.3995738878762));
#36763=CARTESIAN_POINT('Ctrl Pts',(54.2892072715661,23.3465832648026,25.3953233279517));
#36764=CARTESIAN_POINT('Ctrl Pts',(54.3681739328913,23.369063161065,25.3910727680273));
#36765=CARTESIAN_POINT('Ctrl Pts',(54.4480081858695,23.3875207406707,25.3868222081029));
#36766=CARTESIAN_POINT('Ctrl Pts',(54.5273097442534,23.4058551619514,25.3826000100684));
#36767=CARTESIAN_POINT('Ctrl Pts',(54.6074668784613,23.4202207590966,25.378377812034));
#36768=CARTESIAN_POINT('Ctrl Pts',(54.6880495043284,23.4305631319203,25.3741556139995));
#36769=CARTESIAN_POINT('Ctrl Pts',(54.7694440801131,23.4410097144129,25.3698908731301));
#36770=CARTESIAN_POINT('Ctrl Pts',(54.8512722859611,23.4473515030673,25.3656261322607));
#36771=CARTESIAN_POINT('Ctrl Pts',(54.9330895701137,23.4495863414814,25.3613613913914));
#36772=CARTESIAN_POINT('Ctrl Pts',(55.0149068542662,23.4518211798956,25.357096650522));
#36773=CARTESIAN_POINT('Ctrl Pts',(55.0967127365403,23.449949143322,25.3528319096526));
#36774=CARTESIAN_POINT('Ctrl Pts',(55.1780685790446,23.4440216511228,25.3485671687832));
#36775=CARTESIAN_POINT('Ctrl Pts',(55.2587847438053,23.4381407651011,25.3443359603528));
#36776=CARTESIAN_POINT('Ctrl Pts',(55.3393606068678,23.4282459619067,25.3401047519223));
#36777=CARTESIAN_POINT('Ctrl Pts',(55.4193650420496,23.4143494385666,25.3358735434918));
#36778=CARTESIAN_POINT('Ctrl Pts',(55.4992547525024,23.4004728425577,25.3316484025279));
#36779=CARTESIAN_POINT('Ctrl Pts',(55.5785742082945,23.3826060021575,25.327423261564));
#36780=CARTESIAN_POINT('Ctrl Pts',(55.6568959221464,23.3608129950226,25.3231981206002));
#36781=CARTESIAN_POINT('Ctrl Pts',(55.7354191210712,23.3389639246911,25.3189621103283));
#36782=CARTESIAN_POINT('Ctrl Pts',(55.8129389677181,23.3131685020274,25.3147261000564));
#36783=CARTESIAN_POINT('Ctrl Pts',(55.8890334968853,23.2835432317817,25.3104900897844));
#36784=CARTESIAN_POINT('Ctrl Pts',(55.964796222984,23.2540471397526,25.3062725502386));
#36785=CARTESIAN_POINT('Ctrl Pts',(56.0391455966255,23.2207546919595,25.3020550106928));
#36786=CARTESIAN_POINT('Ctrl Pts',(56.1116806788173,23.183830652396,25.297837471147));
#36787=CARTESIAN_POINT('Ctrl Pts',(56.1841918095111,23.1469188053611,25.2936213242568));
#36788=CARTESIAN_POINT('Ctrl Pts',(56.2548894244571,23.1063779586927,25.2894051773666));
#36789=CARTESIAN_POINT('Ctrl Pts',(56.3233949968083,23.062419921457,25.2851890304764));
#36790=CARTESIAN_POINT('Ctrl Pts',(56.3918989351956,23.0184629326885,25.2809729841479));
#36791=CARTESIAN_POINT('Ctrl Pts',(56.4582105442443,22.9710891674222,25.2767569378193));
#36792=CARTESIAN_POINT('Ctrl Pts',(56.5219794533741,22.9205542932985,25.2725408914908));
#36793=CARTESIAN_POINT('Ctrl Pts',(56.5862707665526,22.8696054302387,25.268290306706));
#36794=CARTESIAN_POINT('Ctrl Pts',(56.6479771410842,22.8154437119307,25.2640397219213));
#36795=CARTESIAN_POINT('Ctrl Pts',(56.7067742173164,22.7583719803,25.2597891371366));
#36796=CARTESIAN_POINT('Ctrl Pts',(56.7651783223078,22.7016816885405,25.2555669612063));
#36797=CARTESIAN_POINT('Ctrl Pts',(56.8207116241952,22.6421205487075,25.251344785276));
#36798=CARTESIAN_POINT('Ctrl Pts',(56.8730952145496,22.5800204325361,25.2471226093456));
#36799=CARTESIAN_POINT('Ctrl Pts',(56.9260074983365,22.5172935566608,25.2428578201337));
#36800=CARTESIAN_POINT('Ctrl Pts',(56.9757058398398,22.4519765519319,25.2385930309218));
#36801=CARTESIAN_POINT('Ctrl Pts',(57.0219473713568,22.3844417927321,25.2343282417099));
#36802=CARTESIAN_POINT('Ctrl Pts',(57.0681889028738,22.3169070335323,25.230063452498));
#36803=CARTESIAN_POINT('Ctrl Pts',(57.1109734272501,22.2471549641736,25.2257986632861));
#36804=CARTESIAN_POINT('Ctrl Pts',(57.1501063028945,22.1755820414814,25.2215338740742));
#36805=CARTESIAN_POINT('Ctrl Pts',(57.1889311980197,22.1045724064476,25.2173026492752));
#36806=CARTESIAN_POINT('Ctrl Pts',(57.2243073473097,22.031504217792,25.2130714244762));
#36807=CARTESIAN_POINT('Ctrl Pts',(57.2560112343045,21.9567463408302,25.2088401996772));
#36808=CARTESIAN_POINT('Ctrl Pts',(57.2876696605508,21.8820956604731,25.2046150421041));
#36809=CARTESIAN_POINT('Ctrl Pts',(57.3156661026306,21.8057605282281,25.200389884531));
#36810=CARTESIAN_POINT('Ctrl Pts',(57.3398226093414,21.728134882295,25.196164726958));
#36811=CARTESIAN_POINT('Ctrl Pts',(57.3640411406536,21.6503099236132,25.1919287208083));
#36812=CARTESIAN_POINT('Ctrl Pts',(57.384399771629,21.5711882329147,25.1876927146586));
#36813=CARTESIAN_POINT('Ctrl Pts',(57.4007675983464,21.4911875290864,25.1834567085089));
#36814=CARTESIAN_POINT('Ctrl Pts',(57.4170641365159,21.4115352608879,25.1792391518903));
#36815=CARTESIAN_POINT('Ctrl Pts',(57.4294044593048,21.3310120772491,25.1750215952716));
#36816=CARTESIAN_POINT('Ctrl Pts',(57.437709610775,21.2500442031628,25.170804038653));
#36817=CARTESIAN_POINT('Ctrl Pts',(57.4460120201169,21.1691030623992,25.1665878745533));
#36818=CARTESIAN_POINT('Ctrl Pts',(57.4502818564995,21.0877179848915,25.1623717104537));
#36819=CARTESIAN_POINT('Ctrl Pts',(57.4504918453088,21.0063218727681,25.158155546354));
#36820=CARTESIAN_POINT('Ctrl Pts',(57.4507018291151,20.9249276998684,25.1539394827025));
#36821=CARTESIAN_POINT('Ctrl Pts',(57.4468521575695,20.8435229577976,25.149723419051));
#36822=CARTESIAN_POINT('Ctrl Pts',(57.4389676745274,20.7625406716709,25.1455073553994));
#36823=CARTESIAN_POINT('Ctrl Pts',(57.4310186709482,20.6808956888822,25.1412567907299));
#36824=CARTESIAN_POINT('Ctrl Pts',(57.41896854609,20.5996805870595,25.1370062260604));
#36825=CARTESIAN_POINT('Ctrl Pts',(57.4028958826981,20.5193321033057,25.1327556613909));
#36826=CARTESIAN_POINT('Ctrl Pts',(57.3869304997749,20.439519922888,25.1285334680347));
#36827=CARTESIAN_POINT('Ctrl Pts',(57.3669962883082,20.3605632669893,25.1243112746786));
#36828=CARTESIAN_POINT('Ctrl Pts',(57.343220869384,20.2828764351359,25.1200890813225));
#36829=CARTESIAN_POINT('Ctrl Pts',(57.3192058096602,20.2044065704133,25.1158243309963));
#36830=CARTESIAN_POINT('Ctrl Pts',(57.2912718383737,20.1272327285547,25.1115595806701));
#36831=CARTESIAN_POINT('Ctrl Pts',(57.2596001429528,20.0517608719486,25.1072948303439));
#36832=CARTESIAN_POINT('Ctrl Pts',(57.2279284475319,19.9762890153425,25.1030300800177));
#36833=CARTESIAN_POINT('Ctrl Pts',(57.1925192943806,19.9025195505309,25.0987653296915));
#36834=CARTESIAN_POINT('Ctrl Pts',(57.1536002527356,19.8308309782511,25.0945005793653));
#36835=CARTESIAN_POINT('Ctrl Pts',(57.1149871920646,19.7597060205477,25.0902693584479));
#36836=CARTESIAN_POINT('Ctrl Pts',(57.0727744823731,19.6903626228375,25.0860381375306));
#36837=CARTESIAN_POINT('Ctrl Pts',(57.0271508610185,19.623188598002,25.0818069166132));
#36838=CARTESIAN_POINT('Ctrl Pts',(56.9815926604765,19.556110895623,25.0775817629457));
#36839=CARTESIAN_POINT('Ctrl Pts',(56.9326335211538,19.4911967693597,25.0733566092782));
#36840=CARTESIAN_POINT('Ctrl Pts',(56.880507954045,19.428809341686,25.0691314556107));
#36841=CARTESIAN_POINT('Ctrl Pts',(56.8282484882493,19.3662616549472,25.0648954484876));
#36842=CARTESIAN_POINT('Ctrl Pts',(56.7728065370341,19.3062540761956,25.0606594413645));
#36843=CARTESIAN_POINT('Ctrl Pts',(56.7144621038584,19.2491230927237,25.0564234342414));
#36844=CARTESIAN_POINT('Ctrl Pts',(56.6563718519762,19.1922410040732,25.0522058815571));
#36845=CARTESIAN_POINT('Ctrl Pts',(56.5954046836663,19.1382108320083,25.0479883288727));
#36846=CARTESIAN_POINT('Ctrl Pts',(56.5318759159369,19.0873300263316,25.0437707761884));
#36847=CARTESIAN_POINT('Ctrl Pts',(56.4683681236747,19.0364660201099,25.039554616025));
#36848=CARTESIAN_POINT('Ctrl Pts',(56.4023007741706,18.9887496057174,25.0353384558616));
#36849=CARTESIAN_POINT('Ctrl Pts',(56.3340228175641,18.9444384289887,25.0311222956982));
#36850=CARTESIAN_POINT('Ctrl Pts',(56.2657464875926,18.9001283079172,25.0269062359794));
#36851=CARTESIAN_POINT('Ctrl Pts',(56.1952600458253,18.8592235153788,25.0226901762606));
#36852=CARTESIAN_POINT('Ctrl Pts',(56.1229408055264,18.8219379721221,25.0184741165418));
#36853=CARTESIAN_POINT('Ctrl Pts',(56.0500296124128,18.7843472364686,25.014223547218));
#36854=CARTESIAN_POINT('Ctrl Pts',(55.9752558973944,18.7504355067548,25.0099729778943));
#36855=CARTESIAN_POINT('Ctrl Pts',(55.8990292335745,18.7203735641166,25.0057224085705));
#36856=CARTESIAN_POINT('Ctrl Pts',(55.8233115136671,18.6905123365818,25.0015002190979));
#36857=CARTESIAN_POINT('Ctrl Pts',(55.7461606523289,18.6644497364852,24.9972780296254));
#36858=CARTESIAN_POINT('Ctrl Pts',(55.6679939570079,18.6423031739851,24.9930558401529));
#36859=CARTESIAN_POINT('Ctrl Pts',(55.5890391542837,18.6199333211208,24.9887910809035));
#36860=CARTESIAN_POINT('Ctrl Pts',(55.5090483916766,18.6015590251151,24.984526321654));
#36861=CARTESIAN_POINT('Ctrl Pts',(55.4284610202324,18.587248167726,24.9802615624046));
#36862=CARTESIAN_POINT('Ctrl Pts',(55.3478736487883,18.572937310337,24.9759968031552));
#36863=CARTESIAN_POINT('Ctrl Pts',(55.2666901545566,18.5626898881577,24.9717320439058));
#36864=CARTESIAN_POINT('Ctrl Pts',(55.1853519635064,18.5565199203545,24.9674672846563));
#36865=CARTESIAN_POINT('Ctrl Pts',(55.104653461615,18.550398476639,24.9632360658658));
#36866=CARTESIAN_POINT('Ctrl Pts',(55.0235000796318,18.5482675811919,24.9590048470753));
#36867=CARTESIAN_POINT('Ctrl Pts',(54.9423200086918,18.5501789313089,24.9547736282848));
#36868=CARTESIAN_POINT('Ctrl Pts',(54.8612563448273,18.552087540671,24.9505484767939));
#36869=CARTESIAN_POINT('Ctrl Pts',(54.7801665288857,18.5580268728122,24.9463233253029));
#36870=CARTESIAN_POINT('Ctrl Pts',(54.6994828257887,18.5679967767283,24.9420981738119));
#36871=CARTESIAN_POINT('Ctrl Pts',(54.6185918127283,18.5779922974708,24.9378621661509));
#36872=CARTESIAN_POINT('Ctrl Pts',(54.5381094732769,18.5920391582366,24.9336261584899));
#36873=CARTESIAN_POINT('Ctrl Pts',(54.458470360457,18.6100845413495,24.9293901508289));
#36874=CARTESIAN_POINT('Ctrl Pts',(54.3791782535467,18.6280512965828,24.9251726004263));
#36875=CARTESIAN_POINT('Ctrl Pts',(54.3007224984419,18.6499817064567,24.9209550500238));
#36876=CARTESIAN_POINT('Ctrl Pts',(54.2235239944632,18.6757721146958,24.9167374996213));
#36877=CARTESIAN_POINT('Ctrl Pts',(54.1463509799739,18.7015540074288,24.9125213417743));
#36878=CARTESIAN_POINT('Ctrl Pts',(54.0704348328585,18.7311932203502,24.9083051839273));
#36879=CARTESIAN_POINT('Ctrl Pts',(53.9961812444017,18.7645362548435,24.9040890260804));
#36880=CARTESIAN_POINT('Ctrl Pts',(53.9219294254996,18.7978784947312,24.8998729687097));
#36881=CARTESIAN_POINT('Ctrl Pts',(53.84934051015,18.8349241892326,24.895656911339));
#36882=CARTESIAN_POINT('Ctrl Pts',(53.778798829418,18.8754722993171,24.8914408539682));
#36883=CARTESIAN_POINT('Ctrl Pts',(53.7076796612686,18.9163523553253,24.8871902819665));
#36884=CARTESIAN_POINT('Ctrl Pts',(53.638641825627,18.960792211328,24.8829397099648));
#36885=CARTESIAN_POINT('Ctrl Pts',(53.572050899435,19.0085403302613,24.878689137963));
#36886=CARTESIAN_POINT('Ctrl Pts',(53.505904661363,19.0559695916197,24.8744669508927));
#36887=CARTESIAN_POINT('Ctrl Pts',(53.4421730807613,19.1066627252754,24.8702447638223));
#36888=CARTESIAN_POINT('Ctrl Pts',(53.3811810828112,19.1603327574391,24.866022576752));
#36889=CARTESIAN_POINT('Ctrl Pts',(53.3195740290917,19.2145440091732,24.8617578122846));
#36890=CARTESIAN_POINT('Ctrl Pts',(53.2607624701863,19.2717921978405,24.8574930478171));
#36891=CARTESIAN_POINT('Ctrl Pts',(53.2050416698394,19.3317449706394,24.8532282833497));
#36892=CARTESIAN_POINT('Ctrl Pts',(53.1493208694925,19.3916977434382,24.8489635188822));
#36893=CARTESIAN_POINT('Ctrl Pts',(53.0966910883909,19.4543546901213,24.8446987544148));
#36894=CARTESIAN_POINT('Ctrl Pts',(53.0474034577743,19.5193525087691,24.8404339899473));
#36895=CARTESIAN_POINT('Ctrl Pts',(52.9983789905267,19.5840032820282,24.8361919965032));
#36896=CARTESIAN_POINT('Ctrl Pts',(52.9524752143873,19.6512149433991,24.831950003059));
#36897=CARTESIAN_POINT('Ctrl Pts',(52.9099697495301,19.7206549323499,24.8277080096149));
#36898=CARTESIAN_POINT('Ctrl Pts',(52.8675250489743,19.7899956523612,24.8234720803738));
#36899=CARTESIAN_POINT('Ctrl Pts',(52.8284692525181,19.8615579854376,24.8192361511326));
#36900=CARTESIAN_POINT('Ctrl Pts',(52.7930388342031,19.9349776233974,24.8150002218915));
#36901=CARTESIAN_POINT('Ctrl Pts',(52.7576484095447,20.0083143856833,24.8107690741434));
#36902=CARTESIAN_POINT('Ctrl Pts',(52.725875434281,20.083503875713,24.8065379263954));
#36903=CARTESIAN_POINT('Ctrl Pts',(52.6979115347011,20.1601554025072,24.8023067786473));
#36904=CARTESIAN_POINT('Ctrl Pts',(52.6699708433048,20.2367433136135,24.7980791424715));
#36905=CARTESIAN_POINT('Ctrl Pts',(52.6458331031965,20.3147904181951,24.7938515062957));
#36906=CARTESIAN_POINT('Ctrl Pts',(52.6256421094426,20.3938854418943,24.7896238701199));
#36907=CARTESIAN_POINT('Ctrl Pts',(52.6054609709417,20.4729418591987,24.7853982974593));
#36908=CARTESIAN_POINT('Ctrl Pts',(52.5892228633599,20.5530447324479,24.7811727247988));
#36909=CARTESIAN_POINT('Ctrl Pts',(52.577021547851,20.6337682831571,24.7769471521383));
#36910=CARTESIAN_POINT('Ctrl Pts',(52.5648200476823,20.7144930555703,24.7727215155262));
#36911=CARTESIAN_POINT('Ctrl Pts',(52.5566555379763,20.7958380691267,24.7684958789141));
#36912=CARTESIAN_POINT('Ctrl Pts',(52.5525703438381,20.8773691387166,24.764270242302));
#36913=CARTESIAN_POINT('Ctrl Pts',(52.5504941384457,20.9188054182667,24.7621226602721));
#36914=CARTESIAN_POINT('Ctrl Pts',(52.5494707688368,20.9602896636726,24.7599750782421));
#36915=CARTESIAN_POINT('Ctrl Pts',(52.549500635363,21.0017646284675,24.7578274962121));
#36916=CARTESIAN_POINT('',(52.5495001212409,21.0007708448949,23.9578274962553));
#36917=CARTESIAN_POINT('Ctrl Pts',(52.5495006353634,21.001764629024,24.7578274961833));
#36918=CARTESIAN_POINT('Ctrl Pts',(52.5495679528408,21.0952468472569,24.7529869680962));
#36919=CARTESIAN_POINT('Ctrl Pts',(52.5549885424231,21.1885143020218,24.7481464400091));
#36920=CARTESIAN_POINT('Ctrl Pts',(52.5656650324199,21.2810044761507,24.743305911922));
#36921=CARTESIAN_POINT('Ctrl Pts',(52.5766584178876,21.3762399080658,24.7383217091414));
#36922=CARTESIAN_POINT('Ctrl Pts',(52.5932244071865,21.4706509753609,24.7333375063608));
#36923=CARTESIAN_POINT('Ctrl Pts',(52.6152033071151,21.5636443768948,24.7283533035802));
#36924=CARTESIAN_POINT('Ctrl Pts',(52.6371822070437,21.6566377784288,24.7233691007996));
#36925=CARTESIAN_POINT('Ctrl Pts',(52.6645738460604,21.7482133664511,24.718384898019));
#36926=CARTESIAN_POINT('Ctrl Pts',(52.6971671152198,21.8378012620991,24.7134006952384));
#36927=CARTESIAN_POINT('Ctrl Pts',(52.7248363953362,21.9138547738718,24.7091694749144));
#36928=CARTESIAN_POINT('Ctrl Pts',(52.7563292240878,21.9886786948271,24.7049382545903));
#36929=CARTESIAN_POINT('Ctrl Pts',(52.7915162961357,22.0618615633714,24.7007070342663));
#36930=CARTESIAN_POINT('Ctrl Pts',(52.8266529124041,22.1349394928442,24.6964818812138));
#36931=CARTESIAN_POINT('Ctrl Pts',(52.8654730514026,22.2063806279751,24.6922567281613));
#36932=CARTESIAN_POINT('Ctrl Pts',(52.9077984858989,22.2757911562607,24.6880315751087));
#36933=CARTESIAN_POINT('Ctrl Pts',(52.9502326524672,22.3453799969641,24.6837955678346));
#36934=CARTESIAN_POINT('Ctrl Pts',(52.9961899800574,22.4129273430252,24.6795595605604));
#36935=CARTESIAN_POINT('Ctrl Pts',(53.0454433098682,22.4780589957985,24.6753235532863));
#36936=CARTESIAN_POINT('Ctrl Pts',(53.0944820549032,22.5429068858058,24.6711060012653));
#36937=CARTESIAN_POINT('Ctrl Pts',(53.1467878666111,22.6053597096896,24.6668884492444));
#36938=CARTESIAN_POINT('Ctrl Pts',(53.2020928875876,22.6650766544327,24.6626708972234));
#36939=CARTESIAN_POINT('Ctrl Pts',(53.2573796481305,22.7247738820275,24.6584547377402));
#36940=CARTESIAN_POINT('Ctrl Pts',(53.3156633357472,22.781736683515,24.6542385782569));
#36941=CARTESIAN_POINT('Ctrl Pts',(53.3766369428855,22.8356586378725,24.6500224187737));
#36942=CARTESIAN_POINT('Ctrl Pts',(53.4376090971747,22.8895793074042,24.645806359751));
#36943=CARTESIAN_POINT('Ctrl Pts',(53.5012706945447,22.9404589667043,24.6415903007283));
#36944=CARTESIAN_POINT('Ctrl Pts',(53.5672802094262,22.9880302441608,24.6373742417057));
#36945=CARTESIAN_POINT('Ctrl Pts',(53.6338300533993,23.0359909222239,24.6331236716076));
#36946=CARTESIAN_POINT('Ctrl Pts',(53.7027660508481,23.0805885126075,24.6288731015096));
#36947=CARTESIAN_POINT('Ctrl Pts',(53.7737083905136,23.1215935375333,24.6246225314116));
#36948=CARTESIAN_POINT('Ctrl Pts',(53.8441770432134,23.1623247690387,24.6204003426675));
#36949=CARTESIAN_POINT('Ctrl Pts',(53.9166248808244,23.1995111052045,24.6161781539234));
#36950=CARTESIAN_POINT('Ctrl Pts',(53.9906565497935,23.2329747086622,24.6119559651793));
#36951=CARTESIAN_POINT('Ctrl Pts',(54.0654346748524,23.2667757232703,24.6076912044043));
#36952=CARTESIAN_POINT('Ctrl Pts',(54.1418282981851,23.2967783329379,24.6034264436293));
#36953=CARTESIAN_POINT('Ctrl Pts',(54.2194129392859,23.3228504236489,24.5991616828543));
#36954=CARTESIAN_POINT('Ctrl Pts',(54.2969975803868,23.3489225143599,24.5948969220793));
#36955=CARTESIAN_POINT('Ctrl Pts',(54.3757727580464,23.3710640175984,24.5906321613043));
#36956=CARTESIAN_POINT('Ctrl Pts',(54.4553039735296,23.3891957828415,24.5863674005293));
#36957=CARTESIAN_POINT('Ctrl Pts',(54.5342097074288,23.4071849489154,24.5821361804126));
#36958=CARTESIAN_POINT('Ctrl Pts',(54.6141555072841,23.421294723698,24.577904960296));
#36959=CARTESIAN_POINT('Ctrl Pts',(54.6947255363877,23.4314106506031,24.5736737401793));
#36960=CARTESIAN_POINT('Ctrl Pts',(54.7751800336395,23.4415120719684,24.5694485873398));
#36961=CARTESIAN_POINT('Ctrl Pts',(54.8562565249924,23.447630962083,24.5652234345002));
#36962=CARTESIAN_POINT('Ctrl Pts',(54.937527476602,23.4497035399861,24.5609982816607));
#36963=CARTESIAN_POINT('Ctrl Pts',(55.0190072146233,23.4517814423759,24.556762274334));
#36964=CARTESIAN_POINT('Ctrl Pts',(55.1006819516917,23.4497921171981,24.5525262670073));
#36965=CARTESIAN_POINT('Ctrl Pts',(55.1821141023636,23.4437235325872,24.5482902596807));
#36966=CARTESIAN_POINT('Ctrl Pts',(55.2631914676302,23.4376813877207,24.5440727078849));
#36967=CARTESIAN_POINT('Ctrl Pts',(55.3440278887176,23.4275954811244,24.5398551560892));
#36968=CARTESIAN_POINT('Ctrl Pts',(55.4241917643742,23.4135060797597,24.5356376042934));
#36969=CARTESIAN_POINT('Ctrl Pts',(55.5043291717013,23.3994213304021,24.5314214450395));
#36970=CARTESIAN_POINT('Ctrl Pts',(55.5837940170331,23.381335791731,24.5272052857856));
#36971=CARTESIAN_POINT('Ctrl Pts',(55.6621623684179,23.359341274138,24.5229891265317));
#36972=CARTESIAN_POINT('Ctrl Pts',(55.7405288524091,23.3373472806395,24.5187730677422));
#36973=CARTESIAN_POINT('Ctrl Pts',(55.8177984470749,23.3114446201112,24.5145570089527));
#36974=CARTESIAN_POINT('Ctrl Pts',(55.8935613147325,23.2817752796482,24.5103409501632));
#36975=CARTESIAN_POINT('Ctrl Pts',(55.9699443577297,23.2518630735985,24.5060903798013));
#36976=CARTESIAN_POINT('Ctrl Pts',(56.0447954399595,23.2181223968107,24.5018398094394));
#36977=CARTESIAN_POINT('Ctrl Pts',(56.1177158039986,23.1807479523071,24.4975892390775));
#36978=CARTESIAN_POINT('Ctrl Pts',(56.1901492650474,23.1436230640013,24.4933670505736));
#36979=CARTESIAN_POINT('Ctrl Pts',(56.2606773371968,23.1029130751492,24.4891448620697));
#36980=CARTESIAN_POINT('Ctrl Pts',(56.328936225891,23.0588537484519,24.4849226735659));
#36981=CARTESIAN_POINT('Ctrl Pts',(56.3978833764026,23.0143501667596,24.480657912275));
#36982=CARTESIAN_POINT('Ctrl Pts',(56.464514930647,22.9664296072111,24.476393150984));
#36983=CARTESIAN_POINT('Ctrl Pts',(56.5284897189965,22.91537709836,24.4721283896931));
#36984=CARTESIAN_POINT('Ctrl Pts',(56.592464507346,22.8643245895089,24.4678636284022));
#36985=CARTESIAN_POINT('Ctrl Pts',(56.6537822113085,22.810140498534,24.4635988671113));
#36986=CARTESIAN_POINT('Ctrl Pts',(56.712140730981,22.7531469896491,24.4593341058204));
#36987=CARTESIAN_POINT('Ctrl Pts',(56.7700402808879,22.6966017151877,24.4551028854161));
#36988=CARTESIAN_POINT('Ctrl Pts',(56.825244174904,22.6370790495558,24.4508716650117));
#36989=CARTESIAN_POINT('Ctrl Pts',(56.8774307668126,22.5748663326852,24.4466404446074));
#36990=CARTESIAN_POINT('Ctrl Pts',(56.9295425268185,22.5127428244755,24.4424152914756));
#36991=CARTESIAN_POINT('Ctrl Pts',(56.9786452813961,22.4479372791931,24.4381901383438));
#36992=CARTESIAN_POINT('Ctrl Pts',(57.0244536213447,22.3807743425427,24.433964985212));
#36993=CARTESIAN_POINT('Ctrl Pts',(57.0703796397092,22.3134388690136,24.4297289779578));
#36994=CARTESIAN_POINT('Ctrl Pts',(57.112993962336,22.2437342110515,24.4254929707036));
#36995=CARTESIAN_POINT('Ctrl Pts',(57.1520492113159,22.1720215194588,24.4212569634494));
#36996=CARTESIAN_POINT('Ctrl Pts',(57.1909343069628,22.1006212609913,24.4170394113523));
#36997=CARTESIAN_POINT('Ctrl Pts',(57.2262910452087,22.0272308363188,24.4128218592551));
#36998=CARTESIAN_POINT('Ctrl Pts',(57.2579192361645,21.952234725768,24.4086043071579));
#36999=CARTESIAN_POINT('Ctrl Pts',(57.2895369842162,21.8772633772145,24.4043881475999));
#37000=CARTESIAN_POINT('Ctrl Pts',(57.3174284492104,21.8006878236554,24.4001719880418));
#37001=CARTESIAN_POINT('Ctrl Pts',(57.341440908335,21.7229140493692,24.3959558284837));
#37002=CARTESIAN_POINT('Ctrl Pts',(57.3654527952943,21.6451421282649,24.3917397693876));
#37003=CARTESIAN_POINT('Ctrl Pts',(57.3855857240596,21.5661724877579,24.3875237102915));
#37004=CARTESIAN_POINT('Ctrl Pts',(57.4017367742816,21.486426476524,24.3833076511955));
#37005=CARTESIAN_POINT('Ctrl Pts',(57.4180200303012,21.4060276975208,24.3790570811885));
#37006=CARTESIAN_POINT('Ctrl Pts',(57.4302558079205,21.3248402460121,24.3748065111815));
#37007=CARTESIAN_POINT('Ctrl Pts',(57.4383914885568,21.2433047441661,24.3705559411745));
#37008=CARTESIAN_POINT('Ctrl Pts',(57.4464728469894,21.1623136575121,24.3663337523614));
#37009=CARTESIAN_POINT('Ctrl Pts',(57.4505087331316,21.0809796262463,24.3621115635482));
#37010=CARTESIAN_POINT('Ctrl Pts',(57.4504999857964,20.9997361591577,24.3578893747351));
#37011=CARTESIAN_POINT('Ctrl Pts',(57.4504911502629,20.9176735245613,24.3536246141312));
#37012=CARTESIAN_POINT('Ctrl Pts',(57.4463556836074,20.8357037758953,24.3493598535272));
#37013=CARTESIAN_POINT('Ctrl Pts',(57.4381480872401,20.754268124397,24.3450950929233));
#37014=CARTESIAN_POINT('Ctrl Pts',(57.4299404908729,20.6728324728988,24.3408303323193));
#37015=CARTESIAN_POINT('Ctrl Pts',(57.417660900617,20.5919313852684,24.3365655717154));
#37016=CARTESIAN_POINT('Ctrl Pts',(57.4014162049876,20.511993380759,24.3323008111114));
#37017=CARTESIAN_POINT('Ctrl Pts',(57.3852992661294,20.4326840504696,24.3280695908124));
#37018=CARTESIAN_POINT('Ctrl Pts',(57.3652189746059,20.3540252989922,24.3238383705134));
#37019=CARTESIAN_POINT('Ctrl Pts',(57.3412423599677,20.2764431868243,24.3196071502143));
#37020=CARTESIAN_POINT('Ctrl Pts',(57.3173001261158,20.1989723219722,24.3153819971889));
#37021=CARTESIAN_POINT('Ctrl Pts',(57.2894728015774,20.1225754707219,24.3111568441635));
#37022=CARTESIAN_POINT('Ctrl Pts',(57.2578784100349,20.0476684739556,24.306931691138));
#37023=CARTESIAN_POINT('Ctrl Pts',(57.2262028537188,19.9725690440028,24.3026956838574));
#37024=CARTESIAN_POINT('Ctrl Pts',(57.1907409510164,19.8989675943689,24.2984596765767));
#37025=CARTESIAN_POINT('Ctrl Pts',(57.1516620198987,19.827267804601,24.2942236692961));
#37026=CARTESIAN_POINT('Ctrl Pts',(57.1127533465325,19.7558803940265,24.2900061173072));
#37027=CARTESIAN_POINT('Ctrl Pts',(57.070259312843,19.6863785224298,24.2857885653183));
#37028=CARTESIAN_POINT('Ctrl Pts',(57.024394425453,19.6191388700544,24.2815710133293));
#37029=CARTESIAN_POINT('Ctrl Pts',(56.9785446816035,19.5519214186795,24.27735485388));
#37030=CARTESIAN_POINT('Ctrl Pts',(56.9293265560521,19.4869650869988,24.2731386944306));
#37031=CARTESIAN_POINT('Ctrl Pts',(56.8769983614893,19.4246183316521,24.2689225349812));
#37032=CARTESIAN_POINT('Ctrl Pts',(56.8246714137989,19.3622730618994,24.2647064759942));
#37033=CARTESIAN_POINT('Ctrl Pts',(56.7692348441787,19.3025376002505,24.2604904170071));
#37034=CARTESIAN_POINT('Ctrl Pts',(56.7109868790124,19.2457268884671,24.2562743580201));
#37035=CARTESIAN_POINT('Ctrl Pts',(56.6522621168805,19.1884511445591,24.2520237878853));
#37036=CARTESIAN_POINT('Ctrl Pts',(56.5906800528197,19.1341485998738,24.2477732177505));
#37037=CARTESIAN_POINT('Ctrl Pts',(56.5265823822585,19.0831023814042,24.2435226476157));
#37038=CARTESIAN_POINT('Ctrl Pts',(56.4629126974768,19.0323970030216,24.2393004589112));
#37039=CARTESIAN_POINT('Ctrl Pts',(56.3967613151867,18.9849048213301,24.2350782702068));
#37040=CARTESIAN_POINT('Ctrl Pts',(56.3284929396148,18.9408601894496,24.2308560815023));
#37041=CARTESIAN_POINT('Ctrl Pts',(56.2595362169737,18.8963714574566,24.2265913206523));
#37042=CARTESIAN_POINT('Ctrl Pts',(56.1884199905976,18.8554004320855,24.2223265598024));
#37043=CARTESIAN_POINT('Ctrl Pts',(56.1155445337149,18.8181405537251,24.2180617989524));
#37044=CARTESIAN_POINT('Ctrl Pts',(56.0426690768322,18.7808806753648,24.2137970381024));
#37045=CARTESIAN_POINT('Ctrl Pts',(55.9680348552272,18.7473320829471,24.2095322772524));
#37046=CARTESIAN_POINT('Ctrl Pts',(55.8920598833107,18.7176373174739,24.2052675164025));
#37047=CARTESIAN_POINT('Ctrl Pts',(55.8166824229039,18.688176088963,24.2010362961202));
#37048=CARTESIAN_POINT('Ctrl Pts',(55.7397025854611,18.6623977675449,24.196805075838));
#37049=CARTESIAN_POINT('Ctrl Pts',(55.6615147069631,18.6404770519295,24.1925738555558));
#37050=CARTESIAN_POINT('Ctrl Pts',(55.583438944419,18.6185877690884,24.1883487025478));
#37051=CARTESIAN_POINT('Ctrl Pts',(55.5041590250756,18.6005452304495,24.1841235495398));
#37052=CARTESIAN_POINT('Ctrl Pts',(55.4240883481641,18.5864757463511,24.1798983965318));
#37053=CARTESIAN_POINT('Ctrl Pts',(55.3438119723586,18.5723701182181,24.1756623892469));
#37054=CARTESIAN_POINT('Ctrl Pts',(55.2627412128886,18.5622581498905,24.1714263819619));
#37055=CARTESIAN_POINT('Ctrl Pts',(55.1813070634924,18.556216458291,24.167190374677));
#37056=CARTESIAN_POINT('Ctrl Pts',(55.1002277040579,18.5502010889598,24.1629728227069));
#37057=CARTESIAN_POINT('Ctrl Pts',(55.0187885804917,18.5482206465637,24.1587552707367));
#37058=CARTESIAN_POINT('Ctrl Pts',(54.93742250303,18.5502991393084,24.1545377187666));
#37059=CARTESIAN_POINT('Ctrl Pts',(54.8560832908016,18.5523769457821,24.1503215593365));
#37060=CARTESIAN_POINT('Ctrl Pts',(54.7748175411876,18.5585110141472,24.1461053999063));
#37061=CARTESIAN_POINT('Ctrl Pts',(54.6940581025609,18.5686732417482,24.1418892404762));
#37062=CARTESIAN_POINT('Ctrl Pts',(54.6133005882727,18.5788352272032,24.1376731815088));
#37063=CARTESIAN_POINT('Ctrl Pts',(54.5330498221303,18.5930251219099,24.1334571225415));
#37064=CARTESIAN_POINT('Ctrl Pts',(54.4537321341972,18.6111631138164,24.1292410635741));
#37065=CARTESIAN_POINT('Ctrl Pts',(54.3737651793135,18.6294495770035,24.1249904934174));
#37066=CARTESIAN_POINT('Ctrl Pts',(54.294747120078,18.6517489799349,24.1207399232607));
#37067=CARTESIAN_POINT('Ctrl Pts',(54.2171011245379,18.6779277356637,24.116489353104));
#37068=CARTESIAN_POINT('Ctrl Pts',(54.139973578908,18.7039316932787,24.1122671644201));
#37069=CARTESIAN_POINT('Ctrl Pts',(54.0642002441902,18.7337631263087,24.1080449757363));
#37070=CARTESIAN_POINT('Ctrl Pts',(53.9901757827592,18.7672426687448,24.1038227870524));
#37071=CARTESIAN_POINT('Ctrl Pts',(53.9154049347732,18.8010597844621,24.0995580261592));
#37072=CARTESIAN_POINT('Ctrl Pts',(53.8424188582653,18.8385987690382,24.0952932652661));
#37073=CARTESIAN_POINT('Ctrl Pts',(53.7715971255929,18.8796281863436,24.0910285043729));
#37074=CARTESIAN_POINT('Ctrl Pts',(53.7007753929206,18.920657603649,24.0867637434798));
#37075=CARTESIAN_POINT('Ctrl Pts',(53.6321183733777,18.9651771376472,24.0824989825866));
#37076=CARTESIAN_POINT('Ctrl Pts',(53.5659724915114,19.0129128466778,24.0782342216934));
#37077=CARTESIAN_POINT('Ctrl Pts',(53.5008642707206,19.0598997035385,24.0740363640791));
#37078=CARTESIAN_POINT('Ctrl Pts',(53.4379362932099,19.1101850001007,24.0698385064647));
#37079=CARTESIAN_POINT('Ctrl Pts',(53.3775460234526,19.1635378185256,24.0656406488503));
#37080=CARTESIAN_POINT('Ctrl Pts',(53.3172425789925,19.2168139296543,24.0614488266492));
#37081=CARTESIAN_POINT('Ctrl Pts',(53.2594699503941,19.2731484967592,24.0572570044481));
#37082=CARTESIAN_POINT('Ctrl Pts',(53.2045555862405,19.3322681249374,24.053065182247));
#37083=CARTESIAN_POINT('Ctrl Pts',(53.1497042104883,19.3913199411519,24.04887816819));
#37084=CARTESIAN_POINT('Ctrl Pts',(53.0977049060763,19.453150127131,24.044691154133));
#37085=CARTESIAN_POINT('Ctrl Pts',(53.0488498620535,19.5174470029064,24.0405041400761));
#37086=CARTESIAN_POINT('Ctrl Pts',(53.0000249526541,19.5817042192734,24.0363197086407));
#37087=CARTESIAN_POINT('Ctrl Pts',(52.9543407407577,19.6484247306994,24.0321352772054));
#37088=CARTESIAN_POINT('Ctrl Pts',(52.912049694455,19.7172631713503,24.02795084577));
#37089=CARTESIAN_POINT('Ctrl Pts',(52.8697712616863,19.7860810805625,24.0237676623641));
#37090=CARTESIAN_POINT('Ctrl Pts',(52.8308842326171,19.8570152619749,24.0195844789581));
#37091=CARTESIAN_POINT('Ctrl Pts',(52.7955973479013,19.9296920081489,24.0154012955521));
#37092=CARTESIAN_POINT('Ctrl Pts',(52.7603097468149,20.0023702297574,24.011218027222));
#37093=CARTESIAN_POINT('Ctrl Pts',(52.7286226398433,20.0767906598515,24.0070347588918));
#37094=CARTESIAN_POINT('Ctrl Pts',(52.7006977712595,20.1525570751319,24.0028514905617));
#37095=CARTESIAN_POINT('Ctrl Pts',(52.6727459280927,20.2283966784902,23.9986641813202));
#37096=CARTESIAN_POINT('Ctrl Pts',(52.6485637418823,20.3055844177771,23.9944768720787));
#37097=CARTESIAN_POINT('Ctrl Pts',(52.6282636822496,20.3837069779204,23.9902895628372));
#37098=CARTESIAN_POINT('Ctrl Pts',(52.6079529533278,20.4618705976567,23.986100052833));
#37099=CARTESIAN_POINT('Ctrl Pts',(52.591528507675,20.5409695528187,23.9819105428288));
#37100=CARTESIAN_POINT('Ctrl Pts',(52.5790515600889,20.6205808369471,23.9777210328247));
#37101=CARTESIAN_POINT('Ctrl Pts',(52.5665542265355,20.7003221972033,23.9735246776195));
#37102=CARTESIAN_POINT('Ctrl Pts',(52.5580173158697,20.7805770872105,23.9693283224144));
#37103=CARTESIAN_POINT('Ctrl Pts',(52.5534500674818,20.8609184494799,23.9651319672093));
#37104=CARTESIAN_POINT('Ctrl Pts',(52.5508000429122,20.9075343910461,23.962697143558));
#37105=CARTESIAN_POINT('Ctrl Pts',(52.5494854651526,20.9541794450299,23.9602623199067));
#37106=CARTESIAN_POINT('Ctrl Pts',(52.5495001212409,21.0007708448949,23.9578274962553));
#37107=CARTESIAN_POINT('',(52.5495010260079,20.9977575763378,23.1578275052968));
#37108=CARTESIAN_POINT('Ctrl Pts',(52.5495001212412,21.0007708457221,23.9578274962121));
#37109=CARTESIAN_POINT('Ctrl Pts',(52.5495134171649,21.0430382650271,23.9556186398029));
#37110=CARTESIAN_POINT('Ctrl Pts',(52.5506202182564,21.0852870907162,23.9534097833937));
#37111=CARTESIAN_POINT('Ctrl Pts',(52.5528180575916,21.1274785893789,23.9512009269845));
#37112=CARTESIAN_POINT('Ctrl Pts',(52.5570281739119,21.2082993819897,23.9469697066815));
#37113=CARTESIAN_POINT('Ctrl Pts',(52.5652542756311,21.2890629167757,23.9427384863785));
#37114=CARTESIAN_POINT('Ctrl Pts',(52.5774930832419,21.3693379052562,23.9385072660755));
#37115=CARTESIAN_POINT('Ctrl Pts',(52.5897143412591,21.4494977850218,23.9342821130463));
#37116=CARTESIAN_POINT('Ctrl Pts',(52.6059368079309,21.5291700540761,23.930056960017));
#37117=CARTESIAN_POINT('Ctrl Pts',(52.6261052589627,21.6079259893073,23.9258318069878));
#37118=CARTESIAN_POINT('Ctrl Pts',(52.6463255219447,21.6868842454103,23.9215957997081));
#37119=CARTESIAN_POINT('Ctrl Pts',(52.6705120384248,21.7649209825741,23.9173597924284));
#37120=CARTESIAN_POINT('Ctrl Pts',(52.6985570552922,21.8416119190308,23.9131237851488));
#37121=CARTESIAN_POINT('Ctrl Pts',(52.7264798866173,21.9179687311151,23.9089062331565));
#37122=CARTESIAN_POINT('Ctrl Pts',(52.75822751428,21.99299100249,23.9046886811642));
#37123=CARTESIAN_POINT('Ctrl Pts',(52.7936435003593,22.0662744705249,23.900471129172));
#37124=CARTESIAN_POINT('Ctrl Pts',(52.8290477928857,22.139533742026,23.8962549697194));
#37125=CARTESIAN_POINT('Ctrl Pts',(52.8681178363983,22.2110549320226,23.8920388102668));
#37126=CARTESIAN_POINT('Ctrl Pts',(52.9106496944755,22.2804552123385,23.8878226508143));
#37127=CARTESIAN_POINT('Ctrl Pts',(52.953180539105,22.3498538389867,23.8836065918242));
#37128=CARTESIAN_POINT('Ctrl Pts',(52.9991727904118,22.4171312606115,23.8793905328341));
#37129=CARTESIAN_POINT('Ctrl Pts',(53.0483780804816,22.4819318922459,23.8751744738441));
#37130=CARTESIAN_POINT('Ctrl Pts',(53.097986147337,22.5472629585158,23.8709239037134));
#37131=CARTESIAN_POINT('Ctrl Pts',(53.1508598199829,22.610076107651,23.8666733335826));
#37132=CARTESIAN_POINT('Ctrl Pts',(53.206703034202,22.6700407906574,23.8624227634519));
#37133=CARTESIAN_POINT('Ctrl Pts',(53.2621733784582,22.729605084298,23.858200574745));
#37134=CARTESIAN_POINT('Ctrl Pts',(53.3205733494969,22.7863585519973,23.853978386038));
#37135=CARTESIAN_POINT('Ctrl Pts',(53.3815769138414,22.8400154793341,23.849756197331));
#37136=CARTESIAN_POINT('Ctrl Pts',(53.4431955743353,22.8942134270152,23.8454914364884));
#37137=CARTESIAN_POINT('Ctrl Pts',(53.5074702470363,22.9452517362166,23.8412266756458));
#37138=CARTESIAN_POINT('Ctrl Pts',(53.5740336697725,22.9928798947898,23.8369619148032));
#37139=CARTESIAN_POINT('Ctrl Pts',(53.6405970925086,23.040508053363,23.8326971539606));
#37140=CARTESIAN_POINT('Ctrl Pts',(53.7094488251654,23.0847258550163,23.828432393118));
#37141=CARTESIAN_POINT('Ctrl Pts',(53.780196531644,23.1253305033775,23.8241676322754));
#37142=CARTESIAN_POINT('Ctrl Pts',(53.8503878373329,23.1656158133524,23.8199364119731));
#37143=CARTESIAN_POINT('Ctrl Pts',(53.9227085879526,23.2024957039034,23.8157051916708));
#37144=CARTESIAN_POINT('Ctrl Pts',(53.9967946214461,23.2357390765562,23.8114739713685));
#37145=CARTESIAN_POINT('Ctrl Pts',(54.0707744207519,23.268934780539,23.8072488183401));
#37146=CARTESIAN_POINT('Ctrl Pts',(54.1465140549981,23.2985041343083,23.8030236653116));
#37147=CARTESIAN_POINT('Ctrl Pts',(54.2236233520432,23.3242610762364,23.7987985122832));
#37148=CARTESIAN_POINT('Ctrl Pts',(54.3009307398298,23.3500841867319,23.7945625050033));
#37149=CARTESIAN_POINT('Ctrl Pts',(54.3796144240673,23.3720750430543,23.7903264977234));
#37150=CARTESIAN_POINT('Ctrl Pts',(54.4592594821174,23.3900941283389,23.7860904904436));
#37151=CARTESIAN_POINT('Ctrl Pts',(54.5385575453611,23.4080347087023,23.7818729384522));
#37152=CARTESIAN_POINT('Ctrl Pts',(54.6188081683935,23.4220379427811,23.7776553864609));
#37153=CARTESIAN_POINT('Ctrl Pts',(54.699586851396,23.4320160752236,23.7734378344695));
#37154=CARTESIAN_POINT('Ctrl Pts',(54.7803388631143,23.4419909131136,23.7692216750179));
#37155=CARTESIAN_POINT('Ctrl Pts',(54.8616181275089,23.4479432316177,23.7650055155664));
#37156=CARTESIAN_POINT('Ctrl Pts',(54.942992400024,23.4498368075333,23.7607893561148));
#37157=CARTESIAN_POINT('Ctrl Pts',(55.0243647335545,23.4517303383288,23.7565732971258));
#37158=CARTESIAN_POINT('Ctrl Pts',(55.1058316058827,23.4495653091161,23.7523572381367));
#37159=CARTESIAN_POINT('Ctrl Pts',(55.1869595714351,23.4433576014675,23.7481411791477));
#37160=CARTESIAN_POINT('Ctrl Pts',(55.2687516213392,23.4370990797563,23.7438906090159));
#37161=CARTESIAN_POINT('Ctrl Pts',(55.350198710976,23.4267314108936,23.7396400388842));
#37162=CARTESIAN_POINT('Ctrl Pts',(55.4308625689044,23.412324127624,23.7353894687524));
#37163=CARTESIAN_POINT('Ctrl Pts',(55.5109878272474,23.3980130430362,23.7311672800466));
#37164=CARTESIAN_POINT('Ctrl Pts',(55.5903398378285,23.3797162911962,23.7269450913408));
#37165=CARTESIAN_POINT('Ctrl Pts',(55.6685017508143,23.3575528963648,23.7227229026349));
#37166=CARTESIAN_POINT('Ctrl Pts',(55.7474517668551,23.3351660290197,23.7184581417902));
#37167=CARTESIAN_POINT('Ctrl Pts',(55.8251870907016,23.308834261285,23.7141933809455));
#37168=CARTESIAN_POINT('Ctrl Pts',(55.9012980956155,23.2787303466711,23.7099286201007));
#37169=CARTESIAN_POINT('Ctrl Pts',(55.9774091005293,23.2486264320573,23.705663859256));
#37170=CARTESIAN_POINT('Ctrl Pts',(56.051895374537,23.2147506285081,23.7013990984112));
#37171=CARTESIAN_POINT('Ctrl Pts',(56.1243737877523,23.1773226300701,23.6971343375665));
#37172=CARTESIAN_POINT('Ctrl Pts',(56.1962821889435,23.1401889869885,23.6929031172596));
#37173=CARTESIAN_POINT('Ctrl Pts',(56.2664838678145,23.0994196161714,23.6886718969527));
#37174=CARTESIAN_POINT('Ctrl Pts',(56.3345871906329,23.055195192822,23.6844406766458));
#37175=CARTESIAN_POINT('Ctrl Pts',(56.4025928580535,23.0110341842,23.6802155236126));
#37176=CARTESIAN_POINT('Ctrl Pts',(56.4685057586814,22.963428213733,23.6759903705795));
#37177=CARTESIAN_POINT('Ctrl Pts',(56.5319579971,22.9126042311783,23.6717652175463));
#37178=CARTESIAN_POINT('Ctrl Pts',(56.5955732417271,22.8616496838887,23.6675292102676));
#37179=CARTESIAN_POINT('Ctrl Pts',(56.6567147488336,22.807460791746,23.6632932029889));
#37180=CARTESIAN_POINT('Ctrl Pts',(56.7150403113011,22.7503105383366,23.6590571957102));
#37181=CARTESIAN_POINT('Ctrl Pts',(56.7731117630788,22.6934092750733,23.654839643714));
#37182=CARTESIAN_POINT('Ctrl Pts',(56.8283914159485,22.6335727222424,23.6506220917178));
#37183=CARTESIAN_POINT('Ctrl Pts',(56.8805753616882,22.5711099767398,23.6464045397216));
#37184=CARTESIAN_POINT('Ctrl Pts',(56.9327420774763,22.5086678550145,23.6421883802651));
#37185=CARTESIAN_POINT('Ctrl Pts',(56.9818148181,22.4436016190868,23.6379722208086));
#37186=CARTESIAN_POINT('Ctrl Pts',(57.0275287751062,22.3762548151111,23.6337560613521));
#37187=CARTESIAN_POINT('Ctrl Pts',(57.0732416428415,22.308909615873,23.6295400023581));
#37188=CARTESIAN_POINT('Ctrl Pts',(57.1155956258926,22.2392843419275,23.6253239433641));
#37189=CARTESIAN_POINT('Ctrl Pts',(57.154369044863,22.1677518009133,23.6211078843701));
#37190=CARTESIAN_POINT('Ctrl Pts',(57.1934598489991,22.0956337204241,23.6168573142441));
#37191=CARTESIAN_POINT('Ctrl Pts',(57.2289109573716,22.0215774184445,23.612606744118));
#37192=CARTESIAN_POINT('Ctrl Pts',(57.2605431535074,21.9459888483121,23.608356173992));
#37193=CARTESIAN_POINT('Ctrl Pts',(57.2919641388019,21.870904989437,23.6041339852811));
#37194=CARTESIAN_POINT('Ctrl Pts',(57.3196169536619,21.7943097248618,23.5999117965703));
#37195=CARTESIAN_POINT('Ctrl Pts',(57.3433755813988,21.7166178441149,23.5956896078594));
#37196=CARTESIAN_POINT('Ctrl Pts',(57.3673737662201,21.6381425999246,23.5914248470258));
#37197=CARTESIAN_POINT('Ctrl Pts',(57.3873986735856,21.5585489719529,23.5871600861921));
#37198=CARTESIAN_POINT('Ctrl Pts',(57.4033733485433,21.4782748137963,23.5828953253585));
#37199=CARTESIAN_POINT('Ctrl Pts',(57.419348023501,21.3980006556397,23.5786305645248));
#37200=CARTESIAN_POINT('Ctrl Pts',(57.4312724594035,21.3170464533155,23.5743658036912));
#37201=CARTESIAN_POINT('Ctrl Pts',(57.4391235095687,21.2358532490114,23.5701010428575));
#37202=CARTESIAN_POINT('Ctrl Pts',(57.4469128145653,21.1552985947081,23.565869822553));
#37203=CARTESIAN_POINT('Ctrl Pts',(57.4507218304109,21.0742066178951,23.5616386022485));
#37204=CARTESIAN_POINT('Ctrl Pts',(57.4504900144397,20.9930043491268,23.557407381944));
#37205=CARTESIAN_POINT('Ctrl Pts',(57.4502585308765,20.9119185187286,23.5531822289132));
#37206=CARTESIAN_POINT('Ctrl Pts',(57.4459977246676,20.8307231714723,23.5489570758825));
#37207=CARTESIAN_POINT('Ctrl Pts',(57.437698806098,20.7498504832138,23.5447319228517));
#37208=CARTESIAN_POINT('Ctrl Pts',(57.4293785679397,20.6687700362652,23.5404959155724));
#37209=CARTESIAN_POINT('Ctrl Pts',(57.4169994043282,20.5880143786716,23.5362599082931));
#37210=CARTESIAN_POINT('Ctrl Pts',(57.4006051335561,20.508019062621,23.5320239010138));
#37211=CARTESIAN_POINT('Ctrl Pts',(57.3842822887586,20.4283722673126,23.5278063490201));
#37212=CARTESIAN_POINT('Ctrl Pts',(57.3639793355127,20.3494796620933,23.5235887970264));
#37213=CARTESIAN_POINT('Ctrl Pts',(57.3397912022887,20.2717642004871,23.5193712450326));
#37214=CARTESIAN_POINT('Ctrl Pts',(57.3156110554361,20.1940743987583,23.5151550855786));
#37215=CARTESIAN_POINT('Ctrl Pts',(57.2875484141183,20.1175614123755,23.5109389261246));
#37216=CARTESIAN_POINT('Ctrl Pts',(57.2557483530398,20.042634020994,23.5067227666705));
#37217=CARTESIAN_POINT('Ctrl Pts',(57.2239490496924,19.9677084149805,23.5025067076791));
#37218=CARTESIAN_POINT('Ctrl Pts',(57.188412686306,19.8943687563882,23.4982906486876));
#37219=CARTESIAN_POINT('Ctrl Pts',(57.1493323096355,19.8230034525297,23.4940745896961));
#37220=CARTESIAN_POINT('Ctrl Pts',(57.1099320351043,19.751053978047,23.4898240195671));
#37221=CARTESIAN_POINT('Ctrl Pts',(57.0669296757901,19.6811117586712,23.4855734494382));
#37222=CARTESIAN_POINT('Ctrl Pts',(57.0205691529617,19.6135474951879,23.4813228793092));
#37223=CARTESIAN_POINT('Ctrl Pts',(56.9745181833128,19.5464343640756,23.4771006906009));
#37224=CARTESIAN_POINT('Ctrl Pts',(56.9251540928421,19.4816678658699,23.4728785018925));
#37225=CARTESIAN_POINT('Ctrl Pts',(56.8727570733825,19.4195787921899,23.4686563131842));
#37226=CARTESIAN_POINT('Ctrl Pts',(56.8198317372307,19.3568636772891,23.4643915523449));
#37227=CARTESIAN_POINT('Ctrl Pts',(56.7638122976572,19.2968806385461,23.4601267915056));
#37228=CARTESIAN_POINT('Ctrl Pts',(56.7050249280874,19.2399317500163,23.4558620306664));
#37229=CARTESIAN_POINT('Ctrl Pts',(56.6462375585176,19.1829828614865,23.4515972698271));
#37230=CARTESIAN_POINT('Ctrl Pts',(56.5846826637161,19.1290683922845,23.4473325089878));
#37231=CARTESIAN_POINT('Ctrl Pts',(56.5207182722946,19.0784469337775,23.4430677481486));
#37232=CARTESIAN_POINT('Ctrl Pts',(56.457256933674,19.0282235915648,23.4388365278439));
#37233=CARTESIAN_POINT('Ctrl Pts',(56.3911859179795,18.9810532810875,23.4346053075393));
#37234=CARTESIAN_POINT('Ctrl Pts',(56.3228312038322,18.9372184177262,23.4303740872346));
#37235=CARTESIAN_POINT('Ctrl Pts',(56.2545745055609,18.8934464104911,23.4261489342038));
#37236=CARTESIAN_POINT('Ctrl Pts',(56.1840410006248,18.8530006002341,23.4219237811729));
#37237=CARTESIAN_POINT('Ctrl Pts',(56.1115890524893,18.8161227075713,23.417698628142));
#37238=CARTESIAN_POINT('Ctrl Pts',(56.0389509782095,18.7791500770836,23.4134626208628));
#37239=CARTESIAN_POINT('Ctrl Pts',(55.9643849654187,18.7457640072126,23.4092266135835));
#37240=CARTESIAN_POINT('Ctrl Pts',(55.8882807397064,18.7161638461863,23.4049906063042));
#37241=CARTESIAN_POINT('Ctrl Pts',(55.8125080821701,18.6866926460857,23.4007730543104));
#37242=CARTESIAN_POINT('Ctrl Pts',(55.7352110201091,18.6609746122216,23.3965555023165));
#37243=CARTESIAN_POINT('Ctrl Pts',(55.6567964063242,18.6391593169721,23.3923379503227));
#37244=CARTESIAN_POINT('Ctrl Pts',(55.578407683261,18.6173512246369,23.3881217908686));
#37245=CARTESIAN_POINT('Ctrl Pts',(55.4989025887961,18.5994434364596,23.3839056314144));
#37246=CARTESIAN_POINT('Ctrl Pts',(55.4187032567279,18.585535704798,23.3796894719603));
#37247=CARTESIAN_POINT('Ctrl Pts',(55.3385058356473,18.5716283045294,23.3754734129687));
#37248=CARTESIAN_POINT('Ctrl Pts',(55.2576146681281,18.5617208496152,23.3712573539772));
#37249=CARTESIAN_POINT('Ctrl Pts',(55.1764607818987,18.5558617382702,23.3670412949856));
#37250=CARTESIAN_POINT('Ctrl Pts',(55.0946425992463,18.5499546663543,23.3627907248567));
#37251=CARTESIAN_POINT('Ctrl Pts',(55.0125578543063,18.5481625710354,23.3585401547279));
#37252=CARTESIAN_POINT('Ctrl Pts',(54.9306502824293,18.5504815030964,23.3542895845991));
#37253=CARTESIAN_POINT('Ctrl Pts',(54.8492896144173,18.5527849514497,23.3500673958906));
#37254=CARTESIAN_POINT('Ctrl Pts',(54.7681042239192,18.5591445967131,23.3458452071822));
#37255=CARTESIAN_POINT('Ctrl Pts',(54.6875239798841,18.5695043742371,23.3416230184738));
#37256=CARTESIAN_POINT('Ctrl Pts',(54.6061312490298,18.5799686089118,23.3373582576347));
#37257=CARTESIAN_POINT('Ctrl Pts',(54.5253564147595,18.5945140100771,23.3330934967957));
#37258=CARTESIAN_POINT('Ctrl Pts',(54.4456301487333,18.6130303064332,23.3288287359566));
#37259=CARTESIAN_POINT('Ctrl Pts',(54.3659038827071,18.6315466027892,23.3245639751176));
#37260=CARTESIAN_POINT('Ctrl Pts',(54.2872266305167,18.6540336001583,23.3202992142786));
#37261=CARTESIAN_POINT('Ctrl Pts',(54.2100098007072,18.680330684123,23.3160344534395));
#37262=CARTESIAN_POINT('Ctrl Pts',(54.13340024849,18.7064209526839,23.3118032331343));
#37263=CARTESIAN_POINT('Ctrl Pts',(54.0579409376308,18.7363593847075,23.3075720128291));
#37264=CARTESIAN_POINT('Ctrl Pts',(53.984045916249,18.7700252132121,23.3033407925239));
#37265=CARTESIAN_POINT('Ctrl Pts',(53.9102568551558,18.803642767275,23.2991156394925));
#37266=CARTESIAN_POINT('Ctrl Pts',(53.8380280481248,18.8409769114683,23.2948904864611));
#37267=CARTESIAN_POINT('Ctrl Pts',(53.7677569098642,18.8818576023287,23.2906653334296));
#37268=CARTESIAN_POINT('Ctrl Pts',(53.6973052478841,18.9228433140349,23.2864293261505));
#37269=CARTESIAN_POINT('Ctrl Pts',(53.6288217706353,18.9673936593575,23.2821933188714));
#37270=CARTESIAN_POINT('Ctrl Pts',(53.5626852952752,19.0152892680338,23.2779573115923));
#37271=CARTESIAN_POINT('Ctrl Pts',(53.4968369609406,19.0629762068387,23.2737397595978));
#37272=CARTESIAN_POINT('Ctrl Pts',(53.433315604212,19.1139790529377,23.2695222076034));
#37273=CARTESIAN_POINT('Ctrl Pts',(53.3724675055654,19.168037055626,23.2653046556089));
#37274=CARTESIAN_POINT('Ctrl Pts',(53.3116394975768,19.2220772095916,23.2610884961542));
#37275=CARTESIAN_POINT('Ctrl Pts',(53.2534833421499,19.2791702083826,23.2568723366995));
#37276=CARTESIAN_POINT('Ctrl Pts',(53.1983117449078,19.3390154481564,23.2526561772448));
#37277=CARTESIAN_POINT('Ctrl Pts',(53.1431414622932,19.3988592619394,23.2484401182526));
#37278=CARTESIAN_POINT('Ctrl Pts',(53.0909559107819,19.4614548437374,23.2442240592604));
#37279=CARTESIAN_POINT('Ctrl Pts',(53.0420294689127,19.5264662713756,23.2400080002683));
#37280=CARTESIAN_POINT('Ctrl Pts',(52.9927025328638,19.5920098590766,23.2357574301401));
#37281=CARTESIAN_POINT('Ctrl Pts',(52.9466886098102,19.6600086520088,23.231506860012));
#37282=CARTESIAN_POINT('Ctrl Pts',(52.9042249844769,19.7300876666836,23.2272562898838));
#37283=CARTESIAN_POINT('Ctrl Pts',(52.8620448923899,19.7996987578032,23.2230341011748));
#37284=CARTESIAN_POINT('Ctrl Pts',(52.8233679997169,19.8713619330961,23.2188119124658));
#37285=CARTESIAN_POINT('Ctrl Pts',(52.7883802832879,19.9446856019886,23.2145897237567));
#37286=CARTESIAN_POINT('Ctrl Pts',(52.7530397873723,20.0187485899594,23.210324962919));
#37287=CARTESIAN_POINT('Ctrl Pts',(52.7214634689174,20.0945052969547,23.2060602020813));
#37288=CARTESIAN_POINT('Ctrl Pts',(52.6937921936552,20.171534065906,23.2017954412436));
#37289=CARTESIAN_POINT('Ctrl Pts',(52.666120918393,20.2485628348572,23.197530680406));
#37290=CARTESIAN_POINT('Ctrl Pts',(52.6423547647779,20.3268631860749,23.1932659195683));
#37291=CARTESIAN_POINT('Ctrl Pts',(52.6225818535924,20.4060023509036,23.1890011587306));
#37292=CARTESIAN_POINT('Ctrl Pts',(52.596985294238,20.5084501043372,23.1834803124126));
#37293=CARTESIAN_POINT('Ctrl Pts',(52.5780003177254,20.6126109162437,23.1779594660946));
#37294=CARTESIAN_POINT('Ctrl Pts',(52.5658093151964,20.7177484100749,23.1724386197766));
#37295=CARTESIAN_POINT('Ctrl Pts',(52.5550546758219,20.8104984384828,23.1675682482834));
#37296=CARTESIAN_POINT('Ctrl Pts',(52.5495868147034,20.9040085164618,23.1626978767901));
#37297=CARTESIAN_POINT('Ctrl Pts',(52.5495010260079,20.9977575763378,23.1578275052968));
#37298=CARTESIAN_POINT('',(52.549839723371,21.0005724374191,22.3578274699494));
#37299=CARTESIAN_POINT('Ctrl Pts',(52.5497869278457,20.9977580128137,23.1578274962121));
#37300=CARTESIAN_POINT('Ctrl Pts',(52.5553781978731,21.6127545089065,23.1258742854819));
#37301=CARTESIAN_POINT('Ctrl Pts',(53.1016016749266,23.0515966978432,23.051576643182));
#37302=CARTESIAN_POINT('Ctrl Pts',(55.5179968719808,23.8498389112592,22.9349345693128));
#37303=CARTESIAN_POINT('Ctrl Pts',(57.6754046717511,22.1100055954292,22.8079012746036));
#37304=CARTESIAN_POINT('Ctrl Pts',(57.3833287996288,19.3538996347802,22.6808679798947));
#37305=CARTESIAN_POINT('Ctrl Pts',(54.9091811680088,18.1048912767784,22.5538346851856));
#37306=CARTESIAN_POINT('Ctrl Pts',(52.8824444977937,19.2929844814695,22.4461545239581));
#37307=CARTESIAN_POINT('Ctrl Pts',(52.554303994583,20.5564224075133,22.3808187943003));
#37308=CARTESIAN_POINT('Ctrl Pts',(52.5533783220755,21.0005711032702,22.3578274962121));
#37309=CARTESIAN_POINT('',(52.5495007750096,21.0019489283386,21.5578274962564));
#37310=CARTESIAN_POINT('Ctrl Pts',(52.5495000668907,21.000572565479,22.3578274674285));
#37311=CARTESIAN_POINT('Ctrl Pts',(52.5495204243597,21.0876996773897,22.3533244795148));
#37312=CARTESIAN_POINT('Ctrl Pts',(52.5541917027174,21.1747038922701,22.348821491601));
#37313=CARTESIAN_POINT('Ctrl Pts',(52.5634494157742,21.2610967263463,22.3443185036873));
#37314=CARTESIAN_POINT('Ctrl Pts',(52.5727418499892,21.3478135777309,22.3397986272661));
#37315=CARTESIAN_POINT('Ctrl Pts',(52.5866550846643,21.4339141026509,22.3352787508448));
#37316=CARTESIAN_POINT('Ctrl Pts',(52.6050731906035,21.5189179392099,22.3307588744236));
#37317=CARTESIAN_POINT('Ctrl Pts',(52.6235282272307,21.6040922194711,22.3262299350648));
#37318=CARTESIAN_POINT('Ctrl Pts',(52.6465060677051,21.6881650763028,22.3217009957059));
#37319=CARTESIAN_POINT('Ctrl Pts',(52.6738411873686,21.7706720628239,22.3171720563471));
#37320=CARTESIAN_POINT('Ctrl Pts',(52.70125775696,21.8534248938186,22.3126296221951));
#37321=CARTESIAN_POINT('Ctrl Pts',(52.7330574340931,21.9346021901369,22.3080871880432));
#37322=CARTESIAN_POINT('Ctrl Pts',(52.7690265296219,22.0137591550605,22.3035447538912));
#37323=CARTESIAN_POINT('Ctrl Pts',(52.7789949718184,22.0356966438323,22.30228586785));
#37324=CARTESIAN_POINT('Ctrl Pts',(52.7892833845875,22.0574791148083,22.3010269818088));
#37325=CARTESIAN_POINT('Ctrl Pts',(52.7998866174955,22.0790974720222,22.2997680957676));
#37326=CARTESIAN_POINT('Ctrl Pts',(52.8355249619605,22.1517585620726,22.2955368754627));
#37327=CARTESIAN_POINT('Ctrl Pts',(52.8748335582081,22.2227884963781,22.2913056551578));
#37328=CARTESIAN_POINT('Ctrl Pts',(52.9176398702462,22.2917919879035,22.2870744348529));
#37329=CARTESIAN_POINT('Ctrl Pts',(52.9603848010288,22.3606965332516,22.2828492818218));
#37330=CARTESIAN_POINT('Ctrl Pts',(53.0066172434651,22.4275800151676,22.2786241287906));
#37331=CARTESIAN_POINT('Ctrl Pts',(53.0561179059046,22.4920699227099,22.2743989757595));
#37332=CARTESIAN_POINT('Ctrl Pts',(53.1057457335535,22.5567255022287,22.2701629684803));
#37333=CARTESIAN_POINT('Ctrl Pts',(53.1586583809308,22.618974772684,22.2659269612011));
#37334=CARTESIAN_POINT('Ctrl Pts',(53.214590001068,22.6784699537715,22.2616909539219));
#37335=CARTESIAN_POINT('Ctrl Pts',(53.2702779403224,22.7377059283811,22.2574734019278));
#37336=CARTESIAN_POINT('Ctrl Pts',(53.3289582867809,22.7942114149242,22.2532558499336));
#37337=CARTESIAN_POINT('Ctrl Pts',(53.3903282957173,22.8476761768318,22.2490382979395));
#37338=CARTESIAN_POINT('Ctrl Pts',(53.4516780416729,22.9011232858912,22.2448221384851));
#37339=CARTESIAN_POINT('Ctrl Pts',(53.5157153362577,22.951531358919,22.2406059790307));
#37340=CARTESIAN_POINT('Ctrl Pts',(53.5821021841165,22.9986285382013,22.2363898195762));
#37341=CARTESIAN_POINT('Ctrl Pts',(53.6484874501112,23.0457245952533,22.2321737605844));
#37342=CARTESIAN_POINT('Ctrl Pts',(53.7172217782354,23.0895096473104,22.2279577015925));
#37343=CARTESIAN_POINT('Ctrl Pts',(53.7879370258276,23.1297543512434,22.2237416426006));
#37344=CARTESIAN_POINT('Ctrl Pts',(53.8592311229034,23.1703284837917,22.2194910724721));
#37345=CARTESIAN_POINT('Ctrl Pts',(53.9325383103316,23.2073037894376,22.2152405023437));
#37346=CARTESIAN_POINT('Ctrl Pts',(54.007456428538,23.2404926933042,22.2109899322152));
#37347=CARTESIAN_POINT('Ctrl Pts',(54.0818743120709,23.2734599920252,22.2067677435064));
#37348=CARTESIAN_POINT('Ctrl Pts',(54.1578812188451,23.3026911884024,22.2025455547977));
#37349=CARTESIAN_POINT('Ctrl Pts',(54.2350650546021,23.3280517131948,22.198323366089));
#37350=CARTESIAN_POINT('Ctrl Pts',(54.313027131335,23.3536679469626,22.1940586052506));
#37351=CARTESIAN_POINT('Ctrl Pts',(54.3921895359128,23.3753348859622,22.1897938444122));
#37352=CARTESIAN_POINT('Ctrl Pts',(54.4721161001478,23.3929665351352,22.1855290835739));
#37353=CARTESIAN_POINT('Ctrl Pts',(54.5520426643828,23.4105981843081,22.1812643227355));
#37354=CARTESIAN_POINT('Ctrl Pts',(54.632732902499,23.4241945269557,22.1769995618971));
#37355=CARTESIAN_POINT('Ctrl Pts',(54.7137463454286,23.4337232988252,22.1727348010588));
#37356=CARTESIAN_POINT('Ctrl Pts',(54.794122652023,23.4431771309493,22.1685035807538));
#37357=CARTESIAN_POINT('Ctrl Pts',(54.875118494528,23.4486626394389,22.1642723604489));
#37358=CARTESIAN_POINT('Ctrl Pts',(54.9563081860119,23.4501104618752,22.160041140144));
#37359=CARTESIAN_POINT('Ctrl Pts',(55.0373814571608,23.4515562082355,22.1558159871128));
#37360=CARTESIAN_POINT('Ctrl Pts',(55.1186475643015,23.448975759219,22.1515908340817));
#37361=CARTESIAN_POINT('Ctrl Pts',(55.1996746058428,23.44235138786,22.1473656810505));
#37362=CARTESIAN_POINT('Ctrl Pts',(55.2809098025917,23.4357099987576,22.1431296737713));
#37363=CARTESIAN_POINT('Ctrl Pts',(55.3619042343381,23.4250038346097,22.1388936664921));
#37364=CARTESIAN_POINT('Ctrl Pts',(55.4422215357371,23.4102676953671,22.1346576592129));
#37365=CARTESIAN_POINT('Ctrl Pts',(55.5221889135895,23.395595758009,22.1304401072187));
#37366=CARTESIAN_POINT('Ctrl Pts',(55.6014845873182,23.3769289640167,22.1262225552246));
#37367=CARTESIAN_POINT('Ctrl Pts',(55.6796837303828,23.3543534731754,22.1220050032304));
#37368=CARTESIAN_POINT('Ctrl Pts',(55.7578570538693,23.3317854362476,22.1177888437759));
#37369=CARTESIAN_POINT('Ctrl Pts',(55.8349341193415,23.3053113941992,22.1135726843215));
#37370=CARTESIAN_POINT('Ctrl Pts',(55.9105032338699,23.2750679354939,22.1093565248671));
#37371=CARTESIAN_POINT('Ctrl Pts',(55.9860705477393,23.244825197429,22.1051404658751));
#37372=CARTESIAN_POINT('Ctrl Pts',(56.0601295508799,23.2108133950625,22.1009244068832));
#37373=CARTESIAN_POINT('Ctrl Pts',(56.1322879260922,23.1732175000275,22.0967083478913));
#37374=CARTESIAN_POINT('Ctrl Pts',(56.2050369637089,23.1353138585709,22.0924577777629));
#37375=CARTESIAN_POINT('Ctrl Pts',(56.2758536812153,23.0937673848603,22.0882072076344));
#37376=CARTESIAN_POINT('Ctrl Pts',(56.3443624118618,23.0488142804006,22.0839566375059));
#37377=CARTESIAN_POINT('Ctrl Pts',(56.4124137038637,23.0041613316578,22.0797344487972));
#37378=CARTESIAN_POINT('Ctrl Pts',(56.4781873936258,22.9561474331056,22.0755122600884));
#37379=CARTESIAN_POINT('Ctrl Pts',(56.5413469648059,22.9050458745352,22.0712900713796));
#37380=CARTESIAN_POINT('Ctrl Pts',(56.6051433709626,22.8534290613605,22.0670253105413));
#37381=CARTESIAN_POINT('Ctrl Pts',(56.6662722839316,22.7986622964092,22.062760549703));
#37382=CARTESIAN_POINT('Ctrl Pts',(56.7244249477072,22.741065435222,22.0584957888647));
#37383=CARTESIAN_POINT('Ctrl Pts',(56.7825776114828,22.6834685740348,22.0542310280263));
#37384=CARTESIAN_POINT('Ctrl Pts',(56.8377537486358,22.6230420157234,22.049966267188));
#37385=CARTESIAN_POINT('Ctrl Pts',(56.8896874176529,22.5601383635962,22.0457015063497));
#37386=CARTESIAN_POINT('Ctrl Pts',(56.9412126504114,22.4977294219872,22.0414702860448));
#37387=CARTESIAN_POINT('Ctrl Pts',(56.9897394831863,22.4326482126616,22.0372390657398));
#37388=CARTESIAN_POINT('Ctrl Pts',(57.0349788184697,22.365214803018,22.0330078454349));
#37389=CARTESIAN_POINT('Ctrl Pts',(57.0801532837126,22.2978780881643,22.0287826924038));
#37390=CARTESIAN_POINT('Ctrl Pts',(57.1220493570732,22.228196254636,22.0245575393726));
#37391=CARTESIAN_POINT('Ctrl Pts',(57.1604179572537,22.1565225894793,22.0203323863415));
#37392=CARTESIAN_POINT('Ctrl Pts',(57.1988851248234,22.0846647975622,22.0160963790623));
#37393=CARTESIAN_POINT('Ctrl Pts',(57.2338063765807,22.0108052951242,22.0118603717831));
#37394=CARTESIAN_POINT('Ctrl Pts',(57.2649743458564,21.9353296010564,22.0076243645039));
#37395=CARTESIAN_POINT('Ctrl Pts',(57.2960065236381,21.8601827367937,22.0034068125097));
#37396=CARTESIAN_POINT('Ctrl Pts',(57.3233178689278,21.7834341635921,21.9991892605156));
#37397=CARTESIAN_POINT('Ctrl Pts',(57.3467504259977,21.7054875534548,21.9949717085214));
#37398=CARTESIAN_POINT('Ctrl Pts',(57.3701752461703,21.627566679515,21.990755549067));
#37399=CARTESIAN_POINT('Ctrl Pts',(57.389723687645,21.5484489990632,21.9865393896125));
#37400=CARTESIAN_POINT('Ctrl Pts',(57.4052872879839,21.4685544923089,21.9823232301581));
#37401=CARTESIAN_POINT('Ctrl Pts',(57.4208505174738,21.3886618892788,21.9781071711662));
#37402=CARTESIAN_POINT('Ctrl Pts',(57.432429006806,21.3079929533049,21.9738911121743));
#37403=CARTESIAN_POINT('Ctrl Pts',(57.4399654527367,21.2269776188338,21.9696750531824));
#37404=CARTESIAN_POINT('Ctrl Pts',(57.4475635892925,21.1452991220876,21.9654244830539));
#37405=CARTESIAN_POINT('Ctrl Pts',(57.4510531431762,21.0632690058505,21.9611739129255));
#37406=CARTESIAN_POINT('Ctrl Pts',(57.450428884532,20.9813309922273,21.956923342797));
#37407=CARTESIAN_POINT('Ctrl Pts',(57.4498087941161,20.899940085718,21.9527011540882));
#37408=CARTESIAN_POINT('Ctrl Pts',(57.445129749118,20.8186405207931,21.9484789653795));
#37409=CARTESIAN_POINT('Ctrl Pts',(57.4364389107779,20.737863234079,21.9442567766707));
#37410=CARTESIAN_POINT('Ctrl Pts',(57.4276604431248,20.6562714737934,21.9399920158324));
#37411=CARTESIAN_POINT('Ctrl Pts',(57.4147889015141,20.5752130629985,21.9357272549941));
#37412=CARTESIAN_POINT('Ctrl Pts',(57.3979256256363,20.4951208620703,21.9314624941558));
#37413=CARTESIAN_POINT('Ctrl Pts',(57.3810623497585,20.4150286611421,21.9271977333174));
#37414=CARTESIAN_POINT('Ctrl Pts',(57.3602075245332,20.3359031195936,21.9229329724791));
#37415=CARTESIAN_POINT('Ctrl Pts',(57.3355132204363,20.2581588801048,21.9186682116408));
#37416=CARTESIAN_POINT('Ctrl Pts',(57.3110131265572,20.1810260660535,21.9144369913358));
#37417=CARTESIAN_POINT('Ctrl Pts',(57.2826419008733,20.1049636518159,21.9102057710309));
#37418=CARTESIAN_POINT('Ctrl Pts',(57.2505117203525,20.0303880948772,21.905974550726));
#37419=CARTESIAN_POINT('Ctrl Pts',(57.2184276122618,19.9559194740675,21.9017493976948));
#37420=CARTESIAN_POINT('Ctrl Pts',(57.1825954368418,19.8829338995233,21.8975242446637));
#37421=CARTESIAN_POINT('Ctrl Pts',(57.1431769810457,19.8118322181124,21.8932990916325));
#37422=CARTESIAN_POINT('Ctrl Pts',(57.1036572608236,19.7405478793442,21.8890630843533));
#37423=CARTESIAN_POINT('Ctrl Pts',(57.0605329596327,19.6711575733102,21.8848270770741));
#37424=CARTESIAN_POINT('Ctrl Pts',(57.0140155653455,19.6040445735819,21.8805910697949));
#37425=CARTESIAN_POINT('Ctrl Pts',(56.9677008363784,19.5372239693712,21.8763735178008));
#37426=CARTESIAN_POINT('Ctrl Pts',(56.9180227782772,19.4726612586684,21.8721559658066));
#37427=CARTESIAN_POINT('Ctrl Pts',(56.8652349234924,19.4107080412384,21.8679384138125));
#37428=CARTESIAN_POINT('Ctrl Pts',(56.8124644980563,19.3487752793513,21.863722254358));
#37429=CARTESIAN_POINT('Ctrl Pts',(56.7565866162777,19.2894506533341,21.8595060949036));
#37430=CARTESIAN_POINT('Ctrl Pts',(56.6978953496814,19.2330530196041,21.8552899354492));
#37431=CARTESIAN_POINT('Ctrl Pts',(56.6392054815791,19.1766567297154,21.8510738764573));
#37432=CARTESIAN_POINT('Ctrl Pts',(56.5777026979492,19.1231876147786,21.8468578174654));
#37433=CARTESIAN_POINT('Ctrl Pts',(56.5137171738508,19.0729269428512,21.8426417584735));
#37434=CARTESIAN_POINT('Ctrl Pts',(56.4492078873559,19.0222548552113,21.838391188345));
#37435=CARTESIAN_POINT('Ctrl Pts',(56.3821753944835,18.9748442882929,21.8341406182165));
#37436=CARTESIAN_POINT('Ctrl Pts',(56.3129896904991,18.9309402322207,21.8298900480881));
#37437=CARTESIAN_POINT('Ctrl Pts',(56.2442659453685,18.8873293272801,21.8256678593793));
#37438=CARTESIAN_POINT('Ctrl Pts',(56.1734180948581,18.8471784269523,21.8214456706706));
#37439=CARTESIAN_POINT('Ctrl Pts',(56.1008337990187,18.8106815679445,21.8172234819618));
#37440=CARTESIAN_POINT('Ctrl Pts',(56.0275176391479,18.7738167128287,21.8129587211235));
#37441=CARTESIAN_POINT('Ctrl Pts',(55.9524302643044,18.7406801969708,21.8086939602851));
#37442=CARTESIAN_POINT('Ctrl Pts',(55.8759903276802,18.7114215775266,21.8044291994468));
#37443=CARTESIAN_POINT('Ctrl Pts',(55.7995503910559,18.6821629580824,21.8001644386084));
#37444=CARTESIAN_POINT('Ctrl Pts',(55.7217583706149,18.6567823234117,21.7958996777701));
#37445=CARTESIAN_POINT('Ctrl Pts',(55.6430451197363,18.6353767268372,21.7916349169317));
#37446=CARTESIAN_POINT('Ctrl Pts',(55.5649509151586,18.6141394761921,21.7874036966268));
#37447=CARTESIAN_POINT('Ctrl Pts',(55.4856570861675,18.5967352815704,21.7831724763219));
#37448=CARTESIAN_POINT('Ctrl Pts',(55.4055743798745,18.5832957002584,21.7789412560169));
#37449=CARTESIAN_POINT('Ctrl Pts',(55.3256065065773,18.5698753903654,21.7747161029858));
#37450=CARTESIAN_POINT('Ctrl Pts',(55.2448524572574,18.5604084792876,21.7704909499546));
#37451=CARTESIAN_POINT('Ctrl Pts',(55.1637367620508,18.5549763758292,21.7662657969234));
#37452=CARTESIAN_POINT('Ctrl Pts',(55.0824126838889,18.5495303175158,21.7620297896442));
#37453=CARTESIAN_POINT('Ctrl Pts',(55.0007255565105,18.54813994154,21.757793782365));
#37454=CARTESIAN_POINT('Ctrl Pts',(54.9191120932702,18.5508353676111,21.7535577750859));
#37455=CARTESIAN_POINT('Ctrl Pts',(54.837854200648,18.5535190503462,21.7493402230917));
#37456=CARTESIAN_POINT('Ctrl Pts',(54.7566697995148,18.5602530003514,21.7451226710975));
#37457=CARTESIAN_POINT('Ctrl Pts',(54.6759917872605,18.5710148357643,21.7409051191034));
#37458=CARTESIAN_POINT('Ctrl Pts',(54.5953404130505,18.5817731178639,21.7366889596489));
#37459=CARTESIAN_POINT('Ctrl Pts',(54.5151955561655,18.5965565829204,21.7324728001945));
#37460=CARTESIAN_POINT('Ctrl Pts',(54.4359845830484,18.6152910325491,21.72825664074));
#37461=CARTESIAN_POINT('Ctrl Pts',(54.3567754973683,18.6340250357738,21.7240405817481));
#37462=CARTESIAN_POINT('Ctrl Pts',(54.2785007033965,18.6567097283014,21.7198245227562));
#37463=CARTESIAN_POINT('Ctrl Pts',(54.2015755606311,18.6832201950512,21.7156084637643));
#37464=CARTESIAN_POINT('Ctrl Pts',(54.1240207364234,18.7099476669094,21.7113578936359));
#37465=CARTESIAN_POINT('Ctrl Pts',(54.0478382196937,18.7405636937724,21.7071073235074));
#37466=CARTESIAN_POINT('Ctrl Pts',(53.9734344793227,18.7748902315264,21.7028567533789));
#37467=CARTESIAN_POINT('Ctrl Pts',(53.8995275390797,18.8089875680566,21.6986345646702));
#37468=CARTESIAN_POINT('Ctrl Pts',(53.8273760807769,18.8467457431168,21.6944123759614));
#37469=CARTESIAN_POINT('Ctrl Pts',(53.7573533386638,18.88794424196,21.6901901872527));
#37470=CARTESIAN_POINT('Ctrl Pts',(53.6866245605454,18.9295581433234,21.6859254264143));
#37471=CARTESIAN_POINT('Ctrl Pts',(53.6180680735121,18.9746818691188,21.681660665576));
#37472=CARTESIAN_POINT('Ctrl Pts',(53.5520365436791,19.0230447452814,21.6773959047377));
#37473=CARTESIAN_POINT('Ctrl Pts',(53.4860050138461,19.0714076214441,21.6731311438994));
#37474=CARTESIAN_POINT('Ctrl Pts',(53.422498774619,19.1230092942825,21.6688663830611));
#37475=CARTESIAN_POINT('Ctrl Pts',(53.3618329917431,19.1775403699784,21.6646016222228));
#37476=CARTESIAN_POINT('Ctrl Pts',(53.3025376716798,19.2308395682001,21.660433203933));
#37477=CARTESIAN_POINT('Ctrl Pts',(53.2457192209134,19.2871501507394,21.6562647856433));
#37478=CARTESIAN_POINT('Ctrl Pts',(53.1917061066508,19.346209370786,21.6520963673536));
#37479=CARTESIAN_POINT('Ctrl Pts',(53.1377834356288,19.4051696980486,21.6479349289476));
#37480=CARTESIAN_POINT('Ctrl Pts',(53.0866570900373,19.4668691686288,21.6437734905416));
#37481=CARTESIAN_POINT('Ctrl Pts',(53.0386211593529,19.5310060267442,21.6396120521356));
#37482=CARTESIAN_POINT('Ctrl Pts',(52.9906304144984,19.5950825534136,21.6354545282587));
#37483=CARTESIAN_POINT('Ctrl Pts',(52.9457246053439,19.6615915387263,21.6312970043818));
#37484=CARTESIAN_POINT('Ctrl Pts',(52.9041589788881,19.7301966041057,21.6271394805048));
#37485=CARTESIAN_POINT('Ctrl Pts',(52.862618829397,19.7987596191427,21.6229845049136));
#37486=CARTESIAN_POINT('Ctrl Pts',(52.8244150485781,19.8694157556614,21.6188295293223));
#37487=CARTESIAN_POINT('Ctrl Pts',(52.789759837469,19.9417993224653,21.614674553731));
#37488=CARTESIAN_POINT('Ctrl Pts',(52.7551145136851,20.0141622378334,21.6105207635775));
#37489=CARTESIAN_POINT('Ctrl Pts',(52.7240159556443,20.0882511718659,21.6063669734239));
#37490=CARTESIAN_POINT('Ctrl Pts',(52.6966298602075,20.1636769469204,21.6022131832704));
#37491=CARTESIAN_POINT('Ctrl Pts',(52.6692293987635,20.2391422883029,21.5980572141505));
#37492=CARTESIAN_POINT('Ctrl Pts',(52.6455454572763,20.3159454208665,21.5939012450306));
#37493=CARTESIAN_POINT('Ctrl Pts',(52.6256947355255,20.393679324871,21.5897452759108));
#37494=CARTESIAN_POINT('Ctrl Pts',(52.6058384923861,20.4714348502102,21.5855881508269));
#37495=CARTESIAN_POINT('Ctrl Pts',(52.5898176915594,20.55012119254,21.5814310257429));
#37496=CARTESIAN_POINT('Ctrl Pts',(52.577697972034,20.6293207109754,21.577273900659));
#37497=CARTESIAN_POINT('Ctrl Pts',(52.565562925504,20.7086203877836,21.573111518335));
#37498=CARTESIAN_POINT('Ctrl Pts',(52.5573388603024,20.7884340588284,21.5689491360109));
#37499=CARTESIAN_POINT('Ctrl Pts',(52.5530394926665,20.8683393545888,21.5647867536869));
#37500=CARTESIAN_POINT('Ctrl Pts',(52.5506433964058,20.9128716664535,21.5624670012101));
#37501=CARTESIAN_POINT('Ctrl Pts',(52.5494653701911,20.9574324221442,21.5601472487332));
#37502=CARTESIAN_POINT('Ctrl Pts',(52.5495007750096,21.0019489283386,21.5578274962564));
#37503=CARTESIAN_POINT('',(52.5495006451703,20.9982218044437,20.7578274962121));
#37504=CARTESIAN_POINT('Ctrl Pts',(52.5495007750103,21.0019489291882,21.5578274962121));
#37505=CARTESIAN_POINT('Ctrl Pts',(52.549603842401,21.1315414062361,21.5510744399793));
#37506=CARTESIAN_POINT('Ctrl Pts',(52.5599894688701,21.2607346644996,21.5443213837466));
#37507=CARTESIAN_POINT('Ctrl Pts',(52.5804550312434,21.3882684563092,21.5375683275139));
#37508=CARTESIAN_POINT('Ctrl Pts',(52.5932780109556,21.4681765084389,21.5333371072089));
#37509=CARTESIAN_POINT('Ctrl Pts',(52.6100878594765,21.5475984594314,21.5291058869039));
#37510=CARTESIAN_POINT('Ctrl Pts',(52.6308352261214,21.6261058410628,21.5248746665989));
#37511=CARTESIAN_POINT('Ctrl Pts',(52.6515528424947,21.7045006486037,21.5206495135677));
#37512=CARTESIAN_POINT('Ctrl Pts',(52.6761966455775,21.7819830456807,21.5164243605364));
#37513=CARTESIAN_POINT('Ctrl Pts',(52.704665911512,21.8581326658652,21.5121992075052));
#37514=CARTESIAN_POINT('Ctrl Pts',(52.7332083138438,21.9344779113565,21.507963200226));
#37515=CARTESIAN_POINT('Ctrl Pts',(52.7655957779776,22.0094830584573,21.5037271929468));
#37516=CARTESIAN_POINT('Ctrl Pts',(52.8016758266753,22.0827377701809,21.4994911856677));
#37517=CARTESIAN_POINT('Ctrl Pts',(52.8375986831078,22.1556733283977,21.4952736336734));
#37518=CARTESIAN_POINT('Ctrl Pts',(52.8771818163744,22.2268732485597,21.4910560816792));
#37519=CARTESIAN_POINT('Ctrl Pts',(52.9202264825812,22.2959523009137,21.4868385296849));
#37520=CARTESIAN_POINT('Ctrl Pts',(52.9632569364185,22.3650085449361,21.4826223702304));
#37521=CARTESIAN_POINT('Ctrl Pts',(53.0097464078368,22.4319449174975,21.4784062107759));
#37522=CARTESIAN_POINT('Ctrl Pts',(53.0594512170528,22.4964025765155,21.4741900513214));
#37523=CARTESIAN_POINT('Ctrl Pts',(53.1091548419039,22.5608586996381,21.4699739923294));
#37524=CARTESIAN_POINT('Ctrl Pts',(53.162073367439,22.6228358591552,21.4657579333374));
#37525=CARTESIAN_POINT('Ctrl Pts',(53.217921848186,22.6820070483881,21.4615418743454));
#37526=CARTESIAN_POINT('Ctrl Pts',(53.2742274844283,22.7416625916081,21.457291304217));
#37527=CARTESIAN_POINT('Ctrl Pts',(53.3335109467948,22.798465655308,21.4530407340886));
#37528=CARTESIAN_POINT('Ctrl Pts',(53.3954425421333,22.8521192225136,21.4487901639602));
#37529=CARTESIAN_POINT('Ctrl Pts',(53.4569606149237,22.9054145402715,21.4445679752514));
#37530=CARTESIAN_POINT('Ctrl Pts',(53.5210911569203,22.9556020516917,21.4403457865426));
#37531=CARTESIAN_POINT('Ctrl Pts',(53.5874794686101,23.0024325203117,21.4361235978337));
#37532=CARTESIAN_POINT('Ctrl Pts',(53.6545371705108,23.0497351783348,21.4318588369956));
#37533=CARTESIAN_POINT('Ctrl Pts',(53.723898017794,23.0936124550003,21.4275940761574));
#37534=CARTESIAN_POINT('Ctrl Pts',(53.7951700802675,23.133854520467,21.4233293153193));
#37535=CARTESIAN_POINT('Ctrl Pts',(53.866442142741,23.1740965859337,21.4190645544811));
#37536=CARTESIAN_POINT('Ctrl Pts',(53.9396249607651,23.2107032821244,21.4147997936429));
#37537=CARTESIAN_POINT('Ctrl Pts',(54.0143067729884,23.2435149012707,21.4105350328048));
#37538=CARTESIAN_POINT('Ctrl Pts',(54.0884012444677,23.2760684709638,21.4063038124999));
#37539=CARTESIAN_POINT('Ctrl Pts',(54.1642490439065,23.305008557811,21.4020725921949));
#37540=CARTESIAN_POINT('Ctrl Pts',(54.2414633981289,23.3301443031756,21.39784137189));
#37541=CARTESIAN_POINT('Ctrl Pts',(54.3185670323716,23.3552440056407,21.3936162188589));
#37542=CARTESIAN_POINT('Ctrl Pts',(54.3970328912392,23.3765500582797,21.3893910658277));
#37543=CARTESIAN_POINT('Ctrl Pts',(54.4764531533141,23.3939191609838,21.3851659127966));
#37544=CARTESIAN_POINT('Ctrl Pts',(54.5560774428452,23.4113328842135,21.3809299055174));
#37545=CARTESIAN_POINT('Ctrl Pts',(54.6366606107811,23.4247892199005,21.3766938982382));
#37546=CARTESIAN_POINT('Ctrl Pts',(54.7177752009829,23.434193791139,21.372457890959));
#37547=CARTESIAN_POINT('Ctrl Pts',(54.7985363940386,23.4435573888778,21.3682403389648));
#37548=CARTESIAN_POINT('Ctrl Pts',(54.8798239246373,23.4489043916971,21.3640227869707));
#37549=CARTESIAN_POINT('Ctrl Pts',(54.9612063458353,23.4501929112616,21.3598052349765));
#37550=CARTESIAN_POINT('Ctrl Pts',(55.0425618964092,23.4514810053863,21.3555890755221));
#37551=CARTESIAN_POINT('Ctrl Pts',(55.1240118108655,23.4487132699912,21.3513729160677));
#37552=CARTESIAN_POINT('Ctrl Pts',(55.2051224488941,23.4418998814365,21.3471567566133));
#37553=CARTESIAN_POINT('Ctrl Pts',(55.2862311542206,23.4350866552311,21.3429406976214));
#37554=CARTESIAN_POINT('Ctrl Pts',(55.3670001359959,23.4242280075553,21.3387246386295));
#37555=CARTESIAN_POINT('Ctrl Pts',(55.4470001279844,23.4093860495118,21.3345085796376));
#37556=CARTESIAN_POINT('Ctrl Pts',(55.5276549710213,23.3944226005587,21.3302580095091));
#37557=CARTESIAN_POINT('Ctrl Pts',(55.6075277022202,23.3754104000805,21.3260074393806));
#37558=CARTESIAN_POINT('Ctrl Pts',(55.686189990587,23.3524654188358,21.3217568692522));
#37559=CARTESIAN_POINT('Ctrl Pts',(55.7643270441368,23.3296736431903,21.3175346805434));
#37560=CARTESIAN_POINT('Ctrl Pts',(55.8412693467259,23.3030016580496,21.3133124918347));
#37561=CARTESIAN_POINT('Ctrl Pts',(55.9166151552415,23.2726123530382,21.3090903031259));
#37562=CARTESIAN_POINT('Ctrl Pts',(55.9927206719904,23.2419166340977,21.3048255422876));
#37563=CARTESIAN_POINT('Ctrl Pts',(56.0671968778821,23.2074284143686,21.3005607814492));
#37564=CARTESIAN_POINT('Ctrl Pts',(56.1396549533528,23.1693632331397,21.2962960206109));
#37565=CARTESIAN_POINT('Ctrl Pts',(56.2121130288235,23.1312980519109,21.2920312597725));
#37566=CARTESIAN_POINT('Ctrl Pts',(56.2825525918245,23.0896562096749,21.2877664989342));
#37567=CARTESIAN_POINT('Ctrl Pts',(56.3506161842434,23.0446970858442,21.2835017380958));
#37568=CARTESIAN_POINT('Ctrl Pts',(56.4181444854036,23.0000915464356,21.2792705177909));
#37569=CARTESIAN_POINT('Ctrl Pts',(56.4835873031694,22.9520534895508,21.275039297486));
#37570=CARTESIAN_POINT('Ctrl Pts',(56.5465745545015,22.9008044079727,21.2708080771811));
#37571=CARTESIAN_POINT('Ctrl Pts',(56.6094714865237,22.8496288139906,21.26658292415));
#37572=CARTESIAN_POINT('Ctrl Pts',(56.6699194877135,22.7952516309173,21.2623577711188));
#37573=CARTESIAN_POINT('Ctrl Pts',(56.7275770225726,22.7379378242846,21.2581326180877));
#37574=CARTESIAN_POINT('Ctrl Pts',(56.7853826773179,22.6804767807897,21.2538966108085));
#37575=CARTESIAN_POINT('Ctrl Pts',(56.8403831198812,22.6200642717991,21.2496606035293));
#37576=CARTESIAN_POINT('Ctrl Pts',(56.8922672753953,22.5570082878611,21.2454245962501));
#37577=CARTESIAN_POINT('Ctrl Pts',(56.9439253838756,22.4942270239794,21.241207044256));
#37578=CARTESIAN_POINT('Ctrl Pts',(56.9924939989411,22.428825627201,21.2369894922618));
#37579=CARTESIAN_POINT('Ctrl Pts',(57.0377039845765,22.3611439017389,21.2327719402677));
#37580=CARTESIAN_POINT('Ctrl Pts',(57.0828990429031,22.2934845232429,21.2285557808133));
#37581=CARTESIAN_POINT('Ctrl Pts',(57.1247374159642,22.2235466975424,21.2243396213588));
#37582=CARTESIAN_POINT('Ctrl Pts',(57.162992525052,22.1517003024091,21.2201234619044));
#37583=CARTESIAN_POINT('Ctrl Pts',(57.2012467225981,22.0798556192298,21.2159074029125));
#37584=CARTESIAN_POINT('Ctrl Pts',(57.2359176084042,22.0061028679338,21.2116913439207));
#37585=CARTESIAN_POINT('Ctrl Pts',(57.266824612889,21.9308364111919,21.2074752849288));
#37586=CARTESIAN_POINT('Ctrl Pts',(57.2979846109529,21.8549538504116,21.2032247148003));
#37587=CARTESIAN_POINT('Ctrl Pts',(57.3253186266574,21.7775331261725,21.1989741446718));
#37588=CARTESIAN_POINT('Ctrl Pts',(57.3486918523176,21.6989970192045,21.1947235745433));
#37589=CARTESIAN_POINT('Ctrl Pts',(57.371909012954,21.6209853045299,21.1905013858346));
#37590=CARTESIAN_POINT('Ctrl Pts',(57.3912180642631,21.5418735275523,21.1862791971258));
#37591=CARTESIAN_POINT('Ctrl Pts',(57.4065380379803,21.4620875693566,21.1820570084171));
#37592=CARTESIAN_POINT('Ctrl Pts',(57.4220124822701,21.381497133107,21.1777922475787));
#37593=CARTESIAN_POINT('Ctrl Pts',(57.4334168853248,21.3002193247265,21.1735274867403));
#37594=CARTESIAN_POINT('Ctrl Pts',(57.4407215244208,21.2186977142746,21.169262725902));
#37595=CARTESIAN_POINT('Ctrl Pts',(57.4480261635168,21.1371761038228,21.1649979650636));
#37596=CARTESIAN_POINT('Ctrl Pts',(57.4512310839835,21.0554111752442,21.1607332042252));
#37597=CARTESIAN_POINT('Ctrl Pts',(57.4503604039834,20.9738439186702,21.1564684433868));
#37598=CARTESIAN_POINT('Ctrl Pts',(57.4494965715118,20.8929181539406,21.1522372230819));
#37599=CARTESIAN_POINT('Ctrl Pts',(57.4446178218065,20.8118835001941,21.148006002777));
#37600=CARTESIAN_POINT('Ctrl Pts',(57.4357095938325,20.7311710125144,21.143774782472));
#37601=CARTESIAN_POINT('Ctrl Pts',(57.4268141396339,20.650574260893,21.1395496294409));
#37602=CARTESIAN_POINT('Ctrl Pts',(57.4139007332612,20.5702992160609,21.1353244764097));
#37603=CARTESIAN_POINT('Ctrl Pts',(57.3970068201212,20.490776518322,21.1310993233785));
#37604=CARTESIAN_POINT('Ctrl Pts',(57.3800695071986,20.4110495299743,21.1268633160993));
#37605=CARTESIAN_POINT('Ctrl Pts',(57.3591312212664,20.3320792310835,21.1226273088201));
#37606=CARTESIAN_POINT('Ctrl Pts',(57.3342820752912,20.2542939969571,21.1183913015409));
#37607=CARTESIAN_POINT('Ctrl Pts',(57.3095411911866,20.1768476547571,21.1141737495468));
#37608=CARTESIAN_POINT('Ctrl Pts',(57.2809235879493,20.1005765209318,21.1099561975526));
#37609=CARTESIAN_POINT('Ctrl Pts',(57.248568849674,20.0258909823456,21.1057386455584));
#37610=CARTESIAN_POINT('Ctrl Pts',(57.2162247941972,19.9512301032252,21.101522486104));
#37611=CARTESIAN_POINT('Ctrl Pts',(57.1801462387363,19.8781542059672,21.0973063266495));
#37612=CARTESIAN_POINT('Ctrl Pts',(57.1405211117549,19.8070542258211,21.0930901671951));
#37613=CARTESIAN_POINT('Ctrl Pts',(57.1008969289601,19.7359559398434,21.0888741082032));
#37614=CARTESIAN_POINT('Ctrl Pts',(57.0577265699682,19.6668338829374,21.0846580492113));
#37615=CARTESIAN_POINT('Ctrl Pts',(57.0112434834743,19.6000536081042,21.0804419902193));
#37616=CARTESIAN_POINT('Ctrl Pts',(56.9643799032188,19.5327266940546,21.0761914200909));
#37617=CARTESIAN_POINT('Ctrl Pts',(56.9141493724349,19.4677804798977,21.0719408499624));
#37618=CARTESIAN_POINT('Ctrl Pts',(56.8608340307758,19.4055574767629,21.067690279834));
#37619=CARTESIAN_POINT('Ctrl Pts',(56.8078746802055,19.3437499419331,21.0634680911252));
#37620=CARTESIAN_POINT('Ctrl Pts',(56.7518719561585,19.2846296609929,21.0592459024164));
#37621=CARTESIAN_POINT('Ctrl Pts',(56.6931397962257,19.2284955883666,21.0550237137077));
#37622=CARTESIAN_POINT('Ctrl Pts',(56.6338154426954,19.1717955185344,21.0507589528694));
#37623=CARTESIAN_POINT('Ctrl Pts',(56.5717066695522,19.1181425331317,21.0464941920311));
#37624=CARTESIAN_POINT('Ctrl Pts',(56.5071700637402,19.0678021196148,21.0422294311927));
#37625=CARTESIAN_POINT('Ctrl Pts',(56.4426334579283,19.0174617060978,21.0379646703544));
#37626=CARTESIAN_POINT('Ctrl Pts',(56.3756694506535,18.9704340887847,21.0336999095161));
#37627=CARTESIAN_POINT('Ctrl Pts',(56.306661654817,18.9269381172211,21.0294351486778));
#37628=CARTESIAN_POINT('Ctrl Pts',(56.2381965759975,18.8837842230076,21.0252039283729));
#37629=CARTESIAN_POINT('Ctrl Pts',(56.1674630289766,18.8439447622647,21.020972708068));
#37630=CARTESIAN_POINT('Ctrl Pts',(56.0948153061716,18.8076656971683,21.0167414877631));
#37631=CARTESIAN_POINT('Ctrl Pts',(56.0222717551164,18.7714386537121,21.0125163347319));
#37632=CARTESIAN_POINT('Ctrl Pts',(55.9478198920762,18.7387620722398,21.0082911817008));
#37633=CARTESIAN_POINT('Ctrl Pts',(55.8718418599838,18.7098379923726,21.0040660286696));
#37634=CARTESIAN_POINT('Ctrl Pts',(55.7956686433856,18.6808396077086,20.9998300213904));
#37635=CARTESIAN_POINT('Ctrl Pts',(55.7179618090992,18.655613275635,20.9955940141112));
#37636=CARTESIAN_POINT('Ctrl Pts',(55.6391301544288,18.634315554496,20.991358006832));
#37637=CARTESIAN_POINT('Ctrl Pts',(55.5606419506927,18.6131106225068,20.9871404548379));
#37638=CARTESIAN_POINT('Ctrl Pts',(55.4810391568323,18.595800270702,20.9829229028437));
#37639=CARTESIAN_POINT('Ctrl Pts',(55.4007422799513,18.5824897363073,20.9787053508496));
#37640=CARTESIAN_POINT('Ctrl Pts',(55.3204719152723,18.5691835967483,20.9744891913951));
#37641=CARTESIAN_POINT('Ctrl Pts',(55.2395083809756,18.5598747279479,20.9702730319407));
#37642=CARTESIAN_POINT('Ctrl Pts',(55.1582820536027,18.5546171993924,20.9660568724863));
#37643=CARTESIAN_POINT('Ctrl Pts',(55.0770576616885,18.5493597961132,20.9618408134944));
#37644=CARTESIAN_POINT('Ctrl Pts',(54.9955709531706,18.5481535700658,20.9576247545025));
#37645=CARTESIAN_POINT('Ctrl Pts',(54.9142556595911,18.551000580219,20.9534086955106));
#37646=CARTESIAN_POINT('Ctrl Pts',(54.8322747483795,18.5538708949692,20.9491581253821));
#37647=CARTESIAN_POINT('Ctrl Pts',(54.750468551326,18.5608611081166,20.9449075552536));
#37648=CARTESIAN_POINT('Ctrl Pts',(54.6692778406778,18.5719198729586,20.9406569851252));
#37649=CARTESIAN_POINT('Ctrl Pts',(54.5886292473379,18.5829047974834,20.9364347964164));
#37650=CARTESIAN_POINT('Ctrl Pts',(54.5085883962111,18.5979039597923,20.9322126077077));
#37651=CARTESIAN_POINT('Ctrl Pts',(54.4295767031962,18.6168156780342,20.9279904189989));
#37652=CARTESIAN_POINT('Ctrl Pts',(54.3497683390076,18.6359180822391,20.9237256581606));
#37653=CARTESIAN_POINT('Ctrl Pts',(54.2710104698192,18.6590122500086,20.9194608973222));
#37654=CARTESIAN_POINT('Ctrl Pts',(54.1937195168102,18.6859425174756,20.9151961364839));
#37655=CARTESIAN_POINT('Ctrl Pts',(54.1164285638013,18.7128727849425,20.9109313756456));
#37656=CARTESIAN_POINT('Ctrl Pts',(54.040604949261,18.7436389114226,20.9066666148072));
#37657=CARTESIAN_POINT('Ctrl Pts',(53.9666405616107,18.77803723679,20.9024018539689));
#37658=CARTESIAN_POINT('Ctrl Pts',(53.8932578724681,18.812165033932,20.898170633664));
#37659=CARTESIAN_POINT('Ctrl Pts',(53.8214300745687,18.8499960365009,20.893939413359));
#37660=CARTESIAN_POINT('Ctrl Pts',(53.751555939118,18.8913659215387,20.8897081930541));
#37661=CARTESIAN_POINT('Ctrl Pts',(53.681781998287,18.9326764850568,20.885483040023));
#37662=CARTESIAN_POINT('Ctrl Pts',(53.6139565527698,18.9775156178237,20.8812578869918));
#37663=CARTESIAN_POINT('Ctrl Pts',(53.5484565696458,19.0256717801248,20.8770327339607));
#37664=CARTESIAN_POINT('Ctrl Pts',(53.482788319702,19.0739516536682,20.8727967266815));
#37665=CARTESIAN_POINT('Ctrl Pts',(53.4194579207677,19.1255654163242,20.8685607194023));
#37666=CARTESIAN_POINT('Ctrl Pts',(53.3588185775264,19.1802544714913,20.8643247121231));
#37667=CARTESIAN_POINT('Ctrl Pts',(53.2984434256075,19.2347052593383,20.8601071601289));
#37668=CARTESIAN_POINT('Ctrl Pts',(53.2407362826118,19.2922042916543,20.8558896081348));
#37669=CARTESIAN_POINT('Ctrl Pts',(53.1860135807132,19.3524553054187,20.8516720561406));
#37670=CARTESIAN_POINT('Ctrl Pts',(53.1313089470058,19.4126864256691,20.8474558966862));
#37671=CARTESIAN_POINT('Ctrl Pts',(53.0795871098758,19.4756673790442,20.8432397372318));
#37672=CARTESIAN_POINT('Ctrl Pts',(53.031126859977,19.5410658656074,20.8390235777773));
#37673=CARTESIAN_POINT('Ctrl Pts',(52.9826677647877,19.6064627938572,20.8348075187854));
#37674=CARTESIAN_POINT('Ctrl Pts',(52.9374703782139,19.6742767665566,20.8305914597936));
#37675=CARTESIAN_POINT('Ctrl Pts',(52.8957716089877,19.7441444635399,20.8263754008017));
#37676=CARTESIAN_POINT('Ctrl Pts',(52.8537315086929,19.8145840722631,20.8221248306732));
#37677=CARTESIAN_POINT('Ctrl Pts',(52.8152478265902,19.8871107788478,20.8178742605447));
#37678=CARTESIAN_POINT('Ctrl Pts',(52.7805164157013,19.9613263895579,20.8136236904162));
#37679=CARTESIAN_POINT('Ctrl Pts',(52.7460169094089,20.0350464562976,20.8094015017075));
#37680=CARTESIAN_POINT('Ctrl Pts',(52.7152198387914,20.1104324839184,20.8051793129987));
#37681=CARTESIAN_POINT('Ctrl Pts',(52.6882682680638,20.1870752497561,20.80095712429));
#37682=CARTESIAN_POINT('Ctrl Pts',(52.6610449459197,20.2644908009867,20.7966923634516));
#37683=CARTESIAN_POINT('Ctrl Pts',(52.637745246046,20.3431881105333,20.7924276026133));
#37684=CARTESIAN_POINT('Ctrl Pts',(52.6184641668122,20.4227328822438,20.7881628417749));
#37685=CARTESIAN_POINT('Ctrl Pts',(52.5991830875784,20.5022776539543,20.7838980809366));
#37686=CARTESIAN_POINT('Ctrl Pts',(52.5839206557274,20.5826694025021,20.7796333200982));
#37687=CARTESIAN_POINT('Ctrl Pts',(52.5727182392775,20.6634684204062,20.7753685592599));
#37688=CARTESIAN_POINT('Ctrl Pts',(52.5573596372609,20.7742445163375,20.769521538244));
#37689=CARTESIAN_POINT('Ctrl Pts',(52.5495820092598,20.8860954143571,20.763674517228));
#37690=CARTESIAN_POINT('Ctrl Pts',(52.5495006451703,20.9982218044437,20.7578274962121));
#37691=CARTESIAN_POINT('',(52.5497641805207,20.9991538160394,19.9578275400623));
#37692=CARTESIAN_POINT('Ctrl Pts',(52.5472108677062,20.9982398775261,20.7578264680766));
#37693=CARTESIAN_POINT('Ctrl Pts',(52.5529443810253,21.6987907323952,20.7213294002347));
#37694=CARTESIAN_POINT('Ctrl Pts',(53.2348022320658,23.221863456408,20.6424879008231));
#37695=CARTESIAN_POINT('Ctrl Pts',(55.8195806506902,23.7781630867416,20.521301969842));
#37696=CARTESIAN_POINT('Ctrl Pts',(57.778705419208,21.8177400398511,20.3942686751329));
#37697=CARTESIAN_POINT('Ctrl Pts',(57.1937688630138,19.1086299264319,20.2672353804239));
#37698=CARTESIAN_POINT('Ctrl Pts',(54.6003133464515,18.1311756487213,20.1402020857151));
#37699=CARTESIAN_POINT('Ctrl Pts',(52.7918351476342,19.4700594808486,20.0370663306344));
#37700=CARTESIAN_POINT('Ctrl Pts',(52.5521271605753,20.6428395652265,19.9762750071234));
#37701=CARTESIAN_POINT('Ctrl Pts',(52.5532271445043,20.9991439022597,19.9578281151821));
#37702=CARTESIAN_POINT('',(52.5495010013229,21.0022152838851,19.1578274961645));
#37703=CARTESIAN_POINT('Ctrl Pts',(52.5495001458373,20.9991545719183,19.9578274962121));
#37704=CARTESIAN_POINT('Ctrl Pts',(52.549471344841,21.0826351645882,19.9535120362847));
#37705=CARTESIAN_POINT('Ctrl Pts',(52.5537127576159,21.1660840188203,19.9491965763572));
#37706=CARTESIAN_POINT('Ctrl Pts',(52.5621884503673,21.2490483858156,19.9448811164298));
#37707=CARTESIAN_POINT('Ctrl Pts',(52.5706699431405,21.3320695263584,19.9405627033795));
#37708=CARTESIAN_POINT('Ctrl Pts',(52.5833914368997,21.4146050890858,19.9362442903292));
#37709=CARTESIAN_POINT('Ctrl Pts',(52.6002654346689,21.4962099011055,19.9319258772788));
#37710=CARTESIAN_POINT('Ctrl Pts',(52.6171689861287,21.577957638554,19.9275999008138));
#37711=CARTESIAN_POINT('Ctrl Pts',(52.6382394758439,21.658770945012,19.9232739243488));
#37712=CARTESIAN_POINT('Ctrl Pts',(52.6633387861678,21.7382171914635,19.9189479478837));
#37713=CARTESIAN_POINT('Ctrl Pts',(52.6884622139892,21.817739776453,19.914617814662));
#37714=CARTESIAN_POINT('Ctrl Pts',(52.7176220232487,21.8958922788628,19.9102876814402));
#37715=CARTESIAN_POINT('Ctrl Pts',(52.7506318224984,21.972261822784,19.9059575482185));
#37716=CARTESIAN_POINT('Ctrl Pts',(52.7837104239721,22.0487905435128,19.9016183897132));
#37717=CARTESIAN_POINT('Ctrl Pts',(52.8206548525578,22.1235284940726,19.897279231208));
#37718=CARTESIAN_POINT('Ctrl Pts',(52.861232598174,22.1960870582389,19.8929400727027));
#37719=CARTESIAN_POINT('Ctrl Pts',(52.8824436517367,22.2340153257557,19.8906718805675));
#37720=CARTESIAN_POINT('Ctrl Pts',(52.904646760021,22.271348570579,19.8884036884323));
#37721=CARTESIAN_POINT('Ctrl Pts',(52.9278041874616,22.3080346954489,19.8861354962971));
#37722=CARTESIAN_POINT('Ctrl Pts',(52.9710034278058,22.3764711713755,19.8819042759922));
#37723=CARTESIAN_POINT('Ctrl Pts',(53.0176775874499,22.4428936083075,19.8776730556872));
#37724=CARTESIAN_POINT('Ctrl Pts',(53.0676128757991,22.5069274210202,19.8734418353823));
#37725=CARTESIAN_POINT('Ctrl Pts',(53.1174765604398,22.5708694137272,19.8692166823511));
#37726=CARTESIAN_POINT('Ctrl Pts',(53.1705918029512,22.6324292212306,19.86499152932));
#37727=CARTESIAN_POINT('Ctrl Pts',(53.2267007588123,22.6912599005484,19.8607663762888));
#37728=CARTESIAN_POINT('Ctrl Pts',(53.2829538563221,22.750241713513,19.8565303690096));
#37729=CARTESIAN_POINT('Ctrl Pts',(53.342215810946,22.8064799625865,19.8522943617304));
#37730=CARTESIAN_POINT('Ctrl Pts',(53.404185132303,22.8596572689712,19.8480583544512));
#37731=CARTESIAN_POINT('Ctrl Pts',(53.4658844679367,22.912602894369,19.8438408024571));
#37732=CARTESIAN_POINT('Ctrl Pts',(53.5302672790467,22.962513882173,19.8396232504629));
#37733=CARTESIAN_POINT('Ctrl Pts',(53.5969994009295,23.0091141254314,19.8354056984688));
#37734=CARTESIAN_POINT('Ctrl Pts',(53.6637094893839,23.0556989823496,19.8311895390143));
#37735=CARTESIAN_POINT('Ctrl Pts',(53.7327669673213,23.0989749995541,19.8269733795599));
#37736=CARTESIAN_POINT('Ctrl Pts',(53.8038067226578,23.1387079962541,19.8227572201054));
#37737=CARTESIAN_POINT('Ctrl Pts',(53.8748447852608,23.1784400461973,19.8185411611135));
#37738=CARTESIAN_POINT('Ctrl Pts',(53.947864625042,23.2146290175103,19.8143251021216));
#37739=CARTESIAN_POINT('Ctrl Pts',(54.0224756986029,23.2470862222394,19.8101090431297));
#37740=CARTESIAN_POINT('Ctrl Pts',(54.0976975114716,23.2798091099268,19.8058584730013));
#37741=CARTESIAN_POINT('Ctrl Pts',(54.1745362953992,23.308738649168,19.8016079028728));
#37742=CARTESIAN_POINT('Ctrl Pts',(54.2525721484682,23.3337313163161,19.7973573327443));
#37743=CARTESIAN_POINT('Ctrl Pts',(54.3300869494825,23.3585571052915,19.7931351440356));
#37744=CARTESIAN_POINT('Ctrl Pts',(54.4087824128415,23.3794983747325,19.7889129553268));
#37745=CARTESIAN_POINT('Ctrl Pts',(54.4882344233204,23.3964653647666,19.784690766618));
#37746=CARTESIAN_POINT('Ctrl Pts',(54.568487544673,23.4136034321608,19.7804260057797));
#37747=CARTESIAN_POINT('Ctrl Pts',(54.6495120758896,23.4266865466672,19.7761612449414));
#37748=CARTESIAN_POINT('Ctrl Pts',(54.7308651565917,23.4356758171119,19.771896484103));
#37749=CARTESIAN_POINT('Ctrl Pts',(54.8122182372939,23.4446650875565,19.7676317232647));
#37750=CARTESIAN_POINT('Ctrl Pts',(54.893899382703,23.4495605492491,19.7633669624264));
#37751=CARTESIAN_POINT('Ctrl Pts',(54.9754671981716,23.4503771937468,19.759102201588));
#37752=CARTESIAN_POINT('Ctrl Pts',(55.0563935174008,23.4511874156822,19.7548709812831));
#37753=CARTESIAN_POINT('Ctrl Pts',(55.1375117469533,23.4479858315854,19.7506397609782));
#37754=CARTESIAN_POINT('Ctrl Pts',(55.2183912251447,23.4407489675876,19.7464085406732));
#37755=CARTESIAN_POINT('Ctrl Pts',(55.2991547278249,23.4335224807462,19.7421833876421));
#37756=CARTESIAN_POINT('Ctrl Pts',(55.3796796999174,23.4222722471323,19.7379582346109));
#37757=CARTESIAN_POINT('Ctrl Pts',(55.4595348187269,23.4070267967718,19.7337330815798));
#37758=CARTESIAN_POINT('Ctrl Pts',(55.5395950821221,23.3917421814631,19.7294970743006));
#37759=CARTESIAN_POINT('Ctrl Pts',(55.6189815741237,23.3724417977264,19.7252610670214));
#37760=CARTESIAN_POINT('Ctrl Pts',(55.6972641471716,23.3492068787293,19.7210250597422));
#37761=CARTESIAN_POINT('Ctrl Pts',(55.7752056615044,23.3260731887965,19.716807507748));
#37762=CARTESIAN_POINT('Ctrl Pts',(55.8520524049936,23.2990393010793,19.7125899557539));
#37763=CARTESIAN_POINT('Ctrl Pts',(55.9273911914125,23.2682362813628,19.7083724037597));
#37764=CARTESIAN_POINT('Ctrl Pts',(56.0027051026781,23.2374434321026,19.7041562443053));
#37765=CARTESIAN_POINT('Ctrl Pts',(56.0765116156152,23.2028840980203,19.6999400848509));
#37766=CARTESIAN_POINT('Ctrl Pts',(56.1484159914954,23.1647380812647,19.6957239253964));
#37767=CARTESIAN_POINT('Ctrl Pts',(56.2203186540399,23.1265929734515,19.6915078664046));
#37768=CARTESIAN_POINT('Ctrl Pts',(56.2903188594575,23.0848615717513,19.6872918074127));
#37769=CARTESIAN_POINT('Ctrl Pts',(56.3580463042962,23.0397697138127,19.6830757484208));
#37770=CARTESIAN_POINT('Ctrl Pts',(56.4263281415435,22.9943087502067,19.6788251782923));
#37771=CARTESIAN_POINT('Ctrl Pts',(56.4922994302679,22.9454323139594,19.6745746081638));
#37772=CARTESIAN_POINT('Ctrl Pts',(56.5556118968356,22.8934153998591,19.6703240380353));
#37773=CARTESIAN_POINT('Ctrl Pts',(56.6185016206574,22.8417458071362,19.6661018493266));
#37774=CARTESIAN_POINT('Ctrl Pts',(56.6787676146706,22.7869779088318,19.6618796606178));
#37775=CARTESIAN_POINT('Ctrl Pts',(56.7361044949192,22.7294193917964,19.6576574719091));
#37776=CARTESIAN_POINT('Ctrl Pts',(56.7940195002267,22.6712805149488,19.6533927110707));
#37777=CARTESIAN_POINT('Ctrl Pts',(56.8489456659615,22.6102947882438,19.6491279502324));
#37778=CARTESIAN_POINT('Ctrl Pts',(56.900610185816,22.5468132309922,19.6448631893941));
#37779=CARTESIAN_POINT('Ctrl Pts',(56.9522747056704,22.4833316737407,19.6405984285557));
#37780=CARTESIAN_POINT('Ctrl Pts',(57.0006773464554,22.4173547124163,19.6363336677174));
#37781=CARTESIAN_POINT('Ctrl Pts',(57.0455913707908,22.3492613511645,19.6320689068791));
#37782=CARTESIAN_POINT('Ctrl Pts',(57.0901521653928,22.2817035152903,19.6278376865741));
#37783=CARTESIAN_POINT('Ctrl Pts',(57.131446156631,22.2118091407379,19.6236064662692));
#37784=CARTESIAN_POINT('Ctrl Pts',(57.169220106761,22.1399273566433,19.6193752459643));
#37785=CARTESIAN_POINT('Ctrl Pts',(57.2069398916903,22.068148645996,19.6151500929331));
#37786=CARTESIAN_POINT('Ctrl Pts',(57.2411494457619,21.9943885938192,19.610924939902));
#37787=CARTESIAN_POINT('Ctrl Pts',(57.2716388683287,21.9190250823009,19.6066997868708));
#37788=CARTESIAN_POINT('Ctrl Pts',(57.3022066169946,21.8434679649555,19.6024637795916));
#37789=CARTESIAN_POINT('Ctrl Pts',(57.3290348414209,21.7662995368335,19.5982277723124));
#37790=CARTESIAN_POINT('Ctrl Pts',(57.3519585611881,21.6879252695271,19.5939917650332));
#37791=CARTESIAN_POINT('Ctrl Pts',(57.3747824077128,21.6098924604258,19.5897742130391));
#37792=CARTESIAN_POINT('Ctrl Pts',(57.3937355614453,21.5306647441038,19.5855566610449));
#37793=CARTESIAN_POINT('Ctrl Pts',(57.4087041098994,21.4506603609743,19.5813391090508));
#37794=CARTESIAN_POINT('Ctrl Pts',(57.4236677160794,21.3706823934722,19.5771229495963));
#37795=CARTESIAN_POINT('Ctrl Pts',(57.4346492441949,21.2899287250452,19.5729067901419));
#37796=CARTESIAN_POINT('Ctrl Pts',(57.4415857344128,21.2088285217872,19.5686906306875));
#37797=CARTESIAN_POINT('Ctrl Pts',(57.4485220593482,21.1277302509827,19.5644745716956));
#37798=CARTESIAN_POINT('Ctrl Pts',(57.4514134995091,21.0462859250897,19.5602585127037));
#37799=CARTESIAN_POINT('Ctrl Pts',(57.450249025058,20.9649291402713,19.5560424537118));
#37800=CARTESIAN_POINT('Ctrl Pts',(57.4490750186396,20.8829063981885,19.5517918835833));
#37801=CARTESIAN_POINT('Ctrl Pts',(57.4437783814331,20.8009731168526,19.5475413134549));
#37802=CARTESIAN_POINT('Ctrl Pts',(57.4344013322171,20.7195710362687,19.5432907433264));
#37803=CARTESIAN_POINT('Ctrl Pts',(57.4250868943595,20.6387124843282,19.5390685546176));
#37804=CARTESIAN_POINT('Ctrl Pts',(57.411746506964,20.5583785140341,19.5348463659089));
#37805=CARTESIAN_POINT('Ctrl Pts',(57.3944731135562,20.4789925543175,19.5306241772001));
#37806=CARTESIAN_POINT('Ctrl Pts',(57.3770255533374,20.3988061497138,19.5263594163618));
#37807=CARTESIAN_POINT('Ctrl Pts',(57.3555653550877,20.3195874496795,19.5220946555235));
#37808=CARTESIAN_POINT('Ctrl Pts',(57.3302395361106,20.2417560060594,19.5178298946851));
#37809=CARTESIAN_POINT('Ctrl Pts',(57.3049137171336,20.1639245624393,19.5135651338468));
#37810=CARTESIAN_POINT('Ctrl Pts',(57.2757225093273,20.0874808024105,19.5093003730085));
#37811=CARTESIAN_POINT('Ctrl Pts',(57.242861423422,20.0128207430637,19.5050356121701));
#37812=CARTESIAN_POINT('Ctrl Pts',(57.2102587760063,19.9387478533871,19.5008043918652));
#37813=CARTESIAN_POINT('Ctrl Pts',(57.1739215540254,19.866152925154,19.4965731715603));
#37814=CARTESIAN_POINT('Ctrl Pts',(57.1340057970936,19.7954380431165,19.4923419512554));
#37815=CARTESIAN_POINT('Ctrl Pts',(57.0941472765634,19.7248245612703,19.4881167982242));
#37816=CARTESIAN_POINT('Ctrl Pts',(57.0507206389732,19.656086172909,19.4838916451931));
#37817=CARTESIAN_POINT('Ctrl Pts',(57.0039295815891,19.589604139955,19.4796664921619));
#37818=CARTESIAN_POINT('Ctrl Pts',(56.9570183198623,19.5229513173347,19.4754304848827));
#37819=CARTESIAN_POINT('Ctrl Pts',(56.9067255261239,19.4585668873638,19.4711944776035));
#37820=CARTESIAN_POINT('Ctrl Pts',(56.8533024359616,19.3968093279779,19.4669584703243));
#37821=CARTESIAN_POINT('Ctrl Pts',(56.8001120976083,19.3353208317184,19.4627409183301));
#37822=CARTESIAN_POINT('Ctrl Pts',(56.7438189817862,19.2764367236666,19.458523366336));
#37823=CARTESIAN_POINT('Ctrl Pts',(56.6847127430469,19.2204794962082,19.4543058143418));
#37824=CARTESIAN_POINT('Ctrl Pts',(56.6256260198431,19.1645407445533,19.4500896548874));
#37825=CARTESIAN_POINT('Ctrl Pts',(56.5637283556014,19.1115272737598,19.445873495433));
#37826=CARTESIAN_POINT('Ctrl Pts',(56.4993462126577,19.0617246881341,19.4416573359785));
#37827=CARTESIAN_POINT('Ctrl Pts',(56.4349656038099,19.0119232892029,19.4374412769866));
#37828=CARTESIAN_POINT('Ctrl Pts',(56.3681010023832,18.9653329069072,19.4332252179947));
#37829=CARTESIAN_POINT('Ctrl Pts',(56.2991107505924,18.9221979142143,19.4290091590028));
#37830=CARTESIAN_POINT('Ctrl Pts',(56.2295557695115,18.8787098340465,19.4247585888743));
#37831=CARTESIAN_POINT('Ctrl Pts',(56.1578405760753,18.8387342416609,19.4205080187459));
#37832=CARTESIAN_POINT('Ctrl Pts',(56.0843592278049,18.8024751844235,19.4162574486174));
#37833=CARTESIAN_POINT('Ctrl Pts',(56.0113685207717,18.7664582320076,19.4120352599086));
#37834=CARTESIAN_POINT('Ctrl Pts',(55.9366356280391,18.7341084644212,19.4078130711999));
#37835=CARTESIAN_POINT('Ctrl Pts',(55.8605667255813,18.7055773796394,19.4035908824911));
#37836=CARTESIAN_POINT('Ctrl Pts',(55.7837308239684,18.6767586172757,19.3993261216528));
#37837=CARTESIAN_POINT('Ctrl Pts',(55.7055322819995,18.6518361258678,19.3950613608145));
#37838=CARTESIAN_POINT('Ctrl Pts',(55.6264033379672,18.630913866449,19.3907965999761));
#37839=CARTESIAN_POINT('Ctrl Pts',(55.547274393935,18.6099916070302,19.3865318391378));
#37840=CARTESIAN_POINT('Ctrl Pts',(55.467215532509,18.5930696163763,19.3822670782995));
#37841=CARTESIAN_POINT('Ctrl Pts',(55.3866655114437,18.5801983485707,19.3780023174611));
#37842=CARTESIAN_POINT('Ctrl Pts',(55.3067489820969,18.5674283078219,19.3737710971562));
#37843=CARTESIAN_POINT('Ctrl Pts',(55.2260493203515,18.5585975716892,19.3695398768513));
#37844=CARTESIAN_POINT('Ctrl Pts',(55.1449889801249,18.5537930493022,19.3653086565463));
#37845=CARTESIAN_POINT('Ctrl Pts',(55.0640448747525,18.5489954162639,19.3610835035152));
#37846=CARTESIAN_POINT('Ctrl Pts',(54.9827415782641,18.548212558023,19.356858350484));
#37847=CARTESIAN_POINT('Ctrl Pts',(54.9015098895185,18.5514800494712,19.3526331974529));
#37848=CARTESIAN_POINT('Ctrl Pts',(54.8200695198348,18.5547559349734,19.3483971901737));
#37849=CARTESIAN_POINT('Ctrl Pts',(54.7387015933923,18.562103075311,19.3441611828945));
#37850=CARTESIAN_POINT('Ctrl Pts',(54.6578435414544,18.5735047480212,19.3399251756153));
#37851=CARTESIAN_POINT('Ctrl Pts',(54.5773377689859,18.5848567463315,19.3357076236211));
#37852=CARTESIAN_POINT('Ctrl Pts',(54.4973379019118,18.600227964179,19.331490071627));
#37853=CARTESIAN_POINT('Ctrl Pts',(54.4182719667645,18.6195498859779,19.3272725196328));
#37854=CARTESIAN_POINT('Ctrl Pts',(54.3392321373901,18.6388654281177,19.3230563601784));
#37855=CARTESIAN_POINT('Ctrl Pts',(54.2611260788537,18.6621289735071,19.3188402007239));
#37856=CARTESIAN_POINT('Ctrl Pts',(54.1843707810034,18.6892210778357,19.3146240412695));
#37857=CARTESIAN_POINT('Ctrl Pts',(54.1076173120765,18.7163125366142,19.3104079822776));
#37858=CARTESIAN_POINT('Ctrl Pts',(54.0322149778859,18.7472322171586,19.3061919232857));
#37859=CARTESIAN_POINT('Ctrl Pts',(53.9585634102166,18.7818115320243,19.3019758642938));
#37860=CARTESIAN_POINT('Ctrl Pts',(53.8843089574083,18.8166739006757,19.2977252941654));
#37861=CARTESIAN_POINT('Ctrl Pts',(53.8118345067648,18.8552559037357,19.2934747240369));
#37862=CARTESIAN_POINT('Ctrl Pts',(53.7415251726937,18.8973370790741,19.2892241539084));
#37863=CARTESIAN_POINT('Ctrl Pts',(53.6716853000502,18.9391372748114,19.2850019651997));
#37864=CARTESIAN_POINT('Ctrl Pts',(53.6039820746839,18.9843897442918,19.2807797764909));
#37865=CARTESIAN_POINT('Ctrl Pts',(53.5387630280351,19.0328353496052,19.2765575877821));
#37866=CARTESIAN_POINT('Ctrl Pts',(53.4728863808154,19.0817694296717,19.2722928269438));
#37867=CARTESIAN_POINT('Ctrl Pts',(53.4095446649128,19.1339610915591,19.2680280661055));
#37868=CARTESIAN_POINT('Ctrl Pts',(53.3490596011056,19.1891035233072,19.2637633052671));
#37869=CARTESIAN_POINT('Ctrl Pts',(53.2885745372984,19.2442459550554,19.2594985444288));
#37870=CARTESIAN_POINT('Ctrl Pts',(53.2309464192854,19.3023387693685,19.2552337835905));
#37871=CARTESIAN_POINT('Ctrl Pts',(53.1764555444078,19.3630406637674,19.2509690227521));
#37872=CARTESIAN_POINT('Ctrl Pts',(53.1229452308608,19.4226502297632,19.2467810061315));
#37873=CARTESIAN_POINT('Ctrl Pts',(53.0722501301212,19.4850099234974,19.2425929895108));
#37874=CARTESIAN_POINT('Ctrl Pts',(53.024669961604,19.5498201872146,19.2384049728901));
#37875=CARTESIAN_POINT('Ctrl Pts',(52.9771527445824,19.6145447029582,19.2342224972736));
#37876=CARTESIAN_POINT('Ctrl Pts',(52.9327425628976,19.6817129783031,19.230040021657));
#37877=CARTESIAN_POINT('Ctrl Pts',(52.8917010163663,19.7509901339024,19.2258575460405));
#37878=CARTESIAN_POINT('Ctrl Pts',(52.8507005749442,19.8201979050539,19.2216792593771));
#37879=CARTESIAN_POINT('Ctrl Pts',(52.8130623143615,19.8915099588894,19.2175009727138));
#37880=CARTESIAN_POINT('Ctrl Pts',(52.7790054375102,19.9645612507778,19.2133226860504));
#37881=CARTESIAN_POINT('Ctrl Pts',(52.7449717254275,20.03756285472,19.2091472413694));
#37882=CARTESIAN_POINT('Ctrl Pts',(52.7145147606302,20.1123009185737,19.2049717966884));
#37883=CARTESIAN_POINT('Ctrl Pts',(52.687807788734,20.1883859118023,19.2007963520074));
#37884=CARTESIAN_POINT('Ctrl Pts',(52.661103833147,20.2644623119242,19.1966213789048));
#37885=CARTESIAN_POINT('Ctrl Pts',(52.6381491984721,20.3418848955061,19.1924464058023));
#37886=CARTESIAN_POINT('Ctrl Pts',(52.6190684795368,20.4202454442916,19.1882714326997));
#37887=CARTESIAN_POINT('Ctrl Pts',(52.5999890703565,20.4986006141851,19.1840967461792));
#37888=CARTESIAN_POINT('Ctrl Pts',(52.5847831532995,20.5778931578053,19.1799220596587));
#37889=CARTESIAN_POINT('Ctrl Pts',(52.5735245816719,20.6577029152193,19.1757473731382));
#37890=CARTESIAN_POINT('Ctrl Pts',(52.5622586284001,20.7375649996291,19.1715699494987));
#37891=CARTESIAN_POINT('Ctrl Pts',(52.5549452432902,20.8179445027518,19.1673925258593));
#37892=CARTESIAN_POINT('Ctrl Pts',(52.551606480764,20.8984154295032,19.1632151022198));
#37893=CARTESIAN_POINT('Ctrl Pts',(52.5501711513523,20.9330097700845,19.1614192335506));
#37894=CARTESIAN_POINT('Ctrl Pts',(52.5494697276278,20.9676209861166,19.1596233648813));
#37895=CARTESIAN_POINT('Ctrl Pts',(52.5495010013221,21.002215282968,19.1578274962121));
#37896=CARTESIAN_POINT('',(52.5495000435359,20.9995380808101,18.3578274961844));
#37897=CARTESIAN_POINT('Ctrl Pts',(52.5495010013229,21.002215283885,19.1578274961645));
#37898=CARTESIAN_POINT('Ctrl Pts',(52.5495930447091,21.104031681907,19.1525419752588));
#37899=CARTESIAN_POINT('Ctrl Pts',(52.5560343398191,21.2055657086561,19.1472564543532));
#37900=CARTESIAN_POINT('Ctrl Pts',(52.5686979300326,21.3061380318942,19.1419709334475));
#37901=CARTESIAN_POINT('Ctrl Pts',(52.5816081917137,21.4086693827194,19.1365824569678));
#37902=CARTESIAN_POINT('Ctrl Pts',(52.6009854926653,21.5102013902044,19.1311939804882));
#37903=CARTESIAN_POINT('Ctrl Pts',(52.6266470571175,21.6100377517098,19.1258055040085));
#37904=CARTESIAN_POINT('Ctrl Pts',(52.6296152044612,21.6215853341559,19.1251822453534));
#37905=CARTESIAN_POINT('Ctrl Pts',(52.6326673731257,21.633110255002,19.1245589866982));
#37906=CARTESIAN_POINT('Ctrl Pts',(52.6358032394755,21.6446114546962,19.123935728043));
#37907=CARTESIAN_POINT('Ctrl Pts',(52.6570922200026,21.7226915732393,19.1197045077381));
#37908=CARTESIAN_POINT('Ctrl Pts',(52.6822932908291,21.7998623146875,19.1154732874331));
#37909=CARTESIAN_POINT('Ctrl Pts',(52.7113115953108,21.8757029383536,19.1112420671282));
#37910=CARTESIAN_POINT('Ctrl Pts',(52.7402882895748,21.9514348118734,19.107016914097));
#37911=CARTESIAN_POINT('Ctrl Pts',(52.7730711816813,22.0258399250851,19.1027917610659));
#37912=CARTESIAN_POINT('Ctrl Pts',(52.8095152018074,22.0985110827329,19.0985666080347));
#37913=CARTESIAN_POINT('Ctrl Pts',(52.8460528451539,22.1713689296591,19.0943306007555));
#37914=CARTESIAN_POINT('Ctrl Pts',(52.8862703208193,22.2424834469941,19.0900945934763));
#37915=CARTESIAN_POINT('Ctrl Pts',(52.9299721737715,22.3114629421527,19.0858585861971));
#37916=CARTESIAN_POINT('Ctrl Pts',(52.9734836280536,22.3801419099134,19.0816410342029));
#37917=CARTESIAN_POINT('Ctrl Pts',(53.0204489182305,22.4467040206718,19.0774234822088));
#37918=CARTESIAN_POINT('Ctrl Pts',(53.0706292706656,22.5107874896185,19.0732059302146));
#37919=CARTESIAN_POINT('Ctrl Pts',(53.1207930546899,22.5748497996615,19.0689897707602));
#37920=CARTESIAN_POINT('Ctrl Pts',(53.1741695064926,22.6364347273397,19.0647736113058));
#37921=CARTESIAN_POINT('Ctrl Pts',(53.2304779938119,22.6952115265111,19.0605574518514));
#37922=CARTESIAN_POINT('Ctrl Pts',(53.2867851394142,22.7539869251506,19.0563413928595));
#37923=CARTESIAN_POINT('Ctrl Pts',(53.3460238591996,22.8099539933655,19.0521253338676));
#37924=CARTESIAN_POINT('Ctrl Pts',(53.4078758936407,22.8628180479987,19.0479092748757));
#37925=CARTESIAN_POINT('Ctrl Pts',(53.4702342265021,22.9161148286949,19.0436587047472));
#37926=CARTESIAN_POINT('Ctrl Pts',(53.5352485005538,22.9662572371502,19.0394081346188));
#37927=CARTESIAN_POINT('Ctrl Pts',(53.6025591697091,23.012985190168,19.0351575644903));
#37928=CARTESIAN_POINT('Ctrl Pts',(53.6694203997786,23.0594011366534,19.0309353757816));
#37929=CARTESIAN_POINT('Ctrl Pts',(53.7385470206645,23.102447890352,19.0267131870728));
#37930=CARTESIAN_POINT('Ctrl Pts',(53.8095597292185,23.1419155472851,19.0224909983641));
#37931=CARTESIAN_POINT('Ctrl Pts',(53.8812884555628,23.1817811547412,19.0182262375258));
#37932=CARTESIAN_POINT('Ctrl Pts',(53.9549410823697,23.2179948691113,19.0139614766875));
#37933=CARTESIAN_POINT('Ctrl Pts',(54.0301055002312,23.2503899460578,19.0096967158492));
#37934=CARTESIAN_POINT('Ctrl Pts',(54.1052699180927,23.2827850230044,19.0054319550108));
#37935=CARTESIAN_POINT('Ctrl Pts',(54.1819456531084,23.3113613544749,19.0011671941725));
#37936=CARTESIAN_POINT('Ctrl Pts',(54.2597062346072,23.3360041504502,18.9969024333342));
#37937=CARTESIAN_POINT('Ctrl Pts',(54.3368552621458,23.3604531412972,18.9926712130293));
#37938=CARTESIAN_POINT('Ctrl Pts',(54.4153614196718,23.3811219713792,18.9884399927244));
#37939=CARTESIAN_POINT('Ctrl Pts',(54.4948197526338,23.3978622078157,18.9842087724194));
#37940=CARTESIAN_POINT('Ctrl Pts',(54.5741641479076,23.4145784399249,18.9799836193883));
#37941=CARTESIAN_POINT('Ctrl Pts',(54.6544575558271,23.4273771715644,18.9757584663571));
#37942=CARTESIAN_POINT('Ctrl Pts',(54.7352791765095,23.4361595053712,18.971533313326));
#37943=CARTESIAN_POINT('Ctrl Pts',(54.8163084246817,23.44496440064,18.9672973060468));
#37944=CARTESIAN_POINT('Ctrl Pts',(54.8978681511069,23.4497320992601,18.9630612987676));
#37945=CARTESIAN_POINT('Ctrl Pts',(54.9795232618338,23.4504144451896,18.9588252914884));
#37946=CARTESIAN_POINT('Ctrl Pts',(55.0608226204942,23.4510938182988,18.9546077394942));
#37947=CARTESIAN_POINT('Ctrl Pts',(55.1422160662684,23.4477233502293,18.9503901875));
#37948=CARTESIAN_POINT('Ctrl Pts',(55.2232701464828,23.4403074994126,18.9461726355059));
#37949=CARTESIAN_POINT('Ctrl Pts',(55.3042974644839,23.4328940971412,18.9419564760514));
#37950=CARTESIAN_POINT('Ctrl Pts',(55.3849851768177,23.4214380069487,18.937740316597));
#37951=CARTESIAN_POINT('Ctrl Pts',(55.4649032139365,23.4059956882072,18.9335241571426));
#37952=CARTESIAN_POINT('Ctrl Pts',(55.5448193467704,23.3905537374248,18.9293080981507));
#37953=CARTESIAN_POINT('Ctrl Pts',(55.6239653845857,23.371125836238,18.9250920391587));
#37954=CARTESIAN_POINT('Ctrl Pts',(55.7019211569046,23.3478196139162,18.9208759801668));
#37955=CARTESIAN_POINT('Ctrl Pts',(55.7805150470274,23.3243226152739,18.9166254100384));
#37956=CARTESIAN_POINT('Ctrl Pts',(55.8578986313298,23.2968836313879,18.9123748399099));
#37957=CARTESIAN_POINT('Ctrl Pts',(55.9336584249708,23.2656637428094,18.9081242697814));
#37958=CARTESIAN_POINT('Ctrl Pts',(56.0089123640002,23.2346523120929,18.9039020810726));
#37959=CARTESIAN_POINT('Ctrl Pts',(56.0825637324469,23.1999105699802,18.8996798923639));
#37960=CARTESIAN_POINT('Ctrl Pts',(56.1542304951133,23.1616434058721,18.8954577036551));
#37961=CARTESIAN_POINT('Ctrl Pts',(56.2266198703669,23.1229903957536,18.8911929428168));
#37962=CARTESIAN_POINT('Ctrl Pts',(56.2969839767197,23.0807407202377,18.8869281819785));
#37963=CARTESIAN_POINT('Ctrl Pts',(56.3649592549612,23.0351502358047,18.8826634211401));
#37964=CARTESIAN_POINT('Ctrl Pts',(56.4329345332027,22.9895597513717,18.8783986603018));
#37965=CARTESIAN_POINT('Ctrl Pts',(56.4985206355842,22.9406287976213,18.8741338994635));
#37966=CARTESIAN_POINT('Ctrl Pts',(56.5613898697605,22.8886534686409,18.8698691386251));
#37967=CARTESIAN_POINT('Ctrl Pts',(56.6237646641009,22.837086903557,18.8656379183202));
#37968=CARTESIAN_POINT('Ctrl Pts',(56.6836990991716,22.7823303441399,18.8614066980153));
#37969=CARTESIAN_POINT('Ctrl Pts',(56.7408488812152,22.7246435639783,18.8571754777103));
#37970=CARTESIAN_POINT('Ctrl Pts',(56.7979167144712,22.667039502622,18.8529503246792));
#37971=CARTESIAN_POINT('Ctrl Pts',(56.8522075006449,22.6065138929718,18.848725171648));
#37972=CARTESIAN_POINT('Ctrl Pts',(56.9034099757883,22.5433666816637,18.8445000186169));
#37973=CARTESIAN_POINT('Ctrl Pts',(56.9547439880291,22.4800572477118,18.8402640113377));
#37974=CARTESIAN_POINT('Ctrl Pts',(57.0029734417368,22.4141130309847,18.8360280040585));
#37975=CARTESIAN_POINT('Ctrl Pts',(57.0478219570602,22.3458735015529,18.8317919967793));
#37976=CARTESIAN_POINT('Ctrl Pts',(57.0924750779757,22.2779312756628,18.8275744447852));
#37977=CARTESIAN_POINT('Ctrl Pts',(57.1337763951717,22.2077140821282,18.823356892791));
#37978=CARTESIAN_POINT('Ctrl Pts',(57.1714946272751,22.1355885406763,18.8191393407969));
#37979=CARTESIAN_POINT('Ctrl Pts',(57.2092004056763,22.0634868134374,18.8149231813424));
#37980=CARTESIAN_POINT('Ctrl Pts',(57.2433252330817,21.9894784012216,18.810707021888));
#37981=CARTESIAN_POINT('Ctrl Pts',(57.2736833555524,21.9139552771795,18.8064908624336));
#37982=CARTESIAN_POINT('Ctrl Pts',(57.3040407546505,21.8384339527004,18.8022748034417));
#37983=CARTESIAN_POINT('Ctrl Pts',(57.3306314548942,21.7613984199449,18.7980587444498));
#37984=CARTESIAN_POINT('Ctrl Pts',(57.3533180645943,21.6832600799506,18.7938426854579));
#37985=CARTESIAN_POINT('Ctrl Pts',(57.3761903786898,21.6044821277192,18.7895921153294));
#37986=CARTESIAN_POINT('Ctrl Pts',(57.3950942431044,21.5245836867684,18.785341545201));
#37987=CARTESIAN_POINT('Ctrl Pts',(57.4099408029048,21.4439995230792,18.7810909750725));
#37988=CARTESIAN_POINT('Ctrl Pts',(57.4246882309576,21.3639534267324,18.7768687863638));
#37989=CARTESIAN_POINT('Ctrl Pts',(57.4354323706634,21.2832312105769,18.772646597655));
#37990=CARTESIAN_POINT('Ctrl Pts',(57.4421382295174,21.2022649696059,18.7684244089463));
#37991=CARTESIAN_POINT('Ctrl Pts',(57.4489117032299,21.1204823498463,18.7641596481079));
#37992=CARTESIAN_POINT('Ctrl Pts',(57.4515649864324,21.0384512421352,18.7598948872696));
#37993=CARTESIAN_POINT('Ctrl Pts',(57.4501159290465,20.9566158527516,18.7556301264313));
#37994=CARTESIAN_POINT('Ctrl Pts',(57.4486668716607,20.874780463368,18.7513653655929));
#37995=CARTESIAN_POINT('Ctrl Pts',(57.4431155704733,20.793141268641,18.7471006047546));
#37996=CARTESIAN_POINT('Ctrl Pts',(57.4335331322646,20.7121341559499,18.7428358439163));
#37997=CARTESIAN_POINT('Ctrl Pts',(57.4240260558641,20.631764129809,18.7386046236113));
#37998=CARTESIAN_POINT('Ctrl Pts',(57.4105154173039,20.5517148952583,18.7343734033064));
#37999=CARTESIAN_POINT('Ctrl Pts',(57.3930328039482,20.4724165950035,18.7301421830015));
#38000=CARTESIAN_POINT('Ctrl Pts',(57.3755752594365,20.3932320029612,18.7259170299703));
#38001=CARTESIAN_POINT('Ctrl Pts',(57.3541571511383,20.3147966568229,18.7216918769392));
#38002=CARTESIAN_POINT('Ctrl Pts',(57.3288617307172,20.2375347291836,18.717466723908));
#38003=CARTESIAN_POINT('Ctrl Pts',(57.3035013273793,20.1600743187627,18.7132307166288));
#38004=CARTESIAN_POINT('Ctrl Pts',(57.2742437269267,20.0837938314776,18.7089947093496));
#38005=CARTESIAN_POINT('Ctrl Pts',(57.2412243049294,20.0091095595407,18.7047587020704));
#38006=CARTESIAN_POINT('Ctrl Pts',(57.2083487407692,19.9347506693691,18.7005411500763));
#38007=CARTESIAN_POINT('Ctrl Pts',(57.171744247155,19.8619745461055,18.6963235980821));
#38008=CARTESIAN_POINT('Ctrl Pts',(57.1315934651387,19.7911743097626,18.6921060460879));
#38009=CARTESIAN_POINT('Ctrl Pts',(57.0914559399972,19.7203974500471,18.6878898866335));
#38010=CARTESIAN_POINT('Ctrl Pts',(57.0477746808686,19.651595585791,18.6836737271791));
#38011=CARTESIAN_POINT('Ctrl Pts',(57.0007783176169,19.5851373304261,18.6794575677246));
#38012=CARTESIAN_POINT('Ctrl Pts',(56.9537830741934,19.5186806586267,18.6752415087327));
#38013=CARTESIAN_POINT('Ctrl Pts',(56.903473153044,19.4545678636454,18.6710254497408));
#38014=CARTESIAN_POINT('Ctrl Pts',(56.8501197310983,19.3931374574654,18.6668093907489));
#38015=CARTESIAN_POINT('Ctrl Pts',(56.7963295773054,19.3312042041617,18.6625588206204));
#38016=CARTESIAN_POINT('Ctrl Pts',(56.7394461691812,19.271997829198,18.658308250492));
#38017=CARTESIAN_POINT('Ctrl Pts',(56.679786633396,19.2158287312413,18.6540576803635));
#38018=CARTESIAN_POINT('Ctrl Pts',(56.6205254494258,19.160034679148,18.6498354916547));
#38019=CARTESIAN_POINT('Ctrl Pts',(56.5585254953154,19.1072377246015,18.645613302946));
#38020=CARTESIAN_POINT('Ctrl Pts',(56.4941308588617,19.0577015608828,18.6413911142372));
#38021=CARTESIAN_POINT('Ctrl Pts',(56.4290869343264,19.0076659263622,18.6371263533989));
#38022=CARTESIAN_POINT('Ctrl Pts',(56.3616001641577,18.9609574860517,18.6328615925606));
#38023=CARTESIAN_POINT('Ctrl Pts',(56.2920534648009,18.9178021001605,18.6285968317222));
#38024=CARTESIAN_POINT('Ctrl Pts',(56.2225067654441,18.8746467142693,18.6243320708839));
#38025=CARTESIAN_POINT('Ctrl Pts',(56.1509005896076,18.8350445597497,18.6200673100455));
#38026=CARTESIAN_POINT('Ctrl Pts',(56.0776397409345,18.7991722378254,18.6158025492072));
#38027=CARTESIAN_POINT('Ctrl Pts',(56.0049550577336,18.7635820364835,18.6115713289023));
#38028=CARTESIAN_POINT('Ctrl Pts',(55.9303690961449,18.7315297098856,18.6073401085974));
#38029=CARTESIAN_POINT('Ctrl Pts',(55.8542604046432,18.7032219499789,18.6031088882924));
#38030=CARTESIAN_POINT('Ctrl Pts',(55.7782608476783,18.6749547814186,18.5988837352613));
#38031=CARTESIAN_POINT('Ctrl Pts',(55.7007433294521,18.6504216761331,18.5946585822301));
#38032=CARTESIAN_POINT('Ctrl Pts',(55.6221093956525,18.6297826787738,18.590433429199));
#38033=CARTESIAN_POINT('Ctrl Pts',(55.5432734544425,18.609090660661,18.5861974219198));
#38034=CARTESIAN_POINT('Ctrl Pts',(55.4633157810082,18.592312985504,18.5819614146406));
#38035=CARTESIAN_POINT('Ctrl Pts',(55.3826595623816,18.5795616286883,18.5777254073614));
#38036=CARTESIAN_POINT('Ctrl Pts',(55.3023547438841,18.566865826528,18.5735078553672));
#38037=CARTESIAN_POINT('Ctrl Pts',(55.2213579151492,18.5581614135731,18.5692903033731));
#38038=CARTESIAN_POINT('Ctrl Pts',(55.1400984214831,18.5535080866069,18.5650727513789));
#38039=CARTESIAN_POINT('Ctrl Pts',(55.0588657578531,18.5488562960634,18.5608565919245));
#38040=CARTESIAN_POINT('Ctrl Pts',(54.9773710653145,18.548252961829,18.55664043247));
#38041=CARTESIAN_POINT('Ctrl Pts',(54.8960480340157,18.5517058512572,18.5524242730156));
#38042=CARTESIAN_POINT('Ctrl Pts',(54.81472694048,18.5551586584101,18.5482082140237));
#38043=CARTESIAN_POINT('Ctrl Pts',(54.7335779645077,18.5626674762272,18.5439921550318));
#38044=CARTESIAN_POINT('Ctrl Pts',(54.6530325738938,18.5741880008498,18.5397760960399));
#38045=CARTESIAN_POINT('Ctrl Pts',(54.5718278677954,18.5858028283272,18.5355255259115));
#38046=CARTESIAN_POINT('Ctrl Pts',(54.4912371512862,18.6014952904895,18.531274955783));
#38047=CARTESIAN_POINT('Ctrl Pts',(54.4116931853111,18.6211672312265,18.5270243856545));
#38048=CARTESIAN_POINT('Ctrl Pts',(54.3326803411896,18.6407078207353,18.5228021969458));
#38049=CARTESIAN_POINT('Ctrl Pts',(54.254700743462,18.6641747135276,18.518580008237));
#38050=CARTESIAN_POINT('Ctrl Pts',(54.178162528468,18.6914217751209,18.5143578195283));
#38051=CARTESIAN_POINT('Ctrl Pts',(54.1008525822625,18.718943567551,18.5100930586899));
#38052=CARTESIAN_POINT('Ctrl Pts',(54.0250136980734,18.7503220026461,18.5058282978516));
#38053=CARTESIAN_POINT('Ctrl Pts',(53.9510432772957,18.7853578068019,18.5015635370133));
#38054=CARTESIAN_POINT('Ctrl Pts',(53.877072856518,18.8203936109576,18.4972987761749));
#38055=CARTESIAN_POINT('Ctrl Pts',(53.8049712933018,18.8590864997399,18.4930340153366));
#38056=CARTESIAN_POINT('Ctrl Pts',(53.7351064676168,18.9011920998493,18.4887692544982));
#38057=CARTESIAN_POINT('Ctrl Pts',(53.665791099125,18.9429665572895,18.4845380341933));
#38058=CARTESIAN_POINT('Ctrl Pts',(53.5984174634729,18.9882568490248,18.4803068138884));
#38059=CARTESIAN_POINT('Ctrl Pts',(53.533364487795,19.0368569781243,18.4760755935835));
#38060=CARTESIAN_POINT('Ctrl Pts',(53.4684047935311,19.0853874180402,18.4718504405523));
#38061=CARTESIAN_POINT('Ctrl Pts',(53.4057595195666,19.1372179933486,18.4676252875211));
#38062=CARTESIAN_POINT('Ctrl Pts',(53.3457808679188,19.1920980908643,18.46340013449));
#38063=CARTESIAN_POINT('Ctrl Pts',(53.2856481335295,19.2471191731412,18.4591641272108));
#38064=CARTESIAN_POINT('Ctrl Pts',(53.2281961408405,19.3052052167382,18.4549281199316));
#38065=CARTESIAN_POINT('Ctrl Pts',(53.1737484367813,19.3660613604418,18.4506921126524));
#38066=CARTESIAN_POINT('Ctrl Pts',(53.1195379485322,19.4266523682746,18.4464745606582));
#38067=CARTESIAN_POINT('Ctrl Pts',(53.0683059436126,19.4899890459734,18.4422570086641));
#38068=CARTESIAN_POINT('Ctrl Pts',(53.0203353817722,19.5557430113249,18.4380394566699));
#38069=CARTESIAN_POINT('Ctrl Pts',(52.97238065872,19.6214752662129,18.4338232972155));
#38070=CARTESIAN_POINT('Ctrl Pts',(52.9276855140624,19.6896228484752,18.4296071377611));
#38071=CARTESIAN_POINT('Ctrl Pts',(52.8864916304736,19.7598255679374,18.4253909783066));
#38072=CARTESIAN_POINT('Ctrl Pts',(52.8452987284515,19.8300266146111,18.4211749193147));
#38073=CARTESIAN_POINT('Ctrl Pts',(52.8076071559581,19.9022822995731,18.4169588603229));
#38074=CARTESIAN_POINT('Ctrl Pts',(52.7736136385845,19.9762060658009,18.412742801331));
#38075=CARTESIAN_POINT('Ctrl Pts',(52.7393418625519,20.0507349452868,18.4084922312025));
#38076=CARTESIAN_POINT('Ctrl Pts',(52.7088291779766,20.1269589115716,18.404241661074));
#38077=CARTESIAN_POINT('Ctrl Pts',(52.6822277630573,20.2044611212155,18.3999910909455));
#38078=CARTESIAN_POINT('Ctrl Pts',(52.655803968057,20.2814458419873,18.3957689022368));
#38079=CARTESIAN_POINT('Ctrl Pts',(52.6332394407126,20.3596913199703,18.391546713528));
#38080=CARTESIAN_POINT('Ctrl Pts',(52.6146326940984,20.4387753872683,18.3873245248193));
#38081=CARTESIAN_POINT('Ctrl Pts',(52.5958383365359,20.5186568554863,18.383059763981));
#38082=CARTESIAN_POINT('Ctrl Pts',(52.5810821085045,20.5993934412349,18.3787950031426));
#38083=CARTESIAN_POINT('Ctrl Pts',(52.5704120529877,20.6805431833055,18.3745302423043));
#38084=CARTESIAN_POINT('Ctrl Pts',(52.559741997471,20.7616929253762,18.370265481466));
#38085=CARTESIAN_POINT('Ctrl Pts',(52.5531580891939,20.8432553383636,18.3660007206276));
#38086=CARTESIAN_POINT('Ctrl Pts',(52.5506544696196,20.9247888119655,18.3617359597893));
#38087=CARTESIAN_POINT('Ctrl Pts',(52.5498896509667,20.9496960790609,18.3604331385969));
#38088=CARTESIAN_POINT('Ctrl Pts',(52.549504741528,20.974615071646,18.3591303174045));
#38089=CARTESIAN_POINT('Ctrl Pts',(52.549500043536,20.9995380802805,18.3578274962121));
#38090=CARTESIAN_POINT('',(52.5495007596431,20.9980704896796,17.5578274962389));
#38091=CARTESIAN_POINT('Ctrl Pts',(52.5495000435359,20.9995380808101,18.3578274961844));
#38092=CARTESIAN_POINT('Ctrl Pts',(52.5494848634307,21.0800691517973,18.3536178284245));
#38093=CARTESIAN_POINT('Ctrl Pts',(52.5534437136658,21.1607581475281,18.3494081606647));
#38094=CARTESIAN_POINT('Ctrl Pts',(52.5613972293637,21.2411778950177,18.3451984929048));
#38095=CARTESIAN_POINT('Ctrl Pts',(52.5693394372043,21.3214833062722,18.3409948102117));
#38096=CARTESIAN_POINT('Ctrl Pts',(52.5812649878903,21.4015197655146,18.3367911275187));
#38097=CARTESIAN_POINT('Ctrl Pts',(52.5971425057765,21.4808597638128,18.3325874448257));
#38098=CARTESIAN_POINT('Ctrl Pts',(52.6130021184754,21.5601102898432,18.3283885026548));
#38099=CARTESIAN_POINT('Ctrl Pts',(52.6328047517819,21.6386654567809,18.324189560484));
#38100=CARTESIAN_POINT('Ctrl Pts',(52.6564673664993,21.716104074641,18.3199906183131));
#38101=CARTESIAN_POINT('Ctrl Pts',(52.680115551085,21.7934954682415,18.315794236776));
#38102=CARTESIAN_POINT('Ctrl Pts',(52.7076189086256,21.8697712155354,18.3115978552389));
#38103=CARTESIAN_POINT('Ctrl Pts',(52.7388438626034,21.944522721968,18.3074014737017));
#38104=CARTESIAN_POINT('Ctrl Pts',(52.7700595918591,22.0192521447211,18.3032063318927));
#38105=CARTESIAN_POINT('Ctrl Pts',(52.8049945533822,22.0924577871544,18.2990111900837));
#38106=CARTESIAN_POINT('Ctrl Pts',(52.8434666194345,22.163749985395,18.2948160482747));
#38107=CARTESIAN_POINT('Ctrl Pts',(52.8819394153157,22.235043536074,18.2906208268824));
#38108=CARTESIAN_POINT('Ctrl Pts',(52.9239492241089,22.3044231575566,18.28642560549));
#38109=CARTESIAN_POINT('Ctrl Pts',(52.969268164694,22.3715241387138,18.2822303840977));
#38110=CARTESIAN_POINT('Ctrl Pts',(53.0146326435224,22.4386925455603,18.2780309471829));
#38111=CARTESIAN_POINT('Ctrl Pts',(53.0633126302393,22.5035773495072,18.2738315102681));
#38112=CARTESIAN_POINT('Ctrl Pts',(53.1150374936316,22.5658437340888,18.2696320733533));
#38113=CARTESIAN_POINT('Ctrl Pts',(53.1667890131589,22.6281422073227,18.2654304722808));
#38114=CARTESIAN_POINT('Ctrl Pts',(53.2215882150173,22.6878192283477,18.2612288712084));
#38115=CARTESIAN_POINT('Ctrl Pts',(53.2791265630674,22.7445758407303,18.2570272701359));
#38116=CARTESIAN_POINT('Ctrl Pts',(53.3367653741261,22.8014315511968,18.2528183329911));
#38117=CARTESIAN_POINT('Ctrl Pts',(53.397152531953,22.8553563559036,18.2486093958463));
#38118=CARTESIAN_POINT('Ctrl Pts',(53.4599455767472,22.9060909273746,18.2444004587015));
#38119=CARTESIAN_POINT('Ctrl Pts',(53.508172636479,22.9450566952683,18.2411678608278));
#38120=CARTESIAN_POINT('Ctrl Pts',(53.5578181551207,22.9821414420203,18.237935262954));
#38121=CARTESIAN_POINT('Ctrl Pts',(53.6087162665811,23.0172456030746,18.2347026650802));
#38122=CARTESIAN_POINT('Ctrl Pts',(53.6753379532564,23.0631942316516,18.2304714447753));
#38123=CARTESIAN_POINT('Ctrl Pts',(53.7443632493421,23.1059250847526,18.2262402244704));
#38124=CARTESIAN_POINT('Ctrl Pts',(53.8154483383668,23.1451777574182,18.2220090041654));
#38125=CARTESIAN_POINT('Ctrl Pts',(53.8864314963489,23.1843741444985,18.2177838511343));
#38126=CARTESIAN_POINT('Ctrl Pts',(53.9594681776402,23.2201020337843,18.2135586981031));
#38127=CARTESIAN_POINT('Ctrl Pts',(54.0341849224833,23.252143753414,18.209333545072));
#38128=CARTESIAN_POINT('Ctrl Pts',(54.1090936116363,23.2842677869315,18.2050975377928));
#38129=CARTESIAN_POINT('Ctrl Pts',(54.1856906152162,23.312686424606,18.2008615305136));
#38130=CARTESIAN_POINT('Ctrl Pts',(54.2635739608335,23.3372263345336,18.1966255232344));
#38131=CARTESIAN_POINT('Ctrl Pts',(54.3411179870755,23.3616593298592,18.1924079712402));
#38132=CARTESIAN_POINT('Ctrl Pts',(54.419936726365,23.3822471759544,18.1881904192461));
#38133=CARTESIAN_POINT('Ctrl Pts',(54.4996143839329,23.3988673338126,18.1839728672519));
#38134=CARTESIAN_POINT('Ctrl Pts',(54.5792657337508,23.4154820040728,18.1797567077975));
#38135=CARTESIAN_POINT('Ctrl Pts',(54.6597749838983,23.428131492791,18.1755405483431));
#38136=CARTESIAN_POINT('Ctrl Pts',(54.7407143623583,23.4367439767265,18.1713243888886));
#38137=CARTESIAN_POINT('Ctrl Pts',(54.8216518121969,23.4453562554439,18.1671083298967));
#38138=CARTESIAN_POINT('Ctrl Pts',(54.9030189075409,23.4499316725456,18.1628922709049));
#38139=CARTESIAN_POINT('Ctrl Pts',(54.9843823731307,23.4504502320453,18.158676211913));
#38140=CARTESIAN_POINT('Ctrl Pts',(55.0664118506713,23.4509730362858,18.1544256417845));
#38141=CARTESIAN_POINT('Ctrl Pts',(55.1484371591545,23.4473722413147,18.150175071656));
#38142=CARTESIAN_POINT('Ctrl Pts',(55.2300157798258,23.4396809199219,18.1459245015275));
#38143=CARTESIAN_POINT('Ctrl Pts',(55.3110496930804,23.4320409541389,18.1417023128188));
#38144=CARTESIAN_POINT('Ctrl Pts',(55.3916424097103,23.4203650496643,18.13748012411));
#38145=CARTESIAN_POINT('Ctrl Pts',(55.4713686689262,23.4047373719296,18.1332579354013));
#38146=CARTESIAN_POINT('Ctrl Pts',(55.5518988042531,23.3889521210574,18.1289931745629));
#38147=CARTESIAN_POINT('Ctrl Pts',(55.6315444394973,23.3691350745922,18.1247284137246));
#38148=CARTESIAN_POINT('Ctrl Pts',(55.7098830716639,23.345424540369,18.1204636528863));
#38149=CARTESIAN_POINT('Ctrl Pts',(55.7882217038304,23.3217140061458,18.1161988920479));
#38150=CARTESIAN_POINT('Ctrl Pts',(55.8652529010369,23.2941102071775,18.1119341312096));
#38151=CARTESIAN_POINT('Ctrl Pts',(55.9405766869688,23.2628004211443,18.1076693703713));
#38152=CARTESIAN_POINT('Ctrl Pts',(56.0153080833027,23.2317368732859,18.1034381500663));
#38153=CARTESIAN_POINT('Ctrl Pts',(56.088639080374,23.196908979652,18.0992069297614));
#38154=CARTESIAN_POINT('Ctrl Pts',(56.1601644519263,23.1584644297478,18.0949757094565));
#38155=CARTESIAN_POINT('Ctrl Pts',(56.2315872611019,23.1200750066374,18.0907505564253));
#38156=CARTESIAN_POINT('Ctrl Pts',(56.3012091809258,23.0780794453609,18.0865254033942));
#38157=CARTESIAN_POINT('Ctrl Pts',(56.3686448177645,23.0326735135792,18.082300250363));
#38158=CARTESIAN_POINT('Ctrl Pts',(56.4362536940395,22.9871509357867,18.0780642430838));
#38159=CARTESIAN_POINT('Ctrl Pts',(56.5016646066119,22.9382006299537,18.0738282358047));
#38160=CARTESIAN_POINT('Ctrl Pts',(56.5645139576775,22.886066363157,18.0695922285255));
#38161=CARTESIAN_POINT('Ctrl Pts',(56.6270894889377,22.8341592330697,18.0653746765313));
#38162=CARTESIAN_POINT('Ctrl Pts',(56.6871253670562,22.7790961201122,18.0611571245371));
#38163=CARTESIAN_POINT('Ctrl Pts',(56.7442931774216,22.7211599464316,18.056939572543));
#38164=CARTESIAN_POINT('Ctrl Pts',(56.8014421122767,22.6632429019575,18.0527234130886));
#38165=CARTESIAN_POINT('Ctrl Pts',(56.8557245336385,22.6024550112615,18.0485072536341));
#38166=CARTESIAN_POINT('Ctrl Pts',(56.9068481457506,22.539116759394,18.0442910941797));
#38167=CARTESIAN_POINT('Ctrl Pts',(56.9579705396906,22.4757800167487,18.0400750351878));
#38168=CARTESIAN_POINT('Ctrl Pts',(57.0059339828864,22.4098933962318,18.0358589761959));
#38169=CARTESIAN_POINT('Ctrl Pts',(57.050486742696,22.3418101087813,18.031642917204));
#38170=CARTESIAN_POINT('Ctrl Pts',(57.0954041953105,22.2731695161231,18.0273923470756));
#38171=CARTESIAN_POINT('Ctrl Pts',(57.1368545934555,22.2022965209147,18.0231417769471));
#38172=CARTESIAN_POINT('Ctrl Pts',(57.1746257827272,22.1295808758553,18.0188912068186));
#38173=CARTESIAN_POINT('Ctrl Pts',(57.2121447705427,22.0573507593676,18.0146690181099));
#38174=CARTESIAN_POINT('Ctrl Pts',(57.2460333934679,21.9833029777984,18.0104468294011));
#38175=CARTESIAN_POINT('Ctrl Pts',(57.2761317845893,21.9078404866398,18.0062246406924));
#38176=CARTESIAN_POINT('Ctrl Pts',(57.3065336563686,21.8316171107425,18.001959879854));
#38177=CARTESIAN_POINT('Ctrl Pts',(57.3330682756203,21.753950795488,17.9976951190157));
#38178=CARTESIAN_POINT('Ctrl Pts',(57.3556227631297,21.6752715363655,17.9934303581774));
#38179=CARTESIAN_POINT('Ctrl Pts',(57.378177250639,21.596592277243,17.989165597339));
#38180=CARTESIAN_POINT('Ctrl Pts',(57.3967515596131,21.5169005580579,17.9849008365007));
#38181=CARTESIAN_POINT('Ctrl Pts',(57.4112861714913,21.4366339991052,17.9806360756623));
#38182=CARTESIAN_POINT('Ctrl Pts',(57.4257064748177,21.3569987025619,17.9764048553574));
#38183=CARTESIAN_POINT('Ctrl Pts',(57.4362045146124,21.2764989605317,17.9721736350525));
#38184=CARTESIAN_POINT('Ctrl Pts',(57.4426846622965,21.1955553389236,17.9679424147476));
#38185=CARTESIAN_POINT('Ctrl Pts',(57.4491555179023,21.1147277848037,17.9637172617164));
#38186=CARTESIAN_POINT('Ctrl Pts',(57.4516198871339,21.0334580747564,17.9594921086853));
#38187=CARTESIAN_POINT('Ctrl Pts',(57.4500332920609,20.9521761796451,17.9552669556541));
#38188=CARTESIAN_POINT('Ctrl Pts',(57.448442621089,20.8706854746175,17.9510309483749));
#38189=CARTESIAN_POINT('Ctrl Pts',(57.4427800678572,20.7891829874432,17.9467949410957));
#38190=CARTESIAN_POINT('Ctrl Pts',(57.4330533034165,20.7081064016906,17.9425589338165));
#38191=CARTESIAN_POINT('Ctrl Pts',(57.4233689161953,20.6273830475076,17.9383413818223));
#38192=CARTESIAN_POINT('Ctrl Pts',(57.409655705143,20.5470823568963,17.9341238298282));
#38193=CARTESIAN_POINT('Ctrl Pts',(57.391973317881,20.4676336819958,17.929906277834));
#38194=CARTESIAN_POINT('Ctrl Pts',(57.374296768941,20.3882112392403,17.9256901183796));
#38195=CARTESIAN_POINT('Ctrl Pts',(57.3526537472474,20.3096407070026,17.9214739589252));
#38196=CARTESIAN_POINT('Ctrl Pts',(57.3271550465332,20.2323414565087,17.9172577994707));
#38197=CARTESIAN_POINT('Ctrl Pts',(57.3016569534014,20.1550440478995,17.9130417404788));
#38198=CARTESIAN_POINT('Ctrl Pts',(57.2723035106134,20.0790183019785,17.908825681487));
#38199=CARTESIAN_POINT('Ctrl Pts',(57.2392550035574,20.0046672520996,17.9046096224951));
#38200=CARTESIAN_POINT('Ctrl Pts',(57.2059359733557,19.9297075913728,17.9003590523666));
#38201=CARTESIAN_POINT('Ctrl Pts',(57.1688612869247,19.8564506150345,17.8961084822381));
#38202=CARTESIAN_POINT('Ctrl Pts',(57.1282433935176,19.7852859151436,17.8918579121096));
#38203=CARTESIAN_POINT('Ctrl Pts',(57.0878967092534,19.7145963880308,17.8876357234009));
#38204=CARTESIAN_POINT('Ctrl Pts',(57.0440542953745,19.6459716442108,17.8834135346921));
#38205=CARTESIAN_POINT('Ctrl Pts',(56.9969680460069,19.5797645007861,17.8791913459834));
#38206=CARTESIAN_POINT('Ctrl Pts',(56.9494070282081,19.5128897938574,17.874926585145));
#38207=CARTESIAN_POINT('Ctrl Pts',(56.8985366929528,19.4484820960638,17.8706618243067));
#38208=CARTESIAN_POINT('Ctrl Pts',(56.8446571320856,19.3868694054585,17.8663970634683));
#38209=CARTESIAN_POINT('Ctrl Pts',(56.7907775712184,19.3252567148533,17.86213230263));
#38210=CARTESIAN_POINT('Ctrl Pts',(56.7338891658774,19.266439333083,17.8578675417917));
#38211=CARTESIAN_POINT('Ctrl Pts',(56.6743273478505,19.2107045570281,17.8536027809533));
#38212=CARTESIAN_POINT('Ctrl Pts',(56.6152339582357,19.1554081113249,17.8493715606484));
#38213=CARTESIAN_POINT('Ctrl Pts',(56.5532874940088,19.1029385689575,17.8451403403435));
#38214=CARTESIAN_POINT('Ctrl Pts',(56.4887894776188,19.0536043204601,17.8409091200385));
#38215=CARTESIAN_POINT('Ctrl Pts',(56.4243839468701,19.0043408138221,17.8366839670074));
#38216=CARTESIAN_POINT('Ctrl Pts',(56.3574344966697,18.9582039521519,17.8324588139762));
#38217=CARTESIAN_POINT('Ctrl Pts',(56.2882782868407,18.9154642469714,17.8282336609451));
#38218=CARTESIAN_POINT('Ctrl Pts',(56.2189444174929,18.8726147452088,17.8239976536659));
#38219=CARTESIAN_POINT('Ctrl Pts',(56.1473927848897,18.8331801944124,17.8197616463867));
#38220=CARTESIAN_POINT('Ctrl Pts',(56.0739953056582,18.7973914706821,17.8155256391075));
#38221=CARTESIAN_POINT('Ctrl Pts',(56.0009176019396,18.7617586699835,17.8113080871133));
#38222=CARTESIAN_POINT('Ctrl Pts',(55.9260105188456,18.7297402069917,17.8070905351192));
#38223=CARTESIAN_POINT('Ctrl Pts',(55.849667155473,18.7015187677707,17.802872983125));
#38224=CARTESIAN_POINT('Ctrl Pts',(55.7733489989423,18.6733066466269,17.7986568236706));
#38225=CARTESIAN_POINT('Ctrl Pts',(55.695595939619,18.6488892206766,17.7944406642161));
#38226=CARTESIAN_POINT('Ctrl Pts',(55.6168204228227,18.628400789343,17.7902245047617));
#38227=CARTESIAN_POINT('Ctrl Pts',(55.5380467830875,18.6079128462073,17.7860084457698));
#38228=CARTESIAN_POINT('Ctrl Pts',(55.4582511845508,18.5913538275009,17.7817923867779));
#38229=CARTESIAN_POINT('Ctrl Pts',(55.3778591803299,18.5788075892568,17.777576327786));
#38230=CARTESIAN_POINT('Ctrl Pts',(55.2968091161902,18.5661586520366,17.7733257576575));
#38231=CARTESIAN_POINT('Ctrl Pts',(55.2151533088805,18.5575885826804,17.7690751875291));
#38232=CARTESIAN_POINT('Ctrl Pts',(55.1333343020533,18.5531301191326,17.7648246174006));
#38233=CARTESIAN_POINT('Ctrl Pts',(55.0520616077217,18.5487014251267,17.7606024286918));
#38234=CARTESIAN_POINT('Ctrl Pts',(54.9706283564138,18.5483295373821,17.7563802399831));
#38235=CARTESIAN_POINT('Ctrl Pts',(54.8894675800346,18.5519941106818,17.7521580512743));
#38236=CARTESIAN_POINT('Ctrl Pts',(54.8074884633756,18.5556956337012,17.747893290436));
#38237=CARTESIAN_POINT('Ctrl Pts',(54.7257878308633,18.5635154285282,17.7436285295977));
#38238=CARTESIAN_POINT('Ctrl Pts',(54.6448039944149,18.5753791950871,17.7393637687593));
#38239=CARTESIAN_POINT('Ctrl Pts',(54.5638201579666,18.587242961646,17.735099007921));
#38240=CARTESIAN_POINT('Ctrl Pts',(54.4835535776978,18.6031505432506,17.7308342470827));
#38241=CARTESIAN_POINT('Ctrl Pts',(54.4044275290499,18.6229758768901,17.7265694862443));
#38242=CARTESIAN_POINT('Ctrl Pts',(54.3259237731819,18.6426452926973,17.7223382659394));
#38243=CARTESIAN_POINT('Ctrl Pts',(54.2482482821312,18.6662447714308,17.7181070456345));
#38244=CARTESIAN_POINT('Ctrl Pts',(54.171823668589,18.6936881793455,17.7138758253295));
#38245=CARTESIAN_POINT('Ctrl Pts',(54.0955086425936,18.7210922353341,17.7096506722984));
#38246=CARTESIAN_POINT('Ctrl Pts',(54.0204413656159,18.7523291176063,17.7054255192672));
#38247=CARTESIAN_POINT('Ctrl Pts',(53.9470319464238,18.7872622098071,17.7012003662361));
#38248=CARTESIAN_POINT('Ctrl Pts',(53.8734339413892,18.8222850437153,17.6969643589569));
#38249=CARTESIAN_POINT('Ctrl Pts',(53.8015027792818,18.8610229817423,17.6927283516777));
#38250=CARTESIAN_POINT('Ctrl Pts',(53.7316341116842,18.9032887124459,17.6884923443985));
#38251=CARTESIAN_POINT('Ctrl Pts',(53.662069845399,18.9453703013254,17.6842747924043));
#38252=CARTESIAN_POINT('Ctrl Pts',(53.5945505440541,18.9909487722947,17.6800572404101));
#38253=CARTESIAN_POINT('Ctrl Pts',(53.5294428538567,19.0397928859616,17.675839688416));
#38254=CARTESIAN_POINT('Ctrl Pts',(53.4643566607375,19.0886208724133,17.6716235289616));
#38255=CARTESIAN_POINT('Ctrl Pts',(53.4016808691158,19.1407120815445,17.6674073695071));
#38256=CARTESIAN_POINT('Ctrl Pts',(53.3417519589761,19.195792782289,17.6631912100527));
#38257=CARTESIAN_POINT('Ctrl Pts',(53.281824476821,19.250872170572,17.6589751510608));
#38258=CARTESIAN_POINT('Ctrl Pts',(53.2246440875646,19.3089405934097,17.6547590920689));
#38259=CARTESIAN_POINT('Ctrl Pts',(53.1705119942051,19.3696859545927,17.650543033077));
#38260=CARTESIAN_POINT('Ctrl Pts',(53.1159367950752,19.4309285553684,17.6462924629485));
#38261=CARTESIAN_POINT('Ctrl Pts',(53.0644603578258,19.4948917742077,17.6420418928201));
#38262=CARTESIAN_POINT('Ctrl Pts',(53.0163501468682,19.5612215215085,17.6377913226916));
#38263=CARTESIAN_POINT('Ctrl Pts',(52.9685611718975,19.6271083794225,17.6335691339828));
#38264=CARTESIAN_POINT('Ctrl Pts',(52.9240938115442,19.6953298319304,17.6293469452741));
#38265=CARTESIAN_POINT('Ctrl Pts',(52.8831657703922,19.7655109986877,17.6251247565653));
#38266=CARTESIAN_POINT('Ctrl Pts',(52.8418250537321,19.8363997988388,17.620859995727));
#38267=CARTESIAN_POINT('Ctrl Pts',(52.8040956548996,19.9092876236642,17.6165952348887));
#38268=CARTESIAN_POINT('Ctrl Pts',(52.7701528066361,19.9837659008637,17.6123304740504));
#38269=CARTESIAN_POINT('Ctrl Pts',(52.7362099583727,20.0582441780633,17.608065713212));
#38270=CARTESIAN_POINT('Ctrl Pts',(52.7060537785096,20.1343124360727,17.6038009523737));
#38271=CARTESIAN_POINT('Ctrl Pts',(52.6798078536335,20.2115466697773,17.5995361915354));
#38272=CARTESIAN_POINT('Ctrl Pts',(52.6490720914104,20.3019932078146,17.594541866676));
#38273=CARTESIAN_POINT('Ctrl Pts',(52.6236031156726,20.394314844502,17.5895475418167));
#38274=CARTESIAN_POINT('Ctrl Pts',(52.6035969650079,20.4879426361423,17.5845532169573));
#38275=CARTESIAN_POINT('Ctrl Pts',(52.5837963477951,20.5806085414351,17.5796102013601));
#38276=CARTESIAN_POINT('Ctrl Pts',(52.5693469521956,20.6745538000929,17.5746671857628));
#38277=CARTESIAN_POINT('Ctrl Pts',(52.5603925777194,20.7692059897799,17.5697241701655));
#38278=CARTESIAN_POINT('Ctrl Pts',(52.55320888784,20.8451411630212,17.56575861219));
#38279=CARTESIAN_POINT('Ctrl Pts',(52.5495610265067,20.9215309128402,17.5617930542144));
#38280=CARTESIAN_POINT('Ctrl Pts',(52.5495007596431,20.9980704896796,17.5578274962389));
#38281=CARTESIAN_POINT('',(52.5495004847658,21.0015413750748,16.7578274961829));
#38282=CARTESIAN_POINT('Ctrl Pts',(52.5495007596427,20.9980704901969,17.5578274962121));
#38283=CARTESIAN_POINT('Ctrl Pts',(52.5494367772744,21.0793288204041,17.5536174570045));
#38284=CARTESIAN_POINT('Ctrl Pts',(52.5534188806965,21.1606384794744,17.5494074177969));
#38285=CARTESIAN_POINT('Ctrl Pts',(52.5614357122365,21.2415666873648,17.5451973785892));
#38286=CARTESIAN_POINT('Ctrl Pts',(52.5694509585329,21.3224788925592,17.5409881718723));
#38287=CARTESIAN_POINT('Ctrl Pts',(52.5814993023512,21.403009332813,17.5367789651553));
#38288=CARTESIAN_POINT('Ctrl Pts',(52.5975174476653,21.4827295679027,17.5325697584384));
#38289=CARTESIAN_POINT('Ctrl Pts',(52.6135373592028,21.5624585932572,17.5283600875979));
#38290=CARTESIAN_POINT('Ctrl Pts',(52.6335278482383,21.6413767794714,17.5241504167573));
#38291=CARTESIAN_POINT('Ctrl Pts',(52.6573746430645,21.7190665386757,17.5199407459168));
#38292=CARTESIAN_POINT('Ctrl Pts',(52.6812481566356,21.7968433440793,17.5157263584205));
#38293=CARTESIAN_POINT('Ctrl Pts',(52.7089864656818,21.8733885280204,17.5115119709242));
#38294=CARTESIAN_POINT('Ctrl Pts',(52.7404257598847,21.9483008506836,17.507297583428));
#38295=CARTESIAN_POINT('Ctrl Pts',(52.7718833922335,22.023256868765,17.5030807377324));
#38296=CARTESIAN_POINT('Ctrl Pts',(52.8070461054362,22.0965777093617,17.4988638920367));
#38297=CARTESIAN_POINT('Ctrl Pts',(52.8457034792493,22.1678855897224,17.4946470463411));
#38298=CARTESIAN_POINT('Ctrl Pts',(52.8844312239934,22.239323277192,17.4904225244035));
#38299=CARTESIAN_POINT('Ctrl Pts',(52.9266660919556,22.3087402878762,17.4861980024658));
#38300=CARTESIAN_POINT('Ctrl Pts',(52.9721537441947,22.3757869794472,17.4819734805281));
#38301=CARTESIAN_POINT('Ctrl Pts',(53.0061453314308,22.4258890039142,17.4788166192942));
#38302=CARTESIAN_POINT('Ctrl Pts',(53.0419524019041,22.474668009185,17.4756597580604));
#38303=CARTESIAN_POINT('Ctrl Pts',(53.0794547754144,22.5219908969247,17.4725028968265));
#38304=CARTESIAN_POINT('Ctrl Pts',(53.1297201474162,22.5854189505058,17.4682716765215));
#38305=CARTESIAN_POINT('Ctrl Pts',(53.183225307717,22.6464731487859,17.4640404562166));
#38306=CARTESIAN_POINT('Ctrl Pts',(53.2397176596797,22.7048038985046,17.4598092359117));
#38307=CARTESIAN_POINT('Ctrl Pts',(53.2961290055637,22.7630510060108,17.4555840828805));
#38308=CARTESIAN_POINT('Ctrl Pts',(53.355518715193,22.8185820898921,17.4513589298494));
#38309=CARTESIAN_POINT('Ctrl Pts',(53.4175933442892,22.8710797486911,17.4471337768182));
#38310=CARTESIAN_POINT('Ctrl Pts',(53.4798274406086,22.9237122718622,17.442897769539));
#38311=CARTESIAN_POINT('Ctrl Pts',(53.5447599707556,22.9732953985627,17.4386617622598));
#38312=CARTESIAN_POINT('Ctrl Pts',(53.6120572539298,23.0195457864656,17.4344257549806));
#38313=CARTESIAN_POINT('Ctrl Pts',(53.679061338707,23.0655946723323,17.4302082029865));
#38314=CARTESIAN_POINT('Ctrl Pts',(53.7484092331817,23.108339527016,17.4259906509923));
#38315=CARTESIAN_POINT('Ctrl Pts',(53.8197391798873,23.1475415354556,17.4217730989982));
#38316=CARTESIAN_POINT('Ctrl Pts',(53.8910455750672,23.1867306002838,17.4175569395437));
#38317=CARTESIAN_POINT('Ctrl Pts',(53.9643323157518,23.2223789181121,17.4133407800893));
#38318=CARTESIAN_POINT('Ctrl Pts',(54.0392113547849,23.2542926671632,17.4091246206349));
#38319=CARTESIAN_POINT('Ctrl Pts',(54.1140886096023,23.2862056557744,17.404908561643));
#38320=CARTESIAN_POINT('Ctrl Pts',(54.1905576592002,23.314384071272,17.4006925026511));
#38321=CARTESIAN_POINT('Ctrl Pts',(54.2682100323667,23.3386820419354,17.3964764436592));
#38322=CARTESIAN_POINT('Ctrl Pts',(54.3464980398213,23.3631789070133,17.3922258735307));
#38323=CARTESIAN_POINT('Ctrl Pts',(54.4259883797476,23.3837313476125,17.3879753034022));
#38324=CARTESIAN_POINT('Ctrl Pts',(54.5062482170537,23.4002415351038,17.3837247332737));
#38325=CARTESIAN_POINT('Ctrl Pts',(54.5859721525723,23.4166414826633,17.379502544565));
#38326=CARTESIAN_POINT('Ctrl Pts',(54.6664548673223,23.4290529831988,17.3752803558562));
#38327=CARTESIAN_POINT('Ctrl Pts',(54.747265082537,23.4374321142331,17.3710581671475));
#38328=CARTESIAN_POINT('Ctrl Pts',(54.82889010334,23.4458957316504,17.3667934063091));
#38329=CARTESIAN_POINT('Ctrl Pts',(54.9108487810094,23.4502451797474,17.3625286454708));
#38330=CARTESIAN_POINT('Ctrl Pts',(54.9926966350904,23.4504891166583,17.3582638846324));
#38331=CARTESIAN_POINT('Ctrl Pts',(55.0745444891714,23.4507330535693,17.3539991237941));
#38332=CARTESIAN_POINT('Ctrl Pts',(55.1562810414348,23.4468715662079,17.3497343629558));
#38333=CARTESIAN_POINT('Ctrl Pts',(55.2374690269802,23.4389667302415,17.3454696021174));
#38334=CARTESIAN_POINT('Ctrl Pts',(55.3180185034872,23.4311240624541,17.3412383818125));
#38335=CARTESIAN_POINT('Ctrl Pts',(55.3983300667665,23.4192720537597,17.3370071615076));
#38336=CARTESIAN_POINT('Ctrl Pts',(55.4779730127825,23.4034333876876,17.3327759412026));
#38337=CARTESIAN_POINT('Ctrl Pts',(55.5575017563879,23.3876174331542,17.3285507881715));
#38338=CARTESIAN_POINT('Ctrl Pts',(55.6363633347351,23.3678262647335,17.3243256351403));
#38339=CARTESIAN_POINT('Ctrl Pts',(55.7141319439969,23.3441343426867,17.3201004821092));
#38340=CARTESIAN_POINT('Ctrl Pts',(55.7921003376853,23.3203815570459,17.31586447483));
#38341=CARTESIAN_POINT('Ctrl Pts',(55.8689696703445,23.2927080024995,17.3116284675508));
#38342=CARTESIAN_POINT('Ctrl Pts',(55.9443209387124,23.2612404150619,17.3073924602716));
#38343=CARTESIAN_POINT('Ctrl Pts',(56.0193439193687,23.2299099244841,17.3031749082774));
#38344=CARTESIAN_POINT('Ctrl Pts',(56.0928616009562,23.1948185642367,17.2989573562833));
#38345=CARTESIAN_POINT('Ctrl Pts',(56.1644771698154,23.1561408049983,17.2947398042891));
#38346=CARTESIAN_POINT('Ctrl Pts',(56.2360690928429,23.1174758162761,17.2905236448347));
#38347=CARTESIAN_POINT('Ctrl Pts',(56.305759741577,23.0752270008704,17.2863074853803));
#38348=CARTESIAN_POINT('Ctrl Pts',(56.3731758524629,23.0296153153277,17.2820913259258));
#38349=CARTESIAN_POINT('Ctrl Pts',(56.4405903569595,22.984004716619,17.2778752669339));
#38350=CARTESIAN_POINT('Ctrl Pts',(56.5057300469187,22.9350316685375,17.273659207942));
#38351=CARTESIAN_POINT('Ctrl Pts',(56.5682508737503,22.8829602882115,17.2694431489501));
#38352=CARTESIAN_POINT('Ctrl Pts',(56.6312834734953,22.8304626703681,17.2651925788217));
#38353=CARTESIAN_POINT('Ctrl Pts',(56.6916537591947,22.774816057167,17.2609420086932));
#38354=CARTESIAN_POINT('Ctrl Pts',(56.7490448391351,22.7163310871434,17.2566914385647));
#38355=CARTESIAN_POINT('Ctrl Pts',(56.8060527139339,22.6582366262589,17.252469249856));
#38356=CARTESIAN_POINT('Ctrl Pts',(56.8601207811346,22.597341989153,17.2482470611472));
#38357=CARTESIAN_POINT('Ctrl Pts',(56.9109782867531,22.533985735774,17.2440248724385));
#38358=CARTESIAN_POINT('Ctrl Pts',(56.9623485862017,22.4699906642809,17.2397601116001));
#38359=CARTESIAN_POINT('Ctrl Pts',(57.0104429311022,22.40348445004,17.2354953507618));
#38360=CARTESIAN_POINT('Ctrl Pts',(57.0550275893164,22.3348452558811,17.2312305899234));
#38361=CARTESIAN_POINT('Ctrl Pts',(57.0996122475307,22.2662060617222,17.2269658290851));
#38362=CARTESIAN_POINT('Ctrl Pts',(57.1406870327804,22.1954343365968,17.2227010682468));
#38363=CARTESIAN_POINT('Ctrl Pts',(57.1780670086594,22.1229311447233,17.2184363074084));
#38364=CARTESIAN_POINT('Ctrl Pts',(57.2151530068976,22.050998159673,17.2142050871035));
#38365=CARTESIAN_POINT('Ctrl Pts',(57.2487412133422,21.9770911255402,17.2099738667986));
#38366=CARTESIAN_POINT('Ctrl Pts',(57.2786171503632,21.9015842345953,17.2057426464936));
#38367=CARTESIAN_POINT('Ctrl Pts',(57.3084502473815,21.8261856152472,17.2015174934625));
#38368=CARTESIAN_POINT('Ctrl Pts',(57.3345814775107,21.7491921239713,17.1972923404313));
#38369=CARTESIAN_POINT('Ctrl Pts',(57.3568425247626,21.6710019101842,17.1930671874002));
#38370=CARTESIAN_POINT('Ctrl Pts',(57.3791607597486,21.5926108288857,17.188831180121));
#38371=CARTESIAN_POINT('Ctrl Pts',(57.3975886911264,21.5130172910209,17.1845951728418));
#38372=CARTESIAN_POINT('Ctrl Pts',(57.4120056142599,21.4326420769861,17.1803591655626));
#38373=CARTESIAN_POINT('Ctrl Pts',(57.4263597262582,21.3526170388096,17.1761416135684));
#38374=CARTESIAN_POINT('Ctrl Pts',(57.4367376165063,21.2718175804945,17.1719240615743));
#38375=CARTESIAN_POINT('Ctrl Pts',(57.4430707204082,21.1906717207252,17.1677065095801));
#38376=CARTESIAN_POINT('Ctrl Pts',(57.4494017332632,21.1095526534727,17.1634903501257));
#38377=CARTESIAN_POINT('Ctrl Pts',(57.4516905757335,21.0280878750446,17.1592741906712));
#38378=CARTESIAN_POINT('Ctrl Pts',(57.4499205116746,20.9467108221472,17.1550580312168));
#38379=CARTESIAN_POINT('Ctrl Pts',(57.4481504897927,20.8653357083001,17.1508419722249));
#38380=CARTESIAN_POINT('Ctrl Pts',(57.4423217648956,20.7840487806151,17.146625913233));
#38381=CARTESIAN_POINT('Ctrl Pts',(57.4324697068783,20.7032823309619,17.1424098542411));
#38382=CARTESIAN_POINT('Ctrl Pts',(57.4225370034714,20.6218547563151,17.1381592841126));
#38383=CARTESIAN_POINT('Ctrl Pts',(57.408514837968,20.5409566980519,17.1339087139841));
#38384=CARTESIAN_POINT('Ctrl Pts',(57.390492394246,20.461022854796,17.1296581438557));
#38385=CARTESIAN_POINT('Ctrl Pts',(57.3725902879197,20.3816227366374,17.1254359551469));
#38386=CARTESIAN_POINT('Ctrl Pts',(57.3507413466095,20.3031744321134,17.1212137664382));
#38387=CARTESIAN_POINT('Ctrl Pts',(57.3250832316369,20.2260890128955,17.1169915777294));
#38388=CARTESIAN_POINT('Ctrl Pts',(57.2991664071013,20.1482263450319,17.1127268168911));
#38389=CARTESIAN_POINT('Ctrl Pts',(57.2693633375133,20.0717546536215,17.1084620560528));
#38390=CARTESIAN_POINT('Ctrl Pts',(57.2358650339893,19.9970753768183,17.1041972952144));
#38391=CARTESIAN_POINT('Ctrl Pts',(57.2023667304652,19.9223961000151,17.0999325343761));
#38392=CARTESIAN_POINT('Ctrl Pts',(57.1651734692259,19.849509637768,17.0956677735378));
#38393=CARTESIAN_POINT('Ctrl Pts',(57.1245219620561,19.7787888459642,17.0914030126994));
#38394=CARTESIAN_POINT('Ctrl Pts',(57.0841901617316,19.7086242431636,17.0871717923945));
#38395=CARTESIAN_POINT('Ctrl Pts',(57.0403031164513,19.6403282362304,17.0829405720896));
#38396=CARTESIAN_POINT('Ctrl Pts',(56.9930589413419,19.5742839320758,17.0787093517847));
#38397=CARTESIAN_POINT('Ctrl Pts',(56.9458825110729,19.5083343308308,17.0744841987535));
#38398=CARTESIAN_POINT('Ctrl Pts',(56.8953587799322,19.4446303947001,17.0702590457223));
#38399=CARTESIAN_POINT('Ctrl Pts',(56.8417310225385,19.3835294340386,17.0660338926912));
#38400=CARTESIAN_POINT('Ctrl Pts',(56.787965497595,19.3222715074691,17.061797885412));
#38401=CARTESIAN_POINT('Ctrl Pts',(56.731080218543,19.2636303533888,17.0575618781328));
#38402=CARTESIAN_POINT('Ctrl Pts',(56.6713632912655,19.2079355484218,17.0533258708536));
#38403=CARTESIAN_POINT('Ctrl Pts',(56.6119065365613,19.1524833925895,17.0491083188594));
#38404=CARTESIAN_POINT('Ctrl Pts',(56.5496430924026,19.0999522914064,17.0448907668653));
#38405=CARTESIAN_POINT('Ctrl Pts',(56.4848954180064,19.0506319363487,17.0406732148711));
#38406=CARTESIAN_POINT('Ctrl Pts',(56.4201691218193,19.0013278657502,17.0364570554167));
#38407=CARTESIAN_POINT('Ctrl Pts',(56.3529605938229,18.9552327175379,17.0322408959622));
#38408=CARTESIAN_POINT('Ctrl Pts',(56.2836249481658,18.9125955728593,17.0280247365078));
#38409=CARTESIAN_POINT('Ctrl Pts',(56.2142909546365,18.8699594441375,17.0238086775159));
#38410=CARTESIAN_POINT('Ctrl Pts',(56.1428303408352,18.8307813977141,17.019592618524));
#38411=CARTESIAN_POINT('Ctrl Pts',(56.0696255120111,18.7952661126442,17.0153765595321));
#38412=CARTESIAN_POINT('Ctrl Pts',(55.9958214548911,18.7594601122746,17.0111259894036));
#38413=CARTESIAN_POINT('Ctrl Pts',(55.9202449205161,18.7273773379552,17.0068754192751));
#38414=CARTESIAN_POINT('Ctrl Pts',(55.8433095154918,18.6991785573233,17.0026248491467));
#38415=CARTESIAN_POINT('Ctrl Pts',(55.7668878147366,18.6711680623577,16.9984026604379));
#38416=CARTESIAN_POINT('Ctrl Pts',(55.6891258013491,18.6469899318883,16.9941804717292));
#38417=CARTESIAN_POINT('Ctrl Pts',(55.6104435152623,18.6267513900406,16.9899582830204));
#38418=CARTESIAN_POINT('Ctrl Pts',(55.5309678793967,18.6063087839302,16.9856935221821));
#38419=CARTESIAN_POINT('Ctrl Pts',(55.4505537842166,18.5898857561827,16.9814287613438));
#38420=CARTESIAN_POINT('Ctrl Pts',(55.3696421026568,18.5775394810351,16.9771640005054));
#38421=CARTESIAN_POINT('Ctrl Pts',(55.2887304210971,18.5651932058876,16.9728992396671));
#38422=CARTESIAN_POINT('Ctrl Pts',(55.2073216389819,18.5569236681106,16.9686344788288));
#38423=CARTESIAN_POINT('Ctrl Pts',(55.125857393315,18.5527341446937,16.9643697179904));
#38424=CARTESIAN_POINT('Ctrl Pts',(55.0450338293549,18.5485775700999,16.9601384976855));
#38425=CARTESIAN_POINT('Ctrl Pts',(54.9638525942866,18.5484214315561,16.9559072773806));
#38426=CARTESIAN_POINT('Ctrl Pts',(54.8827430104361,18.5523069946584,16.9516760570757));
#38427=CARTESIAN_POINT('Ctrl Pts',(54.8017497320516,18.556186986135,16.9474509040445));
#38428=CARTESIAN_POINT('Ctrl Pts',(54.7208283613012,18.5640971468667,16.9432257510133));
#38429=CARTESIAN_POINT('Ctrl Pts',(54.6404110317942,18.5760268103907,16.9390005979822));
#38430=CARTESIAN_POINT('Ctrl Pts',(54.5597871134052,18.58798712074,16.934764590703));
#38431=CARTESIAN_POINT('Ctrl Pts',(54.4796703010171,18.6039876300277,16.9305285834238));
#38432=CARTESIAN_POINT('Ctrl Pts',(54.4004937338682,18.6239649651428,16.9262925761446));
#38433=CARTESIAN_POINT('Ctrl Pts',(54.3216621203559,18.6438552637186,16.9220750241504));
#38434=CARTESIAN_POINT('Ctrl Pts',(54.24376303197,18.6676877016687,16.9178574721563));
#38435=CARTESIAN_POINT('Ctrl Pts',(54.1672147221646,18.6953484143974,16.9136399201621));
#38436=CARTESIAN_POINT('Ctrl Pts',(54.0906916868695,18.7229999941881,16.9094237607077));
#38437=CARTESIAN_POINT('Ctrl Pts',(54.0155189813761,18.7544771807362,16.9052076012532));
#38438=CARTESIAN_POINT('Ctrl Pts',(53.9420984431211,18.7896166518106,16.9009914417988));
#38439=CARTESIAN_POINT('Ctrl Pts',(53.8686796543287,18.8247552855825,16.8967753828069));
#38440=CARTESIAN_POINT('Ctrl Pts',(53.7970133686507,18.8635558286649,16.892559323815));
#38441=CARTESIAN_POINT('Ctrl Pts',(53.7274789131453,18.9058079520946,16.8883432648231));
#38442=CARTESIAN_POINT('Ctrl Pts',(53.6573752736946,18.9484059361503,16.8840926946946));
#38443=CARTESIAN_POINT('Ctrl Pts',(53.5894389445941,18.9945120327593,16.8798421245662));
#38444=CARTESIAN_POINT('Ctrl Pts',(53.5240292750327,19.0438658867451,16.8755915544377));
#38445=CARTESIAN_POINT('Ctrl Pts',(53.4590563514206,19.0928902008334,16.8713693657289));
#38446=CARTESIAN_POINT('Ctrl Pts',(53.3965767692371,19.1451186847214,16.8671471770202));
#38447=CARTESIAN_POINT('Ctrl Pts',(53.336908376809,19.2002565452621,16.8629249883114));
#38448=CARTESIAN_POINT('Ctrl Pts',(53.2766383507949,19.2559503582496,16.8586602274731));
#38449=CARTESIAN_POINT('Ctrl Pts',(53.2192368635663,19.3146122011117,16.8543954666348));
#38450=CARTESIAN_POINT('Ctrl Pts',(53.1649910058721,19.375902637934,16.8501307057964));
#38451=CARTESIAN_POINT('Ctrl Pts',(53.1107451481779,19.4371930747563,16.8458659449581));
#38452=CARTESIAN_POINT('Ctrl Pts',(53.0596551706464,19.5011116890745,16.8416011841198));
#38453=CARTESIAN_POINT('Ctrl Pts',(53.0119632919475,19.5672891787119,16.8373364232815));
#38454=CARTESIAN_POINT('Ctrl Pts',(52.9642693426104,19.6334695415775,16.83307147728));
#38455=CARTESIAN_POINT('Ctrl Pts',(52.9197953624586,19.7021563126665,16.8288065312786));
#38456=CARTESIAN_POINT('Ctrl Pts',(52.8788124314755,19.7730062962113,16.8245415852771));
#38457=CARTESIAN_POINT('Ctrl Pts',(52.8378901528898,19.8437514258265,16.8202829511522));
#38458=CARTESIAN_POINT('Ctrl Pts',(52.8004488875799,19.9166530190759,16.8160243170272));
#38459=CARTESIAN_POINT('Ctrl Pts',(52.7667177235425,19.9913372597043,16.8117656829023));
#38460=CARTESIAN_POINT('Ctrl Pts',(52.733026705015,20.0659326140753,16.8075121172369));
#38461=CARTESIAN_POINT('Ctrl Pts',(52.7030372009587,20.1423059881466,16.8032585515714));
#38462=CARTESIAN_POINT('Ctrl Pts',(52.6769327916645,20.2200583383636,16.799004985906));
#38463=CARTESIAN_POINT('Ctrl Pts',(52.6508537261519,20.2977352017704,16.7947555498662));
#38464=CARTESIAN_POINT('Ctrl Pts',(52.628652398988,20.376787948993,16.7905061138265));
#38465=CARTESIAN_POINT('Ctrl Pts',(52.6104640516671,20.4567981943839,16.7862566777868));
#38466=CARTESIAN_POINT('Ctrl Pts',(52.592285823686,20.5367639249625,16.7820096059798));
#38467=CARTESIAN_POINT('Ctrl Pts',(52.5781162378917,20.6176856516973,16.7777625341729));
#38468=CARTESIAN_POINT('Ctrl Pts',(52.5680402033317,20.6991315945648,16.773515462366));
#38469=CARTESIAN_POINT('Ctrl Pts',(52.5579660429577,20.780562388135,16.7692691805328));
#38470=CARTESIAN_POINT('Ctrl Pts',(52.551983977712,20.8625167527755,16.7650228986996));
#38471=CARTESIAN_POINT('Ctrl Pts',(52.5501273132381,20.9445557157339,16.7607766168664));
#38472=CARTESIAN_POINT('Ctrl Pts',(52.5496974840555,20.9635482374755,16.7597935766483));
#38473=CARTESIAN_POINT('Ctrl Pts',(52.549488536141,20.9825452782313,16.7588105364302));
#38474=CARTESIAN_POINT('Ctrl Pts',(52.5495004847655,21.0015413745099,16.7578274962121));
#38475=CARTESIAN_POINT('',(52.5495002472464,21.0011007971719,15.957827496239));
#38476=CARTESIAN_POINT('Ctrl Pts',(52.5495004847658,21.0015413750748,16.7578274961829));
#38477=CARTESIAN_POINT('Ctrl Pts',(52.5495581962121,21.0932918344117,16.7530794474136));
#38478=CARTESIAN_POINT('Ctrl Pts',(52.5547728996673,21.1848479458307,16.7483313986442));
#38479=CARTESIAN_POINT('Ctrl Pts',(52.565054999287,21.2756684485081,16.7435833498749));
#38480=CARTESIAN_POINT('Ctrl Pts',(52.5753836098533,21.366899776572,16.7388138233675));
#38481=CARTESIAN_POINT('Ctrl Pts',(52.5908254338274,21.4573886044141,16.7340442968602));
#38482=CARTESIAN_POINT('Ctrl Pts',(52.6112400460042,21.5466041823713,16.7292747703528));
#38483=CARTESIAN_POINT('Ctrl Pts',(52.6317667984321,21.6363098336761,16.7244790441852));
#38484=CARTESIAN_POINT('Ctrl Pts',(52.6573209987667,21.7247279934454,16.7196833180177));
#38485=CARTESIAN_POINT('Ctrl Pts',(52.6877117586267,21.8113404580119,16.7148875918502));
#38486=CARTESIAN_POINT('Ctrl Pts',(52.6973957506987,21.8389394527082,16.7133594374243));
#38487=CARTESIAN_POINT('Ctrl Pts',(52.7075704774109,21.866355276581,16.7118312829984));
#38488=CARTESIAN_POINT('Ctrl Pts',(52.7182287750057,21.8935716685236,16.7103031285726));
#38489=CARTESIAN_POINT('Ctrl Pts',(52.7477399320168,21.9689295958798,16.7060719082677));
#38490=CARTESIAN_POINT('Ctrl Pts',(52.7810435953473,22.0429652853492,16.7018406879627));
#38491=CARTESIAN_POINT('Ctrl Pts',(52.8180004887935,22.1152705425566,16.6976094676578));
#38492=CARTESIAN_POINT('Ctrl Pts',(52.8549043886411,22.1874721190857,16.6933843146267));
#38493=CARTESIAN_POINT('Ctrl Pts',(52.8954509047876,22.2579477809502,16.6891591615955));
#38494=CARTESIAN_POINT('Ctrl Pts',(52.939452282941,22.3263081677058,16.6849340085644));
#38495=CARTESIAN_POINT('Ctrl Pts',(52.9835666988637,22.3948441695432,16.6806980012852));
#38496=CARTESIAN_POINT('Ctrl Pts',(53.0311535722193,22.4612535770766,16.676461994006));
#38497=CARTESIAN_POINT('Ctrl Pts',(53.0819767087438,22.5251678282073,16.6722259867268));
#38498=CARTESIAN_POINT('Ctrl Pts',(53.1325784208443,22.5888036200142,16.6680084347326));
#38499=CARTESIAN_POINT('Ctrl Pts',(53.1863879708527,22.6499655803971,16.6637908827385));
#38500=CARTESIAN_POINT('Ctrl Pts',(53.2431292900819,22.7083195130396,16.6595733307443));
#38501=CARTESIAN_POINT('Ctrl Pts',(53.2998518746183,22.7666541785411,16.6553571712899));
#38502=CARTESIAN_POINT('Ctrl Pts',(53.3595039821995,22.8221823244247,16.6511410118355));
#38503=CARTESIAN_POINT('Ctrl Pts',(53.4217712421883,22.8746050885497,16.646924852381));
#38504=CARTESIAN_POINT('Ctrl Pts',(53.4840370184745,22.9270266035463,16.6427087933891));
#38505=CARTESIAN_POINT('Ctrl Pts',(53.5489174668984,22.9763425853237,16.6384927343972));
#38506=CARTESIAN_POINT('Ctrl Pts',(53.6160646589281,23.0222940492748,16.6342766754053));
#38507=CARTESIAN_POINT('Ctrl Pts',(53.6837614936266,23.0686216553178,16.6300261052769));
#38508=CARTESIAN_POINT('Ctrl Pts',(53.7537619658826,23.1115291236671,16.6257755351484));
#38509=CARTESIAN_POINT('Ctrl Pts',(53.8256807945839,23.1507962836566,16.6215249650199));
#38510=CARTESIAN_POINT('Ctrl Pts',(53.8971194151244,23.1898012534655,16.6173027763111));
#38511=CARTESIAN_POINT('Ctrl Pts',(53.9704504023963,23.2252142316627,16.6130805876024));
#38512=CARTESIAN_POINT('Ctrl Pts',(54.0452741938042,23.2568670507994,16.6088583988936));
#38513=CARTESIAN_POINT('Ctrl Pts',(54.1208524299715,23.2888390238184,16.6045936380553));
#38514=CARTESIAN_POINT('Ctrl Pts',(54.197953287101,23.3169744174355,16.6003288772169));
#38515=CARTESIAN_POINT('Ctrl Pts',(54.2761491964903,23.3411514825526,16.5960641163786));
#38516=CARTESIAN_POINT('Ctrl Pts',(54.3543451058797,23.3653285476697,16.5917993555402));
#38517=CARTESIAN_POINT('Ctrl Pts',(54.433635584795,23.3855472274969,16.5875345947019));
#38518=CARTESIAN_POINT('Ctrl Pts',(54.5135843376472,23.4017389644626,16.5832698338635));
#38519=CARTESIAN_POINT('Ctrl Pts',(54.5929043275,23.4178033602912,16.5790386135586));
#38520=CARTESIAN_POINT('Ctrl Pts',(54.673169706054,23.4299642119077,16.5748073932536));
#38521=CARTESIAN_POINT('Ctrl Pts',(54.7539619753578,23.4381172122009,16.5705761729487));
#38522=CARTESIAN_POINT('Ctrl Pts',(54.8346383942022,23.4462585216623,16.5663510199175));
#38523=CARTESIAN_POINT('Ctrl Pts',(54.9158397445982,23.4504033474446,16.5621258668864));
#38524=CARTESIAN_POINT('Ctrl Pts',(54.9971370676512,23.4504983276098,16.5579007138552));
#38525=CARTESIAN_POINT('Ctrl Pts',(55.0786432402543,23.4505935517752,16.553664706576));
#38526=CARTESIAN_POINT('Ctrl Pts',(55.1602454153505,23.4466180085095,16.5494286992968));
#38527=CARTESIAN_POINT('Ctrl Pts',(55.2415058443402,23.4385703141697,16.5451926920176));
#38528=CARTESIAN_POINT('Ctrl Pts',(55.3224122407987,23.4305576817368,16.5409751400235));
#38529=CARTESIAN_POINT('Ctrl Pts',(55.402979396355,23.4185083450086,16.5367575880293));
#38530=CARTESIAN_POINT('Ctrl Pts',(55.4827768169721,23.4024730581204,16.5325400360352));
#38531=CARTESIAN_POINT('Ctrl Pts',(55.5625478902963,23.3864430657191,16.5283238765807));
#38532=CARTESIAN_POINT('Ctrl Pts',(55.6415492779336,23.3664298282112,16.5241077171263));
#38533=CARTESIAN_POINT('Ctrl Pts',(55.7193594067178,23.342535441347,16.5198915576719));
#38534=CARTESIAN_POINT('Ctrl Pts',(55.7971676814443,23.3186416238375,16.51567549868));
#38535=CARTESIAN_POINT('Ctrl Pts',(55.8737843096423,23.2908669783861,16.5114594396881));
#38536=CARTESIAN_POINT('Ctrl Pts',(55.9488030288365,23.2593634197425,16.5072433806962));
#38537=CARTESIAN_POINT('Ctrl Pts',(56.0244358241783,23.2276019843432,16.5029928105677));
#38538=CARTESIAN_POINT('Ctrl Pts',(56.0984439814427,23.1920504778421,16.4987422404392));
#38539=CARTESIAN_POINT('Ctrl Pts',(56.1704335976159,23.1529132457143,16.4944916703108));
#38540=CARTESIAN_POINT('Ctrl Pts',(56.2419425329744,23.1140373362275,16.490269481602));
#38541=CARTESIAN_POINT('Ctrl Pts',(56.311459432492,23.0716237369869,16.4860472928933));
#38542=CARTESIAN_POINT('Ctrl Pts',(56.3786263443655,23.0259169905555,16.4818251041845));
#38543=CARTESIAN_POINT('Ctrl Pts',(56.4464704970428,22.979749385156,16.4775603433462));
#38544=CARTESIAN_POINT('Ctrl Pts',(56.5119166183364,22.9302221426357,16.4732955825079));
#38545=CARTESIAN_POINT('Ctrl Pts',(56.5746305732602,22.8776285063223,16.4690308216695));
#38546=CARTESIAN_POINT('Ctrl Pts',(56.637344528184,22.825034870009,16.4647660608312));
#38547=CARTESIAN_POINT('Ctrl Pts',(56.6973260072724,22.7693752147199,16.4605012999929));
#38548=CARTESIAN_POINT('Ctrl Pts',(56.754280837033,22.7109789580292,16.4562365391545));
#38549=CARTESIAN_POINT('Ctrl Pts',(56.8107877412375,22.6530419631055,16.4520053188496));
#38550=CARTESIAN_POINT('Ctrl Pts',(56.8645273599191,22.5921940322417,16.4477740985447));
#38551=CARTESIAN_POINT('Ctrl Pts',(56.9151851318255,22.5287302446261,16.4435428782398));
#38552=CARTESIAN_POINT('Ctrl Pts',(56.9657702640325,22.4653574596401,16.4393177252086));
#38553=CARTESIAN_POINT('Ctrl Pts',(57.013282038641,22.3993766278748,16.4350925721775));
#38554=CARTESIAN_POINT('Ctrl Pts',(57.0574430281834,22.3311192417584,16.4308674191463));
#38555=CARTESIAN_POINT('Ctrl Pts',(57.1017174655301,22.2626865051649,16.4266314118671));
#38556=CARTESIAN_POINT('Ctrl Pts',(57.1426235547403,22.1919658448864,16.4223954045879));
#38557=CARTESIAN_POINT('Ctrl Pts',(57.1799227763783,22.1193243225388,16.4181593973087));
#38558=CARTESIAN_POINT('Ctrl Pts',(57.2170594941013,22.0469992821782,16.4139418453146));
#38559=CARTESIAN_POINT('Ctrl Pts',(57.250620486266,21.9727704948047,16.4097242933204));
#38560=CARTESIAN_POINT('Ctrl Pts',(57.2804149750245,21.8970271967359,16.4055067413262));
#38561=CARTESIAN_POINT('Ctrl Pts',(57.3101996263207,21.8213089073809,16.4012905818718));
#38562=CARTESIAN_POINT('Ctrl Pts',(57.336220073798,21.7440775326862,16.3970744224174));
#38563=CARTESIAN_POINT('Ctrl Pts',(57.3583335157403,21.6657426518827,16.3928582629629));
#38564=CARTESIAN_POINT('Ctrl Pts',(57.3804464307642,21.5874096376408,16.388642203971));
#38565=CARTESIAN_POINT('Ctrl Pts',(57.3986524001108,21.5079736173066,16.3844261449791));
#38566=CARTESIAN_POINT('Ctrl Pts',(57.4128587835408,21.4278583184769,16.3802100859873));
#38567=CARTESIAN_POINT('Ctrl Pts',(57.427181455296,21.3470872247388,16.3759595158588));
#38568=CARTESIAN_POINT('Ctrl Pts',(57.4374386610082,21.2656261500641,16.3717089457303));
#38569=CARTESIAN_POINT('Ctrl Pts',(57.4435885161579,21.1839168662768,16.3674583756018));
#38570=CARTESIAN_POINT('Ctrl Pts',(57.4496973081996,21.1027531623549,16.3632361868931));
#38571=CARTESIAN_POINT('Ctrl Pts',(57.451753482844,21.0213450247708,16.3590139981843));
#38572=CARTESIAN_POINT('Ctrl Pts',(57.4497684241177,20.9401258136087,16.3547918094756));
#38573=CARTESIAN_POINT('Ctrl Pts',(57.4477633501379,20.8580876729716,16.3505270486372));
#38574=CARTESIAN_POINT('Ctrl Pts',(57.4416351252318,20.7762427745138,16.3462622877989));
#38575=CARTESIAN_POINT('Ctrl Pts',(57.4314489675299,20.6950308732054,16.3419975269605));
#38576=CARTESIAN_POINT('Ctrl Pts',(57.421262809828,20.6138189718969,16.3377327661222));
#38577=CARTESIAN_POINT('Ctrl Pts',(57.407018866466,20.5332405309958,16.3334680052839));
#38578=CARTESIAN_POINT('Ctrl Pts',(57.3888344184503,20.453721342878,16.3292032444455));
#38579=CARTESIAN_POINT('Ctrl Pts',(57.3707929833981,20.3748275394152,16.3249720241406));
#38580=CARTESIAN_POINT('Ctrl Pts',(57.3488051943653,20.2966805340988,16.3207408038357));
#38581=CARTESIAN_POINT('Ctrl Pts',(57.3229484253431,20.2197046307994,16.3165095835307));
#38582=CARTESIAN_POINT('Ctrl Pts',(57.2971287331179,20.1428391055576,16.3122844304996));
#38583=CARTESIAN_POINT('Ctrl Pts',(57.2674512261356,20.0671417841638,16.3080592774684));
#38584=CARTESIAN_POINT('Ctrl Pts',(57.2340440088283,19.9930255134224,16.3038341244373));
#38585=CARTESIAN_POINT('Ctrl Pts',(57.2005509697248,19.9187188409653,16.2995981171581));
#38586=CARTESIAN_POINT('Ctrl Pts',(57.1633091442996,19.8460018115726,16.2953621098789));
#38587=CARTESIAN_POINT('Ctrl Pts',(57.1224976202594,19.7752738665346,16.2911261025997));
#38588=CARTESIAN_POINT('Ctrl Pts',(57.0818639024078,19.7048540664783,16.2869085506055));
#38589=CARTESIAN_POINT('Ctrl Pts',(57.0376917524969,19.6364064643124,16.2826909986114));
#38590=CARTESIAN_POINT('Ctrl Pts',(56.9902047767333,19.5703024107638,16.2784734466172));
#38591=CARTESIAN_POINT('Ctrl Pts',(56.9427334800888,19.5042201832698,16.2742572871628));
#38592=CARTESIAN_POINT('Ctrl Pts',(56.8919498021123,19.4404803450574,16.2700411277083));
#38593=CARTESIAN_POINT('Ctrl Pts',(56.8381204555523,19.3794249659827,16.2658249682539));
#38594=CARTESIAN_POINT('Ctrl Pts',(56.7842923916366,19.318371041734,16.261608909262));
#38595=CARTESIAN_POINT('Ctrl Pts',(56.7274191117251,19.2600017974482,16.2573928502701));
#38596=CARTESIAN_POINT('Ctrl Pts',(56.6678064151717,19.2046248270871,16.2531767912782));
#38597=CARTESIAN_POINT('Ctrl Pts',(56.6077057506092,19.1487945608421,16.2489262211497));
#38598=CARTESIAN_POINT('Ctrl Pts',(56.544820955192,19.096006120237,16.2446756510213));
#38599=CARTESIAN_POINT('Ctrl Pts',(56.4795005105318,19.0465342364566,16.2404250808928));
#38600=CARTESIAN_POINT('Ctrl Pts',(56.4146162160586,18.9973926806689,16.236202892184));
#38601=CARTESIAN_POINT('Ctrl Pts',(56.3473291221265,18.9515237400961,16.2319807034753));
#38602=CARTESIAN_POINT('Ctrl Pts',(56.2780095258749,18.9091528267774,16.2277585147665));
#38603=CARTESIAN_POINT('Ctrl Pts',(56.2079909834042,18.8663546895384,16.2234937539282));
#38604=CARTESIAN_POINT('Ctrl Pts',(56.1358991473785,18.8271257496791,16.2192289930899));
#38605=CARTESIAN_POINT('Ctrl Pts',(56.0621388781727,18.791649653367,16.2149642322515));
#38606=CARTESIAN_POINT('Ctrl Pts',(55.988378608967,18.756173557055,16.2106994714132));
#38607=CARTESIAN_POINT('Ctrl Pts',(55.9129503756073,18.7244504318501,16.2064347105749));
#38608=CARTESIAN_POINT('Ctrl Pts',(55.8362755362313,18.6966126080268,16.2021699497365));
#38609=CARTESIAN_POINT('Ctrl Pts',(55.7602037119151,18.6689937168694,16.1979387294316));
#38610=CARTESIAN_POINT('Ctrl Pts',(55.6826195745121,18.6450956221778,16.1937075091267));
#38611=CARTESIAN_POINT('Ctrl Pts',(55.6039215930101,18.6250833784118,16.1894762888218));
#38612=CARTESIAN_POINT('Ctrl Pts',(55.5253364589055,18.6050998308026,16.1852511357906));
#38613=CARTESIAN_POINT('Ctrl Pts',(55.4456410995906,18.5889911812454,16.1810259827594));
#38614=CARTESIAN_POINT('Ctrl Pts',(55.3652518645743,18.5768736464177,16.1768008297283));
#38615=CARTESIAN_POINT('Ctrl Pts',(55.2846561128495,18.5647249821309,16.1725648224491));
#38616=CARTESIAN_POINT('Ctrl Pts',(55.2033633616496,18.5565881198942,16.1683288151699));
#38617=CARTESIAN_POINT('Ctrl Pts',(55.1218063409409,18.552529169672,16.1640928078907));
#38618=CARTESIAN_POINT('Ctrl Pts',(55.0406046449437,18.548487903339,16.1598752558965));
#38619=CARTESIAN_POINT('Ctrl Pts',(54.9591414442423,18.5484891215448,16.1556577039024));
#38620=CARTESIAN_POINT('Ctrl Pts',(54.8778500050207,18.5525462969187,16.1514401519082));
#38621=CARTESIAN_POINT('Ctrl Pts',(54.796585406383,18.5566021327055,16.1472239924538));
#38622=CARTESIAN_POINT('Ctrl Pts',(54.7154929205828,18.5647112430706,16.1430078329994));
#38623=CARTESIAN_POINT('Ctrl Pts',(54.6350045842893,18.5768350042743,16.1387916735449));
#38624=CARTESIAN_POINT('Ctrl Pts',(54.5545181658697,18.5889584765934,16.134575614553));
#38625=CARTESIAN_POINT('Ctrl Pts',(54.4746363279049,18.6050963392071,16.1303595555611));
#38626=CARTESIAN_POINT('Ctrl Pts',(54.3957833328088,18.6251584328448,16.1261434965692));
#38627=CARTESIAN_POINT('Ctrl Pts',(54.316284875567,18.645384747537,16.1218929264408));
#38628=CARTESIAN_POINT('Ctrl Pts',(54.2378326512754,18.6695997317385,16.1176423563123));
#38629=CARTESIAN_POINT('Ctrl Pts',(54.1608464531326,18.6976595441204,16.1133917861838));
#38630=CARTESIAN_POINT('Ctrl Pts',(54.084374298409,18.7255319987389,16.1091695974751));
#38631=CARTESIAN_POINT('Ctrl Pts',(54.0093490604099,18.757197853887,16.1049474087663));
#38632=CARTESIAN_POINT('Ctrl Pts',(53.9361609214986,18.79246819614,16.1007252200576));
#38633=CARTESIAN_POINT('Ctrl Pts',(53.862234830035,18.8280941675903,16.0964604592192));
#38634=CARTESIAN_POINT('Ctrl Pts',(53.7901835194177,18.8673974903808,16.0921956983809));
#38635=CARTESIAN_POINT('Ctrl Pts',(53.7203808197885,18.9101375634662,16.0879309375426));
#38636=CARTESIAN_POINT('Ctrl Pts',(53.6505781201594,18.9528776365517,16.0836661767042));
#38637=CARTESIAN_POINT('Ctrl Pts',(53.5830243930152,18.9990541350055,16.0794014158659));
#38638=CARTESIAN_POINT('Ctrl Pts',(53.5180592965164,19.0483847711809,16.0751366550276));
#38639=CARTESIAN_POINT('Ctrl Pts',(53.4542839150827,19.09681200839,16.0709499953619));
#38640=CARTESIAN_POINT('Ctrl Pts',(53.3927529352554,19.1484689909858,16.0667633356962));
#38641=CARTESIAN_POINT('Ctrl Pts',(53.3338170830797,19.2031180513559,16.0625766760305));
#38642=CARTESIAN_POINT('Ctrl Pts',(53.2723770701508,19.2600891284123,16.0582121268725));
#38643=CARTESIAN_POINT('Ctrl Pts',(53.2137581038291,19.3203119934272,16.0538475777146));
#38644=CARTESIAN_POINT('Ctrl Pts',(53.1583232212213,19.3834676333252,16.0494830285566));
#38645=CARTESIAN_POINT('Ctrl Pts',(53.1052868869398,19.443890664309,16.045307324068));
#38646=CARTESIAN_POINT('Ctrl Pts',(53.0551651738979,19.5069975449245,16.0411316195794));
#38647=CARTESIAN_POINT('Ctrl Pts',(53.0082400431393,19.5724697816697,16.0369559150908));
#38648=CARTESIAN_POINT('Ctrl Pts',(52.9613429297233,19.6379029272486,16.0327827037682));
#38649=CARTESIAN_POINT('Ctrl Pts',(52.9176388882398,19.7056982411438,16.0286094924457));
#38650=CARTESIAN_POINT('Ctrl Pts',(52.8773691903924,19.7755047178104,16.0244362811231));
#38651=CARTESIAN_POINT('Ctrl Pts',(52.837110562581,19.8452920048568,16.0202642170056));
#38652=CARTESIAN_POINT('Ctrl Pts',(52.8002846413469,19.9170889450323,16.0160921528881));
#38653=CARTESIAN_POINT('Ctrl Pts',(52.767088143579,19.9905175130521,16.0119200887706));
#38654=CARTESIAN_POINT('Ctrl Pts',(52.7338900768914,20.0639495514237,16.0077478274746));
#38655=CARTESIAN_POINT('Ctrl Pts',(52.704321967636,20.1390129361383,16.0035755661786));
#38656=CARTESIAN_POINT('Ctrl Pts',(52.6785328728113,20.215308578241,15.9994033048827));
#38657=CARTESIAN_POINT('Ctrl Pts',(52.6527194470096,20.291676202223,15.9952271072255));
#38658=CARTESIAN_POINT('Ctrl Pts',(52.6306923017233,20.3692779518662,15.9910509095682));
#38659=CARTESIAN_POINT('Ctrl Pts',(52.6125507009076,20.4476992718971,15.986874711911));
#38660=CARTESIAN_POINT('Ctrl Pts',(52.5943989802482,20.5261643373231,15.9826961846652));
#38661=CARTESIAN_POINT('Ctrl Pts',(52.5801371996134,20.605449414732,15.9785176574193));
#38662=CARTESIAN_POINT('Ctrl Pts',(52.5698131067276,20.6851319105291,15.9743391301735));
#38663=CARTESIAN_POINT('Ctrl Pts',(52.5594734701288,20.7649343744304,15.9701543118346));
#38664=CARTESIAN_POINT('Ctrl Pts',(52.5530833841282,20.8451349771926,15.9659694934957));
#38665=CARTESIAN_POINT('Ctrl Pts',(52.5506385518353,20.9253089948896,15.9617846751568));
#38666=CARTESIAN_POINT('Ctrl Pts',(52.5498679378346,20.9505799391215,15.9604656155176));
#38667=CARTESIAN_POINT('Ctrl Pts',(52.5494889034741,20.9758482693652,15.9591465558783));
#38668=CARTESIAN_POINT('Ctrl Pts',(52.5495002472464,21.0011007971719,15.957827496239));
#38669=CARTESIAN_POINT('',(52.5495010097513,20.9977754123675,15.1578274961792));
#38670=CARTESIAN_POINT('Ctrl Pts',(52.5495002472466,21.0011007976877,15.9578274962121));
#38671=CARTESIAN_POINT('Ctrl Pts',(52.5495281227704,21.0631548561835,15.9545861175809));
#38672=CARTESIAN_POINT('Ctrl Pts',(52.5519128814938,21.1251536128192,15.9513447389498));
#38673=CARTESIAN_POINT('Ctrl Pts',(52.5566432426686,21.1869706030453,15.9481033603187));
#38674=CARTESIAN_POINT('Ctrl Pts',(52.562818146168,21.2676650648772,15.9438721400138));
#38675=CARTESIAN_POINT('Ctrl Pts',(52.573006453828,21.348204593641,15.9396409197089));
#38676=CARTESIAN_POINT('Ctrl Pts',(52.5871943956603,21.4281581082579,15.935409699404));
#38677=CARTESIAN_POINT('Ctrl Pts',(52.601361992977,21.5079969751308,15.9311845463729));
#38678=CARTESIAN_POINT('Ctrl Pts',(52.6195177533904,21.5872510428542,15.9269593933418));
#38679=CARTESIAN_POINT('Ctrl Pts',(52.6415960399012,21.6654930585591,15.9227342403107));
#38680=CARTESIAN_POINT('Ctrl Pts',(52.6637310446412,21.7439360748525,15.9184982330315));
#38681=CARTESIAN_POINT('Ctrl Pts',(52.6898087124821,21.8213613624831,15.9142622257523));
#38682=CARTESIAN_POINT('Ctrl Pts',(52.7197110011918,21.8973473864198,15.9100262184731));
#38683=CARTESIAN_POINT('Ctrl Pts',(52.7494830126794,21.9730023571645,15.9058086664789));
#38684=CARTESIAN_POINT('Ctrl Pts',(52.783046224873,22.0472301407583,15.9015911144848));
#38685=CARTESIAN_POINT('Ctrl Pts',(52.8202344121191,22.1196303996811,15.8973735624906));
#38686=CARTESIAN_POINT('Ctrl Pts',(52.8574103206717,22.1920067536854,15.8931574030361));
#38687=CARTESIAN_POINT('Ctrl Pts',(52.8982086151773,22.2625563680684,15.8889412435817));
#38688=CARTESIAN_POINT('Ctrl Pts',(52.9424161069486,22.3309014888622,15.8847250841272));
#38689=CARTESIAN_POINT('Ctrl Pts',(52.986622545345,22.3992449811302,15.8805090251353));
#38690=CARTESIAN_POINT('Ctrl Pts',(53.0342377660559,22.4653836944759,15.8762929661434));
#38691=CARTESIAN_POINT('Ctrl Pts',(53.0850048247631,22.5289681909115,15.8720769071515));
#38692=CARTESIAN_POINT('Ctrl Pts',(53.1361874442819,22.5930731670759,15.867826337023));
#38693=CARTESIAN_POINT('Ctrl Pts',(53.1905734528108,22.6545815326246,15.8635757668945));
#38694=CARTESIAN_POINT('Ctrl Pts',(53.2478588328643,22.7131700383874,15.859325196766));
#38695=CARTESIAN_POINT('Ctrl Pts',(53.3047617135433,22.7713673436941,15.8551030080572));
#38696=CARTESIAN_POINT('Ctrl Pts',(53.364524978402,22.8266833892191,15.8508808193484));
#38697=CARTESIAN_POINT('Ctrl Pts',(53.4268157402014,22.878840476124,15.8466586306396));
#38698=CARTESIAN_POINT('Ctrl Pts',(53.4897345768136,22.9315234604758,15.8423938698013));
#38699=CARTESIAN_POINT('Ctrl Pts',(53.5552317788347,22.9809831316379,15.8381291089629));
#38700=CARTESIAN_POINT('Ctrl Pts',(53.6229340988568,23.026977985551,15.8338643481245));
#38701=CARTESIAN_POINT('Ctrl Pts',(53.6906364188788,23.0729728394642,15.8295995872862));
#38702=CARTESIAN_POINT('Ctrl Pts',(53.7605434118993,23.1155026806039,15.8253348264478));
#38703=CARTESIAN_POINT('Ctrl Pts',(53.8322579247294,23.1543743165111,15.8210700656095));
#38704=CARTESIAN_POINT('Ctrl Pts',(53.9034084333622,23.1929402435047,15.8168388453045));
#38705=CARTESIAN_POINT('Ctrl Pts',(53.9766049171274,23.2280499582696,15.8126076249996));
#38706=CARTESIAN_POINT('Ctrl Pts',(54.0514777000664,23.2594812892628,15.8083764046947));
#38707=CARTESIAN_POINT('Ctrl Pts',(54.1262431206751,23.2908675499273,15.8041512516635));
#38708=CARTESIAN_POINT('Ctrl Pts',(54.2026796414736,23.3185857240215,15.7999260986323));
#38709=CARTESIAN_POINT('Ctrl Pts',(54.2803926796746,23.3424592962385,15.7957009456012));
#38710=CARTESIAN_POINT('Ctrl Pts',(54.3583053595421,23.3663941987014,15.791464938322));
#38711=CARTESIAN_POINT('Ctrl Pts',(54.4375007058176,23.3864645014641,15.7872289310428));
#38712=CARTESIAN_POINT('Ctrl Pts',(54.517560524782,23.4025408222861,15.7829929237636));
#38713=CARTESIAN_POINT('Ctrl Pts',(54.59727154199,23.4185471023685,15.7787753717694));
#38714=CARTESIAN_POINT('Ctrl Pts',(54.6778390578833,23.4305940294786,15.7745578197753));
#38715=CARTESIAN_POINT('Ctrl Pts',(54.7588365635377,23.4386042005446,15.7703402677811));
#38716=CARTESIAN_POINT('Ctrl Pts',(54.8398073256583,23.4466117268343,15.7661241083267));
#38717=CARTESIAN_POINT('Ctrl Pts',(54.9212073333003,23.450585098204,15.7619079488723));
#38718=CARTESIAN_POINT('Ctrl Pts',(55.0026035886565,23.450498616879,15.7576917894179));
#38719=CARTESIAN_POINT('Ctrl Pts',(55.0839979045049,23.4504121376148,15.753475730426));
#38720=CARTESIAN_POINT('Ctrl Pts',(55.1653880033248,23.4462659995988,15.7492596714341));
#38721=CARTESIAN_POINT('Ctrl Pts',(55.2463409541387,23.4380866236281,15.7450436124422));
#38722=CARTESIAN_POINT('Ctrl Pts',(55.3279565565775,23.429840294239,15.7407930423138));
#38723=CARTESIAN_POINT('Ctrl Pts',(55.4091273424047,23.4174944251171,15.7365424721853));
#38724=CARTESIAN_POINT('Ctrl Pts',(55.4894168613141,23.4011291897483,15.7322919020569));
#38725=CARTESIAN_POINT('Ctrl Pts',(55.5691702802496,23.3848732264536,15.7280697133481));
#38726=CARTESIAN_POINT('Ctrl Pts',(55.6480537255664,23.3646515852234,15.7238475246394));
#38727=CARTESIAN_POINT('Ctrl Pts',(55.7256533661477,23.3405933953163,15.7196253359306));
#38728=CARTESIAN_POINT('Ctrl Pts',(55.8040354402445,23.3162926278153,15.7153605750923));
#38729=CARTESIAN_POINT('Ctrl Pts',(55.8811072186142,23.2880776756983,15.711095814254));
#38730=CARTESIAN_POINT('Ctrl Pts',(55.956463398109,23.256131205865,15.7068310534157));
#38731=CARTESIAN_POINT('Ctrl Pts',(56.0318195776037,23.2241847360317,15.7025662925774));
#38732=CARTESIAN_POINT('Ctrl Pts',(56.1054597526467,23.1885070163714,15.698301531739));
#38733=CARTESIAN_POINT('Ctrl Pts',(56.1770062509688,23.1493269958711,15.6940367709007));
#38734=CARTESIAN_POINT('Ctrl Pts',(56.2479900664563,23.1104551095984,15.6898055505958));
#38735=CARTESIAN_POINT('Ctrl Pts',(56.3171792225727,23.0679900889066,15.6855743302909));
#38736=CARTESIAN_POINT('Ctrl Pts',(56.3841865965516,23.0221220823498,15.6813431099859));
#38737=CARTESIAN_POINT('Ctrl Pts',(56.4510978866461,22.9763198473042,15.6771179569548));
#38738=CARTESIAN_POINT('Ctrl Pts',(56.5158332276734,22.9271245781314,15.6728928039236));
#38739=CARTESIAN_POINT('Ctrl Pts',(56.578030353825,22.8747721067925,15.6686676508925));
#38740=CARTESIAN_POINT('Ctrl Pts',(56.6403872618897,22.8222851440622,15.6644316436133));
#38741=CARTESIAN_POINT('Ctrl Pts',(56.7001924863258,22.7666249692974,15.6601956363341));
#38742=CARTESIAN_POINT('Ctrl Pts',(56.7571105618316,22.7080728097771,15.6559596290549));
#38743=CARTESIAN_POINT('Ctrl Pts',(56.8137806587014,22.6497757482116,15.6517420770607));
#38744=CARTESIAN_POINT('Ctrl Pts',(56.8675883794462,22.5886121785131,15.6475245250666));
#38745=CARTESIAN_POINT('Ctrl Pts',(56.9182374248148,22.5248984989303,15.6433069730724));
#38746=CARTESIAN_POINT('Ctrl Pts',(56.9688697470208,22.461205856155,15.639090813618));
#38747=CARTESIAN_POINT('Ctrl Pts',(57.0163451758642,22.3949651392182,15.6348746541635));
#38748=CARTESIAN_POINT('Ctrl Pts',(57.0604073382992,22.3265262342987,15.6306584947091));
#38749=CARTESIAN_POINT('Ctrl Pts',(57.1044684508222,22.2580889601396,15.6264424357172));
#38750=CARTESIAN_POINT('Ctrl Pts',(57.1451162079009,22.187453993651,15.6222263767253));
#38751=CARTESIAN_POINT('Ctrl Pts',(57.1821380645935,22.1149994246869,15.6180103177334));
#38752=CARTESIAN_POINT('Ctrl Pts',(57.2194629688372,22.0419517687831,15.6137597476049));
#38753=CARTESIAN_POINT('Ctrl Pts',(57.2531021055102,21.9670550035654,15.6095091774764));
#38754=CARTESIAN_POINT('Ctrl Pts',(57.2828861863247,21.8907193218338,15.6052586073479));
#38755=CARTESIAN_POINT('Ctrl Pts',(57.3124713962881,21.8148933399678,15.6010364186392));
#38756=CARTESIAN_POINT('Ctrl Pts',(57.3382527846846,21.7376480635334,15.5968142299304));
#38757=CARTESIAN_POINT('Ctrl Pts',(57.3601144622165,21.6594012247765,15.5925920412216));
#38758=CARTESIAN_POINT('Ctrl Pts',(57.3821965700116,21.5803654268354,15.5883272803833));
#38759=CARTESIAN_POINT('Ctrl Pts',(57.4002793704857,21.5003082293385,15.584062519545));
#38760=CARTESIAN_POINT('Ctrl Pts',(57.4142965826117,21.4196692283088,15.5797977587066));
#38761=CARTESIAN_POINT('Ctrl Pts',(57.4283137947378,21.3390302272791,15.5755329978683));
#38762=CARTESIAN_POINT('Ctrl Pts',(57.4382654236932,21.2578099087519,15.5712682370299));
#38763=CARTESIAN_POINT('Ctrl Pts',(57.4441390583637,21.176449747467,15.5670034761916));
#38764=CARTESIAN_POINT('Ctrl Pts',(57.4499664993911,21.0957294493094,15.5627722558867));
#38765=CARTESIAN_POINT('Ctrl Pts',(57.4518017582841,21.01456881149,15.5585410355817));
#38766=CARTESIAN_POINT('Ctrl Pts',(57.4495946981662,20.9333962109485,15.5543098152768));
#38767=CARTESIAN_POINT('Ctrl Pts',(57.4473908028181,20.8523400062349,15.5500846622456));
#38768=CARTESIAN_POINT('Ctrl Pts',(57.4411561130793,20.7712723336967,15.5458595092145));
#38769=CARTESIAN_POINT('Ctrl Pts',(57.430892354873,20.6906254551192,15.5416343561833));
#38770=CARTESIAN_POINT('Ctrl Pts',(57.420602229485,20.6097713979573,15.5373983489041));
#38771=CARTESIAN_POINT('Ctrl Pts',(57.4062622805198,20.5293407707785,15.5331623416249));
#38772=CARTESIAN_POINT('Ctrl Pts',(57.3879269084726,20.4497679309669,15.5289263343457));
#38773=CARTESIAN_POINT('Ctrl Pts',(57.3696714193187,20.3705417712585,15.5247087823516));
#38774=CARTESIAN_POINT('Ctrl Pts',(57.3474553457982,20.2921663979111,15.5204912303574));
#38775=CARTESIAN_POINT('Ctrl Pts',(57.3213838769868,20.2150623300758,15.5162736783633));
#38776=CARTESIAN_POINT('Ctrl Pts',(57.2953210163812,20.1379837202497,15.5120575189089));
#38777=CARTESIAN_POINT('Ctrl Pts',(57.2654054372177,20.0621760224383,15.5078413594544));
#38778=CARTESIAN_POINT('Ctrl Pts',(57.2317921151758,19.9880443662694,15.5036252));
#38779=CARTESIAN_POINT('Ctrl Pts',(57.1981795940713,19.9139144765077,15.4994091410081));
#38780=CARTESIAN_POINT('Ctrl Pts',(57.1608696982766,19.8414609719537,15.4951930820162));
#38781=CARTESIAN_POINT('Ctrl Pts',(57.1200648657519,19.7710674489606,15.4909770230243));
#38782=CARTESIAN_POINT('Ctrl Pts',(57.0789260196019,19.7000977100059,15.4867264528958));
#38783=CARTESIAN_POINT('Ctrl Pts',(57.0342349827378,19.6312222558862,15.4824758827674));
#38784=CARTESIAN_POINT('Ctrl Pts',(56.9862446218527,19.5648057441025,15.4782253126389));
#38785=CARTESIAN_POINT('Ctrl Pts',(56.9385746967054,19.4988327010396,15.4740031239302));
#38786=CARTESIAN_POINT('Ctrl Pts',(56.8876497149417,19.435286190896,15.4697809352214));
#38787=CARTESIAN_POINT('Ctrl Pts',(56.8337578322622,19.3744900915045,15.4655587465127));
#38788=CARTESIAN_POINT('Ctrl Pts',(56.7793225602719,19.3130809879107,15.4612939856743));
#38789=CARTESIAN_POINT('Ctrl Pts',(56.721860560484,19.254478418646,15.457029224836));
#38790=CARTESIAN_POINT('Ctrl Pts',(56.6617052580061,19.1989764339368,15.4527644639977));
#38791=CARTESIAN_POINT('Ctrl Pts',(56.6015499555282,19.1434744492277,15.4484997031593));
#38792=CARTESIAN_POINT('Ctrl Pts',(56.5387017615516,19.0910733082628,15.444234942321));
#38793=CARTESIAN_POINT('Ctrl Pts',(56.4735248891911,19.042022816544,15.4399701814827));
#38794=CARTESIAN_POINT('Ctrl Pts',(56.4088606052612,18.9933580861183,15.4357389611778));
#38795=CARTESIAN_POINT('Ctrl Pts',(56.3416616840414,18.9478089665511,15.4315077408728));
#38796=CARTESIAN_POINT('Ctrl Pts',(56.2722608776796,18.9056498599504,15.4272765205679));
#38797=CARTESIAN_POINT('Ctrl Pts',(56.2029595872167,18.8635512065578,15.4230513675368));
#38798=CARTESIAN_POINT('Ctrl Pts',(56.131463076343,18.8248331510826,15.4188262145056));
#38799=CARTESIAN_POINT('Ctrl Pts',(56.0581354825333,18.7897286251222,15.4146010614744));
#38800=CARTESIAN_POINT('Ctrl Pts',(55.9846195130871,18.7545339170479,15.4103650541952));
#38801=CARTESIAN_POINT('Ctrl Pts',(55.9092634217106,18.7229716069748,15.4061290469161));
#38802=CARTESIAN_POINT('Ctrl Pts',(55.8324616679782,18.6952315037412,15.4018930396369));
#38803=CARTESIAN_POINT('Ctrl Pts',(55.7559945213801,18.6676122575975,15.3976754876427));
#38804=CARTESIAN_POINT('Ctrl Pts',(55.6780947202454,18.6437821494739,15.3934579356486));
#38805=CARTESIAN_POINT('Ctrl Pts',(55.599172635453,18.6238808104549,15.3892403836544));
#38806=CARTESIAN_POINT('Ctrl Pts',(55.5202766089375,18.6039860424054,15.3850242242));
#38807=CARTESIAN_POINT('Ctrl Pts',(55.4403594195168,18.5880175810119,15.3808080647455));
#38808=CARTESIAN_POINT('Ctrl Pts',(55.3598455026322,18.5760648803577,15.3765919052911));
#38809=CARTESIAN_POINT('Ctrl Pts',(55.2793335042311,18.5641124645121,15.3723758462992));
#38810=CARTESIAN_POINT('Ctrl Pts',(55.1982252666811,18.5561756863297,15.3681597873073));
#38811=CARTESIAN_POINT('Ctrl Pts',(55.1169528674894,18.5522924445951,15.3639437283154));
#38812=CARTESIAN_POINT('Ctrl Pts',(55.0350152017837,18.5483774160459,15.3596931581869));
#38813=CARTESIAN_POINT('Ctrl Pts',(54.9529111529,18.5485826307513,15.3554425880585));
#38814=CARTESIAN_POINT('Ctrl Pts',(54.8710842288119,18.5528933464315,15.35119201793));
#38815=CARTESIAN_POINT('Ctrl Pts',(54.7898036700836,18.5571752790951,15.3469698292212));
#38816=CARTESIAN_POINT('Ctrl Pts',(54.7087970073659,18.565507944601,15.3427476405125));
#38817=CARTESIAN_POINT('Ctrl Pts',(54.6284926185837,18.5778248379704,15.3385254518037));
#38818=CARTESIAN_POINT('Ctrl Pts',(54.5473785244376,18.5902659219946,15.3342606909654));
#38819=CARTESIAN_POINT('Ctrl Pts',(54.4669814217996,18.6067719339737,15.3299959301271));
#38820=CARTESIAN_POINT('Ctrl Pts',(54.3877291724453,18.6272221587925,15.3257311692887));
#38821=CARTESIAN_POINT('Ctrl Pts',(54.308476923091,18.6476723836113,15.3214664084504));
#38822=CARTESIAN_POINT('Ctrl Pts',(54.2303699677568,18.6720666163101,15.3172016476121));
#38823=CARTESIAN_POINT('Ctrl Pts',(54.1538156861656,18.7002342821451,15.3129368867737));
#38824=CARTESIAN_POINT('Ctrl Pts',(54.0778634714983,18.7281804212468,15.3087056664688));
#38825=CARTESIAN_POINT('Ctrl Pts',(54.0031547675905,18.7599456044963,15.3044744461639));
#38826=CARTESIAN_POINT('Ctrl Pts',(53.9301005622805,18.7953990285842,15.300243225859));
#38827=CARTESIAN_POINT('Ctrl Pts',(53.8571511115877,18.8308016149434,15.2960180728278));
#38828=CARTESIAN_POINT('Ctrl Pts',(53.7858518623981,18.8698817371529,15.2917929197966));
#38829=CARTESIAN_POINT('Ctrl Pts',(53.7165959753696,18.9124597346249,15.2875677667655));
#38830=CARTESIAN_POINT('Ctrl Pts',(53.6471621727555,18.9551471132582,15.2833317594863));
#38831=CARTESIAN_POINT('Ctrl Pts',(53.5797826851319,19.0013501929421,15.2790957522071));
#38832=CARTESIAN_POINT('Ctrl Pts',(53.5148308811937,19.0508404532866,15.2748597449279));
#38833=CARTESIAN_POINT('Ctrl Pts',(53.4501620569523,19.1001150962345,15.2706421929337));
#38834=CARTESIAN_POINT('Ctrl Pts',(53.3879001839283,19.1526480595771,15.2664246409396));
#38835=CARTESIAN_POINT('Ctrl Pts',(53.3283850971496,19.2081702462096,15.2622070889454));
#38836=CARTESIAN_POINT('Ctrl Pts',(53.2688896608987,19.2636741006792,15.257990929491));
#38837=CARTESIAN_POINT('Ctrl Pts',(53.2121395495531,19.3221649015494,15.2537747700365));
#38838=CARTESIAN_POINT('Ctrl Pts',(53.1584400637624,19.3833345271069,15.2495586105821));
#38839=CARTESIAN_POINT('Ctrl Pts',(53.1047418575217,19.4445026951162,15.2453425515902));
#38840=CARTESIAN_POINT('Ctrl Pts',(53.0540944381981,19.5083492107785,15.2411264925983));
#38841=CARTESIAN_POINT('Ctrl Pts',(53.0067639315506,19.5745315768379,15.2369104336064));
#38842=CARTESIAN_POINT('Ctrl Pts',(52.9590459944656,19.6412556878489,15.2326598634779));
#38843=CARTESIAN_POINT('Ctrl Pts',(52.91469981491,19.7103536857576,15.2284092933495));
#38844=CARTESIAN_POINT('Ctrl Pts',(52.8739534856068,19.781444925891,15.224158723221));
#38845=CARTESIAN_POINT('Ctrl Pts',(52.8334792230239,19.8520614837433,15.2199365345122));
#38846=CARTESIAN_POINT('Ctrl Pts',(52.7965570418537,19.9246443002822,15.2157143458035));
#38847=CARTESIAN_POINT('Ctrl Pts',(52.7633633381258,19.9987973767712,15.2114921570947));
#38848=CARTESIAN_POINT('Ctrl Pts',(52.729834943849,20.0736981352324,15.2072273962564));
#38849=CARTESIAN_POINT('Ctrl Pts',(52.7001108142751,20.1502005447704,15.2029626354181));
#38850=CARTESIAN_POINT('Ctrl Pts',(52.6743215162923,20.2278796464157,15.1986978745797));
#38851=CARTESIAN_POINT('Ctrl Pts',(52.6485322183096,20.3055587480609,15.1944331137414));
#38852=CARTESIAN_POINT('Ctrl Pts',(52.6266778186805,20.3844140603575,15.190168352903));
#38853=CARTESIAN_POINT('Ctrl Pts',(52.6088358846536,20.4640107991018,15.1859035920647));
#38854=CARTESIAN_POINT('Ctrl Pts',(52.5846673824411,20.5718317311566,15.1801265904459));
#38855=CARTESIAN_POINT('Ctrl Pts',(52.5677836834025,20.6813408102256,15.174349588827));
#38856=CARTESIAN_POINT('Ctrl Pts',(52.558368406975,20.7917083440411,15.1685725872082));
#38857=CARTESIAN_POINT('Ctrl Pts',(52.5525310073086,20.8601353743076,15.1649908902095));
#38858=CARTESIAN_POINT('Ctrl Pts',(52.549563542799,20.9288920271857,15.1614091932108));
#38859=CARTESIAN_POINT('Ctrl Pts',(52.5495010097519,20.9977754117357,15.1578274962121));
#38860=CARTESIAN_POINT('',(52.5495000127026,21.0002495104095,14.357827496162));
#38861=CARTESIAN_POINT('Ctrl Pts',(52.5495010097513,20.9977754123675,15.1578274961792));
#38862=CARTESIAN_POINT('Ctrl Pts',(52.5494282960771,21.0778733067042,15.1536626835815));
#38863=CARTESIAN_POINT('Ctrl Pts',(52.5532869724308,21.1580880860891,15.1494978709838));
#38864=CARTESIAN_POINT('Ctrl Pts',(52.561084728881,21.237996954398,15.1453330583861));
#38865=CARTESIAN_POINT('Ctrl Pts',(52.5688767052554,21.3178465903721,15.1411713329498));
#38866=CARTESIAN_POINT('Ctrl Pts',(52.5806019247079,21.3973902904168,15.1370096075135));
#38867=CARTESIAN_POINT('Ctrl Pts',(52.5962160347525,21.476206781156,15.1328478820771));
#38868=CARTESIAN_POINT('Ctrl Pts',(52.611823660692,21.5549905416011,15.1286878848895));
#38869=CARTESIAN_POINT('Ctrl Pts',(52.6313168800144,21.6330472229495,15.1245278877019));
#38870=CARTESIAN_POINT('Ctrl Pts',(52.6545998963697,21.7099638046343,15.1203678905143));
#38871=CARTESIAN_POINT('Ctrl Pts',(52.6778808328632,21.7868735153944,15.1162082649374));
#38872=CARTESIAN_POINT('Ctrl Pts',(52.7049507542299,21.8626428709612,15.1120486393605));
#38873=CARTESIAN_POINT('Ctrl Pts',(52.735663910154,21.936873695981,15.1078890137836));
#38874=CARTESIAN_POINT('Ctrl Pts',(52.7664052381512,22.0111726102662,15.1037255727318));
#38875=CARTESIAN_POINT('Ctrl Pts',(52.8007962928464,22.083929731569,15.09956213168));
#38876=CARTESIAN_POINT('Ctrl Pts',(52.8386433136779,22.1547673031788,15.0953986906283));
#38877=CARTESIAN_POINT('Ctrl Pts',(52.8765069502239,22.2256359741152,15.0912334217299));
#38878=CARTESIAN_POINT('Ctrl Pts',(52.917829326728,22.2945830068287,15.0870681528315));
#38879=CARTESIAN_POINT('Ctrl Pts',(52.9623722310994,22.3612579936974,15.0829028839331));
#38880=CARTESIAN_POINT('Ctrl Pts',(53.0069942770859,22.4280514453636,15.0787302143923));
#38881=CARTESIAN_POINT('Ctrl Pts',(53.0548479948803,22.4925644025959,15.0745575448515));
#38882=CARTESIAN_POINT('Ctrl Pts',(53.105653842797,22.5544783326538,15.0703848753107));
#38883=CARTESIAN_POINT('Ctrl Pts',(53.1523871463164,22.6114293059004,15.066546682659));
#38884=CARTESIAN_POINT('Ctrl Pts',(53.2016176127437,22.6661814128854,15.0627084900074));
#38885=CARTESIAN_POINT('Ctrl Pts',(53.2531015155089,22.7185156196214,15.0588702973557));
#38886=CARTESIAN_POINT('Ctrl Pts',(53.3098573259975,22.776208804482,15.0546390770508));
#38887=CARTESIAN_POINT('Ctrl Pts',(53.3695806882398,22.8311955056827,15.0504078567458));
#38888=CARTESIAN_POINT('Ctrl Pts',(53.4319830925651,22.8831551258455,15.0461766364409));
#38889=CARTESIAN_POINT('Ctrl Pts',(53.49429601621,22.9350402395496,15.0419514834098));
#38890=CARTESIAN_POINT('Ctrl Pts',(53.559279998046,22.9839065980349,15.0377263303786));
#38891=CARTESIAN_POINT('Ctrl Pts',(53.6266093548769,23.029469976592,15.0335011773475));
#38892=CARTESIAN_POINT('Ctrl Pts',(53.6941116781151,23.0751504056344,15.0292651700683));
#38893=CARTESIAN_POINT('Ctrl Pts',(53.7639711065245,23.1175105305989,15.0250291627891));
#38894=CARTESIAN_POINT('Ctrl Pts',(53.8358255905565,23.1563042907709,15.0207931555099));
#38895=CARTESIAN_POINT('Ctrl Pts',(53.9073670215419,23.1949290356757,15.0165756035157));
#38896=CARTESIAN_POINT('Ctrl Pts',(53.9808857526134,23.2300181971312,15.0123580515216));
#38897=CARTESIAN_POINT('Ctrl Pts',(54.0559965767771,23.2613729871349,15.0081404995274));
#38898=CARTESIAN_POINT('Ctrl Pts',(54.1310826010555,23.2927174245003,15.003924340073));
#38899=CARTESIAN_POINT('Ctrl Pts',(54.2077592458107,23.3203297600269,14.9997081806186));
#38900=CARTESIAN_POINT('Ctrl Pts',(54.2856199731486,23.3440587508072,14.9954920211641));
#38901=CARTESIAN_POINT('Ctrl Pts',(54.3634788452231,23.3677871761737,14.9912759621722));
#38902=CARTESIAN_POINT('Ctrl Pts',(54.4425212987326,23.3876323062963,14.9870599031803));
#38903=CARTESIAN_POINT('Ctrl Pts',(54.5223256129035,23.4034927563677,14.9828438441884));
#38904=CARTESIAN_POINT('Ctrl Pts',(54.6027831763745,23.4194830343565,14.9785932740599));
#38905=CARTESIAN_POINT('Ctrl Pts',(54.6840146633237,23.4314229876311,14.9743427039315));
#38906=CARTESIAN_POINT('Ctrl Pts',(54.7655792627784,23.4392616030185,14.970092133803));
#38907=CARTESIAN_POINT('Ctrl Pts',(54.8465992484373,23.4470478793016,14.9658699450943));
#38908=CARTESIAN_POINT('Ctrl Pts',(54.9279474398575,23.4507874610616,14.9616477563855));
#38909=CARTESIAN_POINT('Ctrl Pts',(55.0091903341992,23.4504827662641,14.9574255676768));
#38910=CARTESIAN_POINT('Ctrl Pts',(55.0912523968123,23.4501749992433,14.9531608068384));
#38911=CARTESIAN_POINT('Ctrl Pts',(55.1732065418967,23.4457409663673,14.9488960460001));
#38912=CARTESIAN_POINT('Ctrl Pts',(55.2546117595896,23.4372367759163,14.9446312851617));
#38913=CARTESIAN_POINT('Ctrl Pts',(55.3360169772825,23.4287325854653,14.9403665243234));
#38914=CARTESIAN_POINT('Ctrl Pts',(55.4168728013817,23.4161583749615,14.9361017634851));
#38915=CARTESIAN_POINT('Ctrl Pts',(55.496751104762,23.3996225932254,14.9318370026467));
#38916=CARTESIAN_POINT('Ctrl Pts',(55.5760011991983,23.3832168583924,14.9276057823418));
#38917=CARTESIAN_POINT('Ctrl Pts',(55.6545862816944,23.3628501670674,14.9233745620369));
#38918=CARTESIAN_POINT('Ctrl Pts',(55.7320805387498,23.3385911003816,14.919143341732));
#38919=CARTESIAN_POINT('Ctrl Pts',(55.8094636744645,23.3143668194994,14.9149181887008));
#38920=CARTESIAN_POINT('Ctrl Pts',(55.8857586513455,23.2862613860456,14.9106930356696));
#38921=CARTESIAN_POINT('Ctrl Pts',(55.9605500611977,23.2543943377176,14.9064678826385));
#38922=CARTESIAN_POINT('Ctrl Pts',(56.0355336071709,23.2224454242252,14.9022318753593));
#38923=CARTESIAN_POINT('Ctrl Pts',(56.1090053901096,23.1867156462173,14.8979958680801));
#38924=CARTESIAN_POINT('Ctrl Pts',(56.1805623499266,23.1473757910379,14.8937598608009));
#38925=CARTESIAN_POINT('Ctrl Pts',(56.2518075529398,23.1082073303328,14.8895423088067));
#38926=CARTESIAN_POINT('Ctrl Pts',(56.3211541689651,23.0654604016027,14.8853247568126));
#38927=CARTESIAN_POINT('Ctrl Pts',(56.3882263016474,23.0193508821932,14.8811072048184));
#38928=CARTESIAN_POINT('Ctrl Pts',(56.4552762886373,22.973256587098,14.876891045364));
#38929=CARTESIAN_POINT('Ctrl Pts',(56.5200529008093,22.9238021693007,14.8726748859096));
#38930=CARTESIAN_POINT('Ctrl Pts',(56.5822086247988,22.8712472091127,14.8684587264551));
#38931=CARTESIAN_POINT('Ctrl Pts',(56.6443628677435,22.8186935012029,14.8642426674632));
#38932=CARTESIAN_POINT('Ctrl Pts',(56.7038959923662,22.7630396988257,14.8600266084713));
#38933=CARTESIAN_POINT('Ctrl Pts',(56.7604941453531,22.7045851736353,14.8558105494794));
#38934=CARTESIAN_POINT('Ctrl Pts',(56.817555590384,22.6456521608086,14.8515599793509));
#38935=CARTESIAN_POINT('Ctrl Pts',(56.871633447534,22.5838726955937,14.8473094092225));
#38936=CARTESIAN_POINT('Ctrl Pts',(56.9224458363955,22.5195895025058,14.843058839094));
#38937=CARTESIAN_POINT('Ctrl Pts',(56.9729189465974,22.4557355337875,14.8388366503853));
#38938=CARTESIAN_POINT('Ctrl Pts',(57.0201698412542,22.3894115888414,14.8346144616765));
#38939=CARTESIAN_POINT('Ctrl Pts',(57.06396549732,22.3209832231608,14.8303922729677));
#38940=CARTESIAN_POINT('Ctrl Pts',(57.1082027429201,22.251864897497,14.8261275121294));
#38941=CARTESIAN_POINT('Ctrl Pts',(57.1489144387557,22.1805998965061,14.8218627512911));
#38942=CARTESIAN_POINT('Ctrl Pts',(57.1859086038108,22.1075891954087,14.8175979904528));
#38943=CARTESIAN_POINT('Ctrl Pts',(57.2229027688658,22.0345784943113,14.8133332296144));
#38944=CARTESIAN_POINT('Ctrl Pts',(57.2561792659063,21.9598225593947,14.8090684687761));
#38945=CARTESIAN_POINT('Ctrl Pts',(57.2855970775908,21.8837399215314,14.8048037079378));
#38946=CARTESIAN_POINT('Ctrl Pts',(57.3147835306757,21.8082556413142,14.8005724876328));
#38947=CARTESIAN_POINT('Ctrl Pts',(57.3402812640153,21.7311824105463,14.7963412673279));
#38948=CARTESIAN_POINT('Ctrl Pts',(57.3619170165232,21.6529151989793,14.792110047023));
#38949=CARTESIAN_POINT('Ctrl Pts',(57.3835217448763,21.5747602171159,14.7878848939918));
#38950=CARTESIAN_POINT('Ctrl Pts',(57.4012753680749,21.4954150991174,14.7836597409607));
#38951=CARTESIAN_POINT('Ctrl Pts',(57.4150530825258,21.4152937015926,14.7794345879295));
#38952=CARTESIAN_POINT('Ctrl Pts',(57.4288661913705,21.3349664754231,14.7751985806503));
#38953=CARTESIAN_POINT('Ctrl Pts',(57.4386827731848,21.2538594187254,14.7709625733711));
#38954=CARTESIAN_POINT('Ctrl Pts',(57.4444277815552,21.172403801469,14.7667265660919));
#38955=CARTESIAN_POINT('Ctrl Pts',(57.4501477602786,21.0913030671333,14.7625090140978));
#38956=CARTESIAN_POINT('Ctrl Pts',(57.4518315282674,21.0098572692345,14.7582914621036));
#38957=CARTESIAN_POINT('Ctrl Pts',(57.449456654091,20.9284993025971,14.7540739101095));
#38958=CARTESIAN_POINT('Ctrl Pts',(57.4470825640441,20.8471681985094,14.749857750655));
#38959=CARTESIAN_POINT('Ctrl Pts',(57.4406525065804,20.7659253324522,14.7456415912006));
#38960=CARTESIAN_POINT('Ctrl Pts',(57.4301961609244,20.68520344756,14.7414254317462));
#38961=CARTESIAN_POINT('Ctrl Pts',(57.419740064422,20.6044834861068,14.7372093727543));
#38962=CARTESIAN_POINT('Ctrl Pts',(57.4052579313016,20.5242849420636,14.7329933137624));
#38963=CARTESIAN_POINT('Ctrl Pts',(57.3868311260961,20.4450338519344,14.7287772547705));
#38964=CARTESIAN_POINT('Ctrl Pts',(57.3682534857167,20.3651340409973,14.724526684642));
#38965=CARTESIAN_POINT('Ctrl Pts',(57.3456663888561,20.2861977374888,14.7202761145136));
#38966=CARTESIAN_POINT('Ctrl Pts',(57.3192049630619,20.2086476200142,14.7160255443851));
#38967=CARTESIAN_POINT('Ctrl Pts',(57.2929202224673,20.1316153112963,14.7118033556763));
#38968=CARTESIAN_POINT('Ctrl Pts',(57.2628129648474,20.0559511470064,14.7075811669676));
#38969=CARTESIAN_POINT('Ctrl Pts',(57.2290639926738,19.9820491335211,14.7033589782588));
#38970=CARTESIAN_POINT('Ctrl Pts',(57.1949747312058,19.9074019695199,14.6990942174205));
#38971=CARTESIAN_POINT('Ctrl Pts',(57.1571701271272,19.8345531228955,14.6948294565822));
#38972=CARTESIAN_POINT('Ctrl Pts',(57.1158829977023,19.7638813204088,14.6905646957438));
#38973=CARTESIAN_POINT('Ctrl Pts',(57.0745958682774,19.6932095179222,14.6862999349055));
#38974=CARTESIAN_POINT('Ctrl Pts',(57.0298265308859,19.6247151277135,14.6820351740672));
#38975=CARTESIAN_POINT('Ctrl Pts',(56.9818501872891,19.5587435741194,14.6777704132288));
#38976=CARTESIAN_POINT('Ctrl Pts',(56.9342511572664,19.4932908587863,14.6735391929239));
#38977=CARTESIAN_POINT('Ctrl Pts',(56.8833169303911,19.4300759725721,14.669307972619));
#38978=CARTESIAN_POINT('Ctrl Pts',(56.8292854282746,19.3694586567946,14.6650767523141));
#38979=CARTESIAN_POINT('Ctrl Pts',(56.7753314035505,19.3089282620052,14.6608515992829));
#38980=CARTESIAN_POINT('Ctrl Pts',(56.7182892310374,19.2509883841845,14.6566264462518));
#38981=CARTESIAN_POINT('Ctrl Pts',(56.6584389764634,19.1959682898167,14.6524012932206));
#38982=CARTESIAN_POINT('Ctrl Pts',(56.5984349689949,19.1408068510414,14.6481652859414));
#38983=CARTESIAN_POINT('Ctrl Pts',(56.5356087161047,19.0885805944986,14.6439292786622));
#38984=CARTESIAN_POINT('Ctrl Pts',(56.4702818942719,19.0395864208346,14.639693271383));
#38985=CARTESIAN_POINT('Ctrl Pts',(56.4052396860006,18.9908057032345,14.6354757193889));
#38986=CARTESIAN_POINT('Ctrl Pts',(56.3377190215193,18.9452292516613,14.6312581673947));
#38987=CARTESIAN_POINT('Ctrl Pts',(56.26807147156,18.9031106388234,14.6270406154005));
#38988=CARTESIAN_POINT('Ctrl Pts',(56.1984469176373,18.8610059325932,14.6228244559461));
#38989=CARTESIAN_POINT('Ctrl Pts',(56.1266972703255,18.8223570382393,14.6186082964917));
#38990=CARTESIAN_POINT('Ctrl Pts',(56.0532022284365,18.7873736610045,14.6143921370373));
#38991=CARTESIAN_POINT('Ctrl Pts',(55.9797089377853,18.7523911173528,14.6101760780454));
#38992=CARTESIAN_POINT('Ctrl Pts',(55.9044707555147,18.7210741159802,14.6059600190535));
#38993=CARTESIAN_POINT('Ctrl Pts',(55.8278897701911,18.6935852978242,14.6017439600616));
#38994=CARTESIAN_POINT('Ctrl Pts',(55.7506819205734,18.6658714661283,14.5974933899331));
#38995=CARTESIAN_POINT('Ctrl Pts',(55.6721096291193,18.6420489563563,14.5932428198046));
#38996=CARTESIAN_POINT('Ctrl Pts',(55.5926013144509,18.6222334151328,14.5889922496761));
#38997=CARTESIAN_POINT('Ctrl Pts',(55.5136238835892,18.6025501839702,14.5847700609674));
#38998=CARTESIAN_POINT('Ctrl Pts',(55.4337233638658,18.5868206046054,14.5805478722586));
#38999=CARTESIAN_POINT('Ctrl Pts',(55.3533288484233,18.5751063992678,14.5763256835499));
#39000=CARTESIAN_POINT('Ctrl Pts',(55.2721237188736,18.5632740801503,14.5720609227115));
#39001=CARTESIAN_POINT('Ctrl Pts',(55.1904150592977,18.5555386102629,14.5677961618732));
#39002=CARTESIAN_POINT('Ctrl Pts',(55.108647327921,18.5519097222252,14.5635314010349));
#39003=CARTESIAN_POINT('Ctrl Pts',(55.0268795965444,18.5482808341875,14.5592666401965));
#39004=CARTESIAN_POINT('Ctrl Pts',(54.9450532747815,18.5487584609394,14.5550018793582));
#39005=CARTESIAN_POINT('Ctrl Pts',(54.8636078207827,18.5532986648452,14.5507371185198));
#39006=CARTESIAN_POINT('Ctrl Pts',(54.7828029007025,18.5578031619748,14.5465058982149));
#39007=CARTESIAN_POINT('Ctrl Pts',(54.7020698672391,18.5663234092867,14.54227467791));
#39008=CARTESIAN_POINT('Ctrl Pts',(54.6218399940656,18.5788545562252,14.5380434576051));
#39009=CARTESIAN_POINT('Ctrl Pts',(54.541725164915,18.591367734376,14.5338183045739));
#39010=CARTESIAN_POINT('Ctrl Pts',(54.4621125185849,18.6078803184009,14.5295931515428));
#39011=CARTESIAN_POINT('Ctrl Pts',(54.3834305741755,18.6283355226469,14.5253679985116));
#39012=CARTESIAN_POINT('Ctrl Pts',(54.3045464990183,18.6488432754892,14.5211319912324));
#39013=CARTESIAN_POINT('Ctrl Pts',(54.2265983846976,18.6733138986637,14.5168959839532));
#39014=CARTESIAN_POINT('Ctrl Pts',(54.1500101176497,18.7016380942284,14.512659976674));
#39015=CARTESIAN_POINT('Ctrl Pts',(54.0737555276249,18.7298388879507,14.5084424246799));
#39016=CARTESIAN_POINT('Ctrl Pts',(53.9988494021766,18.7618595912587,14.5042248726857));
#39017=CARTESIAN_POINT('Ctrl Pts',(53.9256954313916,18.7975422946474,14.5000073206915));
#39018=CARTESIAN_POINT('Ctrl Pts',(53.8525656143835,18.8332132164192,14.4957911612371));
#39019=CARTESIAN_POINT('Ctrl Pts',(53.7811872207097,18.872543533488,14.4915750017827));
#39020=CARTESIAN_POINT('Ctrl Pts',(53.7119423331204,18.9153279162437,14.4873588423282));
#39021=CARTESIAN_POINT('Ctrl Pts',(53.6426990954968,18.9581112795341,14.4831427833363));
#39022=CARTESIAN_POINT('Ctrl Pts',(53.5755896578124,19.0043482995508,14.4789267243445));
#39023=CARTESIAN_POINT('Ctrl Pts',(53.510968697937,19.0537893147255,14.4747106653526));
#39024=CARTESIAN_POINT('Ctrl Pts',(53.4458187742172,19.1036350361984,14.4704600952241));
#39025=CARTESIAN_POINT('Ctrl Pts',(53.3831986466606,19.1567371696865,14.4662095250956));
#39026=CARTESIAN_POINT('Ctrl Pts',(53.3234377835841,19.2127984488349,14.4619589549671));
#39027=CARTESIAN_POINT('Ctrl Pts',(53.2640759488937,19.2684854020352,14.4577367662584));
#39028=CARTESIAN_POINT('Ctrl Pts',(53.207535593352,19.3270917234887,14.4535145775496));
#39029=CARTESIAN_POINT('Ctrl Pts',(53.1541012418314,19.3882903411,14.4492923888409));
#39030=CARTESIAN_POINT('Ctrl Pts',(53.100128114265,19.4501060214858,14.4450276280025));
#39031=CARTESIAN_POINT('Ctrl Pts',(53.0493242793575,19.5145661867257,14.4407628671642));
#39032=CARTESIAN_POINT('Ctrl Pts',(53.0019389097557,19.5813026645363,14.4364981063258));
#39033=CARTESIAN_POINT('Ctrl Pts',(52.9545535401539,19.648039142347,14.4322333454875));
#39034=CARTESIAN_POINT('Ctrl Pts',(52.910586840545,19.7170514918654,14.4279685846492));
#39035=CARTESIAN_POINT('Ctrl Pts',(52.8702401767789,19.7879466408639,14.4237038238108));
#39036=CARTESIAN_POINT('Ctrl Pts',(52.8284883593983,19.8613108558412,14.4192905341092));
#39037=CARTESIAN_POINT('Ctrl Pts',(52.7904674409891,19.9369463614327,14.4148772444075));
#39038=CARTESIAN_POINT('Ctrl Pts',(52.756419745081,20.0144555363974,14.4104639547059));
#39039=CARTESIAN_POINT('Ctrl Pts',(52.7224608961013,20.091762452386,14.4060621814145));
#39040=CARTESIAN_POINT('Ctrl Pts',(52.6924547829151,20.1709329286654,14.4016604081231));
#39041=CARTESIAN_POINT('Ctrl Pts',(52.666597893662,20.2515450179622,14.3972586348317));
#39042=CARTESIAN_POINT('Ctrl Pts',(52.6407808104884,20.3320330068224,14.3928636379679));
#39043=CARTESIAN_POINT('Ctrl Pts',(52.619100371865,20.4139578091949,14.3884686411041));
#39044=CARTESIAN_POINT('Ctrl Pts',(52.6017052240549,20.4968773333724,14.3840736442403));
#39045=CARTESIAN_POINT('Ctrl Pts',(52.5843426400325,20.5796416318623,14.3796868748286));
#39046=CARTESIAN_POINT('Ctrl Pts',(52.5712494539419,20.6633965462017,14.3753001054169));
#39047=CARTESIAN_POINT('Ctrl Pts',(52.5625242722944,20.7476860549908,14.3709133360052));
#39048=CARTESIAN_POINT('Ctrl Pts',(52.5538484626429,20.8314986062273,14.3665513894075));
#39049=CARTESIAN_POINT('Ctrl Pts',(52.5494914180731,20.9158393193652,14.3621894428098));
#39050=CARTESIAN_POINT('Ctrl Pts',(52.5495000127025,21.0002495094391,14.3578274962121));
#39051=CARTESIAN_POINT('',(52.5495008975342,21.0020973350978,13.5578274962436));
#39052=CARTESIAN_POINT('Ctrl Pts',(52.5495000127026,21.0002495104095,14.357827496162));
#39053=CARTESIAN_POINT('Ctrl Pts',(52.5495087833097,21.086387690449,14.3533762546587));
#39054=CARTESIAN_POINT('Ctrl Pts',(52.5540636293478,21.1724239248653,14.3489250131554));
#39055=CARTESIAN_POINT('Ctrl Pts',(52.5631068447131,21.2578798164185,14.3444737716521));
#39056=CARTESIAN_POINT('Ctrl Pts',(52.5721783102097,21.3436026639214,14.3400086249004));
#39057=CARTESIAN_POINT('Ctrl Pts',(52.5857661358387,21.4287411624085,14.3355434781487));
#39058=CARTESIAN_POINT('Ctrl Pts',(52.6037610884995,21.5128248521774,14.3310783313969));
#39059=CARTESIAN_POINT('Ctrl Pts',(52.6217854790889,21.5970460943875,14.3266058801152));
#39060=CARTESIAN_POINT('Ctrl Pts',(52.644231278249,21.6802087171782,14.3221334288335));
#39061=CARTESIAN_POINT('Ctrl Pts',(52.6709395064187,21.7618579048871,14.3176609775517));
#39062=CARTESIAN_POINT('Ctrl Pts',(52.697723286547,21.8437380609705,14.3131758746462));
#39063=CARTESIAN_POINT('Ctrl Pts',(52.7287934648449,21.9240958649999,14.3086907717407));
#39064=CARTESIAN_POINT('Ctrl Pts',(52.7639427262882,22.0024959444708,14.3042056688353));
#39065=CARTESIAN_POINT('Ctrl Pts',(52.7836267485637,22.0464009611722,14.3016939555908));
#39066=CARTESIAN_POINT('Ctrl Pts',(52.804589200067,22.089692456157,14.2991822423463));
#39067=CARTESIAN_POINT('Ctrl Pts',(52.8267876118373,22.1322977373184,14.2966705291019));
#39068=CARTESIAN_POINT('Ctrl Pts',(52.864182951782,22.2040703933512,14.292439308797));
#39069=CARTESIAN_POINT('Ctrl Pts',(52.9052077781994,22.2741230943974,14.288208088492));
#39070=CARTESIAN_POINT('Ctrl Pts',(52.9496799904678,22.3420648674755,14.2839768681871));
#39071=CARTESIAN_POINT('Ctrl Pts',(52.9940884326965,22.4099092168063,14.2797517151559));
#39072=CARTESIAN_POINT('Ctrl Pts',(53.0419341905162,22.4756482641494,14.2755265621248));
#39073=CARTESIAN_POINT('Ctrl Pts',(53.0929889755298,22.5389149432471,14.2713014090936));
#39074=CARTESIAN_POINT('Ctrl Pts',(53.1441749182307,22.6023441518962,14.2670654018144));
#39075=CARTESIAN_POINT('Ctrl Pts',(53.1985861731568,22.6632878575766,14.2628293945352));
#39076=CARTESIAN_POINT('Ctrl Pts',(53.2559485119627,22.7214048498465,14.258593387256));
#39077=CARTESIAN_POINT('Ctrl Pts',(53.3130609365822,22.7792686400826,14.2543758352619));
#39078=CARTESIAN_POINT('Ctrl Pts',(53.3730984615083,22.8343299574548,14.2501582832677));
#39079=CARTESIAN_POINT('Ctrl Pts',(53.4357508848395,22.8862860217156,14.2459407312735));
#39080=CARTESIAN_POINT('Ctrl Pts',(53.4983826217658,22.9382249312659,14.2417245718191));
#39081=CARTESIAN_POINT('Ctrl Pts',(53.5636271849506,22.9870603272302,14.2375084123647));
#39082=CARTESIAN_POINT('Ctrl Pts',(53.6311400658923,23.0325286543601,14.2332922529102));
#39083=CARTESIAN_POINT('Ctrl Pts',(53.6986513381388,23.0779958980718,14.2290761939183));
#39084=CARTESIAN_POINT('Ctrl Pts',(53.7684304344367,23.1200959736802,14.2248601349264));
#39085=CARTESIAN_POINT('Ctrl Pts',(53.8401037421017,23.1586085612991,14.2206440759345));
#39086=CARTESIAN_POINT('Ctrl Pts',(53.9123637415835,23.197436399054,14.216393505806));
#39087=CARTESIAN_POINT('Ctrl Pts',(53.9865486912519,23.2326175047625,14.2121429356776));
#39088=CARTESIAN_POINT('Ctrl Pts',(54.0622519876235,23.2639741419203,14.2078923655491));
#39089=CARTESIAN_POINT('Ctrl Pts',(54.1374498066208,23.2951214081342,14.2036701768403));
#39090=CARTESIAN_POINT('Ctrl Pts',(54.2141452948428,23.3224950232675,14.1994479881316));
#39091=CARTESIAN_POINT('Ctrl Pts',(54.291923206468,23.3459704824361,14.1952257994228));
#39092=CARTESIAN_POINT('Ctrl Pts',(54.3704853491071,23.3696826435521,14.1909610385845));
#39093=CARTESIAN_POINT('Ctrl Pts',(54.450151394513,23.3894174795893,14.1866962777461));
#39094=CARTESIAN_POINT('Ctrl Pts',(54.5304832116662,23.4050996310907,14.1824315169078));
#39095=CARTESIAN_POINT('Ctrl Pts',(54.6108150288194,23.4207817825921,14.1781667560695));
#39096=CARTESIAN_POINT('Ctrl Pts',(54.6918121316814,23.4324112446808,14.1739019952312));
#39097=CARTESIAN_POINT('Ctrl Pts',(54.773033396672,23.4399664774283,14.1696372343928));
#39098=CARTESIAN_POINT('Ctrl Pts',(54.8536158908956,23.4474622914777,14.1654060140879));
#39099=CARTESIAN_POINT('Ctrl Pts',(54.9347212049248,23.45097588546,14.161174793783));
#39100=CARTESIAN_POINT('Ctrl Pts',(55.0159220904974,23.4504482726706,14.156943573478));
#39101=CARTESIAN_POINT('Ctrl Pts',(55.0970065396835,23.4499214164409,14.1527184204469));
#39102=CARTESIAN_POINT('Ctrl Pts',(55.1781858272457,23.4453648653576,14.1484932674157));
#39103=CARTESIAN_POINT('Ctrl Pts',(55.2590277481769,23.4367714040661,14.1442681143846));
#39104=CARTESIAN_POINT('Ctrl Pts',(55.3400773487485,23.4281558665185,14.1400321071054));
#39105=CARTESIAN_POINT('Ctrl Pts',(55.4207873765294,23.4154826135697,14.1357960998262));
#39106=CARTESIAN_POINT('Ctrl Pts',(55.5007224418401,23.3987970498226,14.131560092547));
#39107=CARTESIAN_POINT('Ctrl Pts',(55.5803092489166,23.3821841811431,14.1273425405528));
#39108=CARTESIAN_POINT('Ctrl Pts',(55.6591273724268,23.3615939777363,14.1231249885587));
#39109=CARTESIAN_POINT('Ctrl Pts',(55.7367542074522,23.3371229081504,14.1189074365645));
#39110=CARTESIAN_POINT('Ctrl Pts',(55.8143554118625,23.312659918355,14.1146912771101));
#39111=CARTESIAN_POINT('Ctrl Pts',(55.8907656658357,23.2843187466799,14.1104751176557));
#39112=CARTESIAN_POINT('Ctrl Pts',(55.9655767208969,23.2522459559431,14.1062589582012));
#39113=CARTESIAN_POINT('Ctrl Pts',(56.0403859933623,23.2201739294359,14.1020428992093));
#39114=CARTESIAN_POINT('Ctrl Pts',(56.1135957158085,23.18437064487,14.0978268402174));
#39115=CARTESIAN_POINT('Ctrl Pts',(56.1848181867184,23.1450305625844,14.0936107812255));
#39116=CARTESIAN_POINT('Ctrl Pts',(56.2566236590583,23.1053684565902,14.0893602110971));
#39117=CARTESIAN_POINT('Ctrl Pts',(56.3264087681686,23.0621116016115,14.0851096409686));
#39118=CARTESIAN_POINT('Ctrl Pts',(56.3938037042642,23.0155052676635,14.0808590708401));
#39119=CARTESIAN_POINT('Ctrl Pts',(56.4607486386162,22.9692101281873,14.0766368821314));
#39120=CARTESIAN_POINT('Ctrl Pts',(56.525334886809,22.9196104380325,14.0724146934226));
#39121=CARTESIAN_POINT('Ctrl Pts',(56.5872326800828,22.8669875921594,14.0681925047139));
#39122=CARTESIAN_POINT('Ctrl Pts',(56.6497545858865,22.8138341526136,14.0639277438755));
#39123=CARTESIAN_POINT('Ctrl Pts',(56.7095331626611,22.7575965824059,14.0596629830372));
#39124=CARTESIAN_POINT('Ctrl Pts',(56.766267526519,22.6986021531731,14.0553982221989));
#39125=CARTESIAN_POINT('Ctrl Pts',(56.823001890377,22.6396077239403,14.0511334613605));
#39126=CARTESIAN_POINT('Ctrl Pts',(56.87669177368,22.5778568414246,14.0468687005222));
#39127=CARTESIAN_POINT('Ctrl Pts',(56.9270798909799,22.5137084738419,14.0426039396839));
#39128=CARTESIAN_POINT('Ctrl Pts',(56.9770717271293,22.4500646059364,14.0383727193789));
#39129=CARTESIAN_POINT('Ctrl Pts',(57.0240010454368,22.3838221996572,14.034141499074));
#39130=CARTESIAN_POINT('Ctrl Pts',(57.0675866198488,22.3153082602273,14.0299102787691));
#39131=CARTESIAN_POINT('Ctrl Pts',(57.1111096955978,22.2468925649912,14.0256851257379));
#39132=CARTESIAN_POINT('Ctrl Pts',(57.151298302633,22.1762121946507,14.0214599727068));
#39133=CARTESIAN_POINT('Ctrl Pts',(57.1879120273654,22.103626390818,14.0172348196756));
#39134=CARTESIAN_POINT('Ctrl Pts',(57.2246198112825,22.0308541169774,14.0129988123964));
#39135=CARTESIAN_POINT('Ctrl Pts',(57.2577340354098,21.9561669823079,14.0087628051172));
#39136=CARTESIAN_POINT('Ctrl Pts',(57.2870567725089,21.8799554359858,14.0045267978381));
#39137=CARTESIAN_POINT('Ctrl Pts',(57.3162517573556,21.8040759254035,14.0003092458439));
#39138=CARTESIAN_POINT('Ctrl Pts',(57.3416880478648,21.726685692201,13.9960916938497));
#39139=CARTESIAN_POINT('Ctrl Pts',(57.3632175547077,21.6481921313324,13.9918741418556));
#39140=CARTESIAN_POINT('Ctrl Pts',(57.3847399529972,21.5697244872519,13.9876579824012));
#39141=CARTESIAN_POINT('Ctrl Pts',(57.4023580063605,21.4901546869514,13.9834418229467));
#39142=CARTESIAN_POINT('Ctrl Pts',(57.4159735008235,21.4099052248002,13.9792256634923));
#39143=CARTESIAN_POINT('Ctrl Pts',(57.4295886708569,21.3296576748311,13.9750096045004));
#39144=CARTESIAN_POINT('Ctrl Pts',(57.4392013949395,21.2487309537676,13.9707935455085));
#39145=CARTESIAN_POINT('Ctrl Pts',(57.4447648452976,21.1675562627805,13.9665774865166));
#39146=CARTESIAN_POINT('Ctrl Pts',(57.4503738360515,21.0857171050834,13.9623269163881));
#39147=CARTESIAN_POINT('Ctrl Pts',(57.4518669064955,21.0036263766372,13.9580763462597));
#39148=CARTESIAN_POINT('Ctrl Pts',(57.4492496222306,20.9217277954623,13.9538257761312));
#39149=CARTESIAN_POINT('Ctrl Pts',(57.4466498137962,20.8403760581075,13.9496035874224));
#39150=CARTESIAN_POINT('Ctrl Pts',(57.4399944738528,20.7592143727547,13.9453813987137));
#39151=CARTESIAN_POINT('Ctrl Pts',(57.4293412325764,20.6786724012723,13.9411592100049));
#39152=CARTESIAN_POINT('Ctrl Pts',(57.4185805751708,20.5973183288908,13.9368944491666));
#39153=CARTESIAN_POINT('Ctrl Pts',(57.4037410291872,20.5165970156022,13.9326296883283));
#39154=CARTESIAN_POINT('Ctrl Pts',(57.3849344340167,20.4369387285195,13.9283649274899));
#39155=CARTESIAN_POINT('Ctrl Pts',(57.3661278388462,20.3572804414367,13.9241001666516));
#39156=CARTESIAN_POINT('Ctrl Pts',(57.3433543902884,20.2786856254416,13.9198354058133));
#39157=CARTESIAN_POINT('Ctrl Pts',(57.3167762003472,20.2015651012732,13.9155706449749));
#39158=CARTESIAN_POINT('Ctrl Pts',(57.2904070365862,20.1250510972863,13.91133942467));
#39159=CARTESIAN_POINT('Ctrl Pts',(57.2601939249194,20.0497013448655,13.9071082043651));
#39160=CARTESIAN_POINT('Ctrl Pts',(57.2262591397946,19.975929449461,13.9028769840602));
#39161=CARTESIAN_POINT('Ctrl Pts',(57.1923730147765,19.9022633377913,13.898651831029));
#39162=CARTESIAN_POINT('Ctrl Pts',(57.1547760078794,19.8301710083846,13.8944266779979));
#39163=CARTESIAN_POINT('Ctrl Pts',(57.1136396091149,19.7600492538893,13.8902015249667));
#39164=CARTESIAN_POINT('Ctrl Pts',(57.072397532598,19.6897473594296,13.8859655176875));
#39165=CARTESIAN_POINT('Ctrl Pts',(57.0275980156906,19.6214266216587,13.8817295104083));
#39166=CARTESIAN_POINT('Ctrl Pts',(56.9794618071307,19.5554650561129,13.8774935031291));
#39167=CARTESIAN_POINT('Ctrl Pts',(56.9315353166829,19.4897908695571,13.8732759511349));
#39168=CARTESIAN_POINT('Ctrl Pts',(56.8803014175048,19.4264557241399,13.8690583991408));
#39169=CARTESIAN_POINT('Ctrl Pts',(56.826022119979,19.365804948194,13.8648408471466));
#39170=CARTESIAN_POINT('Ctrl Pts',(56.7717607442425,19.3051741977545,13.8606246876922));
#39171=CARTESIAN_POINT('Ctrl Pts',(56.7144562767869,19.2472264028543,13.8564085282378));
#39172=CARTESIAN_POINT('Ctrl Pts',(56.6544104585641,19.1922731720213,13.8521923687833));
#39173=CARTESIAN_POINT('Ctrl Pts',(56.5943660711114,19.1373212506125,13.8479763097914));
#39174=CARTESIAN_POINT('Ctrl Pts',(56.5315808064862,19.0853640644655,13.8437602507995));
#39175=CARTESIAN_POINT('Ctrl Pts',(56.4663915841226,19.0366747666231,13.8395441918076));
#39176=CARTESIAN_POINT('Ctrl Pts',(56.4006687463233,18.9875869157693,13.8352936216792));
#39177=CARTESIAN_POINT('Ctrl Pts',(56.3325027880108,18.9418209995924,13.8310430515507));
#39178=CARTESIAN_POINT('Ctrl Pts',(56.2622695545512,18.8996129352776,13.8267924814222));
#39179=CARTESIAN_POINT('Ctrl Pts',(56.1925052743889,18.8576866978126,13.8225702927135));
#39180=CARTESIAN_POINT('Ctrl Pts',(56.1207016848963,18.8192711117173,13.8183481040047));
#39181=CARTESIAN_POINT('Ctrl Pts',(56.047251051513,18.7845507261269,13.8141259152959));
#39182=CARTESIAN_POINT('Ctrl Pts',(55.9730598188581,18.7494802565264,13.8098611544576));
#39183=CARTESIAN_POINT('Ctrl Pts',(55.897188590317,18.7181801091831,13.8055963936193));
#39184=CARTESIAN_POINT('Ctrl Pts',(55.8200595332974,18.6907896129092,13.8013316327809));
#39185=CARTESIAN_POINT('Ctrl Pts',(55.7429304762778,18.6633991166354,13.7970668719426));
#39186=CARTESIAN_POINT('Ctrl Pts',(55.6645440707518,18.6399183481377,13.7928021111043));
#39187=CARTESIAN_POINT('Ctrl Pts',(55.5853334035044,18.6204338511523,13.7885373502659));
#39188=CARTESIAN_POINT('Ctrl Pts',(55.5067456945264,18.6011025914636,13.784306129961));
#39189=CARTESIAN_POINT('Ctrl Pts',(55.4270519584008,18.5856324353945,13.7800749096561));
#39190=CARTESIAN_POINT('Ctrl Pts',(55.3466660209323,18.5741449095358,13.7758436893511));
#39191=CARTESIAN_POINT('Ctrl Pts',(55.266395351272,18.5626738559852,13.77161853632));
#39192=CARTESIAN_POINT('Ctrl Pts',(55.1854349079469,18.5551741557584,13.7673933832888));
#39193=CARTESIAN_POINT('Ctrl Pts',(55.1042110758042,18.5517168665206,13.7631682302577));
#39194=CARTESIAN_POINT('Ctrl Pts',(55.0227785829066,18.5482506956459,13.7589322229785));
#39195=CARTESIAN_POINT('Ctrl Pts',(54.9410818060719,18.5488478384384,13.7546962156993));
#39196=CARTESIAN_POINT('Ctrl Pts',(54.8595580621108,18.5535277822787,13.7504602084201));
#39197=CARTESIAN_POINT('Ctrl Pts',(54.7783894978822,18.5581873367071,13.7462426564259));
#39198=CARTESIAN_POINT('Ctrl Pts',(54.6973929295162,18.5668941721216,13.7420251044318));
#39199=CARTESIAN_POINT('Ctrl Pts',(54.6170005818436,18.5796153826939,13.7378075524376));
#39200=CARTESIAN_POINT('Ctrl Pts',(54.5366347778953,18.5923323930119,13.7335913929832));
#39201=CARTESIAN_POINT('Ctrl Pts',(54.4568732573093,18.609061073712,13.7293752335287));
#39202=CARTESIAN_POINT('Ctrl Pts',(54.3781414551259,18.6297168523219,13.7251590740743));
#39203=CARTESIAN_POINT('Ctrl Pts',(54.2994115289618,18.6503721387463,13.7209430150824));
#39204=CARTESIAN_POINT('Ctrl Pts',(54.2217117218376,18.6749542179751,13.7167269560905));
#39205=CARTESIAN_POINT('Ctrl Pts',(54.1454542316759,18.7033281079267,13.7125108970986));
#39206=CARTESIAN_POINT('Ctrl Pts',(54.0685725252348,18.7319342562963,13.7082603269702));
#39207=CARTESIAN_POINT('Ctrl Pts',(53.9931573125182,18.7643944264607,13.7040097568417));
#39208=CARTESIAN_POINT('Ctrl Pts',(53.919610611055,18.8005207392987,13.6997591867132));
#39209=CARTESIAN_POINT('Ctrl Pts',(53.8465549871979,18.8364058336609,13.6955369980045));
#39210=CARTESIAN_POINT('Ctrl Pts',(53.7753433787473,18.8759079796906,13.6913148092957));
#39211=CARTESIAN_POINT('Ctrl Pts',(53.7063435453016,18.9187976486614,13.687092620587));
#39212=CARTESIAN_POINT('Ctrl Pts',(53.6366479897902,18.9621197721412,13.6828278597486));
#39213=CARTESIAN_POINT('Ctrl Pts',(53.5692094619455,19.008897838649,13.6785630989103));
#39214=CARTESIAN_POINT('Ctrl Pts',(53.5043739391514,19.0588526753205,13.6742983380719));
#39215=CARTESIAN_POINT('Ctrl Pts',(53.4395384163572,19.108807511992,13.6700335772336));
#39216=CARTESIAN_POINT('Ctrl Pts',(53.3773062233166,19.1619387571298,13.6657688163953));
#39217=CARTESIAN_POINT('Ctrl Pts',(53.31798490625,19.2179294418017,13.6615040555569));
#39218=CARTESIAN_POINT('Ctrl Pts',(53.2578972260675,19.2746434616538,13.6571841989189));
#39219=CARTESIAN_POINT('Ctrl Pts',(53.2005478250414,19.3345261821984,13.6528643422808));
#39220=CARTESIAN_POINT('Ctrl Pts',(53.1462943772196,19.3972755339509,13.6485444856428));
#39221=CARTESIAN_POINT('Ctrl Pts',(53.0940287468598,19.4577257828418,13.6443829062535));
#39222=CARTESIAN_POINT('Ctrl Pts',(53.0446365371086,19.5208358806471,13.6402213268642));
#39223=CARTESIAN_POINT('Ctrl Pts',(52.9984030747795,19.5862956465556,13.6360597474749));
#39224=CARTESIAN_POINT('Ctrl Pts',(52.9522128951036,19.6516941306087,13.631902064056));
#39225=CARTESIAN_POINT('Ctrl Pts',(52.9091758730547,19.7194375302414,13.627744380637));
#39226=CARTESIAN_POINT('Ctrl Pts',(52.8695374951604,19.789182191462,13.6235866972181));
#39227=CARTESIAN_POINT('Ctrl Pts',(52.8299232378496,19.8588844119469,13.6194315438156));
#39228=CARTESIAN_POINT('Ctrl Pts',(52.7937037573007,19.9305850612507,13.6152763904132));
#39229=CARTESIAN_POINT('Ctrl Pts',(52.7610806557317,20.0039124436771,13.6111212370107));
#39230=CARTESIAN_POINT('Ctrl Pts',(52.7284667201144,20.0772192236713,13.6069672510612));
#39231=CARTESIAN_POINT('Ctrl Pts',(52.6994473506741,20.15215139047,13.6028132651117));
#39232=CARTESIAN_POINT('Ctrl Pts',(52.6741769814409,20.2283151314556,13.5986592791622));
#39233=CARTESIAN_POINT('Ctrl Pts',(52.6488948802354,20.3045142320704,13.5945033646912));
#39234=CARTESIAN_POINT('Ctrl Pts',(52.627365408381,20.3819455933885,13.5903474502203));
#39235=CARTESIAN_POINT('Ctrl Pts',(52.6096934889834,20.4601990798528,13.5861915357494));
#39236=CARTESIAN_POINT('Ctrl Pts',(52.5920165263288,20.5384748984951,13.5820344352531));
#39237=CARTESIAN_POINT('Ctrl Pts',(52.5781993940604,20.6175728371252,13.5778773347568));
#39238=CARTESIAN_POINT('Ctrl Pts',(52.5682956870323,20.6970736322232,13.5737202342605));
#39239=CARTESIAN_POINT('Ctrl Pts',(52.558381081092,20.776661917005,13.5695585589243));
#39240=CARTESIAN_POINT('Ctrl Pts',(52.55238852971,20.8566534647325,13.5653968835882));
#39241=CARTESIAN_POINT('Ctrl Pts',(52.5503196152149,20.9366260116536,13.561235208252));
#39242=CARTESIAN_POINT('Ctrl Pts',(52.5497549175711,20.9584540325404,13.5600993042492));
#39243=CARTESIAN_POINT('Ctrl Pts',(52.5494822250542,20.9802806517921,13.5589634002464));
#39244=CARTESIAN_POINT('Ctrl Pts',(52.5495008975342,21.0020973350977,13.5578274962436));
#39245=CARTESIAN_POINT('',(52.5495004842277,20.9984594806585,12.7578274961836));
#39246=CARTESIAN_POINT('Ctrl Pts',(52.5495008975348,21.0020973357021,13.5578274962121));
#39247=CARTESIAN_POINT('Ctrl Pts',(52.5496050215771,21.1237544800426,13.5514933144627));
#39248=CARTESIAN_POINT('Ctrl Pts',(52.5587720373766,21.2450363613145,13.5451591327133));
#39249=CARTESIAN_POINT('Ctrl Pts',(52.5768166350929,21.3648734438646,13.5388249509639));
#39250=CARTESIAN_POINT('Ctrl Pts',(52.5809513237883,21.3923325780772,13.5373735542586));
#39251=CARTESIAN_POINT('Ctrl Pts',(52.5855519468644,21.419715988469,13.5359221575533));
#39252=CARTESIAN_POINT('Ctrl Pts',(52.5906159685464,21.4470110054308,13.534470760848));
#39253=CARTESIAN_POINT('Ctrl Pts',(52.6053789835698,21.5265834817712,13.5302395405431));
#39254=CARTESIAN_POINT('Ctrl Pts',(52.6241158628056,21.6055730169194,13.5260083202382));
#39255=CARTESIAN_POINT('Ctrl Pts',(52.6467668473267,21.6835524699388,13.5217770999333));
#39256=CARTESIAN_POINT('Ctrl Pts',(52.6693853519214,21.7614201058803,13.5175519469021));
#39257=CARTESIAN_POINT('Ctrl Pts',(52.6959066862571,21.8382800935975,13.513326793871));
#39258=CARTESIAN_POINT('Ctrl Pts',(52.7262199305186,21.9137146412471,13.5091016408398));
#39259=CARTESIAN_POINT('Ctrl Pts',(52.7566110482845,21.9893429772131,13.5048656335606));
#39260=CARTESIAN_POINT('Ctrl Pts',(52.7908134910257,22.0635380770193,13.5006296262814));
#39261=CARTESIAN_POINT('Ctrl Pts',(52.8286648448361,22.1358934342399,13.4963936190022));
#39262=CARTESIAN_POINT('Ctrl Pts',(52.8663512892215,22.2079335562271,13.4921760670081));
#39263=CARTESIAN_POINT('Ctrl Pts',(52.9076547064636,22.2781495144851,13.4879585150139));
#39264=CARTESIAN_POINT('Ctrl Pts',(52.9523670404461,22.3461610278672,13.4837409630198));
#39265=CARTESIAN_POINT('Ctrl Pts',(52.9970646114331,22.4141500853948,13.4795248035654));
#39266=CARTESIAN_POINT('Ctrl Pts',(53.0451686087826,22.4799357552867,13.475308644111));
#39267=CARTESIAN_POINT('Ctrl Pts',(53.0964266956879,22.5431652293616,13.4710924846565));
#39268=CARTESIAN_POINT('Ctrl Pts',(53.147683561217,22.6063931968062,13.4668764256646));
#39269=CARTESIAN_POINT('Ctrl Pts',(53.2020940732346,22.6670647290788,13.4626603666728));
#39270=CARTESIAN_POINT('Ctrl Pts',(53.2593654158795,22.7248598478032,13.4584443076809));
#39271=CARTESIAN_POINT('Ctrl Pts',(53.3171055610562,22.7831280565013,13.4541937375524));
#39272=CARTESIAN_POINT('Ctrl Pts',(53.377753262231,22.838472191678,13.4499431674239));
#39273=CARTESIAN_POINT('Ctrl Pts',(53.4409716986284,22.8906033443116,13.4456925972954));
#39274=CARTESIAN_POINT('Ctrl Pts',(53.503768020127,22.9423864127871,13.4414704085866));
#39275=CARTESIAN_POINT('Ctrl Pts',(53.5691004377833,22.9909990440902,13.4372482198779));
#39276=CARTESIAN_POINT('Ctrl Pts',(53.6366082941618,23.0362007038727,13.4330260311692));
#39277=CARTESIAN_POINT('Ctrl Pts',(53.7047968290724,23.081858129859,13.4287612703308));
#39278=CARTESIAN_POINT('Ctrl Pts',(53.7752045025753,23.124035162188,13.4244965094924));
#39279=CARTESIAN_POINT('Ctrl Pts',(53.8474343961711,23.1625315671385,13.420231748654));
#39280=CARTESIAN_POINT('Ctrl Pts',(53.9196642897669,23.201027972089,13.4159669878157));
#39281=CARTESIAN_POINT('Ctrl Pts',(53.9937159401067,23.2358436028115,13.4117022269773));
#39282=CARTESIAN_POINT('Ctrl Pts',(54.0691738226618,23.2668288152355,13.4074374661389));
#39283=CARTESIAN_POINT('Ctrl Pts',(54.1440382610055,23.2975703421182,13.403206245834));
#39284=CARTESIAN_POINT('Ctrl Pts',(54.2205676074931,23.324656804284,13.398975025529));
#39285=CARTESIAN_POINT('Ctrl Pts',(54.2983705606061,23.347906808154,13.3947438052241));
#39286=CARTESIAN_POINT('Ctrl Pts',(54.3760619497298,23.3711234731457,13.390518652193));
#39287=CARTESIAN_POINT('Ctrl Pts',(54.455022876685,23.3905144736688,13.3862934991618));
#39288=CARTESIAN_POINT('Ctrl Pts',(54.5348421548412,23.4059464726147,13.3820683461306));
#39289=CARTESIAN_POINT('Ctrl Pts',(54.6148664855094,23.4214181157446,13.3778323388514));
#39290=CARTESIAN_POINT('Ctrl Pts',(54.6957531440898,23.4329102168745,13.3735963315722));
#39291=CARTESIAN_POINT('Ctrl Pts',(54.7770725051384,23.4403388252525,13.369360324293));
#39292=CARTESIAN_POINT('Ctrl Pts',(54.8580375769028,23.4477350689351,13.3651427722989));
#39293=CARTESIAN_POINT('Ctrl Pts',(54.9394311234451,23.4511031026776,13.3609252203047));
#39294=CARTESIAN_POINT('Ctrl Pts',(55.0208208065253,23.4504115458461,13.3567076683106));
#39295=CARTESIAN_POINT('Ctrl Pts',(55.1021836165837,23.4497202173509,13.3524915088561));
#39296=CARTESIAN_POINT('Ctrl Pts',(55.1835421011733,23.4449719640442,13.3482753494017));
#39297=CARTESIAN_POINT('Ctrl Pts',(55.264462995854,23.4361875079361,13.3440591899472));
#39298=CARTESIAN_POINT('Ctrl Pts',(55.3453819623538,23.4274032611438,13.3398431309553));
#39299=CARTESIAN_POINT('Ctrl Pts',(55.4258628975894,23.4145830540475,13.3356270719634));
#39300=CARTESIAN_POINT('Ctrl Pts',(55.5054781732568,23.3977994216283,13.3314110129715));
#39301=CARTESIAN_POINT('Ctrl Pts',(55.585745150823,23.3808784044544,13.3271604428431));
#39302=CARTESIAN_POINT('Ctrl Pts',(55.6651317587422,23.3599288593701,13.3229098727146));
#39303=CARTESIAN_POINT('Ctrl Pts',(55.7432126138556,23.3350771423244,13.3186593025861));
#39304=CARTESIAN_POINT('Ctrl Pts',(55.8207721164321,23.3103913623155,13.3144371138774));
#39305=CARTESIAN_POINT('Ctrl Pts',(55.8970428322707,23.2818555843418,13.3102149251686));
#39306=CARTESIAN_POINT('Ctrl Pts',(55.9716270995667,23.2496424225614,13.3059927364599));
#39307=CARTESIAN_POINT('Ctrl Pts',(56.0469633965112,23.2171044569904,13.3017279756216));
#39308=CARTESIAN_POINT('Ctrl Pts',(56.120578609002,23.1808147472378,13.2974632147832));
#39309=CARTESIAN_POINT('Ctrl Pts',(56.1920892757065,23.1409982271701,13.2931984539449));
#39310=CARTESIAN_POINT('Ctrl Pts',(56.2635999424109,23.1011817071024,13.2889336931066));
#39311=CARTESIAN_POINT('Ctrl Pts',(56.3330056887029,23.0578386864169,13.2846689322683));
#39312=CARTESIAN_POINT('Ctrl Pts',(56.399955471868,23.0112371632373,13.28040417143));
#39313=CARTESIAN_POINT('Ctrl Pts',(56.4663787234119,22.9650021412529,13.276172951125));
#39314=CARTESIAN_POINT('Ctrl Pts',(56.530633609848,22.9153863486505,13.2719417308201));
#39315=CARTESIAN_POINT('Ctrl Pts',(56.5923555456466,22.8626202152475,13.2677105105152));
#39316=CARTESIAN_POINT('Ctrl Pts',(56.6539889765092,22.8099297447866,13.263485357484));
#39317=CARTESIAN_POINT('Ctrl Pts',(56.7130963199011,22.7540982049184,13.2592602044529));
#39318=CARTESIAN_POINT('Ctrl Pts',(56.769342586897,22.6953987909022,13.2550350514217));
#39319=CARTESIAN_POINT('Ctrl Pts',(56.8257333482884,22.6365485804545,13.2507990441425));
#39320=CARTESIAN_POINT('Ctrl Pts',(56.8792479307538,22.5748160170196,13.2465630368633));
#39321=CARTESIAN_POINT('Ctrl Pts',(56.9295828436043,22.510516567161,13.2423270295841));
#39322=CARTESIAN_POINT('Ctrl Pts',(56.9796984591065,22.4464972548463,13.23810947759));
#39323=CARTESIAN_POINT('Ctrl Pts',(57.0266617585143,22.3799337394739,13.2338919255958));
#39324=CARTESIAN_POINT('Ctrl Pts',(57.0702119514747,22.3111722716605,13.2296743736017));
#39325=CARTESIAN_POINT('Ctrl Pts',(57.1137477651521,22.2424335073195,13.2254582141473));
#39326=CARTESIAN_POINT('Ctrl Pts',(57.1538724617397,22.1714986241666,13.2212420546928));
#39327=CARTESIAN_POINT('Ctrl Pts',(57.190368527163,22.0987429022359,13.2170258952384));
#39328=CARTESIAN_POINT('Ctrl Pts',(57.2268637229589,22.0259889139267,13.2128098362465));
#39329=CARTESIAN_POINT('Ctrl Pts',(57.2597302520328,21.9514145891694,13.2085937772546));
#39330=CARTESIAN_POINT('Ctrl Pts',(57.2887971914368,21.8754185664417,13.2043777182627));
#39331=CARTESIAN_POINT('Ctrl Pts',(57.3181020623113,21.7988004677125,13.2001271481342));
#39332=CARTESIAN_POINT('Ctrl Pts',(57.3435446658933,21.7207377308969,13.1958765780058));
#39333=CARTESIAN_POINT('Ctrl Pts',(57.3650005188826,21.6416562909259,13.1916260078773));
#39334=CARTESIAN_POINT('Ctrl Pts',(57.3863131093094,21.5631028844827,13.1874038191685));
#39335=CARTESIAN_POINT('Ctrl Pts',(57.4036919869534,21.483544809274,13.1831816304598));
#39336=CARTESIAN_POINT('Ctrl Pts',(57.4170665674218,21.40340978998,13.178959441751));
#39337=CARTESIAN_POINT('Ctrl Pts',(57.4305760031542,21.3224667730666,13.1746946809127));
#39338=CARTESIAN_POINT('Ctrl Pts',(57.4399998811463,21.2409355945664,13.1704299200744));
#39339=CARTESIAN_POINT('Ctrl Pts',(57.4453192776807,21.1592604163091,13.166165159236));
#39340=CARTESIAN_POINT('Ctrl Pts',(57.4506386742152,21.0775852380518,13.1619003983977));
#39341=CARTESIAN_POINT('Ctrl Pts',(57.4518536463803,20.9957665427361,13.1576356375594));
#39342=CARTESIAN_POINT('Ctrl Pts',(57.4489990326534,20.9142446033025,13.153370876721));
#39343=CARTESIAN_POINT('Ctrl Pts',(57.4461668692516,20.8333637993128,13.1491396564161));
#39344=CARTESIAN_POINT('Ctrl Pts',(57.4393183278817,20.7524718047301,13.1449084361112));
#39345=CARTESIAN_POINT('Ctrl Pts',(57.4284493375912,20.6719999012911,13.1406772158063));
#39346=CARTESIAN_POINT('Ctrl Pts',(57.417595932672,20.5916433889294,13.1364520627751));
#39347=CARTESIAN_POINT('Ctrl Pts',(57.4027335903438,20.511706228188,13.132226909744));
#39348=CARTESIAN_POINT('Ctrl Pts',(57.3839102206162,20.4326180210462,13.1280017567128));
#39349=CARTESIAN_POINT('Ctrl Pts',(57.3650384944096,20.3533266394841,13.1237657494336));
#39350=CARTESIAN_POINT('Ctrl Pts',(57.3421853862492,20.2748890504587,13.1195297421544));
#39351=CARTESIAN_POINT('Ctrl Pts',(57.3154514030215,20.1977313104415,13.1152937348752));
#39352=CARTESIAN_POINT('Ctrl Pts',(57.2888338934559,20.120909728507,13.1110761828811));
#39353=CARTESIAN_POINT('Ctrl Pts',(57.2583693998657,20.0453573116013,13.1068586308869));
#39354=CARTESIAN_POINT('Ctrl Pts',(57.2242074480419,19.9714809296493,13.1026410788927));
#39355=CARTESIAN_POINT('Ctrl Pts',(57.1900567757174,19.897628939998,13.0984249194383));
#39356=CARTESIAN_POINT('Ctrl Pts',(57.1522112645126,19.8254523080053,13.0942087599839));
#39357=CARTESIAN_POINT('Ctrl Pts',(57.1108682971053,19.7553372817201,13.0899926005295));
#39358=CARTESIAN_POINT('Ctrl Pts',(57.0695263148171,19.6852239261339,13.0857765415376));
#39359=CARTESIAN_POINT('Ctrl Pts',(57.0246872791213,19.6171724785061,13.0815604825457));
#39360=CARTESIAN_POINT('Ctrl Pts',(56.9765934620127,19.5515427048309,13.0773444235538));
#39361=CARTESIAN_POINT('Ctrl Pts',(56.9281059662828,19.4853757095258,13.0730938534253));
#39362=CARTESIAN_POINT('Ctrl Pts',(56.8763104288674,19.421670613497,13.0688432832968));
#39363=CARTESIAN_POINT('Ctrl Pts',(56.8214972377978,19.3607629632372,13.0645927131683));
#39364=CARTESIAN_POINT('Ctrl Pts',(56.7670500390859,19.3002619985594,13.0603705244596));
#39365=CARTESIAN_POINT('Ctrl Pts',(56.7096257371693,19.2425215251593,13.0561483357508));
#39366=CARTESIAN_POINT('Ctrl Pts',(56.6495454490545,19.1878327722024,13.0519261470421));
#39367=CARTESIAN_POINT('Ctrl Pts',(56.5888593742285,19.132592595129,13.0476613862037));
#39368=CARTESIAN_POINT('Ctrl Pts',(56.5254638266102,19.0804663341252,13.0433966253654));
#39369=CARTESIAN_POINT('Ctrl Pts',(56.4597217458266,19.0317107238109,13.0391318645271));
#39370=CARTESIAN_POINT('Ctrl Pts',(56.393979665043,18.9829551134966,13.0348671036887));
#39371=CARTESIAN_POINT('Ctrl Pts',(56.3258914876291,18.937570367634,13.0306023428504));
#39372=CARTESIAN_POINT('Ctrl Pts',(56.255846036666,18.8957659393047,13.026337582012));
#39373=CARTESIAN_POINT('Ctrl Pts',(56.1863514634373,18.8542902850563,13.0221063617071));
#39374=CARTESIAN_POINT('Ctrl Pts',(56.1146697196367,18.8161832658581,13.0178751414022));
#39375=CARTESIAN_POINT('Ctrl Pts',(56.041160976075,18.7816821526439,13.0136439210972));
#39376=CARTESIAN_POINT('Ctrl Pts',(55.9677576389066,18.7472305116113,13.0094187680661));
#39377=CARTESIAN_POINT('Ctrl Pts',(55.8925329223964,18.7163747031977,13.0051936150349));
#39378=CARTESIAN_POINT('Ctrl Pts',(55.8158737711765,18.6893074112928,13.0009684620038));
#39379=CARTESIAN_POINT('Ctrl Pts',(55.7390176856833,18.6621705846047,12.9967324547246));
#39380=CARTESIAN_POINT('Ctrl Pts',(55.6607201946426,18.6388420008193,12.9924964474454));
#39381=CARTESIAN_POINT('Ctrl Pts',(55.5813937828006,18.6194682276179,12.9882604401662));
#39382=CARTESIAN_POINT('Ctrl Pts',(55.5024129774331,18.6001788613788,12.984042888172));
#39383=CARTESIAN_POINT('Ctrl Pts',(55.4224126506704,18.5848100361842,12.9798253361779));
#39384=CARTESIAN_POINT('Ctrl Pts',(55.341815745164,18.5734567289335,12.9756077841837));
#39385=CARTESIAN_POINT('Ctrl Pts',(55.2612454509223,18.5621071702866,12.9713916247293));
#39386=CARTESIAN_POINT('Ctrl Pts',(55.1800794291201,18.5547705614661,12.9671754652748));
#39387=CARTESIAN_POINT('Ctrl Pts',(55.0987492442285,18.5514904866911,12.9629593058204));
#39388=CARTESIAN_POINT('Ctrl Pts',(55.0174209972704,18.5482104900736,12.9587432468285));
#39389=CARTESIAN_POINT('Ctrl Pts',(54.9359290595891,18.548986852946,12.9545271878366));
#39390=CARTESIAN_POINT('Ctrl Pts',(54.8547070844642,18.5538110827871,12.9503111288447));
#39391=CARTESIAN_POINT('Ctrl Pts',(54.7728202555785,18.5586748020318,12.9460605587162));
#39392=CARTESIAN_POINT('Ctrl Pts',(54.6912083091062,18.5676529504591,12.9418099885878));
#39393=CARTESIAN_POINT('Ctrl Pts',(54.6103106378111,18.5806834744092,12.9375594184593));
#39394=CARTESIAN_POINT('Ctrl Pts',(54.5299531271754,18.5936269924381,12.9333372297505));
#39395=CARTESIAN_POINT('Ctrl Pts',(54.4503008285854,18.6105687765357,12.9291150410418));
#39396=CARTESIAN_POINT('Ctrl Pts',(54.3717725597401,18.6313969236479,12.924892852333));
#39397=CARTESIAN_POINT('Ctrl Pts',(54.2924524940645,18.6524350799849,12.9206280914947));
#39398=CARTESIAN_POINT('Ctrl Pts',(54.2142797154996,18.6774382644917,12.9163633306564));
#39399=CARTESIAN_POINT('Ctrl Pts',(54.1376667353455,18.7062407295729,12.912098569818));
#39400=CARTESIAN_POINT('Ctrl Pts',(54.0610537551914,18.7350431946541,12.9078338089797));
#39401=CARTESIAN_POINT('Ctrl Pts',(53.9860009897574,18.7676446894243,12.9035690481414));
#39402=CARTESIAN_POINT('Ctrl Pts',(53.9128952572967,18.803832081012,12.899304287303));
#39403=CARTESIAN_POINT('Ctrl Pts',(53.840364470385,18.8397348741281,12.8950730669981));
#39404=CARTESIAN_POINT('Ctrl Pts',(53.7694781981508,18.8793019528073,12.8908418466932));
#39405=CARTESIAN_POINT('Ctrl Pts',(53.700631096504,18.922359342276,12.8866106263883));
#39406=CARTESIAN_POINT('Ctrl Pts',(53.6318827167823,18.9653549904619,12.8823854733571));
#39407=CARTESIAN_POINT('Ctrl Pts',(53.5651680911645,19.0118307649638,12.878160320326));
#39408=CARTESIAN_POINT('Ctrl Pts',(53.5008589292994,19.0615660186278,12.8739351672948));
#39409=CARTESIAN_POINT('Ctrl Pts',(53.4363845597864,19.1114290401561,12.8696991600156));
#39410=CARTESIAN_POINT('Ctrl Pts',(53.3743284490996,19.1645680940725,12.8654631527364));
#39411=CARTESIAN_POINT('Ctrl Pts',(53.315037406826,19.2207160683004,12.8612271454572));
#39412=CARTESIAN_POINT('Ctrl Pts',(53.2560046816452,19.276619419042,12.857009593463));
#39413=CARTESIAN_POINT('Ctrl Pts',(53.1997133269616,19.3355052106891,12.8527920414689));
#39414=CARTESIAN_POINT('Ctrl Pts',(53.146472474467,19.3970695704144,12.8485744894747));
#39415=CARTESIAN_POINT('Ctrl Pts',(53.0932492008907,19.4586136029886,12.8443583300203));
#39416=CARTESIAN_POINT('Ctrl Pts',(53.0430747332105,19.5228340959575,12.8401421705659));
#39417=CARTESIAN_POINT('Ctrl Pts',(52.9962196961089,19.5893920659027,12.8359260111114));
#39418=CARTESIAN_POINT('Ctrl Pts',(52.9493657754679,19.6559484499065,12.8317099521195));
#39419=CARTESIAN_POINT('Ctrl Pts',(52.9058313948651,19.7248418193401,12.8274938931276));
#39420=CARTESIAN_POINT('Ctrl Pts',(52.8658445548617,19.7957031985484,12.8232778341357));
#39421=CARTESIAN_POINT('Ctrl Pts',(52.8255303970245,19.8671446234203,12.8190272640073));
#39422=CARTESIAN_POINT('Ctrl Pts',(52.7888223753672,19.940586015715,12.8147766938788));
#39423=CARTESIAN_POINT('Ctrl Pts',(52.7559065985614,20.015624535241,12.8105261237503));
#39424=CARTESIAN_POINT('Ctrl Pts',(52.723210603208,20.0901620161643,12.8063039350416));
#39425=CARTESIAN_POINT('Ctrl Pts',(52.6942564738011,20.1662749001549,12.8020817463328));
#39426=CARTESIAN_POINT('Ctrl Pts',(52.6691772775385,20.2435506054883,12.7978595576241));
#39427=CARTESIAN_POINT('Ctrl Pts',(52.643845208923,20.3216054781133,12.7935947967857));
#39428=CARTESIAN_POINT('Ctrl Pts',(52.6224667813494,20.4008462843846,12.7893300359474));
#39429=CARTESIAN_POINT('Ctrl Pts',(52.6051264004603,20.4808365457511,12.7850652751091));
#39430=CARTESIAN_POINT('Ctrl Pts',(52.5877860195712,20.5608268071176,12.7808005142707));
#39431=CARTESIAN_POINT('Ctrl Pts',(52.5744837002957,20.6415660377458,12.7765357534324));
#39432=CARTESIAN_POINT('Ctrl Pts',(52.5652501021603,20.7226136539601,12.7722709925941));
#39433=CARTESIAN_POINT('Ctrl Pts',(52.5548262709602,20.8141085033343,12.7674564938001));
#39434=CARTESIAN_POINT('Ctrl Pts',(52.5495584825478,20.9062017589285,12.7626419950061));
#39435=CARTESIAN_POINT('Ctrl Pts',(52.5495004842281,20.998459480112,12.7578274962121));
#39436=CARTESIAN_POINT('',(52.5495002652713,20.9988597830668,11.957827496262));
#39437=CARTESIAN_POINT('Ctrl Pts',(52.5495004842277,20.9984594806585,12.7578274961836));
#39438=CARTESIAN_POINT('Ctrl Pts',(52.5494502298631,21.0783989483802,12.7536558294006));
#39439=CARTESIAN_POINT('Ctrl Pts',(52.5533158347715,21.1584933142817,12.7494841626176));
#39440=CARTESIAN_POINT('Ctrl Pts',(52.5611163582093,21.2383208589397,12.7453124958346));
#39441=CARTESIAN_POINT('Ctrl Pts',(52.5689133596593,21.3181123609344,12.7411427125867));
#39442=CARTESIAN_POINT('Ctrl Pts',(52.5806417568019,21.3976368040027,12.7369729293388));
#39443=CARTESIAN_POINT('Ctrl Pts',(52.5962684716246,21.4764713942033,12.7328031460909));
#39444=CARTESIAN_POINT('Ctrl Pts',(52.611868507349,21.5551713920849,12.7286404818094));
#39445=CARTESIAN_POINT('Ctrl Pts',(52.6313535083502,21.6331834148886,12.7244778175279));
#39446=CARTESIAN_POINT('Ctrl Pts',(52.6546388108824,21.7100923479246,12.7203151532463));
#39447=CARTESIAN_POINT('Ctrl Pts',(52.6779137748999,21.7869671339215,12.7161543371592));
#39448=CARTESIAN_POINT('Ctrl Pts',(52.7049855542601,21.8627393445095,12.7119935210721));
#39449=CARTESIAN_POINT('Ctrl Pts',(52.7357190674315,21.9370069948547,12.707832704985));
#39450=CARTESIAN_POINT('Ctrl Pts',(52.7664489467307,22.011265863934,12.7036723808649));
#39451=CARTESIAN_POINT('Ctrl Pts',(52.800839516234,22.0840200842678,12.6995120567448));
#39452=CARTESIAN_POINT('Ctrl Pts',(52.8387073866657,22.1548872194057,12.6953517326246));
#39453=CARTESIAN_POINT('Ctrl Pts',(52.8767194845923,22.2260242664573,12.691175563063));
#39454=CARTESIAN_POINT('Ctrl Pts',(52.9182352066916,22.2952593910474,12.6869993935014));
#39455=CARTESIAN_POINT('Ctrl Pts',(52.9630232435531,22.3622319713232,12.6828232239397));
#39456=CARTESIAN_POINT('Ctrl Pts',(53.0076998559111,22.4290379359796,12.6786574439297));
#39457=CARTESIAN_POINT('Ctrl Pts',(53.0556322019289,22.4935922376309,12.6744916639197));
#39458=CARTESIAN_POINT('Ctrl Pts',(53.1065492809538,22.555568907038,12.6703258839096));
#39459=CARTESIAN_POINT('Ctrl Pts',(53.1576568425362,22.6177774333135,12.6661445195722));
#39460=CARTESIAN_POINT('Ctrl Pts',(53.2117711769549,22.6773886538559,12.6619631552348));
#39461=CARTESIAN_POINT('Ctrl Pts',(53.2685813071997,22.7341105963063,12.6577817908973));
#39462=CARTESIAN_POINT('Ctrl Pts',(53.3253914374445,22.7908325387567,12.6536004265599));
#39463=CARTESIAN_POINT('Ctrl Pts',(53.3848969618111,22.8446649320933,12.6494190622225));
#39464=CARTESIAN_POINT('Ctrl Pts',(53.4467556182776,22.8953580507777,12.645237697885));
#39465=CARTESIAN_POINT('Ctrl Pts',(53.5093518385911,22.9466556024351,12.6410064775801));
#39466=CARTESIAN_POINT('Ctrl Pts',(53.5746093865146,22.9949450396391,12.6367752572752));
#39467=CARTESIAN_POINT('Ctrl Pts',(53.642207143667,23.0399384327207,12.6325440369703));
#39468=CARTESIAN_POINT('Ctrl Pts',(53.7097079703668,23.0848673084257,12.6283188839391));
#39469=CARTESIAN_POINT('Ctrl Pts',(53.7795419578684,23.1265092713537,12.624093730908));
#39470=CARTESIAN_POINT('Ctrl Pts',(53.8513549141328,23.1646165287905,12.6198685778768));
#39471=CARTESIAN_POINT('Ctrl Pts',(53.9233523549909,23.2028216822377,12.6156325705976));
#39472=CARTESIAN_POINT('Ctrl Pts',(53.9973385762571,23.2374736516977,12.6113965633184));
#39473=CARTESIAN_POINT('Ctrl Pts',(54.072927306216,23.2683664762203,12.6071605560392));
#39474=CARTESIAN_POINT('Ctrl Pts',(54.1481867138992,23.2991247079897,12.6029430040451));
#39475=CARTESIAN_POINT('Ctrl Pts',(54.2250342658871,23.3261562973527,12.5987254520509));
#39476=CARTESIAN_POINT('Ctrl Pts',(54.303065717464,23.3493047600995,12.5945079000568));
#39477=CARTESIAN_POINT('Ctrl Pts',(54.3810714048307,23.3724455797505,12.5902917406023));
#39478=CARTESIAN_POINT('Ctrl Pts',(54.460259770148,23.3917056867734,12.5860755811479));
#39479=CARTESIAN_POINT('Ctrl Pts',(54.5402104408931,23.4069781493267,12.5818594216935));
#39480=CARTESIAN_POINT('Ctrl Pts',(54.6201592065758,23.4222502479682,12.5776433627016));
#39481=CARTESIAN_POINT('Ctrl Pts',(54.7008697846985,23.4335348049145,12.5734273037097));
#39482=CARTESIAN_POINT('Ctrl Pts',(54.7819120349269,23.4407760834395,12.5692112447178));
#39483=CARTESIAN_POINT('Ctrl Pts',(54.8636176677529,23.4480766364558,12.5649606745893));
#39484=CARTESIAN_POINT('Ctrl Pts',(54.9456599512586,23.4512673532029,12.5607101044609));
#39485=CARTESIAN_POINT('Ctrl Pts',(55.0275951472322,23.4503446202217,12.5564595343324));
#39486=CARTESIAN_POINT('Ctrl Pts',(55.1089832549055,23.4494280484074,12.5522373456236));
#39487=CARTESIAN_POINT('Ctrl Pts',(55.1902652359041,23.4444528816744,12.5480151569149));
#39488=CARTESIAN_POINT('Ctrl Pts',(55.2710103282567,23.435467850738,12.5437929682061));
#39489=CARTESIAN_POINT('Ctrl Pts',(55.3525695695665,23.4263922241584,12.5395282073678));
#39490=CARTESIAN_POINT('Ctrl Pts',(55.4335805549402,23.4132254936289,12.5352634465295));
#39491=CARTESIAN_POINT('Ctrl Pts',(55.5136107960271,23.3960705749632,12.5309986856912));
#39492=CARTESIAN_POINT('Ctrl Pts',(55.593641037114,23.3789156562974,12.5267339248528));
#39493=CARTESIAN_POINT('Ctrl Pts',(55.6726900850779,23.3577727360512,12.5224691640145));
#39494=CARTESIAN_POINT('Ctrl Pts',(55.7503438539423,23.332795394125,12.5182044031762));
#39495=CARTESIAN_POINT('Ctrl Pts',(55.8273869088823,23.3080144883891,12.5139731828712));
#39496=CARTESIAN_POINT('Ctrl Pts',(55.9033454696026,23.2793663757153,12.5097419625663));
#39497=CARTESIAN_POINT('Ctrl Pts',(55.9778034900124,23.2469647493718,12.5055107422614));
#39498=CARTESIAN_POINT('Ctrl Pts',(56.0521547428323,23.2146095846927,12.5012855892302));
#39499=CARTESIAN_POINT('Ctrl Pts',(56.12500930601,23.1785117798965,12.497060436199));
#39500=CARTESIAN_POINT('Ctrl Pts',(56.1959669246842,23.1388345810421,12.4928352831679));
#39501=CARTESIAN_POINT('Ctrl Pts',(56.267106830624,23.0990554530612,12.4885992758887));
#39502=CARTESIAN_POINT('Ctrl Pts',(56.3363395858625,23.0556786674869,12.4843632686095));
#39503=CARTESIAN_POINT('Ctrl Pts',(56.4032826897653,23.0089171069521,12.4801272613303));
#39504=CARTESIAN_POINT('Ctrl Pts',(56.4699341383468,22.9623592755122,12.4759097093361));
#39505=CARTESIAN_POINT('Ctrl Pts',(56.5343154566839,22.9124463621612,12.471692157342));
#39506=CARTESIAN_POINT('Ctrl Pts',(56.5960759708961,22.859433178452,12.4674746053478));
#39507=CARTESIAN_POINT('Ctrl Pts',(56.6578160931914,22.8064374984901,12.4632584458934));
#39508=CARTESIAN_POINT('Ctrl Pts',(56.7169367772811,22.7503438835511,12.4590422864389));
#39509=CARTESIAN_POINT('Ctrl Pts',(56.7731202400878,22.6914475647181,12.4548261269845));
#39510=CARTESIAN_POINT('Ctrl Pts',(56.8293023641565,22.6325526492651,12.4506100679926));
#39511=CARTESIAN_POINT('Ctrl Pts',(56.8825470859884,22.5708554998705,12.4463940090007));
#39512=CARTESIAN_POINT('Ctrl Pts',(56.9325743421322,22.5066873139879,12.4421779500088));
#39513=CARTESIAN_POINT('Ctrl Pts',(56.9830111033311,22.4419938705055,12.4379273798803));
#39514=CARTESIAN_POINT('Ctrl Pts',(57.0301771740755,22.3747891182426,12.4336768097519));
#39515=CARTESIAN_POINT('Ctrl Pts',(57.073828913661,22.305443942444,12.4294262396234));
#39516=CARTESIAN_POINT('Ctrl Pts',(57.1171891868536,22.2365617903059,12.4252040509146));
#39517=CARTESIAN_POINT('Ctrl Pts',(57.1570817408366,22.1655681507613,12.4209818622059));
#39518=CARTESIAN_POINT('Ctrl Pts',(57.1933139523331,22.0928513881132,12.4167596734971));
#39519=CARTESIAN_POINT('Ctrl Pts',(57.229911491509,22.0194014257775,12.4124949126588));
#39520=CARTESIAN_POINT('Ctrl Pts',(57.2627742640968,21.9441938415729,12.4082301518205));
#39521=CARTESIAN_POINT('Ctrl Pts',(57.2917542389756,21.867647830711,12.4039653909821));
#39522=CARTESIAN_POINT('Ctrl Pts',(57.3207342138544,21.791101819849,12.3997006301438));
#39523=CARTESIAN_POINT('Ctrl Pts',(57.3458313044062,21.7132178606124,12.3954358693055));
#39524=CARTESIAN_POINT('Ctrl Pts',(57.3669500274368,21.6344271570612,12.3911711084671));
#39525=CARTESIAN_POINT('Ctrl Pts',(57.3879026606768,21.556256108943,12.3869398881622));
#39526=CARTESIAN_POINT('Ctrl Pts',(57.4050178934107,21.4768994071786,12.3827086678573));
#39527=CARTESIAN_POINT('Ctrl Pts',(57.4181656654684,21.3967682753822,12.3784774475523));
#39528=CARTESIAN_POINT('Ctrl Pts',(57.4312945845412,21.3167520460204,12.3742522945212));
#39529=CARTESIAN_POINT('Ctrl Pts',(57.4404672671976,21.2359640470366,12.37002714149));
#39530=CARTESIAN_POINT('Ctrl Pts',(57.4456038516245,21.154829102301,12.3658019884588));
#39531=CARTESIAN_POINT('Ctrl Pts',(57.45075363173,21.0734857251587,12.3615659811796));
#39532=CARTESIAN_POINT('Ctrl Pts',(57.4518464339143,20.9917940749852,12.3573299739004));
#39533=CARTESIAN_POINT('Ctrl Pts',(57.4488537294991,20.9101909719555,12.3530939666213));
#39534=CARTESIAN_POINT('Ctrl Pts',(57.4458740635915,20.8289433944071,12.3488764146271));
#39535=CARTESIAN_POINT('Ctrl Pts',(57.4388444249965,20.7477840619109,12.3446588626329));
#39536=CARTESIAN_POINT('Ctrl Pts',(57.4277887723585,20.6671457874534,12.3404413106388));
#39537=CARTESIAN_POINT('Ctrl Pts',(57.4167367700455,20.5865341379195,12.3362251511843));
#39538=CARTESIAN_POINT('Ctrl Pts',(57.4016614565903,20.5064436650254,12.3320089917299));
#39539=CARTESIAN_POINT('Ctrl Pts',(57.382638586668,20.4273014620932,12.3277928322755));
#39540=CARTESIAN_POINT('Ctrl Pts',(57.3636161700222,20.3481611449593,12.3235767732836));
#39541=CARTESIAN_POINT('Ctrl Pts',(57.3406464936627,20.2699695046497,12.3193607142917));
#39542=CARTESIAN_POINT('Ctrl Pts',(57.3138559848859,20.1931414428738,12.3151446552998));
#39543=CARTESIAN_POINT('Ctrl Pts',(57.2868461786778,20.1156844943254,12.3108940851713));
#39544=CARTESIAN_POINT('Ctrl Pts',(57.2559528422172,20.0396140091258,12.3066435150428));
#39545=CARTESIAN_POINT('Ctrl Pts',(57.2213554990952,19.9653358048915,12.3023929449144));
#39546=CARTESIAN_POINT('Ctrl Pts',(57.1869891653876,19.8915535625697,12.2981707562056));
#39547=CARTESIAN_POINT('Ctrl Pts',(57.1489684121945,19.8195401260059,12.2939485674968));
#39548=CARTESIAN_POINT('Ctrl Pts',(57.1075151123934,19.7496679236965,12.2897263787881));
#39549=CARTESIAN_POINT('Ctrl Pts',(57.065643840926,19.6790912032674,12.2854616179498));
#39550=CARTESIAN_POINT('Ctrl Pts',(57.0202706813945,19.6106995448714,12.2811968571114));
#39551=CARTESIAN_POINT('Ctrl Pts',(56.971667590737,19.54484462629,12.2769320962731));
#39552=CARTESIAN_POINT('Ctrl Pts',(56.9230645000795,19.4789897077085,12.2726673354348));
#39553=CARTESIAN_POINT('Ctrl Pts',(56.8712318331998,19.4156718610565,12.2684025745965));
#39554=CARTESIAN_POINT('Ctrl Pts',(56.8164801299285,19.3552051229485,12.2641378137581));
#39555=CARTESIAN_POINT('Ctrl Pts',(56.7621590255587,19.2952139300647,12.2599065934532));
#39556=CARTESIAN_POINT('Ctrl Pts',(56.7047609707054,19.2378041695224,12.2556753731483));
#39557=CARTESIAN_POINT('Ctrl Pts',(56.6445609685304,19.1833080969008,12.2514441528433));
#39558=CARTESIAN_POINT('Ctrl Pts',(56.5844472889451,19.128890167833,12.2472189998122));
#39559=CARTESIAN_POINT('Ctrl Pts',(56.5215399834475,19.0773779381981,12.242993846781));
#39560=CARTESIAN_POINT('Ctrl Pts',(56.4561527012609,19.0290688594954,12.2387686937499));
#39561=CARTESIAN_POINT('Ctrl Pts',(56.3905974417789,18.9806356767146,12.2345326864707));
#39562=CARTESIAN_POINT('Ctrl Pts',(56.322549768956,18.9354224690416,12.2302966791915));
#39563=CARTESIAN_POINT('Ctrl Pts',(56.252361245682,18.893690060719,12.2260606719123));
#39564=CARTESIAN_POINT('Ctrl Pts',(56.1824785172564,18.8521394706607,12.2218431199181));
#39565=CARTESIAN_POINT('Ctrl Pts',(56.1104739518147,18.8140396593022,12.2176255679239));
#39566=CARTESIAN_POINT('Ctrl Pts',(56.0367242050376,18.7796051763956,12.2134080159298));
#39567=CARTESIAN_POINT('Ctrl Pts',(55.9629988087491,18.7451820629719,12.2091918564754));
#39568=CARTESIAN_POINT('Ctrl Pts',(55.8875297963499,18.7144220712353,12.2049756970209));
#39569=CARTESIAN_POINT('Ctrl Pts',(55.8107171025951,18.687493128754,12.2007595375665));
#39570=CARTESIAN_POINT('Ctrl Pts',(55.7339062391314,18.6605648279349,12.1965434785746));
#39571=CARTESIAN_POINT('Ctrl Pts',(55.6557521970783,18.637467547638,12.1923274195827));
#39572=CARTESIAN_POINT('Ctrl Pts',(55.5766721431692,18.618320027944,12.1881113605908));
#39573=CARTESIAN_POINT('Ctrl Pts',(55.4969447684926,18.5990157735675,12.1838607904624));
#39574=CARTESIAN_POINT('Ctrl Pts',(55.4162766144555,18.5837263693793,12.1796102203339));
#39575=CARTESIAN_POINT('Ctrl Pts',(55.3351060049849,18.5725210164817,12.1753596502054));
#39576=CARTESIAN_POINT('Ctrl Pts',(55.2544773786052,18.5613904826822,12.1711374614967));
#39577=CARTESIAN_POINT('Ctrl Pts',(55.1733534593422,18.5542896065041,12.1669152727879));
#39578=CARTESIAN_POINT('Ctrl Pts',(55.092167479111,18.5512339013711,12.1626930840791));
#39579=CARTESIAN_POINT('Ctrl Pts',(55.0101629044709,18.5481473857074,12.1584283232408));
#39580=CARTESIAN_POINT('Ctrl Pts',(54.9280954960608,18.5491880686115,12.1541635624025));
#39581=CARTESIAN_POINT('Ctrl Pts',(54.8464082069827,18.5543181296175,12.1498988015641));
#39582=CARTESIAN_POINT('Ctrl Pts',(54.7647209179046,18.5594481906234,12.1456340407258));
#39583=CARTESIAN_POINT('Ctrl Pts',(54.6834142196497,18.5686675116084,12.1413692798875));
#39584=CARTESIAN_POINT('Ctrl Pts',(54.602920358367,18.5818854435324,12.1371045190491));
#39585=CARTESIAN_POINT('Ctrl Pts',(54.52305954713,18.5949994220334,12.1328732987442));
#39586=CARTESIAN_POINT('Ctrl Pts',(54.4436993569119,18.6120984721533,12.1286420784393));
#39587=CARTESIAN_POINT('Ctrl Pts',(54.3652680733224,18.6331316827385,12.1244108581344));
#39588=CARTESIAN_POINT('Ctrl Pts',(54.2869492547042,18.6541347331719,12.1201857051032));
#39589=CARTESIAN_POINT('Ctrl Pts',(54.2095571425543,18.6790606205957,12.1159605520721));
#39590=CARTESIAN_POINT('Ctrl Pts',(54.1335117336019,18.7078070905366,12.1117353990409));
#39591=CARTESIAN_POINT('Ctrl Pts',(54.0572709670552,18.7366274090015,12.1074993917617));
#39592=CARTESIAN_POINT('Ctrl Pts',(53.9823842965493,18.769287882134,12.1032633844825));
#39593=CARTESIAN_POINT('Ctrl Pts',(53.9092615009143,18.8056345389584,12.0990273772033));
#39594=CARTESIAN_POINT('Ctrl Pts',(53.8364572840606,18.8418228419681,12.0948098252092));
#39595=CARTESIAN_POINT('Ctrl Pts',(53.765402027165,18.8816650750567,12.090592273215));
#39596=CARTESIAN_POINT('Ctrl Pts',(53.6964802334532,18.9249610923595,12.0863747212209));
#39597=CARTESIAN_POINT('Ctrl Pts',(53.6275811961498,18.9682428143023,12.0821585617664));
#39598=CARTESIAN_POINT('Ctrl Pts',(53.5608146165273,19.014975808746,12.077942402312));
#39599=CARTESIAN_POINT('Ctrl Pts',(53.4965384466261,19.0649150903574,12.0737262428576));
#39600=CARTESIAN_POINT('Ctrl Pts',(53.4322638082958,19.1148531820169,12.0695101838657));
#39601=CARTESIAN_POINT('Ctrl Pts',(53.3704798281551,19.1679971228223,12.0652941248738));
#39602=CARTESIAN_POINT('Ctrl Pts',(53.3115124727321,19.2240607779936,12.0610780658819));
#39603=CARTESIAN_POINT('Ctrl Pts',(53.2520624318294,19.2805833500027,12.0568274957534));
#39604=CARTESIAN_POINT('Ctrl Pts',(53.1954756989531,19.3400733375517,12.0525769256249));
#39605=CARTESIAN_POINT('Ctrl Pts',(53.142048088122,19.4021999677216,12.0483263554964));
#39606=CARTESIAN_POINT('Ctrl Pts',(53.0889772180107,19.4639117730766,12.0441041667877));
#39607=CARTESIAN_POINT('Ctrl Pts',(53.0390236501508,19.5282247093893,12.0398819780789));
#39608=CARTESIAN_POINT('Ctrl Pts',(52.9924353272746,19.5947831715977,12.0356597893702));
#39609=CARTESIAN_POINT('Ctrl Pts',(52.9453772565365,19.6620127396408,12.0313950285319));
#39610=CARTESIAN_POINT('Ctrl Pts',(52.9017529341781,19.731532960029,12.0271302676935));
#39611=CARTESIAN_POINT('Ctrl Pts',(52.8617707609506,19.8029511408157,12.0228655068552));
#39612=CARTESIAN_POINT('Ctrl Pts',(52.8217885877232,19.8743693216024,12.0186007460168));
#39613=CARTESIAN_POINT('Ctrl Pts',(52.7854487200286,19.947685002575,12.0143359851785));
#39614=CARTESIAN_POINT('Ctrl Pts',(52.752909364638,20.0224858433412,12.0100712243402));
#39615=CARTESIAN_POINT('Ctrl Pts',(52.7173238434928,20.1042891510222,12.0054072187024));
#39616=CARTESIAN_POINT('Ctrl Pts',(52.6861685079812,20.1881309433786,12.0007432130646));
#39617=CARTESIAN_POINT('Ctrl Pts',(52.6596573132858,20.2735384671277,11.9960792074268));
#39618=CARTESIAN_POINT('Ctrl Pts',(52.6332226283103,20.3586995098786,11.99142866183));
#39619=CARTESIAN_POINT('Ctrl Pts',(52.6114054762756,20.4454169984112,11.9867781162331));
#39620=CARTESIAN_POINT('Ctrl Pts',(52.5943717616921,20.5331991548254,11.9821275706363));
#39621=CARTESIAN_POINT('Ctrl Pts',(52.5774219366889,20.620548991664,11.9774999285768));
#39622=CARTESIAN_POINT('Ctrl Pts',(52.5652086737941,20.708952755731,11.9728722865173));
#39623=CARTESIAN_POINT('Ctrl Pts',(52.5578475305062,20.7979070368733,11.9682446444578));
#39624=CARTESIAN_POINT('Ctrl Pts',(52.5523240465134,20.8646544874749,11.9647722617259));
#39625=CARTESIAN_POINT('Ctrl Pts',(52.5495315093585,20.9317114843349,11.961299878994));
#39626=CARTESIAN_POINT('Ctrl Pts',(52.5495002652713,20.9988597830668,11.957827496262));
#39627=CARTESIAN_POINT('',(52.5495009324152,21.0021377010802,11.1578274961736));
#39628=CARTESIAN_POINT('Ctrl Pts',(52.5495002652709,20.9988597840325,11.9578274962121));
#39629=CARTESIAN_POINT('Ctrl Pts',(52.5494617060243,21.0817295440113,11.9535421229565));
#39630=CARTESIAN_POINT('Ctrl Pts',(52.5536311635913,21.1645874816312,11.9492567497009));
#39631=CARTESIAN_POINT('Ctrl Pts',(52.5619786838129,21.2469864607974,11.9449713764453));
#39632=CARTESIAN_POINT('Ctrl Pts',(52.5703298476175,21.3294214060365,11.9406841326805));
#39633=CARTESIAN_POINT('Ctrl Pts',(52.5828626554615,21.4113965534959,11.9363968889157));
#39634=CARTESIAN_POINT('Ctrl Pts',(52.5994954785962,21.4924716161569,11.9321096451509));
#39635=CARTESIAN_POINT('Ctrl Pts',(52.61615360331,21.5736700088794,11.9278158797009));
#39636=CARTESIAN_POINT('Ctrl Pts',(52.6369241088679,21.6539651472636,11.9235221142509));
#39637=CARTESIAN_POINT('Ctrl Pts',(52.6616745845297,21.7329287150642,11.9192283488009));
#39638=CARTESIAN_POINT('Ctrl Pts',(52.6864445431347,21.8119544409714,11.9149312034083));
#39639=CARTESIAN_POINT('Ctrl Pts',(52.7152005586122,21.8896460925574,11.9106340580156));
#39640=CARTESIAN_POINT('Ctrl Pts',(52.7477617165096,21.9655946170004,11.906336912623));
#39641=CARTESIAN_POINT('Ctrl Pts',(52.7803906220155,22.0417011619573,11.9020308264757));
#39642=CARTESIAN_POINT('Ctrl Pts',(52.8168402938814,22.1160569342268,11.8977247403284));
#39643=CARTESIAN_POINT('Ctrl Pts',(52.856883369401,22.1882766334696,11.8934186541811));
#39644=CARTESIAN_POINT('Ctrl Pts',(52.8890607823993,22.2463102150313,11.8899584126644));
#39645=CARTESIAN_POINT('Ctrl Pts',(52.9235576151699,22.3029649191521,11.8864981711478));
#39646=CARTESIAN_POINT('Ctrl Pts',(52.9602364172642,22.3580555130572,11.8830379296311));
#39647=CARTESIAN_POINT('Ctrl Pts',(53.0050876484384,22.4254208800177,11.8788067093262));
#39648=CARTESIAN_POINT('Ctrl Pts',(53.0533637774511,22.4906882736688,11.8745754890213));
#39649=CARTESIAN_POINT('Ctrl Pts',(53.1048419648748,22.5534884202659,11.8703442687164));
#39650=CARTESIAN_POINT('Ctrl Pts',(53.1562463361806,22.6161985158481,11.8661191156852));
#39651=CARTESIAN_POINT('Ctrl Pts',(53.2108433545295,22.6764480343051,11.8618939626541));
#39652=CARTESIAN_POINT('Ctrl Pts',(53.2683668120242,22.7338964076037,11.8576688096229));
#39653=CARTESIAN_POINT('Ctrl Pts',(53.3260380449656,22.7914923634606,11.8534328023437));
#39654=CARTESIAN_POINT('Ctrl Pts',(53.3866505051754,22.8462723743405,11.8491967950645));
#39655=CARTESIAN_POINT('Ctrl Pts',(53.4498950709855,22.8979264893681,11.8449607877853));
#39656=CARTESIAN_POINT('Ctrl Pts',(53.5128640951328,22.9493555595943,11.8407432357912));
#39657=CARTESIAN_POINT('Ctrl Pts',(53.5784419805868,22.9976856124538,11.836525683797));
#39658=CARTESIAN_POINT('Ctrl Pts',(53.6462879449976,23.0426487515334,11.8323081318029));
#39659=CARTESIAN_POINT('Ctrl Pts',(53.7141115082144,23.0875970448075,11.8280919723484));
#39660=CARTESIAN_POINT('Ctrl Pts',(53.7842012760034,23.1291803753072,11.823875812894));
#39661=CARTESIAN_POINT('Ctrl Pts',(53.8561865476807,23.1671735131949,11.8196596534396));
#39662=CARTESIAN_POINT('Ctrl Pts',(53.9281701040951,23.2051657457832,11.8154435944477));
#39663=CARTESIAN_POINT('Ctrl Pts',(54.002048662911,23.2395677398193,11.8112275354558));
#39664=CARTESIAN_POINT('Ctrl Pts',(54.0774272063071,23.2702003634784,11.8070114764639));
#39665=CARTESIAN_POINT('Ctrl Pts',(54.1534227712417,23.3010837347341,11.8027609063354));
#39666=CARTESIAN_POINT('Ctrl Pts',(54.2309425523896,23.328135545893,11.798510336207));
#39667=CARTESIAN_POINT('Ctrl Pts',(54.309563280757,23.3512225302427,11.7942597660785));
#39668=CARTESIAN_POINT('Ctrl Pts',(54.3876590518073,23.3741553608265,11.7900375773697));
#39669=CARTESIAN_POINT('Ctrl Pts',(54.466840641655,23.3931761007768,11.785815388661));
#39670=CARTESIAN_POINT('Ctrl Pts',(54.5466818770947,23.4082053337383,11.7815931999523));
#39671=CARTESIAN_POINT('Ctrl Pts',(54.6273281479452,23.4233861057468,11.7773284391139));
#39672=CARTESIAN_POINT('Ctrl Pts',(54.7086469602838,23.4344943596096,11.7730636782756));
#39673=CARTESIAN_POINT('Ctrl Pts',(54.7901946387221,23.4415019886085,11.7687989174373));
#39674=CARTESIAN_POINT('Ctrl Pts',(54.8717423171605,23.4485096176073,11.7645341565989));
#39675=CARTESIAN_POINT('Ctrl Pts',(54.9535183779222,23.4514166688341,11.7602693957606));
#39676=CARTESIAN_POINT('Ctrl Pts',(55.0350819216579,23.4502488667017,11.7560046349223));
#39677=CARTESIAN_POINT('Ctrl Pts',(55.1160040027493,23.4490902488372,11.7517734146174));
#39678=CARTESIAN_POINT('Ctrl Pts',(55.1970203468551,23.4439163437233,11.7475421943124));
#39679=CARTESIAN_POINT('Ctrl Pts',(55.2776998487097,23.4347141606412,11.7433109740075));
#39680=CARTESIAN_POINT('Ctrl Pts',(55.3582636618055,23.4255251728455,11.7390858209764));
#39681=CARTESIAN_POINT('Ctrl Pts',(55.438491133911,23.4123194314266,11.7348606679452));
#39682=CARTESIAN_POINT('Ctrl Pts',(55.5179517639833,23.3951359502514,11.7306355149141));
#39683=CARTESIAN_POINT('Ctrl Pts',(55.5976165252156,23.3779083254048,11.7263995076349));
#39684=CARTESIAN_POINT('Ctrl Pts',(55.6765100275266,23.3566825105134,11.7221635003557));
#39685=CARTESIAN_POINT('Ctrl Pts',(55.7542042267086,23.3315501784038,11.7179274930765));
#39686=CARTESIAN_POINT('Ctrl Pts',(55.8315599305816,23.3065273419402,11.7137099410824));
#39687=CARTESIAN_POINT('Ctrl Pts',(55.9077263120162,23.2776320930379,11.7094923890882));
#39688=CARTESIAN_POINT('Ctrl Pts',(55.9822934953388,23.2450055097962,11.7052748370941));
#39689=CARTESIAN_POINT('Ctrl Pts',(56.0568360582737,23.21238969911,11.7010586776396));
#39690=CARTESIAN_POINT('Ctrl Pts',(56.1297800460681,23.1760451868864,11.6968425181852));
#39691=CARTESIAN_POINT('Ctrl Pts',(56.2007352106399,23.1361613244157,11.6926263587308));
#39692=CARTESIAN_POINT('Ctrl Pts',(56.2716886844939,23.0962784122967,11.6884102997389));
#39693=CARTESIAN_POINT('Ctrl Pts',(56.3406530246077,23.0528565463878,11.684194240747));
#39694=CARTESIAN_POINT('Ctrl Pts',(56.407263530797,23.0061305054479,11.6799781817551));
#39695=CARTESIAN_POINT('Ctrl Pts',(56.4744192865388,22.9590219820084,11.6757276116266));
#39696=CARTESIAN_POINT('Ctrl Pts',(56.5391820932744,22.9085552026386,11.6714770414982));
#39697=CARTESIAN_POINT('Ctrl Pts',(56.601210469907,22.8550135527969,11.6672264713697));
#39698=CARTESIAN_POINT('Ctrl Pts',(56.6628246777715,22.8018294051238,11.6630042826609));
#39699=CARTESIAN_POINT('Ctrl Pts',(56.7217405633723,22.7456116931203,11.6587820939522));
#39700=CARTESIAN_POINT('Ctrl Pts',(56.7776603178603,22.6866754413061,11.6545599052434));
#39701=CARTESIAN_POINT('Ctrl Pts',(56.8341439085955,22.6271449380442,11.6502951444051));
#39702=CARTESIAN_POINT('Ctrl Pts',(56.8875702922149,22.5648411333649,11.6460303835667));
#39703=CARTESIAN_POINT('Ctrl Pts',(56.9376752819753,22.5001215789469,11.6417656227283));
#39704=CARTESIAN_POINT('Ctrl Pts',(56.9877802717357,22.4354020245288,11.63750086189));
#39705=CARTESIAN_POINT('Ctrl Pts',(57.0345636448914,22.368267152392,11.6332361010516));
#39706=CARTESIAN_POINT('Ctrl Pts',(57.0778079507488,22.2991013701037,11.6289713402132));
#39707=CARTESIAN_POINT('Ctrl Pts',(57.1207121584999,22.2304795473288,11.6247401199082));
#39708=CARTESIAN_POINT('Ctrl Pts',(57.1602936913421,22.1596013450064,11.6205088996033));
#39709=CARTESIAN_POINT('Ctrl Pts',(57.1963078793248,22.0868219491782,11.6162776792983));
#39710=CARTESIAN_POINT('Ctrl Pts',(57.2322704254826,22.01414691391,11.6120525262671));
#39711=CARTESIAN_POINT('Ctrl Pts',(57.2646755817379,21.9395765127103,11.6078273732359));
#39712=CARTESIAN_POINT('Ctrl Pts',(57.2933227018554,21.8634936219536,11.6036022202047));
#39713=CARTESIAN_POINT('Ctrl Pts',(57.3220434152709,21.7872152773144,11.5993662129255));
#39714=CARTESIAN_POINT('Ctrl Pts',(57.3469865145598,21.7094170657506,11.5951302056463));
#39715=CARTESIAN_POINT('Ctrl Pts',(57.3679969315569,21.6305083521548,11.5908941983672));
#39716=CARTESIAN_POINT('Ctrl Pts',(57.3889158111208,21.5519434252198,11.586676646373));
#39717=CARTESIAN_POINT('Ctrl Pts',(57.4059360761835,21.4722781024795,11.5824590943788));
#39718=CARTESIAN_POINT('Ctrl Pts',(57.4189540220132,21.391933271599,11.5782415423846));
#39719=CARTESIAN_POINT('Ctrl Pts',(57.4319676696133,21.3116149687539,11.5740253829301));
#39720=CARTESIAN_POINT('Ctrl Pts',(57.4409815479425,21.2306180618886,11.5698092234756));
#39721=CARTESIAN_POINT('Ctrl Pts',(57.4459431556209,21.1493731216499,11.5655930640212));
#39722=CARTESIAN_POINT('Ctrl Pts',(57.4509046450741,21.0681301173136,11.5613770050292));
#39723=CARTESIAN_POINT('Ctrl Pts',(57.4518140286243,20.9866395554796,11.5571609460373));
#39724=CARTESIAN_POINT('Ctrl Pts',(57.4486708272855,20.9053351723125,11.5529448870454));
#39725=CARTESIAN_POINT('Ctrl Pts',(57.4455018968355,20.8233652608236,11.5486943169169));
#39726=CARTESIAN_POINT('Ctrl Pts',(57.4382137317604,20.7415850700323,11.5444437467885));
#39727=CARTESIAN_POINT('Ctrl Pts',(57.4268592840387,20.6604351822186,11.5401931766601));
#39728=CARTESIAN_POINT('Ctrl Pts',(57.4155806509339,20.579827139134,11.5359709879513));
#39729=CARTESIAN_POINT('Ctrl Pts',(57.4002900205224,20.4998414570351,11.5317487992425));
#39730=CARTESIAN_POINT('Ctrl Pts',(57.3810906090871,20.4208991786248,11.5275266105337));
#39731=CARTESIAN_POINT('Ctrl Pts',(57.3616976108925,20.3411609289476,11.5232618496955));
#39732=CARTESIAN_POINT('Ctrl Pts',(57.338316702293,20.2624877082379,11.5189970888572));
#39733=CARTESIAN_POINT('Ctrl Pts',(57.311105063035,20.18529536787,11.514732328019));
#39734=CARTESIAN_POINT('Ctrl Pts',(57.2838934237769,20.108103027502,11.5104675671807));
#39735=CARTESIAN_POINT('Ctrl Pts',(57.2528512960813,20.0323919888855,11.5062028063425));
#39736=CARTESIAN_POINT('Ctrl Pts',(57.2181837662685,19.9585533959617,11.5019380455042));
#39737=CARTESIAN_POINT('Ctrl Pts',(57.1837888818592,19.8852955122224,11.4977068251993));
#39738=CARTESIAN_POINT('Ctrl Pts',(57.14569648065,19.8136059992063,11.4934756048944));
#39739=CARTESIAN_POINT('Ctrl Pts',(57.1040723371263,19.7438830268881,11.4892443845895));
#39740=CARTESIAN_POINT('Ctrl Pts',(57.0625078797113,19.6742600324325,11.4850192315584));
#39741=CARTESIAN_POINT('Ctrl Pts',(57.0174219743112,19.6065983740059,11.4807940785273));
#39742=CARTESIAN_POINT('Ctrl Pts',(56.9690275324282,19.5412742456035,11.4765689254962));
#39743=CARTESIAN_POINT('Ctrl Pts',(56.9205087671717,19.4757823021442,11.472332918217));
#39744=CARTESIAN_POINT('Ctrl Pts',(56.8686646510941,19.4126403386582,11.4680969109378));
#39745=CARTESIAN_POINT('Ctrl Pts',(56.8137550657124,19.3522006154867,11.4638609036586));
#39746=CARTESIAN_POINT('Ctrl Pts',(56.7590847084494,19.2920242139405,11.4596433516645));
#39747=CARTESIAN_POINT('Ctrl Pts',(56.7013758457917,19.2345269075629,11.4554257996703));
#39748=CARTESIAN_POINT('Ctrl Pts',(56.6409258914727,19.1800240472208,11.4512082476762));
#39749=CARTESIAN_POINT('Ctrl Pts',(56.5804958963534,19.1255391824832,11.4469920882218));
#39750=CARTESIAN_POINT('Ctrl Pts',(56.5173269518917,19.0740471114464,11.4427759287674));
#39751=CARTESIAN_POINT('Ctrl Pts',(56.45175237138,19.0258254124337,11.438559769313));
#39752=CARTESIAN_POINT('Ctrl Pts',(56.3861793533778,18.9776048624465,11.4343437103211));
#39753=CARTESIAN_POINT('Ctrl Pts',(56.318201188503,18.9326548040867,11.4301276513293));
#39754=CARTESIAN_POINT('Ctrl Pts',(56.2481820575066,18.8912108210353,11.4259115923374));
#39755=CARTESIAN_POINT('Ctrl Pts',(56.1775897751851,18.8494275925025,11.4216610222089));
#39756=CARTESIAN_POINT('Ctrl Pts',(56.1049233639389,18.8112083613104,11.4174104520804));
#39757=CARTESIAN_POINT('Ctrl Pts',(56.0305817283029,18.776747528667,11.4131598819519));
#39758=CARTESIAN_POINT('Ctrl Pts',(55.9567364781175,18.7425167939465,11.4089376932431));
#39759=CARTESIAN_POINT('Ctrl Pts',(55.8812387650967,18.7119945389902,11.4047155045344));
#39760=CARTESIAN_POINT('Ctrl Pts',(55.8044983303346,18.6853223363741,11.4004933158257));
#39761=CARTESIAN_POINT('Ctrl Pts',(55.726984125387,18.6583811991965,11.3962285549873));
#39762=CARTESIAN_POINT('Ctrl Pts',(55.648202463344,18.6353683273631,11.3919637941489));
#39763=CARTESIAN_POINT('Ctrl Pts',(55.5685879835304,18.6163771365871,11.3876990333105));
#39764=CARTESIAN_POINT('Ctrl Pts',(55.4889735037168,18.5973859458111,11.383434272472));
#39765=CARTESIAN_POINT('Ctrl Pts',(55.4085266915533,18.5824164610675,11.3791695116336));
#39766=CARTESIAN_POINT('Ctrl Pts',(55.3276874022963,18.5715084483622,11.3749047507952));
#39767=CARTESIAN_POINT('Ctrl Pts',(55.247483879732,18.5606862225462,11.3706735304904));
#39768=CARTESIAN_POINT('Ctrl Pts',(55.1665932833734,18.5538211859867,11.3664423101855));
#39769=CARTESIAN_POINT('Ctrl Pts',(55.0854400562631,18.5509899455523,11.3622110898807));
#39770=CARTESIAN_POINT('Ctrl Pts',(55.0044031972008,18.5481627649186,11.3579859368496));
#39771=CARTESIAN_POINT('Ctrl Pts',(54.9231049160502,18.5493579086654,11.3537607838185));
#39772=CARTESIAN_POINT('Ctrl Pts',(54.8419767495782,18.5546004616165,11.3495356307875));
#39773=CARTESIAN_POINT('Ctrl Pts',(54.7606401681106,18.5598564824753,11.3452996235082));
#39774=CARTESIAN_POINT('Ctrl Pts',(54.6794750451078,18.5691807911745,11.341063616229));
#39775=CARTESIAN_POINT('Ctrl Pts',(54.5989182756023,18.5825460293205,11.3368276089498));
#39776=CARTESIAN_POINT('Ctrl Pts',(54.5187124729514,18.5958530382746,11.3326100569557));
#39777=CARTESIAN_POINT('Ctrl Pts',(54.4391101968478,18.6131657708415,11.3283925049616));
#39778=CARTESIAN_POINT('Ctrl Pts',(54.3605376804652,18.6344053196088,11.3241749529675));
#39779=CARTESIAN_POINT('Ctrl Pts',(54.28199110694,18.6556378555602,11.3199587935132));
#39780=CARTESIAN_POINT('Ctrl Pts',(54.2044740663978,18.680794511728,11.3157426340588));
#39781=CARTESIAN_POINT('Ctrl Pts',(54.12840051971,18.7097457355223,11.3115264746044));
#39782=CARTESIAN_POINT('Ctrl Pts',(54.052328785701,18.7386962694676,11.3073104156126));
#39783=CARTESIAN_POINT('Ctrl Pts',(53.977700911284,18.7714410248668,11.3030943566208));
#39784=CARTESIAN_POINT('Ctrl Pts',(53.9049123089564,18.8078017427877,11.298878297629));
#39785=CARTESIAN_POINT('Ctrl Pts',(53.8315278854098,18.8444600964178,11.2946277275004));
#39786=CARTESIAN_POINT('Ctrl Pts',(53.760013420497,18.8847936837206,11.2903771573719));
#39787=CARTESIAN_POINT('Ctrl Pts',(53.690748551739,18.9285727395763,11.2861265872433));
#39788=CARTESIAN_POINT('Ctrl Pts',(53.621946170427,18.972059478936,11.2819043985346));
#39789=CARTESIAN_POINT('Ctrl Pts',(53.5553637835531,19.0189454947302,11.2776822098259));
#39790=CARTESIAN_POINT('Ctrl Pts',(53.491342515972,19.0689632717407,11.2734600211172));
#39791=CARTESIAN_POINT('Ctrl Pts',(53.4266757249664,19.1194853756401,11.2691952602787));
#39792=CARTESIAN_POINT('Ctrl Pts',(53.3646223585371,19.1732024330741,11.2649304994403));
#39793=CARTESIAN_POINT('Ctrl Pts',(53.3054965788037,19.2297998967478,11.2606657386018));
#39794=CARTESIAN_POINT('Ctrl Pts',(53.2463707990704,19.2863973604215,11.2564009777633));
#39795=CARTESIAN_POINT('Ctrl Pts',(53.1901728902236,19.3458748360093,11.2521362169248));
#39796=CARTESIAN_POINT('Ctrl Pts',(53.1371747641931,19.4078843035631,11.2478714560863));
#39797=CARTESIAN_POINT('Ctrl Pts',(53.084978212308,19.4689559042584,11.243671197944));
#39798=CARTESIAN_POINT('Ctrl Pts',(53.0356821499323,19.5327212540277,11.2394709398018));
#39799=CARTESIAN_POINT('Ctrl Pts',(52.989579824359,19.5988715378754,11.2352706816595));
#39800=CARTESIAN_POINT('Ctrl Pts',(52.9435395644599,19.6649327663031,11.2310760781529));
#39801=CARTESIAN_POINT('Ctrl Pts',(52.9006847776686,19.7333721750804,11.2268814746463));
#39802=CARTESIAN_POINT('Ctrl Pts',(52.861269680317,19.8038466362256,11.2226868711397));
#39803=CARTESIAN_POINT('Ctrl Pts',(52.821895136695,19.8742485870276,11.2184965834112));
#39804=CARTESIAN_POINT('Ctrl Pts',(52.7859534871032,19.9466810246936,11.2143062956827));
#39805=CARTESIAN_POINT('Ctrl Pts',(52.753655799209,20.0207717418433,11.2101160079543));
#39806=CARTESIAN_POINT('Ctrl Pts',(52.7200702369489,20.0978168356555,11.2057586319758));
#39807=CARTESIAN_POINT('Ctrl Pts',(52.6904256377389,20.1766547953242,11.2014012559973));
#39808=CARTESIAN_POINT('Ctrl Pts',(52.6649062967312,20.2568394204786,11.1970438800187));
#39809=CARTESIAN_POINT('Ctrl Pts',(52.6403884442667,20.3338772565604,11.1928575061879));
#39810=CARTESIAN_POINT('Ctrl Pts',(52.6196782504374,20.4121575423248,11.1886711323571));
#39811=CARTESIAN_POINT('Ctrl Pts',(52.6028890948132,20.4912667120831,11.1844847585263));
#39812=CARTESIAN_POINT('Ctrl Pts',(52.5861014055014,20.5703689726942,11.1802987503203));
#39813=CARTESIAN_POINT('Ctrl Pts',(52.5732341644404,20.6502995101256,11.1761127421143));
#39814=CARTESIAN_POINT('Ctrl Pts',(52.5643497089472,20.7306342455053,11.1719267339082));
#39815=CARTESIAN_POINT('Ctrl Pts',(52.5554609560948,20.8110078383281,11.1677387009544));
#39816=CARTESIAN_POINT('Ctrl Pts',(52.5505588735669,20.8917855489702,11.1635506680006));
#39817=CARTESIAN_POINT('Ctrl Pts',(52.5496538719983,20.9725390643463,11.1593626350468));
#39818=CARTESIAN_POINT('Ctrl Pts',(52.5495432947839,20.9824058967282,11.1588509221019));
#39819=CARTESIAN_POINT('Ctrl Pts',(52.5494923263623,20.9922723686099,11.158339209157));
#39820=CARTESIAN_POINT('Ctrl Pts',(52.5495009324145,21.0021377003384,11.1578274962121));
#39821=CARTESIAN_POINT('',(52.5495000019056,20.9999033600977,10.3578274961648));
#39822=CARTESIAN_POINT('Ctrl Pts',(52.5495009324152,21.0021377010802,11.1578274961736));
#39823=CARTESIAN_POINT('Ctrl Pts',(52.5495871706129,21.1009946578049,11.152699803984));
#39824=CARTESIAN_POINT('Ctrl Pts',(52.5556592523511,21.1995889286046,11.1475721117945));
#39825=CARTESIAN_POINT('Ctrl Pts',(52.5675996184674,21.2972854418235,11.1424444196049));
#39826=CARTESIAN_POINT('Ctrl Pts',(52.5797203219372,21.3964574818786,11.1372392830196));
#39827=CARTESIAN_POINT('Ctrl Pts',(52.5978878444661,21.494704482279,11.1320341464343));
#39828=CARTESIAN_POINT('Ctrl Pts',(52.6219304938964,21.5913845399908,11.126829009849));
#39829=CARTESIAN_POINT('Ctrl Pts',(52.6311544509903,21.6284758225782,11.1248320603584));
#39830=CARTESIAN_POINT('Ctrl Pts',(52.6412426517189,21.6653366993448,11.1228351108679));
#39831=CARTESIAN_POINT('Ctrl Pts',(52.6521835550092,21.7019317563914,11.1208381613774));
#39832=CARTESIAN_POINT('Ctrl Pts',(52.6753655996086,21.779470897545,11.1166069410728));
#39833=CARTESIAN_POINT('Ctrl Pts',(52.7024364554993,21.8560057658528,11.1123757207682));
#39834=CARTESIAN_POINT('Ctrl Pts',(52.7332910592392,21.9311180525987,11.1081445004636));
#39835=CARTESIAN_POINT('Ctrl Pts',(52.764101419637,22.0061226335826,11.1039193474328));
#39836=CARTESIAN_POINT('Ctrl Pts',(52.7986845770104,22.0797082579402,11.0996941944019));
#39837=CARTESIAN_POINT('Ctrl Pts',(52.836885599102,22.1514713798561,11.0954690413711));
#39838=CARTESIAN_POINT('Ctrl Pts',(52.875184758085,22.2234188583499,11.0912330340918));
#39839=CARTESIAN_POINT('Ctrl Pts',(52.9171202525201,22.2935340081507,11.0869970268126));
#39840=CARTESIAN_POINT('Ctrl Pts',(52.9624871569658,22.3614300071875,11.0827610195333));
#39841=CARTESIAN_POINT('Ctrl Pts',(53.0076564085001,22.4290301993572,11.0785434675394));
#39842=CARTESIAN_POINT('Ctrl Pts',(53.056226979573,22.4944301435069,11.0743259155456));
#39843=CARTESIAN_POINT('Ctrl Pts',(53.1079513664885,22.5572739702529,11.0701083635518));
#39844=CARTESIAN_POINT('Ctrl Pts',(53.1596586751881,22.620097047397,11.0658922040976));
#39845=CARTESIAN_POINT('Ctrl Pts',(53.2145174365962,22.6803653244593,11.0616760446435));
#39846=CARTESIAN_POINT('Ctrl Pts',(53.2722390558199,22.7377549797845,11.0574598851894));
#39847=CARTESIAN_POINT('Ctrl Pts',(53.3299592996544,22.7951432676306,11.0532438261978));
#39848=CARTESIAN_POINT('Ctrl Pts',(53.3905419351955,22.8496527431039,11.0490277672062));
#39849=CARTESIAN_POINT('Ctrl Pts',(53.4536616286813,22.9009965521767,11.0448117082146));
#39850=CARTESIAN_POINT('Ctrl Pts',(53.5172979971973,22.9527606431399,11.0405611380858));
#39851=CARTESIAN_POINT('Ctrl Pts',(53.5835127882373,23.0013066873144,11.0363105679569));
#39852=CARTESIAN_POINT('Ctrl Pts',(53.6519402353701,23.0463834247242,11.032059997828));
#39853=CARTESIAN_POINT('Ctrl Pts',(53.7199107865843,23.0911591809019,11.0278378091196));
#39854=CARTESIAN_POINT('Ctrl Pts',(53.7900640998296,23.1325116337779,11.0236156204111));
#39855=CARTESIAN_POINT('Ctrl Pts',(53.8620158781113,23.1702401683521,11.0193934317027));
#39856=CARTESIAN_POINT('Ctrl Pts',(53.9346931427967,23.20834911797,11.0151286708636));
#39857=CARTESIAN_POINT('Ctrl Pts',(54.0092049032931,23.2427604546778,11.0108639100245));
#39858=CARTESIAN_POINT('Ctrl Pts',(54.0851351159479,23.2733175083847,11.0065991491855));
#39859=CARTESIAN_POINT('Ctrl Pts',(54.1610653286027,23.3038745620916,11.0023343883464));
#39860=CARTESIAN_POINT('Ctrl Pts',(54.2384135170271,23.3305772363051,10.9980696275074));
#39861=CARTESIAN_POINT('Ctrl Pts',(54.3167505443871,23.3533211492282,10.9938048666683));
#39862=CARTESIAN_POINT('Ctrl Pts',(54.3944714842643,23.375886190926,10.9895736463638));
#39863=CARTESIAN_POINT('Ctrl Pts',(54.4734571969759,23.394639177157,10.9853424260592));
#39864=CARTESIAN_POINT('Ctrl Pts',(54.55329923705,23.4094415698207,10.9811112057547));
#39865=CARTESIAN_POINT('Ctrl Pts',(54.6330267892266,23.4242227368892,10.9768860527239));
#39866=CARTESIAN_POINT('Ctrl Pts',(54.7136077767622,23.4350644772212,10.9726608996931));
#39867=CARTESIAN_POINT('Ctrl Pts',(54.7946191185351,23.4418781590261,10.9684357466624));
#39868=CARTESIAN_POINT('Ctrl Pts',(54.875838575193,23.448709344906,10.9641997393831));
#39869=CARTESIAN_POINT('Ctrl Pts',(54.9574901449595,23.4514916244867,10.9599637321038));
#39870=CARTESIAN_POINT('Ctrl Pts',(55.0391376911991,23.4501874399987,10.9557277248245));
#39871=CARTESIAN_POINT('Ctrl Pts',(55.1204295183194,23.4488889375353,10.9515101728307));
#39872=CARTESIAN_POINT('Ctrl Pts',(55.2017168889558,23.4435395035627,10.947292620837));
#39873=CARTESIAN_POINT('Ctrl Pts',(55.2825665871558,23.4341541392901,10.9430750688432));
#39874=CARTESIAN_POINT('Ctrl Pts',(55.3633895906246,23.4247718738513,10.9388589093892));
#39875=CARTESIAN_POINT('Ctrl Pts',(55.4437747471745,23.4113563779819,10.9346427499351));
#39876=CARTESIAN_POINT('Ctrl Pts',(55.5232934879438,23.3939745561462,10.9304265904811));
#39877=CARTESIAN_POINT('Ctrl Pts',(55.6028103339426,23.3765931484842,10.9262105314896));
#39878=CARTESIAN_POINT('Ctrl Pts',(55.6814603512475,23.3552457031302,10.9219944724981));
#39879=CARTESIAN_POINT('Ctrl Pts',(55.7588261118878,23.3300500385007,10.9177784135066));
#39880=CARTESIAN_POINT('Ctrl Pts',(55.8368251607256,23.304648131253,10.9135278433777));
#39881=CARTESIAN_POINT('Ctrl Pts',(55.9135183698222,23.2753348469565,10.9092772732488));
#39882=CARTESIAN_POINT('Ctrl Pts',(55.9884962951118,23.2422812768585,10.9050267031198));
#39883=CARTESIAN_POINT('Ctrl Pts',(56.0629735863762,23.2094484082775,10.9008045144115));
#39884=CARTESIAN_POINT('Ctrl Pts',(56.1357580383577,23.1729253160255,10.8965823257031));
#39885=CARTESIAN_POINT('Ctrl Pts',(56.2064727130147,23.1329261221972,10.8923601369948));
#39886=CARTESIAN_POINT('Ctrl Pts',(56.2779004004225,23.0925236183718,10.8880953761555));
#39887=CARTESIAN_POINT('Ctrl Pts',(56.3472159263617,23.0485747798123,10.8838306153163));
#39888=CARTESIAN_POINT('Ctrl Pts',(56.4140620631266,23.0013442311672,10.8795658544771));
#39889=CARTESIAN_POINT('Ctrl Pts',(56.4809081998916,22.954113682522,10.8753010936378));
#39890=CARTESIAN_POINT('Ctrl Pts',(56.5452846080975,22.9036017717496,10.8710363327986));
#39891=CARTESIAN_POINT('Ctrl Pts',(56.6068708951037,22.8501124767074,10.8667715719594));
#39892=CARTESIAN_POINT('Ctrl Pts',(56.6679728321258,22.7970438522474,10.8625403516524));
#39893=CARTESIAN_POINT('Ctrl Pts',(56.7265575327523,22.7408455411942,10.8583091313454));
#39894=CARTESIAN_POINT('Ctrl Pts',(56.7822871243166,22.6817856154978,10.8540779110384));
#39895=CARTESIAN_POINT('Ctrl Pts',(56.8379368035473,22.6228103776011,10.8498527580051));
#39896=CARTESIAN_POINT('Ctrl Pts',(56.8907391883744,22.5609820099245,10.8456276049719));
#39897=CARTESIAN_POINT('Ctrl Pts',(56.9403904034097,22.4966079420996,10.8414024519387));
#39898=CARTESIAN_POINT('Ctrl Pts',(56.9901691703871,22.4320684999255,10.83716644466));
#39899=CARTESIAN_POINT('Ctrl Pts',(57.0367802042399,22.3649705756235,10.8329304373813));
#39900=CARTESIAN_POINT('Ctrl Pts',(57.0799554647948,22.2956602619786,10.8286944301026));
#39901=CARTESIAN_POINT('Ctrl Pts',(57.1229426209447,22.2266519169874,10.8244768781064));
#39902=CARTESIAN_POINT('Ctrl Pts',(57.1625236247463,22.1554508129655,10.8202593261102));
#39903=CARTESIAN_POINT('Ctrl Pts',(57.1984761815963,22.0824290872633,10.8160417741139));
#39904=CARTESIAN_POINT('Ctrl Pts',(57.2344168677299,22.0094314716739,10.8118256146574));
#39905=CARTESIAN_POINT('Ctrl Pts',(57.2667312808295,21.9346148449387,10.8076094552009));
#39906=CARTESIAN_POINT('Ctrl Pts',(57.295243256997,21.8583755828364,10.8033932957444));
#39907=CARTESIAN_POINT('Ctrl Pts',(57.3237545537818,21.7821381373614,10.7991772367505));
#39908=CARTESIAN_POINT('Ctrl Pts',(57.3484634319622,21.7044785597722,10.7949611777565));
#39909=CARTESIAN_POINT('Ctrl Pts',(57.369242548178,21.6258114715336,10.7907451187626));
#39910=CARTESIAN_POINT('Ctrl Pts',(57.3901917547139,21.5465004430002,10.7864945486366));
#39911=CARTESIAN_POINT('Ctrl Pts',(57.4071464290845,21.4661657931605,10.7822439785105));
#39912=CARTESIAN_POINT('Ctrl Pts',(57.4200283186945,21.3852443208103,10.7779934083845));
#39913=CARTESIAN_POINT('Ctrl Pts',(57.4328241948411,21.3048631679564,10.7737712196737));
#39914=CARTESIAN_POINT('Ctrl Pts',(57.4416015201006,21.2239034786879,10.769549030963));
#39915=CARTESIAN_POINT('Ctrl Pts',(57.4463358233932,21.1427980713562,10.7653268422522));
#39916=CARTESIAN_POINT('Ctrl Pts',(57.4511178624351,21.0608748821574,10.7610620814186));
#39917=CARTESIAN_POINT('Ctrl Pts',(57.4517748855337,20.978803505601,10.7567973205849));
#39918=CARTESIAN_POINT('Ctrl Pts',(57.4483355430156,20.897027582302,10.7525325597513));
#39919=CARTESIAN_POINT('Ctrl Pts',(57.4448962004975,20.815251659003,10.7482677989176));
#39920=CARTESIAN_POINT('Ctrl Pts',(57.437360600708,20.7337716627951,10.744003038084));
#39921=CARTESIAN_POINT('Ctrl Pts',(57.425810432708,20.6530216223381,10.7397382772503));
#39922=CARTESIAN_POINT('Ctrl Pts',(57.4143511018711,20.5729066466346,10.7355070569483));
#39923=CARTESIAN_POINT('Ctrl Pts',(57.3988971971231,20.4932097575724,10.7312758366463));
#39924=CARTESIAN_POINT('Ctrl Pts',(57.37949076006,20.4143602021813,10.7270446163443));
#39925=CARTESIAN_POINT('Ctrl Pts',(57.3601121504693,20.3356237115338,10.7228194633161));
#39926=CARTESIAN_POINT('Ctrl Pts',(57.3367923751243,20.257732589083,10.7185943102879));
#39927=CARTESIAN_POINT('Ctrl Pts',(57.3096249794038,20.1811088567375,10.7143691572596));
#39928=CARTESIAN_POINT('Ctrl Pts',(57.2823877917139,20.104288281042,10.7101331499797));
#39929=CARTESIAN_POINT('Ctrl Pts',(57.2512832627651,20.028742081885,10.7058971426998));
#39930=CARTESIAN_POINT('Ctrl Pts',(57.216456854722,19.9548831351683,10.7016611354198));
#39931=CARTESIAN_POINT('Ctrl Pts',(57.1817821771579,19.8813459745324,10.6974435834286));
#39932=CARTESIAN_POINT('Ctrl Pts',(57.1434181757188,19.809481821746,10.6932260314373));
#39933=CARTESIAN_POINT('Ctrl Pts',(57.101557000381,19.7396792375948,10.689008479446));
#39934=CARTESIAN_POINT('Ctrl Pts',(57.0597096466508,19.6698997006687,10.6847923199944));
#39935=CARTESIAN_POINT('Ctrl Pts',(57.0143676509957,19.6021807790421,10.6805761605429));
#39936=CARTESIAN_POINT('Ctrl Pts',(56.9657685424522,19.536885415456,10.6763600010913));
#39937=CARTESIAN_POINT('Ctrl Pts',(56.9171705919267,19.4715916077256,10.6721439421022));
#39938=CARTESIAN_POINT('Ctrl Pts',(56.8653159613015,19.4087216155108,10.6679278831131));
#39939=CARTESIAN_POINT('Ctrl Pts',(56.8104839818457,19.3486072540186,10.6637118241241));
#39940=CARTESIAN_POINT('Ctrl Pts',(56.7552031675232,19.2880008179797,10.6594612539922));
#39941=CARTESIAN_POINT('Ctrl Pts',(56.696896347794,19.2301956993413,10.6552106838603));
#39942=CARTESIAN_POINT('Ctrl Pts',(56.6358881061925,19.1754944905488,10.6509601137284));
#39943=CARTESIAN_POINT('Ctrl Pts',(56.575287221918,19.1211585264775,10.6467379250224));
#39944=CARTESIAN_POINT('Ctrl Pts',(56.5120212848464,19.06988539592,10.6425157363164));
#39945=CARTESIAN_POINT('Ctrl Pts',(56.4464406955112,19.0219303439037,10.6382935476104));
#39946=CARTESIAN_POINT('Ctrl Pts',(56.3801988600434,18.9734917632548,10.6340287867655));
#39947=CARTESIAN_POINT('Ctrl Pts',(56.3115958385816,18.9284388165062,10.6297640259207));
#39948=CARTESIAN_POINT('Ctrl Pts',(56.2410199284995,18.886987982271,10.6254992650758));
#39949=CARTESIAN_POINT('Ctrl Pts',(56.1704440184173,18.8455371480358,10.621234504231));
#39950=CARTESIAN_POINT('Ctrl Pts',(56.0978956765939,18.8076885922014,10.6169697433862));
#39951=CARTESIAN_POINT('Ctrl Pts',(56.023783882858,18.7736090165471,10.6127049825413));
#39952=CARTESIAN_POINT('Ctrl Pts',(55.9502549470577,18.7397974623522,10.6084737622381));
#39953=CARTESIAN_POINT('Ctrl Pts',(55.8749113572368,18.7095689861589,10.6042425419349));
#39954=CARTESIAN_POINT('Ctrl Pts',(55.7981365778044,18.6831210102444,10.6000113216317));
#39955=CARTESIAN_POINT('Ctrl Pts',(55.7214718880329,18.6567109588765,10.5957861686022));
#39956=CARTESIAN_POINT('Ctrl Pts',(55.6433805203861,18.6340707914778,10.5915610155728));
#39957=CARTESIAN_POINT('Ctrl Pts',(55.5642677949466,18.6153507374068,10.5873358625434));
#39958=CARTESIAN_POINT('Ctrl Pts',(55.4849518320595,18.596582592261,10.5830998552638));
#39959=CARTESIAN_POINT('Ctrl Pts',(55.4046096885351,18.5817549188206,10.5788638479842));
#39960=CARTESIAN_POINT('Ctrl Pts',(55.3236671500716,18.5709693649596,10.5746278407045));
#39961=CARTESIAN_POINT('Ctrl Pts',(55.2430772592082,18.5602308012198,10.5704102887122));
#39962=CARTESIAN_POINT('Ctrl Pts',(55.1618926567472,18.5534992792872,10.5661927367199));
#39963=CARTESIAN_POINT('Ctrl Pts',(55.080544013118,18.5508240340982,10.5619751847275));
#39964=CARTESIAN_POINT('Ctrl Pts',(54.9992222289608,18.5481496722144,10.5577590252749));
#39965=CARTESIAN_POINT('Ctrl Pts',(54.9177369755005,18.5495289427011,10.5535428658223));
#39966=CARTESIAN_POINT('Ctrl Pts',(54.8365220034965,18.5549590607396,10.5493267063697));
#39967=CARTESIAN_POINT('Ctrl Pts',(54.755308966681,18.5603890493895,10.5451106473797));
#39968=CARTESIAN_POINT('Ctrl Pts',(54.674366662329,18.5698696615555,10.5408945883897));
#39969=CARTESIAN_POINT('Ctrl Pts',(54.5941253528281,18.5833461106764,10.5366785293996));
#39970=CARTESIAN_POINT('Ctrl Pts',(54.5132272168649,18.5969328731565,10.532427959269));
#39971=CARTESIAN_POINT('Ctrl Pts',(54.4330420806568,18.6145811278778,10.5281773891384));
#39972=CARTESIAN_POINT('Ctrl Pts',(54.3540001893596,18.6361822205059,10.5239268190078));
#39973=CARTESIAN_POINT('Ctrl Pts',(54.2754860675948,18.6576390807735,10.5197046303009));
#39974=CARTESIAN_POINT('Ctrl Pts',(54.1981003970615,18.6829959478841,10.5154824415941));
#39975=CARTESIAN_POINT('Ctrl Pts',(54.1222476384813,18.7120968023432,10.5112602528872));
#39976=CARTESIAN_POINT('Ctrl Pts',(54.0456300600057,18.7414910793867,10.5069954920448));
#39977=CARTESIAN_POINT('Ctrl Pts',(53.9705769242785,18.7747050730503,10.5027307312023));
#39978=CARTESIAN_POINT('Ctrl Pts',(53.897480667602,18.8115299015777,10.4984659703598));
#39979=CARTESIAN_POINT('Ctrl Pts',(53.8243844109255,18.8483547301051,10.4942012095173));
#39980=CARTESIAN_POINT('Ctrl Pts',(53.7532454204141,18.8887900995583,10.4899364486748));
#39981=CARTESIAN_POINT('Ctrl Pts',(53.6844255225931,18.9325827599646,10.4856716878324));
#39982=CARTESIAN_POINT('Ctrl Pts',(53.6161468638785,18.9760310097988,10.4814404675126));
#39983=CARTESIAN_POINT('Ctrl Pts',(53.5498948890266,19.0229468192873,10.4772092471929));
#39984=CARTESIAN_POINT('Ctrl Pts',(53.4860434019957,19.0731150347363,10.4729780268731));
#39985=CARTESIAN_POINT('Ctrl Pts',(53.4222834735272,19.1232113124765,10.4687528738271));
#39986=CARTESIAN_POINT('Ctrl Pts',(53.3609175590427,19.176550448862,10.4645277207811));
#39987=CARTESIAN_POINT('Ctrl Pts',(53.3022916599641,19.2328733372584,10.4603025677351));
#39988=CARTESIAN_POINT('Ctrl Pts',(53.2435151535691,19.2893409166395,10.4560665604596));
#39989=CARTESIAN_POINT('Ctrl Pts',(53.1874931533305,19.3488073390837,10.4518305531841));
#39990=CARTESIAN_POINT('Ctrl Pts',(53.1345419376873,19.410969960085,10.4475945459086));
#39991=CARTESIAN_POINT('Ctrl Pts',(53.0818214177749,19.4728617534743,10.4433769938996));
#39992=CARTESIAN_POINT('Ctrl Pts',(53.0321452905348,19.5374259501685,10.4391594418906));
#39993=CARTESIAN_POINT('Ctrl Pts',(52.9857884438147,19.6043273818944,10.4349418898816));
#39994=CARTESIAN_POINT('Ctrl Pts',(52.9394469030711,19.6712067242892,10.4307257304123));
#39995=CARTESIAN_POINT('Ctrl Pts',(52.8964227310292,19.7404213873773,10.426509570943));
#39996=CARTESIAN_POINT('Ctrl Pts',(52.8569487769205,19.8116054084365,10.4222934114738));
#39997=CARTESIAN_POINT('Ctrl Pts',(52.8174757633966,19.8827877333238,10.4180773524671));
#39998=CARTESIAN_POINT('Ctrl Pts',(52.781553024109,19.9559389157528,10.4138612934604));
#39999=CARTESIAN_POINT('Ctrl Pts',(52.7493678231144,20.0306677275737,10.4096452344537));
#40000=CARTESIAN_POINT('Ctrl Pts',(52.716919165934,20.1060082418888,10.4053946643429));
#40001=CARTESIAN_POINT('Ctrl Pts',(52.6882697221966,20.1829518983535,10.401144094232));
#40002=CARTESIAN_POINT('Ctrl Pts',(52.6635614850033,20.2610782750249,10.3968935241212));
#40003=CARTESIAN_POINT('Ctrl Pts',(52.6390182266337,20.3386829957958,10.3926713353979));
#40004=CARTESIAN_POINT('Ctrl Pts',(52.6183637628908,20.4174542208098,10.3884491466747));
#40005=CARTESIAN_POINT('Ctrl Pts',(52.6016863081134,20.4969675106823,10.3842269579514));
#40006=CARTESIAN_POINT('Ctrl Pts',(52.584840695537,20.5772825283961,10.3799621971467));
#40007=CARTESIAN_POINT('Ctrl Pts',(52.5720528189215,20.6583541797246,10.3756974363421));
#40008=CARTESIAN_POINT('Ctrl Pts',(52.5633599559602,20.7397394655701,10.3714326755374));
#40009=CARTESIAN_POINT('Ctrl Pts',(52.5546670929989,20.8211247514157,10.3671679147327));
#40010=CARTESIAN_POINT('Ctrl Pts',(52.5500692066164,20.9028231871315,10.3629031539281));
#40011=CARTESIAN_POINT('Ctrl Pts',(52.5495496974743,20.984393435621,10.3586383931234));
#40012=CARTESIAN_POINT('Ctrl Pts',(52.549516771176,20.989563327954,10.358368094153));
#40013=CARTESIAN_POINT('Ctrl Pts',(52.5495002057972,20.9947333245982,10.3580977951825));
#40014=CARTESIAN_POINT('Ctrl Pts',(52.5495000019056,20.9999033591928,10.3578274962121));
#40015=CARTESIAN_POINT('',(52.5495008814216,20.9979215759409,9.55782751980551));
#40016=CARTESIAN_POINT('Ctrl Pts',(52.5495000019056,20.9999033600977,10.3578274961648));
#40017=CARTESIAN_POINT('Ctrl Pts',(52.5494968138749,21.0807423211251,10.3536010857728));
#40018=CARTESIAN_POINT('Ctrl Pts',(52.5534980935076,21.1617346655812,10.3493746753808));
#40019=CARTESIAN_POINT('Ctrl Pts',(52.5615234123392,21.242450369004,10.3451482649887));
#40020=CARTESIAN_POINT('Ctrl Pts',(52.5695372224051,21.3230503214972,10.3409279155107));
#40021=CARTESIAN_POINT('Ctrl Pts',(52.5815635655934,21.4033739609398,10.3367075660326));
#40022=CARTESIAN_POINT('Ctrl Pts',(52.5975700052744,21.4829910666281,10.3324872165545));
#40023=CARTESIAN_POINT('Ctrl Pts',(52.6135579296484,21.5625160759366,10.3282717489282));
#40024=CARTESIAN_POINT('Ctrl Pts',(52.6335167096718,21.6413357210847,10.3240562813019));
#40025=CARTESIAN_POINT('Ctrl Pts',(52.6573622609584,21.7190261981445,10.3198408136756));
#40026=CARTESIAN_POINT('Ctrl Pts',(52.6811926990023,21.7966674352005,10.3156280178007));
#40027=CARTESIAN_POINT('Ctrl Pts',(52.7089048822194,21.8731804803106,10.3114152219258));
#40028=CARTESIAN_POINT('Ctrl Pts',(52.7403641984882,21.9481541512465,10.307202426051));
#40029=CARTESIAN_POINT('Ctrl Pts',(52.771813273478,22.0231034152221,10.3029910016114));
#40030=CARTESIAN_POINT('Ctrl Pts',(52.807006878973,22.0965138706649,10.2987795771719));
#40031=CARTESIAN_POINT('Ctrl Pts',(52.845761842108,22.1679932401696,10.2945681527323));
#40032=CARTESIAN_POINT('Ctrl Pts',(52.8845161352268,22.2394713739015,10.2903568011021));
#40033=CARTESIAN_POINT('Ctrl Pts',(52.926831440305,22.3090180788987,10.2861454494719));
#40034=CARTESIAN_POINT('Ctrl Pts',(52.9724787890595,22.3762659587399,10.2819340978416));
#40035=CARTESIAN_POINT('Ctrl Pts',(53.0181712833848,22.4435803472396,10.277718581153));
#40036=CARTESIAN_POINT('Ctrl Pts',(53.0672021422222,22.508590982125,10.2735030644644));
#40037=CARTESIAN_POINT('Ctrl Pts',(53.1192995361303,22.5709602207568,10.2692875477758));
#40038=CARTESIAN_POINT('Ctrl Pts',(53.1714214988697,22.6333588723628,10.2650700430737));
#40039=CARTESIAN_POINT('Ctrl Pts',(53.2266125609176,22.6931133033122,10.2608525383716));
#40040=CARTESIAN_POINT('Ctrl Pts',(53.2845628387948,22.7499215970884,10.2566350336696));
#40041=CARTESIAN_POINT('Ctrl Pts',(53.3426183863275,22.8068330860473,10.2524098676537));
#40042=CARTESIAN_POINT('Ctrl Pts',(53.4034428159728,22.8607874332666,10.2481847016378));
#40043=CARTESIAN_POINT('Ctrl Pts',(53.4666919790198,22.9115221062802,10.2439595356219));
#40044=CARTESIAN_POINT('Ctrl Pts',(53.5283390882967,22.9609717081519,10.239841389886));
#40045=CARTESIAN_POINT('Ctrl Pts',(53.5922891706085,23.0073626493486,10.2357232441502));
#40046=CARTESIAN_POINT('Ctrl Pts',(53.6581991488266,23.0504928007165,10.2316050984144));
#40047=CARTESIAN_POINT('Ctrl Pts',(53.7259188595341,23.0948072042769,10.2273738781133));
#40048=CARTESIAN_POINT('Ctrl Pts',(53.7959631933162,23.1358463147716,10.2231426578122));
#40049=CARTESIAN_POINT('Ctrl Pts',(53.8679821008772,23.1733581679202,10.2189114375111));
#40050=CARTESIAN_POINT('Ctrl Pts',(53.9398977383606,23.2108162316944,10.2146862844841));
#40051=CARTESIAN_POINT('Ctrl Pts',(54.0137819173865,23.2447568704125,10.210461131457));
#40052=CARTESIAN_POINT('Ctrl Pts',(54.0892559936636,23.2749715613436,10.20623597843));
#40053=CARTESIAN_POINT('Ctrl Pts',(54.1649239598955,23.305263872636,10.2019999711498));
#40054=CARTESIAN_POINT('Ctrl Pts',(54.2421896041229,23.3318108149255,10.1977639638696));
#40055=CARTESIAN_POINT('Ctrl Pts',(54.3206468564639,23.354448885911,10.1935279565894));
#40056=CARTESIAN_POINT('Ctrl Pts',(54.3987622889479,23.3769883281279,10.1893104046));
#40057=CARTESIAN_POINT('Ctrl Pts',(54.4780585208188,23.3956527505162,10.1850928526105));
#40058=CARTESIAN_POINT('Ctrl Pts',(54.5581168994866,23.410329764883,10.1808753006211));
#40059=CARTESIAN_POINT('Ctrl Pts',(54.6381488446949,23.4250019332327,10.1766591411716));
#40060=CARTESIAN_POINT('Ctrl Pts',(54.7189419800299,23.435689224277,10.1724429817221));
#40061=CARTESIAN_POINT('Ctrl Pts',(54.8000669129004,23.4423302419376,10.1682268222726));
#40062=CARTESIAN_POINT('Ctrl Pts',(54.881189912724,23.4489711013558,10.1640107632858));
#40063=CARTESIAN_POINT('Ctrl Pts',(54.9626442309016,23.4515658422601,10.1597947042991));
#40064=CARTESIAN_POINT('Ctrl Pts',(55.0439962339691,23.4501050143609,10.1555786453123));
#40065=CARTESIAN_POINT('Ctrl Pts',(55.1260141553641,23.4486322286484,10.1513280751784));
#40066=CARTESIAN_POINT('Ctrl Pts',(55.2079275989598,23.4430371653713,10.1470775050445));
#40067=CARTESIAN_POINT('Ctrl Pts',(55.2892949814708,23.4333636521687,10.1428269349106));
#40068=CARTESIAN_POINT('Ctrl Pts',(55.3701190668101,23.4237547298649,10.1386047462075));
#40069=CARTESIAN_POINT('Ctrl Pts',(55.4504039085215,23.4101217956555,10.1343825575043));
#40070=CARTESIAN_POINT('Ctrl Pts',(55.5297264190529,23.3925593348875,10.1301603688011));
#40071=CARTESIAN_POINT('Ctrl Pts',(55.6098487350281,23.374819792587,10.1258956079519));
#40072=CARTESIAN_POINT('Ctrl Pts',(55.6889887358762,23.3530711639465,10.1216308471026));
#40073=CARTESIAN_POINT('Ctrl Pts',(55.7667274080766,23.3274619936111,10.1173660862533));
#40074=CARTESIAN_POINT('Ctrl Pts',(55.844466080277,23.3018528232757,10.113101325404));
#40075=CARTESIAN_POINT('Ctrl Pts',(55.9208029975002,23.2723833446981,10.1088365645547));
#40076=CARTESIAN_POINT('Ctrl Pts',(55.9953428574725,23.239250509898,10.1045718037054));
#40077=CARTESIAN_POINT('Ctrl Pts',(56.0692964947102,23.2063782500578,10.100340583297));
#40078=CARTESIAN_POINT('Ctrl Pts',(56.141758576123,23.1697768240893,10.0961093628887));
#40079=CARTESIAN_POINT('Ctrl Pts',(56.2123275880256,23.1296037352785,10.0918781424803));
#40080=CARTESIAN_POINT('Ctrl Pts',(56.2827954089131,23.0894882518602,10.0876529893453));
#40081=CARTESIAN_POINT('Ctrl Pts',(56.3513751509179,23.0458115053795,10.0834278362102));
#40082=CARTESIAN_POINT('Ctrl Pts',(56.4176862966516,22.9987785806052,10.0792026830752));
#40083=CARTESIAN_POINT('Ctrl Pts',(56.4841677910085,22.9516248315881,10.074966675822));
#40084=CARTESIAN_POINT('Ctrl Pts',(56.5483685897364,22.9010978362283,10.0707306685687));
#40085=CARTESIAN_POINT('Ctrl Pts',(56.6099311324859,22.8474501342804,10.0664946613154));
#40086=CARTESIAN_POINT('Ctrl Pts',(56.6712254636377,22.7940361610775,10.0622771092172));
#40087=CARTESIAN_POINT('Ctrl Pts',(56.7299041211222,22.7375289179703,10.058059557119));
#40088=CARTESIAN_POINT('Ctrl Pts',(56.7856456698187,22.6782192323584,10.0538420050208));
#40089=CARTESIAN_POINT('Ctrl Pts',(56.8413688139224,22.6189291294571,10.0496258454624));
#40090=CARTESIAN_POINT('Ctrl Pts',(56.894156456908,22.5568387600887,10.0454096859041));
#40091=CARTESIAN_POINT('Ctrl Pts',(56.9437241855704,22.4922756248189,10.0411935263458));
#40092=CARTESIAN_POINT('Ctrl Pts',(56.9932907331308,22.4277140279624,10.0369774672503));
#40093=CARTESIAN_POINT('Ctrl Pts',(57.0396372366727,22.3606801518038,10.0327614081548));
#40094=CARTESIAN_POINT('Ctrl Pts',(57.0825206301869,22.2915332263809,10.0285453490593));
#40095=CARTESIAN_POINT('Ctrl Pts',(57.1257550493604,22.221820292928,10.0242947790541));
#40096=CARTESIAN_POINT('Ctrl Pts',(57.1654691351802,22.1499599566717,10.0200442090488));
#40097=CARTESIAN_POINT('Ctrl Pts',(57.2014602771032,22.0763470157605,10.0157936390436));
#40098=CARTESIAN_POINT('Ctrl Pts',(57.2372111049968,22.0032255908587,10.011571450233));
#40099=CARTESIAN_POINT('Ctrl Pts',(57.2692884259045,21.9283753503223,10.0073492614225));
#40100=CARTESIAN_POINT('Ctrl Pts',(57.2975422224359,21.852203019312,10.0031270726119));
#40101=CARTESIAN_POINT('Ctrl Pts',(57.3260808983991,21.7752626523898,9.99886231200933));
#40102=CARTESIAN_POINT('Ctrl Pts',(57.350718365958,21.6969738473857,9.99459755140675));
#40103=CARTESIAN_POINT('Ctrl Pts',(57.3713522393082,21.6177692183397,9.99033279080417));
#40104=CARTESIAN_POINT('Ctrl Pts',(57.3919861126584,21.5385645892937,9.9860680302016));
#40105=CARTESIAN_POINT('Ctrl Pts',(57.4086163567899,21.4584446210061,9.98180326959902));
#40106=CARTESIAN_POINT('Ctrl Pts',(57.4211941162249,21.3778482520243,9.97753850899644));
#40107=CARTESIAN_POINT('Ctrl Pts',(57.4336729570077,21.2978857387173,9.9733072888963));
#40108=CARTESIAN_POINT('Ctrl Pts',(57.4422096669418,21.2171544480391,9.96907606879615));
#40109=CARTESIAN_POINT('Ctrl Pts',(57.4467188763498,21.1360771476538,9.96484484869601));
#40110=CARTESIAN_POINT('Ctrl Pts',(57.451221619867,21.0551161064445,9.96061969586944));
#40111=CARTESIAN_POINT('Ctrl Pts',(57.4517083071476,20.9738105012146,9.95639454304287));
#40112=CARTESIAN_POINT('Ctrl Pts',(57.4481449328091,20.8925912575201,9.9521693902163));
#40113=CARTESIAN_POINT('Ctrl Pts',(57.4445724040893,20.8111633599318,9.94793338288593));
#40114=CARTESIAN_POINT('Ctrl Pts',(57.436928911295,20.7298227355339,9.94369737555556));
#40115=CARTESIAN_POINT('Ctrl Pts',(57.4252327702162,20.6490067518182,9.9394613682252));
#40116=CARTESIAN_POINT('Ctrl Pts',(57.4135875871669,20.5685428691288,9.9352438164337));
#40117=CARTESIAN_POINT('Ctrl Pts',(57.3979250544606,20.4885995293403,9.9310262646422));
#40118=CARTESIAN_POINT('Ctrl Pts',(57.3783152464065,20.4096045065293,9.9268087128507));
#40119=CARTESIAN_POINT('Ctrl Pts',(57.3587119130597,20.3306355660571,9.92259255359776));
#40120=CARTESIAN_POINT('Ctrl Pts',(57.33516400446,20.2526147716374,9.91837639434482));
#40121=CARTESIAN_POINT('Ctrl Pts',(57.3077924830991,20.1759586752162,9.91416023509187));
#40122=CARTESIAN_POINT('Ctrl Pts',(57.2804216139367,20.0993044053283,9.90994417630003));
#40123=CARTESIAN_POINT('Ctrl Pts',(57.2492274705443,20.0240152062594,9.90572811750818));
#40124=CARTESIAN_POINT('Ctrl Pts',(57.2143800949908,19.9504900929918,9.90151205871634));
#40125=CARTESIAN_POINT('Ctrl Pts',(57.179247467748,19.8763631219821,9.89726148834727));
#40126=CARTESIAN_POINT('Ctrl Pts',(57.1404017143843,19.8040296911584,9.8930109179782));
#40127=CARTESIAN_POINT('Ctrl Pts',(57.0980646984976,19.7338741093722,9.88876034760913));
#40128=CARTESIAN_POINT('Ctrl Pts',(57.0560103747993,19.6641869695517,9.8845381590949));
#40129=CARTESIAN_POINT('Ctrl Pts',(57.0105115838098,19.5966490383781,9.88031597058068));
#40130=CARTESIAN_POINT('Ctrl Pts',(56.9618287276784,19.5316069009778,9.87609378206645));
#40131=CARTESIAN_POINT('Ctrl Pts',(56.9126549970567,19.4659089366896,9.87182902076996));
#40132=CARTESIAN_POINT('Ctrl Pts',(56.8602329396191,19.4027577539757,9.86756425947346));
#40133=CARTESIAN_POINT('Ctrl Pts',(56.8048705373686,19.3424739539486,9.86329949817697));
#40134=CARTESIAN_POINT('Ctrl Pts',(56.7495081351182,19.2821901539216,9.85903473688047));
#40135=CARTESIAN_POINT('Ctrl Pts',(56.6912057764184,19.2247740288675,9.85476997558398));
#40136=CARTESIAN_POINT('Ctrl Pts',(56.6303057826845,19.1705046310675,9.85050521428748));
#40137=CARTESIAN_POINT('Ctrl Pts',(56.5698847474868,19.1166620443349,9.84627399394399));
#40138=CARTESIAN_POINT('Ctrl Pts',(56.5066802486927,19.0657149278249,9.8420427736005));
#40139=CARTESIAN_POINT('Ctrl Pts',(56.441001221378,19.0179642460372,9.83781155325701));
#40140=CARTESIAN_POINT('Ctrl Pts',(56.3754163732205,18.970282035406,9.8335864001892));
#40141=CARTESIAN_POINT('Ctrl Pts',(56.3073644166057,18.9257874274795,9.82936124712139));
#40142=CARTESIAN_POINT('Ctrl Pts',(56.2371889920002,18.884742652046,9.82513609405359));
#40143=CARTESIAN_POINT('Ctrl Pts',(56.1668332903206,18.8435924346851,9.82090008678379));
#40144=CARTESIAN_POINT('Ctrl Pts',(56.0943435531916,18.805910106625,9.816664079514));
#40145=CARTESIAN_POINT('Ctrl Pts',(56.020097203423,18.7719174284671,9.8124280722442));
#40146=CARTESIAN_POINT('Ctrl Pts',(55.9461743267744,18.7380728480635,9.80821052021823));
#40147=CARTESIAN_POINT('Ctrl Pts',(55.8705105338275,18.7078860370133,9.80399296819226));
#40148=CARTESIAN_POINT('Ctrl Pts',(55.7935032513437,18.6815300648689,9.79977541616629));
#40149=CARTESIAN_POINT('Ctrl Pts',(55.7165213949469,18.6551827948785,9.79555925668192));
#40150=CARTESIAN_POINT('Ctrl Pts',(55.6381973694481,18.6326640023938,9.79134309719755));
#40151=CARTESIAN_POINT('Ctrl Pts',(55.5589467650632,18.6140979140322,9.78712693771319));
#40152=CARTESIAN_POINT('Ctrl Pts',(55.4796980490954,18.5955322680713,9.78291087869327));
#40153=CARTESIAN_POINT('Ctrl Pts',(55.3995232510588,18.5809192439327,9.77869481967335));
#40154=CARTESIAN_POINT('Ctrl Pts',(55.318849838012,18.5703323209131,9.77447876065343));
#40155=CARTESIAN_POINT('Ctrl Pts',(55.2375160628204,18.5596587373329,9.77022819056385));
#40156=CARTESIAN_POINT('Ctrl Pts',(55.1556759455423,18.5530775497303,9.76597762047427));
#40157=CARTESIAN_POINT('Ctrl Pts',(55.0737726952354,18.5506107211311,9.7617270503847));
#40158=CARTESIAN_POINT('Ctrl Pts',(54.9924163187349,18.5481603637213,9.75750486165282));
#40159=CARTESIAN_POINT('Ctrl Pts',(54.9109981179188,18.5497695178218,9.75328267292095));
#40160=CARTESIAN_POINT('Ctrl Pts',(54.8299505016417,18.5554073103872,9.74906048418907));
#40161=CARTESIAN_POINT('Ctrl Pts',(54.7480856878631,18.5611019484247,9.74479572342064));
#40162=CARTESIAN_POINT('Ctrl Pts',(54.6665994561608,18.5709068651232,9.74053096265221));
#40163=CARTESIAN_POINT('Ctrl Pts',(54.5859281813169,18.5847371201104,9.73626620188378));
#40164=CARTESIAN_POINT('Ctrl Pts',(54.505256906473,18.5985673750977,9.73200144111536));
#40165=CARTESIAN_POINT('Ctrl Pts',(54.4254010446554,18.616422800541,9.72773668034693));
#40166=CARTESIAN_POINT('Ctrl Pts',(54.3467806794472,18.6381670742289,9.7234719195785));
#40167=CARTESIAN_POINT('Ctrl Pts',(54.2687786158218,18.6597403423662,9.71924069857201));
#40168=CARTESIAN_POINT('Ctrl Pts',(54.1917001746333,18.6852223634556,9.71500947756553));
#40169=CARTESIAN_POINT('Ctrl Pts',(54.1159657483402,18.7145167487176,9.71077825655904));
#40170=CARTESIAN_POINT('Ctrl Pts',(54.0403399198364,18.7437691279114,9.70655310282302));
#40171=CARTESIAN_POINT('Ctrl Pts',(53.966054708576,18.7768228477731,9.702327949087));
#40172=CARTESIAN_POINT('Ctrl Pts',(53.8935167787501,18.8135313560235,9.69810279535097));
#40173=CARTESIAN_POINT('Ctrl Pts',(53.8207925170533,18.8503341592867,9.69386678824758));
#40174=CARTESIAN_POINT('Ctrl Pts',(53.7498249781623,18.8908104194393,9.68963078114419));
#40175=CARTESIAN_POINT('Ctrl Pts',(53.6810051399095,18.9347632559305,9.68539477404079));
#40176=CARTESIAN_POINT('Ctrl Pts',(53.6124851191255,18.9785246094348,9.68117722133891));
#40177=CARTESIAN_POINT('Ctrl Pts',(53.546094523564,19.0257320657081,9.67695966863703));
#40178=CARTESIAN_POINT('Ctrl Pts',(53.4821942659225,19.0761455347139,9.67274211593515));
#40179=CARTESIAN_POINT('Ctrl Pts',(53.4183151066963,19.1265423583359,9.66852595577348));
#40180=CARTESIAN_POINT('Ctrl Pts',(53.3569250172281,19.1801428048135,9.66430979561181));
#40181=CARTESIAN_POINT('Ctrl Pts',(53.2983537192706,19.2366650388313,9.66009363545015));
#40182=CARTESIAN_POINT('Ctrl Pts',(53.2397838169685,19.2931859260194,9.65587757575247));
#40183=CARTESIAN_POINT('Ctrl Pts',(53.1840329064109,19.3526281386796,9.6516615160548));
#40184=CARTESIAN_POINT('Ctrl Pts',(53.1313945095377,19.4146723458496,9.64744545635713));
#40185=CARTESIAN_POINT('Ctrl Pts',(53.0783252530987,19.4772244016955,9.6431948870665));
#40186=CARTESIAN_POINT('Ctrl Pts',(53.0284200216479,19.5424208892982,9.63894431777586));
#40187=CARTESIAN_POINT('Ctrl Pts',(52.9819375867258,19.6099013178447,9.63469374848523));
#40188=CARTESIAN_POINT('Ctrl Pts',(52.9357655022891,19.6769311980541,9.63047155908142));
#40189=CARTESIAN_POINT('Ctrl Pts',(52.892970841555,19.746214181651,9.62624936967762));
#40190=CARTESIAN_POINT('Ctrl Pts',(52.8537621254998,19.8173702032923,9.62202718027381));
#40191=CARTESIAN_POINT('Ctrl Pts',(52.8141580912278,19.8892436488746,9.61776242103976));
#40192=CARTESIAN_POINT('Ctrl Pts',(52.7782129312753,19.9630276778113,9.61349766180572));
#40193=CARTESIAN_POINT('Ctrl Pts',(52.7460918875118,20.0383095765996,9.60923290257167));
#40194=CARTESIAN_POINT('Ctrl Pts',(52.7139708437484,20.1135914753878,9.60496814333762));
#40195=CARTESIAN_POINT('Ctrl Pts',(52.685674022499,20.1903707697382,9.60070338410357));
#40196=CARTESIAN_POINT('Ctrl Pts',(52.6613146594614,20.2682205742508,9.59643862486952));
#40197=CARTESIAN_POINT('Ctrl Pts',(52.6320142325393,20.3618614672617,9.59130880000159));
#40198=CARTESIAN_POINT('Ctrl Pts',(52.608319660546,20.4573346692796,9.58617897513365));
#40199=CARTESIAN_POINT('Ctrl Pts',(52.5904230808027,20.554029910788,9.58104915026572));
#40200=CARTESIAN_POINT('Ctrl Pts',(52.5727560657076,20.6494848142315,9.57598512715752));
#40201=CARTESIAN_POINT('Ctrl Pts',(52.5607392937498,20.7461305939467,9.57092110404933));
#40202=CARTESIAN_POINT('Ctrl Pts',(52.5545115088973,20.8433593606867,9.56585708094114));
#40203=CARTESIAN_POINT('Ctrl Pts',(52.5512198981138,20.894748299876,9.5631805605626));
#40204=CARTESIAN_POINT('Ctrl Pts',(52.549544665176,20.9462997469006,9.56050404018405));
#40205=CARTESIAN_POINT('Ctrl Pts',(52.5495008814216,20.9979215759409,9.55782751980551));
#40206=CARTESIAN_POINT('',(52.5495637068299,21.001288087881,8.75782746859915));
#40207=CARTESIAN_POINT('Ctrl Pts',(52.5511529243446,20.9979234318819,9.55782749621206));
#40208=CARTESIAN_POINT('Ctrl Pts',(52.5557236291845,21.5660081702359,9.52835344086155));
#40209=CARTESIAN_POINT('Ctrl Pts',(53.0353472451824,22.9572037199135,9.45653495394137));
#40210=CARTESIAN_POINT('Ctrl Pts',(55.3507382576877,23.8752188638192,9.34237203545155));
#40211=CARTESIAN_POINT('Ctrl Pts',(57.6060389677743,22.2643044328178,9.21533874074257));
#40212=CARTESIAN_POINT('Ctrl Pts',(57.4753636898807,19.4958460434894,9.08830544603359));
#40213=CARTESIAN_POINT('Ctrl Pts',(55.0783545536393,18.1045293080376,8.96127215132461));
#40214=CARTESIAN_POINT('Ctrl Pts',(52.9375321800744,19.1968516022151,8.85111283471743));
#40215=CARTESIAN_POINT('Ctrl Pts',(52.5551646396964,20.5095195307769,8.78329794967991));
#40216=CARTESIAN_POINT('Ctrl Pts',(52.5528298189475,21.0012858378839,8.75782749621206));
#40217=CARTESIAN_POINT('Ctrl Pts',(52.5495003385601,21.0012881315349,8.75782746806341));
#40218=CARTESIAN_POINT('Ctrl Pts',(52.5495477704209,21.0915209655461,8.75316030218582));
#40219=CARTESIAN_POINT('Ctrl Pts',(52.5545832033599,21.1815800967497,8.74849313630823));
#40220=CARTESIAN_POINT('Ctrl Pts',(52.5645245535201,21.2709420594764,8.74382597043064));
#40221=CARTESIAN_POINT('Ctrl Pts',(52.5745011987725,21.3606212868266,8.73914223456534));
#40222=CARTESIAN_POINT('Ctrl Pts',(52.5894185286338,21.4495981186264,8.73445849870003));
#40223=CARTESIAN_POINT('Ctrl Pts',(52.6091435960903,21.5373601268089,8.72977476283472));
#40224=CARTESIAN_POINT('Ctrl Pts',(52.6289649037067,21.6255503327513,8.72506817465271));
#40225=CARTESIAN_POINT('Ctrl Pts',(52.653640845938,21.7125135706083,8.7203615864707));
#40226=CARTESIAN_POINT('Ctrl Pts',(52.6829880937164,21.7977506353117,8.71565499828869));
#40227=CARTESIAN_POINT('Ctrl Pts',(52.7005498386225,21.8487575167122,8.71283851949467));
#40228=CARTESIAN_POINT('Ctrl Pts',(52.7197834453385,21.8991466775342,8.71002204070066));
#40229=CARTESIAN_POINT('Ctrl Pts',(52.7406417105928,21.9488152454968,8.70720556190665));
#40230=CARTESIAN_POINT('Ctrl Pts',(52.7719779732677,22.0234344563173,8.70297424553249));
#40231=CARTESIAN_POINT('Ctrl Pts',(52.807073594722,22.0966394811059,8.69874292915832));
#40232=CARTESIAN_POINT('Ctrl Pts',(52.8457793995175,22.168025622346,8.69451161278415));
#40233=CARTESIAN_POINT('Ctrl Pts',(52.8844296988496,22.2393093933893,8.69028636426409));
#40234=CARTESIAN_POINT('Ctrl Pts',(52.9266796796226,22.3087790560095,8.68606111574402));
#40235=CARTESIAN_POINT('Ctrl Pts',(52.9723321610904,22.3760499209882,8.68183586722395));
#40236=CARTESIAN_POINT('Ctrl Pts',(53.0181006288515,22.4434916966824,8.67759988388952));
#40237=CARTESIAN_POINT('Ctrl Pts',(53.0672887193487,22.5087230553778,8.6733639005551));
#40238=CARTESIAN_POINT('Ctrl Pts',(53.1196513535387,22.5713813088334,8.66912791722067));
#40239=CARTESIAN_POINT('Ctrl Pts',(53.1717873054375,22.6337683093875,8.66491027181791));
#40240=CARTESIAN_POINT('Ctrl Pts',(53.2270700786933,22.6936040725748,8.66069262641515));
#40241=CARTESIAN_POINT('Ctrl Pts',(53.2852155477713,22.7505612049839,8.65647498101239));
#40242=CARTESIAN_POINT('Ctrl Pts',(53.3433418054185,22.8074995185921,8.65225872913184));
#40243=CARTESIAN_POINT('Ctrl Pts',(53.4043285487249,22.8615607651248,8.6480424772513));
#40244=CARTESIAN_POINT('Ctrl Pts',(53.4678542208604,22.912453806361,8.64382622537076));
#40245=CARTESIAN_POINT('Ctrl Pts',(53.5313783627541,22.9633456216572,8.63961007505364));
#40246=CARTESIAN_POINT('Ctrl Pts',(53.5974409483611,23.0110690935869,8.63539392473653));
#40247=CARTESIAN_POINT('Ctrl Pts',(53.6656878424604,23.0553737655818,8.63117777441941));
#40248=CARTESIAN_POINT('Ctrl Pts',(53.7344900907205,23.1000389636382,8.62692731548427));
#40249=CARTESIAN_POINT('Ctrl Pts',(53.8055119663668,23.1412291913691,8.62267685654912));
#40250=CARTESIAN_POINT('Ctrl Pts',(53.8783629920347,23.1787337314052,8.61842639761398));
#40251=CARTESIAN_POINT('Ctrl Pts',(53.9507309817837,23.2159895990335,8.61420412118304));
#40252=CARTESIAN_POINT('Ctrl Pts',(54.0249034856629,23.2496083690804,8.60998184475211));
#40253=CARTESIAN_POINT('Ctrl Pts',(54.100476958074,23.2794316280696,8.60575956832118));
#40254=CARTESIAN_POINT('Ctrl Pts',(54.1768070779025,23.3095534798213,8.60149501813393));
#40255=CARTESIAN_POINT('Ctrl Pts',(54.2545659161888,23.3358032384644,8.59723046794667));
#40256=CARTESIAN_POINT('Ctrl Pts',(54.3333231470371,23.3580695968787,8.59296591775942));
#40257=CARTESIAN_POINT('Ctrl Pts',(54.4120803778855,23.380335955293,8.58870136757217));
#40258=CARTESIAN_POINT('Ctrl Pts',(54.4918355175178,23.3986188684309,8.58443681738492));
#40259=CARTESIAN_POINT('Ctrl Pts',(54.57215080854,23.4128604019642,8.58017226719767));
#40260=CARTESIAN_POINT('Ctrl Pts',(54.6518415404474,23.4269911884721,8.57594087960817));
#40261=CARTESIAN_POINT('Ctrl Pts',(54.7323823939831,23.4371962311709,8.57170949201866));
#40262=CARTESIAN_POINT('Ctrl Pts',(54.8133524211428,23.4433814543183,8.56747810442916));
#40263=CARTESIAN_POINT('Ctrl Pts',(54.8942063794495,23.4495578110768,8.56325278244593));
#40264=CARTESIAN_POINT('Ctrl Pts',(54.9754878298991,23.4517257576195,8.55902746046269));
#40265=CARTESIAN_POINT('Ctrl Pts',(55.0567666096346,23.449842403509,8.55480213847945));
#40266=CARTESIAN_POINT('Ctrl Pts',(55.1382501244665,23.4479543053719,8.55056617322983));
#40267=CARTESIAN_POINT('Ctrl Pts',(55.2197304893137,23.4419943955299,8.54633020798022));
#40268=CARTESIAN_POINT('Ctrl Pts',(55.3007700875323,23.4319719579892,8.5420942427306));
#40269=CARTESIAN_POINT('Ctrl Pts',(55.3814607014307,23.4219926805039,8.537876519001));
#40270=CARTESIAN_POINT('Ctrl Pts',(55.461713871787,23.4079858414377,8.53365879527139));
#40271=CARTESIAN_POINT('Ctrl Pts',(55.5411004392141,23.390012670402,8.52944107154179));
#40272=CARTESIAN_POINT('Ctrl Pts',(55.6204608084765,23.3720454306481,8.52522473969276));
#40273=CARTESIAN_POINT('Ctrl Pts',(55.6989546896901,23.3501145608329,8.52100840784372));
#40274=CARTESIAN_POINT('Ctrl Pts',(55.7761630923624,23.3243323996482,8.51679207599469));
#40275=CARTESIAN_POINT('Ctrl Pts',(55.8533696631064,23.2985508501984,8.5125758441868));
#40276=CARTESIAN_POINT('Ctrl Pts',(55.9292903753601,23.2689183393628,8.50835961237891));
#40277=CARTESIAN_POINT('Ctrl Pts',(56.0035227578039,23.2355966372693,8.50414338057102));
#40278=CARTESIAN_POINT('Ctrl Pts',(56.0783561418065,23.2020051554079,8.49989301323083));
#40279=CARTESIAN_POINT('Ctrl Pts',(56.1514732890126,23.1646646543371,8.49564264589063));
#40280=CARTESIAN_POINT('Ctrl Pts',(56.2224854615699,23.1237889599135,8.49139227855044));
#40281=CARTESIAN_POINT('Ctrl Pts',(56.2930297199746,23.0831826040444,8.48716991777532));
#40282=CARTESIAN_POINT('Ctrl Pts',(56.3614962992116,23.0390878089128,8.48294755700019));
#40283=CARTESIAN_POINT('Ctrl Pts',(56.4275332754918,22.9917577657345,8.47872519622507));
#40284=CARTESIAN_POINT('Ctrl Pts',(56.494227278364,22.9439568182429,8.47446082560234));
#40285=CARTESIAN_POINT('Ctrl Pts',(56.5584426838162,22.8928561899661,8.47019645497961));
#40286=CARTESIAN_POINT('Ctrl Pts',(56.6198526878366,22.8387570583708,8.46593208435688));
#40287=CARTESIAN_POINT('Ctrl Pts',(56.6812626918571,22.7846579267755,8.46166771373415));
#40288=CARTESIAN_POINT('Ctrl Pts',(56.7398669943921,22.7275606737917,8.45740334311141));
#40289=CARTESIAN_POINT('Ctrl Pts',(56.7953795976417,22.6678016519874,8.45313897248868));
#40290=CARTESIAN_POINT('Ctrl Pts',(56.8504512593943,22.6085173013567,8.4489084741374));
#40291=CARTESIAN_POINT('Ctrl Pts',(56.9026868253623,22.5463909028656,8.44467797578611));
#40292=CARTESIAN_POINT('Ctrl Pts',(56.9517790360638,22.4817249557127,8.44044747743483));
#40293=CARTESIAN_POINT('Ctrl Pts',(57.0008008247607,22.4171517708446,8.43622304766694));
#40294=CARTESIAN_POINT('Ctrl Pts',(57.0466879346531,22.3500466397073,8.43199861789905));
#40295=CARTESIAN_POINT('Ctrl Pts',(57.0891711073709,22.280747568464,8.42777418813116));
#40296=CARTESIAN_POINT('Ctrl Pts',(57.1317725266013,22.2112556120624,8.42353800019985));
#40297=CARTESIAN_POINT('Ctrl Pts',(57.1709507150789,22.139557834909,8.41930181226854));
#40298=CARTESIAN_POINT('Ctrl Pts',(57.2064760286778,22.0660271032531,8.41506562433723));
#40299=CARTESIAN_POINT('Ctrl Pts',(57.2418390103262,21.9928323682677,8.410848793551));
#40300=CARTESIAN_POINT('Ctrl Pts',(57.2735822177393,21.9178218121813,8.40663196276477));
#40301=CARTESIAN_POINT('Ctrl Pts',(57.3015244230522,21.8413890777127,8.40241513197854));
#40302=CARTESIAN_POINT('Ctrl Pts',(57.3294574165103,21.7649815412284,8.39819969137725));
#40303=CARTESIAN_POINT('Ctrl Pts',(57.3535917367447,21.6871531939148,8.39398425077595));
#40304=CARTESIAN_POINT('Ctrl Pts',(57.3737946118408,21.608316850659,8.38976881017466));
#40305=CARTESIAN_POINT('Ctrl Pts',(57.3939970213169,21.5294823243612,8.38555346672753));
#40306=CARTESIAN_POINT('Ctrl Pts',(57.4102680514289,21.4496402991265,8.3813381232804));
#40307=CARTESIAN_POINT('Ctrl Pts',(57.4225254210937,21.3692165139245,8.37712277983327));
#40308=CARTESIAN_POINT('Ctrl Pts',(57.4348877091442,21.2881043319507,8.37287135466214));
#40309=CARTESIAN_POINT('Ctrl Pts',(57.4431672060169,21.2064008553631,8.36861992949101));
#40310=CARTESIAN_POINT('Ctrl Pts',(57.4473327865741,21.1245491138444,8.36436850431988));
#40311=CARTESIAN_POINT('Ctrl Pts',(57.4514690349426,21.0432737363395,8.36014701581754));
#40312=CARTESIAN_POINT('Ctrl Pts',(57.4515491806293,20.9618526451025,8.35592552731521));
#40313=CARTESIAN_POINT('Ctrl Pts',(57.4475951901096,20.8807186714009,8.35170403881287));
#40314=CARTESIAN_POINT('Ctrl Pts',(57.4435991400281,20.7987216558253,8.34743764530734));
#40315=CARTESIAN_POINT('Ctrl Pts',(57.4354826687089,20.7170183872165,8.34317125180181));
#40316=CARTESIAN_POINT('Ctrl Pts',(57.4233218554622,20.6360474827134,8.33890485829629));
#40317=CARTESIAN_POINT('Ctrl Pts',(57.4111610422155,20.5550765782103,8.33463846479076));
#40318=CARTESIAN_POINT('Ctrl Pts',(57.3949560460808,20.4748384987183,8.33037207128523));
#40319=CARTESIAN_POINT('Ctrl Pts',(57.3748347618231,20.395756585442,8.3261056777797));
#40320=CARTESIAN_POINT('Ctrl Pts',(57.3548751534193,20.3173101005858,8.32187356502907));
#40321=CARTESIAN_POINT('Ctrl Pts',(57.3309870960226,20.2397068125228,8.31764145227843));
#40322=CARTESIAN_POINT('Ctrl Pts',(57.3032583570211,20.1633691430432,8.31340933952779));
#40323=CARTESIAN_POINT('Ctrl Pts',(57.2755693942215,20.0871409780941,8.30918329763998));
#40324=CARTESIAN_POINT('Ctrl Pts',(57.2440508492727,20.0121752590847,8.30495725575217));
#40325=CARTESIAN_POINT('Ctrl Pts',(57.2088409242349,19.9388817118601,8.30073121386437));
#40326=CARTESIAN_POINT('Ctrl Pts',(57.1735498261391,19.8654191934901,8.29649542924796));
#40327=CARTESIAN_POINT('Ctrl Pts',(57.1345504327932,19.7936370202747,8.29225964463156));
#40328=CARTESIAN_POINT('Ctrl Pts',(57.0920314325559,19.7239299646186,8.28802386001516));
#40329=CARTESIAN_POINT('Ctrl Pts',(57.0496866806833,19.6545085774965,8.28380543419222));
#40330=CARTESIAN_POINT('Ctrl Pts',(57.0038513476989,19.5871457373076,8.27958700836927));
#40331=CARTESIAN_POINT('Ctrl Pts',(56.9547580837715,19.5222073609839,8.27536858254633));
#40332=CARTESIAN_POINT('Ctrl Pts',(56.9056811137512,19.4572905375126,8.27115155680627));
#40333=CARTESIAN_POINT('Ctrl Pts',(56.8533486401505,19.394796950326,8.26693453106621));
#40334=CARTESIAN_POINT('Ctrl Pts',(56.7980356953539,19.3350621968875,8.26271750532615));
#40335=CARTESIAN_POINT('Ctrl Pts',(56.7427241819707,19.2753289892919,8.25850058871618));
#40336=CARTESIAN_POINT('Ctrl Pts',(56.6844326672896,19.2183548137282,8.25428367210622));
#40337=CARTESIAN_POINT('Ctrl Pts',(56.6234744229128,19.164439854391,8.25006675549625));
#40338=CARTESIAN_POINT('Ctrl Pts',(56.5620447160188,19.1101079066268,8.24581722446079));
#40339=CARTESIAN_POINT('Ctrl Pts',(56.497907197533,19.0588830315937,8.24156769342533));
#40340=CARTESIAN_POINT('Ctrl Pts',(56.4314165356043,19.0110311838547,8.23731816238987));
#40341=CARTESIAN_POINT('Ctrl Pts',(56.3653407351787,18.9634779026947,8.23309514585707));
#40342=CARTESIAN_POINT('Ctrl Pts',(56.2969414985436,18.9192558818546,8.22887212932427));
#40343=CARTESIAN_POINT('Ctrl Pts',(56.2265945774173,18.8785816082982,8.22464911279147));
#40344=CARTESIAN_POINT('Ctrl Pts',(56.1555851392443,18.8375242703638,8.22038632450468));
#40345=CARTESIAN_POINT('Ctrl Pts',(56.0825915681277,18.800082076633,8.21612353621788));
#40346=CARTESIAN_POINT('Ctrl Pts',(56.0080223597124,18.7664286059497,8.21186074793109));
#40347=CARTESIAN_POINT('Ctrl Pts',(55.9334531512972,18.7327751352665,8.2075979596443));
#40348=CARTESIAN_POINT('Ctrl Pts',(55.8573087757509,18.7029105036105,8.20333517135751));
#40349=CARTESIAN_POINT('Ctrl Pts',(55.7800129604173,18.6769567305836,8.19907238307072));
#40350=CARTESIAN_POINT('Ctrl Pts',(55.7032737514635,18.6511898504121,8.19484029107901));
#40351=CARTESIAN_POINT('Ctrl Pts',(55.6251131108804,18.6291814369582,8.19060819908731));
#40352=CARTESIAN_POINT('Ctrl Pts',(55.5459336251255,18.611086705852,8.1863761070956));
#40353=CARTESIAN_POINT('Ctrl Pts',(55.4668674168221,18.5930178618174,8.18215006970996));
#40354=CARTESIAN_POINT('Ctrl Pts',(55.3867857075107,18.5788516824413,8.17792403232432));
#40355=CARTESIAN_POINT('Ctrl Pts',(55.3061077488199,18.568694117123,8.17369799493868));
#40356=CARTESIAN_POINT('Ctrl Pts',(55.225243648512,18.5585131160898,8.16946220716464));
#40357=CARTESIAN_POINT('Ctrl Pts',(55.1437809937648,18.5523593893563,8.1652264193906));
#40358=CARTESIAN_POINT('Ctrl Pts',(55.0621538300848,18.5502883534167,8.16099063161656));
#40359=CARTESIAN_POINT('Ctrl Pts',(54.980860580322,18.5482257895064,8.15677217126668));
#40360=CARTESIAN_POINT('Ctrl Pts',(54.8994046318173,18.550212601245,8.1525537109168));
#40361=CARTESIAN_POINT('Ctrl Pts',(54.8182196120141,18.5562516208612,8.14833525056691));
#40362=CARTESIAN_POINT('Ctrl Pts',(54.7370612582481,18.5622886569005,8.14411817581281));
#40363=CARTESIAN_POINT('Ctrl Pts',(54.6561741195106,18.572375223175,8.13990110105871));
#40364=CARTESIAN_POINT('Ctrl Pts',(54.5759893141387,18.5864621013385,8.1356840263046));
#40365=CARTESIAN_POINT('Ctrl Pts',(54.4958063114778,18.6005486628014,8.13146704635857));
#40366=CARTESIAN_POINT('Ctrl Pts',(54.4163260682756,18.6186352758291,8.12725006641254));
#40367=CARTESIAN_POINT('Ctrl Pts',(54.3379706678704,18.6406213925273,8.12303308646651));
#40368=CARTESIAN_POINT('Ctrl Pts',(54.2590110176211,18.6627770585802,8.11878358662445));
#40369=CARTESIAN_POINT('Ctrl Pts',(54.1811940994258,18.6888925188956,8.11453408678238));
#40370=CARTESIAN_POINT('Ctrl Pts',(54.1049356366204,18.7188138972438,8.11028458694032));
#40371=CARTESIAN_POINT('Ctrl Pts',(54.0291506767195,18.748549488218,8.106061473029));
#40372=CARTESIAN_POINT('Ctrl Pts',(53.9549052765364,18.782043620346,8.10183835911767));
#40373=CARTESIAN_POINT('Ctrl Pts',(53.8825850493592,18.8190978751708,8.09761524520635));
#40374=CARTESIAN_POINT('Ctrl Pts',(53.8095870391957,18.8564994013535,8.09335255239891));
#40375=CARTESIAN_POINT('Ctrl Pts',(53.7385508952453,18.8975278882631,8.08908985959148));
#40376=CARTESIAN_POINT('Ctrl Pts',(53.6698438676303,18.9419341814414,8.08482716678404));
#40377=CARTESIAN_POINT('Ctrl Pts',(53.6011368400152,18.9863404746197,8.08056447397661));
#40378=CARTESIAN_POINT('Ctrl Pts',(53.5347592808768,19.0341242418496,8.07630178116917));
#40379=CARTESIAN_POINT('Ctrl Pts',(53.471043371659,19.0849955930463,8.07203908836174));
#40380=CARTESIAN_POINT('Ctrl Pts',(53.4086618184736,19.1348015824648,8.06786566603528));
#40381=CARTESIAN_POINT('Ctrl Pts',(53.3485836087252,19.1877652519427,8.06369224370881));
#40382=CARTESIAN_POINT('Ctrl Pts',(53.2911525345021,19.2436428069264,8.05951882138235));
#40383=CARTESIAN_POINT('Ctrl Pts',(53.2328446520373,19.3003734523563,8.05528168283359));
#40384=CARTESIAN_POINT('Ctrl Pts',(53.1772658553803,19.3601074698068,8.05104454428482));
#40385=CARTESIAN_POINT('Ctrl Pts',(53.1247437317707,19.4225450312396,8.04680740573606));
#40386=CARTESIAN_POINT('Ctrl Pts',(53.0731462051794,19.4838834447485,8.04264485757701));
#40387=CARTESIAN_POINT('Ctrl Pts',(53.0244989369235,19.5478306134058,8.03848230941795));
#40388=CARTESIAN_POINT('Ctrl Pts',(52.9790762828846,19.6140643667182,8.0343197612589));
#40389=CARTESIAN_POINT('Ctrl Pts',(52.933681050335,19.680258134957,8.03015972601488));
#40390=CARTESIAN_POINT('Ctrl Pts',(52.8915068401811,19.7487353555256,8.02599969077085));
#40391=CARTESIAN_POINT('Ctrl Pts',(52.8527866955541,19.8191421443668,8.02183965552683));
#40392=CARTESIAN_POINT('Ctrl Pts',(52.8140773001988,19.8895293872661,8.0176807751687));
#40393=CARTESIAN_POINT('Ctrl Pts',(52.778820296948,19.9618447155347,8.01352189481057));
#40394=CARTESIAN_POINT('Ctrl Pts',(52.7472036377794,20.0357081352798,8.00936301445244));
#40395=CARTESIAN_POINT('Ctrl Pts',(52.7145550085216,20.111982462498,8.00506838793241));
#40396=CARTESIAN_POINT('Ctrl Pts',(52.6857887308971,20.1899072118895,8.00077376141238));
#40397=CARTESIAN_POINT('Ctrl Pts',(52.6610579011033,20.2690416509753,7.99647913489234));
#40398=CARTESIAN_POINT('Ctrl Pts',(52.6370856091149,20.3457488984041,7.9923162320792));
#40399=CARTESIAN_POINT('Ctrl Pts',(52.6169048605921,20.4235922076928,7.98815332926606));
#40400=CARTESIAN_POINT('Ctrl Pts',(52.6006037241118,20.5021568909248,7.98399042645292));
#40401=CARTESIAN_POINT('Ctrl Pts',(52.5835288801176,20.5844505218781,7.97962993807944));
#40402=CARTESIAN_POINT('Ctrl Pts',(52.5707111745886,20.6675351198086,7.97526944970597));
#40403=CARTESIAN_POINT('Ctrl Pts',(52.5621909383103,20.7509272621433,7.97090896133249));
#40404=CARTESIAN_POINT('Ctrl Pts',(52.553670702032,20.8343194044779,7.96654847295901));
#40405=CARTESIAN_POINT('Ctrl Pts',(52.5494478931564,20.9180184923135,7.96218798458554));
#40406=CARTESIAN_POINT('Ctrl Pts',(52.5495004857877,21.0015429988506,7.95782749621206));
#40407=CARTESIAN_POINT('Origin',(55.,21.,6.22095488139522));
#40408=CARTESIAN_POINT('',(53.00502528211,20.9993602050363,26.6209548194543));
#40409=CARTESIAN_POINT('Ctrl Pts',(55.164372889159,22.9868942741083,26.4105573801159));
#40410=CARTESIAN_POINT('Ctrl Pts',(54.6931881369,23.0214673262749,26.440680792387));
#40411=CARTESIAN_POINT('Ctrl Pts',(53.5591487190497,22.7217611434947,26.5108130101989));
#40412=CARTESIAN_POINT('Ctrl Pts',(53.0048473617801,21.6235590597841,26.5809452280106));
#40413=CARTESIAN_POINT('Ctrl Pts',(53.0021727671314,20.9993715498994,26.6209540335512));
#40414=CARTESIAN_POINT('',(56.9679107878093,20.6738793264392,26.9999963704729));
#40415=CARTESIAN_POINT('Ctrl Pts',(53.0052501028907,20.9993593108917,26.6209548813952));
#40416=CARTESIAN_POINT('Ctrl Pts',(53.0052617870906,20.9629812046206,26.6232902248096));
#40417=CARTESIAN_POINT('Ctrl Pts',(53.0062685406323,20.9266205928135,26.625625568224));
#40418=CARTESIAN_POINT('Ctrl Pts',(53.008267908903,20.8903148150642,26.6279609116383));
#40419=CARTESIAN_POINT('Ctrl Pts',(53.0120769023975,20.8211487323132,26.6324099708752));
#40420=CARTESIAN_POINT('Ctrl Pts',(53.019500686615,20.7520426805399,26.6368590301121));
#40421=CARTESIAN_POINT('Ctrl Pts',(53.0305342119411,20.6834055083144,26.6413080893491));
#40422=CARTESIAN_POINT('Ctrl Pts',(53.0415511297092,20.614871648112,26.645750451904));
#40423=CARTESIAN_POINT('Ctrl Pts',(53.056166928241,20.5468057473348,26.650192814459));
#40424=CARTESIAN_POINT('Ctrl Pts',(53.0743246331812,20.4796136587808,26.654635177014));
#40425=CARTESIAN_POINT('Ctrl Pts',(53.0924609870389,20.4125005793219,26.6590723159325));
#40426=CARTESIAN_POINT('Ctrl Pts',(53.1141308487093,20.3462597429776,26.663509454851));
#40427=CARTESIAN_POINT('Ctrl Pts',(53.1392261439035,20.2812871095023,26.6679465937695));
#40428=CARTESIAN_POINT('Ctrl Pts',(53.1643056781146,20.216355281786,26.6723809459636));
#40429=CARTESIAN_POINT('Ctrl Pts',(53.1928062020456,20.1526905337474,26.6768152981578));
#40430=CARTESIAN_POINT('Ctrl Pts',(53.2245701952823,20.0906724621897,26.6812496503519));
#40431=CARTESIAN_POINT('Ctrl Pts',(53.256325095761,20.0286721439198,26.6856827331687));
#40432=CARTESIAN_POINT('Ctrl Pts',(53.2913413875328,19.9683180030185,26.6901158159856));
#40433=CARTESIAN_POINT('Ctrl Pts',(53.3294146902202,19.9099668421338,26.6945488988024));
#40434=CARTESIAN_POINT('Ctrl Pts',(53.3674901066498,19.8516124417268,26.6989822277338));
#40435=CARTESIAN_POINT('Ctrl Pts',(53.4086226007211,19.7952616517772,26.7034155566652));
#40436=CARTESIAN_POINT('Ctrl Pts',(53.4525643718967,19.7412424620378,26.7078488855967));
#40437=CARTESIAN_POINT('Ctrl Pts',(53.496553397549,19.6871651806814,26.7122869820791));
#40438=CARTESIAN_POINT('Ctrl Pts',(53.5433574196601,19.6354248854047,26.7167250785616));
#40439=CARTESIAN_POINT('Ctrl Pts',(53.5926888493941,19.5863158457844,26.7211631750441));
#40440=CARTESIAN_POINT('Ctrl Pts',(53.642049523441,19.5371776936869,26.7256039024879));
#40441=CARTESIAN_POINT('Ctrl Pts',(53.6939402212742,19.4906742290622,26.7300446299317));
#40442=CARTESIAN_POINT('Ctrl Pts',(53.7480391520969,19.4470603367105,26.7344853573755));
#40443=CARTESIAN_POINT('Ctrl Pts',(53.8022335380262,19.4033694896264,26.7389339202812));
#40444=CARTESIAN_POINT('Ctrl Pts',(53.8586435366931,19.3625786792873,26.7433824831869));
#40445=CARTESIAN_POINT('Ctrl Pts',(53.9169178693461,19.3248998057554,26.7478310460926));
#40446=CARTESIAN_POINT('Ctrl Pts',(53.9481960140994,19.3046760604662,26.7502187661775));
#40447=CARTESIAN_POINT('Ctrl Pts',(53.9800108165797,19.2853480491996,26.7526064862624));
#40448=CARTESIAN_POINT('Ctrl Pts',(54.0123053327775,19.2669429302991,26.7549942063473));
#40449=CARTESIAN_POINT('Ctrl Pts',(54.0726664323319,19.2325422534952,26.7594570510256));
#40450=CARTESIAN_POINT('Ctrl Pts',(54.1349441451365,19.2012319967431,26.7639198957039));
#40451=CARTESIAN_POINT('Ctrl Pts',(54.1987898135051,19.1732296806777,26.7683827403822));
#40452=CARTESIAN_POINT('Ctrl Pts',(54.2625395383733,19.1452694448394,26.772838878561));
#40453=CARTESIAN_POINT('Ctrl Pts',(54.3278520988388,19.1206074765866,26.7772950167399));
#40454=CARTESIAN_POINT('Ctrl Pts',(54.394353341559,19.0994159614426,26.7817511549187));
#40455=CARTESIAN_POINT('Ctrl Pts',(54.4607754279747,19.0782496705192,26.7862019889647));
#40456=CARTESIAN_POINT('Ctrl Pts',(54.5283829238227,19.0605457743145,26.7906528230106));
#40457=CARTESIAN_POINT('Ctrl Pts',(54.5967824054927,19.0464281088274,26.7951036570565));
#40458=CARTESIAN_POINT('Ctrl Pts',(54.665138176523,19.0323194652243,26.7995516468002));
#40459=CARTESIAN_POINT('Ctrl Pts',(54.7342844529156,19.021792603608,26.8039996365438));
#40460=CARTESIAN_POINT('Ctrl Pts',(54.803814824814,19.014920923606,26.8084476262874));
#40461=CARTESIAN_POINT('Ctrl Pts',(54.8733241422802,19.0080513244115,26.8128942691391));
#40462=CARTESIAN_POINT('Ctrl Pts',(54.9432168394968,19.0048347572317,26.8173409119907));
#40463=CARTESIAN_POINT('Ctrl Pts',(55.0130802840506,19.0052928864946,26.8217875548424));
#40464=CARTESIAN_POINT('Ctrl Pts',(55.0829460631963,19.0057510310665,26.8262343462853));
#40465=CARTESIAN_POINT('Ctrl Pts',(55.1527821003074,19.0098841103251,26.8306811377282));
#40466=CARTESIAN_POINT('Ctrl Pts',(55.2221764182933,19.0176616833511,26.8351279291711));
#40467=CARTESIAN_POINT('Ctrl Pts',(55.2916414064181,19.0254471769416,26.8395792491602));
#40468=CARTESIAN_POINT('Ctrl Pts',(55.3606632921501,19.0368845181813,26.8440305691492));
#40469=CARTESIAN_POINT('Ctrl Pts',(55.428836833603,19.0518915500811,26.8484818891382));
#40470=CARTESIAN_POINT('Ctrl Pts',(55.4970488881697,19.0669070598671,26.8529357238007));
#40471=CARTESIAN_POINT('Ctrl Pts',(55.5644111741879,19.0854961455472,26.8573895584631));
#40472=CARTESIAN_POINT('Ctrl Pts',(55.6305328944282,19.1075265308216,26.8618433931256));
#40473=CARTESIAN_POINT('Ctrl Pts',(55.6967661972704,19.1295940931039,26.8663047437822));
#40474=CARTESIAN_POINT('Ctrl Pts',(55.761754301392,19.1551143698067,26.8707660944387));
#40475=CARTESIAN_POINT('Ctrl Pts',(55.8251264421699,19.1839069635803,26.8752274450953));
#40476=CARTESIAN_POINT('Ctrl Pts',(55.857324023637,19.1985356611799,26.8774941304156));
#40477=CARTESIAN_POINT('Ctrl Pts',(55.8891048586513,19.2140083261596,26.8797608157359));
#40478=CARTESIAN_POINT('Ctrl Pts',(55.9204230327013,19.2302969166064,26.8820275010562));
#40479=CARTESIAN_POINT('Ctrl Pts',(55.9813755574437,19.2619983405348,26.8864390032354));
#40480=CARTESIAN_POINT('Ctrl Pts',(56.0408183362336,19.29692023275,26.8908505054146));
#40481=CARTESIAN_POINT('Ctrl Pts',(56.0983850698236,19.3348940571578,26.8952620075938));
#40482=CARTESIAN_POINT('Ctrl Pts',(56.1558553852743,19.3728042794595,26.8996661209773));
#40483=CARTESIAN_POINT('Ctrl Pts',(56.21145548081,19.4137560119269,26.9040702343608));
#40484=CARTESIAN_POINT('Ctrl Pts',(56.2648431341122,19.4575346329369,26.9084743477443));
#40485=CARTESIAN_POINT('Ctrl Pts',(56.3181807935537,19.5012722582831,26.912874336979));
#40486=CARTESIAN_POINT('Ctrl Pts',(56.3693097326684,19.5478312101843,26.9172743262136));
#40487=CARTESIAN_POINT('Ctrl Pts',(56.4179174630016,19.5969541594747,26.9216743154482));
#40488=CARTESIAN_POINT('Ctrl Pts',(56.4664969640683,19.6460485802819,26.9260717493595));
#40489=CARTESIAN_POINT('Ctrl Pts',(56.5125578089706,19.6977036912373,26.9304691832708));
#40490=CARTESIAN_POINT('Ctrl Pts',(56.5558227743796,19.7516238318432,26.9348666171821));
#40491=CARTESIAN_POINT('Ctrl Pts',(56.5990779999195,19.8055318338721,26.9392630611369));
#40492=CARTESIAN_POINT('Ctrl Pts',(56.6395382830616,19.8617034634036,26.9436595050918));
#40493=CARTESIAN_POINT('Ctrl Pts',(56.6769665367608,19.9198098329069,26.9480559490466));
#40494=CARTESIAN_POINT('Ctrl Pts',(56.7144248914634,19.9779629334183,26.9524559287629));
#40495=CARTESIAN_POINT('Ctrl Pts',(56.7488460713666,20.0380534629174,26.9568559084791));
#40496=CARTESIAN_POINT('Ctrl Pts',(56.7800368660057,20.0997243099135,26.9612558881954));
#40497=CARTESIAN_POINT('Ctrl Pts',(56.8112391841974,20.1614179414284,26.9656574935001));
#40498=CARTESIAN_POINT('Ctrl Pts',(56.8392085358469,20.2246925961809,26.9700590988049));
#40499=CARTESIAN_POINT('Ctrl Pts',(56.8637994165494,20.2891699940422,26.9744607041097));
#40500=CARTESIAN_POINT('Ctrl Pts',(56.8884337482449,20.3537613205989,26.9788700868553));
#40501=CARTESIAN_POINT('Ctrl Pts',(56.9096775275357,20.4195591594962,26.983279469601));
#40502=CARTESIAN_POINT('Ctrl Pts',(56.9274350256771,20.4861694984793,26.9876888523466));
#40503=CARTESIAN_POINT('Ctrl Pts',(56.9439566677346,20.5481440046422,26.9917913583887));
#40504=CARTESIAN_POINT('Ctrl Pts',(56.9574608765223,20.6108214008906,26.9958938644308));
#40505=CARTESIAN_POINT('Ctrl Pts',(56.9679107878093,20.6738793264392,26.9999963704729));
#40506=CARTESIAN_POINT('',(55.3268144232807,19.0322043055145,27.));
#40507=CARTESIAN_POINT('Origin',(55.,21.,27.));
#40508=CARTESIAN_POINT('',(53.0052507551611,21.0017357173056,26.7790451185624));
#40509=CARTESIAN_POINT('Ctrl Pts',(53.0052507551605,21.0017357166396,26.7790451186048));
#40510=CARTESIAN_POINT('Ctrl Pts',(53.0051914603514,20.9335919464819,26.7833890309428));
#40511=CARTESIAN_POINT('Ctrl Pts',(53.0086282717321,20.8653545643158,26.7877329432809));
#40512=CARTESIAN_POINT('Ctrl Pts',(53.015563321049,20.7974200658161,26.7920768556189));
#40513=CARTESIAN_POINT('Ctrl Pts',(53.022494410904,20.7295243534951,26.7964182878656));
#40514=CARTESIAN_POINT('Ctrl Pts',(53.0329197306783,20.6619316909371,26.8007597201123));
#40515=CARTESIAN_POINT('Ctrl Pts',(53.0467893877479,20.5950359686516,26.8051011523591));
#40516=CARTESIAN_POINT('Ctrl Pts',(53.0606562797094,20.5281535829544,26.8094417190812));
#40517=CARTESIAN_POINT('Ctrl Pts',(53.0779660429013,20.4619683635367,26.8137822858032));
#40518=CARTESIAN_POINT('Ctrl Pts',(53.0986176020176,20.3968644106482,26.8181228525253));
#40519=CARTESIAN_POINT('Ctrl Pts',(53.1192727174921,20.3317492463555,26.8224641667266));
#40520=CARTESIAN_POINT('Ctrl Pts',(53.1432706110484,20.2677162048407,26.8268054809278));
#40521=CARTESIAN_POINT('Ctrl Pts',(53.1704608818346,20.2051326037618,26.8311467951291));
#40522=CARTESIAN_POINT('Ctrl Pts',(53.1976845321881,20.1424721732336,26.8354934388539));
#40523=CARTESIAN_POINT('Ctrl Pts',(53.228108166454,20.0812652000635,26.8398400825788));
#40524=CARTESIAN_POINT('Ctrl Pts',(53.2615344726562,20.0218562617195,26.8441867263036));
#40525=CARTESIAN_POINT('Ctrl Pts',(53.294985710061,19.9624030128775,26.8485366119977));
#40526=CARTESIAN_POINT('Ctrl Pts',(53.3314437909819,19.904750892004,26.8528864976917));
#40527=CARTESIAN_POINT('Ctrl Pts',(53.3706686726283,19.8492146211629,26.8572363833858));
#40528=CARTESIAN_POINT('Ctrl Pts',(53.4099641060601,19.7935784600763,26.8615940929964));
#40529=CARTESIAN_POINT('Ctrl Pts',(53.4520359378455,19.7400661293411,26.865951802607));
#40530=CARTESIAN_POINT('Ctrl Pts',(53.4966054601351,19.6889575064078,26.8703095122176));
#40531=CARTESIAN_POINT('Ctrl Pts',(53.5056644870474,19.678569367455,26.8711952432421));
#40532=CARTESIAN_POINT('Ctrl Pts',(53.5148265887909,19.6682804025268,26.8720809742666));
#40533=CARTESIAN_POINT('Ctrl Pts',(53.5240892587333,19.6580927579323,26.8729667052911));
#40534=CARTESIAN_POINT('Ctrl Pts',(53.5719500758757,19.6054525366921,26.877543335017));
#40535=CARTESIAN_POINT('Ctrl Pts',(53.6227079385196,19.5552903614172,26.882119964743));
#40536=CARTESIAN_POINT('Ctrl Pts',(53.6760827272401,19.5079307598546,26.8866965944689));
#40537=CARTESIAN_POINT('Ctrl Pts',(53.731140940504,19.4590774509155,26.8914175696994));
#40538=CARTESIAN_POINT('Ctrl Pts',(53.7889836636027,19.4132068877389,26.8961385449298));
#40539=CARTESIAN_POINT('Ctrl Pts',(53.8492595652905,19.3706369298328,26.9008595201603));
#40540=CARTESIAN_POINT('Ctrl Pts',(53.9074978653635,19.3295060315267,26.9054209048001));
#40541=CARTESIAN_POINT('Ctrl Pts',(53.9680070691629,19.2914564589498,26.9099822894399));
#40542=CARTESIAN_POINT('Ctrl Pts',(54.0304355126644,19.2567351700336,26.9145436740797));
#40543=CARTESIAN_POINT('Ctrl Pts',(54.0928049320613,19.22204670899,26.9191007460756));
#40544=CARTESIAN_POINT('Ctrl Pts',(54.1570895870498,19.1906804991255,26.9236578180716));
#40545=CARTESIAN_POINT('Ctrl Pts',(54.2229100653257,19.1628394746436,26.9282148900675));
#40546=CARTESIAN_POINT('Ctrl Pts',(54.2886860851091,19.135017255403,26.9327688839857));
#40547=CARTESIAN_POINT('Ctrl Pts',(54.3559954457556,19.1107156654368,26.9373228779038));
#40548=CARTESIAN_POINT('Ctrl Pts',(54.424436672141,19.0900904686023,26.941876871822));
#40549=CARTESIAN_POINT('Ctrl Pts',(54.4928501330044,19.0694736390836,26.9464290182569));
#40550=CARTESIAN_POINT('Ctrl Pts',(54.5623941089844,19.0525303673778,26.9509811646918));
#40551=CARTESIAN_POINT('Ctrl Pts',(54.6326511025143,19.03936684971,26.9555333111268));
#40552=CARTESIAN_POINT('Ctrl Pts',(54.7029182418346,19.0262014311028,26.9600861149357));
#40553=CARTESIAN_POINT('Ctrl Pts',(54.7738981562464,19.016816947517,26.9646389187447));
#40554=CARTESIAN_POINT('Ctrl Pts',(54.8451632610788,19.0112684578405,26.9691917225537));
#40555=CARTESIAN_POINT('Ctrl Pts',(54.916433668482,19.0057195553215,26.9737448651198));
#40556=CARTESIAN_POINT('Ctrl Pts',(54.9879888521485,19.0040072420144,26.9782980076859));
#40557=CARTESIAN_POINT('Ctrl Pts',(55.0593980229147,19.0061345488289,26.9828511502521));
#40558=CARTESIAN_POINT('Ctrl Pts',(55.1308564692507,19.0082633235817,26.9874074346933));
#40559=CARTESIAN_POINT('Ctrl Pts',(55.2021682448793,19.0142369843338,26.9919637191345));
#40560=CARTESIAN_POINT('Ctrl Pts',(55.2729054141899,19.0240065290073,26.9965200035757));
#40561=CARTESIAN_POINT('Ctrl Pts',(55.2909146129457,19.0264937881596,26.9976800023838));
#40562=CARTESIAN_POINT('Ctrl Pts',(55.3088866054585,19.0292268269792,26.9988400011919));
#40563=CARTESIAN_POINT('Ctrl Pts',(55.3268144232807,19.0322043055145,27.));
#40564=CARTESIAN_POINT('Ctrl Pts',(55.1644483516311,22.987959834138,26.5685072087751));
#40565=CARTESIAN_POINT('Ctrl Pts',(55.0947777969994,22.993723133612,26.5729580929947));
#40566=CARTESIAN_POINT('Ctrl Pts',(55.0248300995882,22.9958174035433,26.5774089772144));
#40567=CARTESIAN_POINT('Ctrl Pts',(54.9550189243188,22.9942427799369,26.581859861434));
#40568=CARTESIAN_POINT('Ctrl Pts',(54.8851738235987,22.9926673911262,26.5863129086061));
#40569=CARTESIAN_POINT('Ctrl Pts',(54.8154658639627,22.9874195932691,26.5907659557782));
#40570=CARTESIAN_POINT('Ctrl Pts',(54.7463045870801,22.9785515408913,26.5952190029503));
#40571=CARTESIAN_POINT('Ctrl Pts',(54.6770210913026,22.9696678172649,26.5996799193598));
#40572=CARTESIAN_POINT('Ctrl Pts',(54.6082866887087,22.957151146555,26.6041408357693));
#40573=CARTESIAN_POINT('Ctrl Pts',(54.5405011077653,22.9411049251741,26.6086017521787));
#40574=CARTESIAN_POINT('Ctrl Pts',(54.4883383903836,22.9287569523561,26.6120345400769));
#40575=CARTESIAN_POINT('Ctrl Pts',(54.4367373486985,22.9143199493095,26.615467327975));
#40576=CARTESIAN_POINT('Ctrl Pts',(54.3858726940112,22.8978606941867,26.6189001158731));
#40577=CARTESIAN_POINT('Ctrl Pts',(54.3198027005323,22.8764811549897,26.6233590918642));
#40578=CARTESIAN_POINT('Ctrl Pts',(54.2547231915789,22.8516062006253,26.6278180678553));
#40579=CARTESIAN_POINT('Ctrl Pts',(54.1910294196137,22.8233469671375,26.6322770438463));
#40580=CARTESIAN_POINT('Ctrl Pts',(54.1274296624664,22.7951294455252,26.6367294381921));
#40581=CARTESIAN_POINT('Ctrl Pts',(54.0652120250352,22.7635377567045,26.6411818325378));
#40582=CARTESIAN_POINT('Ctrl Pts',(54.004755403991,22.7287324132482,26.6456342268836));
#40583=CARTESIAN_POINT('Ctrl Pts',(53.9443680865756,22.6939669684259,26.6500815172874));
#40584=CARTESIAN_POINT('Ctrl Pts',(53.885738197043,22.6559954285362,26.6545288076912));
#40585=CARTESIAN_POINT('Ctrl Pts',(53.829221865242,22.6150251148736,26.658976098095));
#40586=CARTESIAN_POINT('Ctrl Pts',(53.7727400807916,22.5740798455786,26.6634206699553));
#40587=CARTESIAN_POINT('Ctrl Pts',(53.7183696852096,22.530139725215,26.6678652418157));
#40588=CARTESIAN_POINT('Ctrl Pts',(53.6664382407234,22.4834556268035,26.6723098136761));
#40589=CARTESIAN_POINT('Ctrl Pts',(53.6145210174744,22.4367843126626,26.6767531684067));
#40590=CARTESIAN_POINT('Ctrl Pts',(53.5650417821479,22.3873708385779,26.6811965231372));
#40591=CARTESIAN_POINT('Ctrl Pts',(53.5182940102893,22.3355054932705,26.6856398778677));
#40592=CARTESIAN_POINT('Ctrl Pts',(53.4715432663981,22.2836368505759,26.6900835150886));
#40593=CARTESIAN_POINT('Ctrl Pts',(53.4275246558122,22.2293163913823,26.6945271523096));
#40594=CARTESIAN_POINT('Ctrl Pts',(53.3864926604128,22.1728689729028,26.6989707895305));
#40595=CARTESIAN_POINT('Ctrl Pts',(53.3454167996535,22.116361209166,26.7034191772331));
#40596=CARTESIAN_POINT('Ctrl Pts',(53.3073342142657,22.0577223434595,26.7078675649358));
#40597=CARTESIAN_POINT('Ctrl Pts',(53.2724565978743,21.9973070521518,26.7123159526384));
#40598=CARTESIAN_POINT('Ctrl Pts',(53.2375583093029,21.9368559523257,26.7167669769281));
#40599=CARTESIAN_POINT('Ctrl Pts',(53.2058689924398,21.8746267662481,26.7212180012178));
#40600=CARTESIAN_POINT('Ctrl Pts',(53.1775535288098,21.8109971776439,26.7256690255075));
#40601=CARTESIAN_POINT('Ctrl Pts',(53.1491888716133,21.7472570428577,26.7301277827364));
#40602=CARTESIAN_POINT('Ctrl Pts',(53.1242099429465,21.6821121046642,26.7345865399653));
#40603=CARTESIAN_POINT('Ctrl Pts',(53.1027325404657,21.6159575874134,26.7390452971942));
#40604=CARTESIAN_POINT('Ctrl Pts',(53.0916727483929,21.5818913074653,26.7413413349902));
#40605=CARTESIAN_POINT('Ctrl Pts',(53.0815406442462,21.5475575227488,26.7436373727861));
#40606=CARTESIAN_POINT('Ctrl Pts',(53.0723467389698,21.5130111770124,26.7459334105821));
#40607=CARTESIAN_POINT('Ctrl Pts',(53.0497110534813,21.4279569815042,26.751586328233));
#40608=CARTESIAN_POINT('Ctrl Pts',(53.0326903197989,21.3413349535193,26.757239245884));
#40609=CARTESIAN_POINT('Ctrl Pts',(53.0214612094316,21.2537948319336,26.762892163535));
#40610=CARTESIAN_POINT('Ctrl Pts',(53.0107656520835,21.1704141935701,26.7682764818774));
#40611=CARTESIAN_POINT('Ctrl Pts',(53.0053242516375,21.0862005322065,26.7736608002199));
#40612=CARTESIAN_POINT('Ctrl Pts',(53.0052507551611,21.0017357173056,26.7790451185623));
#40613=CARTESIAN_POINT('Origin',(55.,21.,27.));
#40614=CARTESIAN_POINT('',(52.6675979604224,21.7515656829407,27.));
#40615=CARTESIAN_POINT('',(52.5495,21.,27.));
#40616=CARTESIAN_POINT('Origin',(55.,21.,27.));
#40617=CARTESIAN_POINT('Ctrl Pts',(52.6675979604224,21.7515656829407,27.));
#40618=CARTESIAN_POINT('Ctrl Pts',(52.6581593165275,21.7103708819833,27.));
#40619=CARTESIAN_POINT('Ctrl Pts',(52.6498806799008,21.6689484082415,27.));
#40620=CARTESIAN_POINT('Ctrl Pts',(52.64279639573,21.6273284827364,27.));
#40621=CARTESIAN_POINT('Ctrl Pts',(52.6284952714311,21.5433098700432,27.));
#40622=CARTESIAN_POINT('Ctrl Pts',(52.6190581654961,21.4584860602675,27.));
#40623=CARTESIAN_POINT('Ctrl Pts',(52.6143486107364,21.3732318851031,27.));
#40624=CARTESIAN_POINT('Ctrl Pts',(52.611968832347,21.3301522196133,27.));
#40625=CARTESIAN_POINT('Ctrl Pts',(52.6107970049565,21.2869627536936,27.));
#40626=CARTESIAN_POINT('Ctrl Pts',(52.6108203452642,21.2437130426133,27.));
#40627=CARTESIAN_POINT('Ctrl Pts',(52.6108328628886,21.2205178196194,27.));
#40628=CARTESIAN_POINT('Ctrl Pts',(52.6111891968172,21.1973052874763,27.));
#40629=CARTESIAN_POINT('Ctrl Pts',(52.6118877304625,21.1740832515286,27.));
#40630=CARTESIAN_POINT('Ctrl Pts',(52.6123409031142,21.1590179906353,27.));
#40631=CARTESIAN_POINT('Ctrl Pts',(52.6129380504501,21.143952266255,27.));
#40632=CARTESIAN_POINT('Ctrl Pts',(52.6136780136879,21.128896584471,27.));
#40633=CARTESIAN_POINT('Ctrl Pts',(52.6178472913967,21.0440662641901,27.));
#40634=CARTESIAN_POINT('Ctrl Pts',(52.6265485898479,20.9594741460822,27.));
#40635=CARTESIAN_POINT('Ctrl Pts',(52.6396478697088,20.8754925672425,27.));
#40636=CARTESIAN_POINT('Ctrl Pts',(52.6498009700148,20.8103994168655,27.));
#40637=CARTESIAN_POINT('Ctrl Pts',(52.662597356556,20.7456730539443,27.));
#40638=CARTESIAN_POINT('Ctrl Pts',(52.6779943778682,20.6814954047314,27.));
#40639=CARTESIAN_POINT('Ctrl Pts',(52.6852626539292,20.6511998779559,27.));
#40640=CARTESIAN_POINT('Ctrl Pts',(52.6931106853611,20.6210267642035,27.));
#40641=CARTESIAN_POINT('Ctrl Pts',(52.701535187251,20.59099607487,27.));
#40642=CARTESIAN_POINT('Ctrl Pts',(52.7053028526838,20.5775655371831,27.));
#40643=CARTESIAN_POINT('Ctrl Pts',(52.7091858289863,20.5641634945839,27.));
#40644=CARTESIAN_POINT('Ctrl Pts',(52.7131838689533,20.5507917806399,27.));
#40645=CARTESIAN_POINT('Ctrl Pts',(52.7171931368534,20.5373825141172,27.));
#40646=CARTESIAN_POINT('Ctrl Pts',(52.7213152423352,20.524013371772,27.));
#40647=CARTESIAN_POINT('Ctrl Pts',(52.7255492350363,20.5106867826928,27.));
#40648=CARTESIAN_POINT('Ctrl Pts',(52.7506876133668,20.4315631606711,27.));
#40649=CARTESIAN_POINT('Ctrl Pts',(52.7797692419591,20.3539281551878,27.));
#40650=CARTESIAN_POINT('Ctrl Pts',(52.8126749747748,20.2781287589336,27.));
#40651=CARTESIAN_POINT('Ctrl Pts',(52.8452016800973,20.2032024644977,27.));
#40652=CARTESIAN_POINT('Ctrl Pts',(52.8814654159397,20.1300689107429,27.));
#40653=CARTESIAN_POINT('Ctrl Pts',(52.921392257506,20.0590922664586,27.));
#40654=CARTESIAN_POINT('Ctrl Pts',(52.9601079309623,19.9902686762288,27.));
#40655=CARTESIAN_POINT('Ctrl Pts',(53.0022683739052,19.9234725558841,27.));
#40656=CARTESIAN_POINT('Ctrl Pts',(53.0478373127237,19.8590733051686,27.));
#40657=CARTESIAN_POINT('Ctrl Pts',(53.0676678011867,19.8310483251832,27.));
#40658=CARTESIAN_POINT('Ctrl Pts',(53.0881441430014,19.8034777959598,27.));
#40659=CARTESIAN_POINT('Ctrl Pts',(53.1092649010727,19.7763948758004,27.));
#40660=CARTESIAN_POINT('Ctrl Pts',(53.117566242513,19.7657501552517,27.0000000000001));
#40661=CARTESIAN_POINT('Ctrl Pts',(53.1259678411942,19.7551800576066,27.));
#40662=CARTESIAN_POINT('Ctrl Pts',(53.1344588227666,19.7446996216994,27.));
#40663=CARTESIAN_POINT('Ctrl Pts',(53.1836538089366,19.6839781497331,27.));
#40664=CARTESIAN_POINT('Ctrl Pts',(53.235927021935,19.6261583160513,27.));
#40665=CARTESIAN_POINT('Ctrl Pts',(53.2912060581531,19.5715630117008,27.));
#40666=CARTESIAN_POINT('Ctrl Pts',(53.3132549044344,19.5497868818031,27.));
#40667=CARTESIAN_POINT('Ctrl Pts',(53.3357823343684,19.5285241787662,27.));
#40668=CARTESIAN_POINT('Ctrl Pts',(53.3587851728467,19.5077972530674,27.));
#40669=CARTESIAN_POINT('Ctrl Pts',(53.4176110563557,19.4547916330086,27.));
#40670=CARTESIAN_POINT('Ctrl Pts',(53.4795448432047,19.4052865427495,27.));
#40671=CARTESIAN_POINT('Ctrl Pts',(53.54422871254,19.3593757920684,27.));
#40672=CARTESIAN_POINT('Ctrl Pts',(53.6075401759656,19.3144391356428,27.));
#40673=CARTESIAN_POINT('Ctrl Pts',(53.6734872861446,19.2729459319649,27.));
#40674=CARTESIAN_POINT('Ctrl Pts',(53.7417440169708,19.2350307492206,27.));
#40675=CARTESIAN_POINT('Ctrl Pts',(53.7574393241756,19.2263123351727,27.));
#40676=CARTESIAN_POINT('Ctrl Pts',(53.7732620003945,19.2177807068876,27.));
#40677=CARTESIAN_POINT('Ctrl Pts',(53.789178685159,19.2094527983754,27.));
#40678=CARTESIAN_POINT('Ctrl Pts',(53.8580381744901,19.1734242198219,27.));
#40679=CARTESIAN_POINT('Ctrl Pts',(53.9287388139424,19.1411552595462,27.));
#40680=CARTESIAN_POINT('Ctrl Pts',(54.0009311833521,19.1127073066594,27.));
#40681=CARTESIAN_POINT('Ctrl Pts',(54.0728786828169,19.084355846639,27.));
#40682=CARTESIAN_POINT('Ctrl Pts',(54.1463088594656,19.0597994309732,27.));
#40683=CARTESIAN_POINT('Ctrl Pts',(54.2208852843057,19.0391489920333,27.));
#40684=CARTESIAN_POINT('Ctrl Pts',(54.294838653122,19.0186710792021,27.));
#40685=CARTESIAN_POINT('Ctrl Pts',(54.3699201671869,19.0020341080845,27.));
#40686=CARTESIAN_POINT('Ctrl Pts',(54.4457960554792,18.9893965582189,27.));
#40687=CARTESIAN_POINT('Ctrl Pts',(54.4747700166878,18.9845707843424,27.));
#40688=CARTESIAN_POINT('Ctrl Pts',(54.5038596760197,18.9803287228457,27.));
#40689=CARTESIAN_POINT('Ctrl Pts',(54.5330457778138,18.9766811777813,27.));
#40690=CARTESIAN_POINT('Ctrl Pts',(54.5453585497017,18.9751423840552,27.));
#40691=CARTESIAN_POINT('Ctrl Pts',(54.557688672971,18.9737094744325,27.));
#40692=CARTESIAN_POINT('Ctrl Pts',(54.5700200506845,18.9723846440183,27.));
#40693=CARTESIAN_POINT('Ctrl Pts',(54.6447271119773,18.9643584372752,27.));
#40694=CARTESIAN_POINT('Ctrl Pts',(54.7196133883747,18.9602774590628,27.));
#40695=CARTESIAN_POINT('Ctrl Pts',(54.7943672308826,18.9602361966031,27.));
#40696=CARTESIAN_POINT('Ctrl Pts',(54.8670339703188,18.9601960861779,27.));
#40697=CARTESIAN_POINT('Ctrl Pts',(54.9395763781891,18.9639734317702,27.));
#40698=CARTESIAN_POINT('Ctrl Pts',(55.0116978667239,18.9717019486186,27.));
#40699=CARTESIAN_POINT('Ctrl Pts',(55.0828084700766,18.9793221393173,27.));
#40700=CARTESIAN_POINT('Ctrl Pts',(55.1535105815583,18.9907835686913,27.));
#40701=CARTESIAN_POINT('Ctrl Pts',(55.2234985969135,19.0062592360608,27.));
#40702=CARTESIAN_POINT('Ctrl Pts',(55.2581256631984,19.0139159320977,27.));
#40703=CARTESIAN_POINT('Ctrl Pts',(55.2925775330345,19.0225559423173,27.));
#40704=CARTESIAN_POINT('Ctrl Pts',(55.3268144232807,19.0322043055145,27.));
#40705=CARTESIAN_POINT('Ctrl Pts',(56.9711550749276,20.6733990999081,27.));
#40706=CARTESIAN_POINT('Ctrl Pts',(56.9843403290936,20.7192200369488,27.));
#40707=CARTESIAN_POINT('Ctrl Pts',(56.9957486638496,20.7654588673864,27.));
#40708=CARTESIAN_POINT('Ctrl Pts',(57.0053244209566,20.8120332025565,27.));
#40709=CARTESIAN_POINT('Ctrl Pts',(57.0197547200195,20.8822189411518,27.));
#40710=CARTESIAN_POINT('Ctrl Pts',(57.0300261579609,20.9531657218038,27.));
#40711=CARTESIAN_POINT('Ctrl Pts',(57.0363241708791,21.0245726301505,27.));
#40712=CARTESIAN_POINT('Ctrl Pts',(57.0398083736352,21.0640765419541,27.));
#40713=CARTESIAN_POINT('Ctrl Pts',(57.0420756345699,21.1037217059478,27.));
#40714=CARTESIAN_POINT('Ctrl Pts',(57.04315111989,21.1434595266447,27.));
#40715=CARTESIAN_POINT('Ctrl Pts',(57.0435947853274,21.1598524027472,27.));
#40716=CARTESIAN_POINT('Ctrl Pts',(57.0438355858288,21.1762610615222,27.));
#40717=CARTESIAN_POINT('Ctrl Pts',(57.0438750725979,21.1926821425536,27.));
#40718=CARTESIAN_POINT('Ctrl Pts',(57.0439138408907,21.2088044359754,27.));
#40719=CARTESIAN_POINT('Ctrl Pts',(57.043758487098,21.2249300434683,27.));
#40720=CARTESIAN_POINT('Ctrl Pts',(57.0434112528463,21.2410498327371,27.));
#40721=CARTESIAN_POINT('Ctrl Pts',(57.041793511242,21.3161508736899,27.));
#40722=CARTESIAN_POINT('Ctrl Pts',(57.0360151353344,21.391163881607,27.));
#40723=CARTESIAN_POINT('Ctrl Pts',(57.0262731102432,21.4657603741072,27.));
#40724=CARTESIAN_POINT('Ctrl Pts',(57.0183309920558,21.5265746457048,27.));
#40725=CARTESIAN_POINT('Ctrl Pts',(57.0077535297998,21.5871127615298,27.));
#40726=CARTESIAN_POINT('Ctrl Pts',(56.994622590053,21.6472025604645,27.));
#40727=CARTESIAN_POINT('Ctrl Pts',(56.9891693654016,21.6721576039852,27.));
#40728=CARTESIAN_POINT('Ctrl Pts',(56.9832754808879,21.6970353561712,27.));
#40729=CARTESIAN_POINT('Ctrl Pts',(56.9769457075483,21.7218235275587,27.));
#40730=CARTESIAN_POINT('Ctrl Pts',(56.9732935075575,21.7361259921903,27.));
#40731=CARTESIAN_POINT('Ctrl Pts',(56.96949577252,21.7503997627616,27.));
#40732=CARTESIAN_POINT('Ctrl Pts',(56.9655583005791,21.7646255421325,27.));
#40733=CARTESIAN_POINT('Ctrl Pts',(56.9447075274203,21.8399577611619,27.));
#40734=CARTESIAN_POINT('Ctrl Pts',(56.9199157678371,21.9140520889315,27.));
#40735=CARTESIAN_POINT('Ctrl Pts',(56.8913863602786,21.9865684507146,27.));
#40736=CARTESIAN_POINT('Ctrl Pts',(56.8624995036878,22.0599933803778,27.));
#40737=CARTESIAN_POINT('Ctrl Pts',(56.8297806422816,22.1318015814284,27.));
#40738=CARTESIAN_POINT('Ctrl Pts',(56.7933873856968,22.2016439364836,27.));
#40739=CARTESIAN_POINT('Ctrl Pts',(56.7571899251842,22.2711105389935,27.));
#40740=CARTESIAN_POINT('Ctrl Pts',(56.7173572333979,22.3386334422686,27.));
#40741=CARTESIAN_POINT('Ctrl Pts',(56.6739948998583,22.4038573683784,27.));
#40742=CARTESIAN_POINT('Ctrl Pts',(56.6612704605766,22.4229969722639,27.));
#40743=CARTESIAN_POINT('Ctrl Pts',(56.6482417732324,22.4419384773733,27.));
#40744=CARTESIAN_POINT('Ctrl Pts',(56.6349107419457,22.4606725079749,27.));
#40745=CARTESIAN_POINT('Ctrl Pts',(56.6273072000305,22.4713577268342,27.));
#40746=CARTESIAN_POINT('Ctrl Pts',(56.6196039727324,22.4819772302926,27.));
#40747=CARTESIAN_POINT('Ctrl Pts',(56.611805607223,22.4925235206514,27.));
#40748=CARTESIAN_POINT('Ctrl Pts',(56.5635925023516,22.5577255687555,27.));
#40749=CARTESIAN_POINT('Ctrl Pts',(56.5119013821899,22.6199239206814,27.));
#40750=CARTESIAN_POINT('Ctrl Pts',(56.4569110326642,22.6787619007156,27.));
#40751=CARTESIAN_POINT('Ctrl Pts',(56.4321646798555,22.7052397359183,27.));
#40752=CARTESIAN_POINT('Ctrl Pts',(56.4067494980637,22.7310369552658,27.));
#40753=CARTESIAN_POINT('Ctrl Pts',(56.3806784609636,22.7561201322126,27.));
#40754=CARTESIAN_POINT('Ctrl Pts',(56.3241596085106,22.8104974234369,27.));
#40755=CARTESIAN_POINT('Ctrl Pts',(56.2645614152419,22.861521301469,27.));
#40756=CARTESIAN_POINT('Ctrl Pts',(56.2022367668188,22.9091785543743,27.));
#40757=CARTESIAN_POINT('Ctrl Pts',(56.1399121183956,22.9568358072795,27.));
#40758=CARTESIAN_POINT('Ctrl Pts',(56.0748602656315,23.0011267676018,27.));
#40759=CARTESIAN_POINT('Ctrl Pts',(56.0073956790906,23.0420027201548,27.));
#40760=CARTESIAN_POINT('Ctrl Pts',(55.995921828827,23.0489545830954,27.));
#40761=CARTESIAN_POINT('Ctrl Pts',(55.9843764396863,23.055808551695,27.));
#40762=CARTESIAN_POINT('Ctrl Pts',(55.9727662874617,23.0625611887514,27.));
#40763=CARTESIAN_POINT('Ctrl Pts',(55.9033022392179,23.1029625114202,27.));
#40764=CARTESIAN_POINT('Ctrl Pts',(55.8317582221578,23.1396040058116,27.));
#40765=CARTESIAN_POINT('Ctrl Pts',(55.7585161957843,23.1724925894664,27.));
#40766=CARTESIAN_POINT('Ctrl Pts',(55.6828327620042,23.206477462174,27.));
#40767=CARTESIAN_POINT('Ctrl Pts',(55.6053356039688,23.2364555943728,27.));
#40768=CARTESIAN_POINT('Ctrl Pts',(55.526403821075,23.2623966359773,27.));
#40769=CARTESIAN_POINT('Ctrl Pts',(55.4474720381812,23.2883376775817,27.));
#40770=CARTESIAN_POINT('Ctrl Pts',(55.3671047185148,23.3102419887007,27.));
#40771=CARTESIAN_POINT('Ctrl Pts',(55.2856513531316,23.3280353685059,27.));
#40772=CARTESIAN_POINT('Ctrl Pts',(55.2359251484301,23.3388979920741,27.));
#40773=CARTESIAN_POINT('Ctrl Pts',(55.1857936600202,23.3482276198764,27.));
#40774=CARTESIAN_POINT('Ctrl Pts',(55.1353332201589,23.355998440921,27.));
#40775=CARTESIAN_POINT('Ctrl Pts',(55.1216156589962,23.3581109217724,27.));
#40776=CARTESIAN_POINT('Ctrl Pts',(55.1078812076943,23.3601069820185,27.));
#40777=CARTESIAN_POINT('Ctrl Pts',(55.0941380647184,23.3619855976698,27.));
#40778=CARTESIAN_POINT('Ctrl Pts',(55.0090469708069,23.3736171044575,27.));
#40779=CARTESIAN_POINT('Ctrl Pts',(54.9235470750792,23.3807620486719,27.));
#40780=CARTESIAN_POINT('Ctrl Pts',(54.8380287552821,23.3833903704909,27.));
#40781=CARTESIAN_POINT('Ctrl Pts',(54.7524215968147,23.3860214226794,27.));
#40782=CARTESIAN_POINT('Ctrl Pts',(54.666795005057,23.3841268154452,27.));
#40783=CARTESIAN_POINT('Ctrl Pts',(54.5815186695155,23.377629130775,27.));
#40784=CARTESIAN_POINT('Ctrl Pts',(54.4980822478155,23.3712716395111,27.));
#40785=CARTESIAN_POINT('Ctrl Pts',(54.4149801838723,23.3605077155167,27.));
#40786=CARTESIAN_POINT('Ctrl Pts',(54.3325520387133,23.3452161635882,27.));
#40787=CARTESIAN_POINT('Ctrl Pts',(54.2891983220411,23.3371734542866,27.));
#40788=CARTESIAN_POINT('Ctrl Pts',(54.2460310044596,23.3278774277892,27.));
#40789=CARTESIAN_POINT('Ctrl Pts',(54.203100055607,23.3173046257725,27.));
#40790=CARTESIAN_POINT('Origin',(55.,21.,27.));
#40791=CARTESIAN_POINT('Ctrl Pts',(54.1264352462825,22.7892995080061,7.43479847215643));
#40792=CARTESIAN_POINT('Ctrl Pts',(53.5313636363274,22.4987759919214,7.47714290372609));
#40793=CARTESIAN_POINT('Ctrl Pts',(52.6642537907918,21.2821184890334,7.56183176686541));
#40794=CARTESIAN_POINT('Ctrl Pts',(53.4976472728867,19.1863830377497,7.68886506157439));
#40795=CARTESIAN_POINT('Ctrl Pts',(55.7087280813971,18.7562692203022,7.81589835628338));
#40796=CARTESIAN_POINT('Ctrl Pts',(57.2698128240574,20.3778916813317,7.94293165099235));
#40797=CARTESIAN_POINT('Ctrl Pts',(56.7533256858317,22.5703705433843,8.06996494570134));
#40798=CARTESIAN_POINT('Ctrl Pts',(54.6312789516365,23.3244325802832,8.19699824041032));
#40799=CARTESIAN_POINT('Ctrl Pts',(52.8469659787634,21.9506800446467,8.32403153511931));
#40800=CARTESIAN_POINT('Ctrl Pts',(53.0338008043911,19.706355415659,8.45106482982828));
#40801=CARTESIAN_POINT('Ctrl Pts',(55.0208406626359,18.6465226847945,8.57809812453727));
#40802=CARTESIAN_POINT('Ctrl Pts',(56.9887798196956,19.7413863016522,8.70513141924624));
#40803=CARTESIAN_POINT('Ctrl Pts',(57.1358892072027,21.9886045058084,8.83216471395522));
#40804=CARTESIAN_POINT('Ctrl Pts',(55.3274665165508,23.3306879153509,8.95919800866422));
#40805=CARTESIAN_POINT('Ctrl Pts',(53.2192324453698,22.5389012348763,9.08623130337319));
#40806=CARTESIAN_POINT('Ctrl Pts',(52.7413900137877,20.3381607386649,9.21326459808217));
#40807=CARTESIAN_POINT('Ctrl Pts',(54.3314329386002,18.7433729270463,9.34029789279115));
#40808=CARTESIAN_POINT('Ctrl Pts',(56.5335863102332,19.2146535088455,9.46733118750014));
#40809=CARTESIAN_POINT('Ctrl Pts',(57.3316552158584,21.3205197731518,9.59436448220912));
#40810=CARTESIAN_POINT('Ctrl Pts',(55.9949623455254,23.1329319227209,9.72139777691809));
#40811=CARTESIAN_POINT('Ctrl Pts',(53.7473254531283,22.9925248642322,9.84843107162709));
#40812=CARTESIAN_POINT('Ctrl Pts',(52.6465826422626,21.0278490069435,9.97546436633607));
#40813=CARTESIAN_POINT('Ctrl Pts',(53.7005259934764,19.0376758430876,10.102497661045));
#40814=CARTESIAN_POINT('Ctrl Pts',(55.9442109855123,18.8441209605304,10.229530955754));
#40815=CARTESIAN_POINT('Ctrl Pts',(57.32341763991,20.6243947780001,10.356564250463));
#40816=CARTESIAN_POINT('Ctrl Pts',(56.5754045744307,22.7485563288281,10.483597545172));
#40817=CARTESIAN_POINT('Ctrl Pts',(54.3850198856334,23.2718160732959,10.610630839881));
#40818=CARTESIAN_POINT('Ctrl Pts',(52.7576841304891,21.7151002393188,10.7376641345899));
#40819=CARTESIAN_POINT('Ctrl Pts',(53.183314854842,19.5036698579907,10.864697429299));
#40820=CARTESIAN_POINT('Ctrl Pts',(55.2722231561246,18.6622140037448,10.9917307240079));
#40821=CARTESIAN_POINT('Ctrl Pts',(57.1118958247853,19.9611329073913,11.1187640187169));
#40822=CARTESIAN_POINT('Ctrl Pts',(57.0180089111301,22.2111931495074,11.2457973134259));
#40823=CARTESIAN_POINT('Ctrl Pts',(55.0765211729318,23.3523378415888,11.3728306081349));
#40824=CARTESIAN_POINT('Ctrl Pts',(53.0649739907733,22.3397847418404,11.4998639028438));
#40825=CARTESIAN_POINT('Ctrl Pts',(52.8250521123875,20.1005832461981,11.6268971975528));
#40826=CARTESIAN_POINT('Ctrl Pts',(54.5764175312761,18.6848484492269,11.7539304922618));
#40827=CARTESIAN_POINT('Ctrl Pts',(56.7155965589988,19.3887653002727,11.8809637869708));
#40828=CARTESIAN_POINT('Ctrl Pts',(57.2840503042245,21.5678582733624,12.0079970816798));
#40829=CARTESIAN_POINT('Ctrl Pts',(55.7613273444601,23.2270450119906,12.1350303763887));
#40830=CARTESIAN_POINT('Ctrl Pts',(53.5415663183002,22.8472466015499,12.2620636710978));
#40831=CARTESIAN_POINT('Ctrl Pts',(52.6570834755071,20.7761898793339,12.3890969658067));
#40832=CARTESIAN_POINT('Ctrl Pts',(53.9176726780599,18.9100439289218,12.5161302605157));
#40833=CARTESIAN_POINT('Ctrl Pts',(56.1691935070438,18.957370480498,12.6431635552247));
#40834=CARTESIAN_POINT('Ctrl Pts',(57.3502518243073,20.8748394103778,12.7701968499337));
#40835=CARTESIAN_POINT('Ctrl Pts',(56.3795222160764,22.9068999098553,12.8972301446426));
#40836=CARTESIAN_POINT('Ctrl Pts',(54.1457623160259,23.1930861337697,13.0242634393516));
#40837=CARTESIAN_POINT('Ctrl Pts',(52.6941051314662,21.4713784743956,13.1512967340606));
#40838=CARTESIAN_POINT('Ctrl Pts',(53.3536245809391,19.3180972708369,13.2783300287696));
#40839=CARTESIAN_POINT('Ctrl Pts',(55.5204934603439,18.7046927507208,13.4053633234786));
#40840=CARTESIAN_POINT('Ctrl Pts',(57.2108212594767,20.1927713028513,13.5323966181875));
#40841=CARTESIAN_POINT('Ctrl Pts',(56.8770176687869,22.4199131952045,13.6594299128965));
#40842=CARTESIAN_POINT('Ctrl Pts',(54.8246986773802,23.3470445792831,13.7864632076055));
#40843=CARTESIAN_POINT('Ctrl Pts',(52.9328779208585,22.1253244513384,13.9134965023145));
#40844=CARTESIAN_POINT('Ctrl Pts',(52.9336238605588,19.8733064031411,14.0405297970235));
#40845=CARTESIAN_POINT('Ctrl Pts',(54.8262535466699,18.6528398050389,14.1675630917325));
#40846=CARTESIAN_POINT('Ctrl Pts',(56.8779578972515,19.5813305716253,14.2945963864414));
#40847=CARTESIAN_POINT('Ctrl Pts',(57.2102860149976,21.8086931078973,14.4216296811504));
#40848=CARTESIAN_POINT('Ctrl Pts',(55.5189727893898,23.2956515534217,14.5486629758594));
#40849=CARTESIAN_POINT('Ctrl Pts',(53.3525107434218,22.6808116968638,14.6756962705684));
#40850=CARTESIAN_POINT('Ctrl Pts',(52.6944179083708,20.5270940583868,14.8027295652774));
#40851=CARTESIAN_POINT('Ctrl Pts',(54.1472153424787,18.8063484463683,14.9297628599863));
#40852=CARTESIAN_POINT('Ctrl Pts',(56.3807851645167,19.0940143913699,15.0567961546953));
#40853=CARTESIAN_POINT('Ctrl Pts',(57.350168394301,21.1267175176638,15.1838294494043));
#40854=CARTESIAN_POINT('Ctrl Pts',(56.1678400834611,23.0434036190425,15.3108627441133));
#40855=CARTESIAN_POINT('Ctrl Pts',(53.9162883964239,23.0892386103863,15.4378960388223));
#40856=CARTESIAN_POINT('Ctrl Pts',(52.6569357236264,21.222257975417,15.5649293335312));
#40857=CARTESIAN_POINT('Ctrl Pts',(53.5427903713442,19.1517876450454,15.6919626282402));
#40858=CARTESIAN_POINT('Ctrl Pts',(55.762802512921,18.7734598280885,15.8189959229492));
#40859=CARTESIAN_POINT('Ctrl Pts',(57.2844259882859,20.4336549506721,15.9460292176582));
#40860=CARTESIAN_POINT('Ctrl Pts',(56.7145287987417,22.6123708658803,16.0730625123672));
#40861=CARTESIAN_POINT('Ctrl Pts',(54.5748839213591,23.3148704349348,16.2000958070762));
#40862=CARTESIAN_POINT('Ctrl Pts',(52.8244567590706,21.8979757333586,16.3271291017851));
#40863=CARTESIAN_POINT('Ctrl Pts',(53.0658619735541,19.6589336684897,16.4541623964941));
#40864=CARTESIAN_POINT('Ctrl Pts',(55.078079493554,18.647713367053,16.5811956912031));
#40865=CARTESIAN_POINT('Ctrl Pts',(57.0188108392977,19.7901439730331,16.7082289859121));
#40866=CARTESIAN_POINT('Ctrl Pts',(57.1112071500763,22.040265918081,16.8352622806211));
#40867=CARTESIAN_POINT('Ctrl Pts',(55.2706743990552,23.3379658210827,16.9622955753301));
#40868=CARTESIAN_POINT('Ctrl Pts',(53.1823239896862,22.4951263265638,17.089328870039));
#40869=CARTESIAN_POINT('Ctrl Pts',(52.7581583502224,20.2834144655543,17.216362164748));
#40870=CARTESIAN_POINT('Ctrl Pts',(54.3865250151568,18.727777023744,17.343395459457));
#40871=CARTESIAN_POINT('Ctrl Pts',(56.576562583322,19.2524877019822,17.470428754166));
#40872=CARTESIAN_POINT('Ctrl Pts',(57.3231683049537,21.3771443194757,17.597462048875));
#40873=CARTESIAN_POINT('Ctrl Pts',(55.9427825885663,23.1565040694491,17.7244953435839));
#40874=CARTESIAN_POINT('Ctrl Pts',(53.6992263091515,22.9614628765416,17.8515286382929));
#40875=CARTESIAN_POINT('Ctrl Pts',(52.6466016111188,20.970591938755,17.9785619330019));
#40876=CARTESIAN_POINT('Ctrl Pts',(53.7486456956814,19.0066457374772,18.1055952277109));
#40877=CARTESIAN_POINT('Ctrl Pts',(55.9963751296602,18.8677276412595,18.2326285224199));
#40878=CARTESIAN_POINT('Ctrl Pts',(57.3318670105856,20.6810249918929,18.3596618171288));
#40879=CARTESIAN_POINT('Ctrl Pts',(56.5324032985223,22.7863619290425,18.4866951118378));
#40880=CARTESIAN_POINT('Ctrl Pts',(54.3299380524767,23.2561839014885,18.6137284065468));
#40881=CARTESIAN_POINT('Ctrl Pts',(52.7409522613139,21.6603424302529,18.7407617012558));
#40882=CARTESIAN_POINT('Ctrl Pts',(53.2202519180959,19.4599202696571,18.8677949959648));
#40883=CARTESIAN_POINT('Ctrl Pts',(55.3290111899943,18.6695278487583,18.9948282906738));
#40884=CARTESIAN_POINT('Ctrl Pts',(57.1365421855609,20.0128139485519,19.1218615853827));
#40885=CARTESIAN_POINT('Ctrl Pts',(56.9879484673196,22.2599244827116,19.2488948800917));
#40886=CARTESIAN_POINT('Ctrl Pts',(55.019275954014,23.353503186412,19.3759281748007));
#40887=CARTESIAN_POINT('Ctrl Pts',(53.0329552190706,22.2923171594749,19.5029614695097));
#40888=CARTESIAN_POINT('Ctrl Pts',(52.84757477688,20.0479419819511,19.6299947642187));
#40889=CARTESIAN_POINT('Ctrl Pts',(54.6328608640107,18.6752295455939,19.7570280589276));
#40890=CARTESIAN_POINT('Ctrl Pts',(56.7542835096275,19.4309754053223,19.8840613536367));
#40891=CARTESIAN_POINT('Ctrl Pts',(57.2695607903648,21.6232516583953,20.0110946483456));
#40892=CARTESIAN_POINT('Ctrl Pts',(55.7069273321875,23.2449059129194,20.1381279430546));
#40893=CARTESIAN_POINT('Ctrl Pts',(53.4970620829863,22.8112223575412,20.2651612377636));
#40894=CARTESIAN_POINT('Ctrl Pts',(52.6632211513288,20.7192627148797,20.3921945324726));
#40895=CARTESIAN_POINT('Ctrl Pts',(53.9688328770913,18.884333869561,20.5192278271815));
#40896=CARTESIAN_POINT('Ctrl Pts',(56.2185361854212,18.9864165337207,20.6462611218906));
#40897=CARTESIAN_POINT('Ctrl Pts',(57.3526009806992,20.9320482784099,20.7732944165995));
#40898=CARTESIAN_POINT('Ctrl Pts',(56.3327270654876,22.9398936516653,20.9003277113085));
#40899=CARTESIAN_POINT('Ctrl Pts',(54.0926664546051,23.1716571203244,21.0273610060175));
#40900=CARTESIAN_POINT('Ctrl Pts',(52.6833208110228,21.4151461745151,21.1543943007264));
#40901=CARTESIAN_POINT('Ctrl Pts',(53.3950254542771,19.2785455224038,21.2814275954354));
#40902=CARTESIAN_POINT('Ctrl Pts',(55.5761746959756,18.7180334072183,21.4084608901444));
#40903=CARTESIAN_POINT('Ctrl Pts',(57.2298035498787,20.2467902418298,21.5354941848534));
#40904=CARTESIAN_POINT('Ctrl Pts',(56.8419216578993,22.4651530353571,21.6625274795624));
#40905=CARTESIAN_POINT('Ctrl Pts',(54.7676567399891,23.3420856987698,21.7895607742714));
#40906=CARTESIAN_POINT('Ctrl Pts',(52.9061151635912,22.0747069845831,21.9165940689803));
#40907=CARTESIAN_POINT('Ctrl Pts',(52.9616430951332,19.823373492039,22.0436273636893));
#40908=CARTESIAN_POINT('Ctrl Pts',(54.883401585621,18.6493078422263,22.1706606583983));
#40909=CARTESIAN_POINT('Ctrl Pts',(56.911912491998,19.6274332679986,22.2976939531073));
#40910=CARTESIAN_POINT('Ctrl Pts',(57.1899598215212,21.8622208481452,22.4247272478162));
#40911=CARTESIAN_POINT('Ctrl Pts',(55.4629755827127,23.3075966763422,22.5517605425253));
#40912=CARTESIAN_POINT('Ctrl Pts',(53.3121111203556,22.6402377696025,22.6787938372342));
#40913=CARTESIAN_POINT('Ctrl Pts',(52.7066039993849,20.4711487967183,22.8058271319432));
#40914=CARTESIAN_POINT('Ctrl Pts',(54.2008300948515,18.7862528885265,22.9328604266522));
#40915=CARTESIAN_POINT('Ctrl Pts',(56.4267412525533,19.1281671524571,23.0598937213612));
#40916=CARTESIAN_POINT('Ctrl Pts',(57.3463904308638,21.183849821225,23.1869270160701));
#40917=CARTESIAN_POINT('Ctrl Pts',(56.1177870069067,23.071207623113,23.3139603107791));
#40918=CARTESIAN_POINT('Ctrl Pts',(53.8657866175656,23.0622581831875,23.4409936054881));
#40919=CARTESIAN_POINT('Ctrl Pts',(52.6522224656966,21.1651952176771,23.5680269001971));
#40920=CARTESIAN_POINT('Ctrl Pts',(53.5881808872158,19.1168867257354,23.6950601949061));
#40921=CARTESIAN_POINT('Ctrl Pts',(55.8167392291167,18.7926745043891,23.822093489615));
#40922=CARTESIAN_POINT('Ctrl Pts',(57.2975268021679,20.4893931046865,23.9491267843241));
#40923=CARTESIAN_POINT('Ctrl Pts',(56.6747991790829,22.6536010770382,24.076160079033));
#40924=CARTESIAN_POINT('Ctrl Pts',(54.5186985692507,23.3038441246632,24.203193373742));
#40925=CARTESIAN_POINT('Ctrl Pts',(52.8032565359452,21.8447881057192,24.330226668451));
#40926=CARTESIAN_POINT('Ctrl Pts',(53.0990568643523,19.6122810003745,24.45725996316));
#40927=CARTESIAN_POINT('Ctrl Pts',(55.1352777323281,18.6503087883512,24.5842932578689));
#40928=CARTESIAN_POINT('Ctrl Pts',(57.0476441652364,19.8396112597284,24.711326552578));
#40929=CARTESIAN_POINT('Ctrl Pts',(57.0852771298678,22.0913149235079,24.8383598472869));
#40930=CARTESIAN_POINT('Ctrl Pts',(55.2137212298849,23.3438584215582,24.9653931419959));
#40931=CARTESIAN_POINT('Ctrl Pts',(53.1464918908666,22.45046728724,25.0924264367049));
#40932=CARTESIAN_POINT('Ctrl Pts',(52.7762528735532,20.2290920967572,25.2194597314139));
#40933=CARTESIAN_POINT('Ctrl Pts',(54.4419810779207,18.7135256448128,25.3464930261228));
#40934=CARTESIAN_POINT('Ctrl Pts',(56.6186041564239,19.2913569527159,25.4735263208318));
#40935=CARTESIAN_POINT('Ctrl Pts',(57.3133095927893,21.4335438873502,25.6005596155408));
#40936=CARTESIAN_POINT('Ctrl Pts',(55.8900387814265,23.1788034744911,25.7275929102498));
#40937=CARTESIAN_POINT('Ctrl Pts',(53.6519088779192,22.9292330426812,25.8546262049588));
#40938=CARTESIAN_POINT('Ctrl Pts',(52.6479901933195,20.9133659611559,25.9816594996677));
#40939=CARTESIAN_POINT('Ctrl Pts',(53.7975513738378,18.9767685882894,26.1086927943768));
#40940=CARTESIAN_POINT('Ctrl Pts',(56.0478608304085,18.8926486501099,26.2357260890857));
#40941=CARTESIAN_POINT('Ctrl Pts',(57.3391098950668,20.7377415341185,26.3627593837947));
#40942=CARTESIAN_POINT('Ctrl Pts',(56.4881554930549,22.823310792186,26.4897926785037));
#40943=CARTESIAN_POINT('Ctrl Pts',(54.2759180399637,23.2388230435375,26.6168259732127));
#40944=CARTESIAN_POINT('Ctrl Pts',(52.7242447265499,21.6059770109423,26.7438592679217));
#40945=CARTESIAN_POINT('Ctrl Pts',(53.261008001841,19.4150988751331,26.8709101685003));
#40946=CARTESIAN_POINT('Ctrl Pts',(54.6735570889175,18.9270516578725,26.9556166375094));
#40947=CARTESIAN_POINT('Ctrl Pts',(55.3270406347534,19.0358837922465,26.9979786749487));
#40948=CARTESIAN_POINT('Ctrl Pts',(54.0587940262274,22.9278472244179,7.52381308588823));
#40949=CARTESIAN_POINT('Ctrl Pts',(53.4176452713942,22.6148281062624,7.56615751745789));
#40950=CARTESIAN_POINT('Ctrl Pts',(52.4833940174808,21.3039632792647,7.65084638059721));
#40951=CARTESIAN_POINT('Ctrl Pts',(53.3813182074311,19.0459523902024,7.77787967530619));
#40952=CARTESIAN_POINT('Ctrl Pts',(55.7636057901289,18.5825343176886,7.90491297001517));
#40953=CARTESIAN_POINT('Ctrl Pts',(57.4455672922436,20.3297210500167,8.03194626472416));
#40954=CARTESIAN_POINT('Ctrl Pts',(56.8890879038456,22.6919663140939,8.15897955943315));
#40955=CARTESIAN_POINT('Ctrl Pts',(54.6027284160695,23.504416325045,8.28601285414212));
#40956=CARTESIAN_POINT('Ctrl Pts',(52.6802538404854,22.0242923988863,8.4130461488511));
#40957=CARTESIAN_POINT('Ctrl Pts',(52.8815555221769,19.6061868847859,8.54007944356008));
#40958=CARTESIAN_POINT('Ctrl Pts',(55.0224543814147,18.4642899695951,8.66711273826906));
#40959=CARTESIAN_POINT('Ctrl Pts',(57.1427735480971,19.6439302564397,8.79414603297805));
#40960=CARTESIAN_POINT('Ctrl Pts',(57.3012738009179,22.0651533988816,8.92117932768702));
#40961=CARTESIAN_POINT('Ctrl Pts',(55.3528226617163,23.5111560185922,9.04821262239602));
#40962=CARTESIAN_POINT('Ctrl Pts',(53.0813453688628,22.6580602973593,9.17524591710498));
#40963=CARTESIAN_POINT('Ctrl Pts',(52.5665029954577,20.2869136903762,9.30227921181398));
#40964=CARTESIAN_POINT('Ctrl Pts',(54.2796649482718,18.5686394481893,9.42931250652295));
#40965=CARTESIAN_POINT('Ctrl Pts',(56.6523338314015,19.0764118795115,9.55634580123193));
#40966=CARTESIAN_POINT('Ctrl Pts',(57.5121982183976,21.3453380232191,9.68337909594093));
#40967=CARTESIAN_POINT('Ctrl Pts',(56.0720035341421,23.298087530171,9.81041239064989));
#40968=CARTESIAN_POINT('Ctrl Pts',(53.6503292839014,23.1468085761529,9.93744568535889));
#40969=CARTESIAN_POINT('Ctrl Pts',(52.4643545696455,21.0300053906563,10.0644789800679));
#40970=CARTESIAN_POINT('Ctrl Pts',(53.5999060830955,18.8857306100042,10.1915122747768));
#40971=CARTESIAN_POINT('Ctrl Pts',(56.0173224323485,18.6771885289045,10.3185455694858));
#40972=CARTESIAN_POINT('Ctrl Pts',(57.5033227965594,20.5953111921903,10.4455788641948));
#40973=CARTESIAN_POINT('Ctrl Pts',(56.6973901365099,22.8839492495173,10.5726121589038));
#40974=CARTESIAN_POINT('Ctrl Pts',(54.3374012001631,23.4477256555959,10.6996454536128));
#40975=CARTESIAN_POINT('Ctrl Pts',(52.5840587861548,21.770471352271,10.8266787483217));
#40976=CARTESIAN_POINT('Ctrl Pts',(53.0426466340244,19.3878071288916,10.9537120430307));
#40977=CARTESIAN_POINT('Ctrl Pts',(55.2933017382551,18.4811962871516,11.0807453377397));
#40978=CARTESIAN_POINT('Ctrl Pts',(57.2754225806551,19.8806921188636,11.2077786324487));
#40979=CARTESIAN_POINT('Ctrl Pts',(57.174265884926,22.3049773618469,11.3348119271577));
#40980=CARTESIAN_POINT('Ctrl Pts',(55.082446303811,23.5344823259097,11.4618452218667));
#40981=CARTESIAN_POINT('Ctrl Pts',(52.9151424876759,22.4435259632707,11.5888785165756));
#40982=CARTESIAN_POINT('Ctrl Pts',(52.6566431558126,20.0309402731888,11.7159118112846));
#40983=CARTESIAN_POINT('Ctrl Pts',(54.5436190067747,18.5055833462792,11.8429451059936));
#40984=CARTESIAN_POINT('Ctrl Pts',(56.8484373631626,19.2640053664261,11.9699784007026));
#40985=CARTESIAN_POINT('Ctrl Pts',(57.460907198447,21.6118282552844,12.0970116954116));
#40986=CARTESIAN_POINT('Ctrl Pts',(55.8202778804352,23.3994879145773,12.2240449901205));
#40987=CARTESIAN_POINT('Ctrl Pts',(53.4286379598932,22.9902812344603,12.3510782848295));
#40988=CARTESIAN_POINT('Ctrl Pts',(52.4756684956452,20.7588599795662,12.4781115795385));
#40989=CARTESIAN_POINT('Ctrl Pts',(53.8338667091912,18.7482159958377,12.6051448742475));
#40990=CARTESIAN_POINT('Ctrl Pts',(56.2597256341247,18.7992071019601,12.7321781689565));
#40991=CARTESIAN_POINT('Ctrl Pts',(57.5322347856805,20.8651480681519,12.8592114636654));
#40992=CARTESIAN_POINT('Ctrl Pts',(56.4863403602281,23.0545535736237,12.9862447583744));
#40993=CARTESIAN_POINT('Ctrl Pts',(54.079617615344,23.3628995576089,13.1132780530834));
#40994=CARTESIAN_POINT('Ctrl Pts',(52.5155567850928,21.5078779038655,13.2403113477924));
#40995=CARTESIAN_POINT('Ctrl Pts',(53.2261436568976,19.1878654223903,13.3673446425014));
#40996=CARTESIAN_POINT('Ctrl Pts',(55.5607959250878,18.5269642170526,13.4943779372104));
#40997=CARTESIAN_POINT('Ctrl Pts',(57.3820079364554,20.1302665672765,13.6214112319193));
#40998=CARTESIAN_POINT('Ctrl Pts',(57.0223575129614,22.529858863785,13.7484445266283));
#40999=CARTESIAN_POINT('Ctrl Pts',(54.8111248749932,23.5287791996311,13.8754778213373));
#41000=CARTESIAN_POINT('Ctrl Pts',(52.7728180525535,22.2124597421367,14.0025111160463));
#41001=CARTESIAN_POINT('Ctrl Pts',(52.7736217513052,19.7860650976794,14.1295444107553));
#41002=CARTESIAN_POINT('Ctrl Pts',(54.8128001397719,18.4710962324233,14.2565777054643));
#41003=CARTESIAN_POINT('Ctrl Pts',(57.0233705445013,19.4714812094783,14.3836110001732));
#41004=CARTESIAN_POINT('Ctrl Pts',(57.3814312473215,21.8713112346423,14.5106442948822));
#41005=CARTESIAN_POINT('Ctrl Pts',(55.5591575066651,23.4734067469936,14.6376775895912));
#41006=CARTESIAN_POINT('Ctrl Pts',(53.2249435735374,22.8109590653041,14.7647108843002));
#41007=CARTESIAN_POINT('Ctrl Pts',(52.5158937807075,20.4904763552047,14.8917441790092));
#41008=CARTESIAN_POINT('Ctrl Pts',(54.0811831514666,18.6364912413565,15.0187774737181));
#41009=CARTESIAN_POINT('Ctrl Pts',(56.4877011003582,18.9464315230977,15.1458107684271));
#41010=CARTESIAN_POINT('Ctrl Pts',(57.5321448955836,21.1365294147907,15.2728440631361));
#41011=CARTESIAN_POINT('Ctrl Pts',(56.2582674132478,23.2016269370836,15.3998773578451));
#41012=CARTESIAN_POINT('Ctrl Pts',(53.832375240883,23.2510109895845,15.5269106525541));
#41013=CARTESIAN_POINT('Ctrl Pts',(52.4755093031501,21.2394676906214,15.653943947263));
#41014=CARTESIAN_POINT('Ctrl Pts',(53.4299567929073,19.0086782326316,15.780977241972));
#41015=CARTESIAN_POINT('Ctrl Pts',(55.8218672730494,18.6010560159054,15.908010536681));
#41016=CARTESIAN_POINT('Ctrl Pts',(57.461311972199,20.3898021395946,16.03504383139));
#41017=CARTESIAN_POINT('Ctrl Pts',(56.8472869248829,22.7372187745043,16.162077126099));
#41018=CARTESIAN_POINT('Ctrl Pts',(54.5419666475085,23.4941137707287,16.289110420808));
#41019=CARTESIAN_POINT('Ctrl Pts',(52.6560017035378,21.9675071263385,16.4161437155169));
#41020=CARTESIAN_POINT('Ctrl Pts',(52.9160992280829,19.5550932119557,16.5431770102259));
#41021=CARTESIAN_POINT('Ctrl Pts',(55.0841252871632,18.4655728478819,16.6702103049349));
#41022=CARTESIAN_POINT('Ctrl Pts',(57.1751299074027,19.6964632957773,16.7972435996439));
#41023=CARTESIAN_POINT('Ctrl Pts',(57.2746805809953,22.1208150194284,16.9242768943529));
#41024=CARTESIAN_POINT('Ctrl Pts',(55.2916330589735,23.5189974617389,17.0513101890619));
#41025=CARTESIAN_POINT('Ctrl Pts',(53.0415790449306,22.6108958427156,17.1783434837708));
#41026=CARTESIAN_POINT('Ctrl Pts',(52.58456972532,20.2279283443282,17.3053767784798));
#41027=CARTESIAN_POINT('Ctrl Pts',(54.3390228737627,18.5518359344349,17.4324100731888));
#41028=CARTESIAN_POINT('Ctrl Pts',(56.6986378114894,19.1171756219148,17.5594433678978));
#41029=CARTESIAN_POINT('Ctrl Pts',(57.5030541552832,21.4063470795431,17.6864766626068));
#41030=CARTESIAN_POINT('Ctrl Pts',(56.0157834328264,23.3234848979343,17.8135099573157));
#41031=CARTESIAN_POINT('Ctrl Pts',(53.5985057625751,23.1133414196002,17.9405432520247));
#41032=CARTESIAN_POINT('Ctrl Pts',(52.4643750072844,20.9683148355023,18.0675765467337));
#41033=CARTESIAN_POINT('Ctrl Pts',(53.6517517544994,18.8522978042014,18.1946098414427));
#41034=CARTESIAN_POINT('Ctrl Pts',(56.0735257119335,18.7026231046798,18.3216431361517));
#41035=CARTESIAN_POINT('Ctrl Pts',(57.5124264126573,20.6563263549304,18.4486764308606));
#41036=CARTESIAN_POINT('Ctrl Pts',(56.6510592176025,22.9246821850121,18.5757097255696));
#41037=CARTESIAN_POINT('Ctrl Pts',(54.2780543112314,23.4308830650201,18.7027430202786));
#41038=CARTESIAN_POINT('Ctrl Pts',(52.5660313472582,21.711473577024,18.8297763149876));
#41039=CARTESIAN_POINT('Ctrl Pts',(53.0824437806473,19.3406699547845,18.9568096096966));
#41040=CARTESIAN_POINT('Ctrl Pts',(55.3544869411717,18.4890764524041,19.0838429044055));
#41041=CARTESIAN_POINT('Ctrl Pts',(57.3019773402135,19.9363748881879,19.2108761991145));
#41042=CARTESIAN_POINT('Ctrl Pts',(57.1418778230586,22.3574820236096,19.3379094938235));
#41043=CARTESIAN_POINT('Ctrl Pts',(55.0207685154315,23.5357379048514,19.4649427885325));
#41044=CARTESIAN_POINT('Ctrl Pts',(52.8806444621192,22.3923829061673,19.5919760832415));
#41045=CARTESIAN_POINT('Ctrl Pts',(52.6809097786076,19.9742229294939,19.7190093779505));
#41046=CARTESIAN_POINT('Ctrl Pts',(54.6044328179128,18.4952196388129,19.8460426726595));
#41047=CARTESIAN_POINT('Ctrl Pts',(56.8901198931453,19.3094838531177,19.9730759673684));
#41048=CARTESIAN_POINT('Ctrl Pts',(57.4452957432646,21.6715108199466,20.1001092620774));
#41049=CARTESIAN_POINT('Ctrl Pts',(55.7616656066381,23.4187318075798,20.2271425567864));
#41050=CARTESIAN_POINT('Ctrl Pts',(53.3806877055391,22.9514675878275,20.3541758514954));
#41051=CARTESIAN_POINT('Ctrl Pts',(52.4822814194424,20.6975248730086,20.4812091462044));
#41052=CARTESIAN_POINT('Ctrl Pts',(53.8889883069237,18.7205151741717,20.6082424409133));
#41053=CARTESIAN_POINT('Ctrl Pts',(56.312888978288,18.8305022276979,20.7352757356224));
#41054=CARTESIAN_POINT('Ctrl Pts',(57.5347658402131,20.9267866909505,20.8623090303313));
#41055=CARTESIAN_POINT('Ctrl Pts',(56.4359218021414,23.0901020624526,20.9893423250403));
#41056=CARTESIAN_POINT('Ctrl Pts',(54.0224104744431,23.33981126864,21.1163756197492));
#41057=CARTESIAN_POINT('Ctrl Pts',(52.5039374211234,21.4472914661216,21.2434089144583));
#41058=CARTESIAN_POINT('Ctrl Pts',(53.2707502520462,19.1452511322188,21.3704422091672));
#41059=CARTESIAN_POINT('Ctrl Pts',(55.620788628984,18.5413378573993,21.4974755038762));
#41060=CARTESIAN_POINT('Ctrl Pts',(57.4024600495314,20.1884682607939,21.6245087985852));
#41061=CARTESIAN_POINT('Ctrl Pts',(56.9845439737103,22.5786016817879,21.7515420932942));
#41062=CARTESIAN_POINT('Ctrl Pts',(54.7496661084856,23.5234363467488,21.8785753880032));
#41063=CARTESIAN_POINT('Ctrl Pts',(52.7439830212551,22.1579229011245,22.0056086827121));
#41064=CARTESIAN_POINT('Ctrl Pts',(52.8038105505325,19.7322658183275,22.1326419774211));
#41065=CARTESIAN_POINT('Ctrl Pts',(54.8743732234172,18.4672907852779,22.2596752721301));
#41066=CARTESIAN_POINT('Ctrl Pts',(57.0599542863205,19.5211536957466,22.3867085668391));
#41067=CARTESIAN_POINT('Ctrl Pts',(57.3595311710622,21.9289836952922,22.5137418615481));
#41068=CARTESIAN_POINT('Ctrl Pts',(55.4988243656874,23.4862767958393,22.640775156257));
#41069=CARTESIAN_POINT('Ctrl Pts',(53.1814157567314,22.7672434477095,22.767808450966));
#41070=CARTESIAN_POINT('Ctrl Pts',(52.5290234561101,20.430199181403,22.894841745675));
#41071=CARTESIAN_POINT('Ctrl Pts',(54.1389493616999,18.6148396591396,23.021875040384));
#41072=CARTESIAN_POINT('Ctrl Pts',(56.5372156262214,18.9832287755273,23.148908335093));
#41073=CARTESIAN_POINT('Ctrl Pts',(57.5280743996752,21.1980855446349,23.275941629802));
#41074=CARTESIAN_POINT('Ctrl Pts',(56.2043386638812,23.2315838402376,23.4029749245109));
#41075=CARTESIAN_POINT('Ctrl Pts',(53.7779630456277,23.2219414338976,23.5300082192199));
#41076=CARTESIAN_POINT('Ctrl Pts',(52.4704310917174,21.1779864916192,23.6570415139289));
#41077=CARTESIAN_POINT('Ctrl Pts',(53.4788619536403,18.971074891145,23.7840748086379));
#41078=CARTESIAN_POINT('Ctrl Pts',(55.8799803771704,18.6217585088131,23.9111081033468));
#41079=CARTESIAN_POINT('Ctrl Pts',(57.4754271986143,20.4498561691353,24.0381413980558));
#41080=CARTESIAN_POINT('Ctrl Pts',(56.8044809906924,22.7816414928851,24.1651746927648));
#41081=CARTESIAN_POINT('Ctrl Pts',(54.4814307927619,23.4822336793536,24.2922079874738));
#41082=CARTESIAN_POINT('Ctrl Pts',(52.6331599204118,21.9102011136452,24.4192412821828));
#41083=CARTESIAN_POINT('Ctrl Pts',(52.9518644411195,19.5048281689401,24.5462745768917));
#41084=CARTESIAN_POINT('Ctrl Pts',(55.1457524576671,18.4683692359229,24.6733078716008));
#41085=CARTESIAN_POINT('Ctrl Pts',(57.2061958341146,19.7497608968377,24.8003411663097));
#41086=CARTESIAN_POINT('Ctrl Pts',(57.2467427666359,22.1758168136955,24.9273744610187));
#41087=CARTESIAN_POINT('Ctrl Pts',(55.2302699341218,23.5253463336973,25.0544077557277));
#41088=CARTESIAN_POINT('Ctrl Pts',(53.0029724215312,22.5627787976819,25.1814410504367));
#41089=CARTESIAN_POINT('Ctrl Pts',(52.6040653304014,20.1693997260389,25.3084743451457));
#41090=CARTESIAN_POINT('Ctrl Pts',(54.3987729693717,18.5364810532685,25.4355076398546));
#41091=CARTESIAN_POINT('Ctrl Pts',(56.7439347165923,19.1590545677295,25.5625409345636));
#41092=CARTESIAN_POINT('Ctrl Pts',(57.4924320706083,21.4671137370528,25.6895742292726));
#41093=CARTESIAN_POINT('Ctrl Pts',(55.9589556062135,23.3475109740183,25.8166075239816));
#41094=CARTESIAN_POINT('Ctrl Pts',(53.547524482996,23.0786159890765,25.9436408186906));
#41095=CARTESIAN_POINT('Ctrl Pts',(52.4658711091553,20.9066577783214,26.0706741133995));
#41096=CARTESIAN_POINT('Ctrl Pts',(53.7044442609637,18.8201072296902,26.1977074081085));
#41097=CARTESIAN_POINT('Ctrl Pts',(56.1289980153912,18.7294737786598,26.3247407028175));
#41098=CARTESIAN_POINT('Ctrl Pts',(57.5202301228141,20.7174345305146,26.4517739975265));
#41099=CARTESIAN_POINT('Ctrl Pts',(56.6033852487809,22.964492045205,26.5788072922355));
#41100=CARTESIAN_POINT('Ctrl Pts',(54.2198514610545,23.4121779339536,26.7058405869444));
#41101=CARTESIAN_POINT('Ctrl Pts',(52.5480301270164,21.6528985747657,26.8328738816534));
#41102=CARTESIAN_POINT('Ctrl Pts',(53.126355659332,19.2923779831827,26.9599247822321));
#41103=CARTESIAN_POINT('Ctrl Pts',(54.6482802028138,18.7665406546803,27.0446312512411));
#41104=CARTESIAN_POINT('Ctrl Pts',(55.3523638033544,18.8837997984075,27.0869932886805));
#41105=CARTESIAN_POINT('Ctrl Pts',(53.9911528061724,23.0663949408297,7.61282769962002));
#41106=CARTESIAN_POINT('Ctrl Pts',(53.3039269064612,22.7308802206034,7.65517213118968));
#41107=CARTESIAN_POINT('Ctrl Pts',(52.3025342441699,21.3258080694959,7.739860994329));
#41108=CARTESIAN_POINT('Ctrl Pts',(53.2649891419755,18.905521742655,7.86689428903798));
#41109=CARTESIAN_POINT('Ctrl Pts',(55.8184834988608,18.408799415075,7.99392758374697));
#41110=CARTESIAN_POINT('Ctrl Pts',(57.6213217604298,20.2815504187016,8.12096087845594));
#41111=CARTESIAN_POINT('Ctrl Pts',(57.0248501218595,22.8135620848035,8.24799417316493));
#41112=CARTESIAN_POINT('Ctrl Pts',(54.5741778805022,23.6844000698069,8.37502746787391));
#41113=CARTESIAN_POINT('Ctrl Pts',(52.5135417022076,22.0979047531258,8.50206076258288));
#41114=CARTESIAN_POINT('Ctrl Pts',(52.7293102399626,19.5060183539129,8.62909405729188));
#41115=CARTESIAN_POINT('Ctrl Pts',(55.0240681001933,18.2820572543959,8.75612735200084));
#41116=CARTESIAN_POINT('Ctrl Pts',(57.2967672764985,19.5464742112274,8.88316064670985));
#41117=CARTESIAN_POINT('Ctrl Pts',(57.4666583946333,22.1417022919548,9.01019394141881));
#41118=CARTESIAN_POINT('Ctrl Pts',(55.3781788068818,23.6916241218337,9.13722723612782));
#41119=CARTESIAN_POINT('Ctrl Pts',(52.9434582923559,22.7772193598424,9.26426053083678));
#41120=CARTESIAN_POINT('Ctrl Pts',(52.3916159771276,20.2356666420876,9.39129382554576));
#41121=CARTESIAN_POINT('Ctrl Pts',(54.2278969579434,18.3939059693325,9.51832712025476));
#41122=CARTESIAN_POINT('Ctrl Pts',(56.7710813525697,18.9381702501774,9.64536041496372));
#41123=CARTESIAN_POINT('Ctrl Pts',(57.6927412209364,21.3701562732864,9.77239370967272));
#41124=CARTESIAN_POINT('Ctrl Pts',(56.149044722759,23.4632431376211,9.89942700438167));
#41125=CARTESIAN_POINT('Ctrl Pts',(53.5533331146744,23.3010922880737,10.0264602990907));
#41126=CARTESIAN_POINT('Ctrl Pts',(52.2821264970286,21.0321617743691,10.1534935937996));
#41127=CARTESIAN_POINT('Ctrl Pts',(53.4992861727145,18.7337853769208,10.2805268885086));
#41128=CARTESIAN_POINT('Ctrl Pts',(56.0904338791848,18.5102560972785,10.4075601832176));
#41129=CARTESIAN_POINT('Ctrl Pts',(57.6832279532088,20.5662276063806,10.5345934779266));
#41130=CARTESIAN_POINT('Ctrl Pts',(56.8193756985891,23.0193421702064,10.6616267726356));
#41131=CARTESIAN_POINT('Ctrl Pts',(54.2897825146926,23.6236352378958,10.7886600673446));
#41132=CARTESIAN_POINT('Ctrl Pts',(52.4104334418206,21.8258424652233,10.9156933620535));
#41133=CARTESIAN_POINT('Ctrl Pts',(52.9019784132069,19.2719443997923,11.0427266567625));
#41134=CARTESIAN_POINT('Ctrl Pts',(55.3143803203856,18.3001785705584,11.1697599514715));
#41135=CARTESIAN_POINT('Ctrl Pts',(57.438949336525,19.8002513303359,11.2967932461805));
#41136=CARTESIAN_POINT('Ctrl Pts',(57.3305228587221,22.3987615741865,11.4238265408895));
#41137=CARTESIAN_POINT('Ctrl Pts',(55.0883714346901,23.7166268102304,11.5508598355984));
#41138=CARTESIAN_POINT('Ctrl Pts',(52.7653109845788,22.5472671847012,11.6778931303074));
#41139=CARTESIAN_POINT('Ctrl Pts',(52.4882341992375,19.9612973001794,11.8049264250164));
#41140=CARTESIAN_POINT('Ctrl Pts',(54.5108204822733,18.3263182433315,11.9319597197254));
#41141=CARTESIAN_POINT('Ctrl Pts',(56.9812781673263,19.1392454325794,12.0589930144344));
#41142=CARTESIAN_POINT('Ctrl Pts',(57.6377640926697,21.6557982372063,12.1860263091434));
#41143=CARTESIAN_POINT('Ctrl Pts',(55.8792284164104,23.5719308171641,12.3130596038523));
#41144=CARTESIAN_POINT('Ctrl Pts',(53.3157096014861,23.1333158673706,12.4400928985613));
#41145=CARTESIAN_POINT('Ctrl Pts',(52.2942535157833,20.7415300797984,12.5671261932703));
#41146=CARTESIAN_POINT('Ctrl Pts',(53.7500607403224,18.5863880627537,12.6941594879793));
#41147=CARTESIAN_POINT('Ctrl Pts',(56.3502577612055,18.6410437234223,12.8211927826883));
#41148=CARTESIAN_POINT('Ctrl Pts',(57.7142177470537,20.8554567259259,12.9482260773972));
#41149=CARTESIAN_POINT('Ctrl Pts',(56.5931585043799,23.2022072373923,13.0752593721062));
#41150=CARTESIAN_POINT('Ctrl Pts',(54.013472914662,23.5327129814481,13.2022926668152));
#41151=CARTESIAN_POINT('Ctrl Pts',(52.3370084387196,21.5443773333356,13.3293259615242));
#41152=CARTESIAN_POINT('Ctrl Pts',(53.0986627328562,19.0576335739436,13.4563592562332));
#41153=CARTESIAN_POINT('Ctrl Pts',(55.6010983898319,18.3492356833845,13.5833925509422));
#41154=CARTESIAN_POINT('Ctrl Pts',(57.5531946134341,20.0677618317017,13.7104258456511));
#41155=CARTESIAN_POINT('Ctrl Pts',(57.1676973571359,22.6398045323657,13.8374591403601));
#41156=CARTESIAN_POINT('Ctrl Pts',(54.7975510726062,23.7105138199792,13.9644924350691));
#41157=CARTESIAN_POINT('Ctrl Pts',(52.6127581842486,22.2995950329349,14.0915257297781));
#41158=CARTESIAN_POINT('Ctrl Pts',(52.6136196420517,19.6988237922175,14.2185590244871));
#41159=CARTESIAN_POINT('Ctrl Pts',(54.7993467328741,18.2893526598075,14.345592319196));
#41160=CARTESIAN_POINT('Ctrl Pts',(57.168783191751,19.3616318473313,14.472625613905));
#41161=CARTESIAN_POINT('Ctrl Pts',(57.5525764796455,21.9339293613873,14.599658908614));
#41162=CARTESIAN_POINT('Ctrl Pts',(55.5993422239403,23.6511619405656,14.726692203323));
#41163=CARTESIAN_POINT('Ctrl Pts',(53.097376403653,22.9411064337446,14.853725498032));
#41164=CARTESIAN_POINT('Ctrl Pts',(52.3373696530442,20.4538586520226,14.9807587927409));
#41165=CARTESIAN_POINT('Ctrl Pts',(54.0151509604544,18.4666340363447,15.1077920874499));
#41166=CARTESIAN_POINT('Ctrl Pts',(56.5946170361996,18.7988486548256,15.2348253821589));
#41167=CARTESIAN_POINT('Ctrl Pts',(57.7141213968662,21.1463413119175,15.3618586768679));
#41168=CARTESIAN_POINT('Ctrl Pts',(56.3486947430345,23.3598502551246,15.4888919715769));
#41169=CARTESIAN_POINT('Ctrl Pts',(53.7484620853422,23.4127833687828,15.6159252662859));
#41170=CARTESIAN_POINT('Ctrl Pts',(52.2940828826737,21.2566774058259,15.7429585609948));
#41171=CARTESIAN_POINT('Ctrl Pts',(53.3171232144706,18.8655688202178,15.8699918557038));
#41172=CARTESIAN_POINT('Ctrl Pts',(55.8809320331778,18.4286522037224,15.9970251504128));
#41173=CARTESIAN_POINT('Ctrl Pts',(57.6381979561121,20.3459493285172,16.1240584451218));
#41174=CARTESIAN_POINT('Ctrl Pts',(56.9800450510238,22.8620666831285,16.2510917398307));
#41175=CARTESIAN_POINT('Ctrl Pts',(54.5090493736581,23.6733571065227,16.3781250345398));
#41176=CARTESIAN_POINT('Ctrl Pts',(52.4875466480051,22.0370385193185,16.5051583292487));
#41177=CARTESIAN_POINT('Ctrl Pts',(52.7663364826117,19.4512527554216,16.6321916239577));
#41178=CARTESIAN_POINT('Ctrl Pts',(55.0901710807725,18.2834323287108,16.7592249186667));
#41179=CARTESIAN_POINT('Ctrl Pts',(57.3314489755076,19.6027826185216,16.8862582133757));
#41180=CARTESIAN_POINT('Ctrl Pts',(57.4381540119143,22.2013641207758,17.0132915080847));
#41181=CARTESIAN_POINT('Ctrl Pts',(55.3125917188917,23.7000291023953,17.1403248027936));
#41182=CARTESIAN_POINT('Ctrl Pts',(52.900834100175,22.7266653588675,17.2673580975026));
#41183=CARTESIAN_POINT('Ctrl Pts',(52.4109811004174,20.1724422231019,17.3943913922116));
#41184=CARTESIAN_POINT('Ctrl Pts',(54.2915207323686,18.3758948451258,17.5214246869206));
#41185=CARTESIAN_POINT('Ctrl Pts',(56.8207130396567,18.9818635418474,17.6484579816296));
#41186=CARTESIAN_POINT('Ctrl Pts',(57.6829400056126,21.4355498396105,17.7754912763385));
#41187=CARTESIAN_POINT('Ctrl Pts',(56.0887842770866,23.4904657264195,17.9025245710475));
#41188=CARTESIAN_POINT('Ctrl Pts',(53.4977852159983,23.2652199626587,18.0295578657565));
#41189=CARTESIAN_POINT('Ctrl Pts',(52.2821484034498,20.9660377322496,18.1565911604655));
#41190=CARTESIAN_POINT('Ctrl Pts',(53.5548578133176,18.6979498709256,18.2836244551745));
#41191=CARTESIAN_POINT('Ctrl Pts',(56.1506762942069,18.5375185681002,18.4106577498834));
#41192=CARTESIAN_POINT('Ctrl Pts',(57.6929858147289,20.6316277179677,18.5376910445924));
#41193=CARTESIAN_POINT('Ctrl Pts',(56.7697151366827,23.0630024409818,18.6647243393014));
#41194=CARTESIAN_POINT('Ctrl Pts',(54.226170569986,23.6055822285518,18.7917576340104));
#41195=CARTESIAN_POINT('Ctrl Pts',(52.3911104332023,21.7626047237951,18.9187909287194));
#41196=CARTESIAN_POINT('Ctrl Pts',(52.9446356431986,19.2214196399119,19.0458242234284));
#41197=CARTESIAN_POINT('Ctrl Pts',(55.3799626923489,18.3086250560496,19.1728575181373));
#41198=CARTESIAN_POINT('Ctrl Pts',(57.4674124948662,19.859935827824,19.2998908128463));
#41199=CARTESIAN_POINT('Ctrl Pts',(57.2958071787975,22.4550395645076,19.4269241075553));
#41200=CARTESIAN_POINT('Ctrl Pts',(55.0222610768493,23.7179726232908,19.5539574022643));
#41201=CARTESIAN_POINT('Ctrl Pts',(52.7283337051675,22.4924486528597,19.6809906969732));
#41202=CARTESIAN_POINT('Ctrl Pts',(52.5142447803355,19.9005038770367,19.8080239916823));
#41203=CARTESIAN_POINT('Ctrl Pts',(54.5760047718148,18.3152097320318,19.9350572863912));
#41204=CARTESIAN_POINT('Ctrl Pts',(57.0259562766631,19.1879923009132,20.0620905811002));
#41205=CARTESIAN_POINT('Ctrl Pts',(57.6210306961643,21.7197699814979,20.1891238758092));
#41206=CARTESIAN_POINT('Ctrl Pts',(55.8164038810887,23.5925577022401,20.3161571705182));
#41207=CARTESIAN_POINT('Ctrl Pts',(53.2643133280918,23.0917128181136,20.4431904652271));
#41208=CARTESIAN_POINT('Ctrl Pts',(52.3013416875561,20.6757870311375,20.5702237599362));
#41209=CARTESIAN_POINT('Ctrl Pts',(53.8091437367561,18.5566964787825,20.6972570546451));
#41210=CARTESIAN_POINT('Ctrl Pts',(56.4072417711545,18.6745879216752,20.8242903493541));
#41211=CARTESIAN_POINT('Ctrl Pts',(57.716930699727,20.9215251034911,20.9513236440631));
#41212=CARTESIAN_POINT('Ctrl Pts',(56.5391165387953,23.2403104732399,21.0783569387721));
#41213=CARTESIAN_POINT('Ctrl Pts',(53.9521544942811,23.5079654169557,21.205390233481));
#41214=CARTESIAN_POINT('Ctrl Pts',(52.324554031224,21.479436757728,21.33242352819));
#41215=CARTESIAN_POINT('Ctrl Pts',(53.1464750498154,19.011956742034,21.459456822899));
#41216=CARTESIAN_POINT('Ctrl Pts',(55.665402561992,18.3646423075804,21.586490117608));
#41217=CARTESIAN_POINT('Ctrl Pts',(57.5751165491841,20.130146279758,21.713523412317));
#41218=CARTESIAN_POINT('Ctrl Pts',(57.1271662895212,22.6920503282187,21.840556707026));
#41219=CARTESIAN_POINT('Ctrl Pts',(54.7316754769819,23.7047869947277,21.9675900017349));
#41220=CARTESIAN_POINT('Ctrl Pts',(52.5818508789192,22.2411388176659,22.0946232964439));
#41221=CARTESIAN_POINT('Ctrl Pts',(52.6459780059317,19.641158144616,22.2216565911529));
#41222=CARTESIAN_POINT('Ctrl Pts',(54.8653448612133,18.2852737283293,22.3486898858619));
#41223=CARTESIAN_POINT('Ctrl Pts',(57.207996080643,19.4148741234946,22.4757231805709));
#41224=CARTESIAN_POINT('Ctrl Pts',(57.529102520603,21.9957465424392,22.6027564752798));
#41225=CARTESIAN_POINT('Ctrl Pts',(55.5346731486622,23.6649569153365,22.7297897699888));
#41226=CARTESIAN_POINT('Ctrl Pts',(53.050720393107,22.8942491258165,22.8568230646978));
#41227=CARTESIAN_POINT('Ctrl Pts',(52.3514429128353,20.389249566088,22.9838563594068));
#41228=CARTESIAN_POINT('Ctrl Pts',(54.0770686285482,18.4434264297526,23.1108896541158));
#41229=CARTESIAN_POINT('Ctrl Pts',(56.6476899998897,18.8382903985975,23.2379229488247));
#41230=CARTESIAN_POINT('Ctrl Pts',(57.7097583684865,21.2123212680449,23.3649562435337));
#41231=CARTESIAN_POINT('Ctrl Pts',(56.2908903208558,23.3919600573624,23.4919895382427));
#41232=CARTESIAN_POINT('Ctrl Pts',(53.6901394736897,23.3816246846075,23.6190228329517));
#41233=CARTESIAN_POINT('Ctrl Pts',(52.2886397177381,21.1907777655613,23.7460561276607));
#41234=CARTESIAN_POINT('Ctrl Pts',(53.3695430200646,18.8252630565545,23.8730894223697));
#41235=CARTESIAN_POINT('Ctrl Pts',(55.943221525224,18.4508425132372,24.0001227170786));
#41236=CARTESIAN_POINT('Ctrl Pts',(57.6533275950606,20.4103192335841,24.1271560117877));
#41237=CARTESIAN_POINT('Ctrl Pts',(56.934162802302,22.9096819087321,24.2541893064966));
#41238=CARTESIAN_POINT('Ctrl Pts',(54.444163016273,23.6606232340439,24.3812226012056));
#41239=CARTESIAN_POINT('Ctrl Pts',(52.4630633048785,21.9756141215713,24.5082558959146));
#41240=CARTESIAN_POINT('Ctrl Pts',(52.8046720178866,19.3973753375057,24.6352891906235));
#41241=CARTESIAN_POINT('Ctrl Pts',(55.1562271830061,18.2864296834945,24.7623224853325));
#41242=CARTESIAN_POINT('Ctrl Pts',(57.3647475029929,19.6599105339469,24.8893557800415));
#41243=CARTESIAN_POINT('Ctrl Pts',(57.408208403404,22.2603187038831,25.0163890747505));
#41244=CARTESIAN_POINT('Ctrl Pts',(55.2468186383588,23.7068342458364,25.1434223694595));
#41245=CARTESIAN_POINT('Ctrl Pts',(52.8594529521957,22.6750903081238,25.2704556641685));
#41246=CARTESIAN_POINT('Ctrl Pts',(52.4318777872494,20.1097073553205,25.3974889588775));
#41247=CARTESIAN_POINT('Ctrl Pts',(54.3555648608227,18.3594364617242,25.5245222535864));
#41248=CARTESIAN_POINT('Ctrl Pts',(56.8692652767605,19.0267521827433,25.6515555482954));
#41249=CARTESIAN_POINT('Ctrl Pts',(57.6715545484274,21.5006835867554,25.7785888430044));
#41250=CARTESIAN_POINT('Ctrl Pts',(56.0278724310004,23.5162184735454,25.9056221377133));
#41251=CARTESIAN_POINT('Ctrl Pts',(53.4431400880731,23.2279989354718,26.0326554324224));
#41252=CARTESIAN_POINT('Ctrl Pts',(52.2837520249908,20.899949595487,26.1596887271313));
#41253=CARTESIAN_POINT('Ctrl Pts',(53.6113371480899,18.663445871091,26.2867220218403));
#41254=CARTESIAN_POINT('Ctrl Pts',(56.2101352003739,18.5662989072097,26.4137553165493));
#41255=CARTESIAN_POINT('Ctrl Pts',(57.7013503505611,20.6971275269108,26.5407886112583));
#41256=CARTESIAN_POINT('Ctrl Pts',(56.7186150045072,23.1056732982239,26.6678219059673));
#41257=CARTESIAN_POINT('Ctrl Pts',(54.1637848821451,23.5855328243699,26.7948552006763));
#41258=CARTESIAN_POINT('Ctrl Pts',(52.3718155274831,21.6998201385892,26.9218884953852));
#41259=CARTESIAN_POINT('Ctrl Pts',(52.9917033168228,19.1696570912324,27.0489393959639));
#41260=CARTESIAN_POINT('Ctrl Pts',(54.6230033167101,18.606029651488,27.1336458649729));
#41261=CARTESIAN_POINT('Ctrl Pts',(55.3776869719554,18.7317158045685,27.1760079024124));
#41262=CARTESIAN_POINT('Ctrl Pts',(53.9235115861173,23.2049426572415,7.70184231335182));
#41263=CARTESIAN_POINT('Ctrl Pts',(53.190208541528,22.8469323349445,7.74418674492148));
#41264=CARTESIAN_POINT('Ctrl Pts',(52.121674470859,21.347652859727,7.8288756080608));
#41265=CARTESIAN_POINT('Ctrl Pts',(53.1486600765197,18.7650910951076,7.95590890276978));
#41266=CARTESIAN_POINT('Ctrl Pts',(55.8733612075929,18.2350645124613,8.08294219747876));
#41267=CARTESIAN_POINT('Ctrl Pts',(57.7970762286159,20.2333797873867,8.20997549218775));
#41268=CARTESIAN_POINT('Ctrl Pts',(57.1606123398736,22.935157855513,8.33700878689672));
#41269=CARTESIAN_POINT('Ctrl Pts',(54.5456273449349,23.8643838145687,8.46404208160572));
#41270=CARTESIAN_POINT('Ctrl Pts',(52.3468295639297,22.1715171073655,8.59107537631469));
#41271=CARTESIAN_POINT('Ctrl Pts',(52.5770649577483,19.4058498230397,8.71810867102368));
#41272=CARTESIAN_POINT('Ctrl Pts',(55.025681818972,18.0998245391965,8.84514196573266));
#41273=CARTESIAN_POINT('Ctrl Pts',(57.4507610049,19.449018166015,8.97217526044164));
#41274=CARTESIAN_POINT('Ctrl Pts',(57.6320429883485,22.218251185028,9.09920855515061));
#41275=CARTESIAN_POINT('Ctrl Pts',(55.4035349520473,23.872092225075,9.22624184985961));
#41276=CARTESIAN_POINT('Ctrl Pts',(52.8055712158489,22.8963784223254,9.35327514456858));
#41277=CARTESIAN_POINT('Ctrl Pts',(52.2167289587976,20.1844195937989,9.48030843927757));
#41278=CARTESIAN_POINT('Ctrl Pts',(54.1761289676149,18.2191724904756,9.60734173398655));
#41279=CARTESIAN_POINT('Ctrl Pts',(56.889828873738,18.7999286208435,9.73437502869553));
#41280=CARTESIAN_POINT('Ctrl Pts',(57.8732842234754,21.3949745233537,9.86140832340451));
#41281=CARTESIAN_POINT('Ctrl Pts',(56.2260859113758,23.6283987450711,9.98844161811349));
#41282=CARTESIAN_POINT('Ctrl Pts',(53.4563369454474,23.4553759999944,10.1154749128224));
#41283=CARTESIAN_POINT('Ctrl Pts',(52.0998984244116,21.0343181580819,10.2425082075314));
#41284=CARTESIAN_POINT('Ctrl Pts',(53.3986662623335,18.5818401438375,10.3695415022404));
#41285=CARTESIAN_POINT('Ctrl Pts',(56.1635453260211,18.3433236656525,10.4965747969494));
#41286=CARTESIAN_POINT('Ctrl Pts',(57.8631331098581,20.5371440205708,10.6236080916584));
#41287=CARTESIAN_POINT('Ctrl Pts',(56.9413612606683,23.1547350908955,10.7506413863674));
#41288=CARTESIAN_POINT('Ctrl Pts',(54.2421638292222,23.7995448201956,10.8776746810763));
#41289=CARTESIAN_POINT('Ctrl Pts',(52.2368080974863,21.8812135781755,11.0047079757853));
#41290=CARTESIAN_POINT('Ctrl Pts',(52.7613101923895,19.156081670693,11.1317412704943));
#41291=CARTESIAN_POINT('Ctrl Pts',(55.335458902516,18.1191608539651,11.2587745652033));
#41292=CARTESIAN_POINT('Ctrl Pts',(57.6024760923949,19.7198105418082,11.3858078599123));
#41293=CARTESIAN_POINT('Ctrl Pts',(57.4867798325181,22.492545786526,11.5128411546213));
#41294=CARTESIAN_POINT('Ctrl Pts',(55.0942965655693,23.8987712945513,11.6398744493302));
#41295=CARTESIAN_POINT('Ctrl Pts',(52.6154794814812,22.6510084061315,11.7669077440392));
#41296=CARTESIAN_POINT('Ctrl Pts',(52.3198252426627,19.89165432717,11.8939410387482));
#41297=CARTESIAN_POINT('Ctrl Pts',(54.4780219577718,18.1470531403838,12.0209743334572));
#41298=CARTESIAN_POINT('Ctrl Pts',(57.1141189714901,19.0144854987329,12.1480076281661));
#41299=CARTESIAN_POINT('Ctrl Pts',(57.8146209868923,21.6997682191282,12.2750409228752));
#41300=CARTESIAN_POINT('Ctrl Pts',(55.9381789523853,23.7443737197508,12.4020742175841));
#41301=CARTESIAN_POINT('Ctrl Pts',(53.2027812430792,23.2763505002808,12.5291075122931));
#41302=CARTESIAN_POINT('Ctrl Pts',(52.1128385359212,20.7242001800308,12.6561408070021));
#41303=CARTESIAN_POINT('Ctrl Pts',(53.6662547714537,18.4245601296697,12.7831741017111));
#41304=CARTESIAN_POINT('Ctrl Pts',(56.4407898882863,18.4828803448845,12.9102073964201));
#41305=CARTESIAN_POINT('Ctrl Pts',(57.8962007084268,20.8457653836999,13.037240691129));
#41306=CARTESIAN_POINT('Ctrl Pts',(56.6999766485317,23.3498609011608,13.164273985838));
#41307=CARTESIAN_POINT('Ctrl Pts',(53.94732821398,23.7025264052872,13.291307280547));
#41308=CARTESIAN_POINT('Ctrl Pts',(52.1584600923461,21.5808767628056,13.418340575256));
#41309=CARTESIAN_POINT('Ctrl Pts',(52.9711818088149,18.9274017254969,13.545373869965));
#41310=CARTESIAN_POINT('Ctrl Pts',(55.641400854576,18.1715071497163,13.6724071646739));
#41311=CARTESIAN_POINT('Ctrl Pts',(57.7243812904128,20.0052570961269,13.7994404593829));
#41312=CARTESIAN_POINT('Ctrl Pts',(57.3130372013104,22.7497502009462,13.9264737540919));
#41313=CARTESIAN_POINT('Ctrl Pts',(54.783977270219,23.8922484403271,14.0535070488009));
#41314=CARTESIAN_POINT('Ctrl Pts',(52.4526983159437,22.3867303237331,14.1805403435099));
#41315=CARTESIAN_POINT('Ctrl Pts',(52.453617532798,19.6115824867557,14.3075736382189));
#41316=CARTESIAN_POINT('Ctrl Pts',(54.7858933259761,18.1076090871918,14.4346069329278));
#41317=CARTESIAN_POINT('Ctrl Pts',(57.3141958390006,19.2517824851842,14.5616402276368));
#41318=CARTESIAN_POINT('Ctrl Pts',(57.7237217119695,21.9965474881324,14.6886735223458));
#41319=CARTESIAN_POINT('Ctrl Pts',(55.6395269412154,23.8289171341376,14.8157068170548));
#41320=CARTESIAN_POINT('Ctrl Pts',(52.9698092337686,23.0712538021851,14.9427401117638));
#41321=CARTESIAN_POINT('Ctrl Pts',(52.1588455253809,20.4172409488405,15.0697734064727));
#41322=CARTESIAN_POINT('Ctrl Pts',(53.9491187694424,18.2967768313329,15.1968067011817));
#41323=CARTESIAN_POINT('Ctrl Pts',(56.701532972041,18.6512657865535,15.3238399958907));
#41324=CARTESIAN_POINT('Ctrl Pts',(57.8960978981489,21.1561532090444,15.4508732905997));
#41325=CARTESIAN_POINT('Ctrl Pts',(56.4391220728212,23.5180735731657,15.5779065853087));
#41326=CARTESIAN_POINT('Ctrl Pts',(53.6645489298014,23.574555747981,15.7049398800177));
#41327=CARTESIAN_POINT('Ctrl Pts',(52.1126564621973,21.2738871210305,15.8319731747266));
#41328=CARTESIAN_POINT('Ctrl Pts',(53.2042896360337,18.7224594078039,15.9590064694356));
#41329=CARTESIAN_POINT('Ctrl Pts',(55.9399967933065,18.2562483915393,16.0860397641446));
#41330=CARTESIAN_POINT('Ctrl Pts',(57.8150839400251,20.3020965174398,16.2130730588536));
#41331=CARTESIAN_POINT('Ctrl Pts',(57.1128031771649,22.9869145917525,16.3401063535625));
#41332=CARTESIAN_POINT('Ctrl Pts',(54.4761320998075,23.8526004423166,16.4671396482715));
#41333=CARTESIAN_POINT('Ctrl Pts',(52.3190915924723,22.1065699122985,16.5941729429805));
#41334=CARTESIAN_POINT('Ctrl Pts',(52.6165737371404,19.3474122988875,16.7212062376895));
#41335=CARTESIAN_POINT('Ctrl Pts',(55.0962168743818,18.1012918095397,16.8482395323985));
#41336=CARTESIAN_POINT('Ctrl Pts',(57.4877680436125,19.5091019412658,16.9752728271075));
#41337=CARTESIAN_POINT('Ctrl Pts',(57.6016274428333,22.2819132221231,17.1023061218164));
#41338=CARTESIAN_POINT('Ctrl Pts',(55.3335503788099,23.8810607430516,17.2293394165254));
#41339=CARTESIAN_POINT('Ctrl Pts',(52.7600891554195,22.8424348750194,17.3563727112344));
#41340=CARTESIAN_POINT('Ctrl Pts',(52.2373924755148,20.1169561018757,17.4834060059434));
#41341=CARTESIAN_POINT('Ctrl Pts',(54.2440185909744,18.1999537558167,17.6104393006524));
#41342=CARTESIAN_POINT('Ctrl Pts',(56.9427882678241,18.84655146178,17.7374725953614));
#41343=CARTESIAN_POINT('Ctrl Pts',(57.862825855942,21.4647525996779,17.8645058900703));
#41344=CARTESIAN_POINT('Ctrl Pts',(56.1617851213467,23.6574465549046,17.9915391847793));
#41345=CARTESIAN_POINT('Ctrl Pts',(53.3970646694217,23.4170985057174,18.1185724794883));
#41346=CARTESIAN_POINT('Ctrl Pts',(52.0999217996153,20.963760628997,18.2456057741973));
#41347=CARTESIAN_POINT('Ctrl Pts',(53.4579638721358,18.5436019376496,18.3726390689062));
#41348=CARTESIAN_POINT('Ctrl Pts',(56.2278268764801,18.3724140315205,18.4996723636153));
#41349=CARTESIAN_POINT('Ctrl Pts',(57.8735452168006,20.6069290810051,18.6267056583242));
#41350=CARTESIAN_POINT('Ctrl Pts',(56.8883710557629,23.2013226969515,18.7537389530332));
#41351=CARTESIAN_POINT('Ctrl Pts',(54.1742868287406,23.7802813920835,18.8807722477422));
#41352=CARTESIAN_POINT('Ctrl Pts',(52.2161895191464,21.8137358705663,19.0078055424512));
#41353=CARTESIAN_POINT('Ctrl Pts',(52.8068275057499,19.1021693250393,19.1348388371601));
#41354=CARTESIAN_POINT('Ctrl Pts',(55.4054384435264,18.1281736596952,19.2618721318691));
#41355=CARTESIAN_POINT('Ctrl Pts',(57.6328476495188,19.7834967674601,19.3889054265781));
#41356=CARTESIAN_POINT('Ctrl Pts',(57.4497365345366,22.5525971054056,19.5159387212871));
#41357=CARTESIAN_POINT('Ctrl Pts',(55.0237536382671,23.9002073417302,19.6429720159961));
#41358=CARTESIAN_POINT('Ctrl Pts',(52.5760229482159,22.5925143995522,19.770005310705));
#41359=CARTESIAN_POINT('Ctrl Pts',(52.3475797820632,19.8267848245796,19.897038605414));
#41360=CARTESIAN_POINT('Ctrl Pts',(54.5475767257167,18.1351998252507,20.024071900123));
#41361=CARTESIAN_POINT('Ctrl Pts',(57.1617926601811,19.0665007487085,20.151105194832));
#41362=CARTESIAN_POINT('Ctrl Pts',(57.7967656490639,21.7680291430493,20.278138489541));
#41363=CARTESIAN_POINT('Ctrl Pts',(55.8711421555395,23.7663835969004,20.40517178425));
#41364=CARTESIAN_POINT('Ctrl Pts',(53.1479389506444,23.2319580483999,20.5322050789589));
#41365=CARTESIAN_POINT('Ctrl Pts',(52.1204019556699,20.6540491892665,20.6592383736679));
#41366=CARTESIAN_POINT('Ctrl Pts',(53.7292991665885,18.3928777833932,20.7862716683769));
#41367=CARTESIAN_POINT('Ctrl Pts',(56.5015945640211,18.5186736156525,20.9133049630859));
#41368=CARTESIAN_POINT('Ctrl Pts',(57.8990955592407,20.9162635160316,21.0403382577949));
#41369=CARTESIAN_POINT('Ctrl Pts',(56.6423112754491,23.390518884027,21.1673715525038));
#41370=CARTESIAN_POINT('Ctrl Pts',(53.8818985141192,23.6761195652714,21.2944048472128));
#41371=CARTESIAN_POINT('Ctrl Pts',(52.1451706413245,21.5115820493345,21.4214381419218));
#41372=CARTESIAN_POINT('Ctrl Pts',(53.0221998475846,18.878662351849,21.5484714366308));
#41373=CARTESIAN_POINT('Ctrl Pts',(55.7100164950001,18.1879467577614,21.6755047313398));
#41374=CARTESIAN_POINT('Ctrl Pts',(57.7477730488369,20.071824298722,21.8025380260487));
#41375=CARTESIAN_POINT('Ctrl Pts',(57.2697886053323,22.8054989746496,21.9295713207578));
#41376=CARTESIAN_POINT('Ctrl Pts',(54.7136848454783,23.8861376427066,22.0566046154667));
#41377=CARTESIAN_POINT('Ctrl Pts',(52.4197187365831,22.3243547342073,22.1836379101757));
#41378=CARTESIAN_POINT('Ctrl Pts',(52.488145461331,19.5500504709044,22.3106712048847));
#41379=CARTESIAN_POINT('Ctrl Pts',(54.8563164990095,18.1032566713808,22.4377044995937));
#41380=CARTESIAN_POINT('Ctrl Pts',(57.3560378749654,19.3085945512426,22.5647377943026));
#41381=CARTESIAN_POINT('Ctrl Pts',(57.6986738701439,22.0625093895861,22.6917710890117));
#41382=CARTESIAN_POINT('Ctrl Pts',(55.5705219316369,23.8436370348337,22.8188043837206));
#41383=CARTESIAN_POINT('Ctrl Pts',(52.9200250294827,23.0212548039235,22.9458376784296));
#41384=CARTESIAN_POINT('Ctrl Pts',(52.1738623695604,20.3482999507729,23.0728709731386));
#41385=CARTESIAN_POINT('Ctrl Pts',(54.0151878953965,18.2720132003655,23.1999042678476));
#41386=CARTESIAN_POINT('Ctrl Pts',(56.7581643735579,18.6933520216677,23.3269375625566));
#41387=CARTESIAN_POINT('Ctrl Pts',(57.8914423372978,21.2265569914547,23.4539708572655));
#41388=CARTESIAN_POINT('Ctrl Pts',(56.3774419778305,23.552336274487,23.5810041519745));
#41389=CARTESIAN_POINT('Ctrl Pts',(53.6023159017516,23.5413079353176,23.7080374466835));
#41390=CARTESIAN_POINT('Ctrl Pts',(52.1068483437591,21.2035690395033,23.8350707413925));
#41391=CARTESIAN_POINT('Ctrl Pts',(53.2602240864888,18.679451221964,23.9621040361015));
#41392=CARTESIAN_POINT('Ctrl Pts',(56.0064626732777,18.2799265176612,24.0891373308104));
#41393=CARTESIAN_POINT('Ctrl Pts',(57.8312279915067,20.3707822980329,24.2161706255194));
#41394=CARTESIAN_POINT('Ctrl Pts',(57.0638446139116,23.0377223245789,24.3432039202284));
#41395=CARTESIAN_POINT('Ctrl Pts',(54.4068952397841,23.8390127887343,24.4702372149373));
#41396=CARTESIAN_POINT('Ctrl Pts',(52.2929666893451,22.0410271294973,24.5972705096464));
#41397=CARTESIAN_POINT('Ctrl Pts',(52.6574795946538,19.2899225060713,24.7243038043553));
#41398=CARTESIAN_POINT('Ctrl Pts',(55.1667019083449,18.1044901310662,24.8513370990643));
#41399=CARTESIAN_POINT('Ctrl Pts',(57.5232991718713,19.5700601710561,24.9783703937733));
#41400=CARTESIAN_POINT('Ctrl Pts',(57.569674040172,22.3448205940707,25.1054036884823));
#41401=CARTESIAN_POINT('Ctrl Pts',(55.2633673425956,23.8883221579753,25.2324369831912));
#41402=CARTESIAN_POINT('Ctrl Pts',(52.7159334828604,22.7874018185658,25.3594702779003));
#41403=CARTESIAN_POINT('Ctrl Pts',(52.2596902440975,20.0500149846021,25.4865035726092));
#41404=CARTESIAN_POINT('Ctrl Pts',(54.3123567522736,18.1823918701799,25.6135368673182));
#41405=CARTESIAN_POINT('Ctrl Pts',(56.9945958369287,18.8944497977569,25.7405701620272));
#41406=CARTESIAN_POINT('Ctrl Pts',(57.8506770262465,21.534253436458,25.8676034567362));
#41407=CARTESIAN_POINT('Ctrl Pts',(56.0967892557872,23.6849259730726,25.9946367514452));
#41408=CARTESIAN_POINT('Ctrl Pts',(53.33875569315,23.3773818818673,26.1216700461541));
#41409=CARTESIAN_POINT('Ctrl Pts',(52.1016329408265,20.8932414126525,26.2487033408631));
#41410=CARTESIAN_POINT('Ctrl Pts',(53.5182300352158,18.5067845124918,26.3757366355721));
#41411=CARTESIAN_POINT('Ctrl Pts',(56.2912723853565,18.4031240357596,26.5027699302811));
#41412=CARTESIAN_POINT('Ctrl Pts',(57.8824705783081,20.6768205233068,26.62980322499));
#41413=CARTESIAN_POINT('Ctrl Pts',(56.8338447602333,23.2468545512428,26.7568365196991));
#41414=CARTESIAN_POINT('Ctrl Pts',(54.1077183032358,23.7588877147861,26.883869814408));
#41415=CARTESIAN_POINT('Ctrl Pts',(52.1956009279497,21.7467417024125,27.010903109117));
#41416=CARTESIAN_POINT('Ctrl Pts',(52.8570509743138,19.046936199282,27.1379540096957));
#41417=CARTESIAN_POINT('Ctrl Pts',(54.5977264306064,18.4455186482959,27.2226604787048));
#41418=CARTESIAN_POINT('Ctrl Pts',(55.4030101405564,18.5796318107295,27.2650225161442));
#41419=CARTESIAN_POINT('Ctrl Pts',(52.682543123578,21.7964570772642,27.));
#41420=CARTESIAN_POINT('Ctrl Pts',(52.6775614025261,21.7814932791564,27.));
#41421=CARTESIAN_POINT('Ctrl Pts',(52.6725796814742,21.7665294810485,27.));
#41422=CARTESIAN_POINT('Ctrl Pts',(52.6675979604224,21.7515656829407,27.));
#41423=CARTESIAN_POINT('',(53.8384922642054,19.3763282842596,7.69906393853165));
#41424=CARTESIAN_POINT('Ctrl Pts',(53.8371246242104,19.3752411305972,7.7));
#41425=CARTESIAN_POINT('Ctrl Pts',(53.7954009457829,19.3983180443861,7.69999999999996));
#41426=CARTESIAN_POINT('Ctrl Pts',(53.7546382435995,19.4229469258337,7.7));
#41427=CARTESIAN_POINT('Ctrl Pts',(53.714934131533,19.4491088737553,7.7));
#41428=CARTESIAN_POINT('Ctrl Pts',(53.6548222073576,19.4887179960324,7.69999999999998));
#41429=CARTESIAN_POINT('Ctrl Pts',(53.5971353757259,19.5318385392025,7.69999999999999));
#41430=CARTESIAN_POINT('Ctrl Pts',(53.5419564862638,19.5781218769382,7.69999999999999));
#41431=CARTESIAN_POINT('Ctrl Pts',(53.5118285687018,19.6033927839351,7.7));
#41432=CARTESIAN_POINT('Ctrl Pts',(53.4824486254372,19.6296074937631,7.7));
#41433=CARTESIAN_POINT('Ctrl Pts',(53.4538328165778,19.6567151749008,7.7));
#41434=CARTESIAN_POINT('Ctrl Pts',(53.441927541973,19.6679930104997,7.7));
#41435=CARTESIAN_POINT('Ctrl Pts',(53.4301545553945,19.679425454428,7.70000000000001));
#41436=CARTESIAN_POINT('Ctrl Pts',(53.4185151361639,19.6910090336056,7.7));
#41437=CARTESIAN_POINT('Ctrl Pts',(53.4070875682394,19.7023817778327,7.7));
#41438=CARTESIAN_POINT('Ctrl Pts',(53.3957949213602,19.7138941297562,7.69999999999996));
#41439=CARTESIAN_POINT('Ctrl Pts',(53.3846420678092,19.7255380469733,7.69999999999997));
#41440=CARTESIAN_POINT('Ctrl Pts',(53.3326376402129,19.77983224595,7.69999999999998));
#41441=CARTESIAN_POINT('Ctrl Pts',(53.2836425471235,19.8370110695029,7.69999999999998));
#41442=CARTESIAN_POINT('Ctrl Pts',(53.2377500175545,19.8967020336691,7.69999999999999));
#41443=CARTESIAN_POINT('Ctrl Pts',(53.1912145152524,19.9572292921675,7.7));
#41444=CARTESIAN_POINT('Ctrl Pts',(53.1478684980368,20.02034026621,7.7));
#41445=CARTESIAN_POINT('Ctrl Pts',(53.1078385251695,20.0856923523535,7.7));
#41446=CARTESIAN_POINT('Ctrl Pts',(53.1023914173776,20.0945851852022,7.7));
#41447=CARTESIAN_POINT('Ctrl Pts',(53.0970057638649,20.1035195747242,7.7));
#41448=CARTESIAN_POINT('Ctrl Pts',(53.0916819349052,20.1124947106681,7.69999999999999));
#41449=CARTESIAN_POINT('Ctrl Pts',(53.0841510691443,20.1251905625617,7.69999999999999));
#41450=CARTESIAN_POINT('Ctrl Pts',(53.0767434016693,20.1379690332957,7.69999999999999));
#41451=CARTESIAN_POINT('Ctrl Pts',(53.0694684776847,20.1508123778746,7.69999999999999));
#41452=CARTESIAN_POINT('Ctrl Pts',(53.0310782388569,20.2185875280722,7.69999999999999));
#41453=CARTESIAN_POINT('Ctrl Pts',(52.9963246122019,20.2882608100817,7.69999999999999));
#41454=CARTESIAN_POINT('Ctrl Pts',(52.9653032278674,20.3594518913737,7.7));
#41455=CARTESIAN_POINT('Ctrl Pts',(52.9337377497509,20.431891615352,7.70000000000001));
#41456=CARTESIAN_POINT('Ctrl Pts',(52.9060359082978,20.5059036185587,7.70000000000002));
#41457=CARTESIAN_POINT('Ctrl Pts',(52.8823336043208,20.5811279320593,7.7));
#41458=CARTESIAN_POINT('Ctrl Pts',(52.8649251749872,20.6363772929238,7.69999999999999));
#41459=CARTESIAN_POINT('Ctrl Pts',(52.8496749210952,20.6922815309851,7.7));
#41460=CARTESIAN_POINT('Ctrl Pts',(52.8366516865568,20.7487078095979,7.70000000000001));
#41461=CARTESIAN_POINT('Ctrl Pts',(52.8268614045027,20.7911265482954,7.70000000000001));
#41462=CARTESIAN_POINT('Ctrl Pts',(52.8183299413487,20.8338404939063,7.70000000000001));
#41463=CARTESIAN_POINT('Ctrl Pts',(52.8110920343712,20.8767951347477,7.70000000000003));
#41464=CARTESIAN_POINT('Ctrl Pts',(52.8089129591374,20.8897272426518,7.70000000000003));
#41465=CARTESIAN_POINT('Ctrl Pts',(52.8068508399361,20.9026833709167,7.69999999999999));
#41466=CARTESIAN_POINT('Ctrl Pts',(52.8049077631042,20.9156550025417,7.69999999999999));
#41467=CARTESIAN_POINT('Ctrl Pts',(52.7928947628234,20.9958516328525,7.69999999999999));
#41468=CARTESIAN_POINT('Ctrl Pts',(52.7854650253443,21.0763836557487,7.69999999999999));
#41469=CARTESIAN_POINT('Ctrl Pts',(52.782744337916,21.1568724422313,7.69999999999999));
#41470=CARTESIAN_POINT('Ctrl Pts',(52.7815199940722,21.1930934168272,7.69999999999998));
#41471=CARTESIAN_POINT('Ctrl Pts',(52.7812498521346,21.2293060564157,7.69999999999999));
#41472=CARTESIAN_POINT('Ctrl Pts',(52.7819483744862,21.2654775510389,7.7));
#41473=CARTESIAN_POINT('Ctrl Pts',(52.7834470595638,21.3430837709493,7.70000000000002));
#41474=CARTESIAN_POINT('Ctrl Pts',(52.7894010863567,21.4205001805428,7.7));
#41475=CARTESIAN_POINT('Ctrl Pts',(52.7995773579842,21.4974758085045,7.7));
#41476=CARTESIAN_POINT('Ctrl Pts',(52.8099658437043,21.5760566720218,7.70000000000001));
#41477=CARTESIAN_POINT('Ctrl Pts',(52.8247546273921,21.6541789515393,7.70000000000002));
#41478=CARTESIAN_POINT('Ctrl Pts',(52.8437496449139,21.731577817109,7.70000000000001));
#41479=CARTESIAN_POINT('Ctrl Pts',(52.8469471737087,21.7446067654141,7.70000000000001));
#41480=CARTESIAN_POINT('Ctrl Pts',(52.8502645099437,21.7576170775422,7.70000000000002));
#41481=CARTESIAN_POINT('Ctrl Pts',(52.8536992928806,21.7706015318293,7.70000000000002));
#41482=CARTESIAN_POINT('Ctrl Pts',(52.8742497443937,21.8482880707327,7.69999999999999));
#41483=CARTESIAN_POINT('Ctrl Pts',(52.8989295562313,21.9247867684672,7.69999999999999));
#41484=CARTESIAN_POINT('Ctrl Pts',(52.9274637506463,21.9998324308231,7.7));
#41485=CARTESIAN_POINT('Ctrl Pts',(52.9569490877993,22.0773796229483,7.70000000000001));
#41486=CARTESIAN_POINT('Ctrl Pts',(52.9905501152123,22.1533761176763,7.70000000000002));
#41487=CARTESIAN_POINT('Ctrl Pts',(53.0280202297069,22.2275323910215,7.70000000000002));
#41488=CARTESIAN_POINT('Ctrl Pts',(53.0654903442015,22.3016886643666,7.70000000000002));
#41489=CARTESIAN_POINT('Ctrl Pts',(53.106829935963,22.3740056157837,7.70000000000001));
#41490=CARTESIAN_POINT('Ctrl Pts',(53.1518443452297,22.4441836503775,7.7));
#41491=CARTESIAN_POINT('Ctrl Pts',(53.1793250417929,22.4870264046308,7.69999999999999));
#41492=CARTESIAN_POINT('Ctrl Pts',(53.2081763082173,22.5290717465152,7.70000000000003));
#41493=CARTESIAN_POINT('Ctrl Pts',(53.238362420557,22.5702474500133,7.70000000000002));
#41494=CARTESIAN_POINT('Ctrl Pts',(53.2465684646758,22.5814409960959,7.70000000000001));
#41495=CARTESIAN_POINT('Ctrl Pts',(53.2548687740561,22.5925641633568,7.70000000000003));
#41496=CARTESIAN_POINT('Ctrl Pts',(53.2632582755064,22.6036104304445,7.70000000000003));
#41497=CARTESIAN_POINT('Ctrl Pts',(53.3152020503275,22.6720036256326,7.70000000000003));
#41498=CARTESIAN_POINT('Ctrl Pts',(53.3706073701717,22.7375134092656,7.70000000000001));
#41499=CARTESIAN_POINT('Ctrl Pts',(53.4292194516112,22.7998424876121,7.70000000000002));
#41500=CARTESIAN_POINT('Ctrl Pts',(53.487892423166,22.8622363175366,7.70000000000003));
#41501=CARTESIAN_POINT('Ctrl Pts',(53.5497792603426,22.9214437654044,7.69999999999998));
#41502=CARTESIAN_POINT('Ctrl Pts',(53.6146732957803,22.9771486789419,7.70000000000001));
#41503=CARTESIAN_POINT('Ctrl Pts',(53.6781671893094,23.0316517133942,7.70000000000003));
#41504=CARTESIAN_POINT('Ctrl Pts',(53.7445404747154,23.0828025035925,7.7));
#41505=CARTESIAN_POINT('Ctrl Pts',(53.8136387438114,23.1302752460601,7.7));
#41506=CARTESIAN_POINT('Ctrl Pts',(53.8499814999668,23.155243893265,7.7));
#41507=CARTESIAN_POINT('Ctrl Pts',(53.8870786806954,23.1791945082043,7.7));
#41508=CARTESIAN_POINT('Ctrl Pts',(53.9249115396487,23.2020751695661,7.7));
#41509=CARTESIAN_POINT('Ctrl Pts',(53.8394226943829,19.3776289326463,7.69906393853165));
#41510=CARTESIAN_POINT('Ctrl Pts',(53.8468827378282,19.3722923254447,7.6993759590211));
#41511=CARTESIAN_POINT('Ctrl Pts',(53.8543795903139,19.3670071736118,7.69968797951055));
#41512=CARTESIAN_POINT('Ctrl Pts',(53.8619125385576,19.3617739799992,7.7));
#41513=CARTESIAN_POINT('Origin',(55.,21.,7.7));
#41514=CARTESIAN_POINT('',(56.1178200348344,23.1806945269163,7.7));
#41515=CARTESIAN_POINT('',(57.4505,21.,7.7));
#41516=CARTESIAN_POINT('Origin',(55.,21.,7.7));
#41517=CARTESIAN_POINT('Ctrl Pts',(56.1178200348344,23.1806945269163,7.70000000000001));
#41518=CARTESIAN_POINT('Ctrl Pts',(56.1536233275691,23.1582395113502,7.7));
#41519=CARTESIAN_POINT('Ctrl Pts',(56.188767358605,23.1348032560045,7.69999999999999));
#41520=CARTESIAN_POINT('Ctrl Pts',(56.2232064725664,23.1103828446799,7.7));
#41521=CARTESIAN_POINT('Ctrl Pts',(56.2929518967896,23.0609271023095,7.7));
#41522=CARTESIAN_POINT('Ctrl Pts',(56.3598088918619,23.0074368937122,7.70000000000002));
#41523=CARTESIAN_POINT('Ctrl Pts',(56.4236072141696,22.9502772007722,7.70000000000002));
#41524=CARTESIAN_POINT('Ctrl Pts',(56.4555381659656,22.9216688716826,7.70000000000002));
#41525=CARTESIAN_POINT('Ctrl Pts',(56.4867022725918,22.8921408163768,7.70000000000001));
#41526=CARTESIAN_POINT('Ctrl Pts',(56.5170740148072,22.861736276879,7.70000000000001));
#41527=CARTESIAN_POINT('Ctrl Pts',(56.5334666656307,22.845325924259,7.70000000000001));
#41528=CARTESIAN_POINT('Ctrl Pts',(56.5496284408635,22.8286602173332,7.7));
#41529=CARTESIAN_POINT('Ctrl Pts',(56.5655549643951,22.8117458184104,7.7));
#41530=CARTESIAN_POINT('Ctrl Pts',(56.5758872739768,22.800772626068,7.69999999999999));
#41531=CARTESIAN_POINT('Ctrl Pts',(56.5861181057108,22.7896973004763,7.70000000000001));
#41532=CARTESIAN_POINT('Ctrl Pts',(56.5962408500655,22.7785280899325,7.70000000000001));
#41533=CARTESIAN_POINT('Ctrl Pts',(56.6532768133754,22.7155958790167,7.70000000000001));
#41534=CARTESIAN_POINT('Ctrl Pts',(56.70693971914,22.6496274807739,7.7));
#41535=CARTESIAN_POINT('Ctrl Pts',(56.7570610656381,22.5809809569958,7.69999999999999));
#41536=CARTESIAN_POINT('Ctrl Pts',(56.7959095405622,22.5277738318097,7.69999999999999));
#41537=CARTESIAN_POINT('Ctrl Pts',(56.8326295718789,22.4729569792761,7.70000000000001));
#41538=CARTESIAN_POINT('Ctrl Pts',(56.8671226775623,22.4166891996158,7.70000000000001));
#41539=CARTESIAN_POINT('Ctrl Pts',(56.8834054025986,22.39012757907,7.70000000000001));
#41540=CARTESIAN_POINT('Ctrl Pts',(56.899191619411,22.3632425685576,7.70000000000001));
#41541=CARTESIAN_POINT('Ctrl Pts',(56.9144695005957,22.3360506410446,7.7));
#41542=CARTESIAN_POINT('Ctrl Pts',(56.9213021800373,22.3238896795965,7.7));
#41543=CARTESIAN_POINT('Ctrl Pts',(56.9280331733587,22.3116673301508,7.70000000000001));
#41544=CARTESIAN_POINT('Ctrl Pts',(56.9346613588346,22.299385064033,7.70000000000001));
#41545=CARTESIAN_POINT('Ctrl Pts',(56.9413081562691,22.2870683092863,7.7));
#41546=CARTESIAN_POINT('Ctrl Pts',(56.9478467935192,22.2747001384903,7.7));
#41547=CARTESIAN_POINT('Ctrl Pts',(56.9542762249967,22.2622829412227,7.7));
#41548=CARTESIAN_POINT('Ctrl Pts',(56.9924776523494,22.1885043091617,7.70000000000001));
#41549=CARTESIAN_POINT('Ctrl Pts',(57.0268325187052,22.1129874340337,7.70000000000002));
#41550=CARTESIAN_POINT('Ctrl Pts',(57.0571793379516,22.0360626483818,7.70000000000002));
#41551=CARTESIAN_POINT('Ctrl Pts',(57.0868760352299,21.9607858276332,7.70000000000002));
#41552=CARTESIAN_POINT('Ctrl Pts',(57.1127347053609,21.8841598409799,7.70000000000001));
#41553=CARTESIAN_POINT('Ctrl Pts',(57.1345559806643,21.8064859127151,7.7));
#41554=CARTESIAN_POINT('Ctrl Pts',(57.1559121045188,21.730467714456,7.69999999999999));
#41555=CARTESIAN_POINT('Ctrl Pts',(57.1734012228511,21.6534450032609,7.70000000000001));
#41556=CARTESIAN_POINT('Ctrl Pts',(57.1867882744522,21.5757044772605,7.70000000000002));
#41557=CARTESIAN_POINT('Ctrl Pts',(57.1927334778934,21.5411798293788,7.70000000000003));
#41558=CARTESIAN_POINT('Ctrl Pts',(57.1978689951837,21.5065137364553,7.7));
#41559=CARTESIAN_POINT('Ctrl Pts',(57.2021710133261,21.4717321844435,7.7));
#41560=CARTESIAN_POINT('Ctrl Pts',(57.2038280264685,21.4583353351305,7.7));
#41561=CARTESIAN_POINT('Ctrl Pts',(57.20536138141,21.4449203597091,7.7));
#41562=CARTESIAN_POINT('Ctrl Pts',(57.2067681334423,21.4315055814218,7.7));
#41563=CARTESIAN_POINT('Ctrl Pts',(57.2149185872068,21.3537829070064,7.69999999999999));
#41564=CARTESIAN_POINT('Ctrl Pts',(57.2188406380943,21.2759353641072,7.7));
#41565=CARTESIAN_POINT('Ctrl Pts',(57.218357164912,21.1982424679639,7.69999999999999));
#41566=CARTESIAN_POINT('Ctrl Pts',(57.2181643246661,21.1672535367307,7.69999999999999));
#41567=CARTESIAN_POINT('Ctrl Pts',(57.2172700275202,21.1362892430631,7.69999999999999));
#41568=CARTESIAN_POINT('Ctrl Pts',(57.2156607144632,21.1053676362415,7.7));
#41569=CARTESIAN_POINT('Ctrl Pts',(57.2115281138556,21.0259631657548,7.70000000000001));
#41570=CARTESIAN_POINT('Ctrl Pts',(57.2026838747762,20.9468386113069,7.70000000000001));
#41571=CARTESIAN_POINT('Ctrl Pts',(57.1893169135748,20.8683173591924,7.70000000000001));
#41572=CARTESIAN_POINT('Ctrl Pts',(57.1763427050985,20.7921032459471,7.70000000000002));
#41573=CARTESIAN_POINT('Ctrl Pts',(57.1591068601941,20.7164568346722,7.70000000000001));
#41574=CARTESIAN_POINT('Ctrl Pts',(57.1377429730716,20.64169976062,7.7));
#41575=CARTESIAN_POINT('Ctrl Pts',(57.1328095664832,20.6244366549156,7.7));
#41576=CARTESIAN_POINT('Ctrl Pts',(57.1276540190574,20.6072155631192,7.70000000000002));
#41577=CARTESIAN_POINT('Ctrl Pts',(57.1222879460442,20.59007204879,7.70000000000002));
#41578=CARTESIAN_POINT('Ctrl Pts',(57.0990729898313,20.5159049747478,7.7));
#41579=CARTESIAN_POINT('Ctrl Pts',(57.0718976926733,20.4430944616305,7.70000000000001));
#41580=CARTESIAN_POINT('Ctrl Pts',(57.0409657230395,20.3719309959309,7.70000000000001));
#41581=CARTESIAN_POINT('Ctrl Pts',(57.0101386747369,20.3010089169146,7.70000000000001));
#41582=CARTESIAN_POINT('Ctrl Pts',(56.9755797145763,20.2317219276503,7.69999999999998));
#41583=CARTESIAN_POINT('Ctrl Pts',(56.9374482924625,20.1643863607663,7.69999999999998));
#41584=CARTESIAN_POINT('Ctrl Pts',(56.8996354441195,20.0976133573605,7.69999999999998));
#41585=CARTESIAN_POINT('Ctrl Pts',(56.8583089214272,20.0327585902461,7.69999999999998));
#41586=CARTESIAN_POINT('Ctrl Pts',(56.813592673895,19.9701701334681,7.70000000000001));
#41587=CARTESIAN_POINT('Ctrl Pts',(56.7965173240937,19.9462701004379,7.70000000000002));
#41588=CARTESIAN_POINT('Ctrl Pts',(56.7789474160572,19.9227010037022,7.70000000000001));
#41589=CARTESIAN_POINT('Ctrl Pts',(56.7608889259661,19.8994840987326,7.7));
#41590=CARTESIAN_POINT('Ctrl Pts',(56.7532705735319,19.8896895608949,7.7));
#41591=CARTESIAN_POINT('Ctrl Pts',(56.7455650804365,19.8799576251608,7.69999999999999));
#41592=CARTESIAN_POINT('Ctrl Pts',(56.7377822767593,19.8703012259636,7.69999999999999));
#41593=CARTESIAN_POINT('Ctrl Pts',(56.6906318007196,19.8117999662811,7.7));
#41594=CARTESIAN_POINT('Ctrl Pts',(56.6405649027111,19.755961680436,7.69999999999998));
#41595=CARTESIAN_POINT('Ctrl Pts',(56.5877351390234,19.7030735504476,7.69999999999999));
#41596=CARTESIAN_POINT('Ctrl Pts',(56.5363803686456,19.6516620433412,7.7));
#41597=CARTESIAN_POINT('Ctrl Pts',(56.482414165105,19.6030378011168,7.7));
#41598=CARTESIAN_POINT('Ctrl Pts',(56.4259516963983,19.5575050942091,7.7));
#41599=CARTESIAN_POINT('Ctrl Pts',(56.3702806307515,19.5126105939615,7.7));
#41600=CARTESIAN_POINT('Ctrl Pts',(56.3121822465846,19.470721107261,7.69999999999999));
#41601=CARTESIAN_POINT('Ctrl Pts',(56.2517503094704,19.4321750581638,7.69999999999998));
#41602=CARTESIAN_POINT('Ctrl Pts',(56.2218511525908,19.4131041095217,7.69999999999997));
#41603=CARTESIAN_POINT('Ctrl Pts',(56.1913805690498,19.394852353254,7.69999999999999));
#41604=CARTESIAN_POINT('Ctrl Pts',(56.1603489846691,19.3774656255483,7.7));
#41605=CARTESIAN_POINT('Origin',(55.,21.,7.7));
#41606=CARTESIAN_POINT('Ctrl Pts',(56.4264070134832,19.0036827380914,7.43505745955369));
#41607=CARTESIAN_POINT('Ctrl Pts',(57.0906234180576,19.4782451892435,7.47741949721597));
#41608=CARTESIAN_POINT('Ctrl Pts',(57.8961547049334,21.13426194966,7.56212596644791));
#41609=CARTESIAN_POINT('Ctrl Pts',(56.4549014799736,23.5108937710809,7.68917686724951));
#41610=CARTESIAN_POINT('Ctrl Pts',(53.6801846690842,23.5816210589062,7.8162101619585));
#41611=CARTESIAN_POINT('Ctrl Pts',(52.1146727379514,21.2920254590205,7.94324345666747));
#41612=CARTESIAN_POINT('Ctrl Pts',(53.190410041307,18.7333910992113,8.07027675137646));
#41613=CARTESIAN_POINT('Ctrl Pts',(55.923149040188,18.2508190898123,8.19731004608543));
#41614=CARTESIAN_POINT('Ctrl Pts',(57.8105805181925,20.2848403969102,8.32434334079443));
#41615=CARTESIAN_POINT('Ctrl Pts',(57.1248247841991,22.9738538538107,8.45137663550339));
#41616=CARTESIAN_POINT('Ctrl Pts',(54.4936428464113,23.8555787817053,8.57840993021239));
#41617=CARTESIAN_POINT('Ctrl Pts',(52.3260744517511,22.122918854144,8.70544322492136));
#41618=CARTESIAN_POINT('Ctrl Pts',(52.6066278141553,19.3621336254897,8.83247651963035));
#41619=CARTESIAN_POINT('Ctrl Pts',(55.0784521557293,18.1009225745723,8.95950981433934));
#41620=CARTESIAN_POINT('Ctrl Pts',(57.478447118452,19.4939723991015,9.0865431090483));
#41621=CARTESIAN_POINT('Ctrl Pts',(57.6092851715724,22.2658793094417,9.2135764037573));
#41622=CARTESIAN_POINT('Ctrl Pts',(55.3511751536352,23.878800370662,9.34060969846627));
#41623=CARTESIAN_POINT('Ctrl Pts',(52.7715447710963,22.8560185838881,9.46764299317526));
#41624=CARTESIAN_POINT('Ctrl Pts',(52.2321905331791,20.1339467082752,9.59467628788425));
#41625=CARTESIAN_POINT('Ctrl Pts',(54.2269218321233,18.2047956751683,9.72170958259321));
#41626=CARTESIAN_POINT('Ctrl Pts',(56.9294497022423,18.8348115048152,9.84874287730221));
#41627=CARTESIAN_POINT('Ctrl Pts',(57.8654577101017,21.4471794295255,9.97577617201117));
#41628=CARTESIAN_POINT('Ctrl Pts',(56.1779777751286,23.6501293622297,10.1028094667202));
#41629=CARTESIAN_POINT('Ctrl Pts',(53.4119928410238,23.4267366111919,10.2298427614291));
#41630=CARTESIAN_POINT('Ctrl Pts',(52.0999179046356,20.9815297946576,10.3568760561381));
#41631=CARTESIAN_POINT('Ctrl Pts',(53.4430314779032,18.5532334963378,10.4839093508471));
#41632=CARTESIAN_POINT('Ctrl Pts',(56.211637430355,18.3650897462597,10.6109426455561));
#41633=CARTESIAN_POINT('Ctrl Pts',(57.8709210689259,20.5893547487726,10.737975940265));
#41634=CARTESIAN_POINT('Ctrl Pts',(56.9017147611579,23.1895886081475,10.865009234974));
#41635=CARTESIAN_POINT('Ctrl Pts',(54.1913814736041,23.7851307662754,10.992042529683));
#41636=CARTESIAN_POINT('Ctrl Pts',(52.2213839931885,21.8307288323652,11.119075824392));
#41637=CARTESIAN_POINT('Ctrl Pts',(52.7953659754236,19.1157478608594,11.246109119101));
#41638=CARTESIAN_POINT('Ctrl Pts',(55.3878145854162,18.1259058551238,11.37314241381));
#41639=CARTESIAN_POINT('Ctrl Pts',(57.6251970984125,19.7674589253413,11.5001757085189));
#41640=CARTESIAN_POINT('Ctrl Pts',(57.4590638008941,22.5374727735356,11.6272090032279));
#41641=CARTESIAN_POINT('Ctrl Pts',(55.0415190843716,23.8998436978354,11.7542422979369));
#41642=CARTESIAN_POINT('Ctrl Pts',(52.5859613075013,22.6072443800978,11.8812755926459));
#41643=CARTESIAN_POINT('Ctrl Pts',(52.3405919268156,19.8431223026964,12.0083088873549));
#41644=CARTESIAN_POINT('Ctrl Pts',(54.5300604310133,18.1381869194969,12.1353421820638));
#41645=CARTESIAN_POINT('Ctrl Pts',(57.149785080446,19.0534026060509,12.2623754767728));
#41646=CARTESIAN_POINT('Ctrl Pts',(57.801260399884,21.750837850857,12.3894087714818));
#41647=CARTESIAN_POINT('Ctrl Pts',(55.8880240393673,23.7608387514926,12.5164420661908));
#41648=CARTESIAN_POINT('Ctrl Pts',(53.1617516519464,23.2431362680666,12.6434753608998));
#41649=CARTESIAN_POINT('Ctrl Pts',(52.1184991683894,20.671716184278,12.7705086556088));
#41650=CARTESIAN_POINT('Ctrl Pts',(53.7134229996573,18.400858424705,12.8975419503177));
#41651=CARTESIAN_POINT('Ctrl Pts',(56.4862805425061,18.5096611766257,13.0245752450267));
#41652=CARTESIAN_POINT('Ctrl Pts',(57.8983645324169,20.8985093922302,13.1516085397357));
#41653=CARTESIAN_POINT('Ctrl Pts',(56.6568325395494,23.3802779758105,13.2786418344447));
#41654=CARTESIAN_POINT('Ctrl Pts',(53.8983770339348,23.6827680009414,13.4056751291537));
#41655=CARTESIAN_POINT('Ctrl Pts',(52.1485194037946,21.5290328115554,13.5327084238626));
#41656=CARTESIAN_POINT('Ctrl Pts',(53.0093528720454,18.8909382848755,13.6597417185716));
#41657=CARTESIAN_POINT('Ctrl Pts',(55.6927359111768,18.1838085534531,13.7867750132806));
#41658=CARTESIAN_POINT('Ctrl Pts',(57.7418802045661,20.0550607162118,13.9138083079896));
#41659=CARTESIAN_POINT('Ctrl Pts',(57.2806787314646,22.7914580179515,14.0408416026986));
#41660=CARTESIAN_POINT('Ctrl Pts',(54.7313874181419,23.887674598549,14.1678748974076));
#41661=CARTESIAN_POINT('Ctrl Pts',(52.4280260533891,22.3400624329458,14.2949081921165));
#41662=CARTESIAN_POINT('Ctrl Pts',(52.4794517058251,19.5655476295917,14.4219414868255));
#41663=CARTESIAN_POINT('Ctrl Pts',(54.8385812940423,18.1043547683453,14.5489747815345));
#41664=CARTESIAN_POINT('Ctrl Pts',(57.3454987996377,19.2942882168619,14.6760080762435));
#41665=CARTESIAN_POINT('Ctrl Pts',(57.7049800415428,22.0458968788046,14.8030413709524));
#41666=CARTESIAN_POINT('Ctrl Pts',(55.5878996946444,23.8399280369887,14.9300746656615));
#41667=CARTESIAN_POINT('Ctrl Pts',(52.9325640632467,23.0338451154545,15.0571079603704));
#41668=CARTESIAN_POINT('Ctrl Pts',(52.1700824823932,20.3656624323127,15.1841412550794));
#41669=CARTESIAN_POINT('Ctrl Pts',(53.9985497869111,18.2782515221016,15.3111745497884));
#41670=CARTESIAN_POINT('Ctrl Pts',(56.7439011692209,18.682754648677,15.4382078444974));
#41671=CARTESIAN_POINT('Ctrl Pts',(57.8926128040896,21.2088264156062,15.5652411392064));
#41672=CARTESIAN_POINT('Ctrl Pts',(56.3929744874356,23.5437058366862,15.6922744339153));
#41673=CARTESIAN_POINT('Ctrl Pts',(53.6179895668198,23.5496792874436,15.8193077286243));
#41674=CARTESIAN_POINT('Ctrl Pts',(52.1083130409334,21.2212777372493,15.9463410233333));
#41675=CARTESIAN_POINT('Ctrl Pts',(53.246138803302,18.6902839549081,16.0733743180423));
#41676=CARTESIAN_POINT('Ctrl Pts',(55.9897232792757,18.2739653089702,16.2004076127513));
#41677=CARTESIAN_POINT('Ctrl Pts',(57.8271603458951,20.353484969366,16.3274409074602));
#41678=CARTESIAN_POINT('Ctrl Pts',(57.0761728731458,23.0249255559283,16.4544742021693));
#41679=CARTESIAN_POINT('Ctrl Pts',(54.424332192468,23.8424327400326,16.5815074968782));
#41680=CARTESIAN_POINT('Ctrl Pts',(52.2995478146647,22.057532647702,16.7085407915872));
#41681=CARTESIAN_POINT('Ctrl Pts',(52.6471795182707,19.3044018497907,16.8355740862962));
#41682=CARTESIAN_POINT('Ctrl Pts',(55.1489508979232,18.1036866646984,16.9626073810052));
#41683=CARTESIAN_POINT('Ctrl Pts',(57.514349340715,19.5547094758896,17.0896406757141));
#41684=CARTESIAN_POINT('Ctrl Pts',(57.5777193387807,22.3289771693728,17.2166739704231));
#41685=CARTESIAN_POINT('Ctrl Pts',(55.2810420895108,23.8864914082951,17.3437072651321));
#41686=CARTESIAN_POINT('Ctrl Pts',(52.7270549773104,22.8012601783385,17.4707405598411));
#41687=CARTESIAN_POINT('Ctrl Pts',(52.2540770593384,20.0668737972888,17.59777385455));
#41688=CARTESIAN_POINT('Ctrl Pts',(54.2951462604641,18.1868170141102,17.7248071492591));
#41689=CARTESIAN_POINT('Ctrl Pts',(56.9815487617436,18.8823877099265,17.851840443968));
#41690=CARTESIAN_POINT('Ctrl Pts',(57.8537317588834,21.5167517339861,17.978873738677));
#41691=CARTESIAN_POINT('Ctrl Pts',(56.1131625914016,23.6780004390108,18.105907033386));
#41692=CARTESIAN_POINT('Ctrl Pts',(53.3534303714686,23.3873889010037,18.232940328095));
#41693=CARTESIAN_POINT('Ctrl Pts',(52.1012253911768,20.9109883520029,18.3599736228039));
#41694=CARTESIAN_POINT('Ctrl Pts',(53.5030118417111,18.5160829804156,18.487006917513));
#41695=CARTESIAN_POINT('Ctrl Pts',(56.2753752705501,18.3953435494279,18.6140402122219));
#41696=CARTESIAN_POINT('Ctrl Pts',(57.8800608023822,20.659313808881,18.7410735069309));
#41697=CARTESIAN_POINT('Ctrl Pts',(56.8478884472591,23.2352014658021,18.8681068016399));
#41698=CARTESIAN_POINT('Ctrl Pts',(54.123870134461,23.7646362807697,18.9951400963489));
#41699=CARTESIAN_POINT('Ctrl Pts',(52.2019980624758,21.7628908597228,19.1221733910578));
#41700=CARTESIAN_POINT('Ctrl Pts',(52.8418543646187,19.0626758859906,19.2492066857668));
#41701=CARTESIAN_POINT('Ctrl Pts',(55.4576145557163,18.1361902603989,19.3762399804758));
#41702=CARTESIAN_POINT('Ctrl Pts',(57.6544028454472,19.8316837584284,19.5032732751848));
#41703=CARTESIAN_POINT('Ctrl Pts',(57.4209358182124,22.5968365822257,19.6303065698938));
#41704=CARTESIAN_POINT('Ctrl Pts',(54.9709656877149,23.8999955715394,19.7573398646027));
#41705=CARTESIAN_POINT('Ctrl Pts',(52.5475781055017,22.5480452698882,19.8843731593118));
#41706=CARTESIAN_POINT('Ctrl Pts',(52.3695209028766,19.7787723284191,20.0114064540207));
#41707=CARTESIAN_POINT('Ctrl Pts',(54.5998154780972,18.1276021071817,20.1384397487297));
#41708=CARTESIAN_POINT('Ctrl Pts',(57.1965015239227,19.1062739475724,20.2654730434386));
#41709=CARTESIAN_POINT('Ctrl Pts',(57.7821667043993,21.81875865502,20.3925063381477));
#41710=CARTESIAN_POINT('Ctrl Pts',(55.8206015586093,23.7816236963769,20.5195396328566));
#41711=CARTESIAN_POINT('Ctrl Pts',(53.1077294646894,23.1977555658974,20.6465729275656));
#41712=CARTESIAN_POINT('Ctrl Pts',(52.1273376299221,20.6017184240057,20.7736062222746));
#41713=CARTESIAN_POINT('Ctrl Pts',(53.7770300006112,18.3703304985544,20.9006395169836));
#41714=CARTESIAN_POINT('Ctrl Pts',(56.5464202907784,18.5465531205044,21.0276728116926));
#41715=CARTESIAN_POINT('Ctrl Pts',(57.8999757010312,20.9690445535407,21.1547061064016));
#41716=CARTESIAN_POINT('Ctrl Pts',(56.5984400128888,23.4198774414078,21.2817394011105));
#41717=CARTESIAN_POINT('Ctrl Pts',(53.8334424591756,23.6551762295908,21.4087726958195));
#41718=CARTESIAN_POINT('Ctrl Pts',(52.1364940416356,21.4595116240631,21.5358059905285));
#41719=CARTESIAN_POINT('Ctrl Pts',(53.0612466188837,18.8431382442427,21.6628392852375));
#41720=CARTESIAN_POINT('Ctrl Pts',(55.7610371188136,18.2014932892656,21.7898725799465));
#41721=CARTESIAN_POINT('Ctrl Pts',(57.7640552702745,20.1220388567222,21.9169058746554));
#41722=CARTESIAN_POINT('Ctrl Pts',(57.2364251335552,22.8464073029103,22.0439391693644));
#41723=CARTESIAN_POINT('Ctrl Pts',(54.6612218181301,23.8802858625016,22.1709724640734));
#41724=CARTESIAN_POINT('Ctrl Pts',(52.3961890102348,22.2771004799217,22.2980057587824));
#41725=CARTESIAN_POINT('Ctrl Pts',(52.5150918257906,19.5046576739809,22.4250390534914));
#41726=CARTESIAN_POINT('Ctrl Pts',(54.9090680398321,18.1012849941988,22.5520723482003));
#41727=CARTESIAN_POINT('Ctrl Pts',(57.3862975852447,19.3518491753185,22.6791056429093));
#41728=CARTESIAN_POINT('Ctrl Pts',(57.6787372807074,22.1113882702183,22.8061389376183));
#41729=CARTESIAN_POINT('Ctrl Pts',(55.5186421130676,23.8533888036486,22.9331722323273));
#41730=CARTESIAN_POINT('Ctrl Pts',(52.883700877855,22.9829511672962,23.0602055270362));
#41731=CARTESIAN_POINT('Ctrl Pts',(52.1863506917035,20.2970100455204,23.1872388217453));
#41732=CARTESIAN_POINT('Ctrl Pts',(54.0650549289335,18.2546958237164,23.3142721164542));
#41733=CARTESIAN_POINT('Ctrl Pts',(56.7997540405474,18.725862207337,23.4413054111632));
#41734=CARTESIAN_POINT('Ctrl Pts',(57.8866769548865,21.2791298333439,23.5683387058722));
#41735=CARTESIAN_POINT('Ctrl Pts',(56.330684522312,23.5768383745275,23.6953720005812));
#41736=CARTESIAN_POINT('Ctrl Pts',(53.5563754567649,23.5153062410116,23.8224052952901));
#41737=CARTESIAN_POINT('Ctrl Pts',(52.1037859754078,21.1508695661785,23.9494385899992));
#41738=CARTESIAN_POINT('Ctrl Pts',(53.3028435633851,18.6483033065475,24.0764718847081));
#41739=CARTESIAN_POINT('Ctrl Pts',(56.0557434678534,18.298847829695,24.2035051794171));
#41740=CARTESIAN_POINT('Ctrl Pts',(57.8420507524862,20.4224493134434,24.3305384741261));
#41741=CARTESIAN_POINT('Ctrl Pts',(57.0263005097603,23.0748309749754,24.4575717688351));
#41742=CARTESIAN_POINT('Ctrl Pts',(54.3553579817675,23.8275880254189,24.5846050635441));
#41743=CARTESIAN_POINT('Ctrl Pts',(52.2746216002963,21.9915289454338,24.711638358253));
#41744=CARTESIAN_POINT('Ctrl Pts',(52.6891225191036,19.2476693185881,24.838671652962));
#41745=CARTESIAN_POINT('Ctrl Pts',(55.2193621970339,18.1081670315388,24.965704947671));
#41746=CARTESIAN_POINT('Ctrl Pts',(57.5487629137497,19.616300909826,25.09273824238));
#41747=CARTESIAN_POINT('Ctrl Pts',(57.5446286265918,22.3912888576387,25.2197715370889));
#41748=CARTESIAN_POINT('Ctrl Pts',(55.2107415367077,23.8924742450603,25.346804831798));
#41749=CARTESIAN_POINT('Ctrl Pts',(52.6839125453877,22.7454350638024,25.4738381265069));
#41750=CARTESIAN_POINT('Ctrl Pts',(52.2775845533845,20.0003546545124,25.6008714212159));
#41751=CARTESIAN_POINT('Ctrl Pts',(54.3637959560076,18.1705002200075,25.7279047159249));
#41752=CARTESIAN_POINT('Ctrl Pts',(57.0324592249323,18.9312232492356,25.8549380106339));
#41753=CARTESIAN_POINT('Ctrl Pts',(57.8403478634403,21.5860063262462,25.9819713053429));
#41754=CARTESIAN_POINT('Ctrl Pts',(56.0476279930325,23.704309837158,26.1090046000518));
#41755=CARTESIAN_POINT('Ctrl Pts',(53.2959609336026,23.3465827680974,26.2360378947608));
#41756=CARTESIAN_POINT('Ctrl Pts',(52.1040166225385,20.8405885662721,26.3630711894698));
#41757=CARTESIAN_POINT('Ctrl Pts',(53.5643317699236,18.480228381185,26.4901044841788));
#41758=CARTESIAN_POINT('Ctrl Pts',(56.337469579789,18.4274808217143,26.6171377788878));
#41759=CARTESIAN_POINT('Ctrl Pts',(57.8892510608654,20.7287913102977,26.7441710735968));
#41760=CARTESIAN_POINT('Ctrl Pts',(56.7893549764862,23.2809819920617,26.8712043683057));
#41761=CARTESIAN_POINT('Ctrl Pts',(54.9737389170402,23.5855482158792,26.9558932314451));
#41762=CARTESIAN_POINT('Ctrl Pts',(54.202107399834,23.3201911685949,26.9982376630147));
#41763=CARTESIAN_POINT('Ctrl Pts',(56.3368004103323,19.1290909890044,7.52404542325027));
#41764=CARTESIAN_POINT('Ctrl Pts',(56.9592908732868,19.5738415219392,7.56640746091254));
#41765=CARTESIAN_POINT('Ctrl Pts',(57.7142188459145,21.1258276408493,7.65111393014448));
#41766=CARTESIAN_POINT('Ctrl Pts',(56.3635048601399,23.3531599268327,7.77816483094608));
#41767=CARTESIAN_POINT('Ctrl Pts',(53.7630952040661,23.41944414059,7.90519812565507));
#41768=CARTESIAN_POINT('Ctrl Pts',(52.295928419175,21.2736804781216,8.03223142036406));
#41769=CARTESIAN_POINT('Ctrl Pts',(53.3040881203977,18.8757790167912,8.15926471507303));
#41770=CARTESIAN_POINT('Ctrl Pts',(55.8651570022134,18.4235220844559,8.28629800978201));
#41771=CARTESIAN_POINT('Ctrl Pts',(57.6340204124606,20.3297665800668,8.41333130449099));
#41772=CARTESIAN_POINT('Ctrl Pts',(56.9913437164512,22.8498567496991,8.54036459919998));
#41773=CARTESIAN_POINT('Ctrl Pts',(54.5254521014734,23.676191894064,8.66739789390895));
#41774=CARTESIAN_POINT('Ctrl Pts',(52.4940499196169,22.0523773164323,8.79443118861795));
#41775=CARTESIAN_POINT('Ctrl Pts',(52.7569789759361,19.4650240633855,8.92146448332691));
#41776=CARTESIAN_POINT('Ctrl Pts',(55.0735238070052,18.2830420383076,9.04849777803592));
#41777=CARTESIAN_POINT('Ctrl Pts',(57.3227515664291,19.588580751621,9.17553107274487));
#41778=CARTESIAN_POINT('Ctrl Pts',(57.4453703992343,22.1863570245358,9.30256436745386));
#41779=CARTESIAN_POINT('Ctrl Pts',(55.329114400757,23.6979547074494,9.42959766216286));
#41780=CARTESIAN_POINT('Ctrl Pts',(52.9115358826433,22.7394238678533,9.55663095687182));
#41781=CARTESIAN_POINT('Ctrl Pts',(52.4060637700227,20.1883520027568,9.68366425158081));
#41782=CARTESIAN_POINT('Ctrl Pts',(54.2754864479299,18.3803898515102,9.81069754628979));
#41783=CARTESIAN_POINT('Ctrl Pts',(56.8082420580466,18.9708282128101,9.93773084099876));
#41784=CARTESIAN_POINT('Ctrl Pts',(57.6854502301555,21.4190877072471,10.0647641357078));
#41785=CARTESIAN_POINT('Ctrl Pts',(56.1039774470183,23.4836487660078,10.1917974304167));
#41786=CARTESIAN_POINT('Ctrl Pts',(53.511751132977,23.2742895028874,10.3188307251257));
#41787=CARTESIAN_POINT('Ctrl Pts',(52.2821004815354,20.9826900892612,10.4458640198347));
#41788=CARTESIAN_POINT('Ctrl Pts',(53.5408399288986,18.7069388784791,10.5728973145437));
#41789=CARTESIAN_POINT('Ctrl Pts',(56.1355226094391,18.5306142811318,10.6999306092526));
#41790=CARTESIAN_POINT('Ctrl Pts',(57.6905703818716,20.6151514012811,10.8269639039617));
#41791=CARTESIAN_POINT('Ctrl Pts',(56.7822494204112,23.052039089939,10.9539971986706));
#41792=CARTESIAN_POINT('Ctrl Pts',(54.2421787276209,23.6101694088663,11.0810304933796));
#41793=CARTESIAN_POINT('Ctrl Pts',(52.3959360947117,21.7785426133519,11.2080637880886));
#41794=CARTESIAN_POINT('Ctrl Pts',(52.9338606436813,19.2341162031854,11.3350970827976));
#41795=CARTESIAN_POINT('Ctrl Pts',(55.3634521507654,18.3064558741743,11.4621303775066));
#41796=CARTESIAN_POINT('Ctrl Pts',(57.4602827420143,19.8448869090094,11.5891636722155));
#41797=CARTESIAN_POINT('Ctrl Pts',(57.3045859050014,22.4408890415635,11.7161969669245));
#41798=CARTESIAN_POINT('Ctrl Pts',(55.0389108637997,23.7176760970207,11.8432302616335));
#41799=CARTESIAN_POINT('Ctrl Pts',(52.7376107350945,22.5062776097633,11.9702635563425));
#41800=CARTESIAN_POINT('Ctrl Pts',(52.5076554098029,19.9157971281401,12.0972968510515));
#41801=CARTESIAN_POINT('Ctrl Pts',(54.5595819406981,18.3179654445409,12.2243301457604));
#41802=CARTESIAN_POINT('Ctrl Pts',(57.0147360118826,19.1756874648082,12.3513634404694));
#41803=CARTESIAN_POINT('Ctrl Pts',(57.6252857821193,21.7036703673151,12.4783967351784));
#41804=CARTESIAN_POINT('Ctrl Pts',(55.8322385469154,23.5874034135911,12.6054300298874));
#41805=CARTESIAN_POINT('Ctrl Pts',(53.2772300453221,23.1022228965773,12.7324633245964));
#41806=CARTESIAN_POINT('Ctrl Pts',(52.2995144740184,20.6923389078893,12.8594966193053));
#41807=CARTESIAN_POINT('Ctrl Pts',(53.7942455093638,18.5641359783547,12.9865299140143));
#41808=CARTESIAN_POINT('Ctrl Pts',(56.3929126962432,18.6661037631722,13.1135632087233));
#41809=CARTESIAN_POINT('Ctrl Pts',(57.7162898524779,20.9048850119012,13.2405965034323));
#41810=CARTESIAN_POINT('Ctrl Pts',(56.5527506509611,23.2307493896838,13.3676297981413));
#41811=CARTESIAN_POINT('Ctrl Pts',(53.9675807682189,23.5142370519669,13.4946630928503));
#41812=CARTESIAN_POINT('Ctrl Pts',(52.3276488442428,21.4957990761975,13.6216963875592));
#41813=CARTESIAN_POINT('Ctrl Pts',(53.1344049262782,19.0234291197785,13.7487296822682));
#41814=CARTESIAN_POINT('Ctrl Pts',(55.649218379859,18.3607211365814,13.8757629769772));
#41815=CARTESIAN_POINT('Ctrl Pts',(57.5696358387888,20.114421612929,14.0027962716862));
#41816=CARTESIAN_POINT('Ctrl Pts',(57.1374069499372,22.6789189837497,14.1298295663952));
#41817=CARTESIAN_POINT('Ctrl Pts',(54.7482616067825,23.7062714581164,14.2568628611041));
#41818=CARTESIAN_POINT('Ctrl Pts',(52.5895969420414,22.255879979066,14.3838961558131));
#41819=CARTESIAN_POINT('Ctrl Pts',(52.6377920452821,19.6556596404547,14.5109294505221));
#41820=CARTESIAN_POINT('Ctrl Pts',(54.8487215848493,18.2862586223546,14.6379627452311));
#41821=CARTESIAN_POINT('Ctrl Pts',(57.1981550343987,19.4014406897513,14.7649960399401));
#41822=CARTESIAN_POINT('Ctrl Pts',(57.5350537366225,21.9801938461708,14.8920293346491));
#41823=CARTESIAN_POINT('Ctrl Pts',(55.5509679534706,23.6615243259989,15.019062629358));
#41824=CARTESIAN_POINT('Ctrl Pts',(53.062439975082,22.9060793722914,15.146095924067));
#41825=CARTESIAN_POINT('Ctrl Pts',(52.3478573345588,20.4055113913785,15.273129218776));
#41826=CARTESIAN_POINT('Ctrl Pts',(54.0614606888986,18.4492312168382,15.400162513485));
#41827=CARTESIAN_POINT('Ctrl Pts',(56.6343496467399,18.8283235379467,15.527195808194));
#41828=CARTESIAN_POINT('Ctrl Pts',(57.7108994465729,21.1957079819658,15.654229102903));
#41829=CARTESIAN_POINT('Ctrl Pts',(56.305468108881,23.3839107450426,15.7812623976119));
#41830=CARTESIAN_POINT('Ctrl Pts',(53.7048071856801,23.3895089448189,15.9082956923209));
#41831=CARTESIAN_POINT('Ctrl Pts',(52.2899682370509,21.2073771140749,16.0353289870299));
#41832=CARTESIAN_POINT('Ctrl Pts',(53.3563160127161,18.835379854667,16.1623622817389));
#41833=CARTESIAN_POINT('Ctrl Pts',(55.9275490609236,18.4452142627581,16.2893955764478));
#41834=CARTESIAN_POINT('Ctrl Pts',(57.6495586987047,20.3940989142172,16.4164288711569));
#41835=CARTESIAN_POINT('Ctrl Pts',(56.9457481087146,22.8977201377096,16.5434621658658));
#41836=CARTESIAN_POINT('Ctrl Pts',(54.4604955289412,23.6638716840987,16.6704954605748));
#41837=CARTESIAN_POINT('Ctrl Pts',(52.4691896805641,21.9910986583945,16.7975287552838));
#41838=CARTESIAN_POINT('Ctrl Pts',(52.7949832301137,19.4109189862833,16.9245620499928));
#41839=CARTESIAN_POINT('Ctrl Pts',(55.1395938323219,18.2856324888452,17.0515953447017));
#41840=CARTESIAN_POINT('Ctrl Pts',(57.3563984182741,19.6455023373993,17.1786286394107));
#41841=CARTESIAN_POINT('Ctrl Pts',(57.4157875257419,22.2454910895324,17.3056619341197));
#41842=CARTESIAN_POINT('Ctrl Pts',(55.2633870816867,23.7051625956373,17.4326952288287));
#41843=CARTESIAN_POINT('Ctrl Pts',(52.8698409288001,22.6881053743827,17.5597285235377));
#41844=CARTESIAN_POINT('Ctrl Pts',(52.4265753889884,20.1254925986166,17.6867618182466));
#41845=CARTESIAN_POINT('Ctrl Pts',(54.3394250313344,18.363540606342,17.8137951129556));
#41846=CARTESIAN_POINT('Ctrl Pts',(56.8570682650556,19.0154156902367,17.9408284076646));
#41847=CARTESIAN_POINT('Ctrl Pts',(57.6744609008463,21.4842894934635,18.0678617023736));
#41848=CARTESIAN_POINT('Ctrl Pts',(56.043233940163,23.5097689873227,18.1948949970826));
#41849=CARTESIAN_POINT('Ctrl Pts',(53.4568675460404,23.2374136079795,18.3219282917916));
#41850=CARTESIAN_POINT('Ctrl Pts',(52.2833258320335,20.9165800459181,18.4489615865005));
#41851=CARTESIAN_POINT('Ctrl Pts',(53.5970523382548,18.6721221505331,18.5759948812095));
#41852=CARTESIAN_POINT('Ctrl Pts',(56.1952564512676,18.558967546439,18.7030281759185));
#41853=CARTESIAN_POINT('Ctrl Pts',(57.6991359591011,20.6807156472329,18.8300614706275));
#41854=CARTESIAN_POINT('Ctrl Pts',(56.7318044647805,23.0947865570032,18.9570947653365));
#41855=CARTESIAN_POINT('Ctrl Pts',(54.178908437293,23.590962382839,19.0841280600455));
#41856=CARTESIAN_POINT('Ctrl Pts',(52.3777679842871,21.7149662085759,19.2111613547544));
#41857=CARTESIAN_POINT('Ctrl Pts',(52.9774286415701,19.1843781991577,19.3381946494634));
#41858=CARTESIAN_POINT('Ctrl Pts',(55.4288673008988,18.316094215168,19.4652279441724));
#41859=CARTESIAN_POINT('Ctrl Pts',(57.4876537898647,19.905077150934,19.5922612388814));
#41860=CARTESIAN_POINT('Ctrl Pts',(57.268853114562,22.4965236276708,19.7192945335903));
#41861=CARTESIAN_POINT('Ctrl Pts',(54.9727896174025,23.7178184300489,19.8463278282993));
#41862=CARTESIAN_POINT('Ctrl Pts',(52.7016387581638,22.4507973758109,19.9733611230083));
#41863=CARTESIAN_POINT('Ctrl Pts',(52.5347670733767,19.8554896063698,20.1003944177173));
#41864=CARTESIAN_POINT('Ctrl Pts',(54.6249549896826,18.3080455680173,20.2274277124263));
#41865=CARTESIAN_POINT('Ctrl Pts',(57.0585177377285,19.2252374392353,20.3544610071353));
#41866=CARTESIAN_POINT('Ctrl Pts',(57.6073915487639,21.7673244001521,20.4814943018443));
#41867=CARTESIAN_POINT('Ctrl Pts',(55.7690515329069,23.6068826523971,20.6085275965532));
#41868=CARTESIAN_POINT('Ctrl Pts',(53.2266015210582,23.0596930010373,20.7355608912622));
#41869=CARTESIAN_POINT('Ctrl Pts',(52.3077977051663,20.6267383929101,20.8625941859712));
#41870=CARTESIAN_POINT('Ctrl Pts',(53.8538567312461,18.5355258104161,20.9896274806802));
#41871=CARTESIAN_POINT('Ctrl Pts',(56.4492744775635,18.7006781625187,21.1166607753892));
#41872=CARTESIAN_POINT('Ctrl Pts',(57.7177998078022,20.9709891684928,21.2436940700982));
#41873=CARTESIAN_POINT('Ctrl Pts',(56.4980263311406,23.2678612247765,21.3707273648071));
#41874=CARTESIAN_POINT('Ctrl Pts',(53.9067253704522,23.4883785901712,21.4977606595161));
#41875=CARTESIAN_POINT('Ctrl Pts',(52.3163789129282,21.4306451957916,21.6247939542251));
#41876=CARTESIAN_POINT('Ctrl Pts',(53.1830387183245,18.9786318681331,21.7518272489341));
#41877=CARTESIAN_POINT('Ctrl Pts',(55.7132289192997,18.377294920829,21.8788605436431));
#41878=CARTESIAN_POINT('Ctrl Pts',(57.5904178713067,20.1771922000554,22.005893838352));
#41879=CARTESIAN_POINT('Ctrl Pts',(57.0959333541929,22.7304163656232,22.132927133061));
#41880=CARTESIAN_POINT('Ctrl Pts',(54.6825037957228,23.6993468809889,22.25996042777));
#41881=CARTESIAN_POINT('Ctrl Pts',(52.5597598955672,22.1968732833317,22.386993722479));
#41882=CARTESIAN_POINT('Ctrl Pts',(52.6711932600432,19.5985947796707,22.514027017188));
#41883=CARTESIAN_POINT('Ctrl Pts',(54.9147803673736,18.2833816908058,22.6410603118969));
#41884=CARTESIAN_POINT('Ctrl Pts',(57.236390848458,19.455385680316,22.7680936066059));
#41885=CARTESIAN_POINT('Ctrl Pts',(57.5104595407713,22.0415710814815,22.8951269013149));
#41886=CARTESIAN_POINT('Ctrl Pts',(55.4860611193094,23.6741394899906,23.0221601960239));
#41887=CARTESIAN_POINT('Ctrl Pts',(53.0166463652187,22.858382571772,23.1491934907328));
#41888=CARTESIAN_POINT('Ctrl Pts',(52.3631035782157,20.3411717337866,23.2762267854419));
#41889=CARTESIAN_POINT('Ctrl Pts',(54.1237879912074,18.4271552827118,23.4032600801508));
#41890=CARTESIAN_POINT('Ctrl Pts',(56.6866938518662,18.8687230883979,23.5302933748598));
#41891=CARTESIAN_POINT('Ctrl Pts',(57.7053364862291,21.2615949530694,23.6573266695688));
#41892=CARTESIAN_POINT('Ctrl Pts',(56.2470911869016,23.4149619034869,23.7843599642777));
#41893=CARTESIAN_POINT('Ctrl Pts',(53.6470636616895,23.3572952062854,23.9113932589868));
#41894=CARTESIAN_POINT('Ctrl Pts',(52.2857255608756,21.1413919702215,24.0384265536957));
#41895=CARTESIAN_POINT('Ctrl Pts',(53.4094585911178,18.7960364222356,24.1654598484047));
#41896=CARTESIAN_POINT('Ctrl Pts',(55.9894218744662,18.4685336685102,24.2924931431137));
#41897=CARTESIAN_POINT('Ctrl Pts',(57.6635136929334,20.458730932,24.4195264378227));
#41898=CARTESIAN_POINT('Ctrl Pts',(56.8990087172171,22.9444905083188,24.5465597325316));
#41899=CARTESIAN_POINT('Ctrl Pts',(54.3958542643545,23.6499595114864,24.6735930272407));
#41900=CARTESIAN_POINT('Ctrl Pts',(52.4458293259943,21.9292412954949,24.8006263219496));
#41901=CARTESIAN_POINT('Ctrl Pts',(52.8342913800274,19.3577503813382,24.9276596166586));
#41902=CARTESIAN_POINT('Ctrl Pts',(55.2055819077125,18.2898313999373,25.0546929113676));
#41903=CARTESIAN_POINT('Ctrl Pts',(57.388650137537,19.7032246097807,25.1817262060766));
#41904=CARTESIAN_POINT('Ctrl Pts',(57.384775565471,22.3038883700105,25.3087595007855));
#41905=CARTESIAN_POINT('Ctrl Pts',(55.1975027955429,23.7107695917942,25.4357927954946));
#41906=CARTESIAN_POINT('Ctrl Pts',(52.8294086958177,22.6357871823707,25.5628260902035));
#41907=CARTESIAN_POINT('Ctrl Pts',(52.4486061469625,20.0631521750783,25.6898593849125));
#41908=CARTESIAN_POINT('Ctrl Pts',(54.4037621667412,18.3482488299797,25.8168926796215));
#41909=CARTESIAN_POINT('Ctrl Pts',(56.9047805431344,19.0611833907388,25.9439259743305));
#41910=CARTESIAN_POINT('Ctrl Pts',(57.6619177790366,21.5491935260962,26.0709592690394));
#41911=CARTESIAN_POINT('Ctrl Pts',(55.9818162121494,23.5344256343431,26.1979925637484));
#41912=CARTESIAN_POINT('Ctrl Pts',(53.403008326761,23.1991709081766,26.3250258584574));
#41913=CARTESIAN_POINT('Ctrl Pts',(52.2859417187998,20.8506027606393,26.4520591531664));
#41914=CARTESIAN_POINT('Ctrl Pts',(53.6545201608476,18.6385199300512,26.5790924478753));
#41915=CARTESIAN_POINT('Ctrl Pts',(56.2534500084256,18.5890859617113,26.7061257425844));
#41916=CARTESIAN_POINT('Ctrl Pts',(57.7077488873855,20.7458285859136,26.8331590372933));
#41917=CARTESIAN_POINT('Ctrl Pts',(56.6769480549284,23.1376911597642,26.9601923320024));
#41918=CARTESIAN_POINT('Ctrl Pts',(54.9753886330167,23.4231245943478,27.0448811951416));
#41919=CARTESIAN_POINT('Ctrl Pts',(54.2522308533113,23.1744372236737,27.0872256267113));
#41920=CARTESIAN_POINT('Ctrl Pts',(56.2471938071815,19.2544992399175,7.61303338694684));
#41921=CARTESIAN_POINT('Ctrl Pts',(56.8279583285158,19.6694378546349,7.65539542460912));
#41922=CARTESIAN_POINT('Ctrl Pts',(57.5322829868957,21.1173933320387,7.74010189384106));
#41923=CARTESIAN_POINT('Ctrl Pts',(56.2721082403061,23.1954260825845,7.86715279464267));
#41924=CARTESIAN_POINT('Ctrl Pts',(53.846005739048,23.2572672222738,7.99418608935165));
#41925=CARTESIAN_POINT('Ctrl Pts',(52.4771841003984,21.2553354972227,8.12121938406063));
#41926=CARTESIAN_POINT('Ctrl Pts',(53.4177661994886,19.0181669343711,8.2482526787696));
#41927=CARTESIAN_POINT('Ctrl Pts',(55.8071649642388,18.5962250790995,8.37528597347859));
#41928=CARTESIAN_POINT('Ctrl Pts',(57.4574603067288,20.3746927632235,8.50231926818757));
#41929=CARTESIAN_POINT('Ctrl Pts',(56.8578626487033,22.7258596455877,8.62935256289655));
#41930=CARTESIAN_POINT('Ctrl Pts',(54.5572613565354,23.4968050064229,8.75638585760554));
#41931=CARTESIAN_POINT('Ctrl Pts',(52.6620253874827,21.9818357787205,8.88341915231452));
#41932=CARTESIAN_POINT('Ctrl Pts',(52.9073301377167,19.5679145012814,9.01045244702349));
#41933=CARTESIAN_POINT('Ctrl Pts',(55.0685954582813,18.465161502043,9.13748574173249));
#41934=CARTESIAN_POINT('Ctrl Pts',(57.1670560144063,19.6831891041406,9.26451903644145));
#41935=CARTESIAN_POINT('Ctrl Pts',(57.2814556268961,22.1068347396299,9.39155233115045));
#41936=CARTESIAN_POINT('Ctrl Pts',(55.3070536478788,23.5171090442367,9.51858562585943));
#41937=CARTESIAN_POINT('Ctrl Pts',(53.0515269941901,22.6228291518185,9.6456189205684));
#41938=CARTESIAN_POINT('Ctrl Pts',(52.5799370068662,20.2427572972383,9.7726522152774));
#41939=CARTESIAN_POINT('Ctrl Pts',(54.3240510637364,18.5559840278521,9.89968550998636));
#41940=CARTESIAN_POINT('Ctrl Pts',(56.687034413851,19.106844920805,10.0267188046954));
#41941=CARTESIAN_POINT('Ctrl Pts',(57.5054427502093,21.3909959849688,10.1537520994043));
#41942=CARTESIAN_POINT('Ctrl Pts',(56.029977118908,23.3171681697859,10.2807853941133));
#41943=CARTESIAN_POINT('Ctrl Pts',(53.6115094249302,23.1218423945828,10.4078186888223));
#41944=CARTESIAN_POINT('Ctrl Pts',(52.464283058435,20.9838503838648,10.5348519835313));
#41945=CARTESIAN_POINT('Ctrl Pts',(53.6386483798942,18.8606442606204,10.6618852782403));
#41946=CARTESIAN_POINT('Ctrl Pts',(56.059407788523,18.6961388160039,10.7889185729493));
#41947=CARTESIAN_POINT('Ctrl Pts',(57.5102196948175,20.6409480537896,10.9159518676582));
#41948=CARTESIAN_POINT('Ctrl Pts',(56.6627840796645,22.9144895717303,11.0429851623672));
#41949=CARTESIAN_POINT('Ctrl Pts',(54.2929759816377,23.4352080514572,11.1700184570762));
#41950=CARTESIAN_POINT('Ctrl Pts',(52.570488196235,21.7263563943386,11.2970517517852));
#41951=CARTESIAN_POINT('Ctrl Pts',(53.0723553119393,19.3524845455114,11.4240850464941));
#41952=CARTESIAN_POINT('Ctrl Pts',(55.3390897161145,18.4870058932248,11.5511183412032));
#41953=CARTESIAN_POINT('Ctrl Pts',(57.2953683856162,19.9223148926776,11.6781516359121));
#41954=CARTESIAN_POINT('Ctrl Pts',(57.1501080091089,22.3443053095913,11.8051849306211));
#41955=CARTESIAN_POINT('Ctrl Pts',(55.0363026432278,23.535508496206,11.9322182253301));
#41956=CARTESIAN_POINT('Ctrl Pts',(52.8892601626876,22.4053108394288,12.0592515200391));
#41957=CARTESIAN_POINT('Ctrl Pts',(52.6747188927902,19.9884719535837,12.1862848147481));
#41958=CARTESIAN_POINT('Ctrl Pts',(54.589103450383,18.4977439695851,12.313318109457));
#41959=CARTESIAN_POINT('Ctrl Pts',(56.8796869433191,19.2979723235654,12.440351404166));
#41960=CARTESIAN_POINT('Ctrl Pts',(57.4493111643545,21.6565028837733,12.567384698875));
#41961=CARTESIAN_POINT('Ctrl Pts',(55.7764530544634,23.4139680756897,12.694417993584));
#41962=CARTESIAN_POINT('Ctrl Pts',(53.3927084386978,22.9613095250879,12.821451288293));
#41963=CARTESIAN_POINT('Ctrl Pts',(52.4805297796474,20.7129616315005,12.9484845830019));
#41964=CARTESIAN_POINT('Ctrl Pts',(53.8750680190704,18.7274135320046,13.0755178777109));
#41965=CARTESIAN_POINT('Ctrl Pts',(56.2995448499803,18.8225463497186,13.2025511724199));
#41966=CARTESIAN_POINT('Ctrl Pts',(57.5342151725387,20.9112606315721,13.3295844671289));
#41967=CARTESIAN_POINT('Ctrl Pts',(56.4486687623729,23.0812208035572,13.4566177618379));
#41968=CARTESIAN_POINT('Ctrl Pts',(54.036784502503,23.3457061029925,13.5836510565469));
#41969=CARTESIAN_POINT('Ctrl Pts',(52.506778284691,21.4625653408395,13.7106843512558));
#41970=CARTESIAN_POINT('Ctrl Pts',(53.2594569805109,19.1559199546814,13.8377176459648));
#41971=CARTESIAN_POINT('Ctrl Pts',(55.6057008485412,18.5376337197097,13.9647509406738));
#41972=CARTESIAN_POINT('Ctrl Pts',(57.3973914730114,20.1737825096463,14.0917842353828));
#41973=CARTESIAN_POINT('Ctrl Pts',(56.9941351684097,22.5663799495479,14.2188175300918));
#41974=CARTESIAN_POINT('Ctrl Pts',(54.7651357954234,23.5248683176836,14.3458508248007));
#41975=CARTESIAN_POINT('Ctrl Pts',(52.7511678306937,22.1716975251863,14.4728841195097));
#41976=CARTESIAN_POINT('Ctrl Pts',(52.7961323847391,19.7457716513177,14.5999174142187));
#41977=CARTESIAN_POINT('Ctrl Pts',(54.8588618756563,18.468162476364,14.7269507089277));
#41978=CARTESIAN_POINT('Ctrl Pts',(57.0508112691597,19.5085931626406,14.8539840036367));
#41979=CARTESIAN_POINT('Ctrl Pts',(57.3651274317021,21.9144908135372,14.9810172983457));
#41980=CARTESIAN_POINT('Ctrl Pts',(55.5140362122968,23.4831206150089,15.1080505930546));
#41981=CARTESIAN_POINT('Ctrl Pts',(53.1923158869174,22.7783136291282,15.2350838877636));
#41982=CARTESIAN_POINT('Ctrl Pts',(52.5256321867243,20.4453603504442,15.3621171824726));
#41983=CARTESIAN_POINT('Ctrl Pts',(54.1243715908862,18.6202109115749,15.4891504771816));
#41984=CARTESIAN_POINT('Ctrl Pts',(56.5247981242588,18.9738924272164,15.6161837718905));
#41985=CARTESIAN_POINT('Ctrl Pts',(57.5291860890565,21.1825895483253,15.7432170665996));
#41986=CARTESIAN_POINT('Ctrl Pts',(56.2179617303263,23.2241156533991,15.8702503613085));
#41987=CARTESIAN_POINT('Ctrl Pts',(53.7916248045405,23.2293386021941,15.9972836560175));
#41988=CARTESIAN_POINT('Ctrl Pts',(52.4716234331684,21.1934764909004,16.1243169507265));
#41989=CARTESIAN_POINT('Ctrl Pts',(53.4664932221301,18.980475754426,16.2513502454355));
#41990=CARTESIAN_POINT('Ctrl Pts',(55.8653748425715,18.6164632165459,16.3783835401444));
#41991=CARTESIAN_POINT('Ctrl Pts',(57.4719570515144,20.4347128590685,16.5054168348534));
#41992=CARTESIAN_POINT('Ctrl Pts',(56.8153233442833,22.770514719491,16.6324501295624));
#41993=CARTESIAN_POINT('Ctrl Pts',(54.4966588654143,23.4853106281647,16.7594834242714));
#41994=CARTESIAN_POINT('Ctrl Pts',(52.6388315464635,21.9246646690871,16.8865167189804));
#41995=CARTESIAN_POINT('Ctrl Pts',(52.9427869419565,19.5174361227759,17.0135500136893));
#41996=CARTESIAN_POINT('Ctrl Pts',(55.1302367667208,18.467578312992,17.1405833083984));
#41997=CARTESIAN_POINT('Ctrl Pts',(57.1984474958328,19.736295198909,17.2676166031073));
#41998=CARTESIAN_POINT('Ctrl Pts',(57.2538557127032,22.1620050096919,17.3946498978163));
#41999=CARTESIAN_POINT('Ctrl Pts',(55.2457320738625,23.5238337829797,17.5216831925253));
#42000=CARTESIAN_POINT('Ctrl Pts',(53.0126268802899,22.5749505704269,17.6487164872343));
#42001=CARTESIAN_POINT('Ctrl Pts',(52.5990737186382,20.1841113999444,17.7757497819432));
#42002=CARTESIAN_POINT('Ctrl Pts',(54.383703802205,18.5402641985739,17.9027830766522));
#42003=CARTESIAN_POINT('Ctrl Pts',(56.7325877683674,19.148443670547,18.0298163713612));
#42004=CARTESIAN_POINT('Ctrl Pts',(57.4951900428093,21.4518272529408,18.1568496660702));
#42005=CARTESIAN_POINT('Ctrl Pts',(55.9733052889244,23.3415375356346,18.2838829607792));
#42006=CARTESIAN_POINT('Ctrl Pts',(53.5603047206123,23.0874383149551,18.4109162554881));
#42007=CARTESIAN_POINT('Ctrl Pts',(52.4654262728904,20.9221717398333,18.5379495501971));
#42008=CARTESIAN_POINT('Ctrl Pts',(53.6910928347986,18.8281613206505,18.6649828449061));
#42009=CARTESIAN_POINT('Ctrl Pts',(56.115137631985,18.7225915434501,18.7920161396151));
#42010=CARTESIAN_POINT('Ctrl Pts',(57.5182111158202,20.7021174855848,18.9190494343241));
#42011=CARTESIAN_POINT('Ctrl Pts',(56.6157204823017,22.9543716482043,19.0460827290331));
#42012=CARTESIAN_POINT('Ctrl Pts',(54.2339467401253,23.4172884849082,19.173116023742));
#42013=CARTESIAN_POINT('Ctrl Pts',(52.5535379060985,21.667041557429,19.300149318451));
#42014=CARTESIAN_POINT('Ctrl Pts',(53.1130029185214,19.3060805123247,19.42718261316));
#42015=CARTESIAN_POINT('Ctrl Pts',(55.4001200460813,18.4959981699371,19.554215907869));
#42016=CARTESIAN_POINT('Ctrl Pts',(57.3209047342821,19.9784705434396,19.681249202578));
#42017=CARTESIAN_POINT('Ctrl Pts',(57.1167704109117,22.3962106731159,19.808282497287));
#42018=CARTESIAN_POINT('Ctrl Pts',(54.9746135470903,23.5356412885585,19.9353157919959));
#42019=CARTESIAN_POINT('Ctrl Pts',(52.8556994108257,22.3535494817334,20.0623490867049));
#42020=CARTESIAN_POINT('Ctrl Pts',(52.7000132438769,19.9322068843205,20.1893823814139));
#42021=CARTESIAN_POINT('Ctrl Pts',(54.6500945012683,18.488489028853,20.3164156761229));
#42022=CARTESIAN_POINT('Ctrl Pts',(56.9205339515342,19.3442009308982,20.4434489708319));
#42023=CARTESIAN_POINT('Ctrl Pts',(57.4326163931288,21.7158901452844,20.5704822655408));
#42024=CARTESIAN_POINT('Ctrl Pts',(55.7175015072043,23.4321416084171,20.6975155602498));
#42025=CARTESIAN_POINT('Ctrl Pts',(53.345473577427,22.9216304361771,20.8245488549588));
#42026=CARTESIAN_POINT('Ctrl Pts',(52.4882577804106,20.6517583618146,20.9515821496678));
#42027=CARTESIAN_POINT('Ctrl Pts',(53.930683461881,18.7007211222778,21.0786154443768));
#42028=CARTESIAN_POINT('Ctrl Pts',(56.3521286643486,18.8548032045331,21.2056487390858));
#42029=CARTESIAN_POINT('Ctrl Pts',(57.5356239145732,20.9729337834449,21.3326820337947));
#42030=CARTESIAN_POINT('Ctrl Pts',(56.3976126493923,23.1158450081452,21.4597153285037));
#42031=CARTESIAN_POINT('Ctrl Pts',(53.9800082817287,23.3215809507515,21.5867486232127));
#42032=CARTESIAN_POINT('Ctrl Pts',(52.4962637842209,21.4017787675202,21.7137819179217));
#42033=CARTESIAN_POINT('Ctrl Pts',(53.3048308177651,19.1141254920234,21.8408152126307));
#42034=CARTESIAN_POINT('Ctrl Pts',(55.6654207197859,18.5530965523924,21.9678485073396));
#42035=CARTESIAN_POINT('Ctrl Pts',(57.416780472339,20.2323455433887,22.0948818020486));
#42036=CARTESIAN_POINT('Ctrl Pts',(56.9554415748307,22.6144254283362,22.2219150967576));
#42037=CARTESIAN_POINT('Ctrl Pts',(54.7037857733155,23.5184078994761,22.3489483914666));
#42038=CARTESIAN_POINT('Ctrl Pts',(52.7233307808997,22.1166460867416,22.4759816861756));
#42039=CARTESIAN_POINT('Ctrl Pts',(52.8272946942958,19.6925318853606,22.6030149808846));
#42040=CARTESIAN_POINT('Ctrl Pts',(54.9204926949152,18.4654783874128,22.7300482755935));
#42041=CARTESIAN_POINT('Ctrl Pts',(57.0864841116712,19.5589221853135,22.8570815703025));
#42042=CARTESIAN_POINT('Ctrl Pts',(57.3421818008354,21.9717538927445,22.9841148650115));
#42043=CARTESIAN_POINT('Ctrl Pts',(55.4534801255511,23.4948901763327,23.1111481597205));
#42044=CARTESIAN_POINT('Ctrl Pts',(53.1495918525825,22.7338139762478,23.2381814544295));
#42045=CARTESIAN_POINT('Ctrl Pts',(52.5398564647277,20.3853334220528,23.3652147491384));
#42046=CARTESIAN_POINT('Ctrl Pts',(54.1825210534815,18.5996147417073,23.4922480438474));
#42047=CARTESIAN_POINT('Ctrl Pts',(56.5736336631851,19.0115839694587,23.6192813385564));
#42048=CARTESIAN_POINT('Ctrl Pts',(57.5239960175717,21.244060072795,23.7463146332654));
#42049=CARTESIAN_POINT('Ctrl Pts',(56.1634978514913,23.2530854324462,23.8733479279744));
#42050=CARTESIAN_POINT('Ctrl Pts',(53.7377518666139,23.1992841715592,24.0003812226833));
#42051=CARTESIAN_POINT('Ctrl Pts',(52.4676651463435,21.1319143742643,24.1274145173924));
#42052=CARTESIAN_POINT('Ctrl Pts',(53.5160736188505,18.943769537924,24.2544478121013));
#42053=CARTESIAN_POINT('Ctrl Pts',(55.9231002810787,18.6382195073252,24.3814811068103));
#42054=CARTESIAN_POINT('Ctrl Pts',(57.4849766333806,20.4950125505569,24.5085144015193));
#42055=CARTESIAN_POINT('Ctrl Pts',(56.7717169246738,22.814150041662,24.6355476962283));
#42056=CARTESIAN_POINT('Ctrl Pts',(54.4363505469416,23.4723309975539,24.7625809909372));
#42057=CARTESIAN_POINT('Ctrl Pts',(52.6170370516924,21.8669536455561,24.8896142856462));
#42058=CARTESIAN_POINT('Ctrl Pts',(52.9794602409511,19.4678314440883,25.0166475803552));
#42059=CARTESIAN_POINT('Ctrl Pts',(55.191801618391,18.4714957683358,25.1436808750642));
#42060=CARTESIAN_POINT('Ctrl Pts',(57.2285373613243,19.7901483097356,25.2707141697732));
#42061=CARTESIAN_POINT('Ctrl Pts',(57.2249225043503,22.2164878823824,25.3977474644821));
#42062=CARTESIAN_POINT('Ctrl Pts',(55.184264054378,23.5290649385282,25.5247807591912));
#42063=CARTESIAN_POINT('Ctrl Pts',(52.9749048462477,22.526139300939,25.6518140539001));
#42064=CARTESIAN_POINT('Ctrl Pts',(52.6196277405404,20.1259496956444,25.7788473486091));
#42065=CARTESIAN_POINT('Ctrl Pts',(54.4437283774751,18.5259974399519,25.9058806433181));
#42066=CARTESIAN_POINT('Ctrl Pts',(56.7771018613365,19.191143532242,26.032913938027));
#42067=CARTESIAN_POINT('Ctrl Pts',(57.483487694633,21.5123807259463,26.159947232736));
#42068=CARTESIAN_POINT('Ctrl Pts',(55.9160044312663,23.3645414315281,26.286980527445));
#42069=CARTESIAN_POINT('Ctrl Pts',(53.5100557199194,23.0517590482558,26.414013822154));
#42070=CARTESIAN_POINT('Ctrl Pts',(52.4678668150611,20.8606169550065,26.541047116863));
#42071=CARTESIAN_POINT('Ctrl Pts',(53.7447085517716,18.7968114789175,26.668080411572));
#42072=CARTESIAN_POINT('Ctrl Pts',(56.1694304370623,18.7506911017083,26.7951137062809));
#42073=CARTESIAN_POINT('Ctrl Pts',(57.5262467139057,20.7628658615296,26.9221470009899));
#42074=CARTESIAN_POINT('Ctrl Pts',(56.5645411333706,22.9944003274668,27.0491802956989));
#42075=CARTESIAN_POINT('Ctrl Pts',(54.9770383489932,23.2607009728164,27.1338691588382));
#42076=CARTESIAN_POINT('Ctrl Pts',(54.3023543067887,23.0286832787525,27.1762135904079));
#42077=CARTESIAN_POINT('Ctrl Pts',(56.1575872040306,19.3799074908306,7.70202135064341));
#42078=CARTESIAN_POINT('Ctrl Pts',(56.6966257837449,19.7650341873306,7.74438338830569));
#42079=CARTESIAN_POINT('Ctrl Pts',(57.3503471278769,21.1089590232279,7.82908985753763));
#42080=CARTESIAN_POINT('Ctrl Pts',(56.1807116204721,23.0376922383364,7.95614075833924));
#42081=CARTESIAN_POINT('Ctrl Pts',(53.9289162740299,23.0950903039575,8.08317405304821));
#42082=CARTESIAN_POINT('Ctrl Pts',(52.6584397816218,21.2369905163238,8.2102073477572));
#42083=CARTESIAN_POINT('Ctrl Pts',(53.5314442785794,19.160554851951,8.33724064246617));
#42084=CARTESIAN_POINT('Ctrl Pts',(55.7491729262641,18.768928073743,8.46427393717517));
#42085=CARTESIAN_POINT('Ctrl Pts',(57.2809002009969,20.41961894638,8.59130723188414));
#42086=CARTESIAN_POINT('Ctrl Pts',(56.7243815809553,22.6018625414762,8.71834052659312));
#42087=CARTESIAN_POINT('Ctrl Pts',(54.5890706115975,23.3174181187817,8.84537382130211));
#42088=CARTESIAN_POINT('Ctrl Pts',(52.8300008553486,21.9112942410088,8.97240711601109));
#42089=CARTESIAN_POINT('Ctrl Pts',(53.0576812994974,19.6708049391771,9.09944041072007));
#42090=CARTESIAN_POINT('Ctrl Pts',(55.0636671095574,18.6472809657784,9.22647370542905));
#42091=CARTESIAN_POINT('Ctrl Pts',(57.0113604623833,19.7777974566601,9.35350700013803));
#42092=CARTESIAN_POINT('Ctrl Pts',(57.1175408545581,22.0273124547239,9.48054029484702));
#42093=CARTESIAN_POINT('Ctrl Pts',(55.2849928950004,23.3362633810241,9.607573589556));
#42094=CARTESIAN_POINT('Ctrl Pts',(53.1915181057372,22.5062344357837,9.73460688426498));
#42095=CARTESIAN_POINT('Ctrl Pts',(52.7538102437097,20.2971625917199,9.86164017897397));
#42096=CARTESIAN_POINT('Ctrl Pts',(54.3726156795429,18.7315782041938,9.98867347368293));
#42097=CARTESIAN_POINT('Ctrl Pts',(56.5658267696552,19.2428616288,10.115706768392));
#42098=CARTESIAN_POINT('Ctrl Pts',(57.3254352702633,21.3629042626903,10.2427400631009));
#42099=CARTESIAN_POINT('Ctrl Pts',(55.9559767907978,23.1506875735641,10.3697733578099));
#42100=CARTESIAN_POINT('Ctrl Pts',(53.7112677168834,22.9693952862784,10.4968066525189));
#42101=CARTESIAN_POINT('Ctrl Pts',(52.6464656353348,20.9850106784683,10.6238399472279));
#42102=CARTESIAN_POINT('Ctrl Pts',(53.7364568308897,19.0143496427617,10.7508732419369));
#42103=CARTESIAN_POINT('Ctrl Pts',(55.9832929676071,18.861663350876,10.8779065366458));
#42104=CARTESIAN_POINT('Ctrl Pts',(57.3298690077631,20.6667447062981,11.0049398313548));
#42105=CARTESIAN_POINT('Ctrl Pts',(56.5433187389178,22.7769400535218,11.1319731260638));
#42106=CARTESIAN_POINT('Ctrl Pts',(54.3437732356544,23.2602466940481,11.2590064207728));
#42107=CARTESIAN_POINT('Ctrl Pts',(52.7450402977582,21.6741701753253,11.3860397154818));
#42108=CARTESIAN_POINT('Ctrl Pts',(53.2108499801973,19.4708528878373,11.5130730101907));
#42109=CARTESIAN_POINT('Ctrl Pts',(55.3147272814636,18.6675559122754,11.6401063048997));
#42110=CARTESIAN_POINT('Ctrl Pts',(57.1304540292182,19.9997428763457,11.7671395996087));
#42111=CARTESIAN_POINT('Ctrl Pts',(56.9956301132161,22.2477215776191,11.8941728943177));
#42112=CARTESIAN_POINT('Ctrl Pts',(55.033694422656,23.3533408953913,12.0212061890267));
#42113=CARTESIAN_POINT('Ctrl Pts',(53.0409095902807,22.3043440690943,12.1482394837357));
#42114=CARTESIAN_POINT('Ctrl Pts',(52.8417823757775,20.0611467790271,12.2752727784447));
#42115=CARTESIAN_POINT('Ctrl Pts',(54.6186249600678,18.6775224946293,12.4023060731536));
#42116=CARTESIAN_POINT('Ctrl Pts',(56.7446378747558,19.4202571823225,12.5293393678626));
#42117=CARTESIAN_POINT('Ctrl Pts',(57.2733365465898,21.6093354002316,12.6563726625716));
#42118=CARTESIAN_POINT('Ctrl Pts',(55.7206675620115,23.2405327377881,12.7834059572806));
#42119=CARTESIAN_POINT('Ctrl Pts',(53.5081868320733,22.8203961535986,12.9104392519896));
#42120=CARTESIAN_POINT('Ctrl Pts',(52.6615450852764,20.7335843551119,13.0374725466985));
#42121=CARTESIAN_POINT('Ctrl Pts',(53.955890528777,18.8906910856543,13.1645058414075));
#42122=CARTESIAN_POINT('Ctrl Pts',(56.2061770037176,18.9789889362651,13.2915391361165));
#42123=CARTESIAN_POINT('Ctrl Pts',(57.3521404925994,20.9176362512431,13.4185724308254));
#42124=CARTESIAN_POINT('Ctrl Pts',(56.3445868737848,22.9316922174306,13.5456057255345));
#42125=CARTESIAN_POINT('Ctrl Pts',(54.1059882367871,23.1771751540179,13.6726390202434));
#42126=CARTESIAN_POINT('Ctrl Pts',(52.6859077251393,21.4293316054816,13.7996723149524));
#42127=CARTESIAN_POINT('Ctrl Pts',(53.3845090347436,19.2884107895844,13.9267056096614));
#42128=CARTESIAN_POINT('Ctrl Pts',(55.5621833172234,18.714546302838,14.0537389043704));
#42129=CARTESIAN_POINT('Ctrl Pts',(57.225147107234,20.2331434063634,14.1807721990794));
#42130=CARTESIAN_POINT('Ctrl Pts',(56.8508633868822,22.4538409153462,14.3078054937884));
#42131=CARTESIAN_POINT('Ctrl Pts',(54.7820099840639,23.343465177251,14.4348387884973));
#42132=CARTESIAN_POINT('Ctrl Pts',(52.912738719346,22.0875150713064,14.5618720832063));
#42133=CARTESIAN_POINT('Ctrl Pts',(52.954472724196,19.8358836621806,14.6889053779153));
#42134=CARTESIAN_POINT('Ctrl Pts',(54.8690021664633,18.6500663303734,14.8159386726243));
#42135=CARTESIAN_POINT('Ctrl Pts',(56.9034675039205,19.61574563553,14.9429719673333));
#42136=CARTESIAN_POINT('Ctrl Pts',(57.1952011267819,21.8487877809036,15.0700052620422));
#42137=CARTESIAN_POINT('Ctrl Pts',(55.4771044711229,23.3047169040189,15.1970385567512));
#42138=CARTESIAN_POINT('Ctrl Pts',(53.3221917987528,22.650547885965,15.3240718514602));
#42139=CARTESIAN_POINT('Ctrl Pts',(52.7034070388898,20.4852093095101,15.4511051461692));
#42140=CARTESIAN_POINT('Ctrl Pts',(54.1872824928738,18.7911906063115,15.5781384408781));
#42141=CARTESIAN_POINT('Ctrl Pts',(56.4152466017777,19.119461316486,15.7051717355872));
#42142=CARTESIAN_POINT('Ctrl Pts',(57.3474727315399,21.1694711146848,15.8322050302961));
#42143=CARTESIAN_POINT('Ctrl Pts',(56.1304553517716,23.0643205617556,15.9592383250051));
#42144=CARTESIAN_POINT('Ctrl Pts',(53.8784424234009,23.0691682595693,16.0862716197141));
#42145=CARTESIAN_POINT('Ctrl Pts',(52.6532786292859,21.179575867726,16.213304914423));
#42146=CARTESIAN_POINT('Ctrl Pts',(53.5766704315442,19.1255716541848,16.3403382091321));
#42147=CARTESIAN_POINT('Ctrl Pts',(55.8032006242194,18.7877121703337,16.467371503841));
#42148=CARTESIAN_POINT('Ctrl Pts',(57.294355404324,20.4753268039198,16.59440479855));
#42149=CARTESIAN_POINT('Ctrl Pts',(56.6848985798521,22.6433093012723,16.721438093259));
#42150=CARTESIAN_POINT('Ctrl Pts',(54.5328222018875,23.3067495722308,16.848471387968));
#42151=CARTESIAN_POINT('Ctrl Pts',(52.8084734123629,21.8582306797798,16.975504682677));
#42152=CARTESIAN_POINT('Ctrl Pts',(53.0905906537993,19.6239532592685,17.1025379773859));
#42153=CARTESIAN_POINT('Ctrl Pts',(55.1208797011197,18.6495241371388,17.2295712720949));
#42154=CARTESIAN_POINT('Ctrl Pts',(57.0404965733917,19.8270880604187,17.3566045668039));
#42155=CARTESIAN_POINT('Ctrl Pts',(57.0919238996646,22.0785189298516,17.4836378615129));
#42156=CARTESIAN_POINT('Ctrl Pts',(55.2280770660383,23.342504970322,17.6106711562219));
#42157=CARTESIAN_POINT('Ctrl Pts',(53.1554128317797,22.4617957664712,17.7377044509309));
#42158=CARTESIAN_POINT('Ctrl Pts',(52.7715720482881,20.2427302012723,17.8647377456398));
#42159=CARTESIAN_POINT('Ctrl Pts',(54.4279825730753,18.7169877908057,17.9917710403488));
#42160=CARTESIAN_POINT('Ctrl Pts',(56.6081072716794,19.2814716508572,18.1188043350578));
#42161=CARTESIAN_POINT('Ctrl Pts',(57.3159191847721,21.4193650124183,18.2458376297668));
#42162=CARTESIAN_POINT('Ctrl Pts',(55.9033766376859,23.1733060839466,18.3728709244757));
#42163=CARTESIAN_POINT('Ctrl Pts',(53.6637418951841,22.9374630219308,18.4999042191848));
#42164=CARTESIAN_POINT('Ctrl Pts',(52.6475267137473,20.9277634337484,18.6269375138937));
#42165=CARTESIAN_POINT('Ctrl Pts',(53.7851333313421,18.984200490768,18.7539708086027));
#42166=CARTESIAN_POINT('Ctrl Pts',(56.0350188127026,18.8862155404612,18.8810041033117));
#42167=CARTESIAN_POINT('Ctrl Pts',(57.337286272539,20.7235193239367,19.0080373980207));
#42168=CARTESIAN_POINT('Ctrl Pts',(56.4996364998232,22.8139567394053,19.1350706927297));
#42169=CARTESIAN_POINT('Ctrl Pts',(54.2889850429573,23.2436145869774,19.2621039874386));
#42170=CARTESIAN_POINT('Ctrl Pts',(52.7293078279099,21.6191169062822,19.3891372821476));
#42171=CARTESIAN_POINT('Ctrl Pts',(53.2485771954729,19.4277828254919,19.5161705768566));
#42172=CARTESIAN_POINT('Ctrl Pts',(55.3713727912637,18.6759021247062,19.6432038715656));
#42173=CARTESIAN_POINT('Ctrl Pts',(57.1541556786998,20.0518639359451,19.7702371662746));
#42174=CARTESIAN_POINT('Ctrl Pts',(56.9646877072614,22.295897718561,19.8972704609836));
#42175=CARTESIAN_POINT('Ctrl Pts',(54.976437476778,23.3534641470682,20.0243037556925));
#42176=CARTESIAN_POINT('Ctrl Pts',(53.0097600634877,22.256301587656,20.1513370504015));
#42177=CARTESIAN_POINT('Ctrl Pts',(52.8652594143769,20.0089241622712,20.2783703451105));
#42178=CARTESIAN_POINT('Ctrl Pts',(54.6752340128539,18.6689324896887,20.4054036398195));
#42179=CARTESIAN_POINT('Ctrl Pts',(56.78255016534,19.4631644225609,20.5324369345285));
#42180=CARTESIAN_POINT('Ctrl Pts',(57.2578412374936,21.6644558904165,20.6594702292374));
#42181=CARTESIAN_POINT('Ctrl Pts',(55.6659514815017,23.2574005644372,20.7865035239464));
#42182=CARTESIAN_POINT('Ctrl Pts',(53.4643456337959,22.783567871317,20.9135368186554));
#42183=CARTESIAN_POINT('Ctrl Pts',(52.6687178556547,20.6767783307191,21.0405701133644));
#42184=CARTESIAN_POINT('Ctrl Pts',(54.0075101925159,18.8659164341394,21.1676034080733));
#42185=CARTESIAN_POINT('Ctrl Pts',(56.2549828511337,19.0089282465475,21.2946367027823));
#42186=CARTESIAN_POINT('Ctrl Pts',(57.3534480213442,20.9748783983971,21.4216699974913));
#42187=CARTESIAN_POINT('Ctrl Pts',(56.297198967644,22.963828791514,21.5487032922003));
#42188=CARTESIAN_POINT('Ctrl Pts',(54.0532911930052,23.1547833113319,21.6757365869093));
#42189=CARTESIAN_POINT('Ctrl Pts',(52.6761486555135,21.3729123392486,21.8027698816183));
#42190=CARTESIAN_POINT('Ctrl Pts',(53.4266229172058,19.2496191159138,21.9298031763272));
#42191=CARTESIAN_POINT('Ctrl Pts',(55.6176125202719,18.7288981839558,22.0568364710362));
#42192=CARTESIAN_POINT('Ctrl Pts',(57.2431430733712,20.287498886722,22.1838697657452));
#42193=CARTESIAN_POINT('Ctrl Pts',(56.8149497954683,22.4984344910491,22.3109030604542));
#42194=CARTESIAN_POINT('Ctrl Pts',(54.7250677509081,23.3374689179634,22.4379363551632));
#42195=CARTESIAN_POINT('Ctrl Pts',(52.8869016662319,22.0364188901516,22.5649696498721));
#42196=CARTESIAN_POINT('Ctrl Pts',(52.9833961285485,19.7864689910505,22.6920029445812));
#42197=CARTESIAN_POINT('Ctrl Pts',(54.9262050224566,18.6475750840197,22.8190362392901));
#42198=CARTESIAN_POINT('Ctrl Pts',(56.9365773748846,19.6624586903111,22.9460695339992));
#42199=CARTESIAN_POINT('Ctrl Pts',(57.1739040608994,21.9019367040076,23.073102828708));
#42200=CARTESIAN_POINT('Ctrl Pts',(55.420899131793,23.3156408626749,23.2001361234171));
#42201=CARTESIAN_POINT('Ctrl Pts',(53.2825373399461,22.6092453807235,23.327169418126));
#42202=CARTESIAN_POINT('Ctrl Pts',(52.7166093512399,20.4294951103189,23.454202712835));
#42203=CARTESIAN_POINT('Ctrl Pts',(54.2412541157553,18.7720742007028,23.581236007544));
#42204=CARTESIAN_POINT('Ctrl Pts',(56.460573474504,19.1544448505195,23.708269302253));
#42205=CARTESIAN_POINT('Ctrl Pts',(57.3426555489142,21.2265251925206,23.835302596962));
#42206=CARTESIAN_POINT('Ctrl Pts',(56.0799045160809,23.0912089614057,23.9623358916709));
#42207=CARTESIAN_POINT('Ctrl Pts',(53.8284400715384,23.0412731368329,24.0893691863799));
#42208=CARTESIAN_POINT('Ctrl Pts',(52.6496047318115,21.1224367783073,24.216402481089));
#42209=CARTESIAN_POINT('Ctrl Pts',(53.6226886465833,19.0915026536122,24.3434357757979));
#42210=CARTESIAN_POINT('Ctrl Pts',(55.8567786876913,18.8079053461403,24.4704690705069));
#42211=CARTESIAN_POINT('Ctrl Pts',(57.306439573828,20.5312941691135,24.5975023652159));
#42212=CARTESIAN_POINT('Ctrl Pts',(56.6444251321306,22.6838095750054,24.7245356599248));
#42213=CARTESIAN_POINT('Ctrl Pts',(54.4768468295286,23.2947024836215,24.8515689546338));
#42214=CARTESIAN_POINT('Ctrl Pts',(52.7882447773904,21.8046659956174,24.9786022493428));
#42215=CARTESIAN_POINT('Ctrl Pts',(53.1246291018748,19.5779125068384,25.1056355440518));
#42216=CARTESIAN_POINT('Ctrl Pts',(55.1780213290696,18.6531601367342,25.2326688387608));
#42217=CARTESIAN_POINT('Ctrl Pts',(57.0684245851116,19.8770720096903,25.3597021334698));
#42218=CARTESIAN_POINT('Ctrl Pts',(57.0650694432295,22.1290873947541,25.4867354281787));
#42219=CARTESIAN_POINT('Ctrl Pts',(55.1710253132133,23.3473602852621,25.6137687228878));
#42220=CARTESIAN_POINT('Ctrl Pts',(53.1204009966777,22.4164914195073,25.7408020175967));
#42221=CARTESIAN_POINT('Ctrl Pts',(52.7906493341184,20.1887472162105,25.8678353123057));
#42222=CARTESIAN_POINT('Ctrl Pts',(54.4836945882088,18.7037460499241,25.9948686070146));
#42223=CARTESIAN_POINT('Ctrl Pts',(56.6494231795385,19.3211036737453,26.1219019017237));
#42224=CARTESIAN_POINT('Ctrl Pts',(57.3050576102293,21.4755679257963,26.2489351964326));
#42225=CARTESIAN_POINT('Ctrl Pts',(55.8501926503833,23.1946572287132,26.3759684911416));
#42226=CARTESIAN_POINT('Ctrl Pts',(53.6171031130779,22.9043471883351,26.5030017858506));
#42227=CARTESIAN_POINT('Ctrl Pts',(52.6497919113224,20.8706311493737,26.6300350805596));
#42228=CARTESIAN_POINT('Ctrl Pts',(53.8348969426956,18.9551030277838,26.7570683752686));
#42229=CARTESIAN_POINT('Ctrl Pts',(56.085410865699,18.9122962417053,26.8841016699775));
#42230=CARTESIAN_POINT('Ctrl Pts',(57.3447445404256,20.7799031371454,27.0111349646865));
#42231=CARTESIAN_POINT('Ctrl Pts',(56.452134211813,22.8511094951693,27.1381682593955));
#42232=CARTESIAN_POINT('Ctrl Pts',(54.9786880649696,23.098277351285,27.2228571225348));
#42233=CARTESIAN_POINT('Ctrl Pts',(54.352477760266,22.8829293338312,27.2652015541045));
#42234=CARTESIAN_POINT('Ctrl Pts',(56.0772665381941,23.205491718641,7.7));
#42235=CARTESIAN_POINT('Ctrl Pts',(56.0907843704075,23.1972259880661,7.7));
#42236=CARTESIAN_POINT('Ctrl Pts',(56.104302202621,23.1889602574912,7.7));
#42237=CARTESIAN_POINT('Ctrl Pts',(56.1178200348344,23.1806945269163,7.7));
#42238=CARTESIAN_POINT('Origin',(55.,21.,7.7));
#42239=CARTESIAN_POINT('',(57.6505,21.,7.5));
#42240=CARTESIAN_POINT('Origin',(55.,21.,7.5));
#42241=CARTESIAN_POINT('Origin',(57.6505,21.,7.7));
#42242=CARTESIAN_POINT('Origin',(55.,21.,7.5));
#42243=CARTESIAN_POINT('',(50.95,21.,7.5));
#42244=CARTESIAN_POINT('Origin',(55.,21.,7.5));
#42245=CARTESIAN_POINT('Origin',(55.,21.,27.25));
#42246=CARTESIAN_POINT('',(53.0495,21.,27.5));
#42247=CARTESIAN_POINT('',(52.7995,21.,27.25));
#42248=CARTESIAN_POINT('Origin',(55.,21.,27.5));
#42249=CARTESIAN_POINT('Origin',(55.,21.,27.5));
#42250=CARTESIAN_POINT('Origin',(59.2592935317778,20.2489716315905,6.9));
#42251=CARTESIAN_POINT('',(59.1721341053809,20.1901870544887,6.9));
#42252=CARTESIAN_POINT('',(59.1974959714464,20.3340213444176,6.9));
#42253=CARTESIAN_POINT('Origin',(55.,21.,6.9));
#42254=CARTESIAN_POINT('',(59.0377117873501,20.2880424715656,6.9));
#42255=CARTESIAN_POINT('',(59.0377117873501,20.2880424715656,6.9));
#42256=CARTESIAN_POINT('',(59.5190778752923,20.4265584972782,6.9));
#42257=CARTESIAN_POINT('Origin',(59.5190778752923,20.4265584972782,2.5));
#42258=CARTESIAN_POINT('',(59.1974959714464,20.3340213444176,2.9));
#42259=CARTESIAN_POINT('',(59.1974959714464,20.3340213444176,7.5));
#42260=CARTESIAN_POINT('',(59.0377117873501,20.2880424715656,2.75000000000001));
#42261=CARTESIAN_POINT('',(59.0377117873501,20.2880424715656,2.5));
#42262=CARTESIAN_POINT('Ctrl Pts',(59.1974959714464,20.3340213444176,2.90000000000003));
#42263=CARTESIAN_POINT('Ctrl Pts',(59.1161686921159,20.3106189241037,2.82334460824933));
#42264=CARTESIAN_POINT('Ctrl Pts',(59.0377117873501,20.2880424715656,2.75000000000001));
#42265=CARTESIAN_POINT('Origin',(59.0377117873501,20.2880424715656,2.5));
#42266=CARTESIAN_POINT('',(59.1721341053809,20.1901870544887,2.9));
#42267=CARTESIAN_POINT('',(59.1721341053809,20.1901870544887,7.5));
#42268=CARTESIAN_POINT('Ctrl Pts',(59.0377117873501,20.2880424715656,2.75000000000001));
#42269=CARTESIAN_POINT('Ctrl Pts',(59.1037155602747,20.2399937038996,2.82334460824863));
#42270=CARTESIAN_POINT('Ctrl Pts',(59.1721341053809,20.1901870544887,2.90000000000003));
#42271=CARTESIAN_POINT('Origin',(55.,21.,7.5));
#42272=CARTESIAN_POINT('',(50.7506274441751,21.0730265828477,6.9));
#42273=CARTESIAN_POINT('',(50.75,21.,6.9));
#42274=CARTESIAN_POINT('Origin',(55.,21.,6.9));
#42275=CARTESIAN_POINT('',(50.75,21.,7.3));
#42276=CARTESIAN_POINT('',(50.75,21.,7.5));
#42277=CARTESIAN_POINT('Origin',(55.,21.,7.3));
#42278=CARTESIAN_POINT('',(50.7506274441751,20.9269734171523,6.9));
#42279=CARTESIAN_POINT('Origin',(55.,21.,6.9));
#42280=CARTESIAN_POINT('',(50.7506274441751,20.9269734171523,2.9));
#42281=CARTESIAN_POINT('',(50.7506274441751,20.9269734171523,7.5));
#42282=CARTESIAN_POINT('',(50.8025040285536,20.3340213444176,2.9));
#42283=CARTESIAN_POINT('Origin',(55.,21.,2.9));
#42284=CARTESIAN_POINT('',(50.8025040285536,20.3340213444176,6.9));
#42285=CARTESIAN_POINT('',(50.8025040285536,20.3340213444176,7.5));
#42286=CARTESIAN_POINT('',(50.8278658946191,20.1901870544887,6.9));
#42287=CARTESIAN_POINT('Origin',(55.,21.,6.9));
#42288=CARTESIAN_POINT('',(50.8278658946191,20.1901870544887,2.9));
#42289=CARTESIAN_POINT('',(50.8278658946191,20.1901870544887,7.5));
#42290=CARTESIAN_POINT('',(50.9819194039891,19.6152515304358,2.9));
#42291=CARTESIAN_POINT('Origin',(55.,21.,2.9));
#42292=CARTESIAN_POINT('',(50.9819194039891,19.6152515304358,6.9));
#42293=CARTESIAN_POINT('',(50.9819194039891,19.6152515304358,7.5));
#42294=CARTESIAN_POINT('',(51.0318725286534,19.4780064483894,6.9));
#42295=CARTESIAN_POINT('Origin',(55.,21.,6.9));
#42296=CARTESIAN_POINT('',(51.0318725286534,19.4780064483894,2.9));
#42297=CARTESIAN_POINT('',(51.0318725286534,19.4780064483894,7.5));
#42298=CARTESIAN_POINT('',(51.2834221250874,18.9385565979853,2.9));
#42299=CARTESIAN_POINT('Origin',(55.,21.,2.9));
#42300=CARTESIAN_POINT('',(51.2834221250874,18.9385565979853,6.9));
#42301=CARTESIAN_POINT('',(51.2834221250874,18.9385565979853,7.5));
#42302=CARTESIAN_POINT('',(51.3564487079351,18.8120708461899,6.9));
#42303=CARTESIAN_POINT('Origin',(55.,21.,6.9));
#42304=CARTESIAN_POINT('',(51.3564487079351,18.8120708461899,2.9));
#42305=CARTESIAN_POINT('',(51.3564487079351,18.8120708461899,7.5));
#42306=CARTESIAN_POINT('',(51.6978511842358,18.3244975801642,2.9));
#42307=CARTESIAN_POINT('Origin',(55.,21.,2.9));
#42308=CARTESIAN_POINT('',(51.6978511842358,18.3244975801642,6.9));
#42309=CARTESIAN_POINT('',(51.6978511842358,18.3244975801642,7.5));
#42310=CARTESIAN_POINT('',(51.7917323495003,18.2126143641833,6.9));
#42311=CARTESIAN_POINT('Origin',(55.,21.,6.9));
#42312=CARTESIAN_POINT('',(51.7917323495003,18.2126143641833,2.9));
#42313=CARTESIAN_POINT('',(51.7917323495003,18.2126143641833,7.5));
#42314=CARTESIAN_POINT('',(52.2126143641833,17.7917323495003,2.9));
#42315=CARTESIAN_POINT('Origin',(55.,21.,2.9));
#42316=CARTESIAN_POINT('',(52.2126143641833,17.7917323495003,6.9));
#42317=CARTESIAN_POINT('',(52.2126143641833,17.7917323495003,7.5));
#42318=CARTESIAN_POINT('',(52.3244975801642,17.6978511842358,6.9));
#42319=CARTESIAN_POINT('Origin',(55.,21.,6.9));
#42320=CARTESIAN_POINT('',(52.3244975801642,17.6978511842358,2.9));
#42321=CARTESIAN_POINT('',(52.3244975801642,17.6978511842358,7.5));
#42322=CARTESIAN_POINT('',(52.8120708461899,17.3564487079351,2.9));
#42323=CARTESIAN_POINT('Origin',(55.,21.,2.9));
#42324=CARTESIAN_POINT('',(52.8120708461899,17.3564487079351,6.9));
#42325=CARTESIAN_POINT('',(52.8120708461899,17.3564487079351,7.5));
#42326=CARTESIAN_POINT('',(52.9385565979852,17.2834221250874,6.9));
#42327=CARTESIAN_POINT('Origin',(55.,21.,6.9));
#42328=CARTESIAN_POINT('',(52.9385565979852,17.2834221250874,2.9));
#42329=CARTESIAN_POINT('',(52.9385565979852,17.2834221250874,7.5));
#42330=CARTESIAN_POINT('',(53.4780064483894,17.0318725286534,2.9));
#42331=CARTESIAN_POINT('Origin',(55.,21.,2.9));
#42332=CARTESIAN_POINT('',(53.4780064483894,17.0318725286534,6.9));
#42333=CARTESIAN_POINT('',(53.4780064483894,17.0318725286534,7.5));
#42334=CARTESIAN_POINT('',(53.6152515304358,16.9819194039891,6.9));
#42335=CARTESIAN_POINT('Origin',(55.,21.,6.9));
#42336=CARTESIAN_POINT('',(53.6152515304358,16.9819194039891,2.9));
#42337=CARTESIAN_POINT('',(53.6152515304358,16.9819194039891,7.5));
#42338=CARTESIAN_POINT('',(54.1901870544887,16.8278658946191,2.9));
#42339=CARTESIAN_POINT('Origin',(55.,21.,2.9));
#42340=CARTESIAN_POINT('',(54.1901870544887,16.8278658946191,6.9));
#42341=CARTESIAN_POINT('',(54.1901870544887,16.8278658946191,7.5));
#42342=CARTESIAN_POINT('',(54.3340213444176,16.8025040285536,6.9));
#42343=CARTESIAN_POINT('Origin',(55.,21.,6.9));
#42344=CARTESIAN_POINT('',(54.3340213444176,16.8025040285536,2.9));
#42345=CARTESIAN_POINT('',(54.3340213444176,16.8025040285536,7.5));
#42346=CARTESIAN_POINT('',(54.9269734171523,16.7506274441751,2.9));
#42347=CARTESIAN_POINT('Origin',(55.,21.,2.9));
#42348=CARTESIAN_POINT('',(54.9269734171523,16.7506274441751,6.9));
#42349=CARTESIAN_POINT('',(54.9269734171523,16.7506274441751,7.5));
#42350=CARTESIAN_POINT('',(55.0730265828477,16.7506274441751,6.9));
#42351=CARTESIAN_POINT('Origin',(55.,21.,6.9));
#42352=CARTESIAN_POINT('',(55.0730265828477,16.7506274441751,2.9));
#42353=CARTESIAN_POINT('',(55.0730265828477,16.7506274441751,7.5));
#42354=CARTESIAN_POINT('',(55.6659786555824,16.8025040285536,2.9));
#42355=CARTESIAN_POINT('Origin',(55.,21.,2.9));
#42356=CARTESIAN_POINT('',(55.6659786555824,16.8025040285536,6.9));
#42357=CARTESIAN_POINT('',(55.6659786555824,16.8025040285536,7.5));
#42358=CARTESIAN_POINT('',(55.8098129455113,16.8278658946191,6.9));
#42359=CARTESIAN_POINT('Origin',(55.,21.,6.9));
#42360=CARTESIAN_POINT('',(55.8098129455113,16.8278658946191,2.9));
#42361=CARTESIAN_POINT('',(55.8098129455113,16.8278658946191,7.5));
#42362=CARTESIAN_POINT('',(56.3847484695642,16.9819194039891,2.9));
#42363=CARTESIAN_POINT('Origin',(55.,21.,2.9));
#42364=CARTESIAN_POINT('',(56.3847484695642,16.9819194039891,6.9));
#42365=CARTESIAN_POINT('',(56.3847484695642,16.9819194039891,7.5));
#42366=CARTESIAN_POINT('',(56.5219935516106,17.0318725286534,6.9));
#42367=CARTESIAN_POINT('Origin',(55.,21.,6.9));
#42368=CARTESIAN_POINT('',(56.5219935516106,17.0318725286534,2.9));
#42369=CARTESIAN_POINT('',(56.5219935516106,17.0318725286534,7.5));
#42370=CARTESIAN_POINT('',(57.0614434020148,17.2834221250874,2.9));
#42371=CARTESIAN_POINT('Origin',(55.,21.,2.9));
#42372=CARTESIAN_POINT('',(57.0614434020148,17.2834221250874,6.9));
#42373=CARTESIAN_POINT('',(57.0614434020148,17.2834221250874,7.5));
#42374=CARTESIAN_POINT('',(57.1879291538101,17.3564487079351,6.9));
#42375=CARTESIAN_POINT('Origin',(55.,21.,6.9));
#42376=CARTESIAN_POINT('',(57.1879291538101,17.3564487079351,2.9));
#42377=CARTESIAN_POINT('',(57.1879291538101,17.3564487079351,7.5));
#42378=CARTESIAN_POINT('',(57.6755024198358,17.6978511842358,2.9));
#42379=CARTESIAN_POINT('Origin',(55.,21.,2.9));
#42380=CARTESIAN_POINT('',(57.6755024198358,17.6978511842358,6.9));
#42381=CARTESIAN_POINT('',(57.6755024198358,17.6978511842358,7.5));
#42382=CARTESIAN_POINT('',(57.7873856358167,17.7917323495003,6.9));
#42383=CARTESIAN_POINT('Origin',(55.,21.,6.9));
#42384=CARTESIAN_POINT('',(57.7873856358167,17.7917323495003,2.9));
#42385=CARTESIAN_POINT('',(57.7873856358167,17.7917323495003,7.5));
#42386=CARTESIAN_POINT('',(58.2082676504997,18.2126143641833,2.9));
#42387=CARTESIAN_POINT('Origin',(55.,21.,2.9));
#42388=CARTESIAN_POINT('',(58.2082676504997,18.2126143641833,6.9));
#42389=CARTESIAN_POINT('',(58.2082676504997,18.2126143641833,7.5));
#42390=CARTESIAN_POINT('',(58.3021488157642,18.3244975801642,6.9));
#42391=CARTESIAN_POINT('Origin',(55.,21.,6.9));
#42392=CARTESIAN_POINT('',(58.3021488157642,18.3244975801642,2.9));
#42393=CARTESIAN_POINT('',(58.3021488157642,18.3244975801642,7.5));
#42394=CARTESIAN_POINT('',(58.6435512920649,18.8120708461899,2.9));
#42395=CARTESIAN_POINT('Origin',(55.,21.,2.9));
#42396=CARTESIAN_POINT('',(58.6435512920649,18.8120708461899,6.9));
#42397=CARTESIAN_POINT('',(58.6435512920649,18.8120708461899,7.5));
#42398=CARTESIAN_POINT('',(58.7165778749126,18.9385565979853,6.9));
#42399=CARTESIAN_POINT('Origin',(55.,21.,6.9));
#42400=CARTESIAN_POINT('',(58.7165778749126,18.9385565979853,2.9));
#42401=CARTESIAN_POINT('',(58.7165778749126,18.9385565979853,7.5));
#42402=CARTESIAN_POINT('',(58.9681274713466,19.4780064483894,2.9));
#42403=CARTESIAN_POINT('Origin',(55.,21.,2.9));
#42404=CARTESIAN_POINT('',(58.9681274713466,19.4780064483894,6.9));
#42405=CARTESIAN_POINT('',(58.9681274713466,19.4780064483894,7.5));
#42406=CARTESIAN_POINT('',(59.0180805960109,19.6152515304358,6.9));
#42407=CARTESIAN_POINT('Origin',(55.,21.,6.9));
#42408=CARTESIAN_POINT('',(59.0180805960109,19.6152515304358,2.9));
#42409=CARTESIAN_POINT('',(59.0180805960109,19.6152515304358,7.5));
#42410=CARTESIAN_POINT('Origin',(55.,21.,2.9));
#42411=CARTESIAN_POINT('',(59.2493725558249,20.9269734171523,2.9));
#42412=CARTESIAN_POINT('Origin',(55.,21.,2.9));
#42413=CARTESIAN_POINT('',(59.2493725558249,20.9269734171523,6.9));
#42414=CARTESIAN_POINT('',(59.2493725558249,20.9269734171523,7.5));
#42415=CARTESIAN_POINT('',(59.2493725558249,21.0730265828477,6.9));
#42416=CARTESIAN_POINT('Origin',(55.,21.,6.9));
#42417=CARTESIAN_POINT('',(59.2493725558249,21.0730265828477,2.9));
#42418=CARTESIAN_POINT('',(59.2493725558249,21.0730265828477,7.5));
#42419=CARTESIAN_POINT('',(59.1974959714464,21.6659786555824,2.9));
#42420=CARTESIAN_POINT('Origin',(55.,21.,2.9));
#42421=CARTESIAN_POINT('',(59.1974959714464,21.6659786555824,6.9));
#42422=CARTESIAN_POINT('',(59.1974959714464,21.6659786555824,7.5));
#42423=CARTESIAN_POINT('',(59.1721341053809,21.8098129455113,6.9));
#42424=CARTESIAN_POINT('Origin',(55.,21.,6.9));
#42425=CARTESIAN_POINT('',(59.1721341053809,21.8098129455113,2.9));
#42426=CARTESIAN_POINT('',(59.1721341053809,21.8098129455113,7.5));
#42427=CARTESIAN_POINT('',(59.0180805960109,22.3847484695642,2.9));
#42428=CARTESIAN_POINT('Origin',(55.,21.,2.9));
#42429=CARTESIAN_POINT('',(59.0180805960109,22.3847484695642,6.9));
#42430=CARTESIAN_POINT('',(59.0180805960109,22.3847484695642,7.5));
#42431=CARTESIAN_POINT('',(58.9681274713466,22.5219935516106,6.9));
#42432=CARTESIAN_POINT('Origin',(55.,21.,6.9));
#42433=CARTESIAN_POINT('',(58.9681274713466,22.5219935516106,2.9));
#42434=CARTESIAN_POINT('',(58.9681274713466,22.5219935516106,7.5));
#42435=CARTESIAN_POINT('',(58.7165778749126,23.0614434020147,2.9));
#42436=CARTESIAN_POINT('Origin',(55.,21.,2.9));
#42437=CARTESIAN_POINT('',(58.7165778749126,23.0614434020147,6.9));
#42438=CARTESIAN_POINT('',(58.7165778749126,23.0614434020147,7.5));
#42439=CARTESIAN_POINT('',(58.6435512920649,23.1879291538101,6.9));
#42440=CARTESIAN_POINT('Origin',(55.,21.,6.9));
#42441=CARTESIAN_POINT('',(58.6435512920649,23.1879291538101,2.9));
#42442=CARTESIAN_POINT('',(58.6435512920649,23.1879291538101,7.5));
#42443=CARTESIAN_POINT('',(58.3021488157642,23.6755024198358,2.9));
#42444=CARTESIAN_POINT('Origin',(55.,21.,2.9));
#42445=CARTESIAN_POINT('',(58.3021488157642,23.6755024198358,6.9));
#42446=CARTESIAN_POINT('',(58.3021488157642,23.6755024198358,7.5));
#42447=CARTESIAN_POINT('',(58.2082676504997,23.7873856358167,6.9));
#42448=CARTESIAN_POINT('Origin',(55.,21.,6.9));
#42449=CARTESIAN_POINT('',(58.2082676504997,23.7873856358167,2.9));
#42450=CARTESIAN_POINT('',(58.2082676504997,23.7873856358167,7.5));
#42451=CARTESIAN_POINT('',(57.7873856358167,24.2082676504997,2.9));
#42452=CARTESIAN_POINT('Origin',(55.,21.,2.9));
#42453=CARTESIAN_POINT('',(57.7873856358167,24.2082676504997,6.9));
#42454=CARTESIAN_POINT('',(57.7873856358167,24.2082676504997,7.5));
#42455=CARTESIAN_POINT('',(57.6755024198358,24.3021488157642,6.9));
#42456=CARTESIAN_POINT('Origin',(55.,21.,6.9));
#42457=CARTESIAN_POINT('',(57.6755024198358,24.3021488157642,2.9));
#42458=CARTESIAN_POINT('',(57.6755024198358,24.3021488157642,7.5));
#42459=CARTESIAN_POINT('',(57.1879291538101,24.6435512920649,2.9));
#42460=CARTESIAN_POINT('Origin',(55.,21.,2.9));
#42461=CARTESIAN_POINT('',(57.1879291538101,24.6435512920649,6.9));
#42462=CARTESIAN_POINT('',(57.1879291538101,24.6435512920649,7.5));
#42463=CARTESIAN_POINT('',(57.0614434020147,24.7165778749126,6.9));
#42464=CARTESIAN_POINT('Origin',(55.,21.,6.9));
#42465=CARTESIAN_POINT('',(57.0614434020147,24.7165778749126,2.9));
#42466=CARTESIAN_POINT('',(57.0614434020147,24.7165778749126,7.5));
#42467=CARTESIAN_POINT('',(56.5219935516106,24.9681274713466,2.9));
#42468=CARTESIAN_POINT('Origin',(55.,21.,2.9));
#42469=CARTESIAN_POINT('',(56.5219935516106,24.9681274713466,6.9));
#42470=CARTESIAN_POINT('',(56.5219935516106,24.9681274713466,7.5));
#42471=CARTESIAN_POINT('',(56.3847484695642,25.0180805960109,6.9));
#42472=CARTESIAN_POINT('Origin',(55.,21.,6.9));
#42473=CARTESIAN_POINT('',(56.3847484695642,25.0180805960109,2.9));
#42474=CARTESIAN_POINT('',(56.3847484695642,25.0180805960109,7.5));
#42475=CARTESIAN_POINT('',(55.8098129455113,25.1721341053809,2.9));
#42476=CARTESIAN_POINT('Origin',(55.,21.,2.9));
#42477=CARTESIAN_POINT('',(55.8098129455113,25.1721341053809,6.9));
#42478=CARTESIAN_POINT('',(55.8098129455113,25.1721341053809,7.5));
#42479=CARTESIAN_POINT('',(55.6659786555824,25.1974959714464,6.9));
#42480=CARTESIAN_POINT('Origin',(55.,21.,6.9));
#42481=CARTESIAN_POINT('',(55.6659786555824,25.1974959714464,2.9));
#42482=CARTESIAN_POINT('',(55.6659786555824,25.1974959714464,7.5));
#42483=CARTESIAN_POINT('',(55.0730265828477,25.2493725558249,2.9));
#42484=CARTESIAN_POINT('Origin',(55.,21.,2.9));
#42485=CARTESIAN_POINT('',(55.0730265828477,25.2493725558249,6.9));
#42486=CARTESIAN_POINT('',(55.0730265828477,25.2493725558249,7.5));
#42487=CARTESIAN_POINT('',(54.9269734171523,25.2493725558249,6.9));
#42488=CARTESIAN_POINT('Origin',(55.,21.,6.9));
#42489=CARTESIAN_POINT('',(54.9269734171523,25.2493725558249,2.9));
#42490=CARTESIAN_POINT('',(54.9269734171523,25.2493725558249,7.5));
#42491=CARTESIAN_POINT('',(54.3340213444176,25.1974959714464,2.9));
#42492=CARTESIAN_POINT('Origin',(55.,21.,2.9));
#42493=CARTESIAN_POINT('',(54.3340213444176,25.1974959714464,6.9));
#42494=CARTESIAN_POINT('',(54.3340213444176,25.1974959714464,7.5));
#42495=CARTESIAN_POINT('',(54.1901870544887,25.1721341053809,6.9));
#42496=CARTESIAN_POINT('Origin',(55.,21.,6.9));
#42497=CARTESIAN_POINT('',(54.1901870544887,25.1721341053809,2.9));
#42498=CARTESIAN_POINT('',(54.1901870544887,25.1721341053809,7.5));
#42499=CARTESIAN_POINT('',(53.6152515304358,25.0180805960109,2.9));
#42500=CARTESIAN_POINT('Origin',(55.,21.,2.9));
#42501=CARTESIAN_POINT('',(53.6152515304358,25.0180805960109,6.9));
#42502=CARTESIAN_POINT('',(53.6152515304358,25.0180805960109,7.5));
#42503=CARTESIAN_POINT('',(53.4780064483894,24.9681274713466,6.9));
#42504=CARTESIAN_POINT('Origin',(55.,21.,6.9));
#42505=CARTESIAN_POINT('',(53.4780064483894,24.9681274713466,2.9));
#42506=CARTESIAN_POINT('',(53.4780064483894,24.9681274713466,7.5));
#42507=CARTESIAN_POINT('',(52.9385565979853,24.7165778749126,2.9));
#42508=CARTESIAN_POINT('Origin',(55.,21.,2.9));
#42509=CARTESIAN_POINT('',(52.9385565979853,24.7165778749126,6.9));
#42510=CARTESIAN_POINT('',(52.9385565979853,24.7165778749126,7.5));
#42511=CARTESIAN_POINT('',(52.8120708461899,24.6435512920649,6.9));
#42512=CARTESIAN_POINT('Origin',(55.,21.,6.9));
#42513=CARTESIAN_POINT('',(52.8120708461899,24.6435512920649,2.9));
#42514=CARTESIAN_POINT('',(52.8120708461899,24.6435512920649,7.5));
#42515=CARTESIAN_POINT('',(52.3244975801642,24.3021488157642,2.9));
#42516=CARTESIAN_POINT('Origin',(55.,21.,2.9));
#42517=CARTESIAN_POINT('',(52.3244975801642,24.3021488157642,6.9));
#42518=CARTESIAN_POINT('',(52.3244975801642,24.3021488157642,7.5));
#42519=CARTESIAN_POINT('',(52.2126143641833,24.2082676504997,6.9));
#42520=CARTESIAN_POINT('Origin',(55.,21.,6.9));
#42521=CARTESIAN_POINT('',(52.2126143641833,24.2082676504997,2.9));
#42522=CARTESIAN_POINT('',(52.2126143641833,24.2082676504997,7.5));
#42523=CARTESIAN_POINT('',(51.7917323495003,23.7873856358167,2.9));
#42524=CARTESIAN_POINT('Origin',(55.,21.,2.9));
#42525=CARTESIAN_POINT('',(51.7917323495003,23.7873856358167,6.9));
#42526=CARTESIAN_POINT('',(51.7917323495003,23.7873856358167,7.5));
#42527=CARTESIAN_POINT('',(51.6978511842358,23.6755024198358,6.9));
#42528=CARTESIAN_POINT('Origin',(55.,21.,6.9));
#42529=CARTESIAN_POINT('',(51.6978511842358,23.6755024198358,2.9));
#42530=CARTESIAN_POINT('',(51.6978511842358,23.6755024198358,7.5));
#42531=CARTESIAN_POINT('',(51.3564487079351,23.1879291538101,2.9));
#42532=CARTESIAN_POINT('Origin',(55.,21.,2.9));
#42533=CARTESIAN_POINT('',(51.3564487079351,23.1879291538101,6.9));
#42534=CARTESIAN_POINT('',(51.3564487079351,23.1879291538101,7.5));
#42535=CARTESIAN_POINT('',(51.2834221250874,23.0614434020147,6.9));
#42536=CARTESIAN_POINT('Origin',(55.,21.,6.9));
#42537=CARTESIAN_POINT('',(51.2834221250874,23.0614434020147,2.9));
#42538=CARTESIAN_POINT('',(51.2834221250874,23.0614434020147,7.5));
#42539=CARTESIAN_POINT('',(51.0318725286534,22.5219935516106,2.9));
#42540=CARTESIAN_POINT('Origin',(55.,21.,2.9));
#42541=CARTESIAN_POINT('',(51.0318725286534,22.5219935516106,6.9));
#42542=CARTESIAN_POINT('',(51.0318725286534,22.5219935516106,7.5));
#42543=CARTESIAN_POINT('',(50.9819194039891,22.3847484695642,6.9));
#42544=CARTESIAN_POINT('Origin',(55.,21.,6.9));
#42545=CARTESIAN_POINT('',(50.9819194039891,22.3847484695642,2.9));
#42546=CARTESIAN_POINT('',(50.9819194039891,22.3847484695642,7.5));
#42547=CARTESIAN_POINT('',(50.8278658946191,21.8098129455113,2.9));
#42548=CARTESIAN_POINT('Origin',(55.,21.,2.9));
#42549=CARTESIAN_POINT('',(50.8278658946191,21.8098129455113,6.9));
#42550=CARTESIAN_POINT('',(50.8278658946191,21.8098129455113,7.5));
#42551=CARTESIAN_POINT('',(50.8025040285536,21.6659786555824,6.9));
#42552=CARTESIAN_POINT('Origin',(55.,21.,6.9));
#42553=CARTESIAN_POINT('',(50.8025040285536,21.6659786555824,2.9));
#42554=CARTESIAN_POINT('',(50.8025040285536,21.6659786555824,7.5));
#42555=CARTESIAN_POINT('',(50.7506274441751,21.0730265828477,2.9));
#42556=CARTESIAN_POINT('Origin',(55.,21.,2.9));
#42557=CARTESIAN_POINT('',(50.7506274441751,21.0730265828477,7.5));
#42558=CARTESIAN_POINT('Origin',(59.3508458561075,19.6505407244411,2.5));
#42559=CARTESIAN_POINT('',(58.8527397452222,19.5977174123648,6.9));
#42560=CARTESIAN_POINT('',(59.3508458561075,19.6505407244411,6.9));
#42561=CARTESIAN_POINT('',(58.8527397452222,19.5977174123648,2.75));
#42562=CARTESIAN_POINT('',(58.8527397452222,19.5977174123648,2.5));
#42563=CARTESIAN_POINT('Ctrl Pts',(59.018080596011,19.6152515304358,2.90000000000003));
#42564=CARTESIAN_POINT('Ctrl Pts',(58.9339250731542,19.6063269793218,2.82334460824915));
#42565=CARTESIAN_POINT('Ctrl Pts',(58.8527397452222,19.5977174123648,2.75));
#42566=CARTESIAN_POINT('Origin',(58.8527397452222,19.5977174123648,2.5));
#42567=CARTESIAN_POINT('Ctrl Pts',(58.8527397452222,19.5977174123648,2.75));
#42568=CARTESIAN_POINT('Ctrl Pts',(58.9093971915826,19.5389371785566,2.82334460824922));
#42569=CARTESIAN_POINT('Ctrl Pts',(58.9681274713466,19.4780064483894,2.90000000000003));
#42570=CARTESIAN_POINT('',(58.8527397452222,19.5977174123648,6.9));
#42571=CARTESIAN_POINT('Origin',(59.0641705848991,19.5207628801165,6.9));
#42572=CARTESIAN_POINT('Origin',(55.,21.,2.7));
#42573=CARTESIAN_POINT('',(50.9,21.,2.75000000000001));
#42574=CARTESIAN_POINT('Ctrl Pts',(50.9,21.,2.75000000000001));
#42575=CARTESIAN_POINT('Ctrl Pts',(50.826655391751,21.0358573640328,2.82334460824898));
#42576=CARTESIAN_POINT('Ctrl Pts',(50.7506274441751,21.0730265828477,2.90000000000001));
#42577=CARTESIAN_POINT('',(50.9622882126499,21.7119575284344,2.75));
#42578=CARTESIAN_POINT('Ctrl Pts',(50.8025040285536,21.6659786555824,2.90000000000001));
#42579=CARTESIAN_POINT('Ctrl Pts',(50.8838313078845,21.6893810758964,2.82334460824893));
#42580=CARTESIAN_POINT('Ctrl Pts',(50.9622882126499,21.7119575284344,2.75));
#42581=CARTESIAN_POINT('Ctrl Pts',(50.96228821265,21.7119575284344,2.75));
#42582=CARTESIAN_POINT('Ctrl Pts',(50.8962844397247,21.7600062961009,2.82334460824929));
#42583=CARTESIAN_POINT('Ctrl Pts',(50.8278658946191,21.8098129455113,2.90000000000001));
#42584=CARTESIAN_POINT('',(51.1472602547778,22.4022825876352,2.75000000000001));
#42585=CARTESIAN_POINT('Ctrl Pts',(50.9819194039891,22.3847484695642,2.90000000000001));
#42586=CARTESIAN_POINT('Ctrl Pts',(51.0660749268463,22.3936730206783,2.8233446082487));
#42587=CARTESIAN_POINT('Ctrl Pts',(51.1472602547778,22.4022825876352,2.75000000000001));
#42588=CARTESIAN_POINT('Ctrl Pts',(51.1472602547778,22.4022825876352,2.75000000000001));
#42589=CARTESIAN_POINT('Ctrl Pts',(51.0906028084177,22.4610628214431,2.82334460824887));
#42590=CARTESIAN_POINT('Ctrl Pts',(51.0318725286534,22.5219935516106,2.90000000000001));
#42591=CARTESIAN_POINT('',(51.4492958444838,23.05,2.75000000000001));
#42592=CARTESIAN_POINT('Ctrl Pts',(51.2834221250874,23.0614434020147,2.90000000000001));
#42593=CARTESIAN_POINT('Ctrl Pts',(51.3678488684927,23.0556189159593,2.82334460824942));
#42594=CARTESIAN_POINT('Ctrl Pts',(51.4492958444838,23.05,2.75000000000001));
#42595=CARTESIAN_POINT('Ctrl Pts',(51.4492958444838,23.05,2.75000000000001));
#42596=CARTESIAN_POINT('Ctrl Pts',(51.4037062325258,23.1177256922899,2.82334460824926));
#42597=CARTESIAN_POINT('Ctrl Pts',(51.3564487079351,23.1879291538101,2.90000000000001));
#42598=CARTESIAN_POINT('',(51.8592177832122,23.6354291997148,2.75000000000001));
#42599=CARTESIAN_POINT('Ctrl Pts',(51.6978511842358,23.6755024198358,2.90000000000001));
#42600=CARTESIAN_POINT('Ctrl Pts',(51.7799838843138,23.6551058706724,2.82334460824921));
#42601=CARTESIAN_POINT('Ctrl Pts',(51.8592177832122,23.6354291997148,2.75000000000001));
#42602=CARTESIAN_POINT('Ctrl Pts',(51.8592177832122,23.6354291997148,2.75000000000001));
#42603=CARTESIAN_POINT('Ctrl Pts',(51.8260812229464,23.7100425395973,2.8233446082495));
#42604=CARTESIAN_POINT('Ctrl Pts',(51.7917323495003,23.7873856358167,2.90000000000001));
#42605=CARTESIAN_POINT('',(52.3645708002852,24.1407822167878,2.75));
#42606=CARTESIAN_POINT('Ctrl Pts',(52.2126143641833,24.2082676504997,2.90000000000001));
#42607=CARTESIAN_POINT('Ctrl Pts',(52.2899574604024,24.1739187770537,2.82334460824978));
#42608=CARTESIAN_POINT('Ctrl Pts',(52.3645708002852,24.1407822167878,2.75));
#42609=CARTESIAN_POINT('Ctrl Pts',(52.3645708002852,24.1407822167878,2.75));
#42610=CARTESIAN_POINT('Ctrl Pts',(52.3448941293277,24.220016115686,2.82334460824898));
#42611=CARTESIAN_POINT('Ctrl Pts',(52.3244975801642,24.3021488157642,2.90000000000001));
#42612=CARTESIAN_POINT('',(52.95,24.5507041555162,2.75));
#42613=CARTESIAN_POINT('Ctrl Pts',(52.8120708461899,24.6435512920649,2.90000000000001));
#42614=CARTESIAN_POINT('Ctrl Pts',(52.8822743077101,24.5962937674742,2.82334460824929));
#42615=CARTESIAN_POINT('Ctrl Pts',(52.95,24.5507041555162,2.75));
#42616=CARTESIAN_POINT('Ctrl Pts',(52.95,24.5507041555162,2.75));
#42617=CARTESIAN_POINT('Ctrl Pts',(52.9443810840407,24.6321511315072,2.8233446082493));
#42618=CARTESIAN_POINT('Ctrl Pts',(52.9385565979853,24.7165778749126,2.9));
#42619=CARTESIAN_POINT('',(53.5977174123648,24.8527397452222,2.75));
#42620=CARTESIAN_POINT('Ctrl Pts',(53.4780064483894,24.9681274713466,2.90000000000001));
#42621=CARTESIAN_POINT('Ctrl Pts',(53.5389371785568,24.9093971915825,2.82334460824902));
#42622=CARTESIAN_POINT('Ctrl Pts',(53.5977174123648,24.8527397452222,2.75));
#42623=CARTESIAN_POINT('Ctrl Pts',(53.5977174123648,24.8527397452222,2.75));
#42624=CARTESIAN_POINT('Ctrl Pts',(53.6063269793218,24.9339250731547,2.82334460824958));
#42625=CARTESIAN_POINT('Ctrl Pts',(53.6152515304358,25.018080596011,2.90000000000001));
#42626=CARTESIAN_POINT('',(54.2880424715656,25.0377117873501,2.75000000000001));
#42627=CARTESIAN_POINT('Ctrl Pts',(54.1901870544887,25.1721341053809,2.9));
#42628=CARTESIAN_POINT('Ctrl Pts',(54.2399937038992,25.1037155602753,2.82334460824924));
#42629=CARTESIAN_POINT('Ctrl Pts',(54.2880424715656,25.0377117873501,2.75000000000001));
#42630=CARTESIAN_POINT('Ctrl Pts',(54.2880424715656,25.0377117873501,2.75000000000001));
#42631=CARTESIAN_POINT('Ctrl Pts',(54.3106189241037,25.1161686921158,2.82334460824925));
#42632=CARTESIAN_POINT('Ctrl Pts',(54.3340213444176,25.1974959714464,2.90000000000001));
#42633=CARTESIAN_POINT('',(55.,25.1,2.75));
#42634=CARTESIAN_POINT('Ctrl Pts',(54.9269734171523,25.2493725558249,2.9));
#42635=CARTESIAN_POINT('Ctrl Pts',(54.9641426359669,25.1733446082495,2.82334460824949));
#42636=CARTESIAN_POINT('Ctrl Pts',(55.,25.1,2.75));
#42637=CARTESIAN_POINT('Ctrl Pts',(55.,25.1,2.75));
#42638=CARTESIAN_POINT('Ctrl Pts',(55.0358573640329,25.173344608249,2.82334460824903));
#42639=CARTESIAN_POINT('Ctrl Pts',(55.0730265828477,25.2493725558249,2.90000000000001));
#42640=CARTESIAN_POINT('',(55.7119575284344,25.0377117873501,2.75000000000001));
#42641=CARTESIAN_POINT('Ctrl Pts',(55.6659786555824,25.1974959714464,2.90000000000001));
#42642=CARTESIAN_POINT('Ctrl Pts',(55.6893810758964,25.1161686921158,2.82334460824919));
#42643=CARTESIAN_POINT('Ctrl Pts',(55.7119575284344,25.0377117873501,2.75000000000001));
#42644=CARTESIAN_POINT('Ctrl Pts',(55.7119575284344,25.0377117873501,2.75000000000001));
#42645=CARTESIAN_POINT('Ctrl Pts',(55.7600062961009,25.1037155602753,2.82334460824931));
#42646=CARTESIAN_POINT('Ctrl Pts',(55.8098129455113,25.1721341053809,2.9));
#42647=CARTESIAN_POINT('',(56.4022825876352,24.8527397452222,2.75000000000001));
#42648=CARTESIAN_POINT('Ctrl Pts',(56.3847484695642,25.0180805960109,2.9));
#42649=CARTESIAN_POINT('Ctrl Pts',(56.3936730206782,24.9339250731545,2.82334460824946));
#42650=CARTESIAN_POINT('Ctrl Pts',(56.4022825876352,24.8527397452222,2.75000000000001));
#42651=CARTESIAN_POINT('Ctrl Pts',(56.4022825876352,24.8527397452222,2.75000000000001));
#42652=CARTESIAN_POINT('Ctrl Pts',(56.4610628214436,24.9093971915828,2.82334460824951));
#42653=CARTESIAN_POINT('Ctrl Pts',(56.5219935516106,24.9681274713466,2.90000000000001));
#42654=CARTESIAN_POINT('',(57.05,24.5507041555162,2.75000000000001));
#42655=CARTESIAN_POINT('Ctrl Pts',(57.0614434020147,24.7165778749126,2.9));
#42656=CARTESIAN_POINT('Ctrl Pts',(57.0556189159594,24.6321511315074,2.82334460824945));
#42657=CARTESIAN_POINT('Ctrl Pts',(57.05,24.5507041555162,2.75000000000001));
#42658=CARTESIAN_POINT('Ctrl Pts',(57.05,24.5507041555162,2.75000000000001));
#42659=CARTESIAN_POINT('Ctrl Pts',(57.1177256922902,24.5962937674744,2.82334460824958));
#42660=CARTESIAN_POINT('Ctrl Pts',(57.1879291538101,24.6435512920649,2.9));
#42661=CARTESIAN_POINT('',(57.6354291997148,24.1407822167878,2.75000000000001));
#42662=CARTESIAN_POINT('Ctrl Pts',(57.6755024198358,24.3021488157642,2.9));
#42663=CARTESIAN_POINT('Ctrl Pts',(57.6551058706725,24.2200161156869,2.82334460824982));
#42664=CARTESIAN_POINT('Ctrl Pts',(57.6354291997148,24.1407822167878,2.75000000000001));
#42665=CARTESIAN_POINT('Ctrl Pts',(57.6354291997148,24.1407822167878,2.75000000000001));
#42666=CARTESIAN_POINT('Ctrl Pts',(57.7100425395966,24.1739187770533,2.82334460824876));
#42667=CARTESIAN_POINT('Ctrl Pts',(57.7873856358167,24.2082676504997,2.9));
#42668=CARTESIAN_POINT('',(58.1407822167878,23.6354291997148,2.75000000000001));
#42669=CARTESIAN_POINT('Ctrl Pts',(58.2082676504997,23.7873856358167,2.9));
#42670=CARTESIAN_POINT('Ctrl Pts',(58.1739187770533,23.7100425395967,2.82334460824884));
#42671=CARTESIAN_POINT('Ctrl Pts',(58.1407822167878,23.6354291997148,2.75000000000001));
#42672=CARTESIAN_POINT('Ctrl Pts',(58.1407822167878,23.6354291997148,2.75000000000001));
#42673=CARTESIAN_POINT('Ctrl Pts',(58.220016115686,23.6551058706723,2.82334460824898));
#42674=CARTESIAN_POINT('Ctrl Pts',(58.3021488157642,23.6755024198358,2.9));
#42675=CARTESIAN_POINT('',(58.5507041555162,23.05,2.75));
#42676=CARTESIAN_POINT('Ctrl Pts',(58.6435512920649,23.1879291538101,2.9));
#42677=CARTESIAN_POINT('Ctrl Pts',(58.5962937674744,23.1177256922902,2.82334460824956));
#42678=CARTESIAN_POINT('Ctrl Pts',(58.5507041555162,23.05,2.75));
#42679=CARTESIAN_POINT('Ctrl Pts',(58.5507041555162,23.05,2.75));
#42680=CARTESIAN_POINT('Ctrl Pts',(58.632151131507,23.0556189159593,2.82334460824912));
#42681=CARTESIAN_POINT('Ctrl Pts',(58.7165778749126,23.0614434020147,2.9));
#42682=CARTESIAN_POINT('',(58.8527397452222,22.4022825876352,2.75));
#42683=CARTESIAN_POINT('Ctrl Pts',(58.9681274713466,22.5219935516106,2.9));
#42684=CARTESIAN_POINT('Ctrl Pts',(58.9093971915824,22.4610628214431,2.82334460824888));
#42685=CARTESIAN_POINT('Ctrl Pts',(58.8527397452222,22.4022825876352,2.75));
#42686=CARTESIAN_POINT('Ctrl Pts',(58.8527397452222,22.4022825876352,2.75));
#42687=CARTESIAN_POINT('Ctrl Pts',(58.933925073154,22.3936730206782,2.82334460824898));
#42688=CARTESIAN_POINT('Ctrl Pts',(59.0180805960109,22.3847484695642,2.9));
#42689=CARTESIAN_POINT('',(59.0377117873501,21.7119575284344,2.75000000000001));
#42690=CARTESIAN_POINT('Ctrl Pts',(59.1721341053809,21.8098129455113,2.9));
#42691=CARTESIAN_POINT('Ctrl Pts',(59.1037155602755,21.760006296101,2.82334460824946));
#42692=CARTESIAN_POINT('Ctrl Pts',(59.0377117873501,21.7119575284344,2.75000000000001));
#42693=CARTESIAN_POINT('Ctrl Pts',(59.0377117873501,21.7119575284344,2.75000000000001));
#42694=CARTESIAN_POINT('Ctrl Pts',(59.116168692116,21.6893810758963,2.82334460824939));
#42695=CARTESIAN_POINT('Ctrl Pts',(59.1974959714464,21.6659786555824,2.9));
#42696=CARTESIAN_POINT('',(59.1,21.,2.75000000000001));
#42697=CARTESIAN_POINT('Ctrl Pts',(59.2493725558249,21.0730265828477,2.9));
#42698=CARTESIAN_POINT('Ctrl Pts',(59.1733446082494,21.035857364033,2.82334460824937));
#42699=CARTESIAN_POINT('Ctrl Pts',(59.1,21.,2.75000000000001));
#42700=CARTESIAN_POINT('Ctrl Pts',(59.1,21.,2.75000000000001));
#42701=CARTESIAN_POINT('Ctrl Pts',(59.1733446082493,20.964142635967,2.82334460824927));
#42702=CARTESIAN_POINT('Ctrl Pts',(59.2493725558249,20.9269734171523,2.9));
#42703=CARTESIAN_POINT('',(58.5507041555162,18.95,2.75));
#42704=CARTESIAN_POINT('Ctrl Pts',(58.7165778749126,18.9385565979853,2.90000000000002));
#42705=CARTESIAN_POINT('Ctrl Pts',(58.6321511315069,18.9443810840407,2.82334460824905));
#42706=CARTESIAN_POINT('Ctrl Pts',(58.5507041555162,18.95,2.75));
#42707=CARTESIAN_POINT('Ctrl Pts',(58.5507041555162,18.95,2.75));
#42708=CARTESIAN_POINT('Ctrl Pts',(58.596293767474,18.8822743077104,2.8233446082489));
#42709=CARTESIAN_POINT('Ctrl Pts',(58.6435512920649,18.8120708461898,2.90000000000003));
#42710=CARTESIAN_POINT('',(58.1407822167878,18.3645708002852,2.74999999999999));
#42711=CARTESIAN_POINT('Ctrl Pts',(58.3021488157642,18.3244975801642,2.90000000000002));
#42712=CARTESIAN_POINT('Ctrl Pts',(58.2200161156863,18.3448941293276,2.82334460824921));
#42713=CARTESIAN_POINT('Ctrl Pts',(58.1407822167878,18.3645708002852,2.74999999999999));
#42714=CARTESIAN_POINT('Ctrl Pts',(58.1407822167878,18.3645708002852,2.74999999999999));
#42715=CARTESIAN_POINT('Ctrl Pts',(58.1739187770535,18.2899574604028,2.82334460824939));
#42716=CARTESIAN_POINT('Ctrl Pts',(58.2082676504997,18.2126143641833,2.90000000000002));
#42717=CARTESIAN_POINT('',(57.6354291997148,17.8592177832122,2.75000000000001));
#42718=CARTESIAN_POINT('Ctrl Pts',(57.7873856358167,17.7917323495003,2.90000000000002));
#42719=CARTESIAN_POINT('Ctrl Pts',(57.7100425395974,17.8260812229464,2.82334460824953));
#42720=CARTESIAN_POINT('Ctrl Pts',(57.6354291997148,17.8592177832122,2.75000000000001));
#42721=CARTESIAN_POINT('Ctrl Pts',(57.6354291997148,17.8592177832122,2.75000000000001));
#42722=CARTESIAN_POINT('Ctrl Pts',(57.6551058706724,17.7799838843136,2.82334460824937));
#42723=CARTESIAN_POINT('Ctrl Pts',(57.6755024198358,17.6978511842358,2.90000000000002));
#42724=CARTESIAN_POINT('',(57.05,17.4492958444838,2.75));
#42725=CARTESIAN_POINT('Ctrl Pts',(57.1879291538101,17.3564487079351,2.90000000000002));
#42726=CARTESIAN_POINT('Ctrl Pts',(57.1177256922899,17.4037062325258,2.82334460824927));
#42727=CARTESIAN_POINT('Ctrl Pts',(57.05,17.4492958444838,2.75));
#42728=CARTESIAN_POINT('Ctrl Pts',(57.05,17.4492958444838,2.75));
#42729=CARTESIAN_POINT('Ctrl Pts',(57.0556189159594,17.3678488684924,2.82334460824966));
#42730=CARTESIAN_POINT('Ctrl Pts',(57.0614434020148,17.2834221250874,2.90000000000002));
#42731=CARTESIAN_POINT('',(56.4022825876352,17.1472602547778,2.75000000000001));
#42732=CARTESIAN_POINT('Ctrl Pts',(56.5219935516106,17.0318725286534,2.90000000000002));
#42733=CARTESIAN_POINT('Ctrl Pts',(56.4610628214436,17.0906028084172,2.82334460824948));
#42734=CARTESIAN_POINT('Ctrl Pts',(56.4022825876352,17.1472602547778,2.75000000000001));
#42735=CARTESIAN_POINT('Ctrl Pts',(56.4022825876352,17.1472602547778,2.75000000000001));
#42736=CARTESIAN_POINT('Ctrl Pts',(56.3936730206782,17.0660749268454,2.82334460824955));
#42737=CARTESIAN_POINT('Ctrl Pts',(56.3847484695642,16.981919403989,2.90000000000002));
#42738=CARTESIAN_POINT('',(55.7119575284344,16.9622882126499,2.75000000000001));
#42739=CARTESIAN_POINT('Ctrl Pts',(55.8098129455113,16.8278658946191,2.90000000000002));
#42740=CARTESIAN_POINT('Ctrl Pts',(55.760006296101,16.8962844397245,2.82334460824944));
#42741=CARTESIAN_POINT('Ctrl Pts',(55.7119575284344,16.9622882126499,2.75000000000001));
#42742=CARTESIAN_POINT('Ctrl Pts',(55.7119575284344,16.9622882126499,2.75000000000001));
#42743=CARTESIAN_POINT('Ctrl Pts',(55.6893810758963,16.8838313078841,2.82334460824935));
#42744=CARTESIAN_POINT('Ctrl Pts',(55.6659786555824,16.8025040285536,2.90000000000002));
#42745=CARTESIAN_POINT('',(55.,16.9,2.75000000000001));
#42746=CARTESIAN_POINT('Ctrl Pts',(55.0730265828477,16.7506274441751,2.90000000000002));
#42747=CARTESIAN_POINT('Ctrl Pts',(55.035857364033,16.8266553917508,2.82334460824925));
#42748=CARTESIAN_POINT('Ctrl Pts',(55.,16.9,2.75000000000001));
#42749=CARTESIAN_POINT('Ctrl Pts',(55.,16.9,2.75000000000001));
#42750=CARTESIAN_POINT('Ctrl Pts',(54.964142635967,16.8266553917506,2.82334460824936));
#42751=CARTESIAN_POINT('Ctrl Pts',(54.9269734171523,16.7506274441751,2.90000000000002));
#42752=CARTESIAN_POINT('',(54.2880424715656,16.9622882126499,2.75000000000002));
#42753=CARTESIAN_POINT('Ctrl Pts',(54.3340213444176,16.8025040285536,2.90000000000002));
#42754=CARTESIAN_POINT('Ctrl Pts',(54.3106189241037,16.8838313078841,2.82334460824935));
#42755=CARTESIAN_POINT('Ctrl Pts',(54.2880424715656,16.9622882126499,2.75000000000002));
#42756=CARTESIAN_POINT('Ctrl Pts',(54.2880424715656,16.9622882126499,2.75000000000002));
#42757=CARTESIAN_POINT('Ctrl Pts',(54.2399937038991,16.8962844397246,2.82334460824941));
#42758=CARTESIAN_POINT('Ctrl Pts',(54.1901870544887,16.8278658946191,2.90000000000002));
#42759=CARTESIAN_POINT('',(53.5977174123648,17.1472602547778,2.75));
#42760=CARTESIAN_POINT('Ctrl Pts',(53.6152515304358,16.981919403989,2.90000000000002));
#42761=CARTESIAN_POINT('Ctrl Pts',(53.6063269793218,17.0660749268453,2.82334460824959));
#42762=CARTESIAN_POINT('Ctrl Pts',(53.5977174123648,17.1472602547778,2.75));
#42763=CARTESIAN_POINT('Ctrl Pts',(53.5977174123648,17.1472602547778,2.75));
#42764=CARTESIAN_POINT('Ctrl Pts',(53.5389371785566,17.0906028084174,2.82334460824923));
#42765=CARTESIAN_POINT('Ctrl Pts',(53.4780064483894,17.0318725286534,2.90000000000002));
#42766=CARTESIAN_POINT('',(52.95,17.4492958444838,2.75));
#42767=CARTESIAN_POINT('Ctrl Pts',(52.9385565979853,17.2834221250874,2.90000000000002));
#42768=CARTESIAN_POINT('Ctrl Pts',(52.9443810840407,17.3678488684929,2.8233446082492));
#42769=CARTESIAN_POINT('Ctrl Pts',(52.95,17.4492958444838,2.75));
#42770=CARTESIAN_POINT('Ctrl Pts',(52.95,17.4492958444838,2.75));
#42771=CARTESIAN_POINT('Ctrl Pts',(52.88227430771,17.4037062325258,2.82334460824929));
#42772=CARTESIAN_POINT('Ctrl Pts',(52.8120708461899,17.3564487079351,2.90000000000002));
#42773=CARTESIAN_POINT('',(52.3645708002852,17.8592177832122,2.75000000000001));
#42774=CARTESIAN_POINT('Ctrl Pts',(52.3244975801642,17.6978511842358,2.90000000000002));
#42775=CARTESIAN_POINT('Ctrl Pts',(52.3448941293275,17.7799838843134,2.82334460824955));
#42776=CARTESIAN_POINT('Ctrl Pts',(52.3645708002852,17.8592177832122,2.75000000000001));
#42777=CARTESIAN_POINT('Ctrl Pts',(52.3645708002852,17.8592177832122,2.75000000000001));
#42778=CARTESIAN_POINT('Ctrl Pts',(52.2899574604026,17.8260812229464,2.82334460824958));
#42779=CARTESIAN_POINT('Ctrl Pts',(52.2126143641833,17.7917323495003,2.90000000000002));
#42780=CARTESIAN_POINT('',(51.8592177832122,18.3645708002852,2.75));
#42781=CARTESIAN_POINT('Ctrl Pts',(51.7917323495003,18.2126143641833,2.90000000000002));
#42782=CARTESIAN_POINT('Ctrl Pts',(51.8260812229464,18.2899574604027,2.82334460824945));
#42783=CARTESIAN_POINT('Ctrl Pts',(51.8592177832122,18.3645708002852,2.75));
#42784=CARTESIAN_POINT('Ctrl Pts',(51.8592177832122,18.3645708002852,2.75));
#42785=CARTESIAN_POINT('Ctrl Pts',(51.7799838843133,18.3448941293275,2.82334460824967));
#42786=CARTESIAN_POINT('Ctrl Pts',(51.6978511842358,18.3244975801642,2.90000000000001));
#42787=CARTESIAN_POINT('',(51.4492958444838,18.95,2.75));
#42788=CARTESIAN_POINT('Ctrl Pts',(51.3564487079351,18.8120708461899,2.90000000000001));
#42789=CARTESIAN_POINT('Ctrl Pts',(51.403706232526,18.8822743077104,2.82334460824892));
#42790=CARTESIAN_POINT('Ctrl Pts',(51.4492958444838,18.95,2.75));
#42791=CARTESIAN_POINT('Ctrl Pts',(51.4492958444838,18.95,2.75));
#42792=CARTESIAN_POINT('Ctrl Pts',(51.3678488684935,18.9443810840407,2.8233446082487));
#42793=CARTESIAN_POINT('Ctrl Pts',(51.2834221250874,18.9385565979853,2.90000000000001));
#42794=CARTESIAN_POINT('',(51.1472602547778,19.5977174123648,2.75000000000001));
#42795=CARTESIAN_POINT('Ctrl Pts',(51.0318725286534,19.4780064483894,2.90000000000001));
#42796=CARTESIAN_POINT('Ctrl Pts',(51.090602808417,19.5389371785562,2.82334460824971));
#42797=CARTESIAN_POINT('Ctrl Pts',(51.1472602547778,19.5977174123648,2.75000000000001));
#42798=CARTESIAN_POINT('Ctrl Pts',(51.1472602547778,19.5977174123648,2.75000000000001));
#42799=CARTESIAN_POINT('Ctrl Pts',(51.0660749268459,19.6063269793218,2.82334460824904));
#42800=CARTESIAN_POINT('Ctrl Pts',(50.981919403989,19.6152515304358,2.90000000000001));
#42801=CARTESIAN_POINT('',(50.9622882126499,20.2880424715656,2.75000000000002));
#42802=CARTESIAN_POINT('Ctrl Pts',(50.8278658946191,20.1901870544887,2.90000000000001));
#42803=CARTESIAN_POINT('Ctrl Pts',(50.8962844397244,20.2399937038989,2.8233446082496));
#42804=CARTESIAN_POINT('Ctrl Pts',(50.9622882126499,20.2880424715656,2.75000000000002));
#42805=CARTESIAN_POINT('Ctrl Pts',(50.9622882126499,20.2880424715656,2.75000000000002));
#42806=CARTESIAN_POINT('Ctrl Pts',(50.8838313078844,20.3106189241036,2.82334460824907));
#42807=CARTESIAN_POINT('Ctrl Pts',(50.8025040285536,20.3340213444176,2.90000000000001));
#42808=CARTESIAN_POINT('Ctrl Pts',(50.7506274441751,20.9269734171523,2.90000000000001));
#42809=CARTESIAN_POINT('Ctrl Pts',(50.8266553917513,20.9641426359673,2.8233446082487));
#42810=CARTESIAN_POINT('Ctrl Pts',(50.9,21.,2.75000000000001));
#42811=CARTESIAN_POINT('',(51.15,21.,2.5));
#42812=CARTESIAN_POINT('',(50.95,21.,2.7));
#42813=CARTESIAN_POINT('Origin',(55.,21.,2.5));
#42814=CARTESIAN_POINT('Origin',(58.7455598713677,18.8375,6.9));
#42815=CARTESIAN_POINT('',(58.5507041555162,18.95,6.9));
#42816=CARTESIAN_POINT('',(58.5507041555162,18.95,6.9));
#42817=CARTESIAN_POINT('',(59.0504155872192,18.9155255888326,6.9));
#42818=CARTESIAN_POINT('Origin',(59.0504155872192,18.9155255888326,2.5));
#42819=CARTESIAN_POINT('',(58.5507041555162,18.95,2.5));
#42820=CARTESIAN_POINT('Origin',(58.5507041555162,18.95,2.5));
#42821=CARTESIAN_POINT('Origin',(58.6269154903224,18.2438461534124,2.5));
#42822=CARTESIAN_POINT('',(58.1407822167878,18.3645708002852,6.9));
#42823=CARTESIAN_POINT('',(58.6269154903224,18.2438461534124,6.9));
#42824=CARTESIAN_POINT('',(58.1407822167878,18.3645708002852,2.5));
#42825=CARTESIAN_POINT('Origin',(58.1407822167878,18.3645708002852,2.5));
#42826=CARTESIAN_POINT('',(58.1407822167878,18.3645708002852,6.9));
#42827=CARTESIAN_POINT('Origin',(58.3131422164896,18.2199435881057,6.9));
#42828=CARTESIAN_POINT('Origin',(57.7800564118943,17.6868577835104,6.9));
#42829=CARTESIAN_POINT('',(57.6354291997148,17.8592177832122,6.9));
#42830=CARTESIAN_POINT('',(57.6354291997148,17.8592177832122,6.9));
#42831=CARTESIAN_POINT('',(58.0932134015599,17.6559110579397,6.9));
#42832=CARTESIAN_POINT('Origin',(58.0932134015599,17.6559110579397,2.5));
#42833=CARTESIAN_POINT('',(57.6354291997148,17.8592177832122,2.5));
#42834=CARTESIAN_POINT('Origin',(57.6354291997148,17.8592177832122,2.5));
#42835=CARTESIAN_POINT('Origin',(57.4655255888326,17.1695844127808,2.5));
#42836=CARTESIAN_POINT('',(57.05,17.4492958444838,6.9));
#42837=CARTESIAN_POINT('',(57.4655255888326,17.1695844127808,6.9));
#42838=CARTESIAN_POINT('',(57.05,17.4492958444838,2.5));
#42839=CARTESIAN_POINT('Origin',(57.05,17.4492958444838,2.5));
#42840=CARTESIAN_POINT('',(57.05,17.4492958444838,6.9));
#42841=CARTESIAN_POINT('Origin',(57.1625,17.2544401286323,6.9));
#42842=CARTESIAN_POINT('Origin',(56.4792371198835,16.9358294151009,6.9));
#42843=CARTESIAN_POINT('',(56.4022825876352,17.1472602547778,6.9));
#42844=CARTESIAN_POINT('',(56.4022825876352,17.1472602547778,6.9));
#42845=CARTESIAN_POINT('',(56.7629240287047,16.7996430069558,6.9));
#42846=CARTESIAN_POINT('Origin',(56.7629240287047,16.7996430069558,2.5));
#42847=CARTESIAN_POINT('',(56.4022825876352,17.1472602547778,2.5));
#42848=CARTESIAN_POINT('Origin',(56.4022825876352,17.1472602547778,2.5));
#42849=CARTESIAN_POINT('Origin',(56.0067569140472,16.5573273228812,2.5));
#42850=CARTESIAN_POINT('',(55.7119575284344,16.9622882126499,6.9));
#42851=CARTESIAN_POINT('',(56.0067569140472,16.5573273228812,6.9));
#42852=CARTESIAN_POINT('',(55.7119575284344,16.9622882126499,2.5));
#42853=CARTESIAN_POINT('Origin',(55.7119575284344,16.9622882126499,2.5));
#42854=CARTESIAN_POINT('',(55.7119575284344,16.9622882126499,6.9));
#42855=CARTESIAN_POINT('Origin',(55.7510283684095,16.7407064682222,6.9));
#42856=CARTESIAN_POINT('Origin',(55.,16.675,6.9));
#42857=CARTESIAN_POINT('',(55.,16.9,6.9));
#42858=CARTESIAN_POINT('',(55.,16.9,6.9));
#42859=CARTESIAN_POINT('',(55.22,16.45,6.9));
#42860=CARTESIAN_POINT('Origin',(55.22,16.45,2.5));
#42861=CARTESIAN_POINT('',(55.,16.9,2.5));
#42862=CARTESIAN_POINT('Origin',(55.,16.9,2.5));
#42863=CARTESIAN_POINT('Origin',(54.4265584972782,16.4809221247077,2.5));
#42864=CARTESIAN_POINT('',(54.2880424715656,16.9622882126499,6.9));
#42865=CARTESIAN_POINT('',(54.4265584972782,16.4809221247077,6.9));
#42866=CARTESIAN_POINT('',(54.2880424715656,16.9622882126499,2.5));
#42867=CARTESIAN_POINT('Origin',(54.2880424715656,16.9622882126499,2.5));
#42868=CARTESIAN_POINT('',(54.2880424715656,16.9622882126499,6.9));
#42869=CARTESIAN_POINT('Origin',(54.2489716315905,16.7407064682222,6.9));
#42870=CARTESIAN_POINT('Origin',(53.5207628801165,16.9358294151009,6.9));
#42871=CARTESIAN_POINT('',(53.5977174123648,17.1472602547778,6.9));
#42872=CARTESIAN_POINT('',(53.5977174123648,17.1472602547778,6.9));
#42873=CARTESIAN_POINT('',(53.6505407244411,16.6491541438925,6.9));
#42874=CARTESIAN_POINT('Origin',(53.6505407244411,16.6491541438925,2.5));
#42875=CARTESIAN_POINT('',(53.5977174123648,17.1472602547778,2.5));
#42876=CARTESIAN_POINT('Origin',(53.5977174123648,17.1472602547778,2.5));
#42877=CARTESIAN_POINT('Origin',(52.9155255888326,16.9495844127808,2.5));
#42878=CARTESIAN_POINT('',(52.95,17.4492958444838,6.9));
#42879=CARTESIAN_POINT('',(52.9155255888326,16.9495844127808,6.9));
#42880=CARTESIAN_POINT('',(52.95,17.4492958444838,2.5));
#42881=CARTESIAN_POINT('Origin',(52.95,17.4492958444838,2.5));
#42882=CARTESIAN_POINT('',(52.95,17.4492958444838,6.9));
#42883=CARTESIAN_POINT('Origin',(52.8375,17.2544401286323,6.9));
#42884=CARTESIAN_POINT('Origin',(52.2199435881057,17.6868577835104,6.9));
#42885=CARTESIAN_POINT('',(52.3645708002852,17.8592177832122,6.9));
#42886=CARTESIAN_POINT('',(52.3645708002852,17.8592177832122,6.9));
#42887=CARTESIAN_POINT('',(52.2438461534124,17.3730845096776,6.9));
#42888=CARTESIAN_POINT('Origin',(52.2438461534124,17.3730845096776,2.5));
#42889=CARTESIAN_POINT('',(52.3645708002852,17.8592177832122,2.5));
#42890=CARTESIAN_POINT('Origin',(52.3645708002852,17.8592177832122,2.5));
#42891=CARTESIAN_POINT('Origin',(51.6559110579397,17.9067865984401,2.5));
#42892=CARTESIAN_POINT('',(51.8592177832122,18.3645708002852,6.9));
#42893=CARTESIAN_POINT('',(51.6559110579397,17.9067865984401,6.9));
#42894=CARTESIAN_POINT('',(51.8592177832122,18.3645708002852,2.5));
#42895=CARTESIAN_POINT('Origin',(51.8592177832122,18.3645708002852,2.5));
#42896=CARTESIAN_POINT('',(51.8592177832122,18.3645708002852,6.9));
#42897=CARTESIAN_POINT('Origin',(51.6868577835104,18.2199435881057,6.9));
#42898=CARTESIAN_POINT('Origin',(51.2544401286323,18.8375,6.9));
#42899=CARTESIAN_POINT('',(51.4492958444838,18.95,6.9));
#42900=CARTESIAN_POINT('',(51.4492958444838,18.95,6.9));
#42901=CARTESIAN_POINT('',(51.1695844127808,18.5344744111674,6.9));
#42902=CARTESIAN_POINT('Origin',(51.1695844127808,18.5344744111674,2.5));
#42903=CARTESIAN_POINT('',(51.4492958444838,18.95,2.5));
#42904=CARTESIAN_POINT('Origin',(51.4492958444838,18.95,2.5));
#42905=CARTESIAN_POINT('Origin',(50.7996430069557,19.2370759712953,2.5));
#42906=CARTESIAN_POINT('',(51.1472602547778,19.5977174123648,6.9));
#42907=CARTESIAN_POINT('',(50.7996430069557,19.2370759712953,6.9));
#42908=CARTESIAN_POINT('',(51.1472602547778,19.5977174123648,2.5));
#42909=CARTESIAN_POINT('Origin',(51.1472602547778,19.5977174123648,2.5));
#42910=CARTESIAN_POINT('',(51.1472602547778,19.5977174123648,6.9));
#42911=CARTESIAN_POINT('Origin',(50.9358294151009,19.5207628801165,6.9));
#42912=CARTESIAN_POINT('Origin',(50.7407064682222,20.2489716315905,6.9));
#42913=CARTESIAN_POINT('',(50.9622882126499,20.2880424715656,6.9));
#42914=CARTESIAN_POINT('',(50.9622882126499,20.2880424715656,6.9));
#42915=CARTESIAN_POINT('',(50.5573273228812,19.9932430859528,6.9));
#42916=CARTESIAN_POINT('Origin',(50.5573273228812,19.9932430859528,2.5));
#42917=CARTESIAN_POINT('',(50.9622882126499,20.2880424715656,2.5));
#42918=CARTESIAN_POINT('Origin',(50.9622882126499,20.2880424715656,2.5));
#42919=CARTESIAN_POINT('Origin',(50.45,20.78,2.5));
#42920=CARTESIAN_POINT('',(50.9,21.,6.9));
#42921=CARTESIAN_POINT('',(50.45,20.78,6.9));
#42922=CARTESIAN_POINT('',(50.9,21.,2.5));
#42923=CARTESIAN_POINT('Origin',(50.9,21.,2.5));
#42924=CARTESIAN_POINT('',(50.9,21.,6.9));
#42925=CARTESIAN_POINT('Origin',(50.675,21.,6.9));
#42926=CARTESIAN_POINT('Origin',(50.7407064682222,21.7510283684095,6.9));
#42927=CARTESIAN_POINT('',(50.9622882126499,21.7119575284344,6.9));
#42928=CARTESIAN_POINT('',(50.9622882126499,21.7119575284344,6.9));
#42929=CARTESIAN_POINT('',(50.4809221247077,21.5734415027218,6.9));
#42930=CARTESIAN_POINT('Origin',(50.4809221247077,21.5734415027218,2.5));
#42931=CARTESIAN_POINT('',(50.9622882126499,21.7119575284344,2.5));
#42932=CARTESIAN_POINT('Origin',(50.9622882126499,21.7119575284344,2.5));
#42933=CARTESIAN_POINT('Origin',(50.6491541438925,22.3494592755589,2.5));
#42934=CARTESIAN_POINT('',(51.1472602547778,22.4022825876352,6.9));
#42935=CARTESIAN_POINT('',(50.6491541438925,22.3494592755589,6.9));
#42936=CARTESIAN_POINT('',(51.1472602547778,22.4022825876352,2.5));
#42937=CARTESIAN_POINT('Origin',(51.1472602547778,22.4022825876352,2.5));
#42938=CARTESIAN_POINT('',(51.1472602547778,22.4022825876352,6.9));
#42939=CARTESIAN_POINT('Origin',(50.9358294151009,22.4792371198835,6.9));
#42940=CARTESIAN_POINT('Origin',(51.2544401286323,23.1625,6.9));
#42941=CARTESIAN_POINT('',(51.4492958444838,23.05,6.9));
#42942=CARTESIAN_POINT('',(51.4492958444838,23.05,6.9));
#42943=CARTESIAN_POINT('',(50.9495844127808,23.0844744111674,6.9));
#42944=CARTESIAN_POINT('Origin',(50.9495844127808,23.0844744111674,2.5));
#42945=CARTESIAN_POINT('',(51.4492958444838,23.05,2.5));
#42946=CARTESIAN_POINT('Origin',(51.4492958444838,23.05,2.5));
#42947=CARTESIAN_POINT('Origin',(51.3730845096776,23.7561538465876,2.5));
#42948=CARTESIAN_POINT('',(51.8592177832122,23.6354291997148,6.9));
#42949=CARTESIAN_POINT('',(51.3730845096776,23.7561538465876,6.9));
#42950=CARTESIAN_POINT('',(51.8592177832122,23.6354291997148,2.5));
#42951=CARTESIAN_POINT('Origin',(51.8592177832122,23.6354291997148,2.5));
#42952=CARTESIAN_POINT('',(51.8592177832122,23.6354291997148,6.9));
#42953=CARTESIAN_POINT('Origin',(51.6868577835104,23.7800564118943,6.9));
#42954=CARTESIAN_POINT('Origin',(52.2199435881057,24.3131422164896,6.9));
#42955=CARTESIAN_POINT('',(52.3645708002852,24.1407822167878,6.9));
#42956=CARTESIAN_POINT('',(52.3645708002852,24.1407822167878,6.9));
#42957=CARTESIAN_POINT('',(51.9067865984401,24.3440889420603,6.9));
#42958=CARTESIAN_POINT('Origin',(51.9067865984401,24.3440889420603,2.5));
#42959=CARTESIAN_POINT('',(52.3645708002852,24.1407822167878,2.5));
#42960=CARTESIAN_POINT('Origin',(52.3645708002852,24.1407822167878,2.5));
#42961=CARTESIAN_POINT('Origin',(52.5344744111674,24.8304155872192,2.5));
#42962=CARTESIAN_POINT('',(52.95,24.5507041555162,6.9));
#42963=CARTESIAN_POINT('',(52.5344744111674,24.8304155872192,6.9));
#42964=CARTESIAN_POINT('',(52.95,24.5507041555162,2.5));
#42965=CARTESIAN_POINT('Origin',(52.95,24.5507041555162,2.5));
#42966=CARTESIAN_POINT('',(52.95,24.5507041555162,6.9));
#42967=CARTESIAN_POINT('Origin',(52.8375,24.7455598713677,6.9));
#42968=CARTESIAN_POINT('Origin',(53.5207628801165,25.0641705848991,6.9));
#42969=CARTESIAN_POINT('',(53.5977174123648,24.8527397452222,6.9));
#42970=CARTESIAN_POINT('',(53.5977174123648,24.8527397452222,6.9));
#42971=CARTESIAN_POINT('',(53.2370759712953,25.2003569930442,6.9));
#42972=CARTESIAN_POINT('Origin',(53.2370759712953,25.2003569930442,2.5));
#42973=CARTESIAN_POINT('',(53.5977174123648,24.8527397452222,2.5));
#42974=CARTESIAN_POINT('Origin',(53.5977174123648,24.8527397452222,2.5));
#42975=CARTESIAN_POINT('Origin',(53.9932430859528,25.4426726771188,2.5));
#42976=CARTESIAN_POINT('',(54.2880424715656,25.0377117873501,6.9));
#42977=CARTESIAN_POINT('',(53.9932430859528,25.4426726771188,6.9));
#42978=CARTESIAN_POINT('',(54.2880424715656,25.0377117873501,2.5));
#42979=CARTESIAN_POINT('Origin',(54.2880424715656,25.0377117873501,2.5));
#42980=CARTESIAN_POINT('',(54.2880424715656,25.0377117873501,6.9));
#42981=CARTESIAN_POINT('Origin',(54.2489716315905,25.2592935317778,6.9));
#42982=CARTESIAN_POINT('Origin',(55.,25.325,6.9));
#42983=CARTESIAN_POINT('',(55.,25.1,6.9));
#42984=CARTESIAN_POINT('',(55.,25.1,6.9));
#42985=CARTESIAN_POINT('',(54.78,25.55,6.9));
#42986=CARTESIAN_POINT('Origin',(54.78,25.55,2.5));
#42987=CARTESIAN_POINT('',(55.,25.1,2.5));
#42988=CARTESIAN_POINT('Origin',(55.,25.1,2.5));
#42989=CARTESIAN_POINT('Origin',(55.5734415027219,25.5190778752923,2.5));
#42990=CARTESIAN_POINT('',(55.7119575284344,25.0377117873501,6.9));
#42991=CARTESIAN_POINT('',(55.5734415027219,25.5190778752923,6.9));
#42992=CARTESIAN_POINT('',(55.7119575284344,25.0377117873501,2.5));
#42993=CARTESIAN_POINT('Origin',(55.7119575284344,25.0377117873501,2.5));
#42994=CARTESIAN_POINT('',(55.7119575284344,25.0377117873501,6.9));
#42995=CARTESIAN_POINT('Origin',(55.7510283684095,25.2592935317778,6.9));
#42996=CARTESIAN_POINT('Origin',(56.4792371198835,25.0641705848991,6.9));
#42997=CARTESIAN_POINT('',(56.4022825876352,24.8527397452222,6.9));
#42998=CARTESIAN_POINT('',(56.4022825876352,24.8527397452222,6.9));
#42999=CARTESIAN_POINT('',(56.3494592755589,25.3508458561075,6.9));
#43000=CARTESIAN_POINT('Origin',(56.3494592755589,25.3508458561075,2.5));
#43001=CARTESIAN_POINT('',(56.4022825876352,24.8527397452222,2.5));
#43002=CARTESIAN_POINT('Origin',(56.4022825876352,24.8527397452222,2.5));
#43003=CARTESIAN_POINT('Origin',(57.0844744111674,25.0504155872192,2.5));
#43004=CARTESIAN_POINT('',(57.05,24.5507041555162,6.9));
#43005=CARTESIAN_POINT('',(57.0844744111674,25.0504155872192,6.9));
#43006=CARTESIAN_POINT('',(57.05,24.5507041555162,2.5));
#43007=CARTESIAN_POINT('Origin',(57.05,24.5507041555162,2.5));
#43008=CARTESIAN_POINT('',(57.05,24.5507041555162,6.9));
#43009=CARTESIAN_POINT('Origin',(57.1625,24.7455598713677,6.9));
#43010=CARTESIAN_POINT('Origin',(57.7800564118943,24.3131422164896,6.9));
#43011=CARTESIAN_POINT('',(57.6354291997148,24.1407822167878,6.9));
#43012=CARTESIAN_POINT('',(57.6354291997148,24.1407822167878,6.9));
#43013=CARTESIAN_POINT('',(57.7561538465876,24.6269154903224,6.9));
#43014=CARTESIAN_POINT('Origin',(57.7561538465876,24.6269154903224,2.5));
#43015=CARTESIAN_POINT('',(57.6354291997148,24.1407822167878,2.5));
#43016=CARTESIAN_POINT('Origin',(57.6354291997148,24.1407822167878,2.5));
#43017=CARTESIAN_POINT('Origin',(58.3440889420603,24.0932134015599,2.5));
#43018=CARTESIAN_POINT('',(58.1407822167878,23.6354291997148,6.9));
#43019=CARTESIAN_POINT('',(58.3440889420603,24.0932134015599,6.9));
#43020=CARTESIAN_POINT('',(58.1407822167878,23.6354291997148,2.5));
#43021=CARTESIAN_POINT('Origin',(58.1407822167878,23.6354291997148,2.5));
#43022=CARTESIAN_POINT('',(58.1407822167878,23.6354291997148,6.9));
#43023=CARTESIAN_POINT('Origin',(58.3131422164896,23.7800564118943,6.9));
#43024=CARTESIAN_POINT('Origin',(58.7455598713677,23.1625,6.9));
#43025=CARTESIAN_POINT('',(58.5507041555162,23.05,6.9));
#43026=CARTESIAN_POINT('',(58.5507041555162,23.05,6.9));
#43027=CARTESIAN_POINT('',(58.8304155872192,23.4655255888326,6.9));
#43028=CARTESIAN_POINT('Origin',(58.8304155872192,23.4655255888326,2.5));
#43029=CARTESIAN_POINT('',(58.5507041555162,23.05,2.5));
#43030=CARTESIAN_POINT('Origin',(58.5507041555162,23.05,2.5));
#43031=CARTESIAN_POINT('Origin',(59.2003569930442,22.7629240287047,2.5));
#43032=CARTESIAN_POINT('',(58.8527397452222,22.4022825876352,6.9));
#43033=CARTESIAN_POINT('',(59.2003569930442,22.7629240287047,6.9));
#43034=CARTESIAN_POINT('',(58.8527397452222,22.4022825876352,2.5));
#43035=CARTESIAN_POINT('Origin',(58.8527397452222,22.4022825876352,2.5));
#43036=CARTESIAN_POINT('',(58.8527397452222,22.4022825876352,6.9));
#43037=CARTESIAN_POINT('Origin',(59.0641705848991,22.4792371198835,6.9));
#43038=CARTESIAN_POINT('Origin',(59.2592935317778,21.7510283684095,6.9));
#43039=CARTESIAN_POINT('',(59.0377117873501,21.7119575284344,6.9));
#43040=CARTESIAN_POINT('',(59.0377117873501,21.7119575284344,6.9));
#43041=CARTESIAN_POINT('',(59.4426726771188,22.0067569140472,6.9));
#43042=CARTESIAN_POINT('Origin',(59.4426726771188,22.0067569140472,2.5));
#43043=CARTESIAN_POINT('',(59.0377117873501,21.7119575284344,2.5));
#43044=CARTESIAN_POINT('Origin',(59.0377117873501,21.7119575284344,2.5));
#43045=CARTESIAN_POINT('Origin',(59.55,21.22,2.5));
#43046=CARTESIAN_POINT('',(59.1,21.,6.9));
#43047=CARTESIAN_POINT('',(59.55,21.22,6.9));
#43048=CARTESIAN_POINT('',(59.1,21.,2.5));
#43049=CARTESIAN_POINT('Origin',(59.1,21.,2.5));
#43050=CARTESIAN_POINT('',(59.1,21.,6.9));
#43051=CARTESIAN_POINT('Origin',(59.325,21.,6.9));
#43052=CARTESIAN_POINT('Origin',(55.,21.,7.3));
#43053=CARTESIAN_POINT('Origin',(50.95,21.,7.3));
#43054=CARTESIAN_POINT('Origin',(55.,21.,2.5));
#43055=CARTESIAN_POINT('',(52.4405989232415,21.,2.5));
#43056=CARTESIAN_POINT('Origin',(55.,21.,2.5));
#43057=CARTESIAN_POINT('Origin',(55.,21.,2.65));
#43058=CARTESIAN_POINT('',(52.7423796856917,20.9103130885817,2.8));
#43059=CARTESIAN_POINT('',(52.6905989232415,21.,2.75));
#43060=CARTESIAN_POINT('Ctrl Pts',(52.7423796856916,20.9103130885817,2.8));
#43061=CARTESIAN_POINT('Ctrl Pts',(52.7167726432976,20.9546657870398,2.77617372005609));
#43062=CARTESIAN_POINT('Ctrl Pts',(52.6905989232415,21.,2.75));
#43063=CARTESIAN_POINT('',(53.7935186991706,19.0896869114183,2.8));
#43064=CARTESIAN_POINT('Origin',(55.,21.,2.8));
#43065=CARTESIAN_POINT('',(53.8452994616207,19.,2.75));
#43066=CARTESIAN_POINT('Ctrl Pts',(53.8452994616207,19.,2.75));
#43067=CARTESIAN_POINT('Ctrl Pts',(53.8191257415647,19.0453342129602,2.77617372005608));
#43068=CARTESIAN_POINT('Ctrl Pts',(53.7935186991706,19.0896869114183,2.8));
#43069=CARTESIAN_POINT('',(53.9488609865211,19.,2.8));
#43070=CARTESIAN_POINT('Ctrl Pts',(53.9488609865211,19.,2.8));
#43071=CARTESIAN_POINT('Ctrl Pts',(53.8976469017329,19.,2.77617372005608));
#43072=CARTESIAN_POINT('Ctrl Pts',(53.8452994616207,19.,2.75));
#43073=CARTESIAN_POINT('',(56.0511390134789,19.,2.8));
#43074=CARTESIAN_POINT('Origin',(55.,21.,2.8));
#43075=CARTESIAN_POINT('',(56.1547005383793,19.,2.75));
#43076=CARTESIAN_POINT('Ctrl Pts',(56.1547005383793,19.,2.75));
#43077=CARTESIAN_POINT('Ctrl Pts',(56.1023530982671,19.,2.77617372005608));
#43078=CARTESIAN_POINT('Ctrl Pts',(56.0511390134789,19.,2.8));
#43079=CARTESIAN_POINT('',(56.2064813008294,19.0896869114183,2.8));
#43080=CARTESIAN_POINT('Ctrl Pts',(56.2064813008294,19.0896869114183,2.8));
#43081=CARTESIAN_POINT('Ctrl Pts',(56.1808742584353,19.0453342129602,2.77617372005607));
#43082=CARTESIAN_POINT('Ctrl Pts',(56.1547005383793,19.,2.75));
#43083=CARTESIAN_POINT('',(57.2576203143083,20.9103130885817,2.8));
#43084=CARTESIAN_POINT('Origin',(55.,21.,2.8));
#43085=CARTESIAN_POINT('',(57.3094010767585,21.,2.75));
#43086=CARTESIAN_POINT('Ctrl Pts',(57.3094010767585,21.,2.75));
#43087=CARTESIAN_POINT('Ctrl Pts',(57.2832273567024,20.9546657870398,2.77617372005609));
#43088=CARTESIAN_POINT('Ctrl Pts',(57.2576203143084,20.9103130885817,2.8));
#43089=CARTESIAN_POINT('',(57.2576203143084,21.0896869114183,2.8));
#43090=CARTESIAN_POINT('Ctrl Pts',(57.2576203143084,21.0896869114183,2.8));
#43091=CARTESIAN_POINT('Ctrl Pts',(57.2832273567024,21.0453342129602,2.77617372005609));
#43092=CARTESIAN_POINT('Ctrl Pts',(57.3094010767585,21.,2.75));
#43093=CARTESIAN_POINT('',(56.2064813008294,22.9103130885817,2.8));
#43094=CARTESIAN_POINT('Origin',(55.,21.,2.8));
#43095=CARTESIAN_POINT('',(56.1547005383793,23.,2.75));
#43096=CARTESIAN_POINT('Ctrl Pts',(56.1547005383793,23.,2.75));
#43097=CARTESIAN_POINT('Ctrl Pts',(56.1808742584353,22.9546657870398,2.7761737200561));
#43098=CARTESIAN_POINT('Ctrl Pts',(56.2064813008294,22.9103130885817,2.8));
#43099=CARTESIAN_POINT('',(56.0511390134789,23.,2.8));
#43100=CARTESIAN_POINT('Ctrl Pts',(56.051139013479,23.,2.8));
#43101=CARTESIAN_POINT('Ctrl Pts',(56.1023530982671,23.,2.77617372005609));
#43102=CARTESIAN_POINT('Ctrl Pts',(56.1547005383793,23.,2.75));
#43103=CARTESIAN_POINT('',(53.9488609865211,23.,2.8));
#43104=CARTESIAN_POINT('Origin',(55.,21.,2.8));
#43105=CARTESIAN_POINT('',(53.8452994616207,23.,2.75));
#43106=CARTESIAN_POINT('Ctrl Pts',(53.8452994616207,23.,2.75));
#43107=CARTESIAN_POINT('Ctrl Pts',(53.8976469017329,23.,2.77617372005609));
#43108=CARTESIAN_POINT('Ctrl Pts',(53.948860986521,23.,2.8));
#43109=CARTESIAN_POINT('',(53.7935186991706,22.9103130885817,2.8));
#43110=CARTESIAN_POINT('Ctrl Pts',(53.7935186991706,22.9103130885817,2.8));
#43111=CARTESIAN_POINT('Ctrl Pts',(53.8191257415647,22.9546657870398,2.77617372005606));
#43112=CARTESIAN_POINT('Ctrl Pts',(53.8452994616207,23.,2.75));
#43113=CARTESIAN_POINT('',(52.7423796856917,21.0896869114183,2.8));
#43114=CARTESIAN_POINT('Origin',(55.,21.,2.8));
#43115=CARTESIAN_POINT('Ctrl Pts',(52.6905989232415,21.,2.75));
#43116=CARTESIAN_POINT('Ctrl Pts',(52.7167726432976,21.0453342129602,2.77617372005609));
#43117=CARTESIAN_POINT('Ctrl Pts',(52.7423796856916,21.0896869114183,2.8));
#43118=CARTESIAN_POINT('',(52.5905989232415,21.,2.65));
#43119=CARTESIAN_POINT('Origin',(55.,21.,2.65));
#43120=CARTESIAN_POINT('',(57.2576203143083,20.9103130885817,2.5));
#43121=CARTESIAN_POINT('',(57.2576203143083,20.9103130885817,2.65));
#43122=CARTESIAN_POINT('',(56.2064813008294,19.0896869114183,2.5));
#43123=CARTESIAN_POINT('',(56.2064813008294,19.0896869114183,2.65));
#43124=CARTESIAN_POINT('Origin',(55.,21.,2.5));
#43125=CARTESIAN_POINT('Origin',(55.,21.,2.65));
#43126=CARTESIAN_POINT('',(56.2064813008294,22.9103130885817,2.5));
#43127=CARTESIAN_POINT('',(56.2064813008294,22.9103130885817,2.65));
#43128=CARTESIAN_POINT('',(57.2576203143084,21.0896869114183,2.5));
#43129=CARTESIAN_POINT('',(57.2576203143084,21.0896869114183,2.65));
#43130=CARTESIAN_POINT('Origin',(55.,21.,2.5));
#43131=CARTESIAN_POINT('Origin',(55.,21.,2.65));
#43132=CARTESIAN_POINT('',(53.9488609865211,19.,2.5));
#43133=CARTESIAN_POINT('',(53.9488609865211,19.,2.65));
#43134=CARTESIAN_POINT('',(56.0511390134789,19.,2.5));
#43135=CARTESIAN_POINT('Origin',(55.,21.,2.5));
#43136=CARTESIAN_POINT('',(56.0511390134789,19.,2.65));
#43137=CARTESIAN_POINT('Origin',(55.,21.,2.65));
#43138=CARTESIAN_POINT('',(53.9488609865211,23.,2.5));
#43139=CARTESIAN_POINT('',(53.9488609865211,23.,2.65));
#43140=CARTESIAN_POINT('',(56.0511390134789,23.,2.5));
#43141=CARTESIAN_POINT('',(56.0511390134789,23.,2.65));
#43142=CARTESIAN_POINT('Origin',(55.,21.,2.5));
#43143=CARTESIAN_POINT('Origin',(55.,21.,2.65));
#43144=CARTESIAN_POINT('',(52.7423796856917,20.9103130885817,2.5));
#43145=CARTESIAN_POINT('',(52.7423796856917,20.9103130885817,2.65));
#43146=CARTESIAN_POINT('',(53.7935186991706,19.0896869114183,2.5));
#43147=CARTESIAN_POINT('Origin',(55.,21.,2.5));
#43148=CARTESIAN_POINT('',(53.7935186991706,19.0896869114183,2.65));
#43149=CARTESIAN_POINT('Origin',(55.,21.,2.65));
#43150=CARTESIAN_POINT('',(53.7935186991706,22.9103130885817,2.5));
#43151=CARTESIAN_POINT('',(53.7935186991706,22.9103130885817,2.65));
#43152=CARTESIAN_POINT('',(52.7423796856917,21.0896869114183,2.5));
#43153=CARTESIAN_POINT('Origin',(55.,21.,2.5));
#43154=CARTESIAN_POINT('',(52.7423796856917,21.0896869114183,2.65));
#43155=CARTESIAN_POINT('Origin',(56.1547005383793,23.,2.5));
#43156=CARTESIAN_POINT('',(55.5773502691896,23.,2.5));
#43157=CARTESIAN_POINT('',(56.1547005383793,23.,5.));
#43158=CARTESIAN_POINT('',(56.1547005383793,23.,2.5));
#43159=CARTESIAN_POINT('',(53.8452994616207,23.,5.));
#43160=CARTESIAN_POINT('',(56.1547005383793,23.,5.));
#43161=CARTESIAN_POINT('',(53.8452994616207,23.,2.5));
#43162=CARTESIAN_POINT('Origin',(57.3094010767585,21.,2.5));
#43163=CARTESIAN_POINT('',(57.0207259421637,21.5,2.5));
#43164=CARTESIAN_POINT('',(57.3094010767585,21.,5.));
#43165=CARTESIAN_POINT('',(57.3094010767585,21.,2.5));
#43166=CARTESIAN_POINT('',(57.3094010767585,21.,5.));
#43167=CARTESIAN_POINT('Origin',(56.1547005383793,19.,2.5));
#43168=CARTESIAN_POINT('',(56.4433756729741,19.5,2.5));
#43169=CARTESIAN_POINT('',(56.1547005383793,19.,5.));
#43170=CARTESIAN_POINT('',(56.1547005383793,19.,2.5));
#43171=CARTESIAN_POINT('',(56.1547005383793,19.,5.));
#43172=CARTESIAN_POINT('Origin',(55.,21.,2.5));
#43173=CARTESIAN_POINT('Origin',(55.,21.,2.5));
#43174=CARTESIAN_POINT('Origin',(55.,21.,2.5));
#43175=CARTESIAN_POINT('',(54.4226497308104,19.,2.5));
#43176=CARTESIAN_POINT('Origin',(55.,21.,2.5));
#43177=CARTESIAN_POINT('Origin',(55.,21.,2.5));
#43178=CARTESIAN_POINT('',(52.9792740578363,20.5,2.5));
#43179=CARTESIAN_POINT('Origin',(55.,21.,2.5));
#43180=CARTESIAN_POINT('',(53.5566243270259,22.5,2.5));
#43181=CARTESIAN_POINT('Origin',(57.3094010767585,21.,5.));
#43182=CARTESIAN_POINT('',(53.8452994616207,19.,5.));
#43183=CARTESIAN_POINT('',(53.8452994616207,19.,5.));
#43184=CARTESIAN_POINT('Origin',(55.,21.,5.));
#43185=CARTESIAN_POINT('Origin',(57.3094010767585,21.,5.));
#43186=CARTESIAN_POINT('Origin',(55.,21.,5.));
#43187=CARTESIAN_POINT('Origin',(57.3094010767585,21.,5.));
#43188=CARTESIAN_POINT('Origin',(55.,21.,5.));
#43189=CARTESIAN_POINT('Origin',(57.3094010767585,21.,5.));
#43190=CARTESIAN_POINT('Origin',(55.,21.,5.));
#43191=CARTESIAN_POINT('Origin',(57.3094010767585,21.,5.));
#43192=CARTESIAN_POINT('',(52.6905989232415,21.,5.));
#43193=CARTESIAN_POINT('',(53.8452994616207,23.,5.));
#43194=CARTESIAN_POINT('Origin',(55.,21.,5.));
#43195=CARTESIAN_POINT('Origin',(57.3094010767585,21.,5.));
#43196=CARTESIAN_POINT('',(52.6905989232415,21.,5.));
#43197=CARTESIAN_POINT('Origin',(55.,21.,5.));
#43198=CARTESIAN_POINT('Origin',(55.,21.,5.));
#43199=CARTESIAN_POINT('',(55.,21.,6.38762816056403));
#43200=CARTESIAN_POINT('',(52.6905989232415,21.,5.));
#43201=CARTESIAN_POINT('Origin',(53.8452994616207,19.,2.5));
#43202=CARTESIAN_POINT('',(53.8452994616207,19.,2.5));
#43203=CARTESIAN_POINT('Origin',(52.6905989232415,21.,2.5));
#43204=CARTESIAN_POINT('',(52.6905989232415,21.,2.5));
#43205=CARTESIAN_POINT('Origin',(53.8452994616207,23.,2.5));
#43206=CARTESIAN_POINT('',(0.,0.,0.));
#43207=CARTESIAN_POINT('Origin',(55.,29.,3.45145488139523));
#43208=CARTESIAN_POINT('',(53.0466869980211,29.4044698737854,5.5836423751603));
#43209=CARTESIAN_POINT('',(53.0466869980082,29.4044698737233,5.42540812064255));
#43210=CARTESIAN_POINT('',(53.0466869980082,29.4044698737233,3.45145488139523));
#43211=CARTESIAN_POINT('',(53.8611373905627,27.3623127528964,4.93049999999996));
#43212=CARTESIAN_POINT('Ctrl Pts',(53.0466869980211,29.4044698737854,5.5836423751603));
#43213=CARTESIAN_POINT('Ctrl Pts',(53.0467598410346,29.4048216557467,5.58361735794786));
#43214=CARTESIAN_POINT('Ctrl Pts',(53.0468327795955,29.4051734205221,5.58359234005539));
#43215=CARTESIAN_POINT('Ctrl Pts',(53.052944084167,29.4346067439485,5.58149885155498));
#43216=CARTESIAN_POINT('Ctrl Pts',(53.0596311359168,29.463549813269,5.57942719964456));
#43217=CARTESIAN_POINT('Ctrl Pts',(53.079658569571,29.5421832070144,5.57377511658151));
#43218=CARTESIAN_POINT('Ctrl Pts',(53.0942792715992,29.591525759737,5.57020181656668));
#43219=CARTESIAN_POINT('Ctrl Pts',(53.1281561119192,29.6914874381887,5.56296689427717));
#43220=CARTESIAN_POINT('Ctrl Pts',(53.1475996330664,29.7420029867334,5.5593130896378));
#43221=CARTESIAN_POINT('Ctrl Pts',(53.1726367106895,29.7999071888819,5.55517541185005));
#43222=CARTESIAN_POINT('Ctrl Pts',(53.1762540609445,29.808120571997,5.55458973206913));
#43223=CARTESIAN_POINT('Ctrl Pts',(53.182194225425,29.8213649786112,5.55364761522522));
#43224=CARTESIAN_POINT('Ctrl Pts',(53.1844827387612,29.8264111192952,5.55328921441833));
#43225=CARTESIAN_POINT('Ctrl Pts',(53.1885888050893,29.8353655621017,5.55265428753538));
#43226=CARTESIAN_POINT('Ctrl Pts',(53.1903980261385,29.8392775683841,5.55237726763184));
#43227=CARTESIAN_POINT('Ctrl Pts',(53.1943395988275,29.8477282720442,5.55177965573117));
#43228=CARTESIAN_POINT('Ctrl Pts',(53.1964763867749,29.8522647977318,5.55145933871332));
#43229=CARTESIAN_POINT('Ctrl Pts',(53.2025062824284,29.8649423848354,5.55056544773773));
#43230=CARTESIAN_POINT('Ctrl Pts',(53.2064376176204,29.8730652791062,5.54999415888182));
#43231=CARTESIAN_POINT('Ctrl Pts',(53.2304006381325,29.921732465328,5.54657846256867));
#43232=CARTESIAN_POINT('Ctrl Pts',(53.251752897287,29.9616160414764,5.54380892718374));
#43233=CARTESIAN_POINT('Ctrl Pts',(53.329544218408,30.0957497024807,5.53448041500691));
#43234=CARTESIAN_POINT('Ctrl Pts',(53.3924003014302,30.186050862637,5.52816720503428));
#43235=CARTESIAN_POINT('Ctrl Pts',(53.5448870745863,30.3705658375547,5.51424720056297));
#43236=CARTESIAN_POINT('Ctrl Pts',(53.6369149972079,30.4621207901423,5.50663231156854));
#43237=CARTESIAN_POINT('Ctrl Pts',(53.7493859359876,30.5541047281784,5.49761556419157));
#43238=CARTESIAN_POINT('Ctrl Pts',(53.7617306247401,30.5639584314487,5.49662983864366));
#43239=CARTESIAN_POINT('Ctrl Pts',(53.7819752865071,30.5797280550832,5.49501890204659));
#43240=CARTESIAN_POINT('Ctrl Pts',(53.7898045849945,30.5857338940074,5.49439723334141));
#43241=CARTESIAN_POINT('Ctrl Pts',(53.8038390539862,30.596335231447,5.49328505327765));
#43242=CARTESIAN_POINT('Ctrl Pts',(53.8100269952484,30.60095328638,5.49279543238884));
#43243=CARTESIAN_POINT('Ctrl Pts',(53.8231477326398,30.6106271843221,5.4917587472129));
#43244=CARTESIAN_POINT('Ctrl Pts',(53.8300866354468,30.6156744417553,5.49121136580214));
#43245=CARTESIAN_POINT('Ctrl Pts',(53.8486189765485,30.6289726161707,5.48975159847759));
#43246=CARTESIAN_POINT('Ctrl Pts',(53.8602683376335,30.6371443937267,5.48883622855343));
#43247=CARTESIAN_POINT('Ctrl Pts',(53.917026817361,30.6760598494534,5.48438620008985));
#43248=CARTESIAN_POINT('Ctrl Pts',(53.9632939445138,30.7050651429083,5.4807876177965));
#43249=CARTESIAN_POINT('Ctrl Pts',(54.1864074481192,30.8324967499752,5.46355530959757));
#43250=CARTESIAN_POINT('Ctrl Pts',(54.3763344630289,30.9055173440879,5.4490750849697));
#43251=CARTESIAN_POINT('Ctrl Pts',(54.6071992840641,30.9559887464049,5.43311035353166));
#43252=CARTESIAN_POINT('Ctrl Pts',(54.6406092752949,30.9624023569689,5.43084241964906));
#43253=CARTESIAN_POINT('Ctrl Pts',(54.6826361309647,30.9693606555478,5.42805556969599));
#43254=CARTESIAN_POINT('Ctrl Pts',(54.6911122263776,30.9707078846567,5.42749685439508));
#43255=CARTESIAN_POINT('Ctrl Pts',(54.7045122685035,30.9727491691074,5.42661912461067));
#43256=CARTESIAN_POINT('Ctrl Pts',(54.7094304506579,30.9734795722214,5.42629815312209));
#43257=CARTESIAN_POINT('Ctrl Pts',(54.7182092058252,30.974749782946,5.42572739671727));
#43258=CARTESIAN_POINT('Ctrl Pts',(54.7220686017681,30.9752966600293,5.42547722671951));
#43259=CARTESIAN_POINT('Ctrl Pts',(54.7312869635949,30.9765753512837,5.42488144691789));
#43260=CARTESIAN_POINT('Ctrl Pts',(54.7366473251915,30.9772966862746,5.42453642454854));
#43261=CARTESIAN_POINT('Ctrl Pts',(54.7527691377047,30.9793994487664,5.42350281170371));
#43262=CARTESIAN_POINT('Ctrl Pts',(54.7635391977724,30.9807149159857,5.42281776693858));
#43263=CARTESIAN_POINT('Ctrl Pts',(54.7884146505401,30.9835474395462,5.42124699119317));
#43264=CARTESIAN_POINT('Ctrl Pts',(54.8025267166315,30.9850020483384,5.42036435897924));
#43265=CARTESIAN_POINT('Ctrl Pts',(54.8505508508856,30.9894349280911,5.41738588508356));
#43266=CARTESIAN_POINT('Ctrl Pts',(54.8845246747252,30.991695783145,5.41532137063713));
#43267=CARTESIAN_POINT('Ctrl Pts',(55.0714430634789,30.9993352333717,5.40411637916261));
#43268=CARTESIAN_POINT('Ctrl Pts',(55.2245620306993,30.9879696561106,5.39546385208552));
#43269=CARTESIAN_POINT('Ctrl Pts',(55.4541103597074,30.9440468197256,5.38164807919455));
#43270=CARTESIAN_POINT('Ctrl Pts',(55.5323361852893,30.9240972383442,5.37679113269101));
#43271=CARTESIAN_POINT('Ctrl Pts',(55.6233625220245,30.8949063304474,5.37085166486203));
#43272=CARTESIAN_POINT('Ctrl Pts',(55.6375390683028,30.8901837880418,5.36991830345721));
#43273=CARTESIAN_POINT('Ctrl Pts',(55.6607512822745,30.8821604110354,5.36837565747547));
#43274=CARTESIAN_POINT('Ctrl Pts',(55.6698186621453,30.8789526403198,5.36776941374951));
#43275=CARTESIAN_POINT('Ctrl Pts',(55.6861101445537,30.8730562841087,5.36667343529993));
#43276=CARTESIAN_POINT('Ctrl Pts',(55.6933425761252,30.8703911471479,5.36618448088078));
#43277=CARTESIAN_POINT('Ctrl Pts',(55.7087608854888,30.8646078139443,5.36513687648532));
#43278=CARTESIAN_POINT('Ctrl Pts',(55.7169420106464,30.8614774889824,5.36457783302405));
#43279=CARTESIAN_POINT('Ctrl Pts',(55.739078260069,30.8528399714588,5.36305642212925));
#43280=CARTESIAN_POINT('Ctrl Pts',(55.7529920806579,30.8472291521559,5.36209062484586));
#43281=CARTESIAN_POINT('Ctrl Pts',(55.8266105715767,30.8165721662778,5.35692870868625));
#43282=CARTESIAN_POINT('Ctrl Pts',(55.8851266732236,30.7887897270671,5.35264132666126));
#43283=CARTESIAN_POINT('Ctrl Pts',(56.073780504631,30.6876947972367,5.33819064714519));
#43284=CARTESIAN_POINT('Ctrl Pts',(56.1970357929047,30.6026273879261,5.3276712881522));
#43285=CARTESIAN_POINT('Ctrl Pts',(56.3642577387813,30.4570770415889,5.31234294664548));
#43286=CARTESIAN_POINT('Ctrl Pts',(56.4162624191764,30.4065830171306,5.30740241716296));
#43287=CARTESIAN_POINT('Ctrl Pts',(56.4725126533723,30.3456759060381,5.30195848867342));
#43288=CARTESIAN_POINT('Ctrl Pts',(56.4795548969886,30.3379291747173,5.30127503966523));
#43289=CARTESIAN_POINT('Ctrl Pts',(56.4901298431912,30.3261107270354,5.30024632671909));
#43290=CARTESIAN_POINT('Ctrl Pts',(56.49370743987,30.3220796858166,5.29989787794448));
#43291=CARTESIAN_POINT('Ctrl Pts',(56.5001030722091,30.3148143351866,5.29927426986947));
#43292=CARTESIAN_POINT('Ctrl Pts',(56.50292706706,30.3115853749136,5.29899867453789));
#43293=CARTESIAN_POINT('Ctrl Pts',(56.509081239888,30.3045027073592,5.29839757829528));
#43294=CARTESIAN_POINT('Ctrl Pts',(56.5124070841153,30.300645345744,5.29807239454115));
#43295=CARTESIAN_POINT('Ctrl Pts',(56.5218920686168,30.2895589501389,5.2971438845272));
#43296=CARTESIAN_POINT('Ctrl Pts',(56.5280145066089,30.2822984950842,5.29654318056524));
#43297=CARTESIAN_POINT('Ctrl Pts',(56.5701565504473,30.2315928007642,5.29239662327045));
#43298=CARTESIAN_POINT('Ctrl Pts',(56.6043737659093,30.1866754107808,5.28896915328454));
#43299=CARTESIAN_POINT('Ctrl Pts',(56.6916579319223,30.061405626217,5.2798726688626));
#43300=CARTESIAN_POINT('Ctrl Pts',(56.7408899672203,29.9785665924262,5.27433457303476));
#43301=CARTESIAN_POINT('Ctrl Pts',(56.8430593123045,29.7743464179482,5.26107390515525));
#43302=CARTESIAN_POINT('Ctrl Pts',(56.8902762318413,29.6506374369867,5.25332224917714));
#43303=CARTESIAN_POINT('Ctrl Pts',(56.9290370954948,29.5080256231801,5.24415279051811));
#43304=CARTESIAN_POINT('Ctrl Pts',(56.9329764961587,29.4928245051462,5.24317297793125));
#43305=CARTESIAN_POINT('Ctrl Pts',(56.939083418211,29.4680589679658,5.24157201103533));
#43306=CARTESIAN_POINT('Ctrl Pts',(56.9413606503824,29.4585221040407,5.24095438625694));
#43307=CARTESIAN_POINT('Ctrl Pts',(56.945293374306,29.4414975107157,5.23984969389446));
#43308=CARTESIAN_POINT('Ctrl Pts',(56.9469761840545,29.434016244084,5.23936351328078));
#43309=CARTESIAN_POINT('Ctrl Pts',(56.9504368739863,29.4182058075239,5.23833441584678));
#43310=CARTESIAN_POINT('Ctrl Pts',(56.9522046266746,29.409874601229,5.23779118574829));
#43311=CARTESIAN_POINT('Ctrl Pts',(56.9567594439886,29.387710155499,5.23634331369595));
#43312=CARTESIAN_POINT('Ctrl Pts',(56.9594531239508,29.3738584282556,5.2354357188024));
#43313=CARTESIAN_POINT('Ctrl Pts',(56.9717284256869,29.3069542533562,5.23103799203724));
#43314=CARTESIAN_POINT('Ctrl Pts',(56.9793028575019,29.253560994094,5.22748509753295));
#43315=CARTESIAN_POINT('Ctrl Pts',(56.9951861160448,29.0958882609151,5.21686009187886));
#43316=CARTESIAN_POINT('Ctrl Pts',(56.997468429701,28.9911941364029,5.20962594995398));
#43317=CARTESIAN_POINT('Ctrl Pts',(56.9895148154999,28.8512465375254,5.19985609716229));
#43318=CARTESIAN_POINT('Ctrl Pts',(56.9865408023446,28.8157380861126,5.19736989327771));
#43319=CARTESIAN_POINT('Ctrl Pts',(56.9806418946041,28.7624983000686,5.19364326420605));
#43320=CARTESIAN_POINT('Ctrl Pts',(56.9784259039746,28.7446956152318,5.19239733976931));
#43321=CARTESIAN_POINT('Ctrl Pts',(56.9656162085244,28.6520046695348,5.1859177104549));
#43322=CARTESIAN_POINT('Ctrl Pts',(56.9510084677251,28.5777247394624,5.18074811658668));
#43323=CARTESIAN_POINT('Ctrl Pts',(56.9296209819756,28.4943326688822,5.17509414251862));
#43324=CARTESIAN_POINT('Ctrl Pts',(56.9269476164077,28.4842389324896,5.17441236899198));
#43325=CARTESIAN_POINT('Ctrl Pts',(56.922780346937,28.4689895471189,5.17338675935825));
#43326=CARTESIAN_POINT('Ctrl Pts',(56.9213447398797,28.4638183555879,5.17303973582239));
#43327=CARTESIAN_POINT('Ctrl Pts',(56.9187227990959,28.4545196380427,5.17241719114263));
#43328=CARTESIAN_POINT('Ctrl Pts',(56.9175440065505,28.4503901486285,5.17214125254017));
#43329=CARTESIAN_POINT('Ctrl Pts',(56.9149256185164,28.4413285089472,5.17153688741819));
#43330=CARTESIAN_POINT('Ctrl Pts',(56.9134803030432,28.4363981097868,5.17120879469745));
#43331=CARTESIAN_POINT('Ctrl Pts',(56.9092889252682,28.4223020596539,5.17027274960637));
#43332=CARTESIAN_POINT('Ctrl Pts',(56.9064959004578,28.413150359488,5.16966742812156));
#43333=CARTESIAN_POINT('Ctrl Pts',(56.8867265109213,28.3500044937226,5.16550510092732));
#43334=CARTESIAN_POINT('Ctrl Pts',(56.867522923147,28.2967287121739,5.16206583302436));
#43335=CARTESIAN_POINT('Ctrl Pts',(56.8096549510096,28.1553578307649,5.15295800487276));
#43336=CARTESIAN_POINT('Ctrl Pts',(56.7668454527477,28.0691237814998,5.14741794081993));
#43337=CARTESIAN_POINT('Ctrl Pts',(56.65092522318,27.8726645194238,5.13415503046321));
#43338=CARTESIAN_POINT('Ctrl Pts',(56.5727684096054,27.7659690937386,5.12640349020351));
#43339=CARTESIAN_POINT('Ctrl Pts',(56.4740858556187,27.6559951531108,5.1172318081291));
#43340=CARTESIAN_POINT('Ctrl Pts',(56.4633742118408,27.6443400013257,5.11624370547335));
#43341=CARTESIAN_POINT('Ctrl Pts',(56.4457379630333,27.6256029071172,5.11462805256785));
#43342=CARTESIAN_POINT('Ctrl Pts',(56.4388972015588,27.6184427393707,5.11400403940678));
#43343=CARTESIAN_POINT('Ctrl Pts',(56.426603127475,27.6057649925271,5.11288712632583));
#43344=CARTESIAN_POINT('Ctrl Pts',(56.4211703721253,27.6002276935041,5.11239511613917));
#43345=CARTESIAN_POINT('Ctrl Pts',(56.4096259472681,27.5885976037271,5.11135278914394));
#43346=CARTESIAN_POINT('Ctrl Pts',(56.403506775353,27.5825125174658,5.11080215025016));
#43347=CARTESIAN_POINT('Ctrl Pts',(56.3871189647084,27.5664261412988,5.10933224400521));
#43348=CARTESIAN_POINT('Ctrl Pts',(56.3767818306701,27.5564956516279,5.10840995972341));
#43349=CARTESIAN_POINT('Ctrl Pts',(56.3260199437685,27.5087719415706,5.10390369762393));
#43350=CARTESIAN_POINT('Ctrl Pts',(56.2841447678497,27.4725638307195,5.10025437425244));
#43351=CARTESIAN_POINT('Ctrl Pts',(56.0734505989827,27.3051769295966,5.08220053443745));
#43352=CARTESIAN_POINT('Ctrl Pts',(55.8858329932664,27.2000006483006,5.06684547522726));
#43353=CARTESIAN_POINT('Ctrl Pts',(55.6634479072121,27.1186713946938,5.05102880771687));
#43354=CARTESIAN_POINT('Ctrl Pts',(55.6416308196626,27.1111192608178,5.04950276410035));
#43355=CARTESIAN_POINT('Ctrl Pts',(55.6126294895628,27.101640763293,5.04751226900416));
#43356=CARTESIAN_POINT('Ctrl Pts',(55.6055595562046,27.0993737055664,5.04702998956829));
#43357=CARTESIAN_POINT('Ctrl Pts',(55.5940210191816,27.0957446570491,5.04624788457996));
#43358=CARTESIAN_POINT('Ctrl Pts',(55.5895600618636,27.0943588172985,5.04594672550576));
#43359=CARTESIAN_POINT('Ctrl Pts',(55.5808893885261,27.0916985495937,5.04536377671824));
#43360=CARTESIAN_POINT('Ctrl Pts',(55.5766802665595,27.0904223560222,5.04508188391851));
#43361=CARTESIAN_POINT('Ctrl Pts',(55.5666610625676,27.087420711204,5.04441340645468));
#43362=CARTESIAN_POINT('Ctrl Pts',(55.5608472302511,27.0857077855469,5.04402752588487));
#43363=CARTESIAN_POINT('Ctrl Pts',(55.5412450761933,27.0800293834263,5.04273297309114));
#43364=CARTESIAN_POINT('Ctrl Pts',(55.5274214394433,27.076186065855,5.04183083974647));
#43365=CARTESIAN_POINT('Ctrl Pts',(55.4492052358708,27.0553464697595,5.03678092316811));
#43366=CARTESIAN_POINT('Ctrl Pts',(55.3840284318532,27.0414325067611,5.0327797115616));
#43367=CARTESIAN_POINT('Ctrl Pts',(55.1460042396163,27.0029617864523,5.01851942570968));
#43368=CARTESIAN_POINT('Ctrl Pts',(54.9708367400101,26.9978438435076,5.00861485645763));
#43369=CARTESIAN_POINT('Ctrl Pts',(54.7611181533047,27.0192725900574,4.99576917198283));
#43370=CARTESIAN_POINT('Ctrl Pts',(54.7251106133381,27.0239480808233,4.99353136743136));
#43371=CARTESIAN_POINT('Ctrl Pts',(54.6765202248454,27.0316111829569,4.99045846631094));
#43372=CARTESIAN_POINT('Ctrl Pts',(54.6638081538849,27.0337424557005,4.98964960337045));
#43373=CARTESIAN_POINT('Ctrl Pts',(54.6437047885457,27.0373135827476,4.98836222373275));
#43374=CARTESIAN_POINT('Ctrl Pts',(54.6362993164737,27.0386723729802,4.98788622068686));
#43375=CARTESIAN_POINT('Ctrl Pts',(54.6211783414933,27.0415354218614,4.9869105777871));
#43376=CARTESIAN_POINT('Ctrl Pts',(54.6134636908624,27.043043426221,4.98641082930076));
#43377=CARTESIAN_POINT('Ctrl Pts',(54.5957260146967,27.0466196366109,4.98525713768923));
#43378=CARTESIAN_POINT('Ctrl Pts',(54.5857096563399,27.048719445059,4.98460221884103));
#43379=CARTESIAN_POINT('Ctrl Pts',(54.5543373009053,27.0555487248541,4.98253989138371));
#43380=CARTESIAN_POINT('Ctrl Pts',(54.5330432515918,27.0605523116497,4.98112394801785));
#43381=CARTESIAN_POINT('Ctrl Pts',(54.4280885468073,27.0870427671995,4.97406211674203));
#43382=CARTESIAN_POINT('Ctrl Pts',(54.3458130270717,27.1135949456928,4.9682581280078));
#43383=CARTESIAN_POINT('Ctrl Pts',(54.1227950888987,27.2019159713303,4.95180333239948));
#43384=CARTESIAN_POINT('Ctrl Pts',(53.9871081654211,27.2747115301222,4.94091516715197));
#43385=CARTESIAN_POINT('Ctrl Pts',(53.8611373905627,27.3623127528964,4.93049999999996));
#43386=CARTESIAN_POINT('',(56.1603489846691,27.3774656255483,4.9305));
#43387=CARTESIAN_POINT('Origin',(55.,29.,4.9305));
#43388=CARTESIAN_POINT('Ctrl Pts',(56.1603489846691,27.3774656255483,4.9305));
#43389=CARTESIAN_POINT('Ctrl Pts',(56.2184216902281,27.4189960892435,4.93505709699294));
#43390=CARTESIAN_POINT('Ctrl Pts',(56.2743063157546,27.4636793687382,4.93961419398587));
#43391=CARTESIAN_POINT('Ctrl Pts',(56.3276577251371,27.5112580722691,4.9441712909788));
#43392=CARTESIAN_POINT('Ctrl Pts',(56.382795092379,27.5604294902287,4.94888093845325));
#43393=CARTESIAN_POINT('Ctrl Pts',(56.4352261996819,27.6126933573083,4.95359058592769));
#43394=CARTESIAN_POINT('Ctrl Pts',(56.484606964112,27.6677201027524,4.95830023340213));
#43395=CARTESIAN_POINT('Ctrl Pts',(56.5323524863125,27.7209246395096,4.96285392107065));
#43396=CARTESIAN_POINT('Ctrl Pts',(56.5772462315824,27.7767115451888,4.96740760873917));
#43397=CARTESIAN_POINT('Ctrl Pts',(56.6190157492701,27.834746565714,4.97196129640769));
#43398=CARTESIAN_POINT('Ctrl Pts',(56.6607857488445,27.8927822557777,4.97651503661119));
#43399=CARTESIAN_POINT('Ctrl Pts',(56.6994311820518,27.9530657412654,4.98106877681469));
#43400=CARTESIAN_POINT('Ctrl Pts',(56.7347219369901,28.0152323300263,4.9856225170182));
#43401=CARTESIAN_POINT('Ctrl Pts',(56.770022593053,28.0774163601582,4.99017753481266));
#43402=CARTESIAN_POINT('Ctrl Pts',(56.8019664744604,28.1414841461348,4.99473255260713));
#43403=CARTESIAN_POINT('Ctrl Pts',(56.8303692593991,28.2070460689631,4.99928757040159));
#43404=CARTESIAN_POINT('Ctrl Pts',(56.8587876569103,28.2726440301685,5.00384509201904));
#43405=CARTESIAN_POINT('Ctrl Pts',(56.8836609071208,28.3397373416821,5.00840261363649));
#43406=CARTESIAN_POINT('Ctrl Pts',(56.9048531997708,28.4079173623362,5.01296013525394));
#43407=CARTESIAN_POINT('Ctrl Pts',(56.9260780688309,28.4762021880885,5.01752466261144));
#43408=CARTESIAN_POINT('Ctrl Pts',(56.9436105518529,28.5455766198122,5.02208918996893));
#43409=CARTESIAN_POINT('Ctrl Pts',(56.9573651317897,28.6156182843135,5.02665371732643));
#43410=CARTESIAN_POINT('Ctrl Pts',(56.9711320025852,28.6857225368555,5.03122232346797));
#43411=CARTESIAN_POINT('Ctrl Pts',(56.9811141820617,28.7564947577038,5.03579092960952));
#43412=CARTESIAN_POINT('Ctrl Pts',(56.9872779160048,28.8275063854523,5.04035953575106));
#43413=CARTESIAN_POINT('Ctrl Pts',(56.9934529543083,28.8986482493601,5.04493652076993));
#43414=CARTESIAN_POINT('Ctrl Pts',(56.9957955514951,28.970029940603,5.0495135057888));
#43415=CARTESIAN_POINT('Ctrl Pts',(56.9943240157816,29.0412223553015,5.05409049080767));
#43416=CARTESIAN_POINT('Ctrl Pts',(56.9939904687856,29.0573592494626,5.05512793732693));
#43417=CARTESIAN_POINT('Ctrl Pts',(56.9934611719914,29.0734864424386,5.05616538384619));
#43418=CARTESIAN_POINT('Ctrl Pts',(56.9927367071262,29.0895989875611,5.05720283036545));
#43419=CARTESIAN_POINT('Ctrl Pts',(56.9896539144736,29.1581621962148,5.0616174440485));
#43420=CARTESIAN_POINT('Ctrl Pts',(56.9830210524896,29.2267271840215,5.06603205773156));
#43421=CARTESIAN_POINT('Ctrl Pts',(56.9728321611652,29.29489121108,5.07044667141461));
#43422=CARTESIAN_POINT('Ctrl Pts',(56.9626601262909,29.362942467918,5.07485398158319));
#43423=CARTESIAN_POINT('Ctrl Pts',(56.948943803451,29.4305935908549,5.07926129175177));
#43424=CARTESIAN_POINT('Ctrl Pts',(56.9317292042771,29.4974433071647,5.08366860192035));
#43425=CARTESIAN_POINT('Ctrl Pts',(56.9145379279213,29.5642024536182,5.08806994094245));
#43426=CARTESIAN_POINT('Ctrl Pts',(56.8938579080394,29.6301618682264,5.09247127996455));
#43427=CARTESIAN_POINT('Ctrl Pts',(56.8697864793689,29.6949288338162,5.09687261898666));
#43428=CARTESIAN_POINT('Ctrl Pts',(56.8457327381214,29.7596482093469,5.10127072395289));
#43429=CARTESIAN_POINT('Ctrl Pts',(56.8182927014435,29.8231764060104,5.10566882891913));
#43430=CARTESIAN_POINT('Ctrl Pts',(56.7876135306692,29.8851358243052,5.11006693388537));
#43431=CARTESIAN_POINT('Ctrl Pts',(56.7569460005025,29.947071733318,5.11446337007723));
#43432=CARTESIAN_POINT('Ctrl Pts',(56.7230419956251,30.0074395973588,5.11885980626908));
#43433=CARTESIAN_POINT('Ctrl Pts',(56.6860960352171,30.0658835407892,5.12325624246093));
#43434=CARTESIAN_POINT('Ctrl Pts',(56.6491509646711,30.1243260765678,5.12765257276241));
#43435=CARTESIAN_POINT('Ctrl Pts',(56.6091643529584,30.1808443626743,5.13204890306389));
#43436=CARTESIAN_POINT('Ctrl Pts',(56.5663747139411,30.2351104477034,5.13644523336537));
#43437=CARTESIAN_POINT('Ctrl Pts',(56.5235418517711,30.2894313486022,5.14084600453759));
#43438=CARTESIAN_POINT('Ctrl Pts',(56.4779006207076,30.3414951143212,5.1452467757098));
#43439=CARTESIAN_POINT('Ctrl Pts',(56.4297299175529,30.3910068027707,5.14964754688202));
#43440=CARTESIAN_POINT('Ctrl Pts',(56.3815329085139,30.4405455294126,5.15405072130288));
#43441=CARTESIAN_POINT('Ctrl Pts',(56.3308040462454,30.4875290668789,5.15845389572373));
#43442=CARTESIAN_POINT('Ctrl Pts',(56.2778570511968,30.5317013152722,5.16285707014459));
#43443=CARTESIAN_POINT('Ctrl Pts',(56.2248163567507,30.575951734543,5.16726803678841));
#43444=CARTESIAN_POINT('Ctrl Pts',(56.1695500948677,30.6173806359082,5.17167900343223));
#43445=CARTESIAN_POINT('Ctrl Pts',(56.112402083768,30.6557744914476,5.17608997007605));
#43446=CARTESIAN_POINT('Ctrl Pts',(56.0786490002709,30.6784508888735,5.17869520029434));
#43447=CARTESIAN_POINT('Ctrl Pts',(56.0442399981255,30.7000693996835,5.18130043051263));
#43448=CARTESIAN_POINT('Ctrl Pts',(56.0092496154507,30.7205937278197,5.18390566073091));
#43449=CARTESIAN_POINT('Ctrl Pts',(55.9493356610869,30.7557374891994,5.18836659063431));
#43450=CARTESIAN_POINT('Ctrl Pts',(55.8874677711289,30.7878161804688,5.19282752053772));
#43451=CARTESIAN_POINT('Ctrl Pts',(55.8239917835498,30.8166081314203,5.19728845044112));
#43452=CARTESIAN_POINT('Ctrl Pts',(55.7606106181105,30.84535707218,5.20174271648729));
#43453=CARTESIAN_POINT('Ctrl Pts',(55.6956265641001,30.8708288185757,5.20619698253345));
#43454=CARTESIAN_POINT('Ctrl Pts',(55.6294115023349,30.8928467247055,5.21065124857962));
#43455=CARTESIAN_POINT('Ctrl Pts',(55.5632743336875,30.9148387297291,5.21510027478065));
#43456=CARTESIAN_POINT('Ctrl Pts',(55.4959094944692,30.9333848118939,5.21954930098167));
#43457=CARTESIAN_POINT('Ctrl Pts',(55.4277087213242,30.9483564386947,5.2239983271827));
#43458=CARTESIAN_POINT('Ctrl Pts',(55.3595508949386,30.9633186377014,5.22844455178415));
#43459=CARTESIAN_POINT('Ctrl Pts',(55.290558654364,30.9747107428247,5.23289077638559));
#43460=CARTESIAN_POINT('Ctrl Pts',(55.221137323565,30.9824545005186,5.23733700098703));
#43461=CARTESIAN_POINT('Ctrl Pts',(55.1517363292538,30.9901959897335,5.24178192309844));
#43462=CARTESIAN_POINT('Ctrl Pts',(55.0819069788018,30.99429119944,5.24622684520984));
#43463=CARTESIAN_POINT('Ctrl Pts',(55.0120614315314,30.9947135344128,5.25067176732124));
#43464=CARTESIAN_POINT('Ctrl Pts',(54.9422128242487,30.9951358878885,5.2551168841697));
#43465=CARTESIAN_POINT('Ctrl Pts',(54.8723485065069,30.9918850466157,5.25956200101816));
#43466=CARTESIAN_POINT('Ctrl Pts',(54.8028805958103,30.9849865246374,5.26400711786662));
#43467=CARTESIAN_POINT('Ctrl Pts',(54.7333411857832,30.9780809024066,5.26845680981853));
#43468=CARTESIAN_POINT('Ctrl Pts',(54.6641994834418,30.9675201544059,5.27290650177045));
#43469=CARTESIAN_POINT('Ctrl Pts',(54.5958614759773,30.9533815848167,5.27735619372237));
#43470=CARTESIAN_POINT('Ctrl Pts',(54.5274841733299,30.9392348853784,5.28180844430111));
#43471=CARTESIAN_POINT('Ctrl Pts',(54.4599119575084,30.9215063926186,5.28626069487986));
#43472=CARTESIAN_POINT('Ctrl Pts',(54.3935369530285,30.9003236922056,5.2907129454586));
#43473=CARTESIAN_POINT('Ctrl Pts',(54.3270498994079,30.8791052327988,5.29517271198187));
#43474=CARTESIAN_POINT('Ctrl Pts',(54.2617645475404,30.8544210985306,5.29963247850514));
#43475=CARTESIAN_POINT('Ctrl Pts',(54.1980535338539,30.8264472146591,5.30409224502841));
#43476=CARTESIAN_POINT('Ctrl Pts',(54.1670237598173,30.8128228309735,5.30626432705105));
#43477=CARTESIAN_POINT('Ctrl Pts',(54.1363670647112,30.7984187939596,5.3084364090737));
#43478=CARTESIAN_POINT('Ctrl Pts',(54.106124189597,30.7832592627199,5.31060849109635));
#43479=CARTESIAN_POINT('Ctrl Pts',(54.0439745802264,30.7521061748859,5.31507215563614));
#43480=CARTESIAN_POINT('Ctrl Pts',(53.9833383728733,30.717641484113,5.31953582017592));
#43481=CARTESIAN_POINT('Ctrl Pts',(53.9245898534785,30.6800358863008,5.3239994847157));
#43482=CARTESIAN_POINT('Ctrl Pts',(53.86594127085,30.6424942591534,5.32845555614157));
#43483=CARTESIAN_POINT('Ctrl Pts',(53.809174402341,30.6018226028416,5.33291162756744));
#43484=CARTESIAN_POINT('Ctrl Pts',(53.7546395290766,30.5582377417972,5.3373676989933));
#43485=CARTESIAN_POINT('Ctrl Pts',(53.7001568729434,30.5146946132494,5.34181950373159));
#43486=CARTESIAN_POINT('Ctrl Pts',(53.6479023507712,30.468244116519,5.34627130846988));
#43487=CARTESIAN_POINT('Ctrl Pts',(53.5981967552725,30.4191459493552,5.35072311320817));
#43488=CARTESIAN_POINT('Ctrl Pts',(53.5485220701845,30.3700783148608,5.35517214950336));
#43489=CARTESIAN_POINT('Ctrl Pts',(53.5013935113704,30.3183666195505,5.35962118579854));
#43490=CARTESIAN_POINT('Ctrl Pts',(53.4570969576199,30.2643092043936,5.36407022209372));
#43491=CARTESIAN_POINT('Ctrl Pts',(53.4128130845098,30.2102672640893,5.36851798477676));
#43492=CARTESIAN_POINT('Ctrl Pts',(53.3713599140202,30.1538813147802,5.37296574745979));
#43493=CARTESIAN_POINT('Ctrl Pts',(53.3329836074857,30.0954834136529,5.37741351014282));
#43494=CARTESIAN_POINT('Ctrl Pts',(53.2945859321945,30.0370529953124,5.38186374943623));
#43495=CARTESIAN_POINT('Ctrl Pts',(53.2592688143221,29.9766087928291,5.38631398872963));
#43496=CARTESIAN_POINT('Ctrl Pts',(53.2272349024942,29.9145116027504,5.39076422802304));
#43497=CARTESIAN_POINT('Ctrl Pts',(53.1951917413346,29.8523964830007,5.39521575225907));
#43498=CARTESIAN_POINT('Ctrl Pts',(53.166433881358,29.7886278665477,5.3996672764951));
#43499=CARTESIAN_POINT('Ctrl Pts',(53.1411167183624,29.7235886315776,5.40411880073113));
#43500=CARTESIAN_POINT('Ctrl Pts',(53.1157659750434,29.6584631294949,5.40857622940534));
#43501=CARTESIAN_POINT('Ctrl Pts',(53.0938652001118,29.5920641048668,5.41303365807955));
#43502=CARTESIAN_POINT('Ctrl Pts',(53.0755203145486,29.5247909133979,5.41749108675376));
#43503=CARTESIAN_POINT('Ctrl Pts',(53.0646592635329,29.4849619615071,5.42013009805002));
#43504=CARTESIAN_POINT('Ctrl Pts',(53.0550436614939,29.4448268458996,5.42276910934629));
#43505=CARTESIAN_POINT('Ctrl Pts',(53.0466869980082,29.4044698737233,5.42540812064255));
#43506=CARTESIAN_POINT('Origin',(55.,29.,3.45145488139523));
#43507=CARTESIAN_POINT('',(53.046686998162,29.4044698744659,6.38531629657044));
#43508=CARTESIAN_POINT('',(53.0466869743493,29.404469759467,6.22571516850574));
#43509=CARTESIAN_POINT('',(53.0466869980082,29.4044698737233,3.45145488139523));
#43510=CARTESIAN_POINT('Ctrl Pts',(53.046686998162,29.404469874466,6.38531629657044));
#43511=CARTESIAN_POINT('Ctrl Pts',(53.0475577577059,29.4086750478202,6.3850495438278));
#43512=CARTESIAN_POINT('Ctrl Pts',(53.0484421144563,29.4128774942598,6.38478237233183));
#43513=CARTESIAN_POINT('Ctrl Pts',(53.0523440964602,29.4311269716662,6.38361954233214));
#43514=CARTESIAN_POINT('Ctrl Pts',(53.0554997775915,29.4451436311797,6.38271967662396));
#43515=CARTESIAN_POINT('Ctrl Pts',(53.0607878336167,29.4675016961701,6.3812729657046));
#43516=CARTESIAN_POINT('Ctrl Pts',(53.0628233126949,29.4758656749478,6.3807292136261));
#43517=CARTESIAN_POINT('Ctrl Pts',(53.0665974895298,29.4909485293677,6.37974394047379));
#43518=CARTESIAN_POINT('Ctrl Pts',(53.0683172448876,29.4976720381938,6.37930303275358));
#43519=CARTESIAN_POINT('Ctrl Pts',(53.0724552326884,29.5135051750495,6.3782606605891));
#43520=CARTESIAN_POINT('Ctrl Pts',(53.0749029962216,29.5226068463296,6.37765825571887));
#43521=CARTESIAN_POINT('Ctrl Pts',(53.0822629929287,29.5492204737721,6.37588723677603));
#43522=CARTESIAN_POINT('Ctrl Pts',(53.0873502347284,29.5666826240363,6.37471301778809));
#43523=CARTESIAN_POINT('Ctrl Pts',(53.1331129653527,29.7161236791144,6.36455608905531));
#43524=CARTESIAN_POINT('Ctrl Pts',(53.1871467797638,29.8435935797991,6.35512532152846));
#43525=CARTESIAN_POINT('Ctrl Pts',(53.3193420074771,30.0829309865168,6.33610672863624));
#43526=CARTESIAN_POINT('Ctrl Pts',(53.3966842572105,30.1944601285966,6.32658202078836));
#43527=CARTESIAN_POINT('Ctrl Pts',(53.4945899246505,30.3088154226263,6.31662114456524));
#43528=CARTESIAN_POINT('Ctrl Pts',(53.5045788510581,30.3202169995012,6.31562595680132));
#43529=CARTESIAN_POINT('Ctrl Pts',(53.5185227850067,30.3357715641854,6.31426673347779));
#43530=CARTESIAN_POINT('Ctrl Pts',(53.5223668791216,30.3400226760234,6.3138950921806));
#43531=CARTESIAN_POINT('Ctrl Pts',(53.5289848395267,30.3472782488259,6.3132606075992));
#43532=CARTESIAN_POINT('Ctrl Pts',(53.5317496932293,30.3502908277484,6.31299710819081));
#43533=CARTESIAN_POINT('Ctrl Pts',(53.5375254534981,30.3565453691546,6.31244996991303));
#43534=CARTESIAN_POINT('Ctrl Pts',(53.5405379022808,30.3597858373589,6.31216646076998));
#43535=CARTESIAN_POINT('Ctrl Pts',(53.5478677253153,30.3676180542884,6.31148105351671));
#43536=CARTESIAN_POINT('Ctrl Pts',(53.5521961763001,30.3721994666395,6.31107998818048));
#43537=CARTESIAN_POINT('Ctrl Pts',(53.5675487818023,30.3882957861287,6.30967005721075));
#43538=CARTESIAN_POINT('Ctrl Pts',(53.5786895164332,30.3996993352801,6.30866967152245));
#43539=CARTESIAN_POINT('Ctrl Pts',(53.606500431757,30.4274918274352,6.30622402887145));
#43540=CARTESIAN_POINT('Ctrl Pts',(53.6233246014926,30.4437239724474,6.30478901517503));
#43541=CARTESIAN_POINT('Ctrl Pts',(53.693921730673,30.5094802770394,6.29892825857359));
#43542=CARTESIAN_POINT('Ctrl Pts',(53.7501151197452,30.556329200335,6.29463669068409));
#43543=CARTESIAN_POINT('Ctrl Pts',(53.9444795087286,30.7010395168376,6.28051916701322));
#43544=CARTESIAN_POINT('Ctrl Pts',(54.0924900601227,30.7843987763376,6.27082727671733));
#43545=CARTESIAN_POINT('Ctrl Pts',(54.2703416742453,30.8566488662321,6.25898423167699));
#43546=CARTESIAN_POINT('Ctrl Pts',(54.2915870353529,30.8648585175939,6.25756793671175));
#43547=CARTESIAN_POINT('Ctrl Pts',(54.3225435101036,30.8762154208556,6.25549990560979));
#43548=CARTESIAN_POINT('Ctrl Pts',(54.3321460265683,30.8796549324716,6.25485781939521));
#43549=CARTESIAN_POINT('Ctrl Pts',(54.349126735079,30.8855906815297,6.25372114505847));
#43550=CARTESIAN_POINT('Ctrl Pts',(54.3564940141228,30.8881176522166,6.25322757878406));
#43551=CARTESIAN_POINT('Ctrl Pts',(54.3717748255173,30.8932591345568,6.25220292337203));
#43552=CARTESIAN_POINT('Ctrl Pts',(54.3796903100954,30.8958673227831,6.25167163843889));
#43553=CARTESIAN_POINT('Ctrl Pts',(54.4001079112635,30.9024534604454,6.25029978465087));
#43554=CARTESIAN_POINT('Ctrl Pts',(54.4126331911631,30.9063577590828,6.24945683764299));
#43555=CARTESIAN_POINT('Ctrl Pts',(54.4662363949388,30.9224881866546,6.24584289566559));
#43556=CARTESIAN_POINT('Ctrl Pts',(54.5076614810664,30.9335115029647,6.24303353913215));
#43557=CARTESIAN_POINT('Ctrl Pts',(54.6200143082666,30.9595642119622,6.23536469466131));
#43558=CARTESIAN_POINT('Ctrl Pts',(54.6914547175895,30.9720747947637,6.230434387143));
#43559=CARTESIAN_POINT('Ctrl Pts',(54.8476731469693,30.9907349035604,6.21958026410742));
#43560=CARTESIAN_POINT('Ctrl Pts',(54.9324898441911,30.9954123754082,6.21364027235125));
#43561=CARTESIAN_POINT('Ctrl Pts',(55.106568590734,30.9938988192544,6.20154404726113));
#43562=CARTESIAN_POINT('Ctrl Pts',(55.195652684769,30.9871369211181,6.19540606022436));
#43563=CARTESIAN_POINT('Ctrl Pts',(55.2945143044327,30.9729170952118,6.18884583894524));
#43564=CARTESIAN_POINT('Ctrl Pts',(55.3050231372263,30.9713197198053,6.18815177029238));
#43565=CARTESIAN_POINT('Ctrl Pts',(55.3208738186932,30.9687805782239,6.187110345199));
#43566=CARTESIAN_POINT('Ctrl Pts',(55.3262252224566,30.9679009321158,6.18675968708387));
#43567=CARTESIAN_POINT('Ctrl Pts',(55.3358167149142,30.966284113986,6.18613296086047));
#43568=CARTESIAN_POINT('Ctrl Pts',(55.3400580499016,30.9655550378235,6.1858564511367));
#43569=CARTESIAN_POINT('Ctrl Pts',(55.3493268409547,30.9639308530502,6.18525355846166));
#43570=CARTESIAN_POINT('Ctrl Pts',(55.3543532240828,30.9630301656761,6.18492749189933));
#43571=CARTESIAN_POINT('Ctrl Pts',(55.368670060394,30.9604079226805,6.18400110237566));
#43572=CARTESIAN_POINT('Ctrl Pts',(55.3779519649456,30.9586396190321,6.18340333903162));
#43573=CARTESIAN_POINT('Ctrl Pts',(55.4402296428418,30.9463158410065,6.17940953647328));
#43574=CARTESIAN_POINT('Ctrl Pts',(55.4927953112126,30.9336756221015,6.17612093106042));
#43575=CARTESIAN_POINT('Ctrl Pts',(55.7230093482689,30.8683169486861,6.16182789922688));
#43576=CARTESIAN_POINT('Ctrl Pts',(55.8933151965619,30.7931387684466,6.15146135865577));
#43577=CARTESIAN_POINT('Ctrl Pts',(56.0933143678857,30.6691890199001,6.13729124872138));
#43578=CARTESIAN_POINT('Ctrl Pts',(56.1348117795988,30.6412586292119,6.13423393558637));
#43579=CARTESIAN_POINT('Ctrl Pts',(56.1868396443677,30.6033234988697,6.13022193770194));
#43580=CARTESIAN_POINT('Ctrl Pts',(56.1983733308368,30.5947212691795,6.12932078455072));
#43581=CARTESIAN_POINT('Ctrl Pts',(56.2166608143533,30.5807713970762,6.12787246908252));
#43582=CARTESIAN_POINT('Ctrl Pts',(56.2234749190573,30.5755033689872,6.1273284116399));
#43583=CARTESIAN_POINT('Ctrl Pts',(56.2357172707347,30.5659114114955,6.12634285411743));
#43584=CARTESIAN_POINT('Ctrl Pts',(56.2411575042861,30.5616029487089,6.12590196942683));
#43585=CARTESIAN_POINT('Ctrl Pts',(56.253928376632,30.5513800009336,6.12486001076704));
#43586=CARTESIAN_POINT('Ctrl Pts',(56.2612397745039,30.5454418485448,6.12425799898747));
#43587=CARTESIAN_POINT('Ctrl Pts',(56.2825211524651,30.5279059915603,6.12248938950158));
#43588=CARTESIAN_POINT('Ctrl Pts',(56.2963748692234,30.5161693137892,6.12131721077876));
#43589=CARTESIAN_POINT('Ctrl Pts',(56.4169083904272,30.4111951722558,6.11093020929373));
#43590=CARTESIAN_POINT('Ctrl Pts',(56.5135127305351,30.3070447673084,6.10124183258951));
#43591=CARTESIAN_POINT('Ctrl Pts',(56.6770293303521,30.0880859772198,6.08222299174596));
#43592=CARTESIAN_POINT('Ctrl Pts',(56.7451713177668,29.9750595243364,6.07297227009244));
#43593=CARTESIAN_POINT('Ctrl Pts',(56.808250511512,29.8423133853931,6.06324569867088));
#43594=CARTESIAN_POINT('Ctrl Pts',(56.8146595391249,29.8284156822456,6.06224078732908));
#43595=CARTESIAN_POINT('Ctrl Pts',(56.8232561111802,29.8091957635382,6.06087073666968));
#43596=CARTESIAN_POINT('Ctrl Pts',(56.8255813300257,29.8039362164424,6.06049783235387));
#43597=CARTESIAN_POINT('Ctrl Pts',(56.8295230486201,29.7949149258377,6.05986174674027));
#43598=CARTESIAN_POINT('Ctrl Pts',(56.8311507549924,29.7911581624284,6.05959790227346));
#43599=CARTESIAN_POINT('Ctrl Pts',(56.8345116429221,29.7833352610723,6.05905069108301));
#43600=CARTESIAN_POINT('Ctrl Pts',(56.8362428868957,29.7792683491474,6.05876745098275));
#43601=CARTESIAN_POINT('Ctrl Pts',(56.8404014108947,29.7694086408904,6.05808369670317));
#43602=CARTESIAN_POINT('Ctrl Pts',(56.8428149040626,29.7636100063569,6.05768400566394));
#43603=CARTESIAN_POINT('Ctrl Pts',(56.8512049999241,29.7431805872103,6.05628405327668));
#43604=CARTESIAN_POINT('Ctrl Pts',(56.8570352585872,29.7284898228396,6.0552921147949));
#43605=CARTESIAN_POINT('Ctrl Pts',(56.8921764506903,29.6367785409774,6.04918175999137));
#43606=CARTESIAN_POINT('Ctrl Pts',(56.9168689473078,29.5580637745161,6.04429321371887));
#43607=CARTESIAN_POINT('Ctrl Pts',(56.9689901415571,29.346911362959,6.03156764190196));
#43608=CARTESIAN_POINT('Ctrl Pts',(56.9879556947468,29.2128408072602,6.02385372205077));
#43609=CARTESIAN_POINT('Ctrl Pts',(56.9955874830295,29.0175227669985,6.01216657970325));
#43610=CARTESIAN_POINT('Ctrl Pts',(56.9952028185878,28.9570919116139,6.00849340824957));
#43611=CARTESIAN_POINT('Ctrl Pts',(56.9912942792531,28.8816629345709,6.00379313353684));
#43612=CARTESIAN_POINT('Ctrl Pts',(56.9903392482068,28.8665600324685,6.00284628793918));
#43613=CARTESIAN_POINT('Ctrl Pts',(56.9885525216129,28.8426310381501,6.00133641452591));
#43614=CARTESIAN_POINT('Ctrl Pts',(56.9878336578241,28.8337969130465,6.0007769004887));
#43615=CARTESIAN_POINT('Ctrl Pts',(56.9863822791434,28.817320095069,5.9997292917177));
#43616=CARTESIAN_POINT('Ctrl Pts',(56.9856644662942,28.8096762464264,5.99924166446368));
#43617=CARTESIAN_POINT('Ctrl Pts',(56.9839673074789,28.7926594717303,5.99815239866943));
#43618=CARTESIAN_POINT('Ctrl Pts',(56.9829656355396,28.7832890056479,5.99755007337295));
#43619=CARTESIAN_POINT('Ctrl Pts',(56.9798367055823,28.7558589513339,5.99577935751434));
#43620=CARTESIAN_POINT('Ctrl Pts',(56.977528896779,28.7378213229256,5.99460536384981));
#43621=CARTESIAN_POINT('Ctrl Pts',(56.9556456152207,28.5835681260892,5.98448052866964));
#43622=CARTESIAN_POINT('Ctrl Pts',(56.9222727988645,28.4497098063835,5.97508500323398));
#43623=CARTESIAN_POINT('Ctrl Pts',(56.8291016025179,28.1926071917617,5.95606468749601));
#43624=CARTESIAN_POINT('Ctrl Pts',(56.7698616905146,28.0698973296001,5.94650046650399));
#43625=CARTESIAN_POINT('Ctrl Pts',(56.6906676757398,27.9412746936394,5.93650639913881));
#43626=CARTESIAN_POINT('Ctrl Pts',(56.6825887179724,27.9284815899359,5.93551305842408));
#43627=CARTESIAN_POINT('Ctrl Pts',(56.671251670743,27.9109737293185,5.93415591001705));
#43628=CARTESIAN_POINT('Ctrl Pts',(56.6681179045737,27.9061796200582,5.93378452604483));
#43629=CARTESIAN_POINT('Ctrl Pts',(56.6627122098043,27.8979871239202,5.93315038071906));
#43630=CARTESIAN_POINT('Ctrl Pts',(56.6604504252254,27.8945821343139,5.9328869645658));
#43631=CARTESIAN_POINT('Ctrl Pts',(56.6557185142516,27.8875058005912,5.93233987817836));
#43632=CARTESIAN_POINT('Ctrl Pts',(56.6532466223867,27.8838356984093,5.9320563382285));
#43633=CARTESIAN_POINT('Ctrl Pts',(56.6472223431152,27.8749551643968,5.9313706782385));
#43634=CARTESIAN_POINT('Ctrl Pts',(56.6436573809517,27.8697532365046,5.93096939263456));
#43635=CARTESIAN_POINT('Ctrl Pts',(56.6309806228752,27.8514423679364,5.92955777384316));
#43636=CARTESIAN_POINT('Ctrl Pts',(56.6217359096769,27.8384255928387,5.92855594811371));
#43637=CARTESIAN_POINT('Ctrl Pts',(56.5985458493377,27.8065900718251,5.92610611475485));
#43638=CARTESIAN_POINT('Ctrl Pts',(56.5844231661395,27.7879028844157,5.92466839662416));
#43639=CARTESIAN_POINT('Ctrl Pts',(56.5247348862797,27.7117496067061,5.91879102854432));
#43640=CARTESIAN_POINT('Ctrl Pts',(56.4763435904853,27.6565652956145,5.91448635577703));
#43641=CARTESIAN_POINT('Ctrl Pts',(56.3068538569417,27.4835314533684,5.90037613600066));
#43642=CARTESIAN_POINT('Ctrl Pts',(56.173863119453,27.3784009282983,5.89070219568259));
#43643=CARTESIAN_POINT('Ctrl Pts',(56.0096781102839,27.2795063715418,5.87887804894824));
#43644=CARTESIAN_POINT('Ctrl Pts',(55.989932314196,27.2680698168799,5.877459165992));
#43645=CARTESIAN_POINT('Ctrl Pts',(55.961075773484,27.2520111223426,5.87538802600159));
#43646=CARTESIAN_POINT('Ctrl Pts',(55.9521184228187,27.2471160159493,5.87474545992219));
#43647=CARTESIAN_POINT('Ctrl Pts',(55.9362596749008,27.2386067819257,5.8736082153047));
#43648=CARTESIAN_POINT('Ctrl Pts',(55.9293738867726,27.2349639031118,5.8731145617548));
#43649=CARTESIAN_POINT('Ctrl Pts',(55.915080062402,27.2275086874467,5.87209000016603));
#43650=CARTESIAN_POINT('Ctrl Pts',(55.9076691379463,27.2237022472976,5.8715588979476));
#43651=CARTESIAN_POINT('Ctrl Pts',(55.8885391944048,27.214027594944,5.87018810232118));
#43652=CARTESIAN_POINT('Ctrl Pts',(55.8767859406093,27.2082283258026,5.86934603801476));
#43653=CARTESIAN_POINT('Ctrl Pts',(55.8264725725348,27.1840163722682,5.86574130897188));
#43654=CARTESIAN_POINT('Ctrl Pts',(55.7873857472753,27.1667306052127,5.8629405285689));
#43655=CARTESIAN_POINT('Ctrl Pts',(55.6808782788926,27.1236632922674,5.85530227752049));
#43656=CARTESIAN_POINT('Ctrl Pts',(55.6125680720841,27.1002649630747,5.85039469938749));
#43657=CARTESIAN_POINT('Ctrl Pts',(55.4845628845463,27.0640420375499,5.84121842712118));
#43658=CARTESIAN_POINT('Ctrl Pts',(55.4252526805483,27.0501553485057,5.83697496078905));
#43659=CARTESIAN_POINT('Ctrl Pts',(55.2617105768291,27.0196817382267,5.8253810476877));
#43660=CARTESIAN_POINT('Ctrl Pts',(55.1566391858276,27.008613197887,5.81804295730451));
#43661=CARTESIAN_POINT('Ctrl Pts',(55.035125726017,27.0054946607225,5.80999018001432));
#43662=CARTESIAN_POINT('Ctrl Pts',(55.0190697773188,27.0052765235279,5.80893503327229));
#43663=CARTESIAN_POINT('Ctrl Pts',(54.9965058790845,27.0052424488411,5.80746629805671));
#43664=CARTESIAN_POINT('Ctrl Pts',(54.9899992872413,27.005264457284,5.8070444162579));
#43665=CARTESIAN_POINT('Ctrl Pts',(54.9794723796783,27.0053515737654,5.80636465061021));
#43666=CARTESIAN_POINT('Ctrl Pts',(54.9754520144618,27.0053970007593,5.80610569755592));
#43667=CARTESIAN_POINT('Ctrl Pts',(54.966936811138,27.0055189655325,5.80555866414862));
#43668=CARTESIAN_POINT('Ctrl Pts',(54.9624420376718,27.0055985430264,5.805270758795));
#43669=CARTESIAN_POINT('Ctrl Pts',(54.9512979714052,27.005833529729,5.80455896162135));
#43670=CARTESIAN_POINT('Ctrl Pts',(54.9446490464113,27.0060070025999,5.80413606072854));
#43671=CARTESIAN_POINT('Ctrl Pts',(54.9197422397878,27.0067815074211,5.80255813815024));
#43672=CARTESIAN_POINT('Ctrl Pts',(54.901491377328,27.0076000968734,5.80141449466457));
#43673=CARTESIAN_POINT('Ctrl Pts',(54.8552563327153,27.0103107343628,5.7985434660906));
#43674=CARTESIAN_POINT('Ctrl Pts',(54.8272953755409,27.0125424849386,5.79683152648397));
#43675=CARTESIAN_POINT('Ctrl Pts',(54.6992571707259,27.0254848122089,5.7890665801158));
#43676=CARTESIAN_POINT('Ctrl Pts',(54.6000267391681,27.0431706865036,5.78325205005792));
#43677=CARTESIAN_POINT('Ctrl Pts',(54.3760734205213,27.1008422786077,5.76981948414682));
#43678=CARTESIAN_POINT('Ctrl Pts',(54.2531177754162,27.1457492363395,5.76219700707953));
#43679=CARTESIAN_POINT('Ctrl Pts',(54.1134998649133,27.212896830897,5.75265944960527));
#43680=CARTESIAN_POINT('Ctrl Pts',(54.0917563790041,27.2238486348719,5.75114807200526));
#43681=CARTESIAN_POINT('Ctrl Pts',(54.0615508456732,27.2397623029425,5.74900912771438));
#43682=CARTESIAN_POINT('Ctrl Pts',(54.0529161107412,27.2443930774059,5.74839308955682));
#43683=CARTESIAN_POINT('Ctrl Pts',(54.0379725150755,27.2525495977891,5.74731878244174));
#43684=CARTESIAN_POINT('Ctrl Pts',(54.0316479982493,27.2560463915509,5.74686154023548));
#43685=CARTESIAN_POINT('Ctrl Pts',(54.018487193125,27.2634165987734,5.74590460938088));
#43686=CARTESIAN_POINT('Ctrl Pts',(54.0116545216558,27.2672961845632,5.74540470690573));
#43687=CARTESIAN_POINT('Ctrl Pts',(53.9955048697496,27.2765925491261,5.74421568460849));
#43688=CARTESIAN_POINT('Ctrl Pts',(53.9862085911298,27.2820446221659,5.74352530770837));
#43689=CARTESIAN_POINT('Ctrl Pts',(53.9551242679141,27.3006150906336,5.74119654131422));
#43690=CARTESIAN_POINT('Ctrl Pts',(53.9335437623622,27.3140743312885,5.73954588508074));
#43691=CARTESIAN_POINT('Ctrl Pts',(53.8825847818005,27.3472261651163,5.73556440955052));
#43692=CARTESIAN_POINT('Ctrl Pts',(53.8534619597361,27.3672941512569,5.73322037865256));
#43693=CARTESIAN_POINT('Ctrl Pts',(53.7416250368162,27.4488269815449,5.72394489698141));
#43694=CARTESIAN_POINT('Ctrl Pts',(53.6631983210278,27.5158833566747,5.71682370772235));
#43695=CARTESIAN_POINT('Ctrl Pts',(53.5031638095426,27.6757340626276,5.70106756344419));
#43696=CARTESIAN_POINT('Ctrl Pts',(53.4242602921459,27.7706715172439,5.69243888993308));
#43697=CARTESIAN_POINT('Ctrl Pts',(53.3457078404214,27.8852833528123,5.68323763011562));
#43698=CARTESIAN_POINT('Ctrl Pts',(53.3369553689962,27.8983837578626,5.68220265405569));
#43699=CARTESIAN_POINT('Ctrl Pts',(53.3248360932572,27.9169971711783,5.68075707727969));
#43700=CARTESIAN_POINT('Ctrl Pts',(53.3213397072533,27.9224245427696,5.6803385187077));
#43701=CARTESIAN_POINT('Ctrl Pts',(53.3154995188614,27.9315875619623,5.67963694126219));
#43702=CARTESIAN_POINT('Ctrl Pts',(53.3131416647818,27.9353141464132,5.67935301321466));
#43703=CARTESIAN_POINT('Ctrl Pts',(53.3083534486854,27.9429377500027,5.67877507718099));
#43704=CARTESIAN_POINT('Ctrl Pts',(53.3059241555526,27.9468353930945,5.6784811390642));
#43705=CARTESIAN_POINT('Ctrl Pts',(53.2997610064949,27.956800268785,5.67773346563248));
#43706=CARTESIAN_POINT('Ctrl Pts',(53.2960461141464,27.9628792390494,5.6772809509678));
#43707=CARTESIAN_POINT('Ctrl Pts',(53.2810231671461,27.9877610847784,5.67544283002364));
#43708=CARTESIAN_POINT('Ctrl Pts',(53.2699926520123,28.006730830547,5.67407405642454));
#43709=CARTESIAN_POINT('Ctrl Pts',(53.2416492387349,28.0573796381182,5.67049436836086));
#43710=CARTESIAN_POINT('Ctrl Pts',(53.2248788409193,28.0893542271402,5.6683103904162));
#43711=CARTESIAN_POINT('Ctrl Pts',(53.1290871143118,28.2847063557645,5.65531361808838));
#43712=CARTESIAN_POINT('Ctrl Pts',(53.0717955771144,28.4577865181362,5.64515089894356));
#43713=CARTESIAN_POINT('Ctrl Pts',(53.0289208880002,28.6889544034501,5.63102947708381));
#43714=CARTESIAN_POINT('Ctrl Pts',(53.0212736085615,28.7420400547309,5.62775792800331));
#43715=CARTESIAN_POINT('Ctrl Pts',(53.0142632273663,28.8100159591008,5.62350212513587));
#43716=CARTESIAN_POINT('Ctrl Pts',(53.0129146975151,28.824681865257,5.62258006504534));
#43717=CARTESIAN_POINT('Ctrl Pts',(53.0110294845188,28.8480156521577,5.62110635272926));
#43718=CARTESIAN_POINT('Ctrl Pts',(53.0103867758722,28.856674608041,5.62055801017592));
#43719=CARTESIAN_POINT('Ctrl Pts',(53.0093333416006,28.8722434730398,5.61956935016476));
#43720=CARTESIAN_POINT('Ctrl Pts',(53.0089020099433,28.8791518842997,5.61912968257287));
#43721=CARTESIAN_POINT('Ctrl Pts',(53.007975516364,28.8953458771206,5.61809672794307));
#43722=CARTESIAN_POINT('Ctrl Pts',(53.0075093127419,28.9046328923534,5.6175025489317));
#43723=CARTESIAN_POINT('Ctrl Pts',(53.0063486368736,28.9315052685148,5.61577790630032));
#43724=CARTESIAN_POINT('Ctrl Pts',(53.0058219486616,28.94909663331,5.61464226610543));
#43725=CARTESIAN_POINT('Ctrl Pts',(53.0030727676453,29.1137177129465,5.60394993500629));
#43726=CARTESIAN_POINT('Ctrl Pts',(53.0168824057165,29.2605340668433,5.59387846756103));
#43727=CARTESIAN_POINT('Ctrl Pts',(53.0466869980211,29.4044698737854,5.5836423751603));
#43728=CARTESIAN_POINT('',(53.0052504464614,29.0013346002041,5.45145488139523));
#43729=CARTESIAN_POINT('Ctrl Pts',(53.0466869980082,29.4044698737233,5.42540812064255));
#43730=CARTESIAN_POINT('Ctrl Pts',(53.0341228174013,29.3437934700324,5.42937585424897));
#43731=CARTESIAN_POINT('Ctrl Pts',(53.0244059665824,29.2826156364975,5.43334358785539));
#43732=CARTESIAN_POINT('Ctrl Pts',(53.0175552112802,29.2212243706688,5.43731132146181));
#43733=CARTESIAN_POINT('Ctrl Pts',(53.009415042121,29.1482783571704,5.44202584143961));
#43734=CARTESIAN_POINT('Ctrl Pts',(53.0052996465098,29.0748710602292,5.44674036141742));
#43735=CARTESIAN_POINT('Ctrl Pts',(53.0052504464614,29.0013346002041,5.45145488139523));
#43736=CARTESIAN_POINT('Ctrl Pts',(53.0052504994822,29.0014116246202,5.45274812801779));
#43737=CARTESIAN_POINT('Ctrl Pts',(53.0051243702486,28.823179945905,5.46336349765806));
#43738=CARTESIAN_POINT('Ctrl Pts',(53.0288844422315,28.6457246371508,5.47335752524397));
#43739=CARTESIAN_POINT('Ctrl Pts',(53.0853141557639,28.4393971371445,5.48620705734885));
#43740=CARTESIAN_POINT('Ctrl Pts',(53.0956340276698,28.4052837002946,5.48837053488748));
#43741=CARTESIAN_POINT('Ctrl Pts',(53.1149113918893,28.3472204307118,5.49213320198773));
#43742=CARTESIAN_POINT('Ctrl Pts',(53.1234259273877,28.3231322993833,5.49371838887516));
#43743=CARTESIAN_POINT('Ctrl Pts',(53.1361781117867,28.289147583295,5.49599245218247));
#43744=CARTESIAN_POINT('Ctrl Pts',(53.140037078361,28.2791108877255,5.49666876644954));
#43745=CARTESIAN_POINT('Ctrl Pts',(53.1468394832641,28.261836945149,5.49784114265779));
#43746=CARTESIAN_POINT('Ctrl Pts',(53.1497446665786,28.254584817264,5.49833591375741));
#43747=CARTESIAN_POINT('Ctrl Pts',(53.1553962697641,28.2407134956761,5.4992872989044));
#43748=CARTESIAN_POINT('Ctrl Pts',(53.1581359101351,28.2340916572393,5.49974367781418));
#43749=CARTESIAN_POINT('Ctrl Pts',(53.1646621936556,28.2185548558603,5.50081975660486));
#43750=CARTESIAN_POINT('Ctrl Pts',(53.1684781785465,28.2096524886123,5.50144044466351));
#43751=CARTESIAN_POINT('Ctrl Pts',(53.1819369172502,28.1788753608719,5.50360079200397));
#43752=CARTESIAN_POINT('Ctrl Pts',(53.1919076432231,28.1571471108125,5.50515157542793));
#43753=CARTESIAN_POINT('Ctrl Pts',(53.2670189394738,28.0009338336864,5.5164924795253));
#43754=CARTESIAN_POINT('Ctrl Pts',(53.3466873599294,27.8739902781695,5.52680393141826));
#43755=CARTESIAN_POINT('Ctrl Pts',(53.4941863319689,27.6888233574931,5.54331678543631));
#43756=CARTESIAN_POINT('Ctrl Pts',(53.5530483972595,27.624139638695,5.54941695053602));
#43757=CARTESIAN_POINT('Ctrl Pts',(53.6346300899288,27.545536385824,5.55710080103722));
#43758=CARTESIAN_POINT('Ctrl Pts',(53.6536453904161,27.5279168520392,5.55884242915338));
#43759=CARTESIAN_POINT('Ctrl Pts',(53.6817359458982,27.5028879927363,5.56133829437962));
#43760=CARTESIAN_POINT('Ctrl Pts',(53.6905408397385,27.4951806749556,5.56210999418487));
#43761=CARTESIAN_POINT('Ctrl Pts',(53.7063212244745,27.4816107893552,5.56347352690025));
#43762=CARTESIAN_POINT('Ctrl Pts',(53.7132699465959,27.475717760212,5.56406733786493));
#43763=CARTESIAN_POINT('Ctrl Pts',(53.724123124669,27.466640571138,5.56498427985308));
#43764=CARTESIAN_POINT('Ctrl Pts',(53.7279995710887,27.463423334391,5.56530972473934));
#43765=CARTESIAN_POINT('Ctrl Pts',(53.7319064934698,27.4602057209625,5.56563562782453));
#43766=CARTESIAN_POINT('Ctrl Pts',(53.7319247720948,27.4601906678313,5.56563715252347));
#43767=CARTESIAN_POINT('Ctrl Pts',(53.7319614874054,27.4601604324972,5.56564021501336));
#43768=CARTESIAN_POINT('Ctrl Pts',(53.7319799240775,27.4601452503149,5.56564175280239));
#43769=CARTESIAN_POINT('Ctrl Pts',(53.732016958123,27.4601147547324,5.56564484169033));
#43770=CARTESIAN_POINT('Ctrl Pts',(53.7320355556297,27.4600994412323,5.56564639279954));
#43771=CARTESIAN_POINT('Ctrl Pts',(53.735364856519,27.4573581400278,5.56592406177133));
#43772=CARTESIAN_POINT('Ctrl Pts',(53.7386842826977,27.4546428840048,5.56619938894165));
#43773=CARTESIAN_POINT('Ctrl Pts',(53.7461805916915,27.448551225902,5.56681779141259));
#43774=CARTESIAN_POINT('Ctrl Pts',(53.7503623684838,27.4451809755419,5.56716042735255));
#43775=CARTESIAN_POINT('Ctrl Pts',(53.7626669133761,27.435345991954,5.56816194603189));
#43776=CARTESIAN_POINT('Ctrl Pts',(53.7708267416976,27.4289276133442,5.56881765231527));
#43777=CARTESIAN_POINT('Ctrl Pts',(53.8341825194713,27.3798888338048,5.57384716914853));
#43778=CARTESIAN_POINT('Ctrl Pts',(53.8915354636155,27.3401207356254,5.57804272504762));
#43779=CARTESIAN_POINT('Ctrl Pts',(54.0429511921845,27.2464866546377,5.58855820432079));
#43780=CARTESIAN_POINT('Ctrl Pts',(54.1395283222239,27.1971296729067,5.59476105051674));
#43781=CARTESIAN_POINT('Ctrl Pts',(54.3046189887543,27.1290608273355,5.60520978789602));
#43782=CARTESIAN_POINT('Ctrl Pts',(54.3709673988639,27.1057231059785,5.60936884213672));
#43783=CARTESIAN_POINT('Ctrl Pts',(54.4787135949044,27.0741099043881,5.61617737858332));
#43784=CARTESIAN_POINT('Ctrl Pts',(54.5193828199309,27.0635602469462,5.61875872796345));
#43785=CARTESIAN_POINT('Ctrl Pts',(54.5730770201309,27.0514275718044,5.62219545391431));
#43786=CARTESIAN_POINT('Ctrl Pts',(54.5858290390408,27.0486773354919,5.62301371825951));
#43787=CARTESIAN_POINT('Ctrl Pts',(54.6067665328694,27.0443762139883,5.62436098548788));
#43788=CARTESIAN_POINT('Ctrl Pts',(54.6149365019882,27.04275115246,5.62488763294647));
#43789=CARTESIAN_POINT('Ctrl Pts',(54.6307908632533,27.0397007231144,5.62591153718839));
#43790=CARTESIAN_POINT('Ctrl Pts',(54.6384739360747,27.0382692478609,5.62640859085829));
#43791=CARTESIAN_POINT('Ctrl Pts',(54.6562816734196,27.0350595572168,5.6275627499452));
#43792=CARTESIAN_POINT('Ctrl Pts',(54.6664119969846,27.0333143948594,5.62822088223868));
#43793=CARTESIAN_POINT('Ctrl Pts',(54.6993976136719,27.0278941122551,5.63036916625568));
#43794=CARTESIAN_POINT('Ctrl Pts',(54.7223027995737,27.0245386316445,5.63186924780907));
#43795=CARTESIAN_POINT('Ctrl Pts',(54.9086468084579,27.000545113172,5.64414509551553));
#43796=CARTESIAN_POINT('Ctrl Pts',(55.0739811408788,26.999832187681,5.65556413672351));
#43797=CARTESIAN_POINT('Ctrl Pts',(55.3122225787306,27.0283988556418,5.67227205711633));
#43798=CARTESIAN_POINT('Ctrl Pts',(55.3864006372345,27.0415848314658,5.67749720673242));
#43799=CARTESIAN_POINT('Ctrl Pts',(55.482818101896,27.0644172383239,5.68419592114564));
#43800=CARTESIAN_POINT('Ctrl Pts',(55.5058775449852,27.0703155800818,5.68579061934464));
#43801=CARTESIAN_POINT('Ctrl Pts',(55.5444164403186,27.0809117510184,5.6884374127566));
#43802=CARTESIAN_POINT('Ctrl Pts',(55.5599538682012,27.0853875919484,5.68949941407683));
#43803=CARTESIAN_POINT('Ctrl Pts',(55.5815177858884,27.0918844436673,5.6909646053593));
#43804=CARTESIAN_POINT('Ctrl Pts',(55.587591150264,27.0937459365562,5.69137629788698));
#43805=CARTESIAN_POINT('Ctrl Pts',(55.5978990541474,27.0969592647107,5.69207326035051));
#43806=CARTESIAN_POINT('Ctrl Pts',(55.6021381252689,27.0982962905482,5.69235937013802));
#43807=CARTESIAN_POINT('Ctrl Pts',(55.6102681678322,27.1008904599946,5.69290706460656));
#43808=CARTESIAN_POINT('Ctrl Pts',(55.6141597810002,27.1021454097484,5.69316877830027));
#43809=CARTESIAN_POINT('Ctrl Pts',(55.623484977232,27.1051842435332,5.69379488152643));
#43810=CARTESIAN_POINT('Ctrl Pts',(55.6289148385437,27.1069795575434,5.69415861312416));
#43811=CARTESIAN_POINT('Ctrl Pts',(55.6485755332966,27.1135740446853,5.69547285275241));
#43812=CARTESIAN_POINT('Ctrl Pts',(55.6627601933935,27.1185106790596,5.69641575326356));
#43813=CARTESIAN_POINT('Ctrl Pts',(55.8055803419602,27.1700314902501,5.70586866119001));
#43814=CARTESIAN_POINT('Ctrl Pts',(55.9291744147149,27.2295790814892,5.71372933708038));
#43815=CARTESIAN_POINT('Ctrl Pts',(56.1621867233661,27.3730220832878,5.72962830695051));
#43816=CARTESIAN_POINT('Ctrl Pts',(56.2709618187409,27.4565025581736,5.73763538125252));
#43817=CARTESIAN_POINT('Ctrl Pts',(56.3835069639838,27.5628971745225,5.74724001182875));
#43818=CARTESIAN_POINT('Ctrl Pts',(56.3965069076698,27.5755265977855,5.74837123807565));
#43819=CARTESIAN_POINT('Ctrl Pts',(56.4159953581795,27.5949827954121,5.75010169420315));
#43820=CARTESIAN_POINT('Ctrl Pts',(56.4226108175827,27.6016814896445,5.7506953355887));
#43821=CARTESIAN_POINT('Ctrl Pts',(56.4340211459099,27.6134001650665,5.75173028634165));
#43822=CARTESIAN_POINT('Ctrl Pts',(56.4388377279617,27.6183988492438,5.75217064420853));
#43823=CARTESIAN_POINT('Ctrl Pts',(56.4495781877454,27.6296624573515,5.75316050320812));
#43824=CARTESIAN_POINT('Ctrl Pts',(56.4554877061842,27.63594082368,5.7537106063262));
#43825=CARTESIAN_POINT('Ctrl Pts',(56.471170774334,27.6528207145162,5.75518535941987));
#43826=CARTESIAN_POINT('Ctrl Pts',(56.4808702423791,27.6634900742106,5.7561131031886));
#43827=CARTESIAN_POINT('Ctrl Pts',(56.523867797224,27.7118298689125,5.76029767083468));
#43828=CARTESIAN_POINT('Ctrl Pts',(56.5558476892036,27.7506431352072,5.7636078502144));
#43829=CARTESIAN_POINT('Ctrl Pts',(56.698622549301,27.9379187621129,5.77936465902168));
#43830=CARTESIAN_POINT('Ctrl Pts',(56.7898488000355,28.1001350618055,5.79252054339303));
#43831=CARTESIAN_POINT('Ctrl Pts',(56.8706229093093,28.3063741604563,5.80769572840009));
#43832=CARTESIAN_POINT('Ctrl Pts',(56.8829435403619,28.3405526460518,5.81015935008419));
#43833=CARTESIAN_POINT('Ctrl Pts',(56.9012306551285,28.3959838897776,5.81405391619489));
#43834=CARTESIAN_POINT('Ctrl Pts',(56.9077896145335,28.4170314339323,5.81550974967522));
#43835=CARTESIAN_POINT('Ctrl Pts',(56.9160096185182,28.4450354202302,5.8174126542167));
#43836=CARTESIAN_POINT('Ctrl Pts',(56.9179838361426,28.4518973170305,5.81787623902597));
#43837=CARTESIAN_POINT('Ctrl Pts',(56.9211689660514,28.4631960182846,5.8186349887387));
#43838=CARTESIAN_POINT('Ctrl Pts',(56.9224014349827,28.4676266021654,5.81893136447483));
#43839=CARTESIAN_POINT('Ctrl Pts',(56.9247844722703,28.476309534921,5.81950988132743));
#43840=CARTESIAN_POINT('Ctrl Pts',(56.9259362902992,28.4805614818496,5.81979208906304));
#43841=CARTESIAN_POINT('Ctrl Pts',(56.928737956676,28.4910412939383,5.82048505301578));
#43842=CARTESIAN_POINT('Ctrl Pts',(56.9303717548881,28.4972734732787,5.82089489565217));
#43843=CARTESIAN_POINT('Ctrl Pts',(56.9358812590743,28.5187125811551,5.8222973990816));
#43844=CARTESIAN_POINT('Ctrl Pts',(56.9396078098455,28.5339577180397,5.82328197444759));
#43845=CARTESIAN_POINT('Ctrl Pts',(56.9712177999448,28.6702250760193,5.83198231632844));
#43846=CARTESIAN_POINT('Ctrl Pts',(56.9879260019381,28.7935783999363,5.83916693255887));
#43847=CARTESIAN_POINT('Ctrl Pts',(56.9972739877713,29.0199539569346,5.85232212985626));
#43848=CARTESIAN_POINT('Ctrl Pts',(56.9936206220023,29.1223778672296,5.85826414135199));
#43849=CARTESIAN_POINT('Ctrl Pts',(56.9781703031958,29.2590559335216,5.86653324549573));
#43850=CARTESIAN_POINT('Ctrl Pts',(56.9732888401537,29.2939365033879,5.86867263638917));
#43851=CARTESIAN_POINT('Ctrl Pts',(56.9633109329982,29.3536666583885,5.87239869362057));
#43852=CARTESIAN_POINT('Ctrl Pts',(56.9586590426868,29.3785823418286,5.87397184714782));
#43853=CARTESIAN_POINT('Ctrl Pts',(56.9513588776086,29.4139344894648,5.87623382647598));
#43854=CARTESIAN_POINT('Ctrl Pts',(56.9490987794719,29.4244492566038,5.87691039112654));
#43855=CARTESIAN_POINT('Ctrl Pts',(56.9450429424901,29.4426026202448,5.87808523221383));
#43856=CARTESIAN_POINT('Ctrl Pts',(56.9432869413356,29.4502499176697,5.87858223550771));
#43857=CARTESIAN_POINT('Ctrl Pts',(56.9398284883154,29.4649141122475,5.87953937129112));
#43858=CARTESIAN_POINT('Ctrl Pts',(56.9381329629381,29.4719325286272,5.87999927546284));
#43859=CARTESIAN_POINT('Ctrl Pts',(56.9340476970148,29.4884495902442,5.88108595046646));
#43860=CARTESIAN_POINT('Ctrl Pts',(56.9316260430119,29.4979400775795,5.88171373521028));
#43861=CARTESIAN_POINT('Ctrl Pts',(56.9229374349614,29.5309733676697,5.88391093414111));
#43862=CARTESIAN_POINT('Ctrl Pts',(56.9163093613801,29.5544181100595,5.88549186943257));
#43863=CARTESIAN_POINT('Ctrl Pts',(56.8715252443568,29.7024172484047,5.89561314582776));
#43864=CARTESIAN_POINT('Ctrl Pts',(56.821680662501,29.8230829147425,5.90453613215046));
#43865=CARTESIAN_POINT('Ctrl Pts',(56.7128934658764,30.0272530140889,5.92063535153886));
#43866=CARTESIAN_POINT('Ctrl Pts',(56.6586242518417,30.112753321118,5.92772458299025));
#43867=CARTESIAN_POINT('Ctrl Pts',(56.5812801946533,30.216293863772,5.93650921685234));
#43868=CARTESIAN_POINT('Ctrl Pts',(56.5639815868616,30.2384585484714,5.9384018088601));
#43869=CARTESIAN_POINT('Ctrl Pts',(56.5346609473686,30.2744324394118,5.94148428674759));
#43870=CARTESIAN_POINT('Ctrl Pts',(56.5229074713133,30.2884545613956,5.94268858793973));
#43871=CARTESIAN_POINT('Ctrl Pts',(56.506621268824,30.3073500391843,5.9443130027469));
#43872=CARTESIAN_POINT('Ctrl Pts',(56.5022550572408,30.3123648572918,5.94474427130239));
#43873=CARTESIAN_POINT('Ctrl Pts',(56.4948980868386,30.3207298885599,5.94546377260231));
#43874=CARTESIAN_POINT('Ctrl Pts',(56.4919209725298,30.3240919686844,5.94575298735202));
#43875=CARTESIAN_POINT('Ctrl Pts',(56.4862582925413,30.3304435345939,5.9462993786686));
#43876=CARTESIAN_POINT('Ctrl Pts',(56.4835750153007,30.3334349948763,5.94655672566556));
#43877=CARTESIAN_POINT('Ctrl Pts',(56.4765294703774,30.3412421500516,5.94722843739487));
#43878=CARTESIAN_POINT('Ctrl Pts',(56.4721526374619,30.3460447231754,5.94764172506316));
#43879=CARTESIAN_POINT('Ctrl Pts',(56.4569143420002,30.3626020336426,5.94906722204481));
#43880=CARTESIAN_POINT('Ctrl Pts',(56.4459346074727,30.374247739958,5.95007099988089));
#43881=CARTESIAN_POINT('Ctrl Pts',(56.3554621189796,30.4679228967994,5.95816708621102));
#43882=CARTESIAN_POINT('Ctrl Pts',(56.2691868783676,30.5431288965373,5.96481328119672));
#43883=CARTESIAN_POINT('Ctrl Pts',(56.089622460271,30.6743493260088,5.97773281715732));
#43884=CARTESIAN_POINT('Ctrl Pts',(55.9972692535995,30.7309462415362,5.98398857887714));
#43885=CARTESIAN_POINT('Ctrl Pts',(55.8674839124194,30.7966336459837,5.99271437211588));
#43886=CARTESIAN_POINT('Ctrl Pts',(55.833715520682,30.8125504077134,5.99497783683222));
#43887=CARTESIAN_POINT('Ctrl Pts',(55.7752379966984,30.8381338879296,5.99890084547824));
#43888=CARTESIAN_POINT('Ctrl Pts',(55.7507456702286,30.8482724306315,6.0005448468812));
#43889=CARTESIAN_POINT('Ctrl Pts',(55.71585599014,30.8619070262258,6.00289136577377));
#43890=CARTESIAN_POINT('Ctrl Pts',(55.7056200106054,30.8658102706184,6.00358033635454));
#43891=CARTESIAN_POINT('Ctrl Pts',(55.6879581041119,30.8723790884211,6.00477030318122));
#43892=CARTESIAN_POINT('Ctrl Pts',(55.6805474863075,30.8750853099943,6.00526994212671));
#43893=CARTESIAN_POINT('Ctrl Pts',(55.6663532950211,30.8801735392379,6.0062276955104));
#43894=CARTESIAN_POINT('Ctrl Pts',(55.6595725021178,30.8825629773462,6.00668555571313));
#43895=CARTESIAN_POINT('Ctrl Pts',(55.6419401571575,30.8886693644042,6.00787706769655));
#43896=CARTESIAN_POINT('Ctrl Pts',(55.6310693180359,30.8923294216918,6.00861257155633));
#43897=CARTESIAN_POINT('Ctrl Pts',(55.593814228106,30.9045159604478,6.0111366146564));
#43898=CARTESIAN_POINT('Ctrl Pts',(55.5672850392769,30.9125856681373,6.01293986574604));
#43899=CARTESIAN_POINT('Ctrl Pts',(55.3366673240301,30.977515283591,6.02867353583479));
#43900=CARTESIAN_POINT('Ctrl Pts',(55.1249105147715,31.0020663939471,6.04371963022209));
#43901=CARTESIAN_POINT('Ctrl Pts',(54.8576520012668,30.9904452013711,6.06206383555487));
#43902=CARTESIAN_POINT('Ctrl Pts',(54.8020799479456,30.9856897895796,6.06582940817737));
#43903=CARTESIAN_POINT('Ctrl Pts',(54.7373301971144,30.9774030454849,6.07010717927522));
#43904=CARTESIAN_POINT('Ctrl Pts',(54.7278938533528,30.9761266364305,6.07072784137697));
#43905=CARTESIAN_POINT('Ctrl Pts',(54.7133946408433,30.9740595685501,6.07167688488032));
#43906=CARTESIAN_POINT('Ctrl Pts',(54.708325227481,30.9733169133662,6.07200783167734));
#43907=CARTESIAN_POINT('Ctrl Pts',(54.6990027647369,30.9719144883695,6.07261475753468));
#43908=CARTESIAN_POINT('Ctrl Pts',(54.6947490024847,30.9712604886903,6.07289104355579));
#43909=CARTESIAN_POINT('Ctrl Pts',(54.685156828082,30.969753934718,6.07351261889783));
#43910=CARTESIAN_POINT('Ctrl Pts',(54.6798197536788,30.9688934449975,6.07385746001496));
#43911=CARTESIAN_POINT('Ctrl Pts',(54.6640809465861,30.966290208159,6.07487159647397));
#43912=CARTESIAN_POINT('Ctrl Pts',(54.6536892708555,30.9644866208319,6.07553759346337));
#43913=CARTESIAN_POINT('Ctrl Pts',(54.5640058476712,30.9481873346454,6.08125805676871));
#43914=CARTESIAN_POINT('Ctrl Pts',(54.4856358216565,30.9289783568547,6.08607341876405));
#43915=CARTESIAN_POINT('Ctrl Pts',(54.3065952741266,30.8734014085041,6.09708469817586));
#43916=CARTESIAN_POINT('Ctrl Pts',(54.2072649467573,30.8335797700217,6.10320863638305));
#43917=CARTESIAN_POINT('Ctrl Pts',(54.0335066935849,30.7471479398676,6.11460409602138));
#43918=CARTESIAN_POINT('Ctrl Pts',(53.9580530074242,30.7032260891853,6.11981146278568));
#43919=CARTESIAN_POINT('Ctrl Pts',(53.8676154953236,30.642318290226,6.12654499117124));
#43920=CARTESIAN_POINT('Ctrl Pts',(53.8497124074744,30.6298289570712,6.1279033384047));
#43921=CARTESIAN_POINT('Ctrl Pts',(53.8238002977516,30.6111128435897,6.12990875840758));
#43922=CARTESIAN_POINT('Ctrl Pts',(53.8156276861906,30.6051144976518,6.13054713235738));
#43923=CARTESIAN_POINT('Ctrl Pts',(53.8012861823812,30.5944192848014,6.13167796634376));
#43924=CARTESIAN_POINT('Ctrl Pts',(53.7950982407657,30.5897482253925,6.13216942101721));
#43925=CARTESIAN_POINT('Ctrl Pts',(53.7830582056641,30.5805489494834,6.13313267118159));
#43926=CARTESIAN_POINT('Ctrl Pts',(53.7772037610154,30.5760240061703,6.13360433344885));
#43927=CARTESIAN_POINT('Ctrl Pts',(53.7614500986313,30.5637072647499,6.13488252164843));
#43928=CARTESIAN_POINT('Ctrl Pts',(53.7515994279111,30.5558541922768,6.1356914595393));
#43929=CARTESIAN_POINT('Ctrl Pts',(53.7147008787404,30.5258621934304,6.13875892187169));
#43930=CARTESIAN_POINT('Ctrl Pts',(53.6881634280438,30.5031080530749,6.14104195194072));
#43931=CARTESIAN_POINT('Ctrl Pts',(53.5118231726884,30.3436797899028,6.15675655580967));
#43932=CARTESIAN_POINT('Ctrl Pts',(53.3830373974161,30.1855572873459,6.17116159103879));
#43933=CARTESIAN_POINT('Ctrl Pts',(53.2523220195476,29.9631732114552,6.18884664082957));
#43934=CARTESIAN_POINT('Ctrl Pts',(53.2263097031231,29.9143877175651,6.19257837972626));
#43935=CARTESIAN_POINT('Ctrl Pts',(53.1982378937371,29.8560204997555,6.19682256392062));
#43936=CARTESIAN_POINT('Ctrl Pts',(53.1941820825243,29.8474310833616,6.1974416863755));
#43937=CARTESIAN_POINT('Ctrl Pts',(53.188036096121,29.8341705780667,6.19838876061404));
#43938=CARTESIAN_POINT('Ctrl Pts',(53.1859023462123,29.8295200095293,6.19871926490623));
#43939=CARTESIAN_POINT('Ctrl Pts',(53.1820074233556,29.8209440074579,6.19932565215712));
#43940=CARTESIAN_POINT('Ctrl Pts',(53.1802410617463,29.8170211009625,6.19960183975046));
#43941=CARTESIAN_POINT('Ctrl Pts',(53.1762826174932,29.808153281798,6.20022350419443));
#43942=CARTESIAN_POINT('Ctrl Pts',(53.1740979503492,29.8032051573978,6.20056853076356));
#43943=CARTESIAN_POINT('Ctrl Pts',(53.1677059792656,29.7885669161725,6.20158394798967));
#43944=CARTESIAN_POINT('Ctrl Pts',(53.1635554164891,29.7788520160157,6.20225102614816));
#43945=CARTESIAN_POINT('Ctrl Pts',(53.1278396634481,29.6933818431783,6.208064167495));
#43946=CARTESIAN_POINT('Ctrl Pts',(53.1008962968186,29.6157687884393,6.21296219580502));
#43947=CARTESIAN_POINT('Ctrl Pts',(53.0665961605006,29.4929885107095,6.22044491636916));
#43948=CARTESIAN_POINT('Ctrl Pts',(53.0558836360809,29.4488833620477,6.22308124932006));
#43949=CARTESIAN_POINT('Ctrl Pts',(53.0466869743493,29.404469759467,6.22571516850575));
#43950=CARTESIAN_POINT('Origin',(55.,29.,3.45145488139523));
#43951=CARTESIAN_POINT('',(53.0466869981335,29.4044698743284,7.18242967527062));
#43952=CARTESIAN_POINT('',(53.0466869980042,29.4044698737041,7.02360963496714));
#43953=CARTESIAN_POINT('',(53.0466869980082,29.4044698737233,3.45145488139523));
#43954=CARTESIAN_POINT('Ctrl Pts',(53.0466869981335,29.4044698743284,7.18242967527062));
#43955=CARTESIAN_POINT('Ctrl Pts',(53.0666916447592,29.5010786425753,7.17661931946525));
#43956=CARTESIAN_POINT('Ctrl Pts',(53.0938369179684,29.5960751312477,7.17095413793509));
#43957=CARTESIAN_POINT('Ctrl Pts',(53.1530599331324,29.7570666411215,7.16092930501707));
#43958=CARTESIAN_POINT('Ctrl Pts',(53.1819445957839,29.8240211123612,7.15662490802084));
#43959=CARTESIAN_POINT('Ctrl Pts',(53.233600278732,29.9277444422827,7.14960490747043));
#43960=CARTESIAN_POINT('Ctrl Pts',(53.2540144845991,29.9656147744896,7.14696331199493));
#43961=CARTESIAN_POINT('Ctrl Pts',(53.2822395067726,30.0141494034132,7.14345873691704));
#43962=CARTESIAN_POINT('Ctrl Pts',(53.2889552182893,30.0254393529079,7.14263487657998));
#43963=CARTESIAN_POINT('Ctrl Pts',(53.3001149317604,30.0437853399635,7.14128151710104));
#43964=CARTESIAN_POINT('Ctrl Pts',(53.3044926035728,30.0508814140537,7.14075443000207));
#43965=CARTESIAN_POINT('Ctrl Pts',(53.3130446597757,30.0645514939051,7.13973190469558));
#43966=CARTESIAN_POINT('Ctrl Pts',(53.3172133121716,30.0711289201349,7.13923668317857));
#43967=CARTESIAN_POINT('Ctrl Pts',(53.326926162893,30.0862575002357,7.13809006587162));
#43968=CARTESIAN_POINT('Ctrl Pts',(53.3324975556609,30.0947908535497,7.13743767277651));
#43969=CARTESIAN_POINT('Ctrl Pts',(53.3507036595188,30.1222146055288,7.13532252944452));
#43970=CARTESIAN_POINT('Ctrl Pts',(53.3635955057812,30.1409313303226,7.13385023040724));
#43971=CARTESIAN_POINT('Ctrl Pts',(53.4754177308781,30.2974828099682,7.12128492581618));
#43972=CARTESIAN_POINT('Ctrl Pts',(53.5912251323893,30.4223724427831,7.10950182275871));
#43973=CARTESIAN_POINT('Ctrl Pts',(53.7772962687928,30.5777600381371,7.09261792691267));
#43974=CARTESIAN_POINT('Ctrl Pts',(53.8357121773471,30.6213470895029,7.08756632949024));
#43975=CARTESIAN_POINT('Ctrl Pts',(53.9158119639947,30.6745470387087,7.08106784276053));
#43976=CARTESIAN_POINT('Ctrl Pts',(53.9354651670009,30.687109116457,7.07950561023867));
#43977=CARTESIAN_POINT('Ctrl Pts',(53.9688919564254,30.707658342189,7.07690775189745));
#43978=CARTESIAN_POINT('Ctrl Pts',(53.9825486509922,30.7158302951325,7.0758626004635));
#43979=CARTESIAN_POINT('Ctrl Pts',(54.0017451669593,30.7270073886353,7.07441750944381));
#43980=CARTESIAN_POINT('Ctrl Pts',(54.0072032173153,30.7301507977539,7.07400931112081));
#43981=CARTESIAN_POINT('Ctrl Pts',(54.0165198651018,30.7354578516306,7.0733171996565));
#43982=CARTESIAN_POINT('Ctrl Pts',(54.0203709131133,30.7376345945271,7.07303246319501));
#43983=CARTESIAN_POINT('Ctrl Pts',(54.0277965393561,30.7417992772045,7.07248606549673));
#43984=CARTESIAN_POINT('Ctrl Pts',(54.0313700135177,30.7437890471543,7.07222428269351));
#43985=CARTESIAN_POINT('Ctrl Pts',(54.0399689844973,30.7485425086628,7.07159707347549));
#43986=CARTESIAN_POINT('Ctrl Pts',(54.0450003643735,30.7512955642067,7.07123231311435));
#43987=CARTESIAN_POINT('Ctrl Pts',(54.0633979474697,30.7612594371632,7.0699063943199));
#43988=CARTESIAN_POINT('Ctrl Pts',(54.0768349079327,30.7683394626468,7.06895304585028));
#43989=CARTESIAN_POINT('Ctrl Pts',(54.2102501979229,30.8367016096683,7.05962200653594));
#43990=CARTESIAN_POINT('Ctrl Pts',(54.3360819729028,30.8858422229226,7.05187350183976));
#43991=CARTESIAN_POINT('Ctrl Pts',(54.5995404604579,30.9590538760853,7.0359899908337));
#43992=CARTESIAN_POINT('Ctrl Pts',(54.7366465759225,30.9821447891328,7.0278805683961));
#43993=CARTESIAN_POINT('Ctrl Pts',(54.8931849903518,30.9919711390948,7.01815480816874));
#43994=CARTESIAN_POINT('Ctrl Pts',(54.9113542428573,30.9928623537587,7.01701953450466));
#43995=CARTESIAN_POINT('Ctrl Pts',(54.9389525769092,30.9938379121207,7.0152843135652));
#43996=CARTESIAN_POINT('Ctrl Pts',(54.9483745749343,30.9941041142017,7.0146900090323));
#43997=CARTESIAN_POINT('Ctrl Pts',(54.965474619833,30.9944659730976,7.01360779829824));
#43998=CARTESIAN_POINT('Ctrl Pts',(54.9731520469343,30.9945840931025,7.01312059939424));
#43999=CARTESIAN_POINT('Ctrl Pts',(54.9896930383754,30.9947430641319,7.01206800895863));
#44000=CARTESIAN_POINT('Ctrl Pts',(54.9985565479559,30.994769169014,7.01150216965427));
#44001=CARTESIAN_POINT('Ctrl Pts',(55.0225511871177,30.9946799161412,7.00996533682697));
#44002=CARTESIAN_POINT('Ctrl Pts',(55.0376810669348,30.9944514635071,7.00899085906464));
#44003=CARTESIAN_POINT('Ctrl Pts',(55.1131586459729,30.9924526628192,7.00410144985794));
#44004=CARTESIAN_POINT('Ctrl Pts',(55.1734011806347,30.9881155033851,7.00010792318171));
#44005=CARTESIAN_POINT('Ctrl Pts',(55.3675792227355,30.9652431624853,6.986934621165));
#44006=CARTESIAN_POINT('Ctrl Pts',(55.4998431342191,30.9358316927362,6.97746544346421));
#44007=CARTESIAN_POINT('Ctrl Pts',(55.7062664672906,30.8673505024225,6.96235172744517));
#44008=CARTESIAN_POINT('Ctrl Pts',(55.7827615925344,30.836599386846,6.95668043012796));
#44009=CARTESIAN_POINT('Ctrl Pts',(55.8714098643384,30.7944141247573,6.95018158837856));
#44010=CARTESIAN_POINT('Ctrl Pts',(55.8855962028438,30.7874553436784,6.94914402786589));
#44011=CARTESIAN_POINT('Ctrl Pts',(55.9053042238755,30.7774957858713,6.94770757929789));
#44012=CARTESIAN_POINT('Ctrl Pts',(55.9108962525276,30.7746365899119,6.94730055997782));
#44013=CARTESIAN_POINT('Ctrl Pts',(55.9204008384593,30.7697201466181,6.94660984463038));
#44014=CARTESIAN_POINT('Ctrl Pts',(55.9243202063734,30.7676762311936,6.94632533319063));
#44015=CARTESIAN_POINT('Ctrl Pts',(55.9318568602372,30.7637140125621,6.94577889113273));
#44016=CARTESIAN_POINT('Ctrl Pts',(55.93547505671,30.7617975891357,6.94551684164791));
#44017=CARTESIAN_POINT('Ctrl Pts',(55.9441614424461,30.7571624314138,6.94488835405222));
#44018=CARTESIAN_POINT('Ctrl Pts',(55.9492238595146,30.7544328731092,6.94452258801589));
#44019=CARTESIAN_POINT('Ctrl Pts',(55.9677183692727,30.7443575030099,6.94318796783252));
#44020=CARTESIAN_POINT('Ctrl Pts',(55.9810779828172,30.7368787998858,6.94222706134827));
#44021=CARTESIAN_POINT('Ctrl Pts',(56.1083569115992,30.663690931769,6.93308997531943));
#44022=CARTESIAN_POINT('Ctrl Pts',(56.2156177171251,30.5870116565507,6.92551234873589));
#44023=CARTESIAN_POINT('Ctrl Pts',(56.4211406734027,30.4069353376887,6.90964278370779));
#44024=CARTESIAN_POINT('Ctrl Pts',(56.5174530236151,30.3024734430475,6.90136967346551));
#44025=CARTESIAN_POINT('Ctrl Pts',(56.6127308057256,30.1740776597263,6.89145565248301));
#44026=CARTESIAN_POINT('Ctrl Pts',(56.6233787556746,30.1593103054675,6.89031947132378));
#44027=CARTESIAN_POINT('Ctrl Pts',(56.6392321840964,30.1366768721068,6.88858314369568));
#44028=CARTESIAN_POINT('Ctrl Pts',(56.6445866469688,30.1289159493428,6.887988651114));
#44029=CARTESIAN_POINT('Ctrl Pts',(56.6537866053956,30.1153768855018,6.88695294028633));
#44030=CARTESIAN_POINT('Ctrl Pts',(56.6576573693912,30.1096160491915,6.88651268054141));
#44031=CARTESIAN_POINT('Ctrl Pts',(56.6662601879818,30.0966670459226,6.88552398070469));
#44032=CARTESIAN_POINT('Ctrl Pts',(56.6709759251847,30.0894682543865,6.88497494449933));
#44033=CARTESIAN_POINT('Ctrl Pts',(56.6834341105488,30.070179086908,6.88350530738382));
#44034=CARTESIAN_POINT('Ctrl Pts',(56.6910927470488,30.0580354368958,6.88258164662552));
#44035=CARTESIAN_POINT('Ctrl Pts',(56.7246688569936,30.0035006642109,6.87843977580195));
#44036=CARTESIAN_POINT('Ctrl Pts',(56.7491262761213,29.960235805642,6.87516951345243));
#44037=CARTESIAN_POINT('Ctrl Pts',(56.8481780066025,29.7686489562313,6.86074505841113));
#44038=CARTESIAN_POINT('Ctrl Pts',(56.9057021868245,29.6122640174991,6.84904229574597));
#44039=CARTESIAN_POINT('Ctrl Pts',(56.9543695819128,29.4023884520922,6.83414968234723));
#44040=CARTESIAN_POINT('Ctrl Pts',(56.9637519261193,29.3537738779263,6.83076027603962));
#44041=CARTESIAN_POINT('Ctrl Pts',(56.974106951383,29.2868146491723,6.82621386184849));
#44042=CARTESIAN_POINT('Ctrl Pts',(56.9766495052811,29.2687334788619,6.82499828192145));
#44043=CARTESIAN_POINT('Ctrl Pts',(56.980601837733,29.2375250145556,6.82292378136598));
#44044=CARTESIAN_POINT('Ctrl Pts',(56.9821301835058,29.2244141930124,6.8220594249982));
#44045=CARTESIAN_POINT('Ctrl Pts',(56.9841472007655,29.2054789172412,6.82082230342152));
#44046=CARTESIAN_POINT('Ctrl Pts',(56.9847405551354,29.19966629815,6.82044406323201));
#44047=CARTESIAN_POINT('Ctrl Pts',(56.9857308288667,29.1895244983226,6.81978686603181));
#44048=CARTESIAN_POINT('Ctrl Pts',(56.986139147815,29.1851965095376,6.81950728463812));
#44049=CARTESIAN_POINT('Ctrl Pts',(56.9869721599372,29.1760472153623,6.81891813525641));
#44050=CARTESIAN_POINT('Ctrl Pts',(56.9873934569634,29.1712256838819,6.81860875620718));
#44051=CARTESIAN_POINT('Ctrl Pts',(56.9884835087576,29.1582042416448,6.8177760561605));
#44052=CARTESIAN_POINT('Ctrl Pts',(56.9891190988931,29.1500015421842,6.81725454059352));
#44053=CARTESIAN_POINT('Ctrl Pts',(56.9917820281599,29.112634627375,6.81489166073638));
#44054=CARTESIAN_POINT('Ctrl Pts',(56.9932189540587,29.0834303143754,6.81308055506658));
#44055=CARTESIAN_POINT('Ctrl Pts',(56.9996543405425,28.8466870950551,6.79861136150138));
#44056=CARTESIAN_POINT('Ctrl Pts',(56.9728702123683,28.6395451713328,6.78714507927761));
#44057=CARTESIAN_POINT('Ctrl Pts',(56.9044040008753,28.40536269987,6.77249410984721));
#44058=CARTESIAN_POINT('Ctrl Pts',(56.8932558565437,28.3707701931234,6.77028858205908));
#44059=CARTESIAN_POINT('Ctrl Pts',(56.8725324854121,28.3120145856584,6.76645736062212));
#44060=CARTESIAN_POINT('Ctrl Pts',(56.8634183361255,28.2876982047568,6.76484623770607));
#44061=CARTESIAN_POINT('Ctrl Pts',(56.8498215855671,28.2534709032816,6.76253883412008));
#44062=CARTESIAN_POINT('Ctrl Pts',(56.8457283747993,28.2434074083732,6.76185549228548));
#44063=CARTESIAN_POINT('Ctrl Pts',(56.838528337522,28.2261117241772,6.76067232564928));
#44064=CARTESIAN_POINT('Ctrl Pts',(56.8354605051779,28.2188634931173,6.76017381913831));
#44065=CARTESIAN_POINT('Ctrl Pts',(56.8295024193571,28.2050154915147,6.75921619845525));
#44066=CARTESIAN_POINT('Ctrl Pts',(56.8266191429162,28.1984128396296,6.75875732664263));
#44067=CARTESIAN_POINT('Ctrl Pts',(56.8197638112604,28.1829433120279,6.75767677880472));
#44068=CARTESIAN_POINT('Ctrl Pts',(56.8157626454658,28.1740896114181,6.75705412016706));
#44069=CARTESIAN_POINT('Ctrl Pts',(56.8017069252029,28.1435832526029,6.75489380837529));
#44070=CARTESIAN_POINT('Ctrl Pts',(56.7913287749436,28.1220827897258,6.75334515240792));
#44071=CARTESIAN_POINT('Ctrl Pts',(56.7133041106098,27.9675851788973,6.74202157441482));
#44072=CARTESIAN_POINT('Ctrl Pts',(56.6313208987502,27.8423870618857,6.7317305961901));
#44073=CARTESIAN_POINT('Ctrl Pts',(56.4809338588952,27.6608359609217,6.71530008681886));
#44074=CARTESIAN_POINT('Ctrl Pts',(56.4214103009037,27.5978160551205,6.70925951483155));
#44075=CARTESIAN_POINT('Ctrl Pts',(56.3390668555281,27.5212863780906,6.70163879669598));
#44076=CARTESIAN_POINT('Ctrl Pts',(56.3198166237046,27.5040794709588,6.69990486726887));
#44077=CARTESIAN_POINT('Ctrl Pts',(56.2872115889623,27.4760548288016,6.69705347394267));
#44078=CARTESIAN_POINT('Ctrl Pts',(56.2740417133189,27.4650275833835,6.69592406751638));
#44079=CARTESIAN_POINT('Ctrl Pts',(56.2557003702374,27.4500689450035,6.69438353311118));
#44080=CARTESIAN_POINT('Ctrl Pts',(56.2506501316,27.4459910083239,6.69396266981006));
#44081=CARTESIAN_POINT('Ctrl Pts',(56.2420955459322,27.4391521155836,6.69325547774728));
#44082=CARTESIAN_POINT('Ctrl Pts',(56.2386017082338,27.4363781553091,6.69296824014254));
#44083=CARTESIAN_POINT('Ctrl Pts',(56.2319195618294,27.4311092629728,6.69242195769294));
#44084=CARTESIAN_POINT('Ctrl Pts',(56.2287329323647,27.4286122906235,6.69216276346233));
#44085=CARTESIAN_POINT('Ctrl Pts',(56.2211388849498,27.4226989881247,6.69154815191224));
#44086=CARTESIAN_POINT('Ctrl Pts',(56.2167246711969,27.4192913821079,6.69119334179756));
#44087=CARTESIAN_POINT('Ctrl Pts',(56.2010705451695,27.4073114160271,6.6899434699723));
#44088=CARTESIAN_POINT('Ctrl Pts',(56.1897535536857,27.3988398306306,6.68905509160309));
#44089=CARTESIAN_POINT('Ctrl Pts',(56.059888633158,27.3037637795336,6.67902040280405));
#44090=CARTESIAN_POINT('Ctrl Pts',(55.9321994263362,27.2303676634608,6.67063153464379));
#44091=CARTESIAN_POINT('Ctrl Pts',(55.6807491561,27.1206759602873,6.65467690049963));
#44092=CARTESIAN_POINT('Ctrl Pts',(55.5593044436243,27.0810287404708,6.64718276321157));
#44093=CARTESIAN_POINT('Ctrl Pts',(55.4168149917384,27.0491958472848,6.63813325306116));
#44094=CARTESIAN_POINT('Ctrl Pts',(55.398658487695,27.0454046572768,6.63697605028504));
#44095=CARTESIAN_POINT('Ctrl Pts',(55.3711278638344,27.0400556393345,6.63521411288293));
#44096=CARTESIAN_POINT('Ctrl Pts',(55.3617908190403,27.0383106294631,6.63461529348404));
#44097=CARTESIAN_POINT('Ctrl Pts',(55.3449491322474,27.0352873981992,6.63353276276496));
#44098=CARTESIAN_POINT('Ctrl Pts',(55.3374489177741,27.0339853162307,6.63304981430279));
#44099=CARTESIAN_POINT('Ctrl Pts',(55.3212791127767,27.0312733957904,6.63200669104536));
#44100=CARTESIAN_POINT('Ctrl Pts',(55.3126073227887,27.0298778291378,6.63144607774987));
#44101=CARTESIAN_POINT('Ctrl Pts',(55.2893172418508,27.0262873549437,6.62993709247676));
#44102=CARTESIAN_POINT('Ctrl Pts',(55.2746835239841,27.0241976278128,6.62898544564365));
#44103=CARTESIAN_POINT('Ctrl Pts',(55.2047553091895,27.0150035929815,6.62442027344402));
#44104=CARTESIAN_POINT('Ctrl Pts',(55.149206999144,27.0100573528435,6.62074028525787));
#44105=CARTESIAN_POINT('Ctrl Pts',(54.9146910730861,26.99904939898,6.60497061139637));
#44106=CARTESIAN_POINT('Ctrl Pts',(54.7355440877852,27.0147725812098,6.5922589316747));
#44107=CARTESIAN_POINT('Ctrl Pts',(54.5258768057124,27.0620817668024,6.57753820012826));
#44108=CARTESIAN_POINT('Ctrl Pts',(54.4910277200637,27.0709413159193,6.57510076611379));
#44109=CARTESIAN_POINT('Ctrl Pts',(54.4353829054125,27.0867007949842,6.57124283574848));
#44110=CARTESIAN_POINT('Ctrl Pts',(54.4144290665264,27.0930094158185,6.56979799425634));
#44111=CARTESIAN_POINT('Ctrl Pts',(54.3867985654778,27.1018265969667,6.56790710563729));
#44112=CARTESIAN_POINT('Ctrl Pts',(54.3800263772893,27.1040276958445,6.56744480404991));
#44113=CARTESIAN_POINT('Ctrl Pts',(54.3689039336888,27.1077086827692,6.56668759855882));
#44114=CARTESIAN_POINT('Ctrl Pts',(54.3645468159209,27.1091673987202,6.56639149360175));
#44115=CARTESIAN_POINT('Ctrl Pts',(54.3560163822983,27.1120561122691,6.56581285577817));
#44116=CARTESIAN_POINT('Ctrl Pts',(54.3518427176803,27.1134849162966,6.56553025937061));
#44117=CARTESIAN_POINT('Ctrl Pts',(54.3415653843125,27.1170413705552,6.56483557374667));
#44118=CARTESIAN_POINT('Ctrl Pts',(54.3354671844149,27.1191848886424,6.56442440636526));
#44119=CARTESIAN_POINT('Ctrl Pts',(54.314496113848,27.1266709514708,6.56301366317416));
#44120=CARTESIAN_POINT('Ctrl Pts',(54.2996759327407,27.1321607297954,6.56202228923762));
#44121=CARTESIAN_POINT('Ctrl Pts',(54.1720451895023,27.1811711584973,6.55352039242769));
#44122=CARTESIAN_POINT('Ctrl Pts',(54.063327025177,27.2346957053981,6.54651190223482));
#44123=CARTESIAN_POINT('Ctrl Pts',(53.8708239805844,27.3522932707182,6.53341235394136));
#44124=CARTESIAN_POINT('Ctrl Pts',(53.7859665094858,27.413779142495,6.52734426949235));
#44125=CARTESIAN_POINT('Ctrl Pts',(53.6791750329981,27.5047670868791,6.51891364981743));
#44126=CARTESIAN_POINT('Ctrl Pts',(53.6526488358274,27.5286249014816,6.51674734085933));
#44127=CARTESIAN_POINT('Ctrl Pts',(53.6082091154794,27.5708040411168,6.51297830404808));
#44128=CARTESIAN_POINT('Ctrl Pts',(53.5899823112836,27.5887831562152,6.51138950481195));
#44129=CARTESIAN_POINT('Ctrl Pts',(53.5645635303534,27.6148406542357,6.5091086013084));
#44130=CARTESIAN_POINT('Ctrl Pts',(53.5570829504477,27.6226348877839,6.50842902766213));
#44131=CARTESIAN_POINT('Ctrl Pts',(53.5442698853305,27.6362041303912,6.50725031140425));
#44132=CARTESIAN_POINT('Ctrl Pts',(53.5389074911014,27.6419506568999,6.50675246029609));
#44133=CARTESIAN_POINT('Ctrl Pts',(53.5286861607864,27.6530348012645,6.50579463984382));
#44134=CARTESIAN_POINT('Ctrl Pts',(53.5238219501723,27.6583674038567,6.50533490447229));
#44135=CARTESIAN_POINT('Ctrl Pts',(53.5124429684654,27.6709789076192,6.50425008333531));
#44136=CARTESIAN_POINT('Ctrl Pts',(53.5059525585768,27.6782794458543,6.50362399551756));
#44137=CARTESIAN_POINT('Ctrl Pts',(53.4835241172738,27.7038836853224,6.50143452880689));
#44138=CARTESIAN_POINT('Ctrl Pts',(53.467867241644,27.7224297556653,6.49985972978617));
#44139=CARTESIAN_POINT('Ctrl Pts',(53.3650790563348,27.848793239632,6.48919891931733));
#44140=CARTESIAN_POINT('Ctrl Pts',(53.289067911369,27.965136695496,6.47967469045432));
#44141=CARTESIAN_POINT('Ctrl Pts',(53.1690536038691,28.1987210393171,6.46138297595814));
#44142=CARTESIAN_POINT('Ctrl Pts',(53.1227776159862,28.3141034162764,6.45269090205674));
#44143=CARTESIAN_POINT('Ctrl Pts',(53.083052374847,28.4481067578686,6.44343585836962));
#44144=CARTESIAN_POINT('Ctrl Pts',(53.0787653008339,28.4632210738082,6.44240385757877));
#44145=CARTESIAN_POINT('Ctrl Pts',(53.0729709180718,28.4846088291476,6.44096171638683));
#44146=CARTESIAN_POINT('Ctrl Pts',(53.0713149170892,28.4908408939069,6.44054366647915));
#44147=CARTESIAN_POINT('Ctrl Pts',(53.0685777118761,28.5013468735339,6.43984269259501));
#44148=CARTESIAN_POINT('Ctrl Pts',(53.0674804124074,28.5056165046767,6.43955886279768));
#44149=CARTESIAN_POINT('Ctrl Pts',(53.0652672786344,28.5143478504738,6.43898061770297));
#44150=CARTESIAN_POINT('Ctrl Pts',(53.0641527067173,28.5188098384322,6.43868627486099));
#44151=CARTESIAN_POINT('Ctrl Pts',(53.061347076103,28.5302092073647,6.43793715635705));
#44152=CARTESIAN_POINT('Ctrl Pts',(53.0596777996614,28.537151957181,6.43748360727462));
#44153=CARTESIAN_POINT('Ctrl Pts',(53.053007619738,28.5655645201198,6.43563795798104));
#44154=CARTESIAN_POINT('Ctrl Pts',(53.0483252804419,28.5871084901867,6.43426283870236));
#44155=CARTESIAN_POINT('Ctrl Pts',(53.0368751957249,28.6443481625649,6.43066292646322));
#44156=CARTESIAN_POINT('Ctrl Pts',(53.0307235389978,28.680159792689,6.42846540700149));
#44157=CARTESIAN_POINT('Ctrl Pts',(52.9991521478969,28.8997467933963,6.41521590284308));
#44158=CARTESIAN_POINT('Ctrl Pts',(52.9984936833413,29.0861583468699,6.40483632778336));
#44159=CARTESIAN_POINT('Ctrl Pts',(53.0297639748385,29.315068056609,6.39092058868415));
#44160=CARTESIAN_POINT('Ctrl Pts',(53.0374625283022,29.359921990805,6.38814216583772));
#44161=CARTESIAN_POINT('Ctrl Pts',(53.046686998162,29.404469874466,6.38531629657044));
#44162=CARTESIAN_POINT('Ctrl Pts',(53.0466869743493,29.404469759467,6.22571516850575));
#44163=CARTESIAN_POINT('Ctrl Pts',(53.0336901222297,29.3417038296453,6.22943746026231));
#44164=CARTESIAN_POINT('Ctrl Pts',(53.0237206966933,29.2783219142394,6.23315573173925));
#44165=CARTESIAN_POINT('Ctrl Pts',(53.0091361594068,29.1435060238327,6.24113115979555));
#44166=CARTESIAN_POINT('Ctrl Pts',(53.0052742093992,29.072113868334,6.24539418151947));
#44167=CARTESIAN_POINT('Ctrl Pts',(53.0052401907627,28.9712533874548,6.25157249376068));
#44168=CARTESIAN_POINT('Ctrl Pts',(53.0058811019398,28.9418386165462,6.25339263738129));
#44169=CARTESIAN_POINT('Ctrl Pts',(53.0076881732792,28.9007058025391,6.25596817345258));
#44170=CARTESIAN_POINT('Ctrl Pts',(53.0083079180278,28.888966699742,6.25670666770735));
#44171=CARTESIAN_POINT('Ctrl Pts',(53.0094768959908,28.8700087014318,6.2579051428035));
#44172=CARTESIAN_POINT('Ctrl Pts',(53.0099617385099,28.8627860033684,6.25836311565912));
#44173=CARTESIAN_POINT('Ctrl Pts',(53.0110536867358,28.8477448833479,6.25931976776433));
#44174=CARTESIAN_POINT('Ctrl Pts',(53.0116676032664,28.8399270952741,6.25981865120777));
#44175=CARTESIAN_POINT('Ctrl Pts',(53.0132285217316,28.821446816068,6.26100195342078));
#44176=CARTESIAN_POINT('Ctrl Pts',(53.0142152779156,28.8107880116351,6.26168759915631));
#44177=CARTESIAN_POINT('Ctrl Pts',(53.0177945044293,28.7752448430209,6.26398479840446));
#44178=CARTESIAN_POINT('Ctrl Pts',(53.0207692523406,28.7504022015754,6.26560817886421));
#44179=CARTESIAN_POINT('Ctrl Pts',(53.0289725192607,28.691330454617,6.26951243235895));
#44180=CARTESIAN_POINT('Ctrl Pts',(53.0346264314697,28.6571695517108,6.2718058569667));
#44181=CARTESIAN_POINT('Ctrl Pts',(53.0752693345346,28.4458973920729,6.28621316955182));
#44182=CARTESIAN_POINT('Ctrl Pts',(53.133280930704,28.2740800025001,6.29901819537356));
#44183=CARTESIAN_POINT('Ctrl Pts',(53.2243692819676,28.090741645815,6.31306635217036));
#44184=CARTESIAN_POINT('Ctrl Pts',(53.2355504837523,28.0692297870817,6.31471932230543));
#44185=CARTESIAN_POINT('Ctrl Pts',(53.2634356470972,28.0178899494942,6.3186671259085));
#44186=CARTESIAN_POINT('Ctrl Pts',(53.2805204130662,27.9882756386985,6.32094673851372));
#44187=CARTESIAN_POINT('Ctrl Pts',(53.3028412190259,27.9517856055767,6.32374532525463));
#44188=CARTESIAN_POINT('Ctrl Pts',(53.3073707900135,27.9444869927895,6.32430455731323));
#44189=CARTESIAN_POINT('Ctrl Pts',(53.3145953143114,27.9330120400183,6.32518266545636));
#44190=CARTESIAN_POINT('Ctrl Pts',(53.3172589089077,27.9288162235464,6.32550350674239));
#44191=CARTESIAN_POINT('Ctrl Pts',(53.3220330038915,27.9213576025441,6.32607335621864));
#44192=CARTESIAN_POINT('Ctrl Pts',(53.3241373443133,27.9180910291148,6.32632275351748));
#44193=CARTESIAN_POINT('Ctrl Pts',(53.3291782237629,27.9103160540121,6.32691596757327));
#44194=CARTESIAN_POINT('Ctrl Pts',(53.3321234678105,27.9058133682551,6.32725920378033));
#44195=CARTESIAN_POINT('Ctrl Pts',(53.3410177735145,27.8923351210008,6.32828588559477));
#44196=CARTESIAN_POINT('Ctrl Pts',(53.3470214437224,27.8833955863511,6.32896582955401));
#44197=CARTESIAN_POINT('Ctrl Pts',(53.3610311003458,27.8628956838051,6.3305238017073));
#44198=CARTESIAN_POINT('Ctrl Pts',(53.3690876061914,27.8513703522526,6.33139878101936));
#44199=CARTESIAN_POINT('Ctrl Pts',(53.3968322141058,27.8125604845479,6.33434548800326));
#44200=CARTESIAN_POINT('Ctrl Pts',(53.4170893469668,27.7856879837985,6.33638644313321));
#44201=CARTESIAN_POINT('Ctrl Pts',(53.5302674964805,27.6431975546764,6.34728779310529));
#44202=CARTESIAN_POINT('Ctrl Pts',(53.6351869745191,27.5377012268036,6.35568207480793));
#44203=CARTESIAN_POINT('Ctrl Pts',(53.8183510966638,27.3905802756177,6.36952581144618));
#44204=CARTESIAN_POINT('Ctrl Pts',(53.8893146491604,27.3408130549455,6.37472402115603));
#44205=CARTESIAN_POINT('Ctrl Pts',(53.9762306293578,27.2879387888947,6.38104279747824));
#44206=CARTESIAN_POINT('Ctrl Pts',(53.9892693566838,27.2802090645124,6.38198933575541));
#44207=CARTESIAN_POINT('Ctrl Pts',(54.0107709902327,27.2677912671264,6.3835486516898));
#44208=CARTESIAN_POINT('Ctrl Pts',(54.0191823013398,27.2630147482695,6.38415825476024));
#44209=CARTESIAN_POINT('Ctrl Pts',(54.034349284701,27.2545471886746,6.38525692870694));
#44210=CARTESIAN_POINT('Ctrl Pts',(54.0410922535662,27.2508336981141,6.38574518916298));
#44211=CARTESIAN_POINT('Ctrl Pts',(54.0554930300929,27.2430111922066,6.38678763444405));
#44212=CARTESIAN_POINT('Ctrl Pts',(54.0631565136887,27.2389130160173,6.38734218921769));
#44213=CARTESIAN_POINT('Ctrl Pts',(54.0838904190425,27.2279988461721,6.388842185226));
#44214=CARTESIAN_POINT('Ctrl Pts',(54.0970098150319,27.2212775483199,6.38979091117769));
#44215=CARTESIAN_POINT('Ctrl Pts',(54.165042768132,27.1873697160483,6.39470965361494));
#44216=CARTESIAN_POINT('Ctrl Pts',(54.2211081346196,27.1625810875899,6.39876116265078));
#44217=CARTESIAN_POINT('Ctrl Pts',(54.3448144893781,27.114565736296,6.40770094927617));
#44218=CARTESIAN_POINT('Ctrl Pts',(54.412743493521,27.0923158754541,6.41261078646231));
#44219=CARTESIAN_POINT('Ctrl Pts',(54.6180500092199,27.0370749243969,6.42736632752475));
#44220=CARTESIAN_POINT('Ctrl Pts',(54.757900397643,27.0149678441298,6.43733362084736));
#44221=CARTESIAN_POINT('Ctrl Pts',(54.9181090272729,27.0068390296775,6.44800528327447));
#44222=CARTESIAN_POINT('Ctrl Pts',(54.9373134339272,27.0061426217843,6.44927185161378));
#44223=CARTESIAN_POINT('Ctrl Pts',(54.9635286872229,27.0055711417654,6.45098088704421));
#44224=CARTESIAN_POINT('Ctrl Pts',(54.9705325264032,27.0054553655684,6.451435545384));
#44225=CARTESIAN_POINT('Ctrl Pts',(54.9816518348254,27.005330142174,6.45215413122779));
#44226=CARTESIAN_POINT('Ctrl Pts',(54.9857668937531,27.0052965342396,6.45241936480779));
#44227=CARTESIAN_POINT('Ctrl Pts',(54.9942873414668,27.0052533155991,6.45296705008526));
#44228=CARTESIAN_POINT('Ctrl Pts',(54.9986926798279,27.005245563818,6.4532493870948));
#44229=CARTESIAN_POINT('Ctrl Pts',(55.0092967199724,27.0052620329449,6.4539270605146));
#44230=CARTESIAN_POINT('Ctrl Pts',(55.0154954191258,27.0053005538056,6.45432161041427));
#44231=CARTESIAN_POINT('Ctrl Pts',(55.0369815114805,27.0055342399769,6.45568400494136));
#44232=CARTESIAN_POINT('Ctrl Pts',(55.052267216231,27.0058762647386,6.4566441109457));
#44233=CARTESIAN_POINT('Ctrl Pts',(55.1444800393686,27.0090006500764,6.46238903726044));
#44234=CARTESIAN_POINT('Ctrl Pts',(55.221205637902,27.0160585720634,6.46697268475538));
#44235=CARTESIAN_POINT('Ctrl Pts',(55.3792091456557,27.0398767729622,6.47634488833364));
#44236=CARTESIAN_POINT('Ctrl Pts',(55.4602327391628,27.0573037005231,6.48111504270365));
#44237=CARTESIAN_POINT('Ctrl Pts',(55.6505259559454,27.110809784941,6.49264468816447));
#44238=CARTESIAN_POINT('Ctrl Pts',(55.7582044071864,27.1513938703551,6.49944658264577));
#44239=CARTESIAN_POINT('Ctrl Pts',(55.8760362879693,27.2078399365926,6.50755440069076));
#44240=CARTESIAN_POINT('Ctrl Pts',(55.8902056804436,27.2148358352977,6.50854053970448));
#44241=CARTESIAN_POINT('Ctrl Pts',(55.9130852470149,27.2264723691894,6.51015186086307));
#44242=CARTESIAN_POINT('Ctrl Pts',(55.9218469023253,27.2310106815912,6.51077349420613));
#44243=CARTESIAN_POINT('Ctrl Pts',(55.9374011886622,27.2392143392031,6.51188542827417));
#44244=CARTESIAN_POINT('Ctrl Pts',(55.9442069415694,27.2428544794047,6.51237483718683));
#44245=CARTESIAN_POINT('Ctrl Pts',(55.9585281550571,27.2506215815933,6.51341088182645));
#44246=CARTESIAN_POINT('Ctrl Pts',(55.9660384582823,27.2547576763717,6.51395783337311));
#44247=CARTESIAN_POINT('Ctrl Pts',(55.9859260457451,27.2658779259029,6.51541599451997));
#44248=CARTESIAN_POINT('Ctrl Pts',(55.9982555728153,27.2729460547913,6.51633018055453));
#44249=CARTESIAN_POINT('Ctrl Pts',(56.0574299104708,27.3077141971115,6.52076804559156));
#44250=CARTESIAN_POINT('Ctrl Pts',(56.103199555955,27.3371894108576,6.52435528352325));
#44251=CARTESIAN_POINT('Ctrl Pts',(56.3114313654878,27.4836729576747,6.54142850658865));
#44252=CARTESIAN_POINT('Ctrl Pts',(56.4568553056925,27.6228105563532,6.55574145577927));
#44253=CARTESIAN_POINT('Ctrl Pts',(56.6012530662405,27.8099044842397,6.57173883429098));
#44254=CARTESIAN_POINT('Ctrl Pts',(56.6225937968314,27.8391690579339,6.57415711984861));
#44255=CARTESIAN_POINT('Ctrl Pts',(56.6480926761642,27.8762140847911,6.57710046516448));
#44256=CARTESIAN_POINT('Ctrl Pts',(56.6530105022833,27.8834604626198,6.57767076282761));
#44257=CARTESIAN_POINT('Ctrl Pts',(56.6606657595944,27.8949018672549,6.5785623895592));
#44258=CARTESIAN_POINT('Ctrl Pts',(56.6634353148235,27.8990751148173,6.57888578207171));
#44259=CARTESIAN_POINT('Ctrl Pts',(56.6685379694145,27.9068271604192,6.57948305767277));
#44260=CARTESIAN_POINT('Ctrl Pts',(56.6708752733194,27.9104029946448,6.57975721022623));
#44261=CARTESIAN_POINT('Ctrl Pts',(56.6762128051163,27.9186264316481,6.58038461014332));
#44262=CARTESIAN_POINT('Ctrl Pts',(56.6792051985231,27.923279021575,6.58073734038845));
#44263=CARTESIAN_POINT('Ctrl Pts',(56.6883766432639,27.9376700662044,6.58182169911222));
#44264=CARTESIAN_POINT('Ctrl Pts',(56.6944907501909,27.947449910898,6.58254921859051));
#44265=CARTESIAN_POINT('Ctrl Pts',(56.7519559624721,28.0411672745306,6.58943732700102));
#44266=CARTESIAN_POINT('Ctrl Pts',(56.797121982662,28.1287550716496,6.59524408254966));
#44267=CARTESIAN_POINT('Ctrl Pts',(56.9040063245006,28.3800793837888,6.61117384762291));
#44268=CARTESIAN_POINT('Ctrl Pts',(56.9509534610614,28.5490931830108,6.62115320792036));
#44269=CARTESIAN_POINT('Ctrl Pts',(56.978373532884,28.7439627197549,6.63330215089091));
#44270=CARTESIAN_POINT('Ctrl Pts',(56.9810911758399,28.7659174992277,6.6346784437214));
#44271=CARTESIAN_POINT('Ctrl Pts',(56.984514997263,28.7979370559507,6.63669854124829));
#44272=CARTESIAN_POINT('Ctrl Pts',(56.9855109046531,28.8079696657671,6.63733332205234));
#44273=CARTESIAN_POINT('Ctrl Pts',(56.9871395849604,28.8257467261469,6.63846152450768));
#44274=CARTESIAN_POINT('Ctrl Pts',(56.9878032466555,28.8334881884625,6.63895397332591));
#44275=CARTESIAN_POINT('Ctrl Pts',(56.9890889809182,28.8495909413031,6.6399807647622));
#44276=CARTESIAN_POINT('Ctrl Pts',(56.9897035980167,28.8579526576323,6.64051532953499));
#44277=CARTESIAN_POINT('Ctrl Pts',(56.9911601016814,28.8796371531007,6.64190531428085));
#44278=CARTESIAN_POINT('Ctrl Pts',(56.991920985548,28.8929647791707,6.64276323400183));
#44279=CARTESIAN_POINT('Ctrl Pts',(56.9946643199461,28.9513015365321,6.64653491343137));
#44280=CARTESIAN_POINT('Ctrl Pts',(56.9952552468688,28.9963598002743,6.64949133035863));
#44281=CARTESIAN_POINT('Ctrl Pts',(56.9910417829105,29.1993473372872,6.66301427174421));
#44282=CARTESIAN_POINT('Ctrl Pts',(56.9690099202627,29.3563315039657,6.6740911748947));
#44283=CARTESIAN_POINT('Ctrl Pts',(56.9067302801766,29.5923028271303,6.69103666399445));
#44284=CARTESIAN_POINT('Ctrl Pts',(56.8793837843771,29.674064587153,6.69695138826517));
#44285=CARTESIAN_POINT('Ctrl Pts',(56.8428254438862,29.763632426481,6.70330529757384));
#44286=CARTESIAN_POINT('Ctrl Pts',(56.8387381881853,29.7734222562692,6.70399799250553));
#44287=CARTESIAN_POINT('Ctrl Pts',(56.8324454655494,29.7881627621189,6.70503776256106));
#44288=CARTESIAN_POINT('Ctrl Pts',(56.8302976830356,29.7931376406076,6.7053881243559));
#44289=CARTESIAN_POINT('Ctrl Pts',(56.8264079499274,29.8020474297157,6.70601452433708));
#44290=CARTESIAN_POINT('Ctrl Pts',(56.8246735213666,29.8059854965059,6.70629100226585));
#44291=CARTESIAN_POINT('Ctrl Pts',(56.8208517407689,29.8145873846591,6.70689405891063));
#44292=CARTESIAN_POINT('Ctrl Pts',(56.8187592114624,29.8192488030073,6.70722031972455));
#44293=CARTESIAN_POINT('Ctrl Pts',(56.8127397660176,29.8325212742388,6.70814788497766));
#44294=CARTESIAN_POINT('Ctrl Pts',(56.8087693841898,29.8411126289198,6.70874661917851));
#44295=CARTESIAN_POINT('Ctrl Pts',(56.7815584908717,29.8989094291282,6.71276524014978));
#44296=CARTESIAN_POINT('Ctrl Pts',(56.7563717584758,29.9471790880372,6.71607614452245));
#44297=CARTESIAN_POINT('Ctrl Pts',(56.6344233711701,30.1592526604831,6.73068278461686));
#44298=CARTESIAN_POINT('Ctrl Pts',(56.5165120352766,30.3097350899645,6.74131215017533));
#44299=CARTESIAN_POINT('Ctrl Pts',(56.3461242070602,30.4727715520555,6.75556125943586));
#44300=CARTESIAN_POINT('Ctrl Pts',(56.3121122501544,30.5031524818635,6.75835542897464));
#44301=CARTESIAN_POINT('Ctrl Pts',(56.2663969944422,30.5412527437503,6.7620658617992));
#44302=CARTESIAN_POINT('Ctrl Pts',(56.2556099790925,30.55005320315,6.76293820456724));
#44303=CARTESIAN_POINT('Ctrl Pts',(56.2380819762654,30.564050192361,6.76435109078169));
#44304=CARTESIAN_POINT('Ctrl Pts',(56.2313981797162,30.5693178465673,6.76488879553809));
#44305=CARTESIAN_POINT('Ctrl Pts',(56.2185771156468,30.5792900848745,6.76591833771115));
#44306=CARTESIAN_POINT('Ctrl Pts',(56.2124457847171,30.5840020755474,6.76640987093001));
#44307=CARTESIAN_POINT('Ctrl Pts',(56.1983330162123,30.5947179352342,6.76753947817042));
#44308=CARTESIAN_POINT('Ctrl Pts',(56.1903336261087,30.6006977114044,6.76817847355913));
#44309=CARTESIAN_POINT('Ctrl Pts',(56.1653516279314,30.6190816572252,6.77017029180876));
#44310=CARTESIAN_POINT('Ctrl Pts',(56.1482179736392,30.6312771863464,6.7715310438189));
#44311=CARTESIAN_POINT('Ctrl Pts',(56.0640636579724,30.6891945196858,6.77819131024342));
#44312=CARTESIAN_POINT('Ctrl Pts',(55.9944967452248,30.7310640950781,6.78363114184655));
#44313=CARTESIAN_POINT('Ctrl Pts',(55.801591535736,30.831693386752,6.7985191654965));
#44314=CARTESIAN_POINT('Ctrl Pts',(55.6744542906723,30.8822214053855,6.80815217689868));
#44315=CARTESIAN_POINT('Ctrl Pts',(55.5320360987636,30.9225240756106,6.8183257263553));
#44316=CARTESIAN_POINT('Ctrl Pts',(55.5208841018493,30.925575496297,6.81911816925973));
#44317=CARTESIAN_POINT('Ctrl Pts',(55.4628424304527,30.9409157780111,6.8232188923695));
#44318=CARTESIAN_POINT('Ctrl Pts',(55.415538488929,30.9515905786893,6.82648150993546));
#44319=CARTESIAN_POINT('Ctrl Pts',(55.3593291942646,30.9621381031396,6.83023035843789));
#44320=CARTESIAN_POINT('Ctrl Pts',(55.3507591758218,30.963688216794,6.8307984460385));
#44321=CARTESIAN_POINT('Ctrl Pts',(55.3367971022441,30.9661193042327,6.83171799691199));
#44322=CARTESIAN_POINT('Ctrl Pts',(55.3314112030415,30.9670343217051,6.83207127512843));
#44323=CARTESIAN_POINT('Ctrl Pts',(55.3217735677498,30.9686309644259,6.8327007819814));
#44324=CARTESIAN_POINT('Ctrl Pts',(55.3175233312051,30.9693209586752,6.8329774698283));
#44325=CARTESIAN_POINT('Ctrl Pts',(55.3082589982,30.9707941814143,6.83357854502291));
#44326=CARTESIAN_POINT('Ctrl Pts',(55.3032441423801,30.971572039504,6.83390263036447));
#44327=CARTESIAN_POINT('Ctrl Pts',(55.2890288955388,30.9737214561414,6.83481780275453));
#44328=CARTESIAN_POINT('Ctrl Pts',(55.2798216588205,30.9750478313412,6.83540642634461));
#44329=CARTESIAN_POINT('Ctrl Pts',(55.2203339508917,30.9831931572662,6.83918479795891));
#44330=CARTESIAN_POINT('Ctrl Pts',(55.1698134780151,30.9881565565629,6.84227996578166));
#44331=CARTESIAN_POINT('Ctrl Pts',(54.966750373323,31.0003080106511,6.85446126597659));
#44332=CARTESIAN_POINT('Ctrl Pts',(54.8137969434966,30.9919016364594,6.86308890425721));
#44333=CARTESIAN_POINT('Ctrl Pts',(54.5824862533878,30.952288621832,6.87694815961842));
#44334=CARTESIAN_POINT('Ctrl Pts',(54.5026194798947,30.9334836030646,6.8818805200862));
#44335=CARTESIAN_POINT('Ctrl Pts',(54.4097991862446,30.9054959928171,6.88790341840874));
#44336=CARTESIAN_POINT('Ctrl Pts',(54.3955059477993,30.9010099686771,6.8888390728381));
#44337=CARTESIAN_POINT('Ctrl Pts',(54.3721205180139,30.8933798984495,6.89038405413735));
#44338=CARTESIAN_POINT('Ctrl Pts',(54.3629979777129,30.8903302627229,6.8909903056809));
#44339=CARTESIAN_POINT('Ctrl Pts',(54.3466200413766,30.8847231544339,6.89208530797283));
#44340=CARTESIAN_POINT('Ctrl Pts',(54.3393566644848,30.8821894484184,6.89257327074057));
#44341=CARTESIAN_POINT('Ctrl Pts',(54.323886810592,30.8766924743355,6.89361765400438));
#44342=CARTESIAN_POINT('Ctrl Pts',(54.3156847790155,30.8737172578816,6.8941744603741));
#44343=CARTESIAN_POINT('Ctrl Pts',(54.2941746965986,30.8657545872149,6.89564295050602));
#44344=CARTESIAN_POINT('Ctrl Pts',(54.280900158583,30.8606786233721,6.89655754911394));
#44345=CARTESIAN_POINT('Ctrl Pts',(54.2177373899727,30.8357493634029,6.90095025480894));
#44346=CARTESIAN_POINT('Ctrl Pts',(54.168614092384,30.8140306193279,6.90449006303857));
#44347=CARTESIAN_POINT('Ctrl Pts',(54.0255567801739,30.7437492284303,6.91517802983858));
#44348=CARTESIAN_POINT('Ctrl Pts',(53.9345484111306,30.689677269297,6.92249227999612));
#44349=CARTESIAN_POINT('Ctrl Pts',(53.7507624052646,30.5597092602233,6.93817652536704));
#44350=CARTESIAN_POINT('Ctrl Pts',(53.6596427874565,30.4821387353655,6.94653024156676));
#44351=CARTESIAN_POINT('Ctrl Pts',(53.5648989389195,30.3855554809716,6.95549097517508));
#44352=CARTESIAN_POINT('Ctrl Pts',(53.5539287606786,30.3741022723118,6.95653290946483));
#44353=CARTESIAN_POINT('Ctrl Pts',(53.5386745821129,30.357791399461,6.95798644782903));
#44354=CARTESIAN_POINT('Ctrl Pts',(53.5342761897338,30.3530421930721,6.95840612576579));
#44355=CARTESIAN_POINT('Ctrl Pts',(53.5269180424435,30.345019176266,6.95910903860495));
#44356=CARTESIAN_POINT('Ctrl Pts',(53.5239459195698,30.3417568300958,6.95939319040541));
#44357=CARTESIAN_POINT('Ctrl Pts',(53.5179032259121,30.3350796990789,6.95997132768147));
#44358=CARTESIAN_POINT('Ctrl Pts',(53.5148335827682,30.3316641336367,6.96026524503036));
#44359=CARTESIAN_POINT('Ctrl Pts',(53.5070420201277,30.3229340769405,6.96101196056232));
#44360=CARTESIAN_POINT('Ctrl Pts',(53.5023366178853,30.3176048342012,6.96146354764638));
#44361=CARTESIAN_POINT('Ctrl Pts',(53.4853541207843,30.2981622885126,6.96309621503646));
#44362=CARTESIAN_POINT('Ctrl Pts',(53.4732467744923,30.2839011309568,6.96426560881298));
#44363=CARTESIAN_POINT('Ctrl Pts',(53.4099056700461,30.2071287384328,6.97042580200009));
#44364=CARTESIAN_POINT('Ctrl Pts',(53.3623007487888,30.1417108707432,6.97520832855291));
#44365=CARTESIAN_POINT('Ctrl Pts',(53.2740924655199,30.0035780495066,6.98478744549072));
#44366=CARTESIAN_POINT('Ctrl Pts',(53.2338075213227,29.9308544494379,6.98957257553851));
#44367=CARTESIAN_POINT('Ctrl Pts',(53.1529101035594,29.7605367969924,7.00060035072053));
#44368=CARTESIAN_POINT('Ctrl Pts',(53.1152839154119,29.6618143877731,7.00687543281817));
#44369=CARTESIAN_POINT('Ctrl Pts',(53.0812290330443,29.5455199865914,7.01439622596903));
#44370=CARTESIAN_POINT('Ctrl Pts',(53.0769947523479,29.5304006740588,7.01537614293193));
#44371=CARTESIAN_POINT('Ctrl Pts',(53.0703986791068,29.5057302329335,7.01697929839781));
#44372=CARTESIAN_POINT('Ctrl Pts',(53.0679282400433,29.4962086606766,7.01759904807972));
#44373=CARTESIAN_POINT('Ctrl Pts',(53.0636461863744,29.4791878403923,7.01870888437768));
#44374=CARTESIAN_POINT('Ctrl Pts',(53.0618074495076,29.4716955717669,7.01919809191215));
#44375=CARTESIAN_POINT('Ctrl Pts',(53.0580130530898,29.4558377625538,7.02023504060823));
#44376=CARTESIAN_POINT('Ctrl Pts',(53.0560678880824,29.4474698964312,7.02078310567221));
#44377=CARTESIAN_POINT('Ctrl Pts',(53.0522213635964,29.4304240534228,7.02190144655977));
#44378=CARTESIAN_POINT('Ctrl Pts',(53.0503238028868,29.4217454260556,7.02247182977963));
#44379=CARTESIAN_POINT('Ctrl Pts',(53.0478789049589,29.4101942714901,7.02323238708284));
#44380=CARTESIAN_POINT('Ctrl Pts',(53.047279802351,29.4073327134691,7.02342091185398));
#44381=CARTESIAN_POINT('Ctrl Pts',(53.0466869980042,29.4044698737041,7.02360963496715));
#44382=CARTESIAN_POINT('Origin',(55.,29.,3.45145488139523));
#44383=CARTESIAN_POINT('',(53.0466869993245,29.4044698800802,7.9829668504648));
#44384=CARTESIAN_POINT('',(53.0466869980082,29.4044698737233,7.82538782795618));
#44385=CARTESIAN_POINT('',(53.0466869980082,29.4044698737233,3.45145488139523));
#44386=CARTESIAN_POINT('Ctrl Pts',(53.0466869993245,29.4044698800804,7.98296685046478));
#44387=CARTESIAN_POINT('Ctrl Pts',(53.058256749032,29.4603438613858,7.97899706014529));
#44388=CARTESIAN_POINT('Ctrl Pts',(53.0722308559657,29.5157554395691,7.97504270473785));
#44389=CARTESIAN_POINT('Ctrl Pts',(53.09660062202,29.5973971457715,7.96925228785007));
#44390=CARTESIAN_POINT('Ctrl Pts',(53.1051795072496,29.6240737166142,7.96736626695004));
#44391=CARTESIAN_POINT('Ctrl Pts',(53.1202708552382,29.6678166395263,7.96429308346822));
#44392=CARTESIAN_POINT('Ctrl Pts',(53.1264605265564,29.684989503327,7.9630916300141));
#44393=CARTESIAN_POINT('Ctrl Pts',(53.1352247274185,29.7082972012562,7.961470149161));
#44394=CARTESIAN_POINT('Ctrl Pts',(53.1375952712547,29.7145070831788,7.96103903453475));
#44395=CARTESIAN_POINT('Ctrl Pts',(53.1416201433371,29.724894514447,7.96031954278676));
#44396=CARTESIAN_POINT('Ctrl Pts',(53.1432576083671,29.7290784875535,7.960030186707));
#44397=CARTESIAN_POINT('Ctrl Pts',(53.1463869130747,29.7369954180128,7.95948356681448));
#44398=CARTESIAN_POINT('Ctrl Pts',(53.147875919644,29.7407294471354,7.95922613255389));
#44399=CARTESIAN_POINT('Ctrl Pts',(53.1518041756027,29.7504945570915,7.95855383018765));
#44400=CARTESIAN_POINT('Ctrl Pts',(53.1542616834397,29.7565183111737,7.95814004299468));
#44401=CARTESIAN_POINT('Ctrl Pts',(53.1628856813414,29.7773649598123,7.95671091414849));
#44402=CARTESIAN_POINT('Ctrl Pts',(53.1692018014966,29.792125807633,7.95570406270219));
#44403=CARTESIAN_POINT('Ctrl Pts',(53.2178472440217,29.9021196906272,7.94822779975666));
#44404=CARTESIAN_POINT('Ctrl Pts',(53.2674089238648,29.9939930000087,7.94212831651028));
#44405=CARTESIAN_POINT('Ctrl Pts',(53.3723791147905,30.1566598034611,7.93086833385433));
#44406=CARTESIAN_POINT('Ctrl Pts',(53.4258172509597,30.2283972241488,7.92571049418162));
#44407=CARTESIAN_POINT('Ctrl Pts',(53.5192931652996,30.3377234201072,7.91721248782243));
#44408=CARTESIAN_POINT('Ctrl Pts',(53.55638361103,30.3776675013163,7.91395320651823));
#44409=CARTESIAN_POINT('Ctrl Pts',(53.6117569470897,30.4326067039399,7.90919672110261));
#44410=CARTESIAN_POINT('Ctrl Pts',(53.6287443882276,30.4488749846551,7.90775131565239));
#44411=CARTESIAN_POINT('Ctrl Pts',(53.6594621440349,30.4772681333704,7.90515842363056));
#44412=CARTESIAN_POINT('Ctrl Pts',(53.6730794447241,30.4895115597093,7.90401595915376));
#44413=CARTESIAN_POINT('Ctrl Pts',(53.6939505111383,30.5077635569917,7.902274263741));
#44414=CARTESIAN_POINT('Ctrl Pts',(53.7010816860669,30.5139112985939,7.90168078008074));
#44415=CARTESIAN_POINT('Ctrl Pts',(53.7138893422637,30.5247955900981,7.90061759620665));
#44416=CARTESIAN_POINT('Ctrl Pts',(53.7195491717601,30.5295515321807,7.90014869812735));
#44417=CARTESIAN_POINT('Ctrl Pts',(53.7318746572385,30.5397922554801,7.89912951003128));
#44418=CARTESIAN_POINT('Ctrl Pts',(53.7385497179463,30.5452654325582,7.89857876551159));
#44419=CARTESIAN_POINT('Ctrl Pts',(53.7565134784349,30.5598007525789,7.8970997132618));
#44420=CARTESIAN_POINT('Ctrl Pts',(53.767865483786,30.5687834881847,7.89616827652151));
#44421=CARTESIAN_POINT('Ctrl Pts',(53.8195387105894,30.6087651803162,7.89194210521781));
#44422=CARTESIAN_POINT('Ctrl Pts',(53.8609356982831,30.6383363542787,7.888592685866));
#44423=CARTESIAN_POINT('Ctrl Pts',(54.025675521768,30.7467515489523,7.87539183268403));
#44424=CARTESIAN_POINT('Ctrl Pts',(54.156408452148,30.8135025719006,7.86514014977479));
#44425=CARTESIAN_POINT('Ctrl Pts',(54.3701635191774,30.8944920781916,7.84925561106511));
#44426=CARTESIAN_POINT('Ctrl Pts',(54.4488244908911,30.9188544956094,7.84359128707348));
#44427=CARTESIAN_POINT('Ctrl Pts',(54.5441164810909,30.9420214042953,7.83709955782068));
#44428=CARTESIAN_POINT('Ctrl Pts',(54.5595048530021,30.9455695773487,7.8360625996412));
#44429=CARTESIAN_POINT('Ctrl Pts',(54.581069107399,30.9502727747297,7.834626837203));
#44430=CARTESIAN_POINT('Ctrl Pts',(54.5872102978464,30.951581833536,7.83421991175346));
#44431=CARTESIAN_POINT('Ctrl Pts',(54.5976847959668,30.9537629270249,7.83352930758292));
#44432=CARTESIAN_POINT('Ctrl Pts',(54.6020149798198,30.9546495909957,7.83324481407801));
#44433=CARTESIAN_POINT('Ctrl Pts',(54.6103623133197,30.9563299317769,7.83269836873879));
#44434=CARTESIAN_POINT('Ctrl Pts',(54.6143789842356,30.9571256377098,7.83243629825188));
#44435=CARTESIAN_POINT('Ctrl Pts',(54.6240444389855,30.9590094615944,7.83180770914746));
#44436=CARTESIAN_POINT('Ctrl Pts',(54.6296955743781,30.960085530987,7.83144186308687));
#44437=CARTESIAN_POINT('Ctrl Pts',(54.6504122947935,30.9639375429333,7.83010655575824));
#44438=CARTESIAN_POINT('Ctrl Pts',(54.665505517672,30.9665644436056,7.8291450530694));
#44439=CARTESIAN_POINT('Ctrl Pts',(54.8102424195978,30.9900405748958,7.82002007968978));
#44440=CARTESIAN_POINT('Ctrl Pts',(54.9416352029698,30.9982174090173,7.81245324320272));
#44441=CARTESIAN_POINT('Ctrl Pts',(55.2159389231107,30.9881869584236,7.79651215720499));
#44442=CARTESIAN_POINT('Ctrl Pts',(55.3579852893726,30.9675762250938,7.78815511850839));
#44443=CARTESIAN_POINT('Ctrl Pts',(55.5135038781799,30.9276011321715,7.77818948728048));
#44444=CARTESIAN_POINT('Ctrl Pts',(55.5303543803362,30.9230331663275,7.77709922981147));
#44445=CARTESIAN_POINT('Ctrl Pts',(55.5560607117063,30.9157009305978,7.77541895381105));
#44446=CARTESIAN_POINT('Ctrl Pts',(55.5649611041334,30.9130950098609,7.77483403758255));
#44447=CARTESIAN_POINT('Ctrl Pts',(55.5804748039049,30.9084350958864,7.77380886263698));
#44448=CARTESIAN_POINT('Ctrl Pts',(55.5870962387047,30.9064085390371,7.77336950003555));
#44449=CARTESIAN_POINT('Ctrl Pts',(55.6020260349922,30.90175396677,7.77237469091108));
#44450=CARTESIAN_POINT('Ctrl Pts',(55.6103279550488,30.8991059160222,7.77181859947228));
#44451=CARTESIAN_POINT('Ctrl Pts',(55.6327295148991,30.8917984645812,7.7703100337936));
#44452=CARTESIAN_POINT('Ctrl Pts',(55.6467946902029,30.8870359505526,7.76935420962558));
#44453=CARTESIAN_POINT('Ctrl Pts',(55.7122001169103,30.864072320203,7.76486803601261));
#44454=CARTESIAN_POINT('Ctrl Pts',(55.7628299557096,30.843931707293,7.76127451317597));
#44455=CARTESIAN_POINT('Ctrl Pts',(55.9773159941087,30.7482627279924,7.74551321755942));
#44456=CARTESIAN_POINT('Ctrl Pts',(56.1313262609965,30.6527713697668,7.73270425254582));
#44457=CARTESIAN_POINT('Ctrl Pts',(56.2981490696811,30.5149702224225,7.71788395938611));
#44458=CARTESIAN_POINT('Ctrl Pts',(56.325303075136,30.4912739014594,7.71544080017243));
#44459=CARTESIAN_POINT('Ctrl Pts',(56.3679177708981,30.4520016675498,7.71157486702448));
#44460=CARTESIAN_POINT('Ctrl Pts',(56.3837887632463,30.4368843462613,7.71012763146908));
#44461=CARTESIAN_POINT('Ctrl Pts',(56.4044856083783,30.4165092672847,7.708234121535));
#44462=CARTESIAN_POINT('Ctrl Pts',(56.4095363496569,30.4114834788783,7.70777153729304));
#44463=CARTESIAN_POINT('Ctrl Pts',(56.4178004033383,30.403171657022,7.70701398933276));
#44464=CARTESIAN_POINT('Ctrl Pts',(56.4210294295137,30.3999014409133,7.70671782247437));
#44465=CARTESIAN_POINT('Ctrl Pts',(56.4273353113667,30.3934708198436,7.70613916725052));
#44466=CARTESIAN_POINT('Ctrl Pts',(56.4304130250831,30.3903113302691,7.70585661477593));
#44467=CARTESIAN_POINT('Ctrl Pts',(56.4379727507325,30.3824990656663,7.70516219251697));
#44468=CARTESIAN_POINT('Ctrl Pts',(56.4424427369119,30.3778346242954,7.7047512429944));
#44469=CARTESIAN_POINT('Ctrl Pts',(56.4577544338817,30.3617006500387,7.70334201441788));
#44470=CARTESIAN_POINT('Ctrl Pts',(56.4684829630928,30.3501238733153,7.70235191383899));
#44471=CARTESIAN_POINT('Ctrl Pts',(56.5606221808058,30.2483018714429,7.6938121409686));
#44472=CARTESIAN_POINT('Ctrl Pts',(56.6337757698294,30.1509057225283,7.68676991026199));
#44473=CARTESIAN_POINT('Ctrl Pts',(56.7523250472462,29.9587704404674,7.67365987604715));
#44474=CARTESIAN_POINT('Ctrl Pts',(56.8000029196513,29.8659510928186,7.66761595955041));
#44475=CARTESIAN_POINT('Ctrl Pts',(56.853944639569,29.7370096397422,7.6592162431652));
#44476=CARTESIAN_POINT('Ctrl Pts',(56.8667968878204,29.7038203598276,7.65705498695327));
#44477=CARTESIAN_POINT('Ctrl Pts',(56.887340874969,29.6462390851212,7.65329397121755));
#44478=CARTESIAN_POINT('Ctrl Pts',(56.8954641084144,29.6220098513922,7.65170805895421));
#44479=CARTESIAN_POINT('Ctrl Pts',(56.9063536779131,29.5873327456712,7.64943058800991));
#44480=CARTESIAN_POINT('Ctrl Pts',(56.9095042425722,29.577007486723,7.64875150779693));
#44481=CARTESIAN_POINT('Ctrl Pts',(56.9148031789142,29.5591226196559,7.64757337678411));
#44482=CARTESIAN_POINT('Ctrl Pts',(56.9169909929917,29.55157487952,7.64707561401987));
#44483=CARTESIAN_POINT('Ctrl Pts',(56.9211030596698,29.5370686346339,7.64611777284123));
#44484=CARTESIAN_POINT('Ctrl Pts',(56.9230342494557,29.5301122120459,7.64565792730351));
#44485=CARTESIAN_POINT('Ctrl Pts',(56.9274913059824,29.5137123564863,7.64457255272798));
#44486=CARTESIAN_POINT('Ctrl Pts',(56.9299855849412,29.5042606034239,7.64394601908212));
#44487=CARTESIAN_POINT('Ctrl Pts',(56.9384183556305,29.4713263515948,7.64175920298449));
#44488=CARTESIAN_POINT('Ctrl Pts',(56.9439983420182,29.4477550806724,7.64018755802181));
#44489=CARTESIAN_POINT('Ctrl Pts',(56.9788106603771,29.2877547865987,7.62947109318889));
#44490=CARTESIAN_POINT('Ctrl Pts',(56.9940830311268,29.1487086161036,7.61988170300658));
#44491=CARTESIAN_POINT('Ctrl Pts',(56.9949261205005,28.9665675048193,7.60719387944647));
#44492=CARTESIAN_POINT('Ctrl Pts',(56.9937546860302,28.9239063155554,7.60421663448295));
#44493=CARTESIAN_POINT('Ctrl Pts',(56.9864011264306,28.8005329321703,7.59563092414739));
#44494=CARTESIAN_POINT('Ctrl Pts',(56.9766741263554,28.7201095840579,7.59006228582761));
#44495=CARTESIAN_POINT('Ctrl Pts',(56.9592626409828,28.6250828121043,7.58366824560303));
#44496=CARTESIAN_POINT('Ctrl Pts',(56.9562576166606,28.6097063056806,7.58263960691582));
#44497=CARTESIAN_POINT('Ctrl Pts',(56.9517988137639,28.5882377733724,7.58121332570551));
#44498=CARTESIAN_POINT('Ctrl Pts',(56.9504971323217,28.5821152311545,7.58080770055516));
#44499=CARTESIAN_POINT('Ctrl Pts',(56.9482279179279,28.5716834748861,7.58011863444908));
#44500=CARTESIAN_POINT('Ctrl Pts',(56.9472748597342,28.5673711891368,7.57983438741928));
#44501=CARTESIAN_POINT('Ctrl Pts',(56.9454094996615,28.559062082692,7.57928788634528));
#44502=CARTESIAN_POINT('Ctrl Pts',(56.9444991934145,28.555064885811,7.57902551664782));
#44503=CARTESIAN_POINT('Ctrl Pts',(56.9422778673065,28.5454479700905,7.5783954951841));
#44504=CARTESIAN_POINT('Ctrl Pts',(56.9409547627849,28.5398310391723,7.57802852274043));
#44505=CARTESIAN_POINT('Ctrl Pts',(56.9359993720645,28.5191957419056,7.57668377727222));
#44506=CARTESIAN_POINT('Ctrl Pts',(56.9322168895523,28.5042135246025,7.57571411254403));
#44507=CARTESIAN_POINT('Ctrl Pts',(56.895173697089,28.3643552824329,7.56671214152172));
#44508=CARTESIAN_POINT('Ctrl Pts',(56.8500208496504,28.2429267894257,7.55925662655601));
#44509=CARTESIAN_POINT('Ctrl Pts',(56.7301960047754,27.9968494529237,7.54336245238481));
#44510=CARTESIAN_POINT('Ctrl Pts',(56.653055936557,27.8742611389787,7.5349387361995));
#44511=CARTESIAN_POINT('Ctrl Pts',(56.5522958983302,27.7471142978037,7.52487466339645));
#44512=CARTESIAN_POINT('Ctrl Pts',(56.5410412858105,27.7332968531751,7.52376213246466));
#44513=CARTESIAN_POINT('Ctrl Pts',(56.5236022144679,27.7124631008254,7.5220546537203));
#44514=CARTESIAN_POINT('Ctrl Pts',(56.5175508505609,27.705336188094,7.52146507244251));
#44515=CARTESIAN_POINT('Ctrl Pts',(56.5069259843949,27.6929997352353,7.52043479147969));
#44516=CARTESIAN_POINT('Ctrl Pts',(56.5023749778709,27.687770965709,7.51999501829732));
#44517=CARTESIAN_POINT('Ctrl Pts',(56.4920776350535,27.6760638679754,7.51900332634028));
#44518=CARTESIAN_POINT('Ctrl Pts',(56.4863162094975,27.6695990558419,7.5184507870748));
#44519=CARTESIAN_POINT('Ctrl Pts',(56.47072759648,27.652334946948,7.51696183760949));
#44520=CARTESIAN_POINT('Ctrl Pts',(56.4608237754154,27.6416058610416,7.51602222501837));
#44521=CARTESIAN_POINT('Ctrl Pts',(56.4149657699492,27.5930081269185,7.5116993639499));
#44522=CARTESIAN_POINT('Ctrl Pts',(56.3776538449613,27.5564546024662,7.50825829588231));
#44523=CARTESIAN_POINT('Ctrl Pts',(56.2033846403688,27.3986432426049,7.49250589784078));
#44524=CARTESIAN_POINT('Ctrl Pts',(56.0515797433873,27.2951129324974,7.47951785521477));
#44525=CARTESIAN_POINT('Ctrl Pts',(55.8554481099161,27.1976279752204,7.46451448194547));
#44526=CARTESIAN_POINT('Ctrl Pts',(55.8226174920834,27.1824089685719,7.4620610661412));
#44527=CARTESIAN_POINT('Ctrl Pts',(55.7692039190095,27.1593924923555,7.45818080225043));
#44528=CARTESIAN_POINT('Ctrl Pts',(55.748875188057,27.1510282005852,7.45672928335571));
#44529=CARTESIAN_POINT('Ctrl Pts',(55.7217712387449,27.1403966237849,7.45483108397166));
#44530=CARTESIAN_POINT('Ctrl Pts',(55.7151170565212,27.1378276027448,7.45436799432134));
#44531=CARTESIAN_POINT('Ctrl Pts',(55.7041514725323,27.1336614985584,7.45360983344906));
#44532=CARTESIAN_POINT('Ctrl Pts',(55.6998481432022,27.1320435562548,7.45331355535822));
#44533=CARTESIAN_POINT('Ctrl Pts',(55.691406423735,27.1289029518435,7.45273486297223));
#44534=CARTESIAN_POINT('Ctrl Pts',(55.6872685274846,27.1273791152247,7.45245238356636));
#44535=CARTESIAN_POINT('Ctrl Pts',(55.6770615710574,27.1236586533026,7.4517584160686));
#44536=CARTESIAN_POINT('Ctrl Pts',(55.6709867704976,27.121477714559,7.45134784547262));
#44537=CARTESIAN_POINT('Ctrl Pts',(55.6500557091463,27.1140776581088,7.44994127691316));
#44538=CARTESIAN_POINT('Ctrl Pts',(55.6351478577089,27.1090048282404,7.44895341614856));
#44539=CARTESIAN_POINT('Ctrl Pts',(55.5029815265541,27.0657707830142,7.44030520854156));
#44540=CARTESIAN_POINT('Ctrl Pts',(55.382462655455,27.0383772572288,7.43316759851297));
#44541=CARTESIAN_POINT('Ctrl Pts',(55.1581317439686,27.0088660906528,7.42002900329593));
#44542=CARTESIAN_POINT('Ctrl Pts',(55.0552106473647,27.0033604080661,7.41405493492404));
#44543=CARTESIAN_POINT('Ctrl Pts',(54.9170048944666,27.006664100843,7.40574460306981));
#44544=CARTESIAN_POINT('Ctrl Pts',(54.8817093102582,27.0084470142943,7.40359805861164));
#44545=CARTESIAN_POINT('Ctrl Pts',(54.8211411944945,27.0131222916088,7.39986040500741));
#44546=CARTESIAN_POINT('Ctrl Pts',(54.795841904756,27.0155623259862,7.39828290721759));
#44547=CARTESIAN_POINT('Ctrl Pts',(54.7598963921876,27.019723792608,7.39601543578436));
#44548=CARTESIAN_POINT('Ctrl Pts',(54.7492061730232,27.0210492555022,7.39533778882544));
#44549=CARTESIAN_POINT('Ctrl Pts',(54.7307407916579,27.0234907710482,7.39416134867105));
#44550=CARTESIAN_POINT('Ctrl Pts',(54.7229604455916,27.0245662917111,7.39366383336948));
#44551=CARTESIAN_POINT('Ctrl Pts',(54.7080361239225,27.0267192665489,7.3927059062986));
#44552=CARTESIAN_POINT('Ctrl Pts',(54.7008912394898,27.0277896397483,7.3922457241843));
#44553=CARTESIAN_POINT('Ctrl Pts',(54.6840727336928,27.0304027105315,7.39115868806623));
#44554=CARTESIAN_POINT('Ctrl Pts',(54.6744044186631,27.0319778883208,7.39053082186408));
#44555=CARTESIAN_POINT('Ctrl Pts',(54.6407522096671,27.0377153278892,7.38833484031418));
#44556=CARTESIAN_POINT('Ctrl Pts',(54.61683400196,27.0422452041131,7.38675523663701));
#44557=CARTESIAN_POINT('Ctrl Pts',(54.4647426402105,27.0739436414041,7.37658623668558));
#44558=CARTESIAN_POINT('Ctrl Pts',(54.3394474144801,27.1132427693404,7.36760964848039));
#44559=CARTESIAN_POINT('Ctrl Pts',(54.1265165393998,27.2038539338081,7.35150558040402));
#44560=CARTESIAN_POINT('Ctrl Pts',(54.0372030134549,27.2501035455637,7.34446669077798));
#44561=CARTESIAN_POINT('Ctrl Pts',(53.9279170166428,27.3176057662148,7.33573691058411));
#44562=CARTESIAN_POINT('Ctrl Pts',(53.9043954342116,27.332827819907,7.33385121169732));
#44563=CARTESIAN_POINT('Ctrl Pts',(53.8660915882586,27.3587771773414,7.33077849516072));
#44564=CARTESIAN_POINT('Ctrl Pts',(53.8511225668072,27.3692206342248,7.32957719181216));
#44565=CARTESIAN_POINT('Ctrl Pts',(53.830900105809,27.3837459433206,7.32795587899305));
#44566=CARTESIAN_POINT('Ctrl Pts',(53.8255211616559,27.3876504102281,7.32752478519715));
#44567=CARTESIAN_POINT('Ctrl Pts',(53.8165390476539,27.3942391453251,7.32680531850831));
#44568=CARTESIAN_POINT('Ctrl Pts',(53.8129252892231,27.396908804733,7.32651596680101));
#44569=CARTESIAN_POINT('Ctrl Pts',(53.8060952666062,27.401990234633,7.32596934788591));
#44570=CARTESIAN_POINT('Ctrl Pts',(53.8028772308953,27.4043995490678,7.32571191027209));
#44571=CARTESIAN_POINT('Ctrl Pts',(53.7944702769207,27.4107335100226,7.32503958587472));
#44572=CARTESIAN_POINT('Ctrl Pts',(53.7892931852811,27.4146738818139,7.32462578014157));
#44573=CARTESIAN_POINT('Ctrl Pts',(53.7714068107378,27.4284262242267,7.3231965216192));
#44574=CARTESIAN_POINT('Ctrl Pts',(53.7587963943306,27.4383665587333,7.32218956108257));
#44575=CARTESIAN_POINT('Ctrl Pts',(53.6639988194956,27.5149659015489,7.31461345651484));
#44576=CARTESIAN_POINT('Ctrl Pts',(53.5871023589485,27.5879265476658,7.30842594831309));
#44577=CARTESIAN_POINT('Ctrl Pts',(53.439900501296,27.7517217911272,7.29562064378984));
#44578=CARTESIAN_POINT('Ctrl Pts',(53.3709122049121,27.8432026560081,7.28902582320648));
#44579=CARTESIAN_POINT('Ctrl Pts',(53.2791429265253,27.9895137553325,7.27867825059314));
#44580=CARTESIAN_POINT('Ctrl Pts',(53.2503279811946,28.0402717175552,7.27512389268616));
#44581=CARTESIAN_POINT('Ctrl Pts',(53.2171709388505,28.1051485949626,7.27058502461403));
#44582=CARTESIAN_POINT('Ctrl Pts',(53.210703009256,28.1181526437211,7.26967551919338));
#44583=CARTESIAN_POINT('Ctrl Pts',(53.2006137056474,28.1390056797287,7.26821695281176));
#44584=CARTESIAN_POINT('Ctrl Pts',(53.1969002701736,28.1468097419918,7.26767107610022));
#44585=CARTESIAN_POINT('Ctrl Pts',(53.1899723374444,28.1616165603018,7.26663521678136));
#44586=CARTESIAN_POINT('Ctrl Pts',(53.1867474636532,28.1686143085819,7.26614560141701));
#44587=CARTESIAN_POINT('Ctrl Pts',(53.1795343351045,28.1845078994495,7.26503333213097));
#44588=CARTESIAN_POINT('Ctrl Pts',(53.1755706138886,28.1934145967883,7.26440985640041));
#44589=CARTESIAN_POINT('Ctrl Pts',(53.1655107147186,28.2164733170062,7.26279513176812));
#44590=CARTESIAN_POINT('Ctrl Pts',(53.1595130373644,28.2306673546693,7.26180059177553));
#44591=CARTESIAN_POINT('Ctrl Pts',(53.1179166391773,28.3323799787954,7.25466830177191));
#44592=CARTESIAN_POINT('Ctrl Pts',(53.0884162205546,28.4222482280429,7.24832876228336));
#44593=CARTESIAN_POINT('Ctrl Pts',(53.023562523072,28.6803332287233,7.23006428913969));
#44594=CARTESIAN_POINT('Ctrl Pts',(53.0033931300134,28.8515035560417,7.21783037161033));
#44595=CARTESIAN_POINT('Ctrl Pts',(53.0055596025529,29.0382582085128,7.20536269312291));
#44596=CARTESIAN_POINT('Ctrl Pts',(53.0059069074542,29.0533756303228,7.20436029661958));
#44597=CARTESIAN_POINT('Ctrl Pts',(53.006817465833,29.0798804490078,7.20261646716537));
#44598=CARTESIAN_POINT('Ctrl Pts',(53.0073064990734,29.0912695268911,7.20187156670995));
#44599=CARTESIAN_POINT('Ctrl Pts',(53.008176480545,29.1081523989988,7.20077451358064));
#44600=CARTESIAN_POINT('Ctrl Pts',(53.0084825763716,29.1136495807192,7.20041843336773));
#44601=CARTESIAN_POINT('Ctrl Pts',(53.0090688051341,29.1234467780605,7.19978591454569));
#44602=CARTESIAN_POINT('Ctrl Pts',(53.0093401144347,29.1277472148095,7.19950899806007));
#44603=CARTESIAN_POINT('Ctrl Pts',(53.0099591961832,29.1370787848985,7.19890969838135));
#44604=CARTESIAN_POINT('Ctrl Pts',(53.0103121124014,29.1421094839134,7.19858760254091));
#44605=CARTESIAN_POINT('Ctrl Pts',(53.0113411716254,29.1560223544458,7.19769942173102));
#44606=CARTESIAN_POINT('Ctrl Pts',(53.0120577479138,29.1649015467617,7.19713552410449));
#44607=CARTESIAN_POINT('Ctrl Pts',(53.0161643985336,29.2118620306212,7.19416732481635));
#44608=CARTESIAN_POINT('Ctrl Pts',(53.0205895144708,29.2498475221283,7.19181566616976));
#44609=CARTESIAN_POINT('Ctrl Pts',(53.0314832209871,29.3245925942169,7.18724471848035));
#44610=CARTESIAN_POINT('Ctrl Pts',(53.0378966351962,29.3613437508665,7.18502451419171));
#44611=CARTESIAN_POINT('Ctrl Pts',(53.0457833858183,29.4000874820423,7.18269327447379));
#44612=CARTESIAN_POINT('Ctrl Pts',(53.0462333559396,29.4022790926368,7.18256143578627));
#44613=CARTESIAN_POINT('Ctrl Pts',(53.0466869981335,29.4044698743284,7.18242967527062));
#44614=CARTESIAN_POINT('',(53.0052508017986,28.9982114880629,7.05145488142717));
#44615=CARTESIAN_POINT('Ctrl Pts',(53.0466869980042,29.4044698737041,7.02360963496715));
#44616=CARTESIAN_POINT('Ctrl Pts',(53.0445976879508,29.3943799343589,7.02427478038959));
#44617=CARTESIAN_POINT('Ctrl Pts',(53.0425866133465,29.3842740735815,7.02494239072689));
#44618=CARTESIAN_POINT('Ctrl Pts',(53.0169857519414,29.2502088099897,7.03381838151229));
#44619=CARTESIAN_POINT('Ctrl Pts',(53.00513641142,29.1243248017733,7.04240020381067));
#44620=CARTESIAN_POINT('Ctrl Pts',(53.0052508205679,28.9981906755863,7.05115502780437));
#44621=CARTESIAN_POINT('Ctrl Pts',(53.0052508017986,28.9982114880629,7.05145488142717));
#44622=CARTESIAN_POINT('Ctrl Pts',(53.005330467948,28.9093588590626,7.05712256701506));
#44623=CARTESIAN_POINT('Ctrl Pts',(53.0113506355184,28.8207686812029,7.06279025260296));
#44624=CARTESIAN_POINT('Ctrl Pts',(53.0231839296303,28.7331184037289,7.06845793819085));
#44625=CARTESIAN_POINT('Ctrl Pts',(53.0343123097836,28.6506894875669,7.07378799753146));
#44626=CARTESIAN_POINT('Ctrl Pts',(53.0505813290659,28.5690913732212,7.07911805687207));
#44627=CARTESIAN_POINT('Ctrl Pts',(53.0718472890399,28.4888692087957,7.08444811621268));
#44628=CARTESIAN_POINT('Ctrl Pts',(53.0896261223019,28.4218016281651,7.0889041688155));
#44629=CARTESIAN_POINT('Ctrl Pts',(53.1109431910862,28.355531420224,7.09336022141832));
#44630=CARTESIAN_POINT('Ctrl Pts',(53.1357095494889,28.290458825273,7.09781627402114));
#44631=CARTESIAN_POINT('Ctrl Pts',(53.1604389486801,28.2254833391402,7.10226567678923));
#44632=CARTESIAN_POINT('Ctrl Pts',(53.188607248147,28.1617023720646,7.10671507955732));
#44633=CARTESIAN_POINT('Ctrl Pts',(53.2200752937475,28.0995025804746,7.1111644823254));
#44634=CARTESIAN_POINT('Ctrl Pts',(53.2515066084609,28.0373753912175,7.11560869155486));
#44635=CARTESIAN_POINT('Ctrl Pts',(53.2862297995589,27.9768261459978,7.12005290078431));
#44636=CARTESIAN_POINT('Ctrl Pts',(53.3240577194163,27.9182213559827,7.12449711001376));
#44637=CARTESIAN_POINT('Ctrl Pts',(53.3618620647527,27.8596530887227,7.12893854959307));
#44638=CARTESIAN_POINT('Ctrl Pts',(53.4027670356867,27.803027282564,7.13337998917237));
#44639=CARTESIAN_POINT('Ctrl Pts',(53.4465404238203,27.7486843293255,7.13782142875168));
#44640=CARTESIAN_POINT('Ctrl Pts',(53.4903013669552,27.6943568260673,7.14226160560693));
#44641=CARTESIAN_POINT('Ctrl Pts',(53.5369288016427,27.6423112678627,7.14670178246219));
#44642=CARTESIAN_POINT('Ctrl Pts',(53.5861492903504,27.5928561788775,7.15114195931745));
#44643=CARTESIAN_POINT('Ctrl Pts',(53.6353724656587,27.5433983904864,7.15558237853077));
#44644=CARTESIAN_POINT('Ctrl Pts',(53.687188629292,27.4965316969205,7.16002279774409));
#44645=CARTESIAN_POINT('Ctrl Pts',(53.7412876925744,27.4525275803313,7.16446321695741));
#44646=CARTESIAN_POINT('Ctrl Pts',(53.7954437835132,27.4084770775112,7.16890831696714));
#44647=CARTESIAN_POINT('Ctrl Pts',(53.8518871969525,27.3672954833691,7.17335341697686));
#44648=CARTESIAN_POINT('Ctrl Pts',(53.9102757449189,27.3292131762586,7.17779851698659));
#44649=CARTESIAN_POINT('Ctrl Pts',(53.9686986081662,27.2911084879601,7.18224622940681));
#44650=CARTESIAN_POINT('Ctrl Pts',(54.0290684581531,27.2561069574895,7.18669394182704));
#44651=CARTESIAN_POINT('Ctrl Pts',(54.0910175906236,27.2243934720935,7.19114165424727));
#44652=CARTESIAN_POINT('Ctrl Pts',(54.1530732469453,27.1926254541727,7.19559701467543));
#44653=CARTESIAN_POINT('Ctrl Pts',(54.2167131600073,27.1641569663705,7.20005237510359));
#44654=CARTESIAN_POINT('Ctrl Pts',(54.2815494725857,27.1391248289694,7.20450773553175));
#44655=CARTESIAN_POINT('Ctrl Pts',(54.3137744230974,27.1266833535543,7.20672213921387));
#44656=CARTESIAN_POINT('Ctrl Pts',(54.3462946796159,27.1150899806534,7.208936542896));
#44657=CARTESIAN_POINT('Ctrl Pts',(54.3790614983329,27.1043568532956,7.21115094657813));
#44658=CARTESIAN_POINT('Ctrl Pts',(54.4449982766341,27.0827585454103,7.21560699847377));
#44659=CARTESIAN_POINT('Ctrl Pts',(54.5121924168342,27.0645622877864,7.2200630503694));
#44660=CARTESIAN_POINT('Ctrl Pts',(54.5802597651972,27.0499113615562,7.22451910226504));
#44661=CARTESIAN_POINT('Ctrl Pts',(54.6482255355046,27.035282299151,7.22896850431904));
#44662=CARTESIAN_POINT('Ctrl Pts',(54.7170614532739,27.0241881689483,7.23341790637304));
#44663=CARTESIAN_POINT('Ctrl Pts',(54.7863674258446,27.0167227410774,7.23786730842703));
#44664=CARTESIAN_POINT('Ctrl Pts',(54.8555925013184,27.0092660271948,7.24231151693572));
#44665=CARTESIAN_POINT('Ctrl Pts',(54.9252860579139,27.0054296550877,7.24675572544441));
#44666=CARTESIAN_POINT('Ctrl Pts',(54.9950387736206,27.0052561696466,7.2511999339531));
#44667=CARTESIAN_POINT('Ctrl Pts',(55.0647480190721,27.0050827923226,7.25564137280793));
#44668=CARTESIAN_POINT('Ctrl Pts',(55.1345158625737,27.0085677742324,7.26008281166277));
#44669=CARTESIAN_POINT('Ctrl Pts',(55.203930360552,27.0157016427601,7.2645242505176));
#44670=CARTESIAN_POINT('Ctrl Pts',(55.2733251235887,27.0228334830878,7.26896442664579));
#44671=CARTESIAN_POINT('Ctrl Pts',(55.3423662543198,27.033612100505,7.27340460277399));
#44672=CARTESIAN_POINT('Ctrl Pts',(55.4106460953808,27.0479760895808,7.27784477890218));
#44673=CARTESIAN_POINT('Ctrl Pts',(55.4789296633368,27.0623408626812,7.28228519738697));
#44674=CARTESIAN_POINT('Ctrl Pts',(55.5464513810847,27.0802912929114,7.28672561587176));
#44675=CARTESIAN_POINT('Ctrl Pts',(55.6128147101192,27.1017150652335,7.29116603435654));
#44676=CARTESIAN_POINT('Ctrl Pts',(55.6792479950412,27.1231614210972,7.29561113364051));
#44677=CARTESIAN_POINT('Ctrl Pts',(55.7445199878621,27.148088276039,7.30005623292447));
#44678=CARTESIAN_POINT('Ctrl Pts',(55.8082511540919,27.1763340123781,7.30450133220844));
#44679=CARTESIAN_POINT('Ctrl Pts',(55.8720197755036,27.2045963489028,7.30894904390344));
#44680=CARTESIAN_POINT('Ctrl Pts',(55.9342453317487,27.2361812277723,7.31339675559844));
#44681=CARTESIAN_POINT('Ctrl Pts',(55.9945725563398,27.2708808622088,7.31784446729343));
#44682=CARTESIAN_POINT('Ctrl Pts',(56.0550035159831,27.3056401640412,7.32229982700486));
#44683=CARTESIAN_POINT('Ctrl Pts',(56.1135292180118,27.3435246464504,7.32675518671628));
#44684=CARTESIAN_POINT('Ctrl Pts',(56.169823744429,27.3842834501466,7.3312105464277));
#44685=CARTESIAN_POINT('Ctrl Pts',(56.1978033420369,27.404541457434,7.33342495659966));
#44686=CARTESIAN_POINT('Ctrl Pts',(56.2252322915135,27.4255088867476,7.33563936677162));
#44687=CARTESIAN_POINT('Ctrl Pts',(56.2520738704859,27.4471514609124,7.33785377694358));
#44688=CARTESIAN_POINT('Ctrl Pts',(56.306087108594,27.4907027554484,7.34230982865389));
#44689=CARTESIAN_POINT('Ctrl Pts',(56.357931130304,27.5371608355829,7.34676588036421));
#44690=CARTESIAN_POINT('Ctrl Pts',(56.4072766141824,27.5862814658939,7.35122193207452));
#44691=CARTESIAN_POINT('Ctrl Pts',(56.4565484588945,27.6353287925915,7.35567133393751));
#44692=CARTESIAN_POINT('Ctrl Pts',(56.5033288226362,27.6870304407377,7.36012073580051));
#44693=CARTESIAN_POINT('Ctrl Pts',(56.5473212378837,27.7411018511039,7.3645701376635));
#44694=CARTESIAN_POINT('Ctrl Pts',(56.5912623030984,27.7951101467564,7.3690143459737));
#44695=CARTESIAN_POINT('Ctrl Pts',(56.6324215761606,27.8514823330851,7.37345855428391));
#44696=CARTESIAN_POINT('Ctrl Pts',(56.670540534099,27.9098982219847,7.37790276259411));
#44697=CARTESIAN_POINT('Ctrl Pts',(56.7086357360648,27.9682777057374,7.38234420124593));
#44698=CARTESIAN_POINT('Ctrl Pts',(56.7436941151949,28.0286979566868,7.38678563989775));
#44699=CARTESIAN_POINT('Ctrl Pts',(56.7754993549302,28.090808269317,7.39122707854957));
#44700=CARTESIAN_POINT('Ctrl Pts',(56.8072955522221,28.1529009235678,7.39566725447052));
#44701=CARTESIAN_POINT('Ctrl Pts',(56.8358402235265,28.2166822505069,7.40010743039146));
#44702=CARTESIAN_POINT('Ctrl Pts',(56.8609629482528,28.2817768677282,7.40454760631241));
#44703=CARTESIAN_POINT('Ctrl Pts',(56.8860870442219,28.346875037929,7.40898802458603));
#44704=CARTESIAN_POINT('Ctrl Pts',(56.907788649001,28.4132861836269,7.41342844285964));
#44705=CARTESIAN_POINT('Ctrl Pts',(56.9259460993766,28.4806165339595,7.41786886113326));
#44706=CARTESIAN_POINT('Ctrl Pts',(56.9441226901329,28.548017859485,7.42231396020152));
#44707=CARTESIAN_POINT('Ctrl Pts',(56.958747542426,28.6163398504778,7.42675905926977));
#44708=CARTESIAN_POINT('Ctrl Pts',(56.9697496063415,28.6851761590708,7.43120415833803));
#44709=CARTESIAN_POINT('Ctrl Pts',(56.980758136228,28.7540529231248,7.43565186981443));
#44710=CARTESIAN_POINT('Ctrl Pts',(56.9881395881643,28.8234441200276,7.44009958129082));
#44711=CARTESIAN_POINT('Ctrl Pts',(56.9918748515594,28.8929386240275,7.44454729276721));
#44712=CARTESIAN_POINT('Ctrl Pts',(56.9956165378864,28.9625526265509,7.44900265225781));
#44713=CARTESIAN_POINT('Ctrl Pts',(56.9956995204162,29.032269801885,7.45345801174842));
#44714=CARTESIAN_POINT('Ctrl Pts',(56.9921567962098,29.1016801938195,7.45791337123902));
#44715=CARTESIAN_POINT('Ctrl Pts',(56.99039598407,29.1361786909147,7.46012778326235));
#44716=CARTESIAN_POINT('Ctrl Pts',(56.987740316033,29.1706015002951,7.46234219528569));
#44717=CARTESIAN_POINT('Ctrl Pts',(56.9841985529908,29.2048991576584,7.46455660730903));
#44718=CARTESIAN_POINT('Ctrl Pts',(56.9770714781229,29.2739161892637,7.46901265930649));
#44719=CARTESIAN_POINT('Ctrl Pts',(56.9663251945019,29.3426960836193,7.47346871130395));
#44720=CARTESIAN_POINT('Ctrl Pts',(56.9519852901646,29.4108296355923,7.47792476330141));
#44721=CARTESIAN_POINT('Ctrl Pts',(56.9376667855111,29.478861510704,7.48237416545651));
#44722=CARTESIAN_POINT('Ctrl Pts',(56.9197654043598,29.5462484831796,7.4868235676116));
#44723=CARTESIAN_POINT('Ctrl Pts',(56.8983584450676,29.6125869542691,7.4912729697667));
#44724=CARTESIAN_POINT('Ctrl Pts',(56.8769764729631,29.6788479920432,7.4957171783749));
#44725=CARTESIAN_POINT('Ctrl Pts',(56.8520971994254,29.7440624960506,7.5001613869831));
#44726=CARTESIAN_POINT('Ctrl Pts',(56.8238484662561,29.8078393000067,7.5046055955913));
#44727=CARTESIAN_POINT('Ctrl Pts',(56.7956173378504,29.8715763579129,7.5090470345446));
#44728=CARTESIAN_POINT('Ctrl Pts',(56.7640211132783,29.9338770471652,7.5134884734979));
#44729=CARTESIAN_POINT('Ctrl Pts',(56.7292362103178,29.994368991585,7.5179299124512));
#44730=CARTESIAN_POINT('Ctrl Pts',(56.6944611969147,30.0548437377807,7.52237008867666));
#44731=CARTESIAN_POINT('Ctrl Pts',(56.6564995485811,30.1135103363396,7.52681026490211));
#44732=CARTESIAN_POINT('Ctrl Pts',(56.6155733684929,30.1700214756646,7.53125044112756));
#44733=CARTESIAN_POINT('Ctrl Pts',(56.5746449545579,30.2265356995002,7.53569085970825));
#44734=CARTESIAN_POINT('Ctrl Pts',(56.5307519764274,30.2808938358961,7.54013127828894));
#44735=CARTESIAN_POINT('Ctrl Pts',(56.4841585055315,30.3327794614858,7.54457169686962));
#44736=CARTESIAN_POINT('Ctrl Pts',(56.4375159188712,30.3847197814805,7.54901679624675));
#44737=CARTESIAN_POINT('Ctrl Pts',(56.3881674852917,30.4341820242444,7.55346189562388));
#44738=CARTESIAN_POINT('Ctrl Pts',(56.3364153800509,30.480885375194,7.557906995001));
#44739=CARTESIAN_POINT('Ctrl Pts',(56.2846328598102,30.5276161739625,7.56235470678773));
#44740=CARTESIAN_POINT('Ctrl Pts',(56.2304442359862,30.5715845454544,7.56680241857447));
#44741=CARTESIAN_POINT('Ctrl Pts',(56.1741839674546,30.612550642018,7.5712501303612));
#44742=CARTESIAN_POINT('Ctrl Pts',(56.1178269572052,30.6535871813763,7.57570549016116));
#44743=CARTESIAN_POINT('Ctrl Pts',(56.0593916015765,30.6916108745887,7.58016084996113));
#44744=CARTESIAN_POINT('Ctrl Pts',(55.9992397458495,30.7264262199163,7.58461620976109));
#44745=CARTESIAN_POINT('Ctrl Pts',(55.9693429844244,30.7437301926802,7.58683061906555));
#44746=CARTESIAN_POINT('Ctrl Pts',(55.9390225525708,30.7602423352268,7.58904502837001));
#44747=CARTESIAN_POINT('Ctrl Pts',(55.9083247114548,30.7759430680798,7.59125943767448));
#44748=CARTESIAN_POINT('Ctrl Pts',(55.8465515006347,30.8075376247423,7.59571548956065));
#44749=CARTESIAN_POINT('Ctrl Pts',(55.7830069063956,30.8359672002922,7.60017154144682));
#44750=CARTESIAN_POINT('Ctrl Pts',(55.7180481104491,30.86103048701,7.60462759333299));
#44751=CARTESIAN_POINT('Ctrl Pts',(55.6531862536422,30.8860563713496,7.60907699537553));
#44752=CARTESIAN_POINT('Ctrl Pts',(55.5869148365943,30.9077257631791,7.61352639741806));
#44753=CARTESIAN_POINT('Ctrl Pts',(55.5196144893837,30.9258837828183,7.6179757994606));
#44754=CARTESIAN_POINT('Ctrl Pts',(55.4523926982567,30.9440206075756,7.62242000795491));
#44755=CARTESIAN_POINT('Ctrl Pts',(55.3841448323252,30.9586540740292,7.62686421644922));
#44756=CARTESIAN_POINT('Ctrl Pts',(55.315268608896,30.9696784678583,7.63130842494354));
#44757=CARTESIAN_POINT('Ctrl Pts',(55.2464353095155,30.9806959912235,7.63574986378219));
#44758=CARTESIAN_POINT('Ctrl Pts',(55.1769749113017,30.988108826964,7.64019130262085));
#44759=CARTESIAN_POINT('Ctrl Pts',(55.1072958147491,30.9918622368621,7.64463274145951));
#44760=CARTESIAN_POINT('Ctrl Pts',(55.037636528393,30.9956145796427,7.64907291756974));
#44761=CARTESIAN_POINT('Ctrl Pts',(54.9677591552154,30.9957095357998,7.65351309367997));
#44762=CARTESIAN_POINT('Ctrl Pts',(54.8980759420762,30.9921443343584,7.65795326979021));
#44763=CARTESIAN_POINT('Ctrl Pts',(54.8283889254701,30.9885789383203,7.66239368825527));
#44764=CARTESIAN_POINT('Ctrl Pts',(54.7588965781964,30.9813530154764,7.66683410672033));
#44765=CARTESIAN_POINT('Ctrl Pts',(54.6900080848404,30.9705158144597,7.67127452518539));
#44766=CARTESIAN_POINT('Ctrl Pts',(54.6210469737728,30.9596671895796,7.67571962444707));
#44767=CARTESIAN_POINT('Ctrl Pts',(54.5526914710745,30.9451997649612,7.68016472370876));
#44768=CARTESIAN_POINT('Ctrl Pts',(54.4853416355406,30.9272141371399,7.68460982297044));
#44769=CARTESIAN_POINT('Ctrl Pts',(54.4179522181341,30.9092179390652,7.68905753464167));
#44770=CARTESIAN_POINT('Ctrl Pts',(54.3515701095865,30.8876995731218,7.69350524631289));
#44771=CARTESIAN_POINT('Ctrl Pts',(54.2865785798249,30.8628090185887,7.69795295798412));
#44772=CARTESIAN_POINT('Ctrl Pts',(54.2214752945834,30.8378756637726,7.7024083176697));
#44773=CARTESIAN_POINT('Ctrl Pts',(54.1577678076811,30.8095587446936,7.70686367735528));
#44774=CARTESIAN_POINT('Ctrl Pts',(54.0958170997561,30.7780553549894,7.71131903704085));
#44775=CARTESIAN_POINT('Ctrl Pts',(54.0650262551444,30.7623974874749,7.71353344737388));
#44776=CARTESIAN_POINT('Ctrl Pts',(54.0346689715651,30.7459531607705,7.71574785770691));
#44777=CARTESIAN_POINT('Ctrl Pts',(54.0047868574518,30.7287505208674,7.71796226803994));
#44778=CARTESIAN_POINT('Ctrl Pts',(53.9443850958589,30.6939782236246,7.72243833303645));
#44779=CARTESIAN_POINT('Ctrl Pts',(53.8856890934857,30.6559681027548,7.72691439803296));
#44780=CARTESIAN_POINT('Ctrl Pts',(53.8290670293782,30.6149128585812,7.73139046302947));
#44781=CARTESIAN_POINT('Ctrl Pts',(53.7727928307591,30.574109842983,7.73583902870111));
#44782=CARTESIAN_POINT('Ctrl Pts',(53.7185675837773,30.530299265726,7.74028759437275));
#44783=CARTESIAN_POINT('Ctrl Pts',(53.666728108292,30.483716153879,7.74473616004438));
#44784=CARTESIAN_POINT('Ctrl Pts',(53.6149406275608,30.4371797646776,7.74918026382523));
#44785=CARTESIAN_POINT('Ctrl Pts',(53.5655345327799,30.3878766830037,7.75362436760608));
#44786=CARTESIAN_POINT('Ctrl Pts',(53.5188148507357,30.3360831246966,7.75806847138692));
#44787=CARTESIAN_POINT('Ctrl Pts',(53.4721261933883,30.2843239604471,7.76250962401386));
#44788=CARTESIAN_POINT('Ctrl Pts',(53.4281207344431,30.2300779645987,7.76695077664079));
#44789=CARTESIAN_POINT('Ctrl Pts',(53.3870665053104,30.1736580013821,7.77139192926773));
#44790=CARTESIAN_POINT('Ctrl Pts',(53.3454714476156,30.1164947888531,7.77589158749176));
#44791=CARTESIAN_POINT('Ctrl Pts',(53.3069062974652,30.0571002854678,7.7803912457158));
#44792=CARTESIAN_POINT('Ctrl Pts',(53.2716065449753,29.9958331321701,7.78489090393984));
#44793=CARTESIAN_POINT('Ctrl Pts',(53.2367637564795,29.9353590972686,7.78933231297941));
#44794=CARTESIAN_POINT('Ctrl Pts',(53.2051025141465,29.8730610744932,7.79377372201899));
#44795=CARTESIAN_POINT('Ctrl Pts',(53.1768035530877,29.8093097543378,7.79821513105856));
#44796=CARTESIAN_POINT('Ctrl Pts',(53.1479478797148,29.7443042840779,7.80274391387483));
#44797=CARTESIAN_POINT('Ctrl Pts',(53.1225884276952,29.6777881994564,7.8072726966911));
#44798=CARTESIAN_POINT('Ctrl Pts',(53.1008648448833,29.6101747496414,7.81180147950737));
#44799=CARTESIAN_POINT('Ctrl Pts',(53.0791412620714,29.5425612998265,7.81633026232364));
#44800=CARTESIAN_POINT('Ctrl Pts',(53.0610536560262,29.47385101117,7.82085904513991));
#44801=CARTESIAN_POINT('Ctrl Pts',(53.0466869980082,29.4044698737233,7.82538782795619));
#44802=CARTESIAN_POINT('Origin',(55.,29.,3.45145488139523));
#44803=CARTESIAN_POINT('',(53.0466869980092,29.404469873728,8.78541210591381));
#44804=CARTESIAN_POINT('',(53.0466869433582,29.4044696098012,8.62635914573793));
#44805=CARTESIAN_POINT('',(53.0466869980082,29.4044698737233,3.45145488139523));
#44806=CARTESIAN_POINT('',(53.0052508354721,29.0012981434294,8.01095171076546));
#44807=CARTESIAN_POINT('Ctrl Pts',(53.0466869980092,29.404469873728,8.78541210591381));
#44808=CARTESIAN_POINT('Ctrl Pts',(53.0471763476454,29.4068330979609,8.78525791073123));
#44809=CARTESIAN_POINT('Ctrl Pts',(53.0476699849055,29.4091954287619,8.78510357909714));
#44810=CARTESIAN_POINT('Ctrl Pts',(53.0511509502984,29.4257041076768,8.78402369411619));
#44811=CARTESIAN_POINT('Ctrl Pts',(53.0542876510602,29.4398181929545,8.78309341089251));
#44812=CARTESIAN_POINT('Ctrl Pts',(53.0706602313561,29.5098836375005,8.77843926933478));
#44813=CARTESIAN_POINT('Ctrl Pts',(53.0861562499064,29.5652736190893,8.77464408487961));
#44814=CARTESIAN_POINT('Ctrl Pts',(53.1386457955463,29.7258108077838,8.76329370015989));
#44815=CARTESIAN_POINT('Ctrl Pts',(53.1820782395446,29.8286110184691,8.75555879578595));
#44816=CARTESIAN_POINT('Ctrl Pts',(53.2848874775335,30.0244355553964,8.74014342331277));
#44817=CARTESIAN_POINT('Ctrl Pts',(53.3438592282766,30.1172652160646,8.73249249321695));
#44818=CARTESIAN_POINT('Ctrl Pts',(53.4198655981057,30.2175632246231,8.72415558681927));
#44819=CARTESIAN_POINT('Ctrl Pts',(53.429709300766,30.2302325360583,8.72310133076771));
#44820=CARTESIAN_POINT('Ctrl Pts',(53.4437571326641,30.2478693836482,8.72163365224335));
#44821=CARTESIAN_POINT('Ctrl Pts',(53.4478340420646,30.2529368310685,8.7212119501624));
#44822=CARTESIAN_POINT('Ctrl Pts',(53.4544706607057,30.2611037946156,8.72053242764542));
#44823=CARTESIAN_POINT('Ctrl Pts',(53.4570150411808,30.2642156212326,8.72027353898543));
#44824=CARTESIAN_POINT('Ctrl Pts',(53.4624235911971,30.2707897307754,8.71972670203542));
#44825=CARTESIAN_POINT('Ctrl Pts',(53.4652900879389,30.2742500693926,8.71943892872029));
#44826=CARTESIAN_POINT('Ctrl Pts',(53.472427082998,30.282806592206,8.71872740219586));
#44827=CARTESIAN_POINT('Ctrl Pts',(53.4767114591822,30.2878912198545,8.71830463990576));
#44828=CARTESIAN_POINT('Ctrl Pts',(53.4928616384867,30.3068646491141,8.71672688384933));
#44829=CARTESIAN_POINT('Ctrl Pts',(53.5048930387663,30.3206121617782,8.71558327535639));
#44830=CARTESIAN_POINT('Ctrl Pts',(53.5358718030092,30.3550434879406,8.7127121709201));
#44831=CARTESIAN_POINT('Ctrl Pts',(53.5550701487517,30.3754970428994,8.71100013531827));
#44832=CARTESIAN_POINT('Ctrl Pts',(53.6451182525085,30.4674657971467,8.70323415030831));
#44833=CARTESIAN_POINT('Ctrl Pts',(53.7208909775005,30.5339633712613,8.69741896197683));
#44834=CARTESIAN_POINT('Ctrl Pts',(53.905846003979,30.6730032461,8.68398018520722));
#44835=CARTESIAN_POINT('Ctrl Pts',(54.0177801684663,30.7410776957544,8.67635212630113));
#44836=CARTESIAN_POINT('Ctrl Pts',(54.1575031152611,30.808264185645,8.66680788757141));
#44837=CARTESIAN_POINT('Ctrl Pts',(54.1796362301917,30.8184123766082,8.66529635302767));
#44838=CARTESIAN_POINT('Ctrl Pts',(54.2109273303359,30.8320720127476,8.66315733592696));
#44839=CARTESIAN_POINT('Ctrl Pts',(54.2199344553071,30.8359251832365,8.66254139067008));
#44840=CARTESIAN_POINT('Ctrl Pts',(54.2356327998561,30.842504421852,8.66146730473609));
#44841=CARTESIAN_POINT('Ctrl Pts',(54.2423111783236,30.8452607968761,8.66101019123223));
#44842=CARTESIAN_POINT('Ctrl Pts',(54.2562805984109,30.850937789961,8.66005358964875));
#44843=CARTESIAN_POINT('Ctrl Pts',(54.2635741977936,30.8538517431473,8.65955388812169));
#44844=CARTESIAN_POINT('Ctrl Pts',(54.280910485703,30.8606595198192,8.65836545713902));
#44845=CARTESIAN_POINT('Ctrl Pts',(54.2909677972855,30.8645151933663,8.65767547204381));
#44846=CARTESIAN_POINT('Ctrl Pts',(54.3248541483644,30.8771923918364,8.65534859114199));
#44847=CARTESIAN_POINT('Ctrl Pts',(54.3488195995829,30.8856397282705,8.65369944859847));
#44848=CARTESIAN_POINT('Ctrl Pts',(54.4064734948597,30.9047314058389,8.6497220334942));
#44849=CARTESIAN_POINT('Ctrl Pts',(54.4402952497117,30.9149427618275,8.64738057799504));
#44850=CARTESIAN_POINT('Ctrl Pts',(54.5736023822089,30.9513571563533,8.63811953590363));
#44851=CARTESIAN_POINT('Ctrl Pts',(54.6747737088761,30.9707443300508,8.6310108081723));
#44852=CARTESIAN_POINT('Ctrl Pts',(54.8996009405477,30.9960397037425,8.61525124741179));
#44853=CARTESIAN_POINT('Ctrl Pts',(55.0232507299588,30.9984291764641,8.60660599183199));
#44854=CARTESIAN_POINT('Ctrl Pts',(55.1620370968349,30.9882201509278,8.59739066796584));
#44855=CARTESIAN_POINT('Ctrl Pts',(55.1777235629555,30.9868794028054,8.59635645810611));
#44856=CARTESIAN_POINT('Ctrl Pts',(55.1998163590217,30.9847273452906,8.59491178287156));
#44857=CARTESIAN_POINT('Ctrl Pts',(55.2062366693476,30.9840704754294,8.59449337154652));
#44858=CARTESIAN_POINT('Ctrl Pts',(55.2170380221741,30.9829123787833,8.59379196755199));
#44859=CARTESIAN_POINT('Ctrl Pts',(55.2214207578804,30.9824277677278,8.59350806660202));
#44860=CARTESIAN_POINT('Ctrl Pts',(55.2303699059257,30.9814081876884,8.59292984374982));
#44861=CARTESIAN_POINT('Ctrl Pts',(55.2349361294475,30.9808719584848,8.59263559335114));
#44862=CARTESIAN_POINT('Ctrl Pts',(55.2465823859333,30.9794634565763,8.59188700574447));
#44863=CARTESIAN_POINT('Ctrl Pts',(55.2536597404976,30.9785689749672,8.59143389165318));
#44864=CARTESIAN_POINT('Ctrl Pts',(55.2825297241546,30.974762746517,8.58959233233629));
#44865=CARTESIAN_POINT('Ctrl Pts',(55.3042792422954,30.9715286421758,8.58822077327159));
#44866=CARTESIAN_POINT('Ctrl Pts',(55.3616778719469,30.9620210440397,8.5846324839403));
#44867=CARTESIAN_POINT('Ctrl Pts',(55.3972184337046,30.955135617987,8.58244280888315));
#44868=CARTESIAN_POINT('Ctrl Pts',(55.6113225591814,30.9075763184457,8.56934198057138));
#44869=CARTESIAN_POINT('Ctrl Pts',(55.7837735871049,30.8434395724339,8.55908946026871));
#44870=CARTESIAN_POINT('Ctrl Pts',(55.9908376815435,30.7320422013397,8.54494961267907));
#44871=CARTESIAN_POINT('Ctrl Pts',(56.0356303515982,30.7056372924828,8.54177499739736));
#44872=CARTESIAN_POINT('Ctrl Pts',(56.0915982838198,30.6696266903828,8.53762933017521));
#44873=CARTESIAN_POINT('Ctrl Pts',(56.1037712780878,30.6616043591768,8.53671643313224));
#44874=CARTESIAN_POINT('Ctrl Pts',(56.1230288067323,30.6486081293023,8.53525369715432));
#44875=CARTESIAN_POINT('Ctrl Pts',(56.1301709406775,30.6437202030156,8.53470707481664));
#44876=CARTESIAN_POINT('Ctrl Pts',(56.1429764983931,30.6348334315156,8.53371942137837));
#44877=CARTESIAN_POINT('Ctrl Pts',(56.1486513424993,30.6308512243852,8.53327902471101));
#44878=CARTESIAN_POINT('Ctrl Pts',(56.1619361021709,30.6214251762926,8.5322415958891));
#44879=CARTESIAN_POINT('Ctrl Pts',(56.169528651239,30.6159572509439,8.53164365092297));
#44880=CARTESIAN_POINT('Ctrl Pts',(56.1914974008431,30.5999000935571,8.52989864322451));
#44881=CARTESIAN_POINT('Ctrl Pts',(56.2057699407662,30.5891712246786,8.52874622329895));
#44882=CARTESIAN_POINT('Ctrl Pts',(56.336317558479,30.4882656098584,8.51802759356464));
#44883=CARTESIAN_POINT('Ctrl Pts',(56.4424020712778,30.385690937642,8.50794672681606));
#44884=CARTESIAN_POINT('Ctrl Pts',(56.5480120447472,30.2581842271216,8.4964171367295));
#44885=CARTESIAN_POINT('Ctrl Pts',(56.559597816621,30.2437939891989,8.49512942679026));
#44886=CARTESIAN_POINT('Ctrl Pts',(56.6007131482481,30.1912483620644,8.49047927739289));
#44887=CARTESIAN_POINT('Ctrl Pts',(56.6290566620034,30.1521848114466,8.48711877522837));
#44888=CARTESIAN_POINT('Ctrl Pts',(56.6705522976385,30.0903980712548,8.48198277974947));
#44889=CARTESIAN_POINT('Ctrl Pts',(56.6847193968599,30.0683789471376,8.48018593036477));
#44890=CARTESIAN_POINT('Ctrl Pts',(56.7211006445427,30.0093095509574,8.47546443273589));
#44891=CARTESIAN_POINT('Ctrl Pts',(56.7425533873057,29.9718032287985,8.47256663411431));
#44892=CARTESIAN_POINT('Ctrl Pts',(56.7667184417699,29.9261773979232,8.46918426654362));
#44893=CARTESIAN_POINT('Ctrl Pts',(56.7706167883617,29.9187027917944,8.46863462902968));
#44894=CARTESIAN_POINT('Ctrl Pts',(56.776924496986,29.9064192296812,8.46773895018348));
#44895=CARTESIAN_POINT('Ctrl Pts',(56.7793619556296,29.9016249333387,8.46739124256643));
#44896=CARTESIAN_POINT('Ctrl Pts',(56.7837137702428,29.8929788619906,8.46676763488132));
#44897=CARTESIAN_POINT('Ctrl Pts',(56.7856350756323,29.889130721446,8.46649131286668));
#44898=CARTESIAN_POINT('Ctrl Pts',(56.7898264203119,29.8806675861137,8.46588630089161));
#44899=CARTESIAN_POINT('Ctrl Pts',(56.7920910610675,29.8760500227428,8.46555794397369));
#44900=CARTESIAN_POINT('Ctrl Pts',(56.7985410065383,29.8627690190155,8.46461837391806));
#44901=CARTESIAN_POINT('Ctrl Pts',(56.8026815926539,29.854083846374,8.46400983650715));
#44902=CARTESIAN_POINT('Ctrl Pts',(56.8315050402309,29.7924811138403,8.45973275047185));
#44903=CARTESIAN_POINT('Ctrl Pts',(56.8539192818499,29.7385267260891,8.45618988373333));
#44904=CARTESIAN_POINT('Ctrl Pts',(56.9062500355181,29.5950866044397,8.44709999805547));
#44905=CARTESIAN_POINT('Ctrl Pts',(56.932245405664,29.5043279932132,8.44166691345847));
#44906=CARTESIAN_POINT('Ctrl Pts',(56.9787132256952,29.2842368042079,8.42858758735995));
#44907=CARTESIAN_POINT('Ctrl Pts',(56.9930751777289,29.1540825538138,8.42091109011923));
#44908=CARTESIAN_POINT('Ctrl Pts',(56.9947974714085,29.0076996463334,8.41182619130378));
#44909=CARTESIAN_POINT('Ctrl Pts',(56.9947960021885,28.9919300558255,8.41084206442606));
#44910=CARTESIAN_POINT('Ctrl Pts',(56.9944897664339,28.9663057357634,8.40923338300949));
#44911=CARTESIAN_POINT('Ctrl Pts',(56.99429890841,28.9564501413433,8.40861235782462));
#44912=CARTESIAN_POINT('Ctrl Pts',(56.9938284126205,28.9388822819454,8.40750110094649));
#44913=CARTESIAN_POINT('Ctrl Pts',(56.9935770518839,28.931169411457,8.40701175694995));
#44914=CARTESIAN_POINT('Ctrl Pts',(56.9929517391726,28.9148851690452,8.4059754212361));
#44915=CARTESIAN_POINT('Ctrl Pts',(56.9925672310889,28.906314382412,8.40542811109744));
#44916=CARTESIAN_POINT('Ctrl Pts',(56.9913976589648,28.8835285059193,8.40396797809907));
#44917=CARTESIAN_POINT('Ctrl Pts',(56.9905156941617,28.8693190945943,8.40305216454925));
#44918=CARTESIAN_POINT('Ctrl Pts',(56.9855071615004,28.8005419816199,8.39859302286931));
#44919=CARTESIAN_POINT('Ctrl Pts',(56.9792887277719,28.7461548352643,8.39498539362176));
#44920=CARTESIAN_POINT('Ctrl Pts',(56.9393896668113,28.4907673758662,8.37764757653191));
#44921=CARTESIAN_POINT('Ctrl Pts',(56.8772836977574,28.2954905515171,8.36305632880771));
#44922=CARTESIAN_POINT('Ctrl Pts',(56.7721120674023,28.0836361336892,8.34709360829288));
#44923=CARTESIAN_POINT('Ctrl Pts',(56.7568000917467,28.0546124354514,8.3449076875678));
#44924=CARTESIAN_POINT('Ctrl Pts',(56.7366419769971,28.0185857366959,8.34220743457325));
#44925=CARTESIAN_POINT('Ctrl Pts',(56.7324587430085,28.0112199322495,8.34165606389915));
#44926=CARTESIAN_POINT('Ctrl Pts',(56.725760404761,27.9995985716569,8.34078753395666));
#44927=CARTESIAN_POINT('Ctrl Pts',(56.7232762421965,27.9953254323746,8.3404684786106));
#44928=CARTESIAN_POINT('Ctrl Pts',(56.7188086205444,27.9877057637038,8.3399001526055));
#44929=CARTESIAN_POINT('Ctrl Pts',(56.716831268837,27.9843558253007,8.33965050553661));
#44930=CARTESIAN_POINT('Ctrl Pts',(56.7120756572793,27.9763526602667,8.33905457393747));
#44931=CARTESIAN_POINT('Ctrl Pts',(56.7092882235913,27.9717049534576,8.33870888604583));
#44932=CARTESIAN_POINT('Ctrl Pts',(56.7008048678788,27.9576897996132,8.33766746427776));
#44933=CARTESIAN_POINT('Ctrl Pts',(56.6950505187952,27.9483577110346,8.33697538272542));
#44934=CARTESIAN_POINT('Ctrl Pts',(56.6815677575474,27.9268903077562,8.3353853345737));
#44935=CARTESIAN_POINT('Ctrl Pts',(56.6737843309387,27.9147900784078,8.33449059586083));
#44936=CARTESIAN_POINT('Ctrl Pts',(56.6467398710512,27.8737296251712,8.33145577675558));
#44937=CARTESIAN_POINT('Ctrl Pts',(56.6268518324997,27.845188087313,8.32934853542777));
#44938=CARTESIAN_POINT('Ctrl Pts',(56.5101896246053,27.6867651009654,8.31757769673423));
#44939=CARTESIAN_POINT('Ctrl Pts',(56.3986247380188,27.5685273320437,8.30845360514863));
#44940=CARTESIAN_POINT('Ctrl Pts',(56.222803197247,27.4225958348863,8.29489106082445));
#44941=CARTESIAN_POINT('Ctrl Pts',(56.1695344379213,27.3827061366246,8.29087672061366));
#44942=CARTESIAN_POINT('Ctrl Pts',(56.0980470617953,27.3345547603204,8.28554138469478));
#44943=CARTESIAN_POINT('Ctrl Pts',(56.0815560081281,27.3237984146603,8.28431416109304));
#44944=CARTESIAN_POINT('Ctrl Pts',(56.0566836759589,27.3080952175748,8.28246714045477));
#44945=CARTESIAN_POINT('Ctrl Pts',(56.0484207110797,27.3029625251493,8.28185416932386));
#44946=CARTESIAN_POINT('Ctrl Pts',(56.0335478042022,27.2938740276097,8.28075182676299));
#44947=CARTESIAN_POINT('Ctrl Pts',(56.0269518233965,27.2898956619678,8.28026328863778));
#44948=CARTESIAN_POINT('Ctrl Pts',(56.0128954408432,27.2815282054937,8.27922282194575));
#44949=CARTESIAN_POINT('Ctrl Pts',(56.0054292015416,27.2771492811587,8.27867053928193));
#44950=CARTESIAN_POINT('Ctrl Pts',(55.9853076387526,27.2655233952203,8.27718300540029));
#44951=CARTESIAN_POINT('Ctrl Pts',(55.9726011414008,27.2583665033544,8.27624456233005));
#44952=CARTESIAN_POINT('Ctrl Pts',(55.9079798444097,27.2228964849301,8.27147557734829));
#44953=CARTESIAN_POINT('Ctrl Pts',(55.8549075095272,27.1967650584404,8.26756938521929));
#44954=CARTESIAN_POINT('Ctrl Pts',(55.6876709633612,27.1234655668044,8.25528528327806));
#44955=CARTESIAN_POINT('Ctrl Pts',(55.5702376308585,27.0845116853745,8.24667470788412));
#44956=CARTESIAN_POINT('Ctrl Pts',(55.401437341854,27.0454264671311,8.23460684890185));
#44957=CARTESIAN_POINT('Ctrl Pts',(55.3524953532946,27.0360099284948,8.23114633076581));
#44958=CARTESIAN_POINT('Ctrl Pts',(55.2485069064231,27.0200152378205,8.22392942381763));
#44959=CARTESIAN_POINT('Ctrl Pts',(55.1934305756995,27.0138778595804,8.22018606778666));
#44960=CARTESIAN_POINT('Ctrl Pts',(55.1291559800636,27.0094151981833,8.21595987885241));
#44961=CARTESIAN_POINT('Ctrl Pts',(55.1201423807294,27.0088508503753,8.21537047148527));
#44962=CARTESIAN_POINT('Ctrl Pts',(55.1055739511626,27.0080379988359,8.21442341772966));
#44963=CARTESIAN_POINT('Ctrl Pts',(55.1000214900196,27.0077514772047,8.21406377793684));
#44964=CARTESIAN_POINT('Ctrl Pts',(55.0901590856073,27.0072838865674,8.21342739056677));
#44965=CARTESIAN_POINT('Ctrl Pts',(55.0858496812303,27.0070935789836,8.21315014147792));
#44966=CARTESIAN_POINT('Ctrl Pts',(55.0765388023001,27.0067126590164,8.21255290892033));
#44967=CARTESIAN_POINT('Ctrl Pts',(55.0715372215094,27.0065268902636,8.21223319503527));
#44968=CARTESIAN_POINT('Ctrl Pts',(55.0575609893412,27.0060604532007,8.21134275398049));
#44969=CARTESIAN_POINT('Ctrl Pts',(55.0485849304879,27.0058215487369,8.21077428342502));
#44970=CARTESIAN_POINT('Ctrl Pts',(54.9952126091148,27.0047615893928,8.20741273008998));
#44971=CARTESIAN_POINT('Ctrl Pts',(54.9507969406287,27.0053624482015,8.20469178018524));
#44972=CARTESIAN_POINT('Ctrl Pts',(54.8005753961197,27.0124164654871,8.19563782833387));
#44973=CARTESIAN_POINT('Ctrl Pts',(54.6952727551984,27.0258158428439,8.18953468951974));
#44974=CARTESIAN_POINT('Ctrl Pts',(54.4602159764818,27.0749914084892,8.17557762138048));
#44975=CARTESIAN_POINT('Ctrl Pts',(54.3320297671583,27.1156343574414,8.16770877327091));
#44976=CARTESIAN_POINT('Ctrl Pts',(54.1944626067768,27.1750659146981,8.15840843936318));
#44977=CARTESIAN_POINT('Ctrl Pts',(54.180099703904,27.1814735662994,8.15742690382859));
#44978=CARTESIAN_POINT('Ctrl Pts',(54.1568717847352,27.1921672381511,8.15582162321066));
#44979=CARTESIAN_POINT('Ctrl Pts',(54.1479599190364,27.1963503175325,8.15520138250034));
#44980=CARTESIAN_POINT('Ctrl Pts',(54.1321195658418,27.203929109405,8.15409099906686));
#44981=CARTESIAN_POINT('Ctrl Pts',(54.1251790819601,27.2072993973665,8.15360173873721));
#44982=CARTESIAN_POINT('Ctrl Pts',(54.118152524075,27.2107620041935,8.15310357690825));
#44983=CARTESIAN_POINT('Ctrl Pts',(54.1180466490105,27.2108141898865,8.15309607002942));
#44984=CARTESIAN_POINT('Ctrl Pts',(54.1177887596464,27.2109413316997,8.15307778325715));
#44985=CARTESIAN_POINT('Ctrl Pts',(54.1176367502749,27.2110162977933,8.1530670030174));
#44986=CARTESIAN_POINT('Ctrl Pts',(54.1173457965148,27.211159832859,8.15304636649674));
#44987=CARTESIAN_POINT('Ctrl Pts',(54.117206850563,27.211228398645,8.15303651032698));
#44988=CARTESIAN_POINT('Ctrl Pts',(54.1169408917992,27.2113596800952,8.15301764230519));
#44989=CARTESIAN_POINT('Ctrl Pts',(54.1168138775863,27.2114223931455,8.15300863053929));
#44990=CARTESIAN_POINT('Ctrl Pts',(54.1165707474469,27.2115424704492,8.15299137844165));
#44991=CARTESIAN_POINT('Ctrl Pts',(54.1164546304108,27.2115998324896,8.15298313818617));
#44992=CARTESIAN_POINT('Ctrl Pts',(54.116232349553,27.2117096665957,8.15296736249361));
#44993=CARTESIAN_POINT('Ctrl Pts',(54.1161261847943,27.211762136818,8.15295982711954));
#44994=CARTESIAN_POINT('Ctrl Pts',(54.1159229451708,27.2118626072496,8.15294540029001));
#44995=CARTESIAN_POINT('Ctrl Pts',(54.1158258697616,27.2119106058016,8.15293850890411));
#44996=CARTESIAN_POINT('Ctrl Pts',(54.1156400217996,27.2120025164262,8.15292531449426));
#44997=CARTESIAN_POINT('Ctrl Pts',(54.1155512484882,27.2120464272644,8.15291901150686));
#44998=CARTESIAN_POINT('Ctrl Pts',(54.1153812861664,27.212130513197,8.15290694313924));
#44999=CARTESIAN_POINT('Ctrl Pts',(54.1153000965344,27.2121706872541,8.15290117779046));
#45000=CARTESIAN_POINT('Ctrl Pts',(54.1151446458352,27.2122476201745,8.15289013835576));
#45001=CARTESIAN_POINT('Ctrl Pts',(54.1150703843588,27.2122843781163,8.15288486430396));
#45002=CARTESIAN_POINT('Ctrl Pts',(54.1149281918077,27.212354771609,8.15287476516567));
#45003=CARTESIAN_POINT('Ctrl Pts',(54.1148602604231,27.2123884063735,8.15286994010999));
#45004=CARTESIAN_POINT('Ctrl Pts',(54.1147301823403,27.2124528209722,8.15286070035654));
#45005=CARTESIAN_POINT('Ctrl Pts',(54.114668035342,27.2124836001691,8.15285628568162));
#45006=CARTESIAN_POINT('Ctrl Pts',(54.1145490285704,27.2125425477173,8.15284783148068));
#45007=CARTESIAN_POINT('Ctrl Pts',(54.1144921683139,27.2125707156508,8.15284379195728));
#45008=CARTESIAN_POINT('Ctrl Pts',(54.1143832798162,27.2126246642626,8.15283605582754));
#45009=CARTESIAN_POINT('Ctrl Pts',(54.1143312516281,27.212650444365,8.15283235925588));
#45010=CARTESIAN_POINT('Ctrl Pts',(54.1141982389485,27.212716359727,8.1528229083778));
#45011=CARTESIAN_POINT('Ctrl Pts',(54.1141172559033,27.2127564982966,8.15281715394772));
#45012=CARTESIAN_POINT('Ctrl Pts',(54.1139568574756,27.2128360120172,8.15280575571763));
#45013=CARTESIAN_POINT('Ctrl Pts',(54.1138774419861,27.2128753869593,8.15280011192473));
#45014=CARTESIAN_POINT('Ctrl Pts',(54.1137201416349,27.2129533910067,8.15278893238084));
#45015=CARTESIAN_POINT('Ctrl Pts',(54.1136422566119,27.2129920199411,8.15278339663249));
#45016=CARTESIAN_POINT('Ctrl Pts',(54.1134879809048,27.2130685492242,8.15277243064033));
#45017=CARTESIAN_POINT('Ctrl Pts',(54.1134115901486,27.2131064493683,8.15276700040491));
#45018=CARTESIAN_POINT('Ctrl Pts',(54.1051878579613,27.2171871896666,8.15218237959018));
#45019=CARTESIAN_POINT('Ctrl Pts',(54.0970683729949,27.221285644437,8.15160126197576));
#45020=CARTESIAN_POINT('Ctrl Pts',(54.0739685122751,27.2331446351095,8.14993663567994));
#45021=CARTESIAN_POINT('Ctrl Pts',(54.0590584667462,27.2410397392601,8.1488484488452));
#45022=CARTESIAN_POINT('Ctrl Pts',(54.0256560441113,27.2592730805417,8.1463788285868));
#45023=CARTESIAN_POINT('Ctrl Pts',(54.0072248494119,27.2697185788375,8.1449937227598));
#45024=CARTESIAN_POINT('Ctrl Pts',(53.9485953074711,27.3041908283477,8.14051426695418));
#45025=CARTESIAN_POINT('Ctrl Pts',(53.9090777232144,27.3293388741704,8.13738175681123));
#45026=CARTESIAN_POINT('Ctrl Pts',(53.7076371806353,27.4677268950455,8.1208183630309));
#45027=CARTESIAN_POINT('Ctrl Pts',(53.5623375767471,27.6031548623208,8.10665155905615));
#45028=CARTESIAN_POINT('Ctrl Pts',(53.4251585275416,27.7754925464801,8.09193658266342));
#45029=CARTESIAN_POINT('Ctrl Pts',(53.4113076380329,27.7935171566382,8.09043381708143));
#45030=CARTESIAN_POINT('Ctrl Pts',(53.3933093289834,27.8177865439424,8.08846221613078));
#45031=CARTESIAN_POINT('Ctrl Pts',(53.3888852563978,27.8238227789836,8.08797601528031));
#45032=CARTESIAN_POINT('Ctrl Pts',(53.3817529677131,27.833669875875,8.08718980179458));
#45033=CARTESIAN_POINT('Ctrl Pts',(53.3790240423468,27.8374655438449,8.08688840760071));
#45034=CARTESIAN_POINT('Ctrl Pts',(53.373744935414,27.8448629939448,8.08630429009437));
#45035=CARTESIAN_POINT('Ctrl Pts',(53.3711933406214,27.848463676389,8.08602147639216));
#45036=CARTESIAN_POINT('Ctrl Pts',(53.3650617392373,27.857177439294,8.08534060854149));
#45037=CARTESIAN_POINT('Ctrl Pts',(53.3614937026915,27.8622989681191,8.08494336001744));
#45038=CARTESIAN_POINT('Ctrl Pts',(53.3491172110995,27.8802430701113,8.08356142502039));
#45039=CARTESIAN_POINT('Ctrl Pts',(53.3404344990017,27.8931522473017,8.08258477761368));
#45040=CARTESIAN_POINT('Ctrl Pts',(53.2881647674047,27.9728632955881,8.07665212271868));
#45041=CARTESIAN_POINT('Ctrl Pts',(53.2484610732735,28.0421357450481,8.07191177482973));
#45042=CARTESIAN_POINT('Ctrl Pts',(53.1555421411716,28.2294626789315,8.05966272425286));
#45043=CARTESIAN_POINT('Ctrl Pts',(53.1094790196468,28.3506288573462,8.05227533838761));
#45044=CARTESIAN_POINT('Ctrl Pts',(53.0620083681325,28.5247786913044,8.04153445069465));
#45045=CARTESIAN_POINT('Ctrl Pts',(53.0504549522644,28.5746526538862,8.03844809372298));
#45046=CARTESIAN_POINT('Ctrl Pts',(53.0358931407055,28.650712418942,8.0336899774711));
#45047=CARTESIAN_POINT('Ctrl Pts',(53.0314640679572,28.6766058846017,8.03206141837956));
#45048=CARTESIAN_POINT('Ctrl Pts',(53.0260399462113,28.7125777836419,8.02978374256859));
#45049=CARTESIAN_POINT('Ctrl Pts',(53.0246082386157,28.7225883789649,8.02914827043418));
#45050=CARTESIAN_POINT('Ctrl Pts',(53.0222734521298,28.7398488241723,8.02804960786271));
#45051=CARTESIAN_POINT('Ctrl Pts',(53.0213339623722,28.7470936108333,8.02758756357256));
#45052=CARTESIAN_POINT('Ctrl Pts',(53.0195267044595,28.7616569670688,8.02665689313479));
#45053=CARTESIAN_POINT('Ctrl Pts',(53.0186596562856,28.7689755084668,8.0261882522436));
#45054=CARTESIAN_POINT('Ctrl Pts',(53.0169832861877,28.7838294399719,8.02523509241176));
#45055=CARTESIAN_POINT('Ctrl Pts',(53.0161763134885,28.7913649681525,8.02475050811267));
#45056=CARTESIAN_POINT('Ctrl Pts',(53.0144150978591,28.8087462250547,8.02363031446452));
#45057=CARTESIAN_POINT('Ctrl Pts',(53.0134911172677,28.8185947546147,8.02299377249657));
#45058=CARTESIAN_POINT('Ctrl Pts',(53.010721092675,28.8506846536523,8.02091358617041));
#45059=CARTESIAN_POINT('Ctrl Pts',(53.0091751042848,28.8729495691398,8.01946071785727));
#45060=CARTESIAN_POINT('Ctrl Pts',(53.0061451499444,28.930560992448,8.01567552951475));
#45061=CARTESIAN_POINT('Ctrl Pts',(53.0052274032376,28.9659278090522,8.01332666869485));
#45062=CARTESIAN_POINT('Ctrl Pts',(53.0052504224343,29.0012981915817,8.01095242425188));
#45063=CARTESIAN_POINT('Ctrl Pts',(53.0052504239928,29.0013005840736,8.01095226365531));
#45064=CARTESIAN_POINT('Ctrl Pts',(53.0053388406021,29.1369081142874,8.00184957505844));
#45065=CARTESIAN_POINT('Ctrl Pts',(53.0192545284315,29.2719898001661,7.99237942723991));
#45066=CARTESIAN_POINT('Ctrl Pts',(53.0466869993245,29.4044698800804,7.98296685046478));
#45067=CARTESIAN_POINT('',(53.0052501027731,29.0006399384729,7.85153510469012));
#45068=CARTESIAN_POINT('Ctrl Pts',(53.0466869980082,29.4044698737233,7.82538782795619));
#45069=CARTESIAN_POINT('Ctrl Pts',(53.0325529122127,29.3362119011294,7.82984329733494));
#45070=CARTESIAN_POINT('Ctrl Pts',(53.0220201571551,29.2673051406182,7.83429876671369));
#45071=CARTESIAN_POINT('Ctrl Pts',(53.0151170648001,29.1981597740513,7.83875423609244));
#45072=CARTESIAN_POINT('Ctrl Pts',(53.0120643951503,29.1675824688255,7.84072452353009));
#45073=CARTESIAN_POINT('Ctrl Pts',(53.0097208440697,29.1369585167129,7.84269481096774));
#45074=CARTESIAN_POINT('Ctrl Pts',(53.0080856139562,29.1063232861218,7.84466509840538));
#45075=CARTESIAN_POINT('Ctrl Pts',(53.0062072319163,29.0711327239763,7.846928359402));
#45076=CARTESIAN_POINT('Ctrl Pts',(53.0052613253156,29.035891947952,7.84919162039861));
#45077=CARTESIAN_POINT('Ctrl Pts',(53.0052501010842,29.0006350396436,7.85145488139523));
#45078=CARTESIAN_POINT('Ctrl Pts',(53.0052501373994,29.0007403748082,7.85317985144906));
#45079=CARTESIAN_POINT('Ctrl Pts',(53.0051782706844,28.8071139598332,7.86510701368834));
#45080=CARTESIAN_POINT('Ctrl Pts',(53.0332974065051,28.6144740104776,7.87586527852367));
#45081=CARTESIAN_POINT('Ctrl Pts',(53.1028854012033,28.3816000185706,7.8902825160751));
#45082=CARTESIAN_POINT('Ctrl Pts',(53.1187615718485,28.3348655761312,7.8932454082853));
#45083=CARTESIAN_POINT('Ctrl Pts',(53.144185645828,28.2682464831858,7.89760280475556));
#45084=CARTESIAN_POINT('Ctrl Pts',(53.1523563722456,28.2478543390825,7.89895512368827));
#45085=CARTESIAN_POINT('Ctrl Pts',(53.1676432792812,28.2114550641497,7.90140513167815));
#45086=CARTESIAN_POINT('Ctrl Pts',(53.1746367592018,28.1953986847102,7.90249874781297));
#45087=CARTESIAN_POINT('Ctrl Pts',(53.1856602556443,28.1709734176104,7.90418312755723));
#45088=CARTESIAN_POINT('Ctrl Pts',(53.1895389310317,28.1625368692697,7.90476874941434));
#45089=CARTESIAN_POINT('Ctrl Pts',(53.1966988743869,28.1472454250324,7.90583733585362));
#45090=CARTESIAN_POINT('Ctrl Pts',(53.1999606997407,28.140381579019,7.90631962649599));
#45091=CARTESIAN_POINT('Ctrl Pts',(53.2071495128054,28.1254745252446,7.90737291391453));
#45092=CARTESIAN_POINT('Ctrl Pts',(53.2110915602217,28.117438803687,7.90794442285225));
#45093=CARTESIAN_POINT('Ctrl Pts',(53.2220131414629,28.0955493770993,7.90951159337613));
#45094=CARTESIAN_POINT('Ctrl Pts',(53.2291002934953,28.0817503577574,7.91051097372083));
#45095=CARTESIAN_POINT('Ctrl Pts',(53.267065447613,28.0099049663438,7.91577573055826));
#45096=CARTESIAN_POINT('Ctrl Pts',(53.3006353222276,27.9533346262717,7.92013508337376));
#45097=CARTESIAN_POINT('Ctrl Pts',(53.4216680174323,27.7705921592164,7.93495338316444));
#45098=CARTESIAN_POINT('Ctrl Pts',(53.5208794188734,27.6528665181079,7.94578731747667));
#45099=CARTESIAN_POINT('Ctrl Pts',(53.6655955949209,27.5166090843662,7.95949451744284));
#45100=CARTESIAN_POINT('Ctrl Pts',(53.6996621998492,27.4866573860359,7.96259124876788));
#45101=CARTESIAN_POINT('Ctrl Pts',(53.748040437147,27.4469637482342,7.96678347572212));
#45102=CARTESIAN_POINT('Ctrl Pts',(53.7615001675755,27.4362089158825,7.96792891741035));
#45103=CARTESIAN_POINT('Ctrl Pts',(53.7820324435844,27.4202342616527,7.96964291392799));
#45104=CARTESIAN_POINT('Ctrl Pts',(53.7890025832364,27.41488485604,7.97021908548508));
#45105=CARTESIAN_POINT('Ctrl Pts',(53.8004147631619,27.4062455110561,7.97115293232619));
#45106=CARTESIAN_POINT('Ctrl Pts',(53.8048354498848,27.4029277375999,7.97151237250194));
#45107=CARTESIAN_POINT('Ctrl Pts',(53.8133507818529,27.3965920456828,7.97220024909773));
#45108=CARTESIAN_POINT('Ctrl Pts',(53.817443286168,27.3935713352731,7.97252886980725));
#45109=CARTESIAN_POINT('Ctrl Pts',(53.8215671025125,27.3905518121983,7.97285798786338));
#45110=CARTESIAN_POINT('Ctrl Pts',(53.8215868514777,27.3905373522542,7.97285956396411));
#45111=CARTESIAN_POINT('Ctrl Pts',(53.8216264999087,27.3905083232925,7.97286272808345));
#45112=CARTESIAN_POINT('Ctrl Pts',(53.8216463995561,27.3904937541503,7.97286431611587));
#45113=CARTESIAN_POINT('Ctrl Pts',(53.8216863529331,27.3904645041958,7.97286750438227));
#45114=CARTESIAN_POINT('Ctrl Pts',(53.8217064060929,27.3904498238094,7.97286910457007));
#45115=CARTESIAN_POINT('Ctrl Pts',(53.8217466692585,27.3904203493695,7.97287231736561));
#45116=CARTESIAN_POINT('Ctrl Pts',(53.821766879252,27.3904055553339,7.97287392997161));
#45117=CARTESIAN_POINT('Ctrl Pts',(53.8218074584304,27.3903758519061,7.97287716778841));
#45118=CARTESIAN_POINT('Ctrl Pts',(53.8218278282283,27.3903609420743,7.97287879304737));
#45119=CARTESIAN_POINT('Ctrl Pts',(53.8218687300298,27.3903310048753,7.97288205640828));
#45120=CARTESIAN_POINT('Ctrl Pts',(53.8218892623325,27.3903159772987,7.97288369453331));
#45121=CARTESIAN_POINT('Ctrl Pts',(53.8219304931214,27.3902858017273,7.97288698394135));
#45122=CARTESIAN_POINT('Ctrl Pts',(53.8219511907179,27.3902706543934,7.97288863515258));
#45123=CARTESIAN_POINT('Ctrl Pts',(53.8219927549243,27.3902402372659,7.9728919509563));
#45124=CARTESIAN_POINT('Ctrl Pts',(53.8220136217205,27.3902249673459,7.97289361556285));
#45125=CARTESIAN_POINT('Ctrl Pts',(53.8220555274688,27.3901943027767,7.97289695840539));
#45126=CARTESIAN_POINT('Ctrl Pts',(53.822076566187,27.3901789083088,7.97289863662187));
#45127=CARTESIAN_POINT('Ctrl Pts',(53.8221188190231,27.3901479923014,7.97290200694048));
#45128=CARTESIAN_POINT('Ctrl Pts',(53.8221400331938,27.3901324707336,7.97290369904594));
#45129=CARTESIAN_POINT('Ctrl Pts',(53.8255303786376,27.3876519922626,7.97317411455021));
#45130=CARTESIAN_POINT('Ctrl Pts',(53.8289071945918,27.3851976494757,7.9734420951267));
#45131=CARTESIAN_POINT('Ctrl Pts',(53.8366602707974,27.3795996576406,7.97405429305732));
#45132=CARTESIAN_POINT('Ctrl Pts',(53.8410415739903,27.3764631314709,7.97439802400921));
#45133=CARTESIAN_POINT('Ctrl Pts',(53.8539702548244,27.3672866381343,7.97540597571461));
#45134=CARTESIAN_POINT('Ctrl Pts',(53.8625526759578,27.3612960319134,7.97606695682257));
#45135=CARTESIAN_POINT('Ctrl Pts',(53.9603845055397,27.2941474745379,7.98351481198376));
#45136=CARTESIAN_POINT('Ctrl Pts',(54.0544340146758,27.2402713392987,7.98986678760313));
#45137=CARTESIAN_POINT('Ctrl Pts',(54.2264966772028,27.1595055463054,8.00093123807221));
#45138=CARTESIAN_POINT('Ctrl Pts',(54.302661490933,27.1293193840149,8.00565499964381));
#45139=CARTESIAN_POINT('Ctrl Pts',(54.4614270214716,27.0774439892774,8.01547184908633));
#45140=CARTESIAN_POINT('Ctrl Pts',(54.5439930987406,27.0562053290519,8.02056280009881));
#45141=CARTESIAN_POINT('Ctrl Pts',(54.6488427362445,27.0362838424559,8.02715552292962));
#45142=CARTESIAN_POINT('Ctrl Pts',(54.6700910034197,27.0326025898979,8.02849769562327));
#45143=CARTESIAN_POINT('Ctrl Pts',(54.7013608619136,27.0277059045726,8.03048363336539));
#45144=CARTESIAN_POINT('Ctrl Pts',(54.7113391168775,27.0262208273878,8.03111894207711));
#45145=CARTESIAN_POINT('Ctrl Pts',(54.7289981545191,27.0237293799725,8.03224627515015));
#45146=CARTESIAN_POINT('Ctrl Pts',(54.7366743948,27.0226919342857,8.03273731493095));
#45147=CARTESIAN_POINT('Ctrl Pts',(54.7527468917203,27.0206149846569,8.03376762320148));
#45148=CARTESIAN_POINT('Ctrl Pts',(54.76114409241,27.0195841370265,8.0343071522992));
#45149=CARTESIAN_POINT('Ctrl Pts',(54.7831508070464,27.017024573152,8.03572446486952));
#45150=CARTESIAN_POINT('Ctrl Pts',(54.7967697666477,27.0155825608502,8.03660493527909));
#45151=CARTESIAN_POINT('Ctrl Pts',(54.8537843792192,27.0101387676742,8.04030565199234));
#45152=CARTESIAN_POINT('Ctrl Pts',(54.8972875809921,27.0074196620286,8.04316529798201));
#45153=CARTESIAN_POINT('Ctrl Pts',(55.1332879461497,27.0004175880705,8.05888325087212));
#45154=CARTESIAN_POINT('Ctrl Pts',(55.3255348008295,27.0226031035623,8.07255937847067));
#45155=CARTESIAN_POINT('Ctrl Pts',(55.5643239127779,27.0859609528477,8.08949010822986));
#45156=CARTESIAN_POINT('Ctrl Pts',(55.6164908244172,27.1021203445245,8.09317488126119));
#45157=CARTESIAN_POINT('Ctrl Pts',(55.6768580204353,27.1235724148032,8.09737285986934));
#45158=CARTESIAN_POINT('Ctrl Pts',(55.6857597994288,27.126807332844,8.09799016420973));
#45159=CARTESIAN_POINT('Ctrl Pts',(55.6994294318784,27.1318854012932,8.09893506296532));
#45160=CARTESIAN_POINT('Ctrl Pts',(55.7042136625355,27.1336836273054,8.099265191668));
#45161=CARTESIAN_POINT('Ctrl Pts',(55.7130130637199,27.1370296702158,8.09987124912225));
#45162=CARTESIAN_POINT('Ctrl Pts',(55.7170301215142,27.1385720846138,8.10014747970763));
#45163=CARTESIAN_POINT('Ctrl Pts',(55.7260928516315,27.1420855575564,8.1007696911307));
#45164=CARTESIAN_POINT('Ctrl Pts',(55.7311354977661,27.1440641740094,8.10111521839786));
#45165=CARTESIAN_POINT('Ctrl Pts',(55.7460216969471,27.1499752576161,8.10213339595545));
#45166=CARTESIAN_POINT('Ctrl Pts',(55.7558422175344,27.1539657442208,8.10280270760767));
#45167=CARTESIAN_POINT('Ctrl Pts',(55.8427970332698,27.1901093500087,8.10871176970505));
#45168=CARTESIAN_POINT('Ctrl Pts',(55.9178817307676,27.2270060179964,8.1136943467432));
#45169=CARTESIAN_POINT('Ctrl Pts',(56.0983340129353,27.3302273871267,8.12588862447967));
#45170=CARTESIAN_POINT('Ctrl Pts',(56.2002232800636,27.4018940580011,8.1329906044136));
#45171=CARTESIAN_POINT('Ctrl Pts',(56.3333811355945,27.5155145216936,8.14336211221535));
#45172=CARTESIAN_POINT('Ctrl Pts',(56.3707083773103,27.5499102157675,8.14640577215395));
#45173=CARTESIAN_POINT('Ctrl Pts',(56.4303251666695,27.6092054542406,8.15154095243316));
#45174=CARTESIAN_POINT('Ctrl Pts',(56.4533738396536,27.6333091666162,8.15360023647118));
#45175=CARTESIAN_POINT('Ctrl Pts',(56.4838602010689,27.6668346823559,8.15643386960506));
#45176=CARTESIAN_POINT('Ctrl Pts',(56.4918337919665,27.675763318839,8.1571856827259));
#45177=CARTESIAN_POINT('Ctrl Pts',(56.5050592631595,27.6908439383564,8.15845107151565));
#45178=CARTESIAN_POINT('Ctrl Pts',(56.5103550274791,27.69695715066,8.1589628209023));
#45179=CARTESIAN_POINT('Ctrl Pts',(56.5207072038393,27.7090551732024,8.15997331675761));
#45180=CARTESIAN_POINT('Ctrl Pts',(56.5257658269011,27.7150379055222,8.16047195982389));
#45181=CARTESIAN_POINT('Ctrl Pts',(56.5367973606769,27.7282416692045,8.16157020430357));
#45182=CARTESIAN_POINT('Ctrl Pts',(56.54275486851,27.735475270906,8.16217041239061));
#45183=CARTESIAN_POINT('Ctrl Pts',(56.5633658866787,27.7608636140096,8.16427214928182));
#45184=CARTESIAN_POINT('Ctrl Pts',(56.5777512214011,27.7792326650985,8.16578424756278));
#45185=CARTESIAN_POINT('Ctrl Pts',(56.6905762575426,27.9286283006916,8.17801926972722));
#45186=CARTESIAN_POINT('Ctrl Pts',(56.7728311074475,28.0710572120392,8.18937950248035));
#45187=CARTESIAN_POINT('Ctrl Pts',(56.8443473802909,28.2398741427858,8.20215400905679));
#45188=CARTESIAN_POINT('Ctrl Pts',(56.8516972908301,28.2579584033221,8.20351310807925));
#45189=CARTESIAN_POINT('Ctrl Pts',(56.8884387975637,28.3523069390134,8.21054817692882));
#45190=CARTESIAN_POINT('Ctrl Pts',(56.9133914526277,28.4302252225377,8.21617450750814));
#45191=CARTESIAN_POINT('Ctrl Pts',(56.9373653468214,28.5247202143254,8.22262746872963));
#45192=CARTESIAN_POINT('Ctrl Pts',(56.9410558390742,28.5400243177338,8.22366113555754));
#45193=CARTESIAN_POINT('Ctrl Pts',(56.9459627559037,28.5614845005892,8.22509314792217));
#45194=CARTESIAN_POINT('Ctrl Pts',(56.9473317915747,28.5676045945369,8.2254995597009));
#45195=CARTESIAN_POINT('Ctrl Pts',(56.9496161736368,28.5780475607388,8.2261895558984));
#45196=CARTESIAN_POINT('Ctrl Pts',(56.9505460546672,28.5823671761166,8.22647395165991));
#45197=CARTESIAN_POINT('Ctrl Pts',(56.9523103968837,28.5906975952653,8.22702041769142));
#45198=CARTESIAN_POINT('Ctrl Pts',(56.95314686131,28.5947079038648,8.22728260543257));
#45199=CARTESIAN_POINT('Ctrl Pts',(56.9551296247389,28.6043626834639,8.22791175668868));
#45200=CARTESIAN_POINT('Ctrl Pts',(56.9562638509619,28.6100096371196,8.22827804499206));
#45201=CARTESIAN_POINT('Ctrl Pts',(56.9603353697647,28.6307452221363,8.22961710770363));
#45202=CARTESIAN_POINT('Ctrl Pts',(56.963122772361,28.6458632082343,8.23058186394867));
#45203=CARTESIAN_POINT('Ctrl Pts',(56.9878907333125,28.7894886951186,8.2396511677492));
#45204=CARTESIAN_POINT('Ctrl Pts',(56.9974007269941,28.9198465826145,8.24716799285208));
#45205=CARTESIAN_POINT('Ctrl Pts',(56.9905243007948,29.1929210651952,8.26303145078461));
#45206=CARTESIAN_POINT('Ctrl Pts',(56.9716240657333,29.3348087673227,8.27136104388139));
#45207=CARTESIAN_POINT('Ctrl Pts',(56.9334254809607,29.4911467164158,8.28134020669378));
#45208=CARTESIAN_POINT('Ctrl Pts',(56.9288612492393,29.5087764092044,8.28247669939506));
#45209=CARTESIAN_POINT('Ctrl Pts',(56.9215682140005,29.5354363485407,8.28421340616306));
#45210=CARTESIAN_POINT('Ctrl Pts',(56.9190155971305,29.5445141113622,8.28480796249878));
#45211=CARTESIAN_POINT('Ctrl Pts',(56.91426781817,29.5609503041304,8.28589043878393));
#45212=CARTESIAN_POINT('Ctrl Pts',(56.9120943375698,29.5683148466648,8.28637764973094));
#45213=CARTESIAN_POINT('Ctrl Pts',(56.9073213796683,29.5841500013966,8.28743004810564));
#45214=CARTESIAN_POINT('Ctrl Pts',(56.9047078843137,29.5926161833357,8.28799568191869));
#45215=CARTESIAN_POINT('Ctrl Pts',(56.8974827864586,29.6154796364638,8.28953141865264));
#45216=CARTESIAN_POINT('Ctrl Pts',(56.8927638492993,29.6298421213637,8.29050499746797));
#45217=CARTESIAN_POINT('Ctrl Pts',(56.8684477982419,29.7011079648638,8.29538110489173));
#45218=CARTESIAN_POINT('Ctrl Pts',(56.8464475328608,29.7571524316037,8.29936170931126));
#45219=CARTESIAN_POINT('Ctrl Pts',(56.7668789019433,29.9356622739177,8.31252798930379));
#45220=CARTESIAN_POINT('Ctrl Pts',(56.6993879853999,30.0532795014724,8.32200452630818));
#45221=CARTESIAN_POINT('Ctrl Pts',(56.5724518816859,30.2301303946447,8.33713275703242));
#45222=CARTESIAN_POINT('Ctrl Pts',(56.5202624073695,30.2940752388877,8.34281079875641));
#45223=CARTESIAN_POINT('Ctrl Pts',(56.4535239264509,30.3662158224888,8.34931651813064));
#45224=CARTESIAN_POINT('Ctrl Pts',(56.4426504254366,30.3776927327135,8.35035466028569));
#45225=CARTESIAN_POINT('Ctrl Pts',(56.4272668962547,30.3935480726096,8.35179177111658));
#45226=CARTESIAN_POINT('Ctrl Pts',(56.4228712180596,30.3980359520426,8.35219888079509));
#45227=CARTESIAN_POINT('Ctrl Pts',(56.4153463240153,30.4056464299816,8.35288970286832));
#45228=CARTESIAN_POINT('Ctrl Pts',(56.4122278151736,30.4087795081299,8.35317423128276));
#45229=CARTESIAN_POINT('Ctrl Pts',(56.406201086132,30.4147942707852,8.35372066888673));
#45230=CARTESIAN_POINT('Ctrl Pts',(56.4032943918977,30.4176773870263,8.35398269715249));
#45231=CARTESIAN_POINT('Ctrl Pts',(56.3962839556397,30.4245882705351,8.35461108436352));
#45232=CARTESIAN_POINT('Ctrl Pts',(56.3921716057262,30.4286073104517,8.35497677170313));
#45233=CARTESIAN_POINT('Ctrl Pts',(56.3770535850464,30.4432550280401,8.35631072036938));
#45234=CARTESIAN_POINT('Ctrl Pts',(56.3659427783482,30.453775089757,8.35727104465866));
#45235=CARTESIAN_POINT('Ctrl Pts',(56.2580272130034,30.5536233367732,8.36642076633832));
#45236=CARTESIAN_POINT('Ctrl Pts',(56.1527053856061,30.6332967113054,8.37400961384961));
#45237=CARTESIAN_POINT('Ctrl Pts',(55.9191949633797,30.7760202801605,8.38990375442104));
#45238=CARTESIAN_POINT('Ctrl Pts',(55.7905725054278,30.8368874114338,8.39819027300954));
#45239=CARTESIAN_POINT('Ctrl Pts',(55.6396310435328,30.8895031706067,8.40810494080142));
#45240=CARTESIAN_POINT('Ctrl Pts',(55.6225937989777,30.8951852237519,8.40922600044863));
#45241=CARTESIAN_POINT('Ctrl Pts',(55.5965468996002,30.9034829415232,8.41094388654605));
#45242=CARTESIAN_POINT('Ctrl Pts',(55.5875913838737,30.9062664747814,8.41153524363983));
#45243=CARTESIAN_POINT('Ctrl Pts',(55.5719799154879,30.9109983339104,8.41256748137844));
#45244=CARTESIAN_POINT('Ctrl Pts',(55.5653327611299,30.9129753064665,8.4130074239507));
#45245=CARTESIAN_POINT('Ctrl Pts',(55.5503815434838,30.9173373109663,8.41399799979415));
#45246=CARTESIAN_POINT('Ctrl Pts',(55.5420720624937,30.9197031235706,8.41454924458674));
#45247=CARTESIAN_POINT('Ctrl Pts',(55.5197657845366,30.9258976240372,8.41603105598138));
#45248=CARTESIAN_POINT('Ctrl Pts',(55.5057423516452,30.929627628444,8.41696477198374));
#45249=CARTESIAN_POINT('Ctrl Pts',(55.4420046896465,30.9458382898341,8.4212190800153));
#45250=CARTESIAN_POINT('Ctrl Pts',(55.3918652237134,30.9565519815638,8.42459526557367));
#45251=CARTESIAN_POINT('Ctrl Pts',(55.1793604333108,30.9934636179582,8.43903673866605));
#45252=CARTESIAN_POINT('Ctrl Pts',(55.0145033397704,31.00146012583,8.45063049761431));
#45253=CARTESIAN_POINT('Ctrl Pts',(54.7847139521278,30.984197854818,8.46655766027285));
#45254=CARTESIAN_POINT('Ctrl Pts',(54.7191361735904,30.9759824025713,8.47106545127165));
#45255=CARTESIAN_POINT('Ctrl Pts',(54.6401264777183,30.9620701769926,8.47636372730492));
#45256=CARTESIAN_POINT('Ctrl Pts',(54.6261979584369,30.9594643126329,8.47729262712057));
#45257=CARTESIAN_POINT('Ctrl Pts',(54.6064000915318,30.9555415681116,8.47860452028953));
#45258=CARTESIAN_POINT('Ctrl Pts',(54.6005074787988,30.954346294883,8.47899392175048));
#45259=CARTESIAN_POINT('Ctrl Pts',(54.5903384198048,30.9522356610469,8.47966397008109));
#45260=CARTESIAN_POINT('Ctrl Pts',(54.5860594425998,30.9513328529467,8.47994531507664));
#45261=CARTESIAN_POINT('Ctrl Pts',(54.5771273880849,30.9494176031344,8.48053130959683));
#45262=CARTESIAN_POINT('Ctrl Pts',(54.5724749437298,30.9484025674189,8.48083581107727));
#45263=CARTESIAN_POINT('Ctrl Pts',(54.5601376171116,30.9456645834027,8.48164146642693));
#45264=CARTESIAN_POINT('Ctrl Pts',(54.5524591345759,30.9439127464125,8.48214101142094));
#45265=CARTESIAN_POINT('Ctrl Pts',(54.5195031495712,30.9361882527642,8.48427776483224));
#45266=CARTESIAN_POINT('Ctrl Pts',(54.4943319806861,30.929767389537,8.48589131101878));
#45267=CARTESIAN_POINT('Ctrl Pts',(54.265668734328,30.8666563805137,8.50043977111997));
#45268=CARTESIAN_POINT('Ctrl Pts',(54.0722446236612,30.7784666200613,8.51208338386741));
#45269=CARTESIAN_POINT('Ctrl Pts',(53.8658311991624,30.6413475328652,8.52696109766131));
#45270=CARTESIAN_POINT('Ctrl Pts',(53.8359810413947,30.620314853492,8.52917668332887));
#45271=CARTESIAN_POINT('Ctrl Pts',(53.7858427539271,30.5828862533135,8.53302383471036));
#45272=CARTESIAN_POINT('Ctrl Pts',(53.7652677474955,30.566889554619,8.5346406625211));
#45273=CARTESIAN_POINT('Ctrl Pts',(53.7365561871637,30.543650109021,8.53695483452359));
#45274=CARTESIAN_POINT('Ctrl Pts',(53.7281559159123,30.536736329232,8.53763913457046));
#45275=CARTESIAN_POINT('Ctrl Pts',(53.7137745989997,30.524701207848,8.53882343559457));
#45276=CARTESIAN_POINT('Ctrl Pts',(53.7077664875431,30.5196124840884,8.53932211146326));
#45277=CARTESIAN_POINT('Ctrl Pts',(53.6963210498624,30.5098015166555,8.54027969099137));
#45278=CARTESIAN_POINT('Ctrl Pts',(53.6908788511034,30.5050851271656,8.5407383501809));
#45279=CARTESIAN_POINT('Ctrl Pts',(53.6781644939301,30.4939453139193,8.54181783822952));
#45280=CARTESIAN_POINT('Ctrl Pts',(53.6709134773524,30.4874981398074,8.54243964487541));
#45281=CARTESIAN_POINT('Ctrl Pts',(53.6460419103465,30.4650567727477,8.54459415563102));
#45282=CARTESIAN_POINT('Ctrl Pts',(53.6286612793629,30.4488008449952,8.54613778460997));
#45283=CARTESIAN_POINT('Ctrl Pts',(53.5033168289792,30.3272908985036,8.55755804734225));
#45284=CARTESIAN_POINT('Ctrl Pts',(53.4073247155229,30.2104259018816,8.56796294142006));
#45285=CARTESIAN_POINT('Ctrl Pts',(53.2789883139807,30.0121510594262,8.58442438378906));
#45286=CARTESIAN_POINT('Ctrl Pts',(53.2372074337793,29.9374939929077,8.5903835927923));
#45287=CARTESIAN_POINT('Ctrl Pts',(53.1892904238783,29.8372663513482,8.59791292371472));
#45288=CARTESIAN_POINT('Ctrl Pts',(53.178684409554,29.8139371964776,8.5996335702745));
#45289=CARTESIAN_POINT('Ctrl Pts',(53.1617626335976,29.7747274758743,8.60246547242562));
#45290=CARTESIAN_POINT('Ctrl Pts',(53.155196321472,29.7589589656347,8.60358847458665));
#45291=CARTESIAN_POINT('Ctrl Pts',(53.1464203146975,29.737096914073,8.60512178486127));
#45292=CARTESIAN_POINT('Ctrl Pts',(53.1440367758686,29.7310745680028,8.60554171208159));
#45293=CARTESIAN_POINT('Ctrl Pts',(53.1400621261174,29.7208873306222,8.6062477850384));
#45294=CARTESIAN_POINT('Ctrl Pts',(53.1384555823467,29.7167285543304,8.60653483325504));
#45295=CARTESIAN_POINT('Ctrl Pts',(53.135415809442,29.7087804813747,8.60708110364233));
#45296=CARTESIAN_POINT('Ctrl Pts',(53.1339801667318,29.7049921680535,8.60734047321248));
#45297=CARTESIAN_POINT('Ctrl Pts',(53.130591985456,29.695968717672,8.6079559510489));
#45298=CARTESIAN_POINT('Ctrl Pts',(53.1286498690825,29.6907296650083,8.6083114480895));
#45299=CARTESIAN_POINT('Ctrl Pts',(53.1218496389619,29.6721461567782,8.60956611953298));
#45300=CARTESIAN_POINT('Ctrl Pts',(53.1171119072584,29.6587576882261,8.61045854341411));
#45301=CARTESIAN_POINT('Ctrl Pts',(53.085548406168,29.5664381857209,8.6165408732498));
#45302=CARTESIAN_POINT('Ctrl Pts',(53.0635683757526,29.4859954439104,8.62148610651734));
#45303=CARTESIAN_POINT('Ctrl Pts',(53.0466869433582,29.4044696098012,8.62635914573793));
#45304=CARTESIAN_POINT('Origin',(55.,29.,3.45145488139523));
#45305=CARTESIAN_POINT('',(53.0466870746609,29.4044702439035,9.58304844318572));
#45306=CARTESIAN_POINT('',(53.0466869980009,29.4044698736881,9.42363003822484));
#45307=CARTESIAN_POINT('',(53.0466869980082,29.4044698737233,3.45145488139523));
#45308=CARTESIAN_POINT('Ctrl Pts',(53.0466870746609,29.4044702439035,9.58304844318572));
#45309=CARTESIAN_POINT('Ctrl Pts',(53.0629212292667,29.4828700384529,9.57839245605286));
#45310=CARTESIAN_POINT('Ctrl Pts',(53.0838774118282,29.5603023718,9.57376218584092));
#45311=CARTESIAN_POINT('Ctrl Pts',(53.1356701680259,29.7141753006802,9.56420549992052));
#45312=CARTESIAN_POINT('Ctrl Pts',(53.1666475684883,29.7903092405455,9.55928854534223));
#45313=CARTESIAN_POINT('Ctrl Pts',(53.2113957035532,29.883385594677,9.5529062262179));
#45314=CARTESIAN_POINT('Ctrl Pts',(53.2208681939823,29.9023111447698,9.55158860919816));
#45315=CARTESIAN_POINT('Ctrl Pts',(53.2352630803224,29.9299631278263,9.5496322677227));
#45316=CARTESIAN_POINT('Ctrl Pts',(53.2399531662748,29.9388093267766,9.54900163708479));
#45317=CARTESIAN_POINT('Ctrl Pts',(53.24838463308,29.9544270610249,9.54787960314639));
#45318=CARTESIAN_POINT('Ctrl Pts',(53.2520992072219,29.9612128922966,9.54738915261613));
#45319=CARTESIAN_POINT('Ctrl Pts',(53.2599765092736,29.9754065907911,9.54635703633499));
#45320=CARTESIAN_POINT('Ctrl Pts',(53.2641472788581,29.9828097946619,9.54581509173274));
#45321=CARTESIAN_POINT('Ctrl Pts',(53.2752467853263,30.0022205835238,9.54438448735879));
#45322=CARTESIAN_POINT('Ctrl Pts',(53.2822535229024,30.0141828109329,9.54349304772926));
#45323=CARTESIAN_POINT('Ctrl Pts',(53.3125670569246,30.0647200738163,9.53968431760354));
#45324=CARTESIAN_POINT('Ctrl Pts',(53.337051374791,30.1025697731689,9.53672470203159));
#45325=CARTESIAN_POINT('Ctrl Pts',(53.4793766827536,30.3070492585799,9.52012015679283));
#45326=CARTESIAN_POINT('Ctrl Pts',(53.6209374607404,30.4556209856089,9.5055500372503));
#45327=CARTESIAN_POINT('Ctrl Pts',(53.8049502178952,30.5973991208908,9.48975803476037));
#45328=CARTESIAN_POINT('Ctrl Pts',(53.8277266589832,30.6141881280966,9.48785309992596));
#45329=CARTESIAN_POINT('Ctrl Pts',(53.8658806446695,30.641078555526,9.4847525087568));
#45330=CARTESIAN_POINT('Ctrl Pts',(53.8810539581841,30.6514615801605,9.48354225619057));
#45331=CARTESIAN_POINT('Ctrl Pts',(53.9005940195775,30.6644397780509,9.48201470661506));
#45332=CARTESIAN_POINT('Ctrl Pts',(53.9048294970119,30.6672296948135,9.48168542930842));
#45333=CARTESIAN_POINT('Ctrl Pts',(53.9125030206562,30.6722423993857,9.48109223830474));
#45334=CARTESIAN_POINT('Ctrl Pts',(53.9159373393983,30.6744708032694,9.48082796475142));
#45335=CARTESIAN_POINT('Ctrl Pts',(53.9229247533851,30.6789741734083,9.48029277248145));
#45336=CARTESIAN_POINT('Ctrl Pts',(53.9264781750549,30.6812484212234,9.48002191153501));
#45337=CARTESIAN_POINT('Ctrl Pts',(53.9344251950867,30.6862991753266,9.47941904525199));
#45338=CARTESIAN_POINT('Ctrl Pts',(53.9388224347124,30.689069788366,9.47908742618165));
#45339=CARTESIAN_POINT('Ctrl Pts',(53.9515909899784,30.6970454559404,9.47812998829549));
#45340=CARTESIAN_POINT('Ctrl Pts',(53.959990264535,30.7022057723218,9.47750699795683));
#45341=CARTESIAN_POINT('Ctrl Pts',(54.0166935315869,30.7364665317156,9.4733444223246));
#45342=CARTESIAN_POINT('Ctrl Pts',(54.0661793172897,30.7635724605396,9.46992092134261));
#45343=CARTESIAN_POINT('Ctrl Pts',(54.228078004946,30.8435237755441,9.45916231017186));
#45344=CARTESIAN_POINT('Ctrl Pts',(54.3442983029437,30.8879888685677,9.45207861607605));
#45345=CARTESIAN_POINT('Ctrl Pts',(54.5303026463826,30.939887633603,9.44077206145705));
#45346=CARTESIAN_POINT('Ctrl Pts',(54.5976126791062,30.9549585551151,9.43668973088029));
#45347=CARTESIAN_POINT('Ctrl Pts',(54.7064041304362,30.9734602029374,9.42999577090137));
#45348=CARTESIAN_POINT('Ctrl Pts',(54.7474481387295,30.9791313482567,9.42744941846956));
#45349=CARTESIAN_POINT('Ctrl Pts',(54.8015270885474,30.9848939797551,9.42405381788397));
#45350=CARTESIAN_POINT('Ctrl Pts',(54.8144301621943,30.9861418454432,9.42324065041736));
#45351=CARTESIAN_POINT('Ctrl Pts',(54.8356131613484,30.9879822486269,9.42190039560307));
#45352=CARTESIAN_POINT('Ctrl Pts',(54.843886377314,30.9886490356598,9.42137562978404));
#45353=CARTESIAN_POINT('Ctrl Pts',(54.859944694503,30.9898424451795,9.42035440274547));
#45354=CARTESIAN_POINT('Ctrl Pts',(54.867729209144,30.9903750602085,9.41985813790678));
#45355=CARTESIAN_POINT('Ctrl Pts',(54.8857819108956,30.991503848869,9.41870438085794));
#45356=CARTESIAN_POINT('Ctrl Pts',(54.8960519117186,30.9920662991893,9.41804585208336));
#45357=CARTESIAN_POINT('Ctrl Pts',(54.9295570385912,30.9936414527312,9.41589013576712));
#45358=CARTESIAN_POINT('Ctrl Pts',(54.9528049011314,30.9943272048731,9.4143828805405));
#45359=CARTESIAN_POINT('Ctrl Pts',(55.1406846059619,30.9965823330495,9.40210430218785));
#45360=CARTESIAN_POINT('Ctrl Pts',(55.3048925877464,30.9781690635832,9.39068893716648));
#45361=CARTESIAN_POINT('Ctrl Pts',(55.5388543884596,30.9220930204886,9.37392638300965));
#45362=CARTESIAN_POINT('Ctrl Pts',(55.6117060589764,30.9001638817124,9.36864617136044));
#45363=CARTESIAN_POINT('Ctrl Pts',(55.7056143148866,30.865933709072,9.36188596900769));
#45364=CARTESIAN_POINT('Ctrl Pts',(55.7279482970938,30.8573345285957,9.36028199566582));
#45365=CARTESIAN_POINT('Ctrl Pts',(55.7651573987638,30.8422336916814,9.35762217847848));
#45366=CARTESIAN_POINT('Ctrl Pts',(55.7801172487516,30.8359487841865,9.35655624473106));
#45367=CARTESIAN_POINT('Ctrl Pts',(55.8008204191682,30.8269522442517,9.35508752981595));
#45368=CARTESIAN_POINT('Ctrl Pts',(55.8066295229105,30.8243948755541,9.35467613621507));
#45369=CARTESIAN_POINT('Ctrl Pts',(55.8164749123956,30.8200043762972,9.35398023363882));
#45370=CARTESIAN_POINT('Ctrl Pts',(55.8205174463477,30.8181854509298,9.35369487987156));
#45371=CARTESIAN_POINT('Ctrl Pts',(55.8282679723809,30.8146670121401,9.35314857123481));
#45372=CARTESIAN_POINT('Ctrl Pts',(55.8319768426479,30.8129695896632,9.35288748758152));
#45373=CARTESIAN_POINT('Ctrl Pts',(55.8408497350366,30.8088758095767,9.35226364557963));
#45374=CARTESIAN_POINT('Ctrl Pts',(55.8460087911326,30.8064686818755,9.35190153746928));
#45375=CARTESIAN_POINT('Ctrl Pts',(55.8646053839787,30.797694688492,9.35059825280139));
#45376=CARTESIAN_POINT('Ctrl Pts',(55.8779823247171,30.791199522991,9.34966453411634));
#45377=CARTESIAN_POINT('Ctrl Pts',(56.0161332342461,30.7222008432487,9.34004797304366));
#45378=CARTESIAN_POINT('Ctrl Pts',(56.1341114986657,30.6469077318902,9.33204302059598));
#45379=CARTESIAN_POINT('Ctrl Pts',(56.3484976829093,30.4760375574891,9.31611203851446));
#45380=CARTESIAN_POINT('Ctrl Pts',(56.4449508762514,30.3817536447246,9.30822576688206));
#45381=CARTESIAN_POINT('Ctrl Pts',(56.5427263751081,30.2646531941541,9.29876432214763));
#45382=CARTESIAN_POINT('Ctrl Pts',(56.5540890891429,30.2506635998045,9.29763939155595));
#45383=CARTESIAN_POINT('Ctrl Pts',(56.5710818667813,30.2291531735158,9.29591678305528));
#45384=CARTESIAN_POINT('Ctrl Pts',(56.5768511337334,30.221743120833,9.2953246214681));
#45385=CARTESIAN_POINT('Ctrl Pts',(56.5867902383234,30.208789648711,9.29429149451994));
#45386=CARTESIAN_POINT('Ctrl Pts',(56.5909839175347,30.2032646622589,9.29385147247178));
#45387=CARTESIAN_POINT('Ctrl Pts',(56.6003309557442,30.1908160593666,9.29286138837444));
#45388=CARTESIAN_POINT('Ctrl Pts',(56.6054683415163,30.1838806762978,9.29231071880553));
#45389=CARTESIAN_POINT('Ctrl Pts',(56.6190983177958,30.1652285625857,9.29083207970321));
#45390=CARTESIAN_POINT('Ctrl Pts',(56.6275085622282,30.1534525683509,9.28990098420736));
#45391=CARTESIAN_POINT('Ctrl Pts',(56.6648605689016,30.0999305291931,9.28567923959813));
#45392=CARTESIAN_POINT('Ctrl Pts',(56.6923272344461,30.0571828835495,9.28233404890007));
#45393=CARTESIAN_POINT('Ctrl Pts',(56.8118328617738,29.8545789071831,9.26658961948357));
#45394=CARTESIAN_POINT('Ctrl Pts',(56.8830435181873,29.6834994285822,9.25349149439364));
#45395=CARTESIAN_POINT('Ctrl Pts',(56.9434004817155,29.4529179469108,9.23716295247995));
#45396=CARTESIAN_POINT('Ctrl Pts',(56.9549436670145,29.4001705817781,9.23352106089846));
#45397=CARTESIAN_POINT('Ctrl Pts',(56.9659771044791,29.3377140769954,9.22936535192815));
#45398=CARTESIAN_POINT('Ctrl Pts',(56.9675541780455,29.3284011845437,9.22874975632469));
#45399=CARTESIAN_POINT('Ctrl Pts',(56.9698817329363,29.3140375549769,9.22780691257717));
#45400=CARTESIAN_POINT('Ctrl Pts',(56.9706790464509,29.3089947005647,9.22747714697915));
#45401=CARTESIAN_POINT('Ctrl Pts',(56.9721127335726,29.2996955924127,9.22687143008134));
#45402=CARTESIAN_POINT('Ctrl Pts',(56.9727546926228,29.2954403584541,9.22659517948702));
#45403=CARTESIAN_POINT('Ctrl Pts',(56.9741746188858,29.2858173423959,9.22597251457005));
#45404=CARTESIAN_POINT('Ctrl Pts',(56.9749444666062,29.2804484525763,9.22562655678444));
#45405=CARTESIAN_POINT('Ctrl Pts',(56.977158581962,29.2645459225875,9.22460592192089));
#45406=CARTESIAN_POINT('Ctrl Pts',(56.9785405690673,29.2540036055051,9.22393460748502));
#45407=CARTESIAN_POINT('Ctrl Pts',(56.9912663811667,29.1505121268705,9.21739194519921));
#45408=CARTESIAN_POINT('Ctrl Pts',(56.9961377890792,29.0568712389921,9.21184452678314));
#45409=CARTESIAN_POINT('Ctrl Pts',(56.9936514464864,28.922034796767,9.20396415077414));
#45410=CARTESIAN_POINT('Ctrl Pts',(56.9916161515464,28.8808788626741,9.20157371489591));
#45411=CARTESIAN_POINT('Ctrl Pts',(56.9766394036156,28.6949787911995,9.19074375865892));
#45412=CARTESIAN_POINT('Ctrl Pts',(56.949183164245,28.551871666362,9.18227746006094));
#45413=CARTESIAN_POINT('Ctrl Pts',(56.9010420998777,28.3955150138639,9.17213446920513));
#45414=CARTESIAN_POINT('Ctrl Pts',(56.8954106222268,28.3780822382142,9.17099128851613));
#45415=CARTESIAN_POINT('Ctrl Pts',(56.8865107930642,28.3517763246286,9.16924643044634));
#45416=CARTESIAN_POINT('Ctrl Pts',(56.8834180435864,28.34284448277,9.16865049335632));
#45417=CARTESIAN_POINT('Ctrl Pts',(56.8776975571026,28.3266958869117,9.1675665560186));
#45418=CARTESIAN_POINT('Ctrl Pts',(56.8750913852583,28.3194716472468,9.16707927411058));
#45419=CARTESIAN_POINT('Ctrl Pts',(56.8693946274083,28.3039615709289,9.16602790803968));
#45420=CARTESIAN_POINT('Ctrl Pts',(56.866290537898,28.2956809020408,9.16546338501665));
#45421=CARTESIAN_POINT('Ctrl Pts',(56.8577576501786,28.2733705366715,9.1639335761702));
#45422=CARTESIAN_POINT('Ctrl Pts',(56.8522251245152,28.2593813859716,9.16296485945009));
#45423=CARTESIAN_POINT('Ctrl Pts',(56.8240849595031,28.1905161748066,9.15814797679511));
#45424=CARTESIAN_POINT('Ctrl Pts',(56.7991962943826,28.1366104644012,9.15422397637789));
#45425=CARTESIAN_POINT('Ctrl Pts',(56.7095932397148,27.9632982234795,9.14108762670742));
#45426=CARTESIAN_POINT('Ctrl Pts',(56.6350982025969,27.8493890358803,9.13157789411601));
#45427=CARTESIAN_POINT('Ctrl Pts',(56.497444818211,27.6795628040207,9.1163843632431));
#45428=CARTESIAN_POINT('Ctrl Pts',(56.4412946946562,27.6184907503992,9.11067607143012));
#45429=CARTESIAN_POINT('Ctrl Pts',(56.3700705436731,27.5501084800544,9.1041395129003));
#45430=CARTESIAN_POINT('Ctrl Pts',(56.3585079060432,27.5392690113728,9.10309876626112));
#45431=CARTESIAN_POINT('Ctrl Pts',(56.3421785383655,27.5243225716828,9.10165868930248));
#45432=CARTESIAN_POINT('Ctrl Pts',(56.3375200650745,27.5200989291875,9.101251174327));
#45433=CARTESIAN_POINT('Ctrl Pts',(56.3295519149469,27.5129428999809,9.10055987224279));
#45434=CARTESIAN_POINT('Ctrl Pts',(56.326252339191,27.5099993800346,9.1002752663979));
#45435=CARTESIAN_POINT('Ctrl Pts',(56.3198799655207,27.5043525857226,9.09972884389562));
#45436=CARTESIAN_POINT('Ctrl Pts',(56.3168086168745,27.5016477789005,9.09946690723354));
#45437=CARTESIAN_POINT('Ctrl Pts',(56.3094061995396,27.4951691236515,9.09883895978292));
#45438=CARTESIAN_POINT('Ctrl Pts',(56.3050670808205,27.4914044682882,9.09847361852502));
#45439=CARTESIAN_POINT('Ctrl Pts',(56.2891436535107,27.4777092883983,9.09714265504694));
#45440=CARTESIAN_POINT('Ctrl Pts',(56.277461426206,27.4678927232152,9.09618492255271));
#45441=CARTESIAN_POINT('Ctrl Pts',(56.1630081960595,27.3739371336043,9.08696887568781));
#45442=CARTESIAN_POINT('Ctrl Pts',(56.0521734604722,27.3001148163087,9.07932152273101));
#45443=CARTESIAN_POINT('Ctrl Pts',(55.8108853689013,27.1721129183092,9.06345755135915));
#45444=CARTESIAN_POINT('Ctrl Pts',(55.6803915945405,27.1196365957924,9.05526242006114));
#45445=CARTESIAN_POINT('Ctrl Pts',(55.5278628728143,27.0762734427691,9.04543107533549));
#45446=CARTESIAN_POINT('Ctrl Pts',(55.5101762476722,27.0715075211143,9.04428803631034));
#45447=CARTESIAN_POINT('Ctrl Pts',(55.4832677859087,27.0646527071757,9.04254335086274));
#45448=CARTESIAN_POINT('Ctrl Pts',(55.4740922901799,27.0623846118992,9.04194744297643));
#45449=CARTESIAN_POINT('Ctrl Pts',(55.4574326851246,27.0583919337905,9.04086353658711));
#45450=CARTESIAN_POINT('Ctrl Pts',(55.4499540352015,27.0566451925302,9.04037625622628));
#45451=CARTESIAN_POINT('Ctrl Pts',(55.4338421475247,27.0529800296137,9.03932486855463));
#45452=CARTESIAN_POINT('Ctrl Pts',(55.4252058922145,27.0510757533583,9.03876032222565));
#45453=CARTESIAN_POINT('Ctrl Pts',(55.4018441987151,27.0460872203015,9.03723038907686));
#45454=CARTESIAN_POINT('Ctrl Pts',(55.3870962961026,27.0431120758194,9.03626157041945));
#45455=CARTESIAN_POINT('Ctrl Pts',(55.3139888127193,27.0292226143452,9.03144322658926));
#45456=CARTESIAN_POINT('Ctrl Pts',(55.2552010981877,27.0207517412582,9.02751781095116));
#45457=CARTESIAN_POINT('Ctrl Pts',(55.0377957239877,26.9992719234312,9.01280849003101));
#45458=CARTESIAN_POINT('Ctrl Pts',(54.8781700891338,27.0026298796944,9.001577538853));
#45459=CARTESIAN_POINT('Ctrl Pts',(54.6746889918854,27.0314073877667,8.98739629280573));
#45460=CARTESIAN_POINT('Ctrl Pts',(54.6289457058607,27.0395144981569,8.98422244072869));
#45461=CARTESIAN_POINT('Ctrl Pts',(54.5664066301552,27.0528660229284,8.97993653281451));
#45462=CARTESIAN_POINT('Ctrl Pts',(54.549337081132,27.0567457927715,8.97877230523381));
#45463=CARTESIAN_POINT('Ctrl Pts',(54.5199010625942,27.0638451045723,8.97677679019698));
#45464=CARTESIAN_POINT('Ctrl Pts',(54.5075105980079,27.0669596543449,8.97594057998621));
#45465=CARTESIAN_POINT('Ctrl Pts',(54.4895722407362,27.0716524400323,8.97473626008998));
#45466=CARTESIAN_POINT('Ctrl Pts',(54.4840002167434,27.0731359583144,8.97436306108693));
#45467=CARTESIAN_POINT('Ctrl Pts',(54.4742487945974,27.0757775493957,8.97371158889935));
#45468=CARTESIAN_POINT('Ctrl Pts',(54.4700666369413,27.0769251180672,8.97343272458887));
#45469=CARTESIAN_POINT('Ctrl Pts',(54.4611865952873,27.0793929373537,8.97284177624467));
#45470=CARTESIAN_POINT('Ctrl Pts',(54.4564898013933,27.0807167901991,8.97252990126463));
#45471=CARTESIAN_POINT('Ctrl Pts',(54.4437141380367,27.0843684364214,8.9716833291817));
#45472=CARTESIAN_POINT('Ctrl Pts',(54.4356449427866,27.0867301228209,8.97115054192122));
#45473=CARTESIAN_POINT('Ctrl Pts',(54.3978378163487,27.098055484479,8.9686621881177));
#45474=CARTESIAN_POINT('Ctrl Pts',(54.3682951677902,27.1076624275052,8.96674091714015));
#45475=CARTESIAN_POINT('Ctrl Pts',(54.1450040832168,27.1860868897679,8.95231171174125));
#45476=CARTESIAN_POINT('Ctrl Pts',(53.9627047528751,27.2838012642721,8.94094279944695));
#45477=CARTESIAN_POINT('Ctrl Pts',(53.7547391584642,27.4407168242663,8.92529714442832));
#45478=CARTESIAN_POINT('Ctrl Pts',(53.712322075242,27.4755580267179,8.9219483000231));
#45479=CARTESIAN_POINT('Ctrl Pts',(53.6607691719418,27.5215916038688,8.91764106516368));
#45480=CARTESIAN_POINT('Ctrl Pts',(53.6502429534061,27.5311955558391,8.91674850352265));
#45481=CARTESIAN_POINT('Ctrl Pts',(53.6335432045502,27.5467632533205,8.91531076752127));
#45482=CARTESIAN_POINT('Ctrl Pts',(53.6273035817171,27.5526556196751,8.91476861785809));
#45483=CARTESIAN_POINT('Ctrl Pts',(53.6155263387598,27.5639220817934,8.91373572470794));
#45484=CARTESIAN_POINT('Ctrl Pts',(53.6099814860972,27.5692884168674,8.91324532009406));
#45485=CARTESIAN_POINT('Ctrl Pts',(53.5974279708174,27.5815796324077,8.91212555587818));
#45486=CARTESIAN_POINT('Ctrl Pts',(53.5904392408955,27.5885244965228,8.91149533122864));
#45487=CARTESIAN_POINT('Ctrl Pts',(53.5724106732602,27.6067073380958,8.90985149323946));
#45488=CARTESIAN_POINT('Ctrl Pts',(53.5614521754252,27.6180246527265,8.90883438802049));
#45489=CARTESIAN_POINT('Ctrl Pts',(53.4603658985925,27.7249260258943,8.89928083086915));
#45490=CARTESIAN_POINT('Ctrl Pts',(53.3797701644002,27.8290472370523,8.89033949761056));
#45491=CARTESIAN_POINT('Ctrl Pts',(53.2591067995655,28.021482104707,8.87456353198744));
#45492=CARTESIAN_POINT('Ctrl Pts',(53.2141242439784,28.1062132515969,8.86784241256776));
#45493=CARTESIAN_POINT('Ctrl Pts',(53.1526417335254,28.2453693657681,8.85740620544516));
#45494=CARTESIAN_POINT('Ctrl Pts',(53.1320690747568,28.2978352851099,8.8536001271766));
#45495=CARTESIAN_POINT('Ctrl Pts',(53.1106392407729,28.3601292878444,8.84928286212643));
#45496=CARTESIAN_POINT('Ctrl Pts',(53.1076000202736,28.3691744043055,8.84866088495536));
#45497=CARTESIAN_POINT('Ctrl Pts',(53.103027987653,28.3831118231407,8.84771036809934));
#45498=CARTESIAN_POINT('Ctrl Pts',(53.1014489843403,28.3879886596338,8.84737924785006));
#45499=CARTESIAN_POINT('Ctrl Pts',(53.098579380892,28.3969695698789,8.84677225421259));
#45500=CARTESIAN_POINT('Ctrl Pts',(53.0972832621853,28.4010717182088,8.84649607207644));
#45501=CARTESIAN_POINT('Ctrl Pts',(53.0943906109038,28.4103309728315,8.84587507196094));
#45502=CARTESIAN_POINT('Ctrl Pts',(53.0928017385375,28.4154903777272,8.84553069958124));
#45503=CARTESIAN_POINT('Ctrl Pts',(53.0881802769191,28.4307167257565,8.84451910270566));
#45504=CARTESIAN_POINT('Ctrl Pts',(53.0852062528604,28.4408014510849,8.84385515297177));
#45505=CARTESIAN_POINT('Ctrl Pts',(53.0607663816614,28.5261572256575,8.83828286711351));
#45506=CARTESIAN_POINT('Ctrl Pts',(53.0436656390178,28.6026174969733,8.83359987630482));
#45507=CARTESIAN_POINT('Ctrl Pts',(53.0139813176481,28.7851986005292,8.82272297364465));
#45508=CARTESIAN_POINT('Ctrl Pts',(53.0053362195786,28.8917083089376,8.81660852304238));
#45509=CARTESIAN_POINT('Ctrl Pts',(53.0051727022678,29.0955686315939,8.80464977371496));
#45510=CARTESIAN_POINT('Ctrl Pts',(53.0121945389434,29.1926010975497,8.79884651696826));
#45511=CARTESIAN_POINT('Ctrl Pts',(53.0284983074822,29.3040534939942,8.79185370977796));
#45512=CARTESIAN_POINT('Ctrl Pts',(53.0309185144273,29.3193517386526,8.79088684825428));
#45513=CARTESIAN_POINT('Ctrl Pts',(53.0351559686856,29.3442542714803,8.7893008353633));
#45514=CARTESIAN_POINT('Ctrl Pts',(53.0368661209276,29.3538763035654,8.78868504842196));
#45515=CARTESIAN_POINT('Ctrl Pts',(53.0400513753408,29.3710638200922,8.78757960302407));
#45516=CARTESIAN_POINT('Ctrl Pts',(53.0414997617339,29.3786341029149,8.78709079687659));
#45517=CARTESIAN_POINT('Ctrl Pts',(53.0441951859792,29.3922928947487,8.78620533548143));
#45518=CARTESIAN_POINT('Ctrl Pts',(53.045426876134,29.3983843464669,8.78580917318068));
#45519=CARTESIAN_POINT('Ctrl Pts',(53.0466869980092,29.404469873728,8.78541210591381));
#45520=CARTESIAN_POINT('Ctrl Pts',(53.0466869433582,29.4044696098012,8.62635914573793));
#45521=CARTESIAN_POINT('Ctrl Pts',(53.0339617519014,29.3430155919505,8.63003243338377));
#45522=CARTESIAN_POINT('Ctrl Pts',(53.0241335957554,29.2809461466272,8.633664504864));
#45523=CARTESIAN_POINT('Ctrl Pts',(53.0092986084201,29.1463066780345,8.64154158808043));
#45524=CARTESIAN_POINT('Ctrl Pts',(53.0052933510497,29.0737709068806,8.64578545019623));
#45525=CARTESIAN_POINT('Ctrl Pts',(53.0052143251304,28.9403687723671,8.65375965806322));
#45526=CARTESIAN_POINT('Ctrl Pts',(53.0079592341221,28.8795911913357,8.65745684262587));
#45527=CARTESIAN_POINT('Ctrl Pts',(53.0148509017096,28.8039374181489,8.66218413492357));
#45528=CARTESIAN_POINT('Ctrl Pts',(53.0163985773011,28.7888534763602,8.66313283702782));
#45529=CARTESIAN_POINT('Ctrl Pts',(53.0191240084723,28.7649754066958,8.66464504693492));
#45530=CARTESIAN_POINT('Ctrl Pts',(53.0201887506642,28.756168775202,8.66520502324));
#45531=CARTESIAN_POINT('Ctrl Pts',(53.0222845615333,28.7397536633467,8.6662531115338));
#45532=CARTESIAN_POINT('Ctrl Pts',(53.0233008897726,28.7321434409339,8.66674075311983));
#45533=CARTESIAN_POINT('Ctrl Pts',(53.0256614638483,28.7152131021653,8.66782955572197));
#45534=CARTESIAN_POINT('Ctrl Pts',(53.0270278151354,28.7058963018412,8.66843140006313));
#45535=CARTESIAN_POINT('Ctrl Pts',(53.0312200749308,28.6786552807828,8.67019912156417));
#45536=CARTESIAN_POINT('Ctrl Pts',(53.0342245936739,28.6607599110723,8.67137057180523));
#45537=CARTESIAN_POINT('Ctrl Pts',(53.0622986407156,28.5064686953323,8.68156167208651));
#45538=CARTESIAN_POINT('Ctrl Pts',(53.101280203247,28.3730157249933,8.69103349600716));
#45539=CARTESIAN_POINT('Ctrl Pts',(53.204821199865,28.1199216006208,8.71005608366088));
#45540=CARTESIAN_POINT('Ctrl Pts',(53.2683938458869,28.000624895526,8.71954095136477));
#45541=CARTESIAN_POINT('Ctrl Pts',(53.3519792973415,27.8760401127119,8.72946809080181));
#45542=CARTESIAN_POINT('Ctrl Pts',(53.3605819111638,27.8635289586691,8.73046494493539));
#45543=CARTESIAN_POINT('Ctrl Pts',(53.3726297011737,27.8464288670951,8.73182602505888));
#45544=CARTESIAN_POINT('Ctrl Pts',(53.3759528151812,27.8417551245087,8.73219788392165));
#45545=CARTESIAN_POINT('Ctrl Pts',(53.3816804136443,27.833772746842,8.73283264538639));
#45546=CARTESIAN_POINT('Ctrl Pts',(53.3840749802726,27.8304570888838,8.73309620531474));
#45547=CARTESIAN_POINT('Ctrl Pts',(53.3890807897185,27.8235704737932,8.73364336498074));
#45548=CARTESIAN_POINT('Ctrl Pts',(53.3916937306331,27.820000815035,8.73392683550291));
#45549=CARTESIAN_POINT('Ctrl Pts',(53.3980560227791,27.8113693867685,8.73461197997416));
#45550=CARTESIAN_POINT('Ctrl Pts',(53.401817558563,27.8063165715681,8.73501282276074));
#45551=CARTESIAN_POINT('Ctrl Pts',(53.4151688815038,27.7885581818633,8.73642109211247));
#45552=CARTESIAN_POINT('Ctrl Pts',(53.4248870479576,27.775949274491,8.7374200654158));
#45553=CARTESIAN_POINT('Ctrl Pts',(53.4492181556541,27.745150384719,8.73986160133772));
#45554=CARTESIAN_POINT('Ctrl Pts',(53.4640015635813,27.7270974955134,8.74129396545186));
#45555=CARTESIAN_POINT('Ctrl Pts',(53.5262487159168,27.6537479185619,8.74713842522752));
#45556=CARTESIAN_POINT('Ctrl Pts',(53.5764113039279,27.6008093879875,8.75141712260328));
#45557=CARTESIAN_POINT('Ctrl Pts',(53.752562042392,27.4342157733545,8.76554339734793));
#45558=CARTESIAN_POINT('Ctrl Pts',(53.8901003336186,27.3338971240844,8.77525437258152));
#45559=CARTESIAN_POINT('Ctrl Pts',(54.0585846095429,27.2412272844805,8.7871177409156));
#45560=CARTESIAN_POINT('Ctrl Pts',(54.0786896069976,27.2306126776088,8.78853150610421));
#45561=CARTESIAN_POINT('Ctrl Pts',(54.108064486066,27.2157403525991,8.79059650927869));
#45562=CARTESIAN_POINT('Ctrl Pts',(54.1171929775767,27.2112062149685,8.79123813760003));
#45563=CARTESIAN_POINT('Ctrl Pts',(54.1333564992454,27.2033316251375,8.79237427943566));
#45564=CARTESIAN_POINT('Ctrl Pts',(54.1403771453484,27.1999620138441,8.79286777418812));
#45565=CARTESIAN_POINT('Ctrl Pts',(54.1549545495421,27.1930702122522,8.79389255546922));
#45566=CARTESIAN_POINT('Ctrl Pts',(54.1625140071921,27.1895541213319,8.79442403941102));
#45567=CARTESIAN_POINT('Ctrl Pts',(54.1820381294309,27.1806214161179,8.79579699336725));
#45568=CARTESIAN_POINT('Ctrl Pts',(54.1940344976324,27.1752754595303,8.79664084884711));
#45569=CARTESIAN_POINT('Ctrl Pts',(54.2455194370674,27.1529389162304,8.80026415186306));
#45570=CARTESIAN_POINT('Ctrl Pts',(54.2854963652778,27.137109865231,8.80308220907734));
#45571=CARTESIAN_POINT('Ctrl Pts',(54.394475753681,27.0979829455769,8.81078219123228));
#45572=CARTESIAN_POINT('Ctrl Pts',(54.4642894265538,27.0771529419011,8.81573565910689));
#45573=CARTESIAN_POINT('Ctrl Pts',(54.6312663400331,27.037133102232,8.82758363536409));
#45574=CARTESIAN_POINT('Ctrl Pts',(54.7290342899673,27.021266137794,8.83452508477089));
#45575=CARTESIAN_POINT('Ctrl Pts',(54.847581976215,27.0109801991336,8.8427598748806));
#45576=CARTESIAN_POINT('Ctrl Pts',(54.867618598136,27.0095462277785,8.84414514028256));
#45577=CARTESIAN_POINT('Ctrl Pts',(54.943370030991,27.0052738178297,8.84935067876955));
#45578=CARTESIAN_POINT('Ctrl Pts',(54.9991792297645,27.0044699833988,8.85312173641572));
#45579=CARTESIAN_POINT('Ctrl Pts',(55.063996596931,27.0062563270266,8.85737512596282));
#45580=CARTESIAN_POINT('Ctrl Pts',(55.0730378615593,27.0065670625668,8.85796554968094));
#45581=CARTESIAN_POINT('Ctrl Pts',(55.0876365129166,27.0071682545114,8.85891391234663));
#45582=CARTESIAN_POINT('Ctrl Pts',(55.0931952255836,27.0074204718616,8.85927385338326));
#45583=CARTESIAN_POINT('Ctrl Pts',(55.103061596589,27.0079095200346,8.85991056991172));
#45584=CARTESIAN_POINT('Ctrl Pts',(55.1073696146435,27.0081370679286,8.86018784891336));
#45585=CARTESIAN_POINT('Ctrl Pts',(55.1166709735545,27.008658626772,8.86078491476619));
#45586=CARTESIAN_POINT('Ctrl Pts',(55.1216639530849,27.0089574427859,8.86110443349912));
#45587=CARTESIAN_POINT('Ctrl Pts',(55.1356023392242,27.0098442442184,8.86199377617303));
#45588=CARTESIAN_POINT('Ctrl Pts',(55.1445451169611,27.0104737641912,8.86256135249215));
#45589=CARTESIAN_POINT('Ctrl Pts',(55.1975007508767,27.0145604845682,8.86590602106181));
#45590=CARTESIAN_POINT('Ctrl Pts',(55.2413968545781,27.0194180567326,8.86861182223439));
#45591=CARTESIAN_POINT('Ctrl Pts',(55.3888156308679,27.040706399693,8.87758118215502));
#45592=CARTESIAN_POINT('Ctrl Pts',(55.4911983146346,27.0638345989884,8.88361965625112));
#45593=CARTESIAN_POINT('Ctrl Pts',(55.7100035059867,27.131746371403,8.89693269806536));
#45594=CARTESIAN_POINT('Ctrl Pts',(55.8249932578367,27.1795996074377,8.90420940960151));
#45595=CARTESIAN_POINT('Ctrl Pts',(55.9562613016356,27.2492334900576,8.91335756276838));
#45596=CARTESIAN_POINT('Ctrl Pts',(55.9775350575996,27.2610220872304,8.91486749967388));
#45597=CARTESIAN_POINT('Ctrl Pts',(56.0070490099876,27.2780896076299,8.91700354039067));
#45598=CARTESIAN_POINT('Ctrl Pts',(56.0154745387334,27.2830449733191,8.91761812666999));
#45599=CARTESIAN_POINT('Ctrl Pts',(56.0300590172571,27.2917675500995,8.9186905103074));
#45600=CARTESIAN_POINT('Ctrl Pts',(56.0362346163038,27.2955066736166,8.91914728865245));
#45601=CARTESIAN_POINT('Ctrl Pts',(56.0490899206826,27.3033858252593,8.92010384400551));
#45602=CARTESIAN_POINT('Ctrl Pts',(56.0557657186988,27.3075319607317,8.92060383792477));
#45603=CARTESIAN_POINT('Ctrl Pts',(56.071554022037,27.31746735783,8.92179416727123));
#45604=CARTESIAN_POINT('Ctrl Pts',(56.0806442968801,27.3232913162408,8.92248576918895));
#45605=CARTESIAN_POINT('Ctrl Pts',(56.1110937195471,27.3431501301637,8.92482387854965));
#45606=CARTESIAN_POINT('Ctrl Pts',(56.1322295746422,27.3575211309882,8.9264827943959));
#45607=CARTESIAN_POINT('Ctrl Pts',(56.182127083131,27.3928690034287,8.93048807357716));
#45608=CARTESIAN_POINT('Ctrl Pts',(56.21061394839,27.4142168839691,8.93284786581775));
#45609=CARTESIAN_POINT('Ctrl Pts',(56.3202247492292,27.5010338299848,8.94222126387747));
#45610=CARTESIAN_POINT('Ctrl Pts',(56.3967290785025,27.5720516842204,8.94942910954438));
#45611=CARTESIAN_POINT('Ctrl Pts',(56.5496285809665,27.7380811708835,8.96515364908256));
#45612=CARTESIAN_POINT('Ctrl Pts',(56.6236004788266,27.8347898953716,8.97365926549698));
#45613=CARTESIAN_POINT('Ctrl Pts',(56.6967221996578,27.9509954889552,8.98275166740897));
#45614=CARTESIAN_POINT('Ctrl Pts',(56.7049697317664,27.96445428017,8.98378862452541));
#45615=CARTESIAN_POINT('Ctrl Pts',(56.7163669278282,27.9835582308935,8.98523645209028));
#45616=CARTESIAN_POINT('Ctrl Pts',(56.7196499961326,27.9891225620709,8.98565531387402));
#45617=CARTESIAN_POINT('Ctrl Pts',(56.72512889531,27.9985124507206,8.9863572544016));
#45618=CARTESIAN_POINT('Ctrl Pts',(56.7273391569256,28.0023294857427,8.98664124448828));
#45619=CARTESIAN_POINT('Ctrl Pts',(56.7318264575111,28.0101384928698,8.98721943628707));
#45620=CARTESIAN_POINT('Ctrl Pts',(56.734102389273,28.0141310498923,8.98751356769985));
#45621=CARTESIAN_POINT('Ctrl Pts',(56.7398715270099,28.0243333590517,8.98826148660413));
#45622=CARTESIAN_POINT('Ctrl Pts',(56.7433453342593,28.0305540892133,8.98871405527718));
#45623=CARTESIAN_POINT('Ctrl Pts',(56.757367348263,28.055983166626,8.99055053578103));
#45624=CARTESIAN_POINT('Ctrl Pts',(56.7676324748415,28.0753469269005,8.99191767831141));
#45625=CARTESIAN_POINT('Ctrl Pts',(56.7939237708745,28.1269805638565,8.99549157665237));
#45626=CARTESIAN_POINT('Ctrl Pts',(56.8093989144137,28.159523168094,8.99767154549399));
#45627=CARTESIAN_POINT('Ctrl Pts',(56.8969696595348,28.3573207785658,9.01059514996441));
#45628=CARTESIAN_POINT('Ctrl Pts',(56.947271299809,28.531307575048,9.02069645124172));
#45629=CARTESIAN_POINT('Ctrl Pts',(56.9814506393162,28.7636606783768,9.03479364372171));
#45630=CARTESIAN_POINT('Ctrl Pts',(56.9871715998522,28.8179254432515,9.03812037631632));
#45631=CARTESIAN_POINT('Ctrl Pts',(56.9916123178096,28.8871787201719,9.04244154257054));
#45632=CARTESIAN_POINT('Ctrl Pts',(56.9923973064914,28.9020141847028,9.0433715524119));
#45633=CARTESIAN_POINT('Ctrl Pts',(56.9933797676268,28.9255646313478,9.04485532526244));
#45634=CARTESIAN_POINT('Ctrl Pts',(56.993685959376,28.9342747111131,9.04540570637596));
#45635=CARTESIAN_POINT('Ctrl Pts',(56.9941329710121,28.949908038901,9.04639656327099));
#45636=CARTESIAN_POINT('Ctrl Pts',(56.9942948402786,28.9568305812597,9.04683637729215));
#45637=CARTESIAN_POINT('Ctrl Pts',(56.994589142589,28.9730243310096,9.0478677594611));
#45638=CARTESIAN_POINT('Ctrl Pts',(56.9946929819655,28.9822958370831,9.04846020644303));
#45639=CARTESIAN_POINT('Ctrl Pts',(56.9948059392661,29.0090165397491,9.05017342181876));
#45640=CARTESIAN_POINT('Ctrl Pts',(56.9946507447887,29.0264652174341,9.05129925217472));
#45641=CARTESIAN_POINT('Ctrl Pts',(56.9911452086702,29.1856796636067,9.06163961237966));
#45642=CARTESIAN_POINT('Ctrl Pts',(56.9729161528102,29.3266856651235,9.07132993736857));
#45643=CARTESIAN_POINT('Ctrl Pts',(56.9089868983004,29.5936511461629,9.09043190483563));
#45644=CARTESIAN_POINT('Ctrl Pts',(56.865255489369,29.719360944655,9.09976459903682));
#45645=CARTESIAN_POINT('Ctrl Pts',(56.8029299277564,29.8536416616001,9.10956131935182));
#45646=CARTESIAN_POINT('Ctrl Pts',(56.7963468054112,29.8674091302034,9.11056330836447));
#45647=CARTESIAN_POINT('Ctrl Pts',(56.7870686310291,29.8862540672901,9.1119301020083));
#45648=CARTESIAN_POINT('Ctrl Pts',(56.7845088629206,29.8913970405553,9.11230262370906));
#45649=CARTESIAN_POINT('Ctrl Pts',(56.7800874954173,29.9001848811438,9.11293822247558));
#45650=CARTESIAN_POINT('Ctrl Pts',(56.7782368489789,29.9038351737172,9.11320196058803));
#45651=CARTESIAN_POINT('Ctrl Pts',(56.7743634056875,29.9114173676052,9.11374916619371));
#45652=CARTESIAN_POINT('Ctrl Pts',(56.7723387570832,29.9153482637589,9.11403250606704));
#45653=CARTESIAN_POINT('Ctrl Pts',(56.7674033403298,29.9248527079061,9.11471680703336));
#45654=CARTESIAN_POINT('Ctrl Pts',(56.7644792250177,29.9304193494136,9.11511694200707));
#45655=CARTESIAN_POINT('Ctrl Pts',(56.7540933302514,29.9499659271914,9.11651999490905));
#45656=CARTESIAN_POINT('Ctrl Pts',(56.746491108611,29.9638711109603,9.11751454249604));
#45657=CARTESIAN_POINT('Ctrl Pts',(56.6981128591645,30.0499074444926,9.1236551203135));
#45658=CARTESIAN_POINT('Ctrl Pts',(56.6530365776821,30.1195383623674,9.12856885887016));
#45659=CARTESIAN_POINT('Ctrl Pts',(56.5231220956694,30.2951884972068,9.14134978664947));
#45660=CARTESIAN_POINT('Ctrl Pts',(56.4315876693103,30.3956970323677,9.14909484268164));
#45661=CARTESIAN_POINT('Ctrl Pts',(56.2862365603152,30.5258320256136,9.16076686370978));
#45662=CARTESIAN_POINT('Ctrl Pts',(56.2401572629954,30.5635142490026,9.16438669119289));
#45663=CARTESIAN_POINT('Ctrl Pts',(56.180397587677,30.6080782747756,9.16902625657335));
#45664=CARTESIAN_POINT('Ctrl Pts',(56.1682279547663,30.6169408242262,9.16996827828832));
#45665=CARTESIAN_POINT('Ctrl Pts',(56.1487502291927,30.6307908278767,9.17147220735112));
#45666=CARTESIAN_POINT('Ctrl Pts',(56.1415071056893,30.6358689852694,9.17203064908879));
#45667=CARTESIAN_POINT('Ctrl Pts',(56.1279130982254,30.6452655056541,9.17307734023843));
#45668=CARTESIAN_POINT('Ctrl Pts',(56.1215705669622,30.6495957086155,9.17356513022025));
#45669=CARTESIAN_POINT('Ctrl Pts',(56.1073691152046,30.6591716257776,9.17465616735537));
#45670=CARTESIAN_POINT('Ctrl Pts',(56.0994976492308,30.6643983163253,9.17526011130222));
#45671=CARTESIAN_POINT('Ctrl Pts',(56.0762703728932,30.6795846624958,9.17704012042851));
#45672=CARTESIAN_POINT('Ctrl Pts',(56.0608146035181,30.6893889114735,9.17822187720772));
#45673=CARTESIAN_POINT('Ctrl Pts',(55.9241024519535,30.7734954138644,9.18865452849517));
#45674=CARTESIAN_POINT('Ctrl Pts',(55.7953804149375,30.8348315440107,9.19838255002727));
#45675=CARTESIAN_POINT('Ctrl Pts',(55.5378401612045,30.9253229480719,9.21738241669839));
#45676=CARTESIAN_POINT('Ctrl Pts',(55.4104448065578,30.9564460318103,9.22657205271839));
#45677=CARTESIAN_POINT('Ctrl Pts',(55.2657186252561,30.9770322855557,9.23624702864736));
#45678=CARTESIAN_POINT('Ctrl Pts',(55.2505010913404,30.9790180098671,9.2372547553672));
#45679=CARTESIAN_POINT('Ctrl Pts',(55.2295457028681,30.9815068673438,9.23862794323933));
#45680=CARTESIAN_POINT('Ctrl Pts',(55.2238267926976,30.9821610085647,9.23900121590713));
#45681=CARTESIAN_POINT('Ctrl Pts',(55.2140339886487,30.9832382076427,9.23963776358058));
#45682=CARTESIAN_POINT('Ctrl Pts',(55.2099615162392,30.9836734859811,9.23990170385414));
#45683=CARTESIAN_POINT('Ctrl Pts',(55.2014920190159,30.9845523572671,9.24044896394319));
#45684=CARTESIAN_POINT('Ctrl Pts',(55.19709483377,30.9849938839615,9.24073215793868));
#45685=CARTESIAN_POINT('Ctrl Pts',(55.1864504205745,30.9860269837559,9.24141551310351));
#45686=CARTESIAN_POINT('Ctrl Pts',(55.1802017295913,30.9866037044988,9.24181485380407));
#45687=CARTESIAN_POINT('Ctrl Pts',(55.1582440985284,30.9885258216843,9.24321207107382));
#45688=CARTESIAN_POINT('Ctrl Pts',(55.142521551041,30.9897144976411,9.24420166955198));
#45689=CARTESIAN_POINT('Ctrl Pts',(55.0449583985146,30.99592815997,9.25028424800081));
#45690=CARTESIAN_POINT('Ctrl Pts',(54.9628775016304,30.9960900445842,9.25514963820476));
#45691=CARTESIAN_POINT('Ctrl Pts',(54.7358001410951,30.982520521511,9.26846233415437));
#45692=CARTESIAN_POINT('Ctrl Pts',(54.5919810933355,30.9579858950746,9.27675761395452));
#45693=CARTESIAN_POINT('Ctrl Pts',(54.4022424608979,30.9037865037627,9.28862532778164));
#45694=CARTESIAN_POINT('Ctrl Pts',(54.3529541697322,30.8876038052835,9.29179286536457));
#45695=CARTESIAN_POINT('Ctrl Pts',(54.2907024865597,30.8644400784415,9.29593047234084));
#45696=CARTESIAN_POINT('Ctrl Pts',(54.2771060716231,30.8592106172561,9.29684267137894));
#45697=CARTESIAN_POINT('Ctrl Pts',(54.2555275314168,30.8506385830807,9.2983045489736));
#45698=CARTESIAN_POINT('Ctrl Pts',(54.247507604182,30.8473921110868,9.29885101759913));
#45699=CARTESIAN_POINT('Ctrl Pts',(54.2330997268035,30.841450406801,9.29983854186114));
#45700=CARTESIAN_POINT('Ctrl Pts',(54.2267041926349,30.8387738365748,9.30027896418759));
#45701=CARTESIAN_POINT('Ctrl Pts',(54.2118789257908,30.8324783466594,9.30130477328933));
#45702=CARTESIAN_POINT('Ctrl Pts',(54.2034599984423,30.8288345304843,9.30189099391295));
#45703=CARTESIAN_POINT('Ctrl Pts',(54.1793351363773,30.8181948079571,9.303581630362));
#45704=CARTESIAN_POINT('Ctrl Pts',(54.1636944352306,30.8110538782385,9.30469094524407));
#45705=CARTESIAN_POINT('Ctrl Pts',(54.1285089680757,30.7944365914974,9.30721723835268));
#45706=CARTESIAN_POINT('Ctrl Pts',(54.1090230066409,30.7848415156968,9.30863815459307));
#45707=CARTESIAN_POINT('Ctrl Pts',(54.0465054187845,30.7527783601519,9.31326910091151));
#45708=CARTESIAN_POINT('Ctrl Pts',(54.0041387413426,30.7290585957074,9.31652024617999));
#45709=CARTESIAN_POINT('Ctrl Pts',(53.8661777342329,30.6450652506076,9.32748305733285));
#45710=CARTESIAN_POINT('Ctrl Pts',(53.7748464040783,30.578222816338,9.33537995111363));
#45711=CARTESIAN_POINT('Ctrl Pts',(53.6154587579674,30.439361385762,9.35009308193447));
#45712=CARTESIAN_POINT('Ctrl Pts',(53.5461232957958,30.3692927925865,9.35689324698141));
#45713=CARTESIAN_POINT('Ctrl Pts',(53.4753388251414,30.2862927084301,9.36405816488137));
#45714=CARTESIAN_POINT('Ctrl Pts',(53.4685035406163,30.2781467977636,9.36475251360451));
#45715=CARTESIAN_POINT('Ctrl Pts',(53.4582804068789,30.2657636738789,9.36579427166871));
#45716=CARTESIAN_POINT('Ctrl Pts',(53.4548442933306,30.2615668138262,9.36614498583346));
#45717=CARTESIAN_POINT('Ctrl Pts',(53.4487127132625,30.2540150859693,9.3667717602668));
#45718=CARTESIAN_POINT('Ctrl Pts',(53.4460109556245,30.2506654760099,9.36704826263214));
#45719=CARTESIAN_POINT('Ctrl Pts',(53.440127727406,30.2433230146068,9.36765107403969));
#45720=CARTESIAN_POINT('Ctrl Pts',(53.4369507419554,30.239326689692,9.36797706713424));
#45721=CARTESIAN_POINT('Ctrl Pts',(53.4279404882153,30.2279029462622,9.36890310710753));
#45722=CARTESIAN_POINT('Ctrl Pts',(53.4221444834489,30.2204461197527,9.36950059698377));
#45723=CARTESIAN_POINT('Ctrl Pts',(53.3835996994863,30.1701228996162,9.37348835233874));
#45724=CARTESIAN_POINT('Ctrl Pts',(53.3525452861601,30.1259802979351,9.37677154541507));
#45725=CARTESIAN_POINT('Ctrl Pts',(53.2575319217559,29.978559298931,9.38724728457753));
#45726=CARTESIAN_POINT('Ctrl Pts',(53.2012020971099,29.8706910060105,9.39418406983926));
#45727=CARTESIAN_POINT('Ctrl Pts',(53.1349386626491,29.7094834498775,9.40436892285359));
#45728=CARTESIAN_POINT('Ctrl Pts',(53.1167979495078,29.6598258502138,9.40748084197396));
#45729=CARTESIAN_POINT('Ctrl Pts',(53.0825149897801,29.5529933806987,9.41419402490627));
#45730=CARTESIAN_POINT('Ctrl Pts',(53.0669119579143,29.4957015797813,9.41780520397248));
#45731=CARTESIAN_POINT('Ctrl Pts',(53.0513919897812,29.4267125639665,9.42220626268059));
#45732=CARTESIAN_POINT('Ctrl Pts',(53.0489919156069,29.4156010501272,9.42291666214691));
#45733=CARTESIAN_POINT('Ctrl Pts',(53.0466869980009,29.4044698736881,9.42363003822484));
#45734=CARTESIAN_POINT('Origin',(55.,29.,3.45145488139523));
#45735=CARTESIAN_POINT('',(53.0466869980528,29.4044698739386,10.38234667127));
#45736=CARTESIAN_POINT('',(53.046686906026,29.4044694295118,10.2256126172116));
#45737=CARTESIAN_POINT('',(53.0466869980082,29.4044698737233,3.45145488139523));
#45738=CARTESIAN_POINT('',(53.0052500005621,28.9999526465424,9.60767889029237));
#45739=CARTESIAN_POINT('Ctrl Pts',(53.0466869980528,29.4044698739386,10.38234667127));
#45740=CARTESIAN_POINT('Ctrl Pts',(53.0495690730458,29.418388326014,10.3813700720195));
#45741=CARTESIAN_POINT('Ctrl Pts',(53.0525999295262,29.4322760519837,10.3803968981023));
#45742=CARTESIAN_POINT('Ctrl Pts',(53.0659164325032,29.4903088798927,10.3763384924675));
#45743=CARTESIAN_POINT('Ctrl Pts',(53.0775575452908,29.5341327205029,10.3732935163058));
#45744=CARTESIAN_POINT('Ctrl Pts',(53.0931574468468,29.5857064922055,10.3697627720438));
#45745=CARTESIAN_POINT('Ctrl Pts',(53.0956846717732,29.5938718333258,10.3692053724519));
#45746=CARTESIAN_POINT('Ctrl Pts',(53.0998983088677,29.6071823754082,10.3682996436764));
#45747=CARTESIAN_POINT('Ctrl Pts',(53.101553291598,29.6123373013907,10.3679495863005));
#45748=CARTESIAN_POINT('Ctrl Pts',(53.1045612374735,29.621577006171,10.367323506836));
#45749=CARTESIAN_POINT('Ctrl Pts',(53.1059064428019,29.625664186882,10.3670470470468));
#45750=CARTESIAN_POINT('Ctrl Pts',(53.1088791695915,29.6345988596246,10.366443769413));
#45751=CARTESIAN_POINT('Ctrl Pts',(53.1105121055804,29.6394444511355,10.3661172711826));
#45752=CARTESIAN_POINT('Ctrl Pts',(53.1152262281519,29.6532574511882,10.365188346825));
#45753=CARTESIAN_POINT('Ctrl Pts',(53.118352794664,29.6622093865426,10.3645885027962));
#45754=CARTESIAN_POINT('Ctrl Pts',(53.1399962193134,29.7227873677053,10.360541950609));
#45755=CARTESIAN_POINT('Ctrl Pts',(53.1605734442592,29.7736580474306,10.3572059697192));
#45756=CARTESIAN_POINT('Ctrl Pts',(53.2642710874475,30.0023986563568,10.3422153684849));
#45757=CARTESIAN_POINT('Ctrl Pts',(53.3712601990154,30.1682351125603,10.3312624043519));
#45758=CARTESIAN_POINT('Ctrl Pts',(53.5273378627706,30.3460750710649,10.3169054423481));
#45759=CARTESIAN_POINT('Ctrl Pts',(53.5548328177161,30.37555201321,10.3144282951032));
#45760=CARTESIAN_POINT('Ctrl Pts',(53.5925661032047,30.4136245646633,10.3110832037014));
#45761=CARTESIAN_POINT('Ctrl Pts',(53.6020260386991,30.4229804544224,10.3102489258938));
#45762=CARTESIAN_POINT('Ctrl Pts',(53.6175917323802,30.4380699145239,10.3088827889616));
#45763=CARTESIAN_POINT('Ctrl Pts',(53.6236413559673,30.4438609964227,10.3083534312968));
#45764=CARTESIAN_POINT('Ctrl Pts',(53.6353762496506,30.4549536104352,10.3073295451221));
#45765=CARTESIAN_POINT('Ctrl Pts',(53.6410564046646,30.4602603502263,10.3068352527054));
#45766=CARTESIAN_POINT('Ctrl Pts',(53.654319455554,30.4725070787383,10.3056840233319));
#45767=CARTESIAN_POINT('Ctrl Pts',(53.6619252136078,30.4794218749748,10.3050260421009));
#45768=CARTESIAN_POINT('Ctrl Pts',(53.6864219311068,30.5013496956282,10.3029135396763));
#45769=CARTESIAN_POINT('Ctrl Pts',(53.7035142137582,30.5161341591406,10.3014496459182));
#45770=CARTESIAN_POINT('Ctrl Pts',(53.7924942332987,30.5904949725454,10.2938769090778));
#45771=CARTESIAN_POINT('Ctrl Pts',(53.8682398251174,30.6452534830512,10.2875801836952));
#45772=CARTESIAN_POINT('Ctrl Pts',(54.0541636482885,30.760732251701,10.2725129889987));
#45773=CARTESIAN_POINT('Ctrl Pts',(54.1668045260358,30.8167466349176,10.2636617426247));
#45774=CARTESIAN_POINT('Ctrl Pts',(54.335977836697,30.8818098369856,10.2512263658725));
#45775=CARTESIAN_POINT('Ctrl Pts',(54.3888170236623,30.8996289869442,10.2474589358557));
#45776=CARTESIAN_POINT('Ctrl Pts',(54.4510216936421,30.9177414270883,10.2432091060772));
#45777=CARTESIAN_POINT('Ctrl Pts',(54.459722668644,30.9202108672135,10.2426188138007));
#45778=CARTESIAN_POINT('Ctrl Pts',(54.4738028851581,30.9241037170545,10.2416706202782));
#45779=CARTESIAN_POINT('Ctrl Pts',(54.4791716972671,30.9255639170195,10.2413107180681));
#45780=CARTESIAN_POINT('Ctrl Pts',(54.4887140546065,30.9281164007025,10.2406740438168));
#45781=CARTESIAN_POINT('Ctrl Pts',(54.4928851036639,30.929217627894,10.2403967685246));
#45782=CARTESIAN_POINT('Ctrl Pts',(54.501900445257,30.9315665710594,10.239799680712));
#45783=CARTESIAN_POINT('Ctrl Pts',(54.5067458645648,30.9328095985027,10.2394801365001));
#45784=CARTESIAN_POINT('Ctrl Pts',(54.5202895211314,30.9362297943436,10.2385906510481));
#45785=CARTESIAN_POINT('Ctrl Pts',(54.5289979668841,30.9383665938054,10.2380229585962));
#45786=CARTESIAN_POINT('Ctrl Pts',(54.5806990007094,30.950683521716,10.2346761086877));
#45787=CARTESIAN_POINT('Ctrl Pts',(54.624009301221,30.9594925835633,10.2319683507442));
#45788=CARTESIAN_POINT('Ctrl Pts',(54.7710568645391,30.9843452148307,10.2229881150481));
#45789=CARTESIAN_POINT('Ctrl Pts',(54.8757601674787,30.9936420442041,10.2169413334741));
#45790=CARTESIAN_POINT('Ctrl Pts',(55.1048237348402,30.9958566914059,10.2036296340241));
#45791=CARTESIAN_POINT('Ctrl Pts',(55.2287579617121,30.985471384532,10.1963627789262));
#45792=CARTESIAN_POINT('Ctrl Pts',(55.374854130337,30.959362972407,10.1872258538473));
#45793=CARTESIAN_POINT('Ctrl Pts',(55.3987107719586,30.954647926769,10.1857161296592));
#45794=CARTESIAN_POINT('Ctrl Pts',(55.4320256460817,30.9474282817201,10.1835804204124));
#45795=CARTESIAN_POINT('Ctrl Pts',(55.4415613268412,30.9452883232437,10.182965949786));
#45796=CARTESIAN_POINT('Ctrl Pts',(55.4581126833832,30.9414459674622,10.1818937107096));
#45797=CARTESIAN_POINT('Ctrl Pts',(55.4651356129703,30.9397753825082,10.1814369605777));
#45798=CARTESIAN_POINT('Ctrl Pts',(55.4797848789184,30.9362065477715,10.180480408078));
#45799=CARTESIAN_POINT('Ctrl Pts',(55.4874093612983,30.9343012788357,10.1799803885014));
#45800=CARTESIAN_POINT('Ctrl Pts',(55.5054825717024,30.9296713528955,10.1787898947011));
#45801=CARTESIAN_POINT('Ctrl Pts',(55.5159207413699,30.9269068326108,10.17809815305));
#45802=CARTESIAN_POINT('Ctrl Pts',(55.5509998253696,30.9173107707106,10.1757590734199));
#45803=CARTESIAN_POINT('Ctrl Pts',(55.5755308554245,30.9100904516269,10.174099313024));
#45804=CARTESIAN_POINT('Ctrl Pts',(55.6338835050969,30.8916891490242,10.1700916242326));
#45805=CARTESIAN_POINT('Ctrl Pts',(55.6675567524781,30.880070173855,10.167730245548));
#45806=CARTESIAN_POINT('Ctrl Pts',(55.7986014462323,30.8308887289958,10.1583470747256));
#45807=CARTESIAN_POINT('Ctrl Pts',(55.8932651326754,30.7866143241155,10.1511305955659));
#45808=CARTESIAN_POINT('Ctrl Pts',(56.0895559994211,30.6752954436137,10.135409264161));
#45809=CARTESIAN_POINT('Ctrl Pts',(56.1894194729557,30.6059369982914,10.1269159392035));
#45810=CARTESIAN_POINT('Ctrl Pts',(56.2944610502715,30.517777138703,10.1178342410082));
#45811=CARTESIAN_POINT('Ctrl Pts',(56.3064344986906,30.5074832639866,10.1167969320462));
#45812=CARTESIAN_POINT('Ctrl Pts',(56.3231341421418,30.4927777310115,10.1153487005424));
#45813=CARTESIAN_POINT('Ctrl Pts',(56.3279626954465,30.4884839248695,10.1149297808473));
#45814=CARTESIAN_POINT('Ctrl Pts',(56.3360522328033,30.4812195818173,10.1142277711554));
#45815=CARTESIAN_POINT('Ctrl Pts',(56.3393243534943,30.4782615789316,10.1139437694234));
#45816=CARTESIAN_POINT('Ctrl Pts',(56.3459853791995,30.4721997279641,10.1133655810159));
#45817=CARTESIAN_POINT('Ctrl Pts',(56.3493734109576,30.4690949863342,10.1130714644863));
#45818=CARTESIAN_POINT('Ctrl Pts',(56.357986034671,30.461147575945,10.1123236300263));
#45819=CARTESIAN_POINT('Ctrl Pts',(56.3631955231479,30.4562885285496,10.11187113037));
#45820=CARTESIAN_POINT('Ctrl Pts',(56.3843170379587,30.4363752001297,10.1100352935692));
#45821=CARTESIAN_POINT('Ctrl Pts',(56.4000072989275,30.4210865678213,10.1086687109356));
#45822=CARTESIAN_POINT('Ctrl Pts',(56.4408130376617,30.3799933704081,10.1050966360637));
#45823=CARTESIAN_POINT('Ctrl Pts',(56.4654879503862,30.3537611619265,10.1029178968978));
#45824=CARTESIAN_POINT('Ctrl Pts',(56.6091296023158,30.1925207405835,10.0900162602896));
#45825=CARTESIAN_POINT('Ctrl Pts',(56.7100926744953,30.042590259918,10.0799336850375));
#45826=CARTESIAN_POINT('Ctrl Pts',(56.8138254146022,29.8319112989469,10.065840992096));
#45827=CARTESIAN_POINT('Ctrl Pts',(56.8360224934992,29.7817030346368,10.0624946878773));
#45828=CARTESIAN_POINT('Ctrl Pts',(56.8615723158017,29.7167967780808,10.0581513665782));
#45829=CARTESIAN_POINT('Ctrl Pts',(56.8668689394584,29.7028865143727,10.0572196100878));
#45830=CARTESIAN_POINT('Ctrl Pts',(56.8750214607103,29.6807335398309,10.055733689976));
#45831=CARTESIAN_POINT('Ctrl Pts',(56.877979881727,29.6725289512857,10.055182925316));
#45832=CARTESIAN_POINT('Ctrl Pts',(56.8831901475673,29.6577768378664,10.0541917353995));
#45833=CARTESIAN_POINT('Ctrl Pts',(56.8854619006575,29.6512364543924,10.0537519746699));
#45834=CARTESIAN_POINT('Ctrl Pts',(56.8906935210182,29.6359177547879,10.0527211804419));
#45835=CARTESIAN_POINT('Ctrl Pts',(56.8936263588951,29.6271304405155,10.0521292714356));
#45836=CARTESIAN_POINT('Ctrl Pts',(56.9018943740286,29.6017710904626,10.0504191543564));
#45837=CARTESIAN_POINT('Ctrl Pts',(56.9070738374667,29.5851495552795,10.0492959126677));
#45838=CARTESIAN_POINT('Ctrl Pts',(56.9511171342135,29.4370091218193,10.0392614627375));
#45839=CARTESIAN_POINT('Ctrl Pts',(56.976531744876,29.3019007898177,10.0299075200651));
#45840=CARTESIAN_POINT('Ctrl Pts',(56.9993109129814,29.0279263631165,10.0107918941993));
#45841=CARTESIAN_POINT('Ctrl Pts',(56.9964655033797,28.889749982484,10.0010854107477));
#45842=CARTESIAN_POINT('Ctrl Pts',(56.9775354058949,28.7380715721173,9.99097350566615));
#45843=CARTESIAN_POINT('Ctrl Pts',(56.9755087813167,28.7232006685105,9.98998830541222));
#45844=CARTESIAN_POINT('Ctrl Pts',(56.9724793636188,28.7027032703608,9.98864020060802));
#45845=CARTESIAN_POINT('Ctrl Pts',(56.9716200049681,28.6970565344992,9.98826985272575));
#45846=CARTESIAN_POINT('Ctrl Pts',(56.9701046355262,28.6873788799004,9.98763699892714));
#45847=CARTESIAN_POINT('Ctrl Pts',(56.9694604841787,28.6833461801242,9.98737384414405));
#45848=CARTESIAN_POINT('Ctrl Pts',(56.968091967137,28.6749443357144,9.98682678110305));
#45849=CARTESIAN_POINT('Ctrl Pts',(56.9673654306842,28.670575595047,9.98654300572342));
#45850=CARTESIAN_POINT('Ctrl Pts',(56.965565918277,28.6599732484891,9.98585590639869));
#45851=CARTESIAN_POINT('Ctrl Pts',(56.964477818784,28.653742187183,9.98545342531314));
#45852=CARTESIAN_POINT('Ctrl Pts',(56.9605177328844,28.6316842176639,9.98403302468994));
#45853=CARTESIAN_POINT('Ctrl Pts',(56.9574838828276,28.6158864965843,9.98302375292391));
#45854=CARTESIAN_POINT('Ctrl Pts',(56.94951708552,28.5769512050477,9.98055225078294));
#45855=CARTESIAN_POINT('Ctrl Pts',(56.9443629224555,28.553860923034,9.9791005464766));
#45856=CARTESIAN_POINT('Ctrl Pts',(56.9212628061124,28.4583944737858,9.97313640610307));
#45857=CARTESIAN_POINT('Ctrl Pts',(56.8996754475119,28.386956590116,9.9687630983016));
#45858=CARTESIAN_POINT('Ctrl Pts',(56.8169881925049,28.1601009400205,9.95470215577796));
#45859=CARTESIAN_POINT('Ctrl Pts',(56.7403987723663,28.0111204047871,9.9451329520471));
#45860=CARTESIAN_POINT('Ctrl Pts',(56.6344471595296,27.8563041998709,9.93356235028809));
#45861=CARTESIAN_POINT('Ctrl Pts',(56.6224694444249,27.8393749731165,9.9322740523967));
#45862=CARTESIAN_POINT('Ctrl Pts',(56.6035775823074,27.8135373818747,9.93027017498601));
#45863=CARTESIAN_POINT('Ctrl Pts',(56.5968479685092,27.8044954354465,9.92956162505039));
#45864=CARTESIAN_POINT('Ctrl Pts',(56.5852913793253,27.7892396159635,9.92835344023985));
#45865=CARTESIAN_POINT('Ctrl Pts',(56.5805035572744,27.7829963157455,9.92785533460698));
#45866=CARTESIAN_POINT('Ctrl Pts',(56.5707451524356,27.7704261050039,9.92684491292012));
#45867=CARTESIAN_POINT('Ctrl Pts',(56.5657729782752,27.7641006211836,9.92633254000641));
#45868=CARTESIAN_POINT('Ctrl Pts',(56.5534357289488,27.7485994106841,9.92506712973168));
#45869=CARTESIAN_POINT('Ctrl Pts',(56.5460275511586,27.7394585289619,9.9243123865968));
#45870=CARTESIAN_POINT('Ctrl Pts',(56.5182567663241,27.705805492649,9.92150141248882));
#45871=CARTESIAN_POINT('Ctrl Pts',(56.4973894458384,27.6817179035125,9.91942493336286));
#45872=CARTESIAN_POINT('Ctrl Pts',(56.4438669293128,27.6228466933229,9.91418266389034));
#45873=CARTESIAN_POINT('Ctrl Pts',(56.4105253612589,27.588716700212,9.91098981920189));
#45874=CARTESIAN_POINT('Ctrl Pts',(56.2380275214923,27.4243635371041,9.89483003549955));
#45875=CARTESIAN_POINT('Ctrl Pts',(56.0819570479171,27.3133762427855,9.88119559215382));
#45876=CARTESIAN_POINT('Ctrl Pts',(55.8883226319175,27.2137605166992,9.86657798900654));
#45877=CARTESIAN_POINT('Ctrl Pts',(55.8638623968812,27.2018035356543,9.86477169064446));
#45878=CARTESIAN_POINT('Ctrl Pts',(55.831892603013,27.1869786276877,9.8624694342865));
#45879=CARTESIAN_POINT('Ctrl Pts',(55.8246011290096,27.1836506991593,9.86194823733075));
#45880=CARTESIAN_POINT('Ctrl Pts',(55.812917650065,27.1784030557935,9.86111952391067));
#45881=CARTESIAN_POINT('Ctrl Pts',(55.8085385331707,27.1764551076325,9.86081034542445));
#45882=CARTESIAN_POINT('Ctrl Pts',(55.8001606095793,27.1727644958179,9.8602216334051));
#45883=CARTESIAN_POINT('Ctrl Pts',(55.7961630883288,27.1710191564822,9.85994194679333));
#45884=CARTESIAN_POINT('Ctrl Pts',(55.7867067333492,27.1669273385498,9.85928314645982));
#45885=CARTESIAN_POINT('Ctrl Pts',(55.781243034054,27.1645920915607,9.85890470733511));
#45886=CARTESIAN_POINT('Ctrl Pts',(55.7630929143796,27.1569302562574,9.85765458160374));
#45887=CARTESIAN_POINT('Ctrl Pts',(55.750361492667,27.1517103768047,9.85678902507696));
#45888=CARTESIAN_POINT('Ctrl Pts',(55.6796925758607,27.1235867248475,9.85204157713664));
#45889=CARTESIAN_POINT('Ctrl Pts',(55.6207550883577,27.1032729646532,9.84829244817451));
#45890=CARTESIAN_POINT('Ctrl Pts',(55.4088153647025,27.0411654802553,9.8352291888377));
#45891=CARTESIAN_POINT('Ctrl Pts',(55.2519020388455,27.0148776444196,9.82626528922662));
#45892=CARTESIAN_POINT('Ctrl Pts',(55.0335836777962,27.0046301481973,9.81319400996679));
#45893=CARTESIAN_POINT('Ctrl Pts',(54.9735487066553,27.0045231150141,9.80954420042224));
#45894=CARTESIAN_POINT('Ctrl Pts',(54.8985131368656,27.0077760806353,9.80487012341394));
#45895=CARTESIAN_POINT('Ctrl Pts',(54.8834304084885,27.008601687515,9.8039249845544));
#45896=CARTESIAN_POINT('Ctrl Pts',(54.8595205925043,27.0101830348796,9.80241719114877));
#45897=CARTESIAN_POINT('Ctrl Pts',(54.8506864646157,27.010826432235,9.80185803288893));
#45898=CARTESIAN_POINT('Ctrl Pts',(54.8342023672404,27.0121374112109,9.80081069074307));
#45899=CARTESIAN_POINT('Ctrl Pts',(54.8265513742967,27.012790373792,9.80032297141463));
#45900=CARTESIAN_POINT('Ctrl Pts',(54.8095098011816,27.0143439272724,9.79923298471219));
#45901=CARTESIAN_POINT('Ctrl Pts',(54.8001215030099,27.0152669861094,9.79863002687059));
#45902=CARTESIAN_POINT('Ctrl Pts',(54.7726120058559,27.0181688890737,9.79685579525983));
#45903=CARTESIAN_POINT('Ctrl Pts',(54.7545113570441,27.020329537037,9.7956788857739));
#45904=CARTESIAN_POINT('Ctrl Pts',(54.5911811373924,27.0421004323816,9.78497009870276));
#45905=CARTESIAN_POINT('Ctrl Pts',(54.4485231394684,27.0774077268452,9.77492883083884));
#45906=CARTESIAN_POINT('Ctrl Pts',(54.1925431457231,27.1716166297644,9.7559338576299));
#45907=CARTESIAN_POINT('Ctrl Pts',(54.0784403644572,27.2263862987119,9.74707793014061));
#45908=CARTESIAN_POINT('Ctrl Pts',(53.9569549464975,27.2996099100484,9.73768681087294));
#45909=CARTESIAN_POINT('Ctrl Pts',(53.943728775343,27.3077941682116,9.73666522575495));
#45910=CARTESIAN_POINT('Ctrl Pts',(53.9252669192777,27.3195190363828,9.73524187051626));
#45911=CARTESIAN_POINT('Ctrl Pts',(53.919950662539,27.3229308615527,9.73483231405498));
#45912=CARTESIAN_POINT('Ctrl Pts',(53.9109706983788,27.3287543628982,9.73414116019926));
#45913=CARTESIAN_POINT('Ctrl Pts',(53.9072986079801,27.3311529523888,9.73385871865714));
#45914=CARTESIAN_POINT('Ctrl Pts',(53.9002745310404,27.3357741648256,9.73331885798567));
#45915=CARTESIAN_POINT('Ctrl Pts',(53.896921314201,27.3379948402088,9.733061309224));
#45916=CARTESIAN_POINT('Ctrl Pts',(53.8883594841403,27.3437022573785,9.73240409067887));
#45917=CARTESIAN_POINT('Ctrl Pts',(53.8831604992021,27.3472034666383,9.73200537564485));
#45918=CARTESIAN_POINT('Ctrl Pts',(53.8642100798863,27.3600957016342,9.73055305626359));
#45919=CARTESIAN_POINT('Ctrl Pts',(53.8505594347303,27.3696346176597,9.7295088476598));
#45920=CARTESIAN_POINT('Ctrl Pts',(53.8169046124162,27.393785063307,9.7269349869487));
#45921=CARTESIAN_POINT('Ctrl Pts',(53.7970496904925,27.4086006831486,9.72541702399541));
#45922=CARTESIAN_POINT('Ctrl Pts',(53.7137906291889,27.4731769958865,9.71902979454633));
#45923=CARTESIAN_POINT('Ctrl Pts',(53.6531531755986,27.5263892383107,9.71432081920447));
#45924=CARTESIAN_POINT('Ctrl Pts',(53.4838765212235,27.6941402765568,9.7004631684836));
#45925=CARTESIAN_POINT('Ctrl Pts',(53.3854280604051,27.8180307082878,9.69137989380192));
#45926=CARTESIAN_POINT('Ctrl Pts',(53.2900633231478,27.9725207817267,9.68019192523581));
#45927=CARTESIAN_POINT('Ctrl Pts',(53.2778948316235,27.9930488112211,9.67870919637831));
#45928=CARTESIAN_POINT('Ctrl Pts',(53.2614229027687,28.0220088688517,9.67662044695475));
#45929=CARTESIAN_POINT('Ctrl Pts',(53.2568064698014,28.0302612274474,9.67602558500137));
#45930=CARTESIAN_POINT('Ctrl Pts',(53.2484622638812,28.0454294980589,9.67493266161727));
#45931=CARTESIAN_POINT('Ctrl Pts',(53.2447163235432,28.0523352404296,9.67443525491053));
#45932=CARTESIAN_POINT('Ctrl Pts',(53.2372102271168,28.0663701264627,9.67342461426553));
#45933=CARTESIAN_POINT('Ctrl Pts',(53.2334522928931,28.07350028627,9.67291131395324));
#45934=CARTESIAN_POINT('Ctrl Pts',(53.2242833787699,28.0911556240099,9.67164053931098));
#45935=CARTESIAN_POINT('Ctrl Pts',(53.2189227128478,28.1017064477949,9.67088132686099));
#45936=CARTESIAN_POINT('Ctrl Pts',(53.1992573694939,28.1412797565151,9.66803406566511));
#45937=CARTESIAN_POINT('Ctrl Pts',(53.1855662725116,28.1705999007872,9.6659250824205));
#45938=CARTESIAN_POINT('Ctrl Pts',(53.1530701165786,28.2448516047975,9.66058251691468));
#45939=CARTESIAN_POINT('Ctrl Pts',(53.1351870010847,28.2901613252473,9.65732053421681));
#45940=CARTESIAN_POINT('Ctrl Pts',(53.087007981703,28.4266616106876,9.64749429688095));
#45941=CARTESIAN_POINT('Ctrl Pts',(53.0616228603348,28.5194308407119,9.6408105480962));
#45942=CARTESIAN_POINT('Ctrl Pts',(53.0208816117651,28.7258026560622,9.62614955016616));
#45943=CARTESIAN_POINT('Ctrl Pts',(53.0084205342428,28.8396541017884,9.61819241389745));
#45944=CARTESIAN_POINT('Ctrl Pts',(53.0055328640902,28.9647238913065,9.60996833674216));
#45945=CARTESIAN_POINT('Ctrl Pts',(53.0053714639023,28.9754933620863,9.60926446488619));
#45946=CARTESIAN_POINT('Ctrl Pts',(53.0052730197494,28.9897890285981,9.60833627449039));
#45947=CARTESIAN_POINT('Ctrl Pts',(53.0052580891371,28.9933142555978,9.60810788431084));
#45948=CARTESIAN_POINT('Ctrl Pts',(53.0052508595823,28.9978772359666,9.60781291889297));
#45949=CARTESIAN_POINT('Ctrl Pts',(53.0052500251962,28.9989149398816,9.60774588249731));
#45950=CARTESIAN_POINT('Ctrl Pts',(53.0052500005621,28.9999526465424,9.60767889029237));
#45951=CARTESIAN_POINT('Ctrl Pts',(53.0052500005549,28.9999529473371,9.60767887087368));
#45952=CARTESIAN_POINT('Ctrl Pts',(53.0052499758941,29.000998421014,9.60761137725482));
#45953=CARTESIAN_POINT('Ctrl Pts',(53.005250773152,29.0020438978185,9.60754392846873));
#45954=CARTESIAN_POINT('Ctrl Pts',(53.0052578036797,29.0065833662361,9.60725126225896));
#45955=CARTESIAN_POINT('Ctrl Pts',(53.0052723951246,29.0100773799544,9.60702650522149));
#45956=CARTESIAN_POINT('Ctrl Pts',(53.0053240150624,29.0176644004869,9.6065395837483));
#45957=CARTESIAN_POINT('Ctrl Pts',(53.0053644607703,29.0217573505928,9.60627761129943));
#45958=CARTESIAN_POINT('Ctrl Pts',(53.005503607383,29.0324938046946,9.60559220016993));
#45959=CARTESIAN_POINT('Ctrl Pts',(53.0056229039718,29.0391370582672,9.60516988931161));
#45960=CARTESIAN_POINT('Ctrl Pts',(53.0061825007537,29.063513836217,9.60362643214059));
#45961=CARTESIAN_POINT('Ctrl Pts',(53.0068261641602,29.0812424682206,9.60251590105475));
#45962=CARTESIAN_POINT('Ctrl Pts',(53.0084820983296,29.1145799638644,9.60044624452814));
#45963=CARTESIAN_POINT('Ctrl Pts',(53.0094415994123,29.1301898770908,9.59948484584387));
#45964=CARTESIAN_POINT('Ctrl Pts',(53.0169604534845,29.2327922197205,9.59320695819293));
#45965=CARTESIAN_POINT('Ctrl Pts',(53.0290309706326,29.3192034122154,9.58811224818012));
#45966=CARTESIAN_POINT('Ctrl Pts',(53.0466870746609,29.4044702439035,9.58304844318572));
#45967=CARTESIAN_POINT('',(53.0052509575277,28.9983381707197,9.45054880350992));
#45968=CARTESIAN_POINT('Ctrl Pts',(53.0466869980009,29.4044698736881,9.42363003822484));
#45969=CARTESIAN_POINT('Ctrl Pts',(53.0459416970957,29.4008705797895,9.42386071017391));
#45970=CARTESIAN_POINT('Ctrl Pts',(53.0452063454643,29.39726923002,9.42409169317728));
#45971=CARTESIAN_POINT('Ctrl Pts',(53.042735689669,29.3849963486351,9.42487947785384));
#45972=CARTESIAN_POINT('Ctrl Pts',(53.0410481227673,29.376315436298,9.42543776448021));
#45973=CARTESIAN_POINT('Ctrl Pts',(53.0380029722169,29.3600752802278,9.42648431520925));
#45974=CARTESIAN_POINT('Ctrl Pts',(53.0366312084331,29.3525188364851,9.42697212099367));
#45975=CARTESIAN_POINT('Ctrl Pts',(53.0340280434432,29.3376924565463,9.42793098056701));
#45976=CARTESIAN_POINT('Ctrl Pts',(53.0327932462526,29.3304232358528,9.42840191856188));
#45977=CARTESIAN_POINT('Ctrl Pts',(53.0301021431149,29.3140308080912,9.42946581604622));
#45978=CARTESIAN_POINT('Ctrl Pts',(53.0286688671776,29.3049040423193,9.43005948974283));
#45979=CARTESIAN_POINT('Ctrl Pts',(53.0252105952784,29.2818381886003,9.43156334767361));
#45980=CARTESIAN_POINT('Ctrl Pts',(53.0232697702393,29.2678871768863,9.43247613613497));
#45981=CARTESIAN_POINT('Ctrl Pts',(53.010597734152,29.1691466070122,9.43896009296105));
#45982=CARTESIAN_POINT('Ctrl Pts',(53.0051794209271,29.0837777997029,9.44469429247309));
#45983=CARTESIAN_POINT('Ctrl Pts',(53.0052506940152,28.9983360368706,9.45054848948101));
#45984=CARTESIAN_POINT('Ctrl Pts',(53.0052506922627,28.9983381391186,9.4505483454417));
#45985=CARTESIAN_POINT('Ctrl Pts',(53.0053360688677,28.8958596912809,9.45756983960953));
#45986=CARTESIAN_POINT('Ctrl Pts',(53.0133185283999,28.7935409683466,9.46474865672663));
#45987=CARTESIAN_POINT('Ctrl Pts',(53.0417524955803,28.6114204569449,9.47755645448682));
#45988=CARTESIAN_POINT('Ctrl Pts',(53.0593460938601,28.5313929905911,9.48319153730964));
#45989=CARTESIAN_POINT('Ctrl Pts',(53.0861323595426,28.4375176667941,9.48965343160242));
#45990=CARTESIAN_POINT('Ctrl Pts',(53.0906342468335,28.4224204141284,9.49068785799599));
#45991=CARTESIAN_POINT('Ctrl Pts',(53.0971783369115,28.4013877451173,9.49212073586949));
#45992=CARTESIAN_POINT('Ctrl Pts',(53.0990702685024,28.3954066890209,9.49252726625751));
#45993=CARTESIAN_POINT('Ctrl Pts',(53.1023429541446,28.3852278269214,9.49321740277765));
#45994=CARTESIAN_POINT('Ctrl Pts',(53.1037094909693,28.3810255293687,9.49350182104717));
#45995=CARTESIAN_POINT('Ctrl Pts',(53.1063696633716,28.3729366149144,9.49404828209716));
#45996=CARTESIAN_POINT('Ctrl Pts',(53.1076613134889,28.3690494179567,9.49431044262206));
#45997=CARTESIAN_POINT('Ctrl Pts',(53.1107974350566,28.3597075781107,9.49493946354938));
#45998=CARTESIAN_POINT('Ctrl Pts',(53.1126535812137,28.354256851091,9.4953056493554));
#45999=CARTESIAN_POINT('Ctrl Pts',(53.1195474751755,28.3342960250955,9.49664384706668));
#46000=CARTESIAN_POINT('Ctrl Pts',(53.1247293166695,28.319835771151,9.49760785453345));
#46001=CARTESIAN_POINT('Ctrl Pts',(53.1755413179797,28.1830384014123,9.50668876950381));
#46002=CARTESIAN_POINT('Ctrl Pts',(53.2329192510483,28.0653818655933,9.51421608376746));
#46003=CARTESIAN_POINT('Ctrl Pts',(53.343425568204,27.8859015597017,9.52645647427454));
#46004=CARTESIAN_POINT('Ctrl Pts',(53.3895315308279,27.8202353933873,9.53111945293398));
#46005=CARTESIAN_POINT('Ctrl Pts',(53.4672402839038,27.7226338684504,9.5385504370169));
#46006=CARTESIAN_POINT('Ctrl Pts',(53.4961801786764,27.6886868676587,9.54123842635654));
#46007=CARTESIAN_POINT('Ctrl Pts',(53.5465529826735,27.6334610827604,9.54581594942825));
#46008=CARTESIAN_POINT('Ctrl Pts',(53.567375608819,27.6116470010812,9.54768147987465));
#46009=CARTESIAN_POINT('Ctrl Pts',(53.5965462103473,27.5824426645817,9.55026419949747));
#46010=CARTESIAN_POINT('Ctrl Pts',(53.6044741536321,27.5746372591323,9.55096313130802));
#46011=CARTESIAN_POINT('Ctrl Pts',(53.6176322581613,27.56189754124,9.55211850213845));
#46012=CARTESIAN_POINT('Ctrl Pts',(53.6228246111244,27.5569243950305,9.55257325416506));
#46013=CARTESIAN_POINT('Ctrl Pts',(53.6337063205593,27.5466142994162,9.55352392727902));
#46014=CARTESIAN_POINT('Ctrl Pts',(53.6394003149998,27.5412824442345,9.55402005415353));
#46015=CARTESIAN_POINT('Ctrl Pts',(53.6526651782905,27.5290064656959,9.55517288012548));
#46016=CARTESIAN_POINT('Ctrl Pts',(53.6602586571839,27.5220872056808,9.55583061067058));
#46017=CARTESIAN_POINT('Ctrl Pts',(53.6851645613722,27.4997423573191,9.55798102065656));
#46018=CARTESIAN_POINT('Ctrl Pts',(53.70269204625,27.4845603860608,9.55948369911505));
#46019=CARTESIAN_POINT('Ctrl Pts',(53.8487892743152,27.3624059680822,9.57192759293028));
#46020=CARTESIAN_POINT('Ctrl Pts',(53.9900595205541,27.2717063888752,9.58353597148203));
#46021=CARTESIAN_POINT('Ctrl Pts',(54.207842460338,27.1677860628093,9.60034511316957));
#46022=CARTESIAN_POINT('Ctrl Pts',(54.276469392384,27.1396166148063,9.60548955985397));
#46023=CARTESIAN_POINT('Ctrl Pts',(54.3687790892687,27.1076091008016,9.61209451489979));
#46024=CARTESIAN_POINT('Ctrl Pts',(54.3911854622391,27.1002820961431,9.61367385542165));
#46025=CARTESIAN_POINT('Ctrl Pts',(54.4290507003729,27.0886387575816,9.61629713395748));
#46026=CARTESIAN_POINT('Ctrl Pts',(54.4444408744317,27.0841088238704,9.61735082704268));
#46027=CARTESIAN_POINT('Ctrl Pts',(54.4659670015113,27.078054048192,9.61880563409571));
#46028=CARTESIAN_POINT('Ctrl Pts',(54.4720576044124,27.0763720955708,9.61921515133751));
#46029=CARTESIAN_POINT('Ctrl Pts',(54.482429374154,27.0735608467089,9.61990882631535));
#46030=CARTESIAN_POINT('Ctrl Pts',(54.4867064679319,27.072416820097,9.62019381622719));
#46031=CARTESIAN_POINT('Ctrl Pts',(54.4949375083668,27.0702445408815,9.62074017174274));
#46032=CARTESIAN_POINT('Ctrl Pts',(54.4988908318044,27.0692141872465,9.62100166190868));
#46033=CARTESIAN_POINT('Ctrl Pts',(54.5083844573914,27.0667709884579,9.62162746434251));
#46034=CARTESIAN_POINT('Ctrl Pts',(54.5139277609839,27.0653697942057,9.62199111717304));
#46035=CARTESIAN_POINT('Ctrl Pts',(54.5340857271592,27.0603665263138,9.62330742317342));
#46036=CARTESIAN_POINT('Ctrl Pts',(54.5487354462649,27.0569059579732,9.62425241733721));
#46037=CARTESIAN_POINT('Ctrl Pts',(54.6972737366062,27.0235886971723,9.63372971889622));
#46038=CARTESIAN_POINT('Ctrl Pts',(54.8338841506935,27.0074485383128,9.64160856401191));
#46039=CARTESIAN_POINT('Ctrl Pts',(55.1076711734894,27.0034795333221,9.65751678658724));
#46040=CARTESIAN_POINT('Ctrl Pts',(55.2440791306989,27.0155339251103,9.66551404193645));
#46041=CARTESIAN_POINT('Ctrl Pts',(55.3959234597077,27.0448532392174,9.6751048628551));
#46042=CARTESIAN_POINT('Ctrl Pts',(55.413622082804,27.0485208221932,9.67623298081443));
#46043=CARTESIAN_POINT('Ctrl Pts',(55.4404474455923,27.0544609989755,9.67795947653587));
#46044=CARTESIAN_POINT('Ctrl Pts',(55.4496122926045,27.0565585323131,9.67855229915918));
#46045=CARTESIAN_POINT('Ctrl Pts',(55.4655133706311,27.0603162646877,9.67958615727658));
#46046=CARTESIAN_POINT('Ctrl Pts',(55.4722564565403,27.061946974783,9.68002624514899));
#46047=CARTESIAN_POINT('Ctrl Pts',(55.4873622339189,27.0656835874223,9.68101592894047));
#46048=CARTESIAN_POINT('Ctrl Pts',(55.4957200112584,27.0678086022267,9.68156612911156));
#46049=CARTESIAN_POINT('Ctrl Pts',(55.5180331267686,27.0736361455722,9.68304218227929));
#46050=CARTESIAN_POINT('Ctrl Pts',(55.5319622775878,27.077436051199,9.68397114219285));
#46051=CARTESIAN_POINT('Ctrl Pts',(55.5944062635061,27.0952014688741,9.68817038106894));
#46052=CARTESIAN_POINT('Ctrl Pts',(55.6424179645967,27.1108534578942,9.69149449666976));
#46053=CARTESIAN_POINT('Ctrl Pts',(55.8631616941933,27.1922049157091,9.70723759566076));
#46054=CARTESIAN_POINT('Ctrl Pts',(56.0268137616826,27.2798821530425,9.7203604592127));
#46055=CARTESIAN_POINT('Ctrl Pts',(56.219636844515,27.4206238315568,9.73671485530023));
#46056=CARTESIAN_POINT('Ctrl Pts',(56.2619445606678,27.454218586595,9.74035869072997));
#46057=CARTESIAN_POINT('Ctrl Pts',(56.3099935952219,27.4956617481897,9.74451631665368));
#46058=CARTESIAN_POINT('Ctrl Pts',(56.3171029937693,27.5018823452057,9.74513199006277));
#46059=CARTESIAN_POINT('Ctrl Pts',(56.3279865516533,27.5115426277974,9.74607492724682));
#46060=CARTESIAN_POINT('Ctrl Pts',(56.3317920290417,27.5149465925349,9.74640470924202));
#46061=CARTESIAN_POINT('Ctrl Pts',(56.3387808784571,27.5212465244928,9.74701044127508));
#46062=CARTESIAN_POINT('Ctrl Pts',(56.3419679355262,27.5241381695752,9.74728669072402));
#46063=CARTESIAN_POINT('Ctrl Pts',(56.3491504332117,27.530697415725,9.74790933427302));
#46064=CARTESIAN_POINT('Ctrl Pts',(56.3531402837717,27.5343710054415,9.74825527197328));
#46065=CARTESIAN_POINT('Ctrl Pts',(56.3649062378751,27.5452933170343,9.74927579282326));
#46066=CARTESIAN_POINT('Ctrl Pts',(56.3726395785295,27.5525881129492,9.7499470144441));
#46067=CARTESIAN_POINT('Ctrl Pts',(56.4499211104742,27.6266636044718,9.75666404576276));
#46068=CARTESIAN_POINT('Ctrl Pts',(56.5146087759355,27.6983512733615,9.76236613089779));
#46069=CARTESIAN_POINT('Ctrl Pts',(56.6395177159165,27.8587601040813,9.77423558020565));
#46070=CARTESIAN_POINT('Ctrl Pts',(56.6982893321938,27.9482111100355,9.78037242202436));
#46071=CARTESIAN_POINT('Ctrl Pts',(56.7753296469176,28.088902235911,9.78985568581314));
#46072=CARTESIAN_POINT('Ctrl Pts',(56.7991432882776,28.1368793303052,9.79306062131764));
#46073=CARTESIAN_POINT('Ctrl Pts',(56.8304832998937,28.2069687799051,9.79774412149385));
#46074=CARTESIAN_POINT('Ctrl Pts',(56.8395976856202,28.2283472824962,9.7991727267698));
#46075=CARTESIAN_POINT('Ctrl Pts',(56.8552230825568,28.2668490799455,9.80174889416493));
#46076=CARTESIAN_POINT('Ctrl Pts',(56.8618757290859,28.2839122313541,9.80289172880693));
#46077=CARTESIAN_POINT('Ctrl Pts',(56.8716038384508,28.3099159792574,9.80463616493265));
#46078=CARTESIAN_POINT('Ctrl Pts',(56.8748523528716,28.318791123227,9.80523203040897));
#46079=CARTESIAN_POINT('Ctrl Pts',(56.8806260680405,28.3349194517617,9.80631589150973));
#46080=CARTESIAN_POINT('Ctrl Pts',(56.883172696741,28.3421648116684,9.80680316927669));
#46081=CARTESIAN_POINT('Ctrl Pts',(56.888561886439,28.3577852507839,9.8078545871825));
#46082=CARTESIAN_POINT('Ctrl Pts',(56.8913907052689,28.3661648645643,9.80841916656646));
#46083=CARTESIAN_POINT('Ctrl Pts',(56.8988815608539,28.3888512491494,9.80994927715174));
#46084=CARTESIAN_POINT('Ctrl Pts',(56.9034375194463,28.403192185941,9.81091824153763));
#46085=CARTESIAN_POINT('Ctrl Pts',(56.9251742786741,28.4743955588294,9.81573868131982));
#46086=CARTESIAN_POINT('Ctrl Pts',(56.9399698718405,28.5319490216354,9.81966612755386));
#46087=CARTESIAN_POINT('Ctrl Pts',(56.9800688781851,28.7229101178879,9.83280433425878));
#46088=CARTESIAN_POINT('Ctrl Pts',(56.9943286854381,28.8582369062114,9.84231208604171));
#46089=CARTESIAN_POINT('Ctrl Pts',(56.9949923949745,29.0767891165306,9.85750172841403));
#46090=CARTESIAN_POINT('Ctrl Pts',(56.9900824657855,29.1595801791502,9.86320822322789));
#46091=CARTESIAN_POINT('Ctrl Pts',(56.9781154026179,29.2575618268934,9.86974294992048));
#46092=CARTESIAN_POINT('Ctrl Pts',(56.9760069651293,29.2732675468439,9.87078354183027));
#46093=CARTESIAN_POINT('Ctrl Pts',(56.9728007347376,29.2951683548048,9.87222344242186));
#46094=CARTESIAN_POINT('Ctrl Pts',(56.971860524448,29.3013854199484,9.87263093316545));
#46095=CARTESIAN_POINT('Ctrl Pts',(56.9702090978858,29.3119667021194,9.87332220639564));
#46096=CARTESIAN_POINT('Ctrl Pts',(56.9695127430637,29.3163331613723,9.87360680745689));
#46097=CARTESIAN_POINT('Ctrl Pts',(56.968143889916,29.3247367248853,9.87415323042804));
#46098=CARTESIAN_POINT('Ctrl Pts',(56.9674734822896,29.328774100442,9.87441517228775));
#46099=CARTESIAN_POINT('Ctrl Pts',(56.965832164826,29.3384737290061,9.87504314515319));
#46100=CARTESIAN_POINT('Ctrl Pts',(56.9648492040429,29.3441339460175,9.87540850650723));
#46101=CARTESIAN_POINT('Ctrl Pts',(56.9611657809141,29.3648139595006,9.87673964521521));
#46102=CARTESIAN_POINT('Ctrl Pts',(56.9583173570028,29.3798073295202,9.87769753006313));
#46103=CARTESIAN_POINT('Ctrl Pts',(56.9290256875976,29.5248901405142,9.88690930303182));
#46104=CARTESIAN_POINT('Ctrl Pts',(56.8898266658836,29.6520851490981,9.89455289946474));
#46105=CARTESIAN_POINT('Ctrl Pts',(56.7836444059424,29.904122816633,9.91043733821508));
#46106=CARTESIAN_POINT('Ctrl Pts',(56.7154587988827,30.0276280791224,9.9186572198982));
#46107=CARTESIAN_POINT('Ctrl Pts',(56.6244826906004,30.1577612851378,9.92850396082088));
#46108=CARTESIAN_POINT('Ctrl Pts',(56.6139102949083,30.1724541491756,9.92963371510011));
#46109=CARTESIAN_POINT('Ctrl Pts',(56.597541739919,30.1945611952276,9.93136220630375));
#46110=CARTESIAN_POINT('Ctrl Pts',(56.5918904706328,30.2020818543581,9.93195536811335));
#46111=CARTESIAN_POINT('Ctrl Pts',(56.581530993039,30.2156669861914,9.93303637448017));
#46112=CARTESIAN_POINT('Ctrl Pts',(56.5768405427671,30.2217448192102,9.93352351947392));
#46113=CARTESIAN_POINT('Ctrl Pts',(56.5666506743015,30.2347923085853,9.93457698730869));
#46114=CARTESIAN_POINT('Ctrl Pts',(56.5611395956579,30.2417526079383,9.93514376425288));
#46115=CARTESIAN_POINT('Ctrl Pts',(56.5460709382021,30.260524924223,9.93668560544819));
#46116=CARTESIAN_POINT('Ctrl Pts',(56.53642471704,30.2722647123701,9.9376641921941));
#46117=CARTESIAN_POINT('Ctrl Pts',(56.4872186143846,30.3307744816435,9.94261528462617));
#46118=CARTESIAN_POINT('Ctrl Pts',(56.4456570318063,30.3758104342456,9.94666881979499));
#46119=CARTESIAN_POINT('Ctrl Pts',(56.2900758247581,30.529553162102,9.96141419288964));
#46120=CARTESIAN_POINT('Ctrl Pts',(56.1653495569065,30.6265848223277,9.97253177881446));
#46121=CARTESIAN_POINT('Ctrl Pts',(55.9910987118607,30.7317254031406,9.98657241061256));
#46122=CARTESIAN_POINT('Ctrl Pts',(55.9508422835098,30.7541519424434,9.98971988688185));
#46123=CARTESIAN_POINT('Ctrl Pts',(55.8943499612955,30.7831065022833,9.99397378403834));
#46124=CARTESIAN_POINT('Ctrl Pts',(55.8787530821983,30.790844414494,9.99513161158623));
#46125=CARTESIAN_POINT('Ctrl Pts',(55.8515867512439,30.8038817635485,9.99711725392325));
#46126=CARTESIAN_POINT('Ctrl Pts',(55.8400644126504,30.8092764339178,9.9979499292518));
#46127=CARTESIAN_POINT('Ctrl Pts',(55.8232546074597,30.8169514436016,9.99915012083318));
#46128=CARTESIAN_POINT('Ctrl Pts',(55.8180079112515,30.8193195860626,9.99952267888443));
#46129=CARTESIAN_POINT('Ctrl Pts',(55.8087917209322,30.8234314658229,10.0001734270476));
#46130=CARTESIAN_POINT('Ctrl Pts',(55.8048266971107,30.8251850173134,10.000452204058));
#46131=CARTESIAN_POINT('Ctrl Pts',(55.7963818471959,30.8288869236203,10.0010433993271));
#46132=CARTESIAN_POINT('Ctrl Pts',(55.7919005704293,30.8308317546181,10.0013556058933));
#46133=CARTESIAN_POINT('Ctrl Pts',(55.7796653729336,30.8360883852332,10.0022040244171));
#46134=CARTESIAN_POINT('Ctrl Pts',(55.7718974222734,30.8393675618542,10.0027383124441));
#46135=CARTESIAN_POINT('Ctrl Pts',(55.7351861414385,30.8545914029928,10.0052439169423));
#46136=CARTESIAN_POINT('Ctrl Pts',(55.7059832527734,30.8659034902259,10.0071803615581));
#46137=CARTESIAN_POINT('Ctrl Pts',(55.4833665999367,30.9461612293699,10.0216042786443));
#46138=CARTESIAN_POINT('Ctrl Pts',(55.2806014413385,30.9855654544182,10.0329598561837));
#46139=CARTESIAN_POINT('Ctrl Pts',(55.0205587099119,30.9953980999633,10.0485880663818));
#46140=CARTESIAN_POINT('Ctrl Pts',(54.9656885783205,30.9952087979307,10.0519356417687));
#46141=CARTESIAN_POINT('Ctrl Pts',(54.8966663524097,30.9921226627856,10.0562414441393));
#46142=CARTESIAN_POINT('Ctrl Pts',(54.8824408601993,30.9913338189283,10.0571338969357));
#46143=CARTESIAN_POINT('Ctrl Pts',(54.8596623148908,30.989825756979,10.0585714988692));
#46144=CARTESIAN_POINT('Ctrl Pts',(54.8511031645073,30.9892035938218,10.0591136243213));
#46145=CARTESIAN_POINT('Ctrl Pts',(54.8348559724147,30.9879171404027,10.0601464981653));
#46146=CARTESIAN_POINT('Ctrl Pts',(54.827167231888,30.987263429567,10.0606369078677));
#46147=CARTESIAN_POINT('Ctrl Pts',(54.8096697139541,30.9856734454236,10.0617567211384));
#46148=CARTESIAN_POINT('Ctrl Pts',(54.7998637524608,30.984709078516,10.0623869900399));
#46149=CARTESIAN_POINT('Ctrl Pts',(54.7743974470396,30.9820139473264,10.064031020264));
#46150=CARTESIAN_POINT('Ctrl Pts',(54.7587499928447,30.9801702476956,10.0650482748138));
#46151=CARTESIAN_POINT('Ctrl Pts',(54.6129358232106,30.9612353966709,10.0745961132229));
#46152=CARTESIAN_POINT('Ctrl Pts',(54.4847565821058,30.9315215476126,10.0835309761045));
#46153=CARTESIAN_POINT('Ctrl Pts',(54.2698834093651,30.8587895409991,10.0992867036722));
#46154=CARTESIAN_POINT('Ctrl Pts',(54.1816413926526,30.8216636711942,10.1059939321268));
#46155=CARTESIAN_POINT('Ctrl Pts',(54.0459512514499,30.7527181313321,10.116436364918));
#46156=CARTESIAN_POINT('Ctrl Pts',(53.9966097122881,30.7249461087004,10.1202609216073));
#46157=CARTESIAN_POINT('Ctrl Pts',(53.9403943409392,30.6900753396555,10.1245963202701));
#46158=CARTESIAN_POINT('Ctrl Pts',(53.9323131197786,30.6849817627873,10.125218988419));
#46159=CARTESIAN_POINT('Ctrl Pts',(53.9199500020293,30.6770646567884,10.1261703355741));
#46160=CARTESIAN_POINT('Ctrl Pts',(53.9156420163624,30.6742824211915,10.1265016020197));
#46161=CARTESIAN_POINT('Ctrl Pts',(53.9077399701651,30.6691357333901,10.1271087340785));
#46162=CARTESIAN_POINT('Ctrl Pts',(53.9041428402204,30.666776276315,10.1273849094593));
#46163=CARTESIAN_POINT('Ctrl Pts',(53.8960511044921,30.66143116393,10.128005732962));
#46164=CARTESIAN_POINT('Ctrl Pts',(53.8915609702659,30.6584389031172,10.1283499366483));
#46165=CARTESIAN_POINT('Ctrl Pts',(53.8783681618668,30.6495695971501,10.1293605747934));
#46166=CARTESIAN_POINT('Ctrl Pts',(53.8696995317367,30.6436419010416,10.1300237437421));
#46167=CARTESIAN_POINT('Ctrl Pts',(53.7978441631585,30.5936691512846,10.1355169785491));
#46168=CARTESIAN_POINT('Ctrl Pts',(53.7372026165893,30.5460613348966,10.1401289402219));
#46169=CARTESIAN_POINT('Ctrl Pts',(53.570576160553,30.3988853932701,10.1532093808646));
#46170=CARTESIAN_POINT('Ctrl Pts',(53.4725259012915,30.2911067530876,10.1614653410175));
#46171=CARTESIAN_POINT('Ctrl Pts',(53.3494357415144,30.1219412049327,10.1739544003478));
#46172=CARTESIAN_POINT('Ctrl Pts',(53.3143326301787,30.0684749480322,10.1778380972421));
#46173=CARTESIAN_POINT('Ctrl Pts',(53.2742761830909,30.0005636627152,10.1827471833781));
#46174=CARTESIAN_POINT('Ctrl Pts',(53.2668380374022,29.9876233734652,10.1836814787001));
#46175=CARTESIAN_POINT('Ctrl Pts',(53.2552802890311,29.966983411356,10.1851705192136));
#46176=CARTESIAN_POINT('Ctrl Pts',(53.2510647288182,29.9593378971974,10.1857218405727));
#46177=CARTESIAN_POINT('Ctrl Pts',(53.2432298588933,29.9449049683259,10.1867622493972));
#46178=CARTESIAN_POINT('Ctrl Pts',(53.2395993433071,29.9381237941058,10.1872509290967));
#46179=CARTESIAN_POINT('Ctrl Pts',(53.231521273635,29.9228233385789,10.1883533012213));
#46180=CARTESIAN_POINT('Ctrl Pts',(53.2270959077578,29.9142926195885,10.1889677577493));
#46181=CARTESIAN_POINT('Ctrl Pts',(53.215943098064,29.8924080415755,10.1905438131376));
#46182=CARTESIAN_POINT('Ctrl Pts',(53.2093039429204,29.8790100984037,10.1915084448982));
#46183=CARTESIAN_POINT('Ctrl Pts',(53.1675495408933,29.792312296337,10.1977501970633));
#46184=CARTESIAN_POINT('Ctrl Pts',(53.1367958100224,29.7170080939009,10.2031747726119));
#46185=CARTESIAN_POINT('Ctrl Pts',(53.0845700925143,29.5628491908539,10.2142760587746));
#46186=CARTESIAN_POINT('Ctrl Pts',(53.0631910746295,29.4841733732124,10.219939613526));
#46187=CARTESIAN_POINT('Ctrl Pts',(53.046686906026,29.4044694295118,10.2256126172116));
#46188=CARTESIAN_POINT('Origin',(55.,29.,3.45145488139523));
#46189=CARTESIAN_POINT('',(53.0466869981205,29.4044698742655,11.1853016190124));
#46190=CARTESIAN_POINT('',(53.0466869605703,29.4044696929239,11.0269053946991));
#46191=CARTESIAN_POINT('',(53.0466869980082,29.4044698737233,3.45145488139523));
#46192=CARTESIAN_POINT('Ctrl Pts',(53.0466869981205,29.4044698742655,11.1853016190124));
#46193=CARTESIAN_POINT('Ctrl Pts',(53.0479173957098,29.4104118535368,11.184903118068));
#46194=CARTESIAN_POINT('Ctrl Pts',(53.0491749170844,29.4163482693752,11.1845037845888));
#46195=CARTESIAN_POINT('Ctrl Pts',(53.0612457493572,29.4720758323217,11.1807436998875));
#46196=CARTESIAN_POINT('Ctrl Pts',(53.073935115407,29.5214374187202,11.1773269476064));
#46197=CARTESIAN_POINT('Ctrl Pts',(53.1370384659788,29.7329601762889,11.1623207508052));
#46198=CARTESIAN_POINT('Ctrl Pts',(53.2061450379722,29.8887813661741,11.1502458245123));
#46199=CARTESIAN_POINT('Ctrl Pts',(53.3086358224714,30.0578736706919,11.1368086806637));
#46200=CARTESIAN_POINT('Ctrl Pts',(53.3236321127687,30.0814806293452,11.1349264384882));
#46201=CARTESIAN_POINT('Ctrl Pts',(53.3492149677126,30.1199413102985,11.1318587351635));
#46202=CARTESIAN_POINT('Ctrl Pts',(53.3595173270891,30.1349785978192,11.1306590437985));
#46203=CARTESIAN_POINT('Ctrl Pts',(53.3738541828781,30.1553014647984,11.129039535674));
#46204=CARTESIAN_POINT('Ctrl Pts',(53.3777107475931,30.1607106778413,11.1286086657285));
#46205=CARTESIAN_POINT('Ctrl Pts',(53.3842203626667,30.1697452309607,11.1278894683531));
#46206=CARTESIAN_POINT('Ctrl Pts',(53.3868587385396,30.1733810180536,11.1276001636494));
#46207=CARTESIAN_POINT('Ctrl Pts',(53.3918817450293,30.1802539579623,11.1270535557052));
#46208=CARTESIAN_POINT('Ctrl Pts',(53.3942639111198,30.1834928562604,11.1267960825059));
#46209=CARTESIAN_POINT('Ctrl Pts',(53.4005282873806,30.1919564468405,11.1261235224744));
#46210=CARTESIAN_POINT('Ctrl Pts',(53.4044263450956,30.197169430461,11.1257095181733));
#46211=CARTESIAN_POINT('Ctrl Pts',(53.4180393422656,30.2151898803768,11.1242788679372));
#46212=CARTESIAN_POINT('Ctrl Pts',(53.4278838233706,30.2278993173337,11.1232707362546));
#46213=CARTESIAN_POINT('Ctrl Pts',(53.5019203996787,30.3211318586019,11.115870373929));
#46214=CARTESIAN_POINT('Ctrl Pts',(53.5721167289946,30.3967056303169,11.1098390345751));
#46215=CARTESIAN_POINT('Ctrl Pts',(53.711862243571,30.5255526901074,11.0987812377998));
#46216=CARTESIAN_POINT('Ctrl Pts',(53.7796759668888,30.5803223307149,11.0937552727402));
#46217=CARTESIAN_POINT('Ctrl Pts',(53.8971812832609,30.6631390302291,11.0852756192782));
#46218=CARTESIAN_POINT('Ctrl Pts',(53.9448812926906,30.693801743741,11.0818905250617));
#46219=CARTESIAN_POINT('Ctrl Pts',(54.0146825961297,30.7345780404748,11.0769653965981));
#46220=CARTESIAN_POINT('Ctrl Pts',(54.0357645831624,30.7463852244605,11.075481551706));
#46221=CARTESIAN_POINT('Ctrl Pts',(54.0735719803378,30.7666663503262,11.0728233446672));
#46222=CARTESIAN_POINT('Ctrl Pts',(54.0902123710778,30.7752930186779,11.0716543365598));
#46223=CARTESIAN_POINT('Ctrl Pts',(54.1154543093734,30.787930781863,11.0698813405863));
#46224=CARTESIAN_POINT('Ctrl Pts',(54.1239672621804,30.7921172385842,11.0692834401493));
#46225=CARTESIAN_POINT('Ctrl Pts',(54.1392941516113,30.7995193165221,11.0682069072867));
#46226=CARTESIAN_POINT('Ctrl Pts',(54.1460970978525,30.8027573766767,11.0677290595288));
#46227=CARTESIAN_POINT('Ctrl Pts',(54.1607322937888,30.8096219976689,11.0667009392318));
#46228=CARTESIAN_POINT('Ctrl Pts',(54.1685700407108,30.8132364093234,11.0661502621887));
#46229=CARTESIAN_POINT('Ctrl Pts',(54.1896112181133,30.8227745343384,11.0646715818871));
#46230=CARTESIAN_POINT('Ctrl Pts',(54.2028558693172,30.8286055336138,11.0637404523625));
#46231=CARTESIAN_POINT('Ctrl Pts',(54.2628790592461,30.8542549024386,11.0595182625735));
#46232=CARTESIAN_POINT('Ctrl Pts',(54.3103373569291,30.8724244171051,11.0561726463161));
#46233=CARTESIAN_POINT('Ctrl Pts',(54.5330619060581,30.9480784776424,11.0404281760269));
#46234=CARTESIAN_POINT('Ctrl Pts',(54.7150649256158,30.9828852408997,11.0273305334125));
#46235=CARTESIAN_POINT('Ctrl Pts',(54.9531032915996,30.9949287553075,11.0110024958234));
#46236=CARTESIAN_POINT('Ctrl Pts',(55.0070957009292,30.9954675712134,11.0073606422615));
#46237=CARTESIAN_POINT('Ctrl Pts',(55.0704890120499,30.9935265415539,11.0032049707928));
#46238=CARTESIAN_POINT('Ctrl Pts',(55.0799277550418,30.9931704229922,11.0025893767182));
#46239=CARTESIAN_POINT('Ctrl Pts',(55.0944641096882,30.9925185468703,11.0016465348096));
#46240=CARTESIAN_POINT('Ctrl Pts',(55.0995635591539,30.9922702444036,11.0013167695369));
#46241=CARTESIAN_POINT('Ctrl Pts',(55.1089595725383,30.9917765671847,11.000711052944));
#46242=CARTESIAN_POINT('Ctrl Pts',(55.1132562776703,30.9915368684109,11.0004348023314));
#46243=CARTESIAN_POINT('Ctrl Pts',(55.1229665896756,30.9909636352675,10.9998121370069));
#46244=CARTESIAN_POINT('Ctrl Pts',(55.1283796244238,30.9906219261404,10.9994661788346));
#46245=CARTESIAN_POINT('Ctrl Pts',(55.1443994302832,30.9895450255104,10.9984455417617));
#46246=CARTESIAN_POINT('Ctrl Pts',(55.1550019892645,30.9887470927683,10.9977742255248));
#46247=CARTESIAN_POINT('Ctrl Pts',(55.2588827455396,30.9800933644161,10.9912334696443));
#46248=CARTESIAN_POINT('Ctrl Pts',(55.3515180749092,30.9657644204252,10.9856877460274));
#46249=CARTESIAN_POINT('Ctrl Pts',(55.4830098840597,30.9358275740894,10.9778074504149));
#46250=CARTESIAN_POINT('Ctrl Pts',(55.5229119951667,30.9254324365484,10.9754154090299));
#46251=CARTESIAN_POINT('Ctrl Pts',(55.7030022551476,30.8725043358041,10.9645155078979));
#46252=CARTESIAN_POINT('Ctrl Pts',(55.8385435394685,30.815852949008,10.9559798898452));
#46253=CARTESIAN_POINT('Ctrl Pts',(55.9820615388183,30.736344700073,10.9457991949431));
#46254=CARTESIAN_POINT('Ctrl Pts',(55.9973542254578,30.7276059451016,10.9446994248852));
#46255=CARTESIAN_POINT('Ctrl Pts',(56.0205471010052,30.7139421766547,10.9430075271734));
#46256=CARTESIAN_POINT('Ctrl Pts',(56.0285321184148,30.7091623231774,10.9424206139127));
#46257=CARTESIAN_POINT('Ctrl Pts',(56.0424023387193,30.7007271737196,10.9413932595839));
#46258=CARTESIAN_POINT('Ctrl Pts',(56.0483025343716,30.6970967413966,10.9409537276399));
#46259=CARTESIAN_POINT('Ctrl Pts',(56.0615612288514,30.688843048078,10.9399602872031));
#46260=CARTESIAN_POINT('Ctrl Pts',(56.0689086300643,30.6842023097892,10.9394057444101));
#46261=CARTESIAN_POINT('Ctrl Pts',(56.0886369614801,30.6715604777657,10.937905735818));
#46262=CARTESIAN_POINT('Ctrl Pts',(56.1009597175034,30.6634700315696,10.9369569847941));
#46263=CARTESIAN_POINT('Ctrl Pts',(56.1577384577369,30.6252849613021,10.9325293727329));
#46264=CARTESIAN_POINT('Ctrl Pts',(56.2010540858673,30.5935425080134,10.9289892165654));
#46265=CARTESIAN_POINT('Ctrl Pts',(56.370142381797,30.4588183006083,10.9144885636206));
#46266=CARTESIAN_POINT('Ctrl Pts',(56.4843870804772,30.3423943466993,10.9030265472225));
#46267=CARTESIAN_POINT('Ctrl Pts',(56.6228996924192,30.1616701758897,10.8872942103337));
#46268=CARTESIAN_POINT('Ctrl Pts',(56.6600146073323,30.1079865511835,10.8828447958437));
#46269=CARTESIAN_POINT('Ctrl Pts',(56.7018652099514,30.040615501885,10.8776075479342));
#46270=CARTESIAN_POINT('Ctrl Pts',(56.7091683818849,30.0285763388076,10.8766845751651));
#46271=CARTESIAN_POINT('Ctrl Pts',(56.7193997067,30.0113002413017,10.8753795228245));
#46272=CARTESIAN_POINT('Ctrl Pts',(56.7224324712386,30.0061261917491,10.8749911236577));
#46273=CARTESIAN_POINT('Ctrl Pts',(56.7276350274129,29.9971578997408,10.874322237993));
#46274=CARTESIAN_POINT('Ctrl Pts',(56.7298157534512,29.993370084897,10.8740410600041));
#46275=CARTESIAN_POINT('Ctrl Pts',(56.7343495700943,29.9854348623235,10.8734548234153));
#46276=CARTESIAN_POINT('Ctrl Pts',(56.7367002511536,29.9812861651738,10.8731499163506));
#46277=CARTESIAN_POINT('Ctrl Pts',(56.7429082084445,29.9702376124107,10.8723420143372));
#46278=CARTESIAN_POINT('Ctrl Pts',(56.7467394328504,29.9633231058578,10.871840644242));
#46279=CARTESIAN_POINT('Ctrl Pts',(56.763105813286,29.9333667534069,10.8696859537068));
#46280=CARTESIAN_POINT('Ctrl Pts',(56.7752275405135,29.9101005103275,10.8680567871382));
#46281=CARTESIAN_POINT('Ctrl Pts',(56.8806455135975,29.6976372627188,10.8535149778111));
#46282=CARTESIAN_POINT('Ctrl Pts',(56.9438476582421,29.4949812605348,10.8418855281712));
#46283=CARTESIAN_POINT('Ctrl Pts',(56.9793533405505,29.2500399628906,10.827025941114));
#46284=CARTESIAN_POINT('Ctrl Pts',(56.9835965967408,29.21378479698,10.8248111297885));
#46285=CARTESIAN_POINT('Ctrl Pts',(56.9891602693871,29.1514851699476,10.8209652043284));
#46286=CARTESIAN_POINT('Ctrl Pts',(56.9909690288687,29.1254932779681,10.8193488151818));
#46287=CARTESIAN_POINT('Ctrl Pts',(56.992810643918,29.0886094747079,10.8170351632214));
#46288=CARTESIAN_POINT('Ctrl Pts',(56.9932642323921,29.0777405552135,10.8163509364347));
#46289=CARTESIAN_POINT('Ctrl Pts',(56.993892821994,29.0589997160505,10.8151667218523));
#46290=CARTESIAN_POINT('Ctrl Pts',(56.9941101610349,29.0511293934325,10.8146680586413));
#46291=CARTESIAN_POINT('Ctrl Pts',(56.9944370761235,29.0360579777306,10.8137104752412));
#46292=CARTESIAN_POINT('Ctrl Pts',(56.9945542585883,29.0288571602491,10.81325179936));
#46293=CARTESIAN_POINT('Ctrl Pts',(56.9947377917281,29.0119527398768,10.8121722290512));
#46294=CARTESIAN_POINT('Ctrl Pts',(56.9947723333937,29.002249041973,10.8115503564651));
#46295=CARTESIAN_POINT('Ctrl Pts',(56.994647120394,28.96874299574,10.8093953987938));
#46296=CARTESIAN_POINT('Ctrl Pts',(56.9941321359902,28.944944767473,10.8078513828529));
#46297=CARTESIAN_POINT('Ctrl Pts',(56.9872369048706,28.7706181310325,10.7964382816055));
#46298=CARTESIAN_POINT('Ctrl Pts',(56.96424702481,28.6212599827965,10.786041848419));
#46299=CARTESIAN_POINT('Ctrl Pts',(56.8939010301089,28.3629038921197,10.7673795819106));
#46300=CARTESIAN_POINT('Ctrl Pts',(56.8532208825915,28.2527847747689,10.7592059604423));
#46301=CARTESIAN_POINT('Ctrl Pts',(56.7976056360496,28.1352417241513,10.75063518569));
#46302=CARTESIAN_POINT('Ctrl Pts',(56.7919938366106,28.1236718602279,10.749793457039));
#46303=CARTESIAN_POINT('Ctrl Pts',(56.7836972318426,28.1069797484381,10.748582696393));
#46304=CARTESIAN_POINT('Ctrl Pts',(56.7811015522182,28.1018139127747,10.7482085004851));
#46305=CARTESIAN_POINT('Ctrl Pts',(56.7765185975514,28.0927910608531,10.747555900586));
#46306=CARTESIAN_POINT('Ctrl Pts',(56.7745411482423,28.0889291458236,10.7472768988925));
#46307=CARTESIAN_POINT('Ctrl Pts',(56.7703166265176,28.0807446836479,10.7466863268141));
#46308=CARTESIAN_POINT('Ctrl Pts',(56.7680663143756,28.0764239046193,10.7463749614147));
#46309=CARTESIAN_POINT('Ctrl Pts',(56.7619064716202,28.0647015374453,10.745531224554));
#46310=CARTESIAN_POINT('Ctrl Pts',(56.7579660929301,28.0573161448546,10.7450007413924));
#46311=CARTESIAN_POINT('Ctrl Pts',(56.7393686967835,28.0229814886399,10.7425386128614));
#46312=CARTESIAN_POINT('Ctrl Pts',(56.7241368926758,27.996346250165,10.7406403968461));
#46313=CARTESIAN_POINT('Ctrl Pts',(56.6019263594041,27.7936412023188,10.7262030553403));
#46314=CARTESIAN_POINT('Ctrl Pts',(56.4688612769897,27.6347391440333,10.7148138465871));
#46315=CARTESIAN_POINT('Ctrl Pts',(56.2724894900143,27.4628556887063,10.699141639253));
#46316=CARTESIAN_POINT('Ctrl Pts',(56.229703036479,27.4284174349074,10.6957908767106));
#46317=CARTESIAN_POINT('Ctrl Pts',(56.1740920263018,27.3873194408094,10.6914814773104));
#46318=CARTESIAN_POINT('Ctrl Pts',(56.1625404088881,27.3789724082071,10.6905887518947));
#46319=CARTESIAN_POINT('Ctrl Pts',(56.1438904645085,27.3657981058144,10.6891508145615));
#46320=CARTESIAN_POINT('Ctrl Pts',(56.1368485600079,27.3608915308453,10.6886086288669));
#46321=CARTESIAN_POINT('Ctrl Pts',(56.1234159129372,27.3516602927348,10.6875757076763));
#46322=CARTESIAN_POINT('Ctrl Pts',(56.1170312973135,27.3473269585053,10.6870853113305));
#46323=CARTESIAN_POINT('Ctrl Pts',(56.1024384251102,27.337545749628,10.6859656226645));
#46324=CARTESIAN_POINT('Ctrl Pts',(56.0942146795669,27.3321214537507,10.6853354657309));
#46325=CARTESIAN_POINT('Ctrl Pts',(56.0727399293934,27.318184117613,10.6836919206335));
#46326=CARTESIAN_POINT('Ctrl Pts',(56.0594278867333,27.3097668362873,10.682675042638));
#46327=CARTESIAN_POINT('Ctrl Pts',(55.9340270504829,27.2325386027843,10.6731119944592));
#46328=CARTESIAN_POINT('Ctrl Pts',(55.8155106487474,27.1748268703832,10.6641599451784));
#46329=CARTESIAN_POINT('Ctrl Pts',(55.6020376745032,27.0958412660723,10.6483501118685));
#46330=CARTESIAN_POINT('Ctrl Pts',(55.5095802179762,27.0690420951221,10.6416056283205));
#46331=CARTESIAN_POINT('Ctrl Pts',(55.3608951535313,27.0373729641743,10.6311797646546));
#46332=CARTESIAN_POINT('Ctrl Pts',(55.3057699006022,27.0280324025505,10.6274046216544));
#46333=CARTESIAN_POINT('Ctrl Pts',(55.2408713594164,27.0198234276597,10.6231177368504));
#46334=CARTESIAN_POINT('Ctrl Pts',(55.231413963883,27.0186959205171,10.6224969289618));
#46335=CARTESIAN_POINT('Ctrl Pts',(55.2168582063221,27.0170662345597,10.6215478175747));
#46336=CARTESIAN_POINT('Ctrl Pts',(55.2117655336011,27.0165159037767,10.6212169451255));
#46337=CARTESIAN_POINT('Ctrl Pts',(55.2023915699497,27.0155394373256,10.6206101861181));
#46338=CARTESIAN_POINT('Ctrl Pts',(55.1981110352372,27.0151075367222,10.6203339925379));
#46339=CARTESIAN_POINT('Ctrl Pts',(55.1884515891324,27.0141644697298,10.6197126927414));
#46340=CARTESIAN_POINT('Ctrl Pts',(55.1830719868308,27.0136613068226,10.6193680341015));
#46341=CARTESIAN_POINT('Ctrl Pts',(55.1671972038752,27.0122415529256,10.6183548081336));
#46342=CARTESIAN_POINT('Ctrl Pts',(55.1566965381588,27.0113862227185,10.6176895313233));
#46343=CARTESIAN_POINT('Ctrl Pts',(55.0665914375948,27.0047648811474,10.612019428782));
#46344=CARTESIAN_POINT('Ctrl Pts',(54.9867039625937,27.0036974297328,10.6072490160118));
#46345=CARTESIAN_POINT('Ctrl Pts',(54.7797659816205,27.0133601742127,10.5950765589432));
#46346=CARTESIAN_POINT('Ctrl Pts',(54.6534355426449,27.0314638439355,10.5878102759338));
#46347=CARTESIAN_POINT('Ctrl Pts',(54.4798802030211,27.0735706225143,10.5772330332545));
#46348=CARTESIAN_POINT('Ctrl Pts',(54.4305564535005,27.0875700711281,10.5741597757567));
#46349=CARTESIAN_POINT('Ctrl Pts',(54.3603872276319,27.1104414125342,10.5696534696104));
#46350=CARTESIAN_POINT('Ctrl Pts',(54.3390662326753,27.1177931439971,10.568266066649));
#46351=CARTESIAN_POINT('Ctrl Pts',(54.3010706376584,27.1316196606291,10.5657579652111));
#46352=CARTESIAN_POINT('Ctrl Pts',(54.2843496323999,27.1379602944284,10.564641634116));
#46353=CARTESIAN_POINT('Ctrl Pts',(54.2590079767507,27.1479616538364,10.5629295174205));
#46354=CARTESIAN_POINT('Ctrl Pts',(54.250323833365,27.1514598044487,10.5623391440559));
#46355=CARTESIAN_POINT('Ctrl Pts',(54.235252037774,27.1576547047003,10.5613079910349));
#46356=CARTESIAN_POINT('Ctrl Pts',(54.2288531736067,27.1603238863828,10.5608681430407));
#46357=CARTESIAN_POINT('Ctrl Pts',(54.2145019829606,27.1663982815804,10.5598769531324));
#46358=CARTESIAN_POINT('Ctrl Pts',(54.2065576699362,27.1698219590532,10.5593249947485));
#46359=CARTESIAN_POINT('Ctrl Pts',(54.1853019587432,27.1791467171951,10.5578392495165));
#46360=CARTESIAN_POINT('Ctrl Pts',(54.1720326874393,27.1851419651319,10.5569022841117));
#46361=CARTESIAN_POINT('Ctrl Pts',(54.1118692052364,27.2131218269267,10.5526098664729));
#46362=CARTESIAN_POINT('Ctrl Pts',(54.0657802010192,27.2367806514338,10.5491975868977));
#46363=CARTESIAN_POINT('Ctrl Pts',(53.8609279150984,27.3522249210113,10.5334474576494));
#46364=CARTESIAN_POINT('Ctrl Pts',(53.7143722319871,27.4638389675572,10.5204262365663));
#46365=CARTESIAN_POINT('Ctrl Pts',(53.5471728835833,27.6320730994778,10.5041781176262));
#46366=CARTESIAN_POINT('Ctrl Pts',(53.5107516800801,27.6718165755646,10.5005423337591));
#46367=CARTESIAN_POINT('Ctrl Pts',(53.4698898958908,27.7202032301406,10.4963926498353));
#46368=CARTESIAN_POINT('Ctrl Pts',(53.4638494511345,27.727459940722,10.4957773001635));
#46369=CARTESIAN_POINT('Ctrl Pts',(53.4546228365756,27.7387058065863,10.4948347522434));
#46370=CARTESIAN_POINT('Ctrl Pts',(53.4514001721478,27.7426646453096,10.4945050389598));
#46371=CARTESIAN_POINT('Ctrl Pts',(53.4454886793395,27.7499837455226,10.4938993710734));
#46372=CARTESIAN_POINT('Ctrl Pts',(53.4427955392515,27.7533403228703,10.4936231175417));
#46373=CARTESIAN_POINT('Ctrl Pts',(53.4367320774332,27.7609477847521,10.4930003870121));
#46374=CARTESIAN_POINT('Ctrl Pts',(53.4333682252884,27.7652037115515,10.4926543669801));
#46375=CARTESIAN_POINT('Ctrl Pts',(53.4234601155921,27.7778450608105,10.4916333764883));
#46376=CARTESIAN_POINT('Ctrl Pts',(53.4169653986011,27.7862693194231,10.4909617721521));
#46377=CARTESIAN_POINT('Ctrl Pts',(53.3506008822971,27.8737892988014,10.4840699691063));
#46378=CARTESIAN_POINT('Ctrl Pts',(53.2966346134733,27.9572057746131,10.4782138183344));
#46379=CARTESIAN_POINT('Ctrl Pts',(53.1881314881602,28.1559911507267,10.4650028524586));
#46380=CARTESIAN_POINT('Ctrl Pts',(53.1379975507274,28.2732510592699,10.4577085693707));
#46381=CARTESIAN_POINT('Ctrl Pts',(53.0811457175145,28.4517010914942,10.4465002439396));
#46382=CARTESIAN_POINT('Ctrl Pts',(53.0655119645662,28.5097057585235,10.4428451306343));
#46383=CARTESIAN_POINT('Ctrl Pts',(53.0493482015937,28.5826275201633,10.4381928876952));
#46384=CARTESIAN_POINT('Ctrl Pts',(53.046335308905,28.5969659042384,10.437275502051));
#46385=CARTESIAN_POINT('Ctrl Pts',(53.0417912933126,28.6198402932392,10.4358072478891));
#46386=CARTESIAN_POINT('Ctrl Pts',(53.0401573745232,28.6283555178188,10.4352596389853));
#46387=CARTESIAN_POINT('Ctrl Pts',(53.0371772654387,28.6444528542036,10.4342223585928));
#46388=CARTESIAN_POINT('Ctrl Pts',(53.0358193602937,28.6520326565767,10.4337330673491));
#46389=CARTESIAN_POINT('Ctrl Pts',(53.0328496574708,28.6691809486894,10.4326240746163));
#46390=CARTESIAN_POINT('Ctrl Pts',(53.0312637300384,28.6787536635291,10.432003570335));
#46391=CARTESIAN_POINT('Ctrl Pts',(53.0273637659834,28.7034082541043,10.4304016148792));
#46392=CARTESIAN_POINT('Ctrl Pts',(53.0251528556004,28.7185055765894,10.42941695894));
#46393=CARTESIAN_POINT('Ctrl Pts',(53.0111433060758,28.8224770909891,10.4226091811801));
#46394=CARTESIAN_POINT('Ctrl Pts',(53.0051764273415,28.9120211813228,10.4166051860083));
#46395=CARTESIAN_POINT('Ctrl Pts',(53.0053199386138,29.0852451139712,10.40474182193));
#46396=CARTESIAN_POINT('Ctrl Pts',(53.0106437099445,29.1687467095709,10.3989125419693));
#46397=CARTESIAN_POINT('Ctrl Pts',(53.0266490509963,29.2945956694281,10.3900729023009));
#46398=CARTESIAN_POINT('Ctrl Pts',(53.0335050515345,29.3373401353415,10.3870619400876));
#46399=CARTESIAN_POINT('Ctrl Pts',(53.0433414089626,29.388052704001,10.3834990366669));
#46400=CARTESIAN_POINT('Ctrl Pts',(53.0449883625416,29.3962666255798,10.3829222587101));
#46401=CARTESIAN_POINT('Ctrl Pts',(53.0466869980528,29.4044698739386,10.38234667127));
#46402=CARTESIAN_POINT('Ctrl Pts',(53.046686906026,29.4044694295118,10.2256126172116));
#46403=CARTESIAN_POINT('Ctrl Pts',(53.0350407226984,29.3482262607362,10.2296157780208));
#46404=CARTESIAN_POINT('Ctrl Pts',(53.0258218492307,29.2914710729161,10.2336223948554));
#46405=CARTESIAN_POINT('Ctrl Pts',(53.0139553736562,29.1911698338599,10.2405792198535));
#46406=CARTESIAN_POINT('Ctrl Pts',(53.0102590915804,29.1478200512932,10.2435455173555));
#46407=CARTESIAN_POINT('Ctrl Pts',(53.0071062847788,29.0876518767495,10.2475787081908));
#46408=CARTESIAN_POINT('Ctrl Pts',(53.0064404082734,29.0709112546044,10.2486918633672));
#46409=CARTESIAN_POINT('Ctrl Pts',(53.0056502091502,29.0418203681737,10.2506084139827));
#46410=CARTESIAN_POINT('Ctrl Pts',(53.005429534729,29.0294738671999,10.2514162463307));
#46411=CARTESIAN_POINT('Ctrl Pts',(53.0052746918278,29.0114389476523,10.2525873706492));
#46412=CARTESIAN_POINT('Ctrl Pts',(53.0052501855137,29.0057518792958,10.252955376216));
#46413=CARTESIAN_POINT('Ctrl Pts',(53.0052498607057,28.9957378010465,10.2536010117082));
#46414=CARTESIAN_POINT('Ctrl Pts',(53.0052637986602,28.991410880354,10.2538791984862));
#46415=CARTESIAN_POINT('Ctrl Pts',(53.0053237018397,28.9821596742046,10.2544722838053));
#46416=CARTESIAN_POINT('Ctrl Pts',(53.0053738218267,28.9772355041171,10.254786951314));
#46417=CARTESIAN_POINT('Ctrl Pts',(53.0055616906364,28.963702257855,10.2556490924921));
#46418=CARTESIAN_POINT('Ctrl Pts',(53.0057369467571,28.9550936890837,10.2561945361551));
#46419=CARTESIAN_POINT('Ctrl Pts',(53.0069977259391,28.9081143910642,10.2591562739429));
#46420=CARTESIAN_POINT('Ctrl Pts',(53.0091349875553,28.8697771872304,10.2615189698474));
#46421=CARTESIAN_POINT('Ctrl Pts',(53.019586270932,28.7464774220151,10.269010849271));
#46422=CARTESIAN_POINT('Ctrl Pts',(53.032246465273,28.661975556857,10.273983407082));
#46423=CARTESIAN_POINT('Ctrl Pts',(53.0821684856085,28.4310316076204,10.28771179323));
#46424=CARTESIAN_POINT('Ctrl Pts',(53.1306857634178,28.2876370783362,10.2964324430252));
#46425=CARTESIAN_POINT('Ctrl Pts',(53.2050263701861,28.1295615073894,10.3071923573722));
#46426=CARTESIAN_POINT('Ctrl Pts',(53.2155344597733,28.108217424236,10.3086698410969));
#46427=CARTESIAN_POINT('Ctrl Pts',(53.2308614757275,28.0784412317783,10.3107683386989));
#46428=CARTESIAN_POINT('Ctrl Pts',(53.2353643392029,28.0698480442936,10.3113783947861));
#46429=CARTESIAN_POINT('Ctrl Pts',(53.24331848095,28.0549341500002,10.3124451134721));
#46430=CARTESIAN_POINT('Ctrl Pts',(53.2467416628636,28.0485986013929,10.3129007841581));
#46431=CARTESIAN_POINT('Ctrl Pts',(53.2539794183607,28.0353748457618,10.3138572351222));
#46432=CARTESIAN_POINT('Ctrl Pts',(53.2578006142291,28.0284904236114,10.3143582440335));
#46433=CARTESIAN_POINT('Ctrl Pts',(53.2669992972825,28.0121465065167,10.3155550931965));
#46434=CARTESIAN_POINT('Ctrl Pts',(53.2724135783117,28.0027081128945,10.3162522372658));
#46435=CARTESIAN_POINT('Ctrl Pts',(53.2910612276461,27.9708083454527,10.3186291357621));
#46436=CARTESIAN_POINT('Ctrl Pts',(53.3046571312825,27.9485630590077,10.3203218656568));
#46437=CARTESIAN_POINT('Ctrl Pts',(53.3383407352497,27.8958033127008,10.3244239187341));
#46438=CARTESIAN_POINT('Ctrl Pts',(53.3588377833842,27.8655626339511,10.3268475452018));
#46439=CARTESIAN_POINT('Ctrl Pts',(53.5036790097016,27.6640152125446,10.343501870294));
#46440=CARTESIAN_POINT('Ctrl Pts',(53.6537460258476,27.5129196402236,10.3587083204905));
#46441=CARTESIAN_POINT('Ctrl Pts',(53.8454512160862,27.3731311190602,10.3746090677654));
#46442=CARTESIAN_POINT('Ctrl Pts',(53.8664633857991,27.3584214479719,10.3763086787094));
#46443=CARTESIAN_POINT('Ctrl Pts',(53.8942609989628,27.33974994105,10.3784955172523));
#46444=CARTESIAN_POINT('Ctrl Pts',(53.9007932989818,27.3354178812729,10.379005061237));
#46445=CARTESIAN_POINT('Ctrl Pts',(53.9113279967889,27.3285205872392,10.379819626343));
#46446=CARTESIAN_POINT('Ctrl Pts',(53.9153142458423,27.3259310128522,10.3801262139349));
#46447=CARTESIAN_POINT('Ctrl Pts',(53.9229882947404,27.320984662802,10.3807132385846));
#46448=CARTESIAN_POINT('Ctrl Pts',(53.9266746154415,27.3186257599857,10.3809938084781));
#46449=CARTESIAN_POINT('Ctrl Pts',(53.9354605608555,27.3130442401722,10.3816592212217));
#46450=CARTESIAN_POINT('Ctrl Pts',(53.940567145963,27.3098325576558,10.3820433502638));
#46451=CARTESIAN_POINT('Ctrl Pts',(53.9578162253593,27.2990929927712,10.3833323320043));
#46452=CARTESIAN_POINT('Ctrl Pts',(53.9700253293506,27.2916721998946,10.38423052009));
#46453=CARTESIAN_POINT('Ctrl Pts',(54.0400560904264,27.2501306681416,10.3893085001337));
#46454=CARTESIAN_POINT('Ctrl Pts',(54.0994973549946,27.2188116755968,10.3933344535615));
#46455=CARTESIAN_POINT('Ctrl Pts',(54.3160514350864,27.1183301816542,10.4074116833743));
#46456=CARTESIAN_POINT('Ctrl Pts',(54.4803524552498,27.066496715233,10.4171007556858));
#46457=CARTESIAN_POINT('Ctrl Pts',(54.6928507255704,27.0285418110605,10.4301569637365));
#46458=CARTESIAN_POINT('Ctrl Pts',(54.7366828672855,27.0222103981964,10.4328723853485));
#46459=CARTESIAN_POINT('Ctrl Pts',(54.7943780152452,27.0158284099807,10.4364923205691));
#46460=CARTESIAN_POINT('Ctrl Pts',(54.8080840464261,27.0144558551782,10.4373555950078));
#46461=CARTESIAN_POINT('Ctrl Pts',(54.8302467709426,27.0124680440881,10.4387573358217));
#46462=CARTESIAN_POINT('Ctrl Pts',(54.8386952488474,27.011764549097,10.4392930453349));
#46463=CARTESIAN_POINT('Ctrl Pts',(54.8548662731484,27.0105217543932,10.4403211487774));
#46464=CARTESIAN_POINT('Ctrl Pts',(54.862587992884,27.0099735112418,10.4408132543663));
#46465=CARTESIAN_POINT('Ctrl Pts',(54.8803433233945,27.008816712521,10.4419476078609));
#46466=CARTESIAN_POINT('Ctrl Pts',(54.8903786684757,27.0082390298562,10.4425908042254));
#46467=CARTESIAN_POINT('Ctrl Pts',(54.9217625901733,27.0066703211804,10.4446089515019));
#46468=CARTESIAN_POINT('Ctrl Pts',(54.9431224280297,27.0059465443453,10.4459921359856));
#46469=CARTESIAN_POINT('Ctrl Pts',(55.0481797974832,27.0040759980108,10.4528449994996));
#46470=CARTESIAN_POINT('Ctrl Pts',(55.1318704857231,27.0078551995579,10.4584644013651));
#46471=CARTESIAN_POINT('Ctrl Pts',(55.3237270353406,27.0286618493743,10.4716876386143));
#46472=CARTESIAN_POINT('Ctrl Pts',(55.4312306644319,27.0493562326891,10.4793561429385));
#46473=CARTESIAN_POINT('Ctrl Pts',(55.6158140029894,27.1008992570814,10.492649588523));
#46474=CARTESIAN_POINT('Ctrl Pts',(55.6936999077347,27.1279438821387,10.4982959963964));
#46475=CARTESIAN_POINT('Ctrl Pts',(55.7794478044841,27.1638081887538,10.5044001791477));
#46476=CARTESIAN_POINT('Ctrl Pts',(55.7891651861763,27.167963546166,10.5050902103229));
#46477=CARTESIAN_POINT('Ctrl Pts',(55.8038066109382,27.1743626418544,10.5061267839308));
#46478=CARTESIAN_POINT('Ctrl Pts',(55.8087551239265,27.1765494296717,10.5064765837486));
#46479=CARTESIAN_POINT('Ctrl Pts',(55.8176231437749,27.1805114812061,10.5071023909059));
#46480=CARTESIAN_POINT('Ctrl Pts',(55.8215458428407,27.1822793106631,10.5073788342229));
#46481=CARTESIAN_POINT('Ctrl Pts',(55.8301207040129,27.1861771428477,10.5079822959901));
#46482=CARTESIAN_POINT('Ctrl Pts',(55.8347703955529,27.1883123535018,10.5083089933811));
#46483=CARTESIAN_POINT('Ctrl Pts',(55.8480268890261,27.194461812322,10.5092390569006));
#46484=CARTESIAN_POINT('Ctrl Pts',(55.8566134478797,27.198519730605,10.5098398309845));
#46485=CARTESIAN_POINT('Ctrl Pts',(55.9149166143125,27.2265843210733,10.5139100252239));
#46486=CARTESIAN_POINT('Ctrl Pts',(55.9636518427676,27.2525870798069,10.5172672302328));
#46487=CARTESIAN_POINT('Ctrl Pts',(56.1853549714155,27.3829783601173,10.5326151036141));
#46488=CARTESIAN_POINT('Ctrl Pts',(56.3428973653652,27.5112215840867,10.5438708305135));
#46489=CARTESIAN_POINT('Ctrl Pts',(56.5023590486919,27.6872898844324,10.5583419401807));
#46490=CARTESIAN_POINT('Ctrl Pts',(56.5255062890806,27.7142625142157,10.5605323358436));
#46491=CARTESIAN_POINT('Ctrl Pts',(56.5559173241261,27.7516772772596,10.5635439997119));
#46492=CARTESIAN_POINT('Ctrl Pts',(56.5638207852027,27.7615926035183,10.5643396524925));
#46493=CARTESIAN_POINT('Ctrl Pts',(56.5761954366325,27.7774246478945,10.5656065473039));
#46494=CARTESIAN_POINT('Ctrl Pts',(56.5807291739131,27.7832922198068,10.5660753161907));
#46495=CARTESIAN_POINT('Ctrl Pts',(56.5899321204793,27.7953409521138,10.5670364379988));
#46496=CARTESIAN_POINT('Ctrl Pts',(56.5945982446578,27.80152429947,10.5675289000155));
#46497=CARTESIAN_POINT('Ctrl Pts',(56.605259469547,27.8158245813264,10.5686661201026));
#46498=CARTESIAN_POINT('Ctrl Pts',(56.6112291910843,27.8239600880884,10.5693118429407));
#46499=CARTESIAN_POINT('Ctrl Pts',(56.6297701179323,27.8496337361131,10.5713459192947));
#46500=CARTESIAN_POINT('Ctrl Pts',(56.6421182859114,27.8673302982771,10.5727426933415));
#46501=CARTESIAN_POINT('Ctrl Pts',(56.7018391537842,27.9559479068702,10.5797137639257));
#46502=CARTESIAN_POINT('Ctrl Pts',(56.7449107445599,28.029647271972,10.5854437215525));
#46503=CARTESIAN_POINT('Ctrl Pts',(56.8348137828815,28.2089372016656,10.5991979691759));
#46504=CARTESIAN_POINT('Ctrl Pts',(56.8774616090698,28.3162913452631,10.607301680632));
#46505=CARTESIAN_POINT('Ctrl Pts',(56.9158326236954,28.4441718255519,10.6165402510007));
#46506=CARTESIAN_POINT('Ctrl Pts',(56.9208302197223,28.4616962821369,10.6177971678152));
#46507=CARTESIAN_POINT('Ctrl Pts',(56.9290439595196,28.4920705440284,10.6199576824002));
#46508=CARTESIAN_POINT('Ctrl Pts',(56.9323735170887,28.5048883633434,10.6208639131236));
#46509=CARTESIAN_POINT('Ctrl Pts',(56.9464615495164,28.5614312406258,10.6248349599033));
#46510=CARTESIAN_POINT('Ctrl Pts',(56.9558662656171,28.6054838785606,10.6278593601577));
#46511=CARTESIAN_POINT('Ctrl Pts',(56.9652700431564,28.6582193667054,10.6313694031988));
#46512=CARTESIAN_POINT('Ctrl Pts',(56.9667138358292,28.6666277786656,10.6319257428232));
#46513=CARTESIAN_POINT('Ctrl Pts',(56.9689848385807,28.6803822183651,10.6328300997086));
#46514=CARTESIAN_POINT('Ctrl Pts',(56.9698443094873,28.6857227037458,10.6331798366538));
#46515=CARTESIAN_POINT('Ctrl Pts',(56.9713484150483,28.6953173760913,10.6338055774295));
#46516=CARTESIAN_POINT('Ctrl Pts',(56.9720010162079,28.6995701946013,10.6340820168166));
#46517=CARTESIAN_POINT('Ctrl Pts',(56.9733996605177,28.7088857128001,10.6346855238921));
#46518=CARTESIAN_POINT('Ctrl Pts',(56.9741399838849,28.7139491762335,10.6350122701672));
#46519=CARTESIAN_POINT('Ctrl Pts',(56.9761990774471,28.7284212315035,10.6359426132004));
#46520=CARTESIAN_POINT('Ctrl Pts',(56.9774701498546,28.7378366233103,10.6365436154714));
#46521=CARTESIAN_POINT('Ctrl Pts',(56.9856803637684,28.8021137369989,10.640619644003));
#46522=CARTESIAN_POINT('Ctrl Pts',(56.9904035269121,28.8572397402892,10.6439820863451));
#46523=CARTESIAN_POINT('Ctrl Pts',(57.0017560467262,29.1157834878625,10.6594236973491));
#46524=CARTESIAN_POINT('Ctrl Pts',(56.9795276978379,29.3192372298545,10.6707591252862));
#46525=CARTESIAN_POINT('Ctrl Pts',(56.918028907439,29.5489721143186,10.6852625930721));
#46526=CARTESIAN_POINT('Ctrl Pts',(56.9083011262369,29.5818864735817,10.6873792934897));
#46527=CARTESIAN_POINT('Ctrl Pts',(56.8938765195091,29.6264309378896,10.690304705856));
#46528=CARTESIAN_POINT('Ctrl Pts',(56.8899116326901,29.6382930365026,10.6910896869985));
#46529=CARTESIAN_POINT('Ctrl Pts',(56.8834297425095,29.6570954697695,10.6923437677455));
#46530=CARTESIAN_POINT('Ctrl Pts',(56.8809852655695,29.664060599425,10.6928104838228));
#46531=CARTESIAN_POINT('Ctrl Pts',(56.8758917249126,29.6783199993225,10.6937704809354));
#46532=CARTESIAN_POINT('Ctrl Pts',(56.8732386446973,29.685612691185,10.6942638876669));
#46533=CARTESIAN_POINT('Ctrl Pts',(56.8670035068345,29.7024452336274,10.6954084717785));
#46534=CARTESIAN_POINT('Ctrl Pts',(56.8633907912754,29.7119734218592,10.6960606557505));
#46535=CARTESIAN_POINT('Ctrl Pts',(56.8517075832032,29.7420886343454,10.6981358304062));
#46536=CARTESIAN_POINT('Ctrl Pts',(56.8433679274945,29.7625687732652,10.6995677339656));
#46537=CARTESIAN_POINT('Ctrl Pts',(56.7995789965492,29.8651853943119,10.7068499338198));
#46538=CARTESIAN_POINT('Ctrl Pts',(56.7589778640264,29.9449991381945,10.7128721331996));
#46539=CARTESIAN_POINT('Ctrl Pts',(56.6604405534051,30.1102064157275,10.7260907744026));
#46540=CARTESIAN_POINT('Ctrl Pts',(56.6009558802444,30.1943867739529,10.73331019486));
#46541=CARTESIAN_POINT('Ctrl Pts',(56.482979896208,30.3365999390005,10.7461255235278));
#46542=CARTESIAN_POINT('Ctrl Pts',(56.426878599694,30.3963342512788,10.7517364140023));
#46543=CARTESIAN_POINT('Ctrl Pts',(56.3595680370643,30.4596964989118,10.7578074190578));
#46544=CARTESIAN_POINT('Ctrl Pts',(56.3518199140318,30.4668749258188,10.7584970388792));
#46545=CARTESIAN_POINT('Ctrl Pts',(56.340018235709,30.4776359310917,10.7595331183805));
#46546=CARTESIAN_POINT('Ctrl Pts',(56.3360066686391,30.4812639872418,10.7598828309417));
#46547=CARTESIAN_POINT('Ctrl Pts',(56.3287775352729,30.4877487477433,10.7605085459773));
#46548=CARTESIAN_POINT('Ctrl Pts',(56.3255654519433,30.4906113874324,10.7607849838447));
#46549=CARTESIAN_POINT('Ctrl Pts',(56.3185125646593,30.4968561615193,10.7613885085125));
#46550=CARTESIAN_POINT('Ctrl Pts',(56.3146680045797,30.5002339119567,10.761715273762));
#46551=CARTESIAN_POINT('Ctrl Pts',(56.3036481380033,30.5098408460756,10.7626457252992));
#46552=CARTESIAN_POINT('Ctrl Pts',(56.2964411490592,30.5160337079596,10.7632468161508));
#46553=CARTESIAN_POINT('Ctrl Pts',(56.2469657134213,30.5579364054363,10.767325113329));
#46554=CARTESIAN_POINT('Ctrl Pts',(56.2032673768529,30.5919290710427,10.7706895921694));
#46555=CARTESIAN_POINT('Ctrl Pts',(55.9920541777211,30.7425566662864,10.7861683262419));
#46556=CARTESIAN_POINT('Ctrl Pts',(55.8087050722569,30.8348516582826,10.7975353488147));
#46557=CARTESIAN_POINT('Ctrl Pts',(55.5823396905267,30.9081543563048,10.8120519231057));
#46558=CARTESIAN_POINT('Ctrl Pts',(55.5498891720246,30.9177576109,10.8141396307958));
#46559=CARTESIAN_POINT('Ctrl Pts',(55.5051991105093,30.9297554558347,10.8170310409521));
#46560=CARTESIAN_POINT('Ctrl Pts',(55.4931570295078,30.9328679193741,10.8178117335872));
#46561=CARTESIAN_POINT('Ctrl Pts',(55.4739360547926,30.9376445675464,10.8190606697128));
#46562=CARTESIAN_POINT('Ctrl Pts',(55.4667755562385,30.9393819716401,10.8195265653349));
#46563=CARTESIAN_POINT('Ctrl Pts',(55.4520482564599,30.9428690776637,10.8204861451413));
#46564=CARTESIAN_POINT('Ctrl Pts',(55.4444805428587,30.9446143379468,10.8209799618274));
#46565=CARTESIAN_POINT('Ctrl Pts',(55.4269195650122,30.9485563725602,10.8221276503424));
#46566=CARTESIAN_POINT('Ctrl Pts',(55.416919275081,30.9507205242393,10.8227825463726));
#46567=CARTESIAN_POINT('Ctrl Pts',(55.3850337483867,30.9573644527695,10.8248751301049));
#46568=CARTESIAN_POINT('Ctrl Pts',(55.3630903336494,30.9615534484491,10.8263219435899));
#46569=CARTESIAN_POINT('Ctrl Pts',(55.2511602236223,30.9809784316085,10.8337386835625));
#46570=CARTESIAN_POINT('Ctrl Pts',(55.1602860144448,30.9903922589665,10.8398878143379));
#46571=CARTESIAN_POINT('Ctrl Pts',(54.9828251411902,30.9965431117853,10.852100186989));
#46572=CARTESIAN_POINT('Ctrl Pts',(54.8964526215905,30.9939298406651,10.8581365283839));
#46573=CARTESIAN_POINT('Ctrl Pts',(54.7147616270727,30.9765932393952,10.8708354484242));
#46574=CARTESIAN_POINT('Ctrl Pts',(54.6197723353993,30.9605389720721,10.8774746793239));
#46575=CARTESIAN_POINT('Ctrl Pts',(54.5159771247606,30.9351647013695,10.8844928999035));
#46576=CARTESIAN_POINT('Ctrl Pts',(54.5056710087397,30.9325577418094,10.8851870471155));
#46577=CARTESIAN_POINT('Ctrl Pts',(54.4901390399321,30.928496506684,10.8862285632749));
#46578=CARTESIAN_POINT('Ctrl Pts',(54.4848976621158,30.9271031519031,10.8865792348255));
#46579=CARTESIAN_POINT('Ctrl Pts',(54.4755075754509,30.9245658674375,10.8872059640997));
#46580=CARTESIAN_POINT('Ctrl Pts',(54.4713568417557,30.9234298775484,10.8874824636349));
#46581=CARTESIAN_POINT('Ctrl Pts',(54.4622894716872,30.9209167130579,10.8880853050008));
#46582=CARTESIAN_POINT('Ctrl Pts',(54.4573744419035,30.9195340934358,10.8884113306473));
#46583=CARTESIAN_POINT('Ctrl Pts',(54.44338098808,30.915539630377,10.8893375564395));
#46584=CARTESIAN_POINT('Ctrl Pts',(54.434315589454,30.9128821071736,10.8899351979694));
#46585=CARTESIAN_POINT('Ctrl Pts',(54.3735576568381,30.8946012034681,10.8939266984291));
#46586=CARTESIAN_POINT('Ctrl Pts',(54.322494071468,30.8769471445177,10.8972132540807));
#46587=CARTESIAN_POINT('Ctrl Pts',(54.1001235644696,30.7898070794933,10.9114780764638));
#46588=CARTESIAN_POINT('Ctrl Pts',(53.9382465763814,30.6987862041523,10.9218209064492));
#46589=CARTESIAN_POINT('Ctrl Pts',(53.751098866752,30.5562184408159,10.9359849281507));
#46590=CARTESIAN_POINT('Ctrl Pts',(53.7121657212748,30.5241561940714,10.9390668628493));
#46591=CARTESIAN_POINT('Ctrl Pts',(53.6637070203923,30.4810661323083,10.9431070734989));
#46592=CARTESIAN_POINT('Ctrl Pts',(53.6530275125162,30.4713602265913,10.9440108630092));
#46593=CARTESIAN_POINT('Ctrl Pts',(53.636137072563,30.4556716042274,10.9454624019386));
#46594=CARTESIAN_POINT('Ctrl Pts',(53.6298578667981,30.4497628893232,10.9460070213086));
#46595=CARTESIAN_POINT('Ctrl Pts',(53.6185956571647,30.439026662849,10.946993011114));
#46596=CARTESIAN_POINT('Ctrl Pts',(53.6135991311149,30.4342134860504,10.9474337618296));
#46597=CARTESIAN_POINT('Ctrl Pts',(53.6085281671203,30.4292773419323,10.9478845028505));
#46598=CARTESIAN_POINT('Ctrl Pts',(53.6084284778147,30.4291802827151,10.9478933652562));
#46599=CARTESIAN_POINT('Ctrl Pts',(53.6082328022992,30.4289897297946,10.9479107635255));
#46600=CARTESIAN_POINT('Ctrl Pts',(53.6081368154871,30.4288962369787,10.9479192993444));
#46601=CARTESIAN_POINT('Ctrl Pts',(53.6079483179992,30.4287126001484,10.9479360643327));
#46602=CARTESIAN_POINT('Ctrl Pts',(53.6078558066219,30.4286224567841,10.9479442934756));
#46603=CARTESIAN_POINT('Ctrl Pts',(53.607674050519,30.4284453186715,10.9479604634835));
#46604=CARTESIAN_POINT('Ctrl Pts',(53.6075848052084,30.4283583245622,10.9479684043198));
#46605=CARTESIAN_POINT('Ctrl Pts',(53.6007183386965,30.4216638086814,10.9485794501217));
#46606=CARTESIAN_POINT('Ctrl Pts',(53.5939883225987,30.4150082369068,10.9491846421686));
#46607=CARTESIAN_POINT('Ctrl Pts',(53.574324941759,30.3952835767955,10.9509716727746));
#46608=CARTESIAN_POINT('Ctrl Pts',(53.5615248933915,30.382083558152,10.9521592662796));
#46609=CARTESIAN_POINT('Ctrl Pts',(53.5326175947253,30.3514363484568,10.9548985449528));
#46610=CARTESIAN_POINT('Ctrl Pts',(53.5166359954398,30.3338749859522,10.9564552656265));
#46611=CARTESIAN_POINT('Ctrl Pts',(53.4645205901585,30.2745129239468,10.9616762091697));
#46612=CARTESIAN_POINT('Ctrl Pts',(53.4298126716526,30.2314995227753,10.96539414302));
#46613=CARTESIAN_POINT('Ctrl Pts',(53.3547992983306,30.1302016185715,10.9739958229886));
#46614=CARTESIAN_POINT('Ctrl Pts',(53.3157236029943,30.0710989654623,10.9789079403431));
#46615=CARTESIAN_POINT('Ctrl Pts',(53.2181185175537,29.9048761294885,10.9923366594161));
#46616=CARTESIAN_POINT('Ctrl Pts',(53.1661326736707,29.7942533014942,11.000876740139));
#46617=CARTESIAN_POINT('Ctrl Pts',(53.119202302704,29.6647377972203,11.0099993780796));
#46618=CARTESIAN_POINT('Ctrl Pts',(53.1140050060943,29.649845548715,11.0110355530373));
#46619=CARTESIAN_POINT('Ctrl Pts',(53.1069290566603,29.6287699732057,11.0124824830614));
#46620=CARTESIAN_POINT('Ctrl Pts',(53.1049031225325,29.6226372166187,11.0129012165313));
#46621=CARTESIAN_POINT('Ctrl Pts',(53.1015439296516,29.6123002224271,11.0136030041663));
#46622=CARTESIAN_POINT('Ctrl Pts',(53.1001947750544,29.6081012431901,11.0138869688013));
#46623=CARTESIAN_POINT('Ctrl Pts',(53.0974680764198,29.599517278291,11.0144651692206));
#46624=CARTESIAN_POINT('Ctrl Pts',(53.0960917445688,29.5951319543999,11.0147593343632));
#46625=CARTESIAN_POINT('Ctrl Pts',(53.0926198461209,29.5839343358586,11.015507443055));
#46626=CARTESIAN_POINT('Ctrl Pts',(53.0905455888152,29.5771154263083,11.0159601665655));
#46627=CARTESIAN_POINT('Ctrl Pts',(53.0822370125922,29.5492666030976,11.017798088019));
#46628=CARTESIAN_POINT('Ctrl Pts',(53.0763129438462,29.5281447535067,11.0191664835478));
#46629=CARTESIAN_POINT('Ctrl Pts',(53.0618155657209,29.4729708204912,11.0226850761764));
#46630=CARTESIAN_POINT('Ctrl Pts',(53.0537968846057,29.4388057818093,11.0248091069509));
#46631=CARTESIAN_POINT('Ctrl Pts',(53.0466869605703,29.4044696929237,11.0269053946991));
#46632=CARTESIAN_POINT('Origin',(55.,29.,3.45145488139523));
#46633=CARTESIAN_POINT('',(53.0466870113635,29.4044699382201,11.9837090255998));
#46634=CARTESIAN_POINT('',(53.0466869751866,29.4044697635106,11.8238528479472));
#46635=CARTESIAN_POINT('',(53.0466869980082,29.4044698737233,3.45145488139523));
#46636=CARTESIAN_POINT('',(53.0052503739419,28.9987785905819,11.2108651376668));
#46637=CARTESIAN_POINT('Ctrl Pts',(53.0466870113634,29.4044699382199,11.9837090255998));
#46638=CARTESIAN_POINT('Ctrl Pts',(53.0538097894638,29.4388680817256,11.9816662505898));
#46639=CARTESIAN_POINT('Ctrl Pts',(53.061844969036,29.4730963065561,11.9796169044452));
#46640=CARTESIAN_POINT('Ctrl Pts',(53.09498543007,29.5991713655257,11.9719638822383));
#46641=CARTESIAN_POINT('Ctrl Pts',(53.1257370561887,29.6893633633536,11.9662738775896));
#46642=CARTESIAN_POINT('Ctrl Pts',(53.1688157940404,29.7912206098217,11.9594075582874));
#46643=CARTESIAN_POINT('Ctrl Pts',(53.1749907810353,29.8053613968169,11.9584442761393));
#46644=CARTESIAN_POINT('Ctrl Pts',(53.1853364467838,29.8283229538182,11.9568629656974));
#46645=CARTESIAN_POINT('Ctrl Pts',(53.1894089606461,29.8371874401807,11.9562482680825));
#46646=CARTESIAN_POINT('Ctrl Pts',(53.1968144769038,29.8529999476218,11.955144024865));
#46647=CARTESIAN_POINT('Ctrl Pts',(53.2001230496378,29.8599592444974,11.9546553242181));
#46648=CARTESIAN_POINT('Ctrl Pts',(53.2072261186174,29.874679369694,11.9536157925928));
#46649=CARTESIAN_POINT('Ctrl Pts',(53.2110308638909,29.8824350490196,11.9530646153756));
#46650=CARTESIAN_POINT('Ctrl Pts',(53.2213592625894,29.9031473406664,11.951583177748));
#46651=CARTESIAN_POINT('Ctrl Pts',(53.2279739758153,29.9160577181682,11.950649770706));
#46652=CARTESIAN_POINT('Ctrl Pts',(53.2617914738048,29.9803244939344,11.9459520974273));
#46653=CARTESIAN_POINT('Ctrl Pts',(53.2910862348425,30.0305423812689,11.9421148823816));
#46654=CARTESIAN_POINT('Ctrl Pts',(53.3839858434895,30.1749147579098,11.9305729581624));
#46655=CARTESIAN_POINT('Ctrl Pts',(53.4534814039693,30.2649906761116,11.9226806801986));
#46656=CARTESIAN_POINT('Ctrl Pts',(53.5575751184224,30.3784306675668,11.9119501063205));
#46657=CARTESIAN_POINT('Ctrl Pts',(53.5857963253953,30.4073694310569,11.9091351249319));
#46658=CARTESIAN_POINT('Ctrl Pts',(53.6221757422883,30.4424738257972,11.9056366151245));
#46659=CARTESIAN_POINT('Ctrl Pts',(53.6295276653558,30.4494605917484,11.9049359775062));
#46660=CARTESIAN_POINT('Ctrl Pts',(53.6509347266875,30.4694959161019,11.9029148558657));
#46661=CARTESIAN_POINT('Ctrl Pts',(53.6651254282159,30.4823984858458,11.9015983446014));
#46662=CARTESIAN_POINT('Ctrl Pts',(53.7148983943834,30.5263590369731,11.8970660815459));
#46663=CARTESIAN_POINT('Ctrl Pts',(53.7513989316061,30.5563592810732,11.8938896479144));
#46664=CARTESIAN_POINT('Ctrl Pts',(53.7958037704429,30.5902873217469,11.8902269799941));
#46665=CARTESIAN_POINT('Ctrl Pts',(53.8027085526086,30.5954922505024,11.8896630115996));
#46666=CARTESIAN_POINT('Ctrl Pts',(53.8140156356351,30.6039009596227,11.8887487864025));
#46667=CARTESIAN_POINT('Ctrl Pts',(53.8183975077816,30.6071318405387,11.888396748283));
#46668=CARTESIAN_POINT('Ctrl Pts',(53.8262676947547,30.6128851688339,11.8877685668948));
#46669=CARTESIAN_POINT('Ctrl Pts',(53.829750986991,30.6154142938848,11.8874919726828));
#46670=CARTESIAN_POINT('Ctrl Pts',(53.8373704220097,30.6209089818593,11.8868900745541));
#46671=CARTESIAN_POINT('Ctrl Pts',(53.8415097304841,30.6238699947694,11.886565079314));
#46672=CARTESIAN_POINT('Ctrl Pts',(53.8533018009081,30.63223729691,11.8856447294673));
#46673=CARTESIAN_POINT('Ctrl Pts',(53.8609815053392,30.6376056393879,11.8850518826844));
#46674=CARTESIAN_POINT('Ctrl Pts',(53.9117166687611,30.672541456117,11.8811760558672));
#46675=CARTESIAN_POINT('Ctrl Pts',(53.9558854363231,30.7004650390624,11.8779933688827));
#46676=CARTESIAN_POINT('Ctrl Pts',(54.1445262919131,30.8095985842591,11.8649588488438));
#46677=CARTESIAN_POINT('Ctrl Pts',(54.2977321777928,30.8743822915618,11.8556353385642));
#46678=CARTESIAN_POINT('Ctrl Pts',(54.5232934893647,30.9381684704359,11.8416916431834));
#46679=CARTESIAN_POINT('Ctrl Pts',(54.5903082454484,30.9534321814295,11.8375318522071));
#46680=CARTESIAN_POINT('Ctrl Pts',(54.6734479399201,30.9679019476223,11.8322842268581));
#46681=CARTESIAN_POINT('Ctrl Pts',(54.6889548439021,30.9704124472356,11.8313019109951));
#46682=CARTESIAN_POINT('Ctrl Pts',(54.7133853949728,30.9740720717457,11.8297480557055));
#46683=CARTESIAN_POINT('Ctrl Pts',(54.7222901401247,30.9753444524265,11.8291803874578));
#46684=CARTESIAN_POINT('Ctrl Pts',(54.7387313690129,30.977580336771,11.828129751617));
#46685=CARTESIAN_POINT('Ctrl Pts',(54.7462653684731,30.9785610983962,11.8276473347592));
#46686=CARTESIAN_POINT('Ctrl Pts',(54.7629685407394,30.9806385143998,11.8265755560198));
#46687=CARTESIAN_POINT('Ctrl Pts',(54.7721400530382,30.9817145801723,11.8259855610913));
#46688=CARTESIAN_POINT('Ctrl Pts',(54.7984837710797,30.9846201147672,11.8242864432542));
#46689=CARTESIAN_POINT('Ctrl Pts',(54.8156723594207,30.9862902810139,11.8231723867311));
#46690=CARTESIAN_POINT('Ctrl Pts',(54.9585046570007,30.9982989767491,11.8138675277587));
#46691=CARTESIAN_POINT('Ctrl Pts',(55.0848245668128,30.9969263900102,11.8053069640964));
#46692=CARTESIAN_POINT('Ctrl Pts',(55.3452942197386,30.9693319960172,11.7871381271022));
#46693=CARTESIAN_POINT('Ctrl Pts',(55.4786256416514,30.9412411329144,11.7775475019371));
#46694=CARTESIAN_POINT('Ctrl Pts',(55.6320341887414,30.8921399300865,11.7667580337657));
#46695=CARTESIAN_POINT('Ctrl Pts',(55.6558534778024,30.8840162119009,11.7650910430821));
#46696=CARTESIAN_POINT('Ctrl Pts',(55.6868304025286,30.8727925989438,11.7629396610332));
#46697=CARTESIAN_POINT('Ctrl Pts',(55.6941314372249,30.8700988404741,11.7624338134846));
#46698=CARTESIAN_POINT('Ctrl Pts',(55.7058548877583,30.8656952904802,11.7616237373361));
#46699=CARTESIAN_POINT('Ctrl Pts',(55.7102872107107,30.8640123709163,11.761317972123));
#46700=CARTESIAN_POINT('Ctrl Pts',(55.7188041916714,30.860743747667,11.7607314524022));
#46701=CARTESIAN_POINT('Ctrl Pts',(55.7228896508877,30.8591603786117,11.7604505716039));
#46702=CARTESIAN_POINT('Ctrl Pts',(55.7326159392391,30.8553539307358,11.7597829188126));
#46703=CARTESIAN_POINT('Ctrl Pts',(55.738251968181,30.8531185489593,11.7593968739072));
#46704=CARTESIAN_POINT('Ctrl Pts',(55.7573013836866,30.8454624016728,11.7580946172874));
#46705=CARTESIAN_POINT('Ctrl Pts',(55.7706663294563,30.839921275164,11.7571852581777));
#46706=CARTESIAN_POINT('Ctrl Pts',(55.8472771708882,30.8071770414912,11.7519909041624));
#46707=CARTESIAN_POINT('Ctrl Pts',(55.9091477563348,30.7768567233536,11.7478675446533));
#46708=CARTESIAN_POINT('Ctrl Pts',(56.1428155803405,30.6469367531515,11.7321182818738));
#46709=CARTESIAN_POINT('Ctrl Pts',(56.3009187131702,30.5251358285314,11.7209488020052));
#46710=CARTESIAN_POINT('Ctrl Pts',(56.4544611727968,30.3653222830452,11.7072813000356));
#46711=CARTESIAN_POINT('Ctrl Pts',(56.470189554697,30.3483711819584,11.7058437532572));
#46712=CARTESIAN_POINT('Ctrl Pts',(56.4924671750096,30.3235084425439,11.7037503031641));
#46713=CARTESIAN_POINT('Ctrl Pts',(56.4992559379192,30.3158132437027,11.7031043907966));
#46714=CARTESIAN_POINT('Ctrl Pts',(56.5110990150491,30.3021782329434,11.7019632571737));
#46715=CARTESIAN_POINT('Ctrl Pts',(56.5161784730587,30.2962604748537,11.7014690835676));
#46716=CARTESIAN_POINT('Ctrl Pts',(56.5265979565976,30.2839763572886,11.7004454322746));
#46717=CARTESIAN_POINT('Ctrl Pts',(56.5319331579411,30.2776061221461,11.6999157721246));
#46718=CARTESIAN_POINT('Ctrl Pts',(56.5455165401668,30.2611801358291,11.6985529110487));
#46719=CARTESIAN_POINT('Ctrl Pts',(56.5537063569369,30.251076837829,11.6977173914426));
#46720=CARTESIAN_POINT('Ctrl Pts',(56.5878062896415,30.2081584707105,11.6941790443864));
#46721=CARTESIAN_POINT('Ctrl Pts',(56.612778533835,30.1746151168608,11.691439826361));
#46722=CARTESIAN_POINT('Ctrl Pts',(56.6766227509312,30.0829803829853,11.684019867879));
#46723=CARTESIAN_POINT('Ctrl Pts',(56.7135244987207,30.0235929263517,11.6792739305129));
#46724=CARTESIAN_POINT('Ctrl Pts',(56.8059840648276,29.8557325788596,11.6660710123327));
#46725=CARTESIAN_POINT('Ctrl Pts',(56.8548432237346,29.7439167276699,11.6574899931631));
#46726=CARTESIAN_POINT('Ctrl Pts',(56.8972043280262,29.6162830842908,11.648255654697));
#46727=CARTESIAN_POINT('Ctrl Pts',(56.9010926088437,29.6041820964544,11.6473857163542));
#46728=CARTESIAN_POINT('Ctrl Pts',(56.9184008720312,29.5484938820193,11.6434100451176));
#46729=CARTESIAN_POINT('Ctrl Pts',(56.9304404092784,29.5044878526238,11.6403457743088));
#46730=CARTESIAN_POINT('Ctrl Pts',(56.9429364623159,29.4517729252662,11.6367956308598));
#46731=CARTESIAN_POINT('Ctrl Pts',(56.9448577638329,29.4434288638555,11.6362372452116));
#46732=CARTESIAN_POINT('Ctrl Pts',(56.9479071435624,29.4297844608363,11.6353302405198));
#46733=CARTESIAN_POINT('Ctrl Pts',(56.9490674329746,29.4244915383214,11.6349798853519));
#46734=CARTESIAN_POINT('Ctrl Pts',(56.951110448509,29.4149868635746,11.6343534909203));
#46735=CARTESIAN_POINT('Ctrl Pts',(56.9520011235146,29.4107769395934,11.6340770119628));
#46736=CARTESIAN_POINT('Ctrl Pts',(56.9539196163733,29.4015617052602,11.6334739464279));
#46737=CARTESIAN_POINT('Ctrl Pts',(56.9549418270598,29.3965553234961,11.6331476777984));
#46738=CARTESIAN_POINT('Ctrl Pts',(56.9578026098338,29.3822644165273,11.6322200652341));
#46739=CARTESIAN_POINT('Ctrl Pts',(56.9595943841911,29.3729705095743,11.6316212919688));
#46740=CARTESIAN_POINT('Ctrl Pts',(56.9712436677294,29.3101433574549,11.6276016649165));
#46741=CARTESIAN_POINT('Ctrl Pts',(56.9789734774285,29.2562335592232,11.6242898566734));
#46742=CARTESIAN_POINT('Ctrl Pts',(57.0037781264875,29.0126322177332,11.609669940758));
#46743=CARTESIAN_POINT('Ctrl Pts',(56.995845593778,28.8214082726878,11.5990294180597));
#46744=CARTESIAN_POINT('Ctrl Pts',(56.9525953196037,28.5895599521107,11.584776824973));
#46745=CARTESIAN_POINT('Ctrl Pts',(56.9427469146776,28.5452215248382,11.5819937612321));
#46746=CARTESIAN_POINT('Ctrl Pts',(56.9279192842535,28.4878007913889,11.578296086202));
#46747=CARTESIAN_POINT('Ctrl Pts',(56.9243031840296,28.4743784284856,11.5774250121243));
#46748=CARTESIAN_POINT('Ctrl Pts',(56.9182488684211,28.4528060805927,11.5760136872611));
#46749=CARTESIAN_POINT('Ctrl Pts',(56.9158982487471,28.4446318306983,11.5754762636879));
#46750=CARTESIAN_POINT('Ctrl Pts',(56.9113105863261,28.4290541021622,11.5744469307145));
#46751=CARTESIAN_POINT('Ctrl Pts',(56.9090826192967,28.4216480953487,11.5739553233128));
#46752=CARTESIAN_POINT('Ctrl Pts',(56.9038763566283,28.4046998196502,11.5728250746603));
#46753=CARTESIAN_POINT('Ctrl Pts',(56.900869306746,28.3951666686216,11.5721855083454));
#46754=CARTESIAN_POINT('Ctrl Pts',(56.8912996301227,28.3656046258594,11.5701901133847));
#46755=CARTESIAN_POINT('Ctrl Pts',(56.884491304176,28.3456573910055,11.5688263144881));
#46756=CARTESIAN_POINT('Ctrl Pts',(56.8498311674311,28.2491400272354,11.5621400556822));
#46757=CARTESIAN_POINT('Ctrl Pts',(56.8176251675408,28.1742265167114,11.5566760275323));
#46758=CARTESIAN_POINT('Ctrl Pts',(56.7187263105764,27.9781974219045,11.5416490434608));
#46759=CARTESIAN_POINT('Ctrl Pts',(56.6438879186226,27.8616988453802,11.5318954278903));
#46760=CARTESIAN_POINT('Ctrl Pts',(56.5494951613292,27.7437112196883,11.5215201700771));
#46761=CARTESIAN_POINT('Ctrl Pts',(56.5412700791149,27.7336338170292,11.520629962992));
#46762=CARTESIAN_POINT('Ctrl Pts',(56.5039730460282,27.688839045318,11.5166570048513));
#46763=CARTESIAN_POINT('Ctrl Pts',(56.4738201013662,27.6550342048124,11.5136151319945));
#46764=CARTESIAN_POINT('Ctrl Pts',(56.4366384099086,27.6161030907107,11.5100875089959));
#46765=CARTESIAN_POINT('Ctrl Pts',(56.4306969766072,27.6099616035171,11.5095302686884));
#46766=CARTESIAN_POINT('Ctrl Pts',(56.4209273631805,27.5999920377761,11.5086247460369));
#46767=CARTESIAN_POINT('Ctrl Pts',(56.4171228123291,27.5961411031845,11.5082747367804));
#46768=CARTESIAN_POINT('Ctrl Pts',(56.4102660808543,27.5892570546196,11.5076487081754));
#46769=CARTESIAN_POINT('Ctrl Pts',(56.407219732517,27.5862182975295,11.5073722514483));
#46770=CARTESIAN_POINT('Ctrl Pts',(56.4005312713572,27.5795895410592,11.5067689393829));
#46771=CARTESIAN_POINT('Ctrl Pts',(56.3968851829895,27.5760036864981,11.5064424039287));
#46772=CARTESIAN_POINT('Ctrl Pts',(56.3864374739455,27.5658073169048,11.5055132668322));
#46773=CARTESIAN_POINT('Ctrl Pts',(56.379602331889,27.5592311303847,11.5049132491439));
#46774=CARTESIAN_POINT('Ctrl Pts',(56.3328778016414,27.5149142069323,11.5008623015948));
#46775=CARTESIAN_POINT('Ctrl Pts',(56.2914876971954,27.4787821444609,11.4975223748204));
#46776=CARTESIAN_POINT('Ctrl Pts',(56.0947852974662,27.3208921594911,11.4824678473761));
#46777=CARTESIAN_POINT('Ctrl Pts',(55.9234448269947,27.220894492859,11.4714608277996));
#46778=CARTESIAN_POINT('Ctrl Pts',(55.7035812332166,27.133035519094,11.4570844675676));
#46779=CARTESIAN_POINT('Ctrl Pts',(55.6665350575063,27.1194911271889,11.4546592651777));
#46780=CARTESIAN_POINT('Ctrl Pts',(55.6165902578969,27.102892155519,11.4513743377371));
#46781=CARTESIAN_POINT('Ctrl Pts',(55.6040261598805,27.0988545282641,11.4505467352006));
#46782=CARTESIAN_POINT('Ctrl Pts',(55.583447633618,27.0924659476589,11.4491887867839));
#46783=CARTESIAN_POINT('Ctrl Pts',(55.5754567397167,27.0900400948422,11.4486608849259));
#46784=CARTESIAN_POINT('Ctrl Pts',(55.5599903610336,27.0854507268678,11.4476378810787));
#46785=CARTESIAN_POINT('Ctrl Pts',(55.5525169732418,27.0832806373436,11.4471430027919));
#46786=CARTESIAN_POINT('Ctrl Pts',(55.5350880668318,27.0783301103488,11.4459874895153));
#46787=CARTESIAN_POINT('Ctrl Pts',(55.5251233255616,27.0755832337051,11.4453257859688));
#46788=CARTESIAN_POINT('Ctrl Pts',(55.4930009525672,27.0669964609852,11.4431890826612));
#46789=CARTESIAN_POINT('Ctrl Pts',(55.4707645475696,27.0614610425126,11.4417044058973));
#46790=CARTESIAN_POINT('Ctrl Pts',(55.3549361880035,27.0347376999368,11.4339390822388));
#46791=CARTESIAN_POINT('Ctrl Pts',(55.2600126176054,27.0199433374644,11.427459521726));
#46792=CARTESIAN_POINT('Ctrl Pts',(55.0488567160701,27.0024807283037,11.4128570621028));
#46793=CARTESIAN_POINT('Ctrl Pts',(54.9327002420843,27.0030173186758,11.4046961807989));
#46794=CARTESIAN_POINT('Ctrl Pts',(54.8040248069984,27.014855753693,11.3958023955393));
#46795=CARTESIAN_POINT('Ctrl Pts',(54.7908116447361,27.0162045976485,11.3948910869031));
#46796=CARTESIAN_POINT('Ctrl Pts',(54.728436001254,27.0232022500196,11.3906009278552));
#46797=CARTESIAN_POINT('Ctrl Pts',(54.6794768891601,27.0305477455254,11.3872681312033));
#46798=CARTESIAN_POINT('Ctrl Pts',(54.6222310056602,27.0413282946609,11.3834492880775));
#46799=CARTESIAN_POINT('Ctrl Pts',(54.6136350219797,27.0430057811014,11.3828779550546));
#46800=CARTESIAN_POINT('Ctrl Pts',(54.5996808671677,27.0458244295359,11.3819542134975));
#46801=CARTESIAN_POINT('Ctrl Pts',(54.5943159666013,27.0469311238259,11.3815999632858));
#46802=CARTESIAN_POINT('Ctrl Pts',(54.5847411719375,27.0489474078351,11.3809694158557));
#46803=CARTESIAN_POINT('Ctrl Pts',(54.5805296097572,27.0498485431788,11.3806926529407));
#46804=CARTESIAN_POINT('Ctrl Pts',(54.5713728979939,27.0518388133912,11.3800922115206));
#46805=CARTESIAN_POINT('Ctrl Pts',(54.566428971824,27.0529331376466,11.3797688298633));
#46806=CARTESIAN_POINT('Ctrl Pts',(54.552465748608,27.0560796791825,11.3788576532064));
#46807=CARTESIAN_POINT('Ctrl Pts',(54.5434563430241,27.058175853239,11.3782722876881));
#46808=CARTESIAN_POINT('Ctrl Pts',(54.4861988745874,27.071918197102,11.3745664627704));
#46809=CARTESIAN_POINT('Ctrl Pts',(54.4383807057545,27.0853000993161,11.371536445795));
#46810=CARTESIAN_POINT('Ctrl Pts',(54.2538069756808,27.1444645128716,11.3599196234041));
#46811=CARTESIAN_POINT('Ctrl Pts',(54.1216758668048,27.2032339470628,11.3517473629666));
#46812=CARTESIAN_POINT('Ctrl Pts',(53.9184069212259,27.3214718333907,11.3379180168667));
#46813=CARTESIAN_POINT('Ctrl Pts',(53.8430145038438,27.3725228420936,11.3324697879212));
#46814=CARTESIAN_POINT('Ctrl Pts',(53.759280764476,27.4379888114136,11.3258699931241));
#46815=CARTESIAN_POINT('Ctrl Pts',(53.7472980900504,27.4475821828451,11.3249116515866));
#46816=CARTESIAN_POINT('Ctrl Pts',(53.7279019400991,27.4634816046326,11.3233368335462));
#46817=CARTESIAN_POINT('Ctrl Pts',(53.72042165207,27.4697054206964,11.3227236413917));
#46818=CARTESIAN_POINT('Ctrl Pts',(53.7071019055503,27.4809537794479,11.3216210558356));
#46819=CARTESIAN_POINT('Ctrl Pts',(53.7012454126589,27.4859579193552,11.32113249723));
#46820=CARTESIAN_POINT('Ctrl Pts',(53.6891281575991,27.496433669793,11.3201136985883));
#46821=CARTESIAN_POINT('Ctrl Pts',(53.6828723379975,27.501910745286,11.3195832391479));
#46822=CARTESIAN_POINT('Ctrl Pts',(53.6663449730392,27.5165642779621,11.3181697250393));
#46823=CARTESIAN_POINT('Ctrl Pts',(53.6561340625161,27.5258081540246,11.3172838759529));
#46824=CARTESIAN_POINT('Ctrl Pts',(53.633856039885,27.5464001191484,11.3153228820191));
#46825=CARTESIAN_POINT('Ctrl Pts',(53.6218330016006,27.5577941788005,11.3142458320497));
#46826=CARTESIAN_POINT('Ctrl Pts',(53.5862915794664,27.5923265642092,11.3110046863194));
#46827=CARTESIAN_POINT('Ctrl Pts',(53.5632048138538,27.6158990693339,11.3088223648409));
#46828=CARTESIAN_POINT('Ctrl Pts',(53.4782440662304,27.7070644653922,11.3004923645913));
#46829=CARTESIAN_POINT('Ctrl Pts',(53.4204734174192,27.778314324193,11.2941948282522));
#46830=CARTESIAN_POINT('Ctrl Pts',(53.2872586678309,27.9679254346141,11.2780882970514));
#46831=CARTESIAN_POINT('Ctrl Pts',(53.219007671074,28.0907515932836,11.2682127299869));
#46832=CARTESIAN_POINT('Ctrl Pts',(53.1583928870555,28.233364184433,11.2579642444861));
#46833=CARTESIAN_POINT('Ctrl Pts',(53.1527473294175,28.2470691704283,11.2569914392865));
#46834=CARTESIAN_POINT('Ctrl Pts',(53.1451478451073,28.2661175994676,11.255657211214));
#46835=CARTESIAN_POINT('Ctrl Pts',(53.143063392378,28.2714079800785,11.255288543607));
#46836=CARTESIAN_POINT('Ctrl Pts',(53.1395232481445,28.280506817126,11.2546578098463));
#46837=CARTESIAN_POINT('Ctrl Pts',(53.1380565726748,28.2843109204666,11.2543951042004));
#46838=CARTESIAN_POINT('Ctrl Pts',(53.1350190227311,28.2922619264598,11.2538481361846));
#46839=CARTESIAN_POINT('Ctrl Pts',(53.1334503014349,28.2964096010042,11.2535640108065));
#46840=CARTESIAN_POINT('Ctrl Pts',(53.1296671302251,28.3065139484548,11.2528746865588));
#46841=CARTESIAN_POINT('Ctrl Pts',(53.1274672647498,28.312476105509,11.2524703438871));
#46842=CARTESIAN_POINT('Ctrl Pts',(53.119734640586,28.3337457938983,11.2510360570699));
#46843=CARTESIAN_POINT('Ctrl Pts',(53.1143606139754,28.3491108890693,11.2500149862326));
#46844=CARTESIAN_POINT('Ctrl Pts',(53.1015199791031,28.3873185120338,11.2475090360808));
#46845=CARTESIAN_POINT('Ctrl Pts',(53.0942767583475,28.4102339221479,11.2460350666133));
#46846=CARTESIAN_POINT('Ctrl Pts',(53.065700507284,28.5066715184883,11.2399310645363));
#46847=CARTESIAN_POINT('Ctrl Pts',(53.0481931860629,28.5812644162781,11.2354470003281));
#46848=CARTESIAN_POINT('Ctrl Pts',(53.0152780457432,28.7696556976421,11.2243161395955));
#46849=CARTESIAN_POINT('Ctrl Pts',(53.0053205872547,28.8841094408609,11.2177155023488));
#46850=CARTESIAN_POINT('Ctrl Pts',(53.0052503739419,28.9987785905819,11.2108651376668));
#46851=CARTESIAN_POINT('Ctrl Pts',(53.0052503724545,28.9987810220628,11.2108649924095));
#46852=CARTESIAN_POINT('Ctrl Pts',(53.0052251363528,29.0400776714371,11.2083979187618));
#46853=CARTESIAN_POINT('Ctrl Pts',(53.0064823250465,29.0813635842419,11.2059024965257));
#46854=CARTESIAN_POINT('Ctrl Pts',(53.0105224873157,29.1469853474418,11.201870489345));
#46855=CARTESIAN_POINT('Ctrl Pts',(53.012473669472,29.171360649133,11.2003583762426));
#46856=CARTESIAN_POINT('Ctrl Pts',(53.0158391803227,29.2055006727038,11.1982175515189));
#46857=CARTESIAN_POINT('Ctrl Pts',(53.0168786565615,29.2153007583507,11.1976003577433));
#46858=CARTESIAN_POINT('Ctrl Pts',(53.0188444825034,29.2326104578244,11.1965053329133));
#46859=CARTESIAN_POINT('Ctrl Pts',(53.0197410262588,29.2401233099652,11.1960284332538));
#46860=CARTESIAN_POINT('Ctrl Pts',(53.0215964810996,29.2549540111086,11.195083704607));
#46861=CARTESIAN_POINT('Ctrl Pts',(53.0225533064496,29.2622720022626,11.194615947827));
#46862=CARTESIAN_POINT('Ctrl Pts',(53.0245401617277,29.2768385653728,11.1936816227368));
#46863=CARTESIAN_POINT('Ctrl Pts',(53.0255695316201,29.2840871118157,11.1932150819902));
#46864=CARTESIAN_POINT('Ctrl Pts',(53.0284194031172,29.3033910996125,11.1919682465461));
#46865=CARTESIAN_POINT('Ctrl Pts',(53.0303105441874,29.3154356449729,11.1911857467973));
#46866=CARTESIAN_POINT('Ctrl Pts',(53.0365993420809,29.3532244479218,11.1887160336788));
#46867=CARTESIAN_POINT('Ctrl Pts',(53.0413920055579,29.3788986797824,11.1870165602275));
#46868=CARTESIAN_POINT('Ctrl Pts',(53.0466869981205,29.4044698742655,11.1853016190124));
#46869=CARTESIAN_POINT('',(53.0052506385882,29.0015961351009,11.0506343150513));
#46870=CARTESIAN_POINT('Ctrl Pts',(53.0466869605703,29.4044696929237,11.0269053946991));
#46871=CARTESIAN_POINT('Ctrl Pts',(53.0192628668241,29.2720300049911,11.0349911058038));
#46872=CARTESIAN_POINT('Ctrl Pts',(53.0053590218994,29.1370467887781,11.0426855070452));
#46873=CARTESIAN_POINT('Ctrl Pts',(53.0052506385882,29.0015961350858,11.0506343150522));
#46874=CARTESIAN_POINT('Ctrl Pts',(53.0052506370171,29.0015941704433,11.0506344303456));
#46875=CARTESIAN_POINT('Ctrl Pts',(53.0051767730351,28.9091698430059,11.056058275815));
#46876=CARTESIAN_POINT('Ctrl Pts',(53.0115263315731,28.8168599802161,11.06157678144));
#46877=CARTESIAN_POINT('Ctrl Pts',(53.0261316534095,28.7118025760173,11.0681441965659));
#46878=CARTESIAN_POINT('Ctrl Pts',(53.0281506133318,28.6982981820567,11.0689937331365));
#46879=CARTESIAN_POINT('Ctrl Pts',(53.0317395704682,28.6758695805716,11.070414087241));
#46880=CARTESIAN_POINT('Ctrl Pts',(53.0332320371722,28.6669333049153,11.0709824962544));
#46881=CARTESIAN_POINT('Ctrl Pts',(53.0360411853563,28.6507909005072,11.072013923958));
#46882=CARTESIAN_POINT('Ctrl Pts',(53.0373367891327,28.6435812305822,11.0724762756496));
#46883=CARTESIAN_POINT('Ctrl Pts',(53.040057152452,28.6289079205794,11.073420780494));
#46884=CARTESIAN_POINT('Ctrl Pts',(53.0414849043694,28.6214449648288,11.0739030208879));
#46885=CARTESIAN_POINT('Ctrl Pts',(53.044692251646,28.6051839115285,11.0749579151741));
#46886=CARTESIAN_POINT('Ctrl Pts',(53.0464886581377,28.5963893368791,11.0755310923333));
#46887=CARTESIAN_POINT('Ctrl Pts',(53.0515746267285,28.5723199014462,11.0771072172899));
#46888=CARTESIAN_POINT('Ctrl Pts',(53.0549843462386,28.5570713538066,11.0781139543558));
#46889=CARTESIAN_POINT('Ctrl Pts',(53.074062017748,28.4762264202601,11.083496500005));
#46890=CARTESIAN_POINT('Ctrl Pts',(53.0928683404346,28.411422938835,11.0879714208204));
#46891=CARTESIAN_POINT('Ctrl Pts',(53.1330197167672,28.2953891285185,11.0962808707681));
#46892=CARTESIAN_POINT('Ctrl Pts',(53.1532902066643,28.2438557597506,11.1000825100931));
#46893=CARTESIAN_POINT('Ctrl Pts',(53.2200644579192,28.0928603256301,11.1115177851662));
#46894=CARTESIAN_POINT('Ctrl Pts',(53.2726604718383,27.9963211116007,11.1192364239334));
#46895=CARTESIAN_POINT('Ctrl Pts',(53.3625609857995,27.8595033831485,11.1304516136219));
#46896=CARTESIAN_POINT('Ctrl Pts',(53.3940123305174,27.8156251438108,11.1340928339998));
#46897=CARTESIAN_POINT('Ctrl Pts',(53.4330166166528,27.7656257287041,11.138247880553));
#46898=CARTESIAN_POINT('Ctrl Pts',(53.4388788154513,27.7582200593934,11.1388634488277));
#46899=CARTESIAN_POINT('Ctrl Pts',(53.447990559914,27.7468757744544,11.1398062595493));
#46900=CARTESIAN_POINT('Ctrl Pts',(53.4512029024119,27.7429076491068,11.1401360191826));
#46901=CARTESIAN_POINT('Ctrl Pts',(53.4571510481737,27.7356174653597,11.1407417302603));
#46902=CARTESIAN_POINT('Ctrl Pts',(53.4598823552929,27.7322919408812,11.1410179809589));
#46903=CARTESIAN_POINT('Ctrl Pts',(53.4660804561657,27.7247949916834,11.1416406525282));
#46904=CARTESIAN_POINT('Ctrl Pts',(53.4695535089778,27.7206288576123,11.1419866168159));
#46905=CARTESIAN_POINT('Ctrl Pts',(53.4798850920328,27.7083377838782,11.1430072895517));
#46906=CARTESIAN_POINT('Ctrl Pts',(53.4867917667126,27.7002533060767,11.1436786349842));
#46907=CARTESIAN_POINT('Ctrl Pts',(53.5579917743521,27.6182483527136,11.1504930088693));
#46908=CARTESIAN_POINT('Ctrl Pts',(53.6275925076459,27.5490939764906,11.1562810465238));
#46909=CARTESIAN_POINT('Ctrl Pts',(53.7905273469978,27.4094671138518,11.1688027241763));
#46910=CARTESIAN_POINT('Ctrl Pts',(53.8855282881106,27.3415154380705,11.1754916727222));
#46911=CARTESIAN_POINT('Ctrl Pts',(54.0260812719248,27.2585393833329,11.1851957646198));
#46912=CARTESIAN_POINT('Ctrl Pts',(54.0670607519601,27.2362464219997,11.1880021767607));
#46913=CARTESIAN_POINT('Ctrl Pts',(54.1276809976627,27.205972860229,11.1921478067746));
#46914=CARTESIAN_POINT('Ctrl Pts',(54.1467283362051,27.1968357707435,11.1934495042572));
#46915=CARTESIAN_POINT('Ctrl Pts',(54.1811849419512,27.1809749923955,11.1958050348111));
#46916=CARTESIAN_POINT('Ctrl Pts',(54.1965410531613,27.174140265133,11.1968550746472));
#46917=CARTESIAN_POINT('Ctrl Pts',(54.220336124091,27.1639078145889,11.1984834000007));
#46918=CARTESIAN_POINT('Ctrl Pts',(54.2287152625281,27.1603722870987,11.1990570261803));
#46919=CARTESIAN_POINT('Ctrl Pts',(54.2371954977776,27.1568622241155,11.1996378800133));
#46920=CARTESIAN_POINT('Ctrl Pts',(54.2372728223297,27.1568302243292,11.1996431763852));
#46921=CARTESIAN_POINT('Ctrl Pts',(54.237428968657,27.1567656166584,11.1996538717335));
#46922=CARTESIAN_POINT('Ctrl Pts',(54.2375077905893,27.1567330089311,11.1996592707218));
#46923=CARTESIAN_POINT('Ctrl Pts',(54.2376669701355,27.1566671701401,11.1996701739403));
#46924=CARTESIAN_POINT('Ctrl Pts',(54.2377473279252,27.156633939236,11.1996756781836));
#46925=CARTESIAN_POINT('Ctrl Pts',(54.2379096189275,27.1565668383592,11.1996867946377));
#46926=CARTESIAN_POINT('Ctrl Pts',(54.2379915522124,27.1565329685995,11.1996924068545));
#46927=CARTESIAN_POINT('Ctrl Pts',(54.2381570354275,27.1564645737052,11.1997037420826));
#46928=CARTESIAN_POINT('Ctrl Pts',(54.2382405852373,27.1564300488745,11.1997094650868));
#46929=CARTESIAN_POINT('Ctrl Pts',(54.2383784502063,27.1563730906598,11.1997189086266));
#46930=CARTESIAN_POINT('Ctrl Pts',(54.2384327641477,27.1563506539394,11.1997226290615));
#46931=CARTESIAN_POINT('Ctrl Pts',(54.2385464369865,27.1563037023418,11.1997304155308));
#46932=CARTESIAN_POINT('Ctrl Pts',(54.2386057961258,27.1562791879107,11.1997344815843));
#46933=CARTESIAN_POINT('Ctrl Pts',(54.2387300408201,27.1562278837454,11.1997429922784));
#46934=CARTESIAN_POINT('Ctrl Pts',(54.2387949264862,27.1562010946189,11.1997474369296));
#46935=CARTESIAN_POINT('Ctrl Pts',(54.2389307532673,27.156145024665,11.1997567410669));
#46936=CARTESIAN_POINT('Ctrl Pts',(54.239001694661,27.1561157445053,11.1997616005757));
#46937=CARTESIAN_POINT('Ctrl Pts',(54.2391502150572,27.1560544546284,11.1997717743174));
#46938=CARTESIAN_POINT('Ctrl Pts',(54.2392277944371,27.1560224456935,11.1997770885805));
#46939=CARTESIAN_POINT('Ctrl Pts',(54.2393902319972,27.1559554366164,11.1997882157666));
#46940=CARTESIAN_POINT('Ctrl Pts',(54.2394750905147,27.1559204374598,11.1997940287178));
#46941=CARTESIAN_POINT('Ctrl Pts',(54.2396527919452,27.1558471604044,11.1998062016306));
#46942=CARTESIAN_POINT('Ctrl Pts',(54.2397456354921,27.1558088835938,11.1998125616418));
#46943=CARTESIAN_POINT('Ctrl Pts',(54.2399400852995,27.1557287345289,11.1998258820107));
#46944=CARTESIAN_POINT('Ctrl Pts',(54.2400416920212,27.1556868637048,11.1998328424074));
#46945=CARTESIAN_POINT('Ctrl Pts',(54.2402545256621,27.1555991782713,11.199847422311));
#46946=CARTESIAN_POINT('Ctrl Pts',(54.2403657532592,27.1555533653291,11.1998550418734));
#46947=CARTESIAN_POINT('Ctrl Pts',(54.2405987740959,27.1554574122718,11.1998710049035));
#46948=CARTESIAN_POINT('Ctrl Pts',(54.2407205682898,27.1554072741037,11.1998793484474));
#46949=CARTESIAN_POINT('Ctrl Pts',(54.2409757658472,27.1553022482591,11.1998968309617));
#46950=CARTESIAN_POINT('Ctrl Pts',(54.2411091700964,27.1552473630328,11.1999059700057));
#46951=CARTESIAN_POINT('Ctrl Pts',(54.2413887383561,27.1551323784122,11.1999251223841));
#46952=CARTESIAN_POINT('Ctrl Pts',(54.2415349035882,27.1550722819034,11.1999351358179));
#46953=CARTESIAN_POINT('Ctrl Pts',(54.2418412649093,27.1549463625951,11.1999561241052));
#46954=CARTESIAN_POINT('Ctrl Pts',(54.2420014623424,27.1548805433249,11.19996709907));
#46955=CARTESIAN_POINT('Ctrl Pts',(54.2422949223019,27.154760016019,11.1999872039255));
#46956=CARTESIAN_POINT('Ctrl Pts',(54.242428186415,27.154705299819,11.1999963338896));
#46957=CARTESIAN_POINT('Ctrl Pts',(54.2427699477376,27.1545650211291,11.2000197482638));
#46958=CARTESIAN_POINT('Ctrl Pts',(54.2429784488883,27.1544794814349,11.2000340330585));
#46959=CARTESIAN_POINT('Ctrl Pts',(54.2435129074148,27.1542603202635,11.2000706502894));
#46960=CARTESIAN_POINT('Ctrl Pts',(54.2438388826662,27.1541267510385,11.2000929842324));
#46961=CARTESIAN_POINT('Ctrl Pts',(54.2513582620289,27.1510479914536,11.2006081797998));
#46962=CARTESIAN_POINT('Ctrl Pts',(54.2585687020462,27.1481448195484,11.2011024427319));
#46963=CARTESIAN_POINT('Ctrl Pts',(54.2751881568124,27.1415658758767,11.2022423040393));
#46964=CARTESIAN_POINT('Ctrl Pts',(54.2846084311702,27.1379193092652,11.2028888625588));
#46965=CARTESIAN_POINT('Ctrl Pts',(54.3148458457613,27.126477794034,11.2049659008887));
#46966=CARTESIAN_POINT('Ctrl Pts',(54.3357651494386,27.1189594186327,11.2064054551363));
#46967=CARTESIAN_POINT('Ctrl Pts',(54.5213715369854,27.0557348590577,11.2192052769545));
#46968=CARTESIAN_POINT('Ctrl Pts',(54.6925313301588,27.0214422622765,11.2312956838045));
#46969=CARTESIAN_POINT('Ctrl Pts',(54.9657041672717,27.0030389612919,11.2503567917627));
#46970=CARTESIAN_POINT('Ctrl Pts',(55.0658647217664,27.0038296361361,11.2572723810671));
#46971=CARTESIAN_POINT('Ctrl Pts',(55.1764623906592,27.0130404073134,11.2645641521427));
#46972=CARTESIAN_POINT('Ctrl Pts',(55.1873642100168,27.0140387556618,11.2652790987927));
#46973=CARTESIAN_POINT('Ctrl Pts',(55.2036468969991,27.0156651394719,11.266340670464));
#46974=CARTESIAN_POINT('Ctrl Pts',(55.2090341084174,27.0162254058106,11.2666908717954));
#46975=CARTESIAN_POINT('Ctrl Pts',(55.2182861419752,27.0172257183547,11.2672904708707));
#46976=CARTESIAN_POINT('Ctrl Pts',(55.2221520181459,27.0176551325566,11.2675404522504));
#46977=CARTESIAN_POINT('Ctrl Pts',(55.2309297652658,27.0186561484762,11.2681067791808));
#46978=CARTESIAN_POINT('Ctrl Pts',(55.2358407766467,27.0192347075428,11.268422732906));
#46979=CARTESIAN_POINT('Ctrl Pts',(55.2491678441229,27.0208550175699,11.2692778264275));
#46980=CARTESIAN_POINT('Ctrl Pts',(55.2575796038254,27.0219321978807,11.2698150357994));
#46981=CARTESIAN_POINT('Ctrl Pts',(55.2986067582139,27.0274521429859,11.2724240676346));
#46982=CARTESIAN_POINT('Ctrl Pts',(55.3311176842266,27.0326483754199,11.2744571672946));
#46983=CARTESIAN_POINT('Ctrl Pts',(55.5636799573556,27.0757479214197,11.2888485689236));
#46984=CARTESIAN_POINT('Ctrl Pts',(55.7570269342608,27.1432795891194,11.3001195995548));
#46985=CARTESIAN_POINT('Ctrl Pts',(55.9851235877938,27.2646174476047,11.315637204581));
#46986=CARTESIAN_POINT('Ctrl Pts',(56.0323460457051,27.2922875191933,11.3189765773551));
#46987=CARTESIAN_POINT('Ctrl Pts',(56.0903450285641,27.3295575613019,11.3232731226583));
#46988=CARTESIAN_POINT('Ctrl Pts',(56.1022383607847,27.3373813420324,11.3241648735549));
#46989=CARTESIAN_POINT('Ctrl Pts',(56.1211632839835,27.3501230177068,11.3256016126305));
#46990=CARTESIAN_POINT('Ctrl Pts',(56.1282487965111,27.3549602389235,11.3261435836601));
#46991=CARTESIAN_POINT('Ctrl Pts',(56.1416480140955,27.3642350637088,11.3271763375125));
#46992=CARTESIAN_POINT('Ctrl Pts',(56.1479676173911,27.3686639029365,11.3276667828341));
#46993=CARTESIAN_POINT('Ctrl Pts',(56.1623010398905,27.3788334353158,11.328786920785));
#46994=CARTESIAN_POINT('Ctrl Pts',(56.170298273157,27.3845970521586,11.3294174806135));
#46995=CARTESIAN_POINT('Ctrl Pts',(56.190977627709,27.3997348472565,11.3310627694155));
#46996=CARTESIAN_POINT('Ctrl Pts',(56.2035916861997,27.4092004217546,11.3320810004226));
#46997=CARTESIAN_POINT('Ctrl Pts',(56.3198912977781,27.4986466006772,11.3416082309948));
#46998=CARTESIAN_POINT('Ctrl Pts',(56.4155582209887,27.5884907417956,11.3505192794644));
#46999=CARTESIAN_POINT('Ctrl Pts',(56.5642008691953,27.7585033218186,11.3662031736123));
#47000=CARTESIAN_POINT('Ctrl Pts',(56.6215010430894,27.8343357128936,11.3728620074662));
#47001=CARTESIAN_POINT('Ctrl Pts',(56.7045000295729,27.962206410939,11.383326558291));
#47002=CARTESIAN_POINT('Ctrl Pts',(56.733717580542,28.0117892052258,11.3872159803154));
#47003=CARTESIAN_POINT('Ctrl Pts',(56.7652595442498,28.0710337795722,11.3916149595212));
#47004=CARTESIAN_POINT('Ctrl Pts',(56.7697045602931,28.0795298617922,11.3922400129659));
#47005=CARTESIAN_POINT('Ctrl Pts',(56.7764362293486,28.0926256213812,11.3931942263326));
#47006=CARTESIAN_POINT('Ctrl Pts',(56.7787665945079,28.0972024902508,11.3935259974834));
#47007=CARTESIAN_POINT('Ctrl Pts',(56.7830162067056,28.105629119362,11.3941336094542));
#47008=CARTESIAN_POINT('Ctrl Pts',(56.7849406731348,28.1094760757955,11.3944097635522));
#47009=CARTESIAN_POINT('Ctrl Pts',(56.7892470684695,28.1181544889911,11.3950299857938));
#47010=CARTESIAN_POINT('Ctrl Pts',(56.7916218764551,28.1229893781989,11.3953736134827));
#47011=CARTESIAN_POINT('Ctrl Pts',(56.7985497886887,28.1372395489647,11.39638097881));
#47012=CARTESIAN_POINT('Ctrl Pts',(56.8030485498886,28.1466812575976,11.3970414824349));
#47013=CARTESIAN_POINT('Ctrl Pts',(56.8379331835604,28.2214026429685,11.40221752678));
#47014=CARTESIAN_POINT('Ctrl Pts',(56.8648420246144,28.2882564661799,11.4065429188741));
#47015=CARTESIAN_POINT('Ctrl Pts',(56.9444395663345,28.521775064005,11.4210962456151));
#47016=CARTESIAN_POINT('Ctrl Pts',(56.9788354861453,28.6938036829274,11.4309528728006));
#47017=CARTESIAN_POINT('Ctrl Pts',(56.9932374945223,28.9111594352699,11.4441485162267));
#47018=CARTESIAN_POINT('Ctrl Pts',(56.9946923734695,28.9542804791905,11.4467975103225));
#47019=CARTESIAN_POINT('Ctrl Pts',(56.99476537855,29.0105619864894,11.4503105398052));
#47020=CARTESIAN_POINT('Ctrl Pts',(56.9946524120196,29.0237110350117,11.4511352144567));
#47021=CARTESIAN_POINT('Ctrl Pts',(56.994255339853,29.0451969973119,11.4524895721761));
#47022=CARTESIAN_POINT('Ctrl Pts',(56.9940489264057,29.0535350800062,11.4530168362547));
#47023=CARTESIAN_POINT('Ctrl Pts',(56.9935487268386,29.06965385284,11.4540394640852));
#47024=CARTESIAN_POINT('Ctrl Pts',(56.9932616646249,29.0774346113075,11.4545346096159));
#47025=CARTESIAN_POINT('Ctrl Pts',(56.9924940056851,29.0953882406103,11.4556807000366));
#47026=CARTESIAN_POINT('Ctrl Pts',(56.9919810434053,29.1055594407311,11.456332639337));
#47027=CARTESIAN_POINT('Ctrl Pts',(56.990074019455,29.13837510108,11.4584448037075));
#47028=CARTESIAN_POINT('Ctrl Pts',(56.9883715616364,29.1609991750557,11.4599145400454));
#47029=CARTESIAN_POINT('Ctrl Pts',(56.9706370009248,29.352873172703,11.4724992754705));
#47030=CARTESIAN_POINT('Ctrl Pts',(56.9334156968592,29.5194328918238,11.4843076048697));
#47031=CARTESIAN_POINT('Ctrl Pts',(56.8407904073717,29.7752031435464,11.5032528194016));
#47032=CARTESIAN_POINT('Ctrl Pts',(56.7987082313077,29.8683908740254,11.5103225661561));
#47033=CARTESIAN_POINT('Ctrl Pts',(56.744085483942,29.9681573558627,11.5178044196688));
#47034=CARTESIAN_POINT('Ctrl Pts',(56.7384105845374,29.9783105314687,11.5185646924057));
#47035=CARTESIAN_POINT('Ctrl Pts',(56.7298966243721,29.9932351392568,11.5196798975187));
#47036=CARTESIAN_POINT('Ctrl Pts',(56.7271260534956,29.998045074131,11.5200389434309));
#47037=CARTESIAN_POINT('Ctrl Pts',(56.7221867913369,30.0065378698789,11.5206721704081));
#47038=CARTESIAN_POINT('Ctrl Pts',(56.7200263062706,30.0102253880732,11.520946863337));
#47039=CARTESIAN_POINT('Ctrl Pts',(56.7153146800594,30.018208263435,11.5215409702845));
#47040=CARTESIAN_POINT('Ctrl Pts',(56.712759251383,30.0225009865374,11.5218601041405));
#47041=CARTESIAN_POINT('Ctrl Pts',(56.7057089265652,30.0342438431595,11.5227322917705));
#47042=CARTESIAN_POINT('Ctrl Pts',(56.7011813069444,30.0416743429283,11.5232832841574));
#47043=CARTESIAN_POINT('Ctrl Pts',(56.6779296990015,30.0792777475948,11.5260683514539));
#47044=CARTESIAN_POINT('Ctrl Pts',(56.6584497701847,30.1089784716266,11.5282571768284));
#47045=CARTESIAN_POINT('Ctrl Pts',(56.5235827966939,30.3030988308923,11.5426002473784));
#47046=CARTESIAN_POINT('Ctrl Pts',(56.384718077233,30.4498083940027,11.5537364029792));
#47047=CARTESIAN_POINT('Ctrl Pts',(56.1832905434293,30.606804112294,11.5690775599648));
#47048=CARTESIAN_POINT('Ctrl Pts',(56.1389675135638,30.6385201148349,11.5724032847463));
#47049=CARTESIAN_POINT('Ctrl Pts',(56.0815140352899,30.6761733422431,11.5766844254249));
#47050=CARTESIAN_POINT('Ctrl Pts',(56.0695405298957,30.6838386859315,11.5775750040077));
#47051=CARTESIAN_POINT('Ctrl Pts',(56.0502154314054,30.6959211780004,11.5790103019502));
#47052=CARTESIAN_POINT('Ctrl Pts',(56.0429153689251,30.7004201315897,11.5795520150633));
#47053=CARTESIAN_POINT('Ctrl Pts',(56.028990297087,30.7088786079672,11.5805845690374));
#47054=CARTESIAN_POINT('Ctrl Pts',(56.0223708568591,30.7128470324534,11.5810750743839));
#47055=CARTESIAN_POINT('Ctrl Pts',(56.0072381223122,30.7218002934895,11.5821957572079));
#47056=CARTESIAN_POINT('Ctrl Pts',(55.998710595643,30.7267605584172,11.5828268050143));
#47057=CARTESIAN_POINT('Ctrl Pts',(55.9764346339918,30.7394977617485,11.584474205524));
#47058=CARTESIAN_POINT('Ctrl Pts',(55.9626302119269,30.7471748936516,11.5854940750603));
#47059=CARTESIAN_POINT('Ctrl Pts',(55.8487434066712,30.8087520015826,11.5939014310232));
#47060=CARTESIAN_POINT('Ctrl Pts',(55.7443292361195,30.8541616358887,11.6015864159689));
#47061=CARTESIAN_POINT('Ctrl Pts',(55.5191178840482,30.9300052446717,11.6180157406892));
#47062=CARTESIAN_POINT('Ctrl Pts',(55.3981702014958,30.9585362527315,11.6267587365386));
#47063=CARTESIAN_POINT('Ctrl Pts',(55.229270909195,30.9820765757837,11.6383863038472));
#47064=CARTESIAN_POINT('Ctrl Pts',(55.1829704066307,30.9868858300555,11.6415124074608));
#47065=CARTESIAN_POINT('Ctrl Pts',(55.1274674476777,30.9906939280707,11.6451551823163));
#47066=CARTESIAN_POINT('Ctrl Pts',(55.1183903006699,30.9912543809673,11.6457475911816));
#47067=CARTESIAN_POINT('Ctrl Pts',(55.1042870712974,30.9920283806608,11.646662504895));
#47068=CARTESIAN_POINT('Ctrl Pts',(55.0992636172063,30.9922850193292,11.6469873035451));
#47069=CARTESIAN_POINT('Ctrl Pts',(55.0899335041494,30.9927263002338,11.6475884722788));
#47070=CARTESIAN_POINT('Ctrl Pts',(55.0856272482452,30.9929159836027,11.647865106625));
#47071=CARTESIAN_POINT('Ctrl Pts',(55.0758010861741,30.993316901565,11.6484944737691));
#47072=CARTESIAN_POINT('Ctrl Pts',(55.0702808997442,30.9935191676066,11.64884670693));
#47073=CARTESIAN_POINT('Ctrl Pts',(55.0558537119054,30.993987795505,11.64976395579));
#47074=CARTESIAN_POINT('Ctrl Pts',(55.0469455263116,30.9942174129774,11.6503270090435));
#47075=CARTESIAN_POINT('Ctrl Pts',(54.985534342647,30.9953886148407,11.6541876066196));
#47076=CARTESIAN_POINT('Ctrl Pts',(54.9330085987675,30.9943164685395,11.6573841402503));
#47077=CARTESIAN_POINT('Ctrl Pts',(54.762663358078,30.9841002088027,11.6675820582695));
#47078=CARTESIAN_POINT('Ctrl Pts',(54.6456000893342,30.9665671405793,11.674338794889));
#47079=CARTESIAN_POINT('Ctrl Pts',(54.4310573289674,30.914642796971,11.6872228406813));
#47080=CARTESIAN_POINT('Ctrl Pts',(54.3333655511008,30.8828562472095,11.6932959173462));
#47081=CARTESIAN_POINT('Ctrl Pts',(54.216655678899,30.8346554927968,11.7010785500937));
#47082=CARTESIAN_POINT('Ctrl Pts',(54.1949169279538,30.8252206102214,11.702551157675));
#47083=CARTESIAN_POINT('Ctrl Pts',(54.1638179458321,30.8110596021933,11.704693600754));
#47084=CARTESIAN_POINT('Ctrl Pts',(54.1543182873272,30.8066432255937,11.7053529237307));
#47085=CARTESIAN_POINT('Ctrl Pts',(54.1378033478903,30.7988066601301,11.7065078914939));
#47086=CARTESIAN_POINT('Ctrl Pts',(54.1307724733942,30.7954197201834,11.707002386718));
#47087=CARTESIAN_POINT('Ctrl Pts',(54.116308301459,30.7883471085804,11.7080255454397));
#47088=CARTESIAN_POINT('Ctrl Pts',(54.108877772405,30.7846561492121,11.708554384587));
#47089=CARTESIAN_POINT('Ctrl Pts',(54.08991049671,30.7750865643953,11.7099126974463));
#47090=CARTESIAN_POINT('Ctrl Pts',(54.0784077102076,30.7691418409684,11.7107444599615));
#47091=CARTESIAN_POINT('Ctrl Pts',(54.0338060328609,30.7455383491732,11.7140014929461));
#47092=CARTESIAN_POINT('Ctrl Pts',(54.0011518347511,30.727060201742,11.716455327511));
#47093=CARTESIAN_POINT('Ctrl Pts',(53.8455808004784,30.6331385214987,11.7284941146177));
#47094=CARTESIAN_POINT('Ctrl Pts',(53.7305862545401,30.5454453602615,11.7385170621569));
#47095=CARTESIAN_POINT('Ctrl Pts',(53.554418469581,30.3780742330368,11.7554478092301));
#47096=CARTESIAN_POINT('Ctrl Pts',(53.4879209909797,30.3047664452506,11.7623080824137));
#47097=CARTESIAN_POINT('Ctrl Pts',(53.4165316190242,30.2132403889172,11.7700068399111));
#47098=CARTESIAN_POINT('Ctrl Pts',(53.4061121366401,30.1995190210127,11.7711397341577));
#47099=CARTESIAN_POINT('Ctrl Pts',(53.3920085517055,30.1804377568026,11.7726842012654));
#47100=CARTESIAN_POINT('Ctrl Pts',(53.3881712780076,30.1751927370725,11.77310557299));
#47101=CARTESIAN_POINT('Ctrl Pts',(53.3817423034834,30.166314496629,11.7738133735093));
#47102=CARTESIAN_POINT('Ctrl Pts',(53.379137060122,30.162691192376,11.7741007146021));
#47103=CARTESIAN_POINT('Ctrl Pts',(53.3741925220906,30.1557655402927,11.7746470061117));
#47104=CARTESIAN_POINT('Ctrl Pts',(53.3718510931912,30.1524647835488,11.774906106986));
#47105=CARTESIAN_POINT('Ctrl Pts',(53.3663105937225,30.144603650465,11.7755202545913));
#47106=CARTESIAN_POINT('Ctrl Pts',(53.3631205283975,30.1400369248669,11.7758746962761));
#47107=CARTESIAN_POINT('Ctrl Pts',(53.3519231939686,30.1238635289034,11.7771219969975));
#47108=CARTESIAN_POINT('Ctrl Pts',(53.3440196850044,30.1121850623111,11.7780082085665));
#47109=CARTESIAN_POINT('Ctrl Pts',(53.2550712399639,29.9777015268172,11.7880615295092));
#47110=CARTESIAN_POINT('Ctrl Pts',(53.1877167505972,29.8463564868758,11.7964675023511));
#47111=CARTESIAN_POINT('Ctrl Pts',(53.0978000261856,29.6098134243791,11.8111852845085));
#47112=CARTESIAN_POINT('Ctrl Pts',(53.0681362896592,29.5080553194961,11.8173932560157));
#47113=CARTESIAN_POINT('Ctrl Pts',(53.0466869751866,29.4044697635106,11.8238528479472));
#47114=CARTESIAN_POINT('Origin',(55.,29.,3.45145488139523));
#47115=CARTESIAN_POINT('',(53.0466869981368,29.4044698743445,12.7818778464297));
#47116=CARTESIAN_POINT('',(53.0466869618782,29.40446969924,12.6249522205985));
#47117=CARTESIAN_POINT('',(53.0466869980082,29.4044698737233,3.45145488139523));
#47118=CARTESIAN_POINT('Ctrl Pts',(53.0466869981368,29.4044698743445,12.7818778464297));
#47119=CARTESIAN_POINT('Ctrl Pts',(53.0469807175671,29.4058883384094,12.7817808958998));
#47120=CARTESIAN_POINT('Ctrl Pts',(53.0472759905022,29.4073065231312,12.7816840045254));
#47121=CARTESIAN_POINT('Ctrl Pts',(53.0508269250449,29.4242689082659,12.7805256115402));
#47122=CARTESIAN_POINT('Ctrl Pts',(53.0542666696385,29.4397745153647,12.7794716157396));
#47123=CARTESIAN_POINT('Ctrl Pts',(53.059784672939,29.4633150901057,12.7778805836053));
#47124=CARTESIAN_POINT('Ctrl Pts',(53.0617284056302,29.4713805469485,12.7773371087376));
#47125=CARTESIAN_POINT('Ctrl Pts',(53.0654257556411,29.4863129439443,12.7763342637471));
#47126=CARTESIAN_POINT('Ctrl Pts',(53.0671657510172,29.4931830856705,12.7758741902327));
#47127=CARTESIAN_POINT('Ctrl Pts',(53.0700923085679,29.5044847953235,12.7751196865686));
#47128=CARTESIAN_POINT('Ctrl Pts',(53.0712575919899,29.5089217334113,12.7748240717453));
#47129=CARTESIAN_POINT('Ctrl Pts',(53.0735748342935,29.5176225947702,12.7742455933827));
#47130=CARTESIAN_POINT('Ctrl Pts',(53.0747256630267,29.5218867671066,12.7739626707361));
#47131=CARTESIAN_POINT('Ctrl Pts',(53.0776027074517,29.5324080602647,12.7732659549003));
#47132=CARTESIAN_POINT('Ctrl Pts',(53.0793453377625,29.538660713488,12.7728530959449));
#47133=CARTESIAN_POINT('Ctrl Pts',(53.0854797427908,29.5602630103817,12.7714304733238));
#47134=CARTESIAN_POINT('Ctrl Pts',(53.0900253867448,29.5755688233227,12.7704290973774));
#47135=CARTESIAN_POINT('Ctrl Pts',(53.1287771273081,29.7005336338774,12.7622950028036));
#47136=CARTESIAN_POINT('Ctrl Pts',(53.1722180030145,29.8071198302848,12.7556138070175));
#47137=CARTESIAN_POINT('Ctrl Pts',(53.2583711081099,29.9753174010266,12.7446364069224));
#47138=CARTESIAN_POINT('Ctrl Pts',(53.2957887879018,30.0393165683998,12.7403464341676));
#47139=CARTESIAN_POINT('Ctrl Pts',(53.3833185954148,30.171540967188,12.7309981990839));
#47140=CARTESIAN_POINT('Ctrl Pts',(53.434383462705,30.2389549345588,12.7259248507387));
#47141=CARTESIAN_POINT('Ctrl Pts',(53.5006892289883,30.3158209917544,12.7196246731006));
#47142=CARTESIAN_POINT('Ctrl Pts',(53.5119789453286,30.3285747940256,12.7185611613115));
#47143=CARTESIAN_POINT('Ctrl Pts',(53.5285580851662,30.3468275382929,12.717011682796));
#47144=CARTESIAN_POINT('Ctrl Pts',(53.533718112029,30.3524433995764,12.716531110956));
#47145=CARTESIAN_POINT('Ctrl Pts',(53.5442094291191,30.3637308989587,12.7155573053078));
#47146=CARTESIAN_POINT('Ctrl Pts',(53.5495419627123,30.3694011940714,12.7150640235623));
#47147=CARTESIAN_POINT('Ctrl Pts',(53.560660914068,30.3810866087176,12.7140388568684));
#47148=CARTESIAN_POINT('Ctrl Pts',(53.5664521615184,30.387096902307,12.7135067696218));
#47149=CARTESIAN_POINT('Ctrl Pts',(53.5814824381475,30.402501012635,12.7121304824753));
#47150=CARTESIAN_POINT('Ctrl Pts',(53.5907770110707,30.4118398342138,12.7112838749136));
#47151=CARTESIAN_POINT('Ctrl Pts',(53.6281408870226,30.448645022466,12.7078975961662));
#47152=CARTESIAN_POINT('Ctrl Pts',(53.6569245260463,30.4753703738079,12.705326399433));
#47153=CARTESIAN_POINT('Ctrl Pts',(53.7897970430816,30.5916293569452,12.693613143375));
#47154=CARTESIAN_POINT('Ctrl Pts',(53.902160051911,30.6711109754286,12.6840856601796));
#47155=CARTESIAN_POINT('Ctrl Pts',(54.1115938632293,30.7889620011166,12.6673376095533));
#47156=CARTESIAN_POINT('Ctrl Pts',(54.2052082189494,30.8324739062092,12.6601692430189));
#47157=CARTESIAN_POINT('Ctrl Pts',(54.3180257856908,30.8746305574751,12.6521776693993));
#47158=CARTESIAN_POINT('Ctrl Pts',(54.3343566065144,30.8804912861943,12.6510362977437));
#47159=CARTESIAN_POINT('Ctrl Pts',(54.3570447364804,30.8883008856725,12.6494738504019));
#47160=CARTESIAN_POINT('Ctrl Pts',(54.3633378864325,30.8904319775887,12.6490429180195));
#47161=CARTESIAN_POINT('Ctrl Pts',(54.3739038021108,30.8939512386906,12.6483236455304));
#47162=CARTESIAN_POINT('Ctrl Pts',(54.3781707756586,30.8953564731948,12.6480343277204));
#47163=CARTESIAN_POINT('Ctrl Pts',(54.3862653810412,30.8979919766568,12.6474877167445));
#47164=CARTESIAN_POINT('Ctrl Pts',(54.3900920346013,30.8992251052471,12.6472302534951));
#47165=CARTESIAN_POINT('Ctrl Pts',(54.4001229472724,30.9024240959168,12.6465577592845));
#47166=CARTESIAN_POINT('Ctrl Pts',(54.4063332068295,30.9043711982228,12.6461438104408));
#47167=CARTESIAN_POINT('Ctrl Pts',(54.4279100276121,30.9110203716658,12.6447135488102));
#47168=CARTESIAN_POINT('Ctrl Pts',(54.4433242650814,30.915567268953,12.6437057441309));
#47169=CARTESIAN_POINT('Ctrl Pts',(54.5631483565472,30.9493444376689,12.6359671451629));
#47170=CARTESIAN_POINT('Ctrl Pts',(54.6697433670408,30.9702080482977,12.6296372771496));
#47171=CARTESIAN_POINT('Ctrl Pts',(54.8892131666344,30.9948400571664,12.6168002770721));
#47172=CARTESIAN_POINT('Ctrl Pts',(55.0017613389849,30.9979128181507,12.6103129097961));
#47173=CARTESIAN_POINT('Ctrl Pts',(55.1520442615367,30.9893126425146,12.6012908456711));
#47174=CARTESIAN_POINT('Ctrl Pts',(55.1900500859954,30.9860420315021,12.5989796643989));
#47175=CARTESIAN_POINT('Ctrl Pts',(55.2547043451046,30.9786053721479,12.5949814732795));
#47176=CARTESIAN_POINT('Ctrl Pts',(55.2814053186271,30.9749846737277,12.5933108433031));
#47177=CARTESIAN_POINT('Ctrl Pts',(55.3189152194206,30.969122181462,12.5909329380871));
#47178=CARTESIAN_POINT('Ctrl Pts',(55.3297921431914,30.9673297174679,12.5902397214954));
#47179=CARTESIAN_POINT('Ctrl Pts',(55.348437426219,30.9640980964444,12.5890448382132));
#47180=CARTESIAN_POINT('Ctrl Pts',(55.3562131967178,30.9627027609968,12.5885445604634));
#47181=CARTESIAN_POINT('Ctrl Pts',(55.3710329026332,30.959952448083,12.5875872479403));
#47182=CARTESIAN_POINT('Ctrl Pts',(55.378078233747,30.9586055908613,12.5871304769543));
#47183=CARTESIAN_POINT('Ctrl Pts',(55.396289149536,30.9550222872038,12.5859454255917));
#47184=CARTESIAN_POINT('Ctrl Pts',(55.4074430001156,30.9527282008281,12.5852153311277));
#47185=CARTESIAN_POINT('Ctrl Pts',(55.4392753333226,30.9458964319583,12.583119171732));
#47186=CARTESIAN_POINT('Ctrl Pts',(55.4599015373,30.9411249989401,12.5817457573221));
#47187=CARTESIAN_POINT('Ctrl Pts',(55.6375786384987,30.8970323775887,12.5697795394161));
#47188=CARTESIAN_POINT('Ctrl Pts',(55.7893503483131,30.8390607756676,12.5585644909368));
#47189=CARTESIAN_POINT('Ctrl Pts',(56.0272010954461,30.7132953853573,12.5398157953161));
#47190=CARTESIAN_POINT('Ctrl Pts',(56.1178000634325,30.6556120318695,12.5323675653387));
#47191=CARTESIAN_POINT('Ctrl Pts',(56.2135251244105,30.5832080491782,12.5244576851107));
#47192=CARTESIAN_POINT('Ctrl Pts',(56.2236458039212,30.5753989721196,12.5236209921141));
#47193=CARTESIAN_POINT('Ctrl Pts',(56.2382230593088,30.5639259829635,12.5224161085554));
#47194=CARTESIAN_POINT('Ctrl Pts',(56.2427396715284,30.5603393655242,12.5220428221697));
#47195=CARTESIAN_POINT('Ctrl Pts',(56.250625287318,30.5540214804236,12.5213912512246));
#47196=CARTESIAN_POINT('Ctrl Pts',(56.2540010231757,30.5512987482055,12.5211123749626));
#47197=CARTESIAN_POINT('Ctrl Pts',(56.2611556148693,30.5454895283538,12.5205214600203));
#47198=CARTESIAN_POINT('Ctrl Pts',(56.2649320364964,30.5424001787604,12.5202096300353));
#47199=CARTESIAN_POINT('Ctrl Pts',(56.2751824261471,30.5339517505051,12.519363308362));
#47200=CARTESIAN_POINT('Ctrl Pts',(56.2816340094107,30.5285654924379,12.5188307246091));
#47201=CARTESIAN_POINT('Ctrl Pts',(56.3117415347404,30.5031048775729,12.5163446995061));
#47202=CARTESIAN_POINT('Ctrl Pts',(56.3349625019758,30.4825199803991,12.514425476324));
#47203=CARTESIAN_POINT('Ctrl Pts',(56.508349319307,30.3214371952223,12.4999955531089));
#47204=CARTESIAN_POINT('Ctrl Pts',(56.6364681248181,30.1590111191995,12.4886248397088));
#47205=CARTESIAN_POINT('Ctrl Pts',(56.7644602352575,29.9320509535065,12.4729768284465));
#47206=CARTESIAN_POINT('Ctrl Pts',(56.7894299815248,29.8831638721457,12.4696278131885));
#47207=CARTESIAN_POINT('Ctrl Pts',(56.8183040055526,29.8203664709771,12.4653203855262));
#47208=CARTESIAN_POINT('Ctrl Pts',(56.8241176511922,29.8073570346285,12.464427809293));
#47209=CARTESIAN_POINT('Ctrl Pts',(56.8332086375814,29.7864142087479,12.4629900553531));
#47210=CARTESIAN_POINT('Ctrl Pts',(56.8365750857559,29.7785198567145,12.4624479024795));
#47211=CARTESIAN_POINT('Ctrl Pts',(56.8428714222693,29.7634867560393,12.4614150068315));
#47212=CARTESIAN_POINT('Ctrl Pts',(56.8458110418532,29.7563522332293,12.4609246029548));
#47213=CARTESIAN_POINT('Ctrl Pts',(56.8524096261533,29.7400697341147,12.459804845473));
#47214=CARTESIAN_POINT('Ctrl Pts',(56.8560423360711,29.7309114005182,12.459174626859));
#47215=CARTESIAN_POINT('Ctrl Pts',(56.8653066195212,29.7070409698004,12.4575308149755));
#47216=CARTESIAN_POINT('Ctrl Pts',(56.8708319382767,29.6922886342081,12.4565137300095));
#47217=CARTESIAN_POINT('Ctrl Pts',(56.9208045725075,29.5538952469641,12.4469593702906));
#47218=CARTESIAN_POINT('Ctrl Pts',(56.9531007330669,29.426234631655,12.4380171297419));
#47219=CARTESIAN_POINT('Ctrl Pts',(56.9867412635985,29.2023107019161,12.4222896991071));
#47220=CARTESIAN_POINT('Ctrl Pts',(56.9941264447753,29.1073812093336,12.4156190822399));
#47221=CARTESIAN_POINT('Ctrl Pts',(56.9950631103932,28.9553076072849,12.4051829705105));
#47222=CARTESIAN_POINT('Ctrl Pts',(56.9929725583891,28.8983343042015,12.4013311509275));
#47223=CARTESIAN_POINT('Ctrl Pts',(56.9876847042695,28.8319862647204,12.3969690147217));
#47224=CARTESIAN_POINT('Ctrl Pts',(56.9868559761586,28.822454407065,12.396345335888));
#47225=CARTESIAN_POINT('Ctrl Pts',(56.9854774396395,28.8078197948792,12.3953927740173));
#47226=CARTESIAN_POINT('Ctrl Pts',(56.9849764817205,28.8027127398921,12.3950612934741));
#47227=CARTESIAN_POINT('Ctrl Pts',(56.984019347162,28.7933280431443,12.3944539578454));
#47228=CARTESIAN_POINT('Ctrl Pts',(56.9835690428404,28.7890499570381,12.3941777915038));
#47229=CARTESIAN_POINT('Ctrl Pts',(56.9825231289395,28.7794128800063,12.3935572233162));
#47230=CARTESIAN_POINT('Ctrl Pts',(56.9819196297804,28.7740548362671,12.3932132642148));
#47231=CARTESIAN_POINT('Ctrl Pts',(56.9803117541251,28.7602819679727,12.3923317068439));
#47232=CARTESIAN_POINT('Ctrl Pts',(56.9792754541041,28.7518708780475,12.3917958292416));
#47233=CARTESIAN_POINT('Ctrl Pts',(56.972525621047,28.6998214539949,12.3884937290925));
#47234=CARTESIAN_POINT('Ctrl Pts',(56.9654223242158,28.6563719727547,12.3857982192397));
#47235=CARTESIAN_POINT('Ctrl Pts',(56.9521007887792,28.5889778749672,12.3816634594334));
#47236=CARTESIAN_POINT('Ctrl Pts',(56.9468658581084,28.5648562515874,12.3801929312834));
#47237=CARTESIAN_POINT('Ctrl Pts',(56.9313726420217,28.4993561800107,12.37621084027));
#47238=CARTESIAN_POINT('Ctrl Pts',(56.9202334216269,28.4581989903333,12.3737206098934));
#47239=CARTESIAN_POINT('Ctrl Pts',(56.8833808671552,28.3375154408049,12.3663770209431));
#47240=CARTESIAN_POINT('Ctrl Pts',(56.8539810328816,28.2592144146441,12.3615546783459));
#47241=CARTESIAN_POINT('Ctrl Pts',(56.7858590401036,28.1074836800017,12.3517677098077));
#47242=CARTESIAN_POINT('Ctrl Pts',(56.7472965761595,28.034168608491,12.3468141078856));
#47243=CARTESIAN_POINT('Ctrl Pts',(56.6932543802115,27.9453111121851,12.3403874789645));
#47244=CARTESIAN_POINT('Ctrl Pts',(56.681924158206,27.9273350389749,12.3390646514332));
#47245=CARTESIAN_POINT('Ctrl Pts',(56.6648269473191,27.9011463368598,12.337102026232));
#47246=CARTESIAN_POINT('Ctrl Pts',(56.6592814534784,27.8927903586988,12.3364703986549));
#47247=CARTESIAN_POINT('Ctrl Pts',(56.6493458815801,27.8780616755569,12.3353472379894));
#47248=CARTESIAN_POINT('Ctrl Pts',(56.6449812567447,27.8716719877798,12.3348566644428));
#47249=CARTESIAN_POINT('Ctrl Pts',(56.6357506204271,27.8583259936068,12.3338249461486));
#47250=CARTESIAN_POINT('Ctrl Pts',(56.6308771687532,27.8513750455905,12.3332835264904));
#47251=CARTESIAN_POINT('Ctrl Pts',(56.6179498966411,27.833185160458,12.3318558106746));
#47252=CARTESIAN_POINT('Ctrl Pts',(56.609823443596,27.8219986407486,12.3309667549569));
#47253=CARTESIAN_POINT('Ctrl Pts',(56.5749104778022,27.7749749638184,12.3271817531637));
#47254=CARTESIAN_POINT('Ctrl Pts',(56.5470403225838,27.7399622759849,12.3242441343239));
#47255=CARTESIAN_POINT('Ctrl Pts',(56.3939753250386,27.5604098677388,12.3085229482105));
#47256=CARTESIAN_POINT('Ctrl Pts',(56.2496602941024,27.4335029933563,12.2949413010943));
#47257=CARTESIAN_POINT('Ctrl Pts',(56.0439061910508,27.2993364814037,12.2781087408986));
#47258=CARTESIAN_POINT('Ctrl Pts',(55.9970590764081,27.2714541074201,12.2744306170181));
#47259=CARTESIAN_POINT('Ctrl Pts',(55.9407979191054,27.2410183450529,12.2702391888441));
#47260=CARTESIAN_POINT('Ctrl Pts',(55.9324390631535,27.2365730553797,12.2696221471703));
#47261=CARTESIAN_POINT('Ctrl Pts',(55.9195199596595,27.2298201449515,12.2686775641504));
#47262=CARTESIAN_POINT('Ctrl Pts',(55.9149820975493,27.2274703280323,12.2683474911085));
#47263=CARTESIAN_POINT('Ctrl Pts',(55.9066064345219,27.2231739387031,12.267741485731));
#47264=CARTESIAN_POINT('Ctrl Pts',(55.902771380429,27.2212223538216,12.2674652519518));
#47265=CARTESIAN_POINT('Ctrl Pts',(55.8940933592255,27.2168415715172,12.2668429706206));
#47266=CARTESIAN_POINT('Ctrl Pts',(55.889246799769,27.2144196890535,12.2664973770948));
#47267=CARTESIAN_POINT('Ctrl Pts',(55.8748848028341,27.2073158096509,12.2654788221483));
#47268=CARTESIAN_POINT('Ctrl Pts',(55.8653416528803,27.2026898264538,12.2648092030439));
#47269=CARTESIAN_POINT('Ctrl Pts',(55.7783528166889,27.1613760024374,12.2587663115671));
#47270=CARTESIAN_POINT('Ctrl Pts',(55.6986447001155,27.1296335501159,12.2536637070502));
#47271=CARTESIAN_POINT('Ctrl Pts',(55.5331329645086,27.0757859887222,12.2434632996674));
#47272=CARTESIAN_POINT('Ctrl Pts',(55.4474104211088,27.054067156049,12.2383800131883));
#47273=CARTESIAN_POINT('Ctrl Pts',(55.2891787274565,27.0249895912462,12.2289766640238));
#47274=CARTESIAN_POINT('Ctrl Pts',(55.2171702024508,27.0157806819274,12.2246904993772));
#47275=CARTESIAN_POINT('Ctrl Pts',(55.1020526795171,27.0074007087402,12.2176971814632));
#47276=CARTESIAN_POINT('Ctrl Pts',(55.0591942192437,27.0056674499854,12.2150632937176));
#47277=CARTESIAN_POINT('Ctrl Pts',(55.0031933620288,27.0052093931292,12.2115675280871));
#47278=CARTESIAN_POINT('Ctrl Pts',(54.9900708043404,27.0052315520567,12.2107445187354));
#47279=CARTESIAN_POINT('Ctrl Pts',(54.9686154417186,27.005479496088,12.209392202544));
#47280=CARTESIAN_POINT('Ctrl Pts',(54.9602820096874,27.0056280414954,12.2088653004958));
#47281=CARTESIAN_POINT('Ctrl Pts',(54.9441637224632,27.0060164164032,12.2078428821351));
#47282=CARTESIAN_POINT('Ctrl Pts',(54.9363788480573,27.0062496225048,12.2073475809117));
#47283=CARTESIAN_POINT('Ctrl Pts',(54.9184037419414,27.0068934747523,12.2062004111372));
#47284=CARTESIAN_POINT('Ctrl Pts',(54.9082149646363,27.0073366889396,12.2055475422439));
#47285=CARTESIAN_POINT('Ctrl Pts',(54.8752929394498,27.0090218362612,12.2034292715091));
#47286=CARTESIAN_POINT('Ctrl Pts',(54.8525780991494,27.0105748036605,12.2019542813809));
#47287=CARTESIAN_POINT('Ctrl Pts',(54.6612150089133,27.0269531557886,12.1894095930878));
#47288=CARTESIAN_POINT('Ctrl Pts',(54.4950886623826,27.0628032986198,12.1776532116537));
#47289=CARTESIAN_POINT('Ctrl Pts',(54.2666424042816,27.1435111129261,12.1607783175178));
#47290=CARTESIAN_POINT('Ctrl Pts',(54.1991456005843,27.1716132918691,12.1557104095432));
#47291=CARTESIAN_POINT('Ctrl Pts',(54.1122935776851,27.2135087903003,12.1491932020922));
#47292=CARTESIAN_POINT('Ctrl Pts',(54.0914271279094,27.2240301324643,12.147627948555));
#47293=CARTESIAN_POINT('Ctrl Pts',(54.0566478650104,27.2423401120278,12.1450255987048));
#47294=CARTESIAN_POINT('Ctrl Pts',(54.0426352136535,27.2499330765607,12.1439789364462));
#47295=CARTESIAN_POINT('Ctrl Pts',(54.0232101475868,27.2607619883571,12.1425321261216));
#47296=CARTESIAN_POINT('Ctrl Pts',(54.0177202268807,27.2638566514157,12.1421236938401));
#47297=CARTESIAN_POINT('Ctrl Pts',(54.0084012250866,27.269168117333,12.1414313050845));
#47298=CARTESIAN_POINT('Ctrl Pts',(54.0045647103038,27.2713717224522,12.1411465237209));
#47299=CARTESIAN_POINT('Ctrl Pts',(53.9971963651563,27.2756365945551,12.1406001338026));
#47300=CARTESIAN_POINT('Ctrl Pts',(53.9936635181788,27.2776959704575,12.1403384031488));
#47301=CARTESIAN_POINT('Ctrl Pts',(53.9851937603913,27.2826681406235,12.1397114446968));
#47302=CARTESIAN_POINT('Ctrl Pts',(53.9802629891993,27.2855913993721,12.1393468817709));
#47303=CARTESIAN_POINT('Ctrl Pts',(53.9623353057765,27.2963247205819,12.1380226829196));
#47304=CARTESIAN_POINT('Ctrl Pts',(53.9494145678477,27.3042618841627,12.1370708298266));
#47305=CARTESIAN_POINT('Ctrl Pts',(53.8233671803382,27.3836861356027,12.1277971116481));
#47306=CARTESIAN_POINT('Ctrl Pts',(53.7175985178434,27.466249022772,12.1200962504797));
#47307=CARTESIAN_POINT('Ctrl Pts',(53.6158559968772,27.5636081977957,12.111916902352));
#47308=CARTESIAN_POINT('Ctrl Pts',(53.610851254808,27.5684477675121,12.1115124383648));
#47309=CARTESIAN_POINT('Ctrl Pts',(53.5115931108928,27.6654407336976,12.1034463747051));
#47310=CARTESIAN_POINT('Ctrl Pts',(53.4266910328677,27.7666727975071,12.0957150572584));
#47311=CARTESIAN_POINT('Ctrl Pts',(53.3418616630034,27.8909670392705,12.086389355817));
#47312=CARTESIAN_POINT('Ctrl Pts',(53.3315439851451,27.9065507134296,12.0852234561522));
#47313=CARTESIAN_POINT('Ctrl Pts',(53.3162995543261,27.9302938980027,12.0834509320837));
#47314=CARTESIAN_POINT('Ctrl Pts',(53.3112096252535,27.9383477968127,12.0828503326364));
#47315=CARTESIAN_POINT('Ctrl Pts',(53.3021185782943,27.9529635618515,12.0817614257736));
#47316=CARTESIAN_POINT('Ctrl Pts',(53.2980972926105,27.9595127118127,12.0812738681964));
#47317=CARTESIAN_POINT('Ctrl Pts',(53.2895590352827,27.9736002255042,12.0802258131476));
#47318=CARTESIAN_POINT('Ctrl Pts',(53.2850538469439,27.9811455064953,12.0796649014469));
#47319=CARTESIAN_POINT('Ctrl Pts',(53.2730945654491,28.0014789534306,12.0781543297065));
#47320=CARTESIAN_POINT('Ctrl Pts',(53.2657328271436,28.0143205318152,12.0772013830375));
#47321=CARTESIAN_POINT('Ctrl Pts',(53.2311111292295,28.0763022459907,12.0726059440563));
#47322=CARTESIAN_POINT('Ctrl Pts',(53.2057952194443,28.1264935291507,12.0688958513932));
#47323=CARTESIAN_POINT('Ctrl Pts',(53.1160457451258,28.324844784901,12.0542681238157));
#47324=CARTESIAN_POINT('Ctrl Pts',(53.0675850115898,28.4795406667179,12.0428693902826));
#47325=CARTESIAN_POINT('Ctrl Pts',(53.0267901116386,28.7008247081689,12.0273344514217));
#47326=CARTESIAN_POINT('Ctrl Pts',(53.0182625760941,28.7638189554259,12.0230047605399));
#47327=CARTESIAN_POINT('Ctrl Pts',(53.0115515312456,28.8409612466387,12.0178929337683));
#47328=CARTESIAN_POINT('Ctrl Pts',(53.0104918948063,28.8548167946697,12.0169822758678));
#47329=CARTESIAN_POINT('Ctrl Pts',(53.009184388195,28.8746351419822,12.0156914535194));
#47330=CARTESIAN_POINT('Ctrl Pts',(53.0088183780508,28.8805893704338,12.0153051515565));
#47331=CARTESIAN_POINT('Ctrl Pts',(53.0082307806828,28.8909037237693,12.0146386937589));
#47332=CARTESIAN_POINT('Ctrl Pts',(53.007996787886,28.8952630679949,12.0143578603055));
#47333=CARTESIAN_POINT('Ctrl Pts',(53.0075666182819,28.9038008397764,12.0138095334786));
#47334=CARTESIAN_POINT('Ctrl Pts',(53.007369272093,28.9079791219841,12.0135419721796));
#47335=CARTESIAN_POINT('Ctrl Pts',(53.0068614750438,28.9194991921929,12.0128063536769));
#47336=CARTESIAN_POINT('Ctrl Pts',(53.006578443521,28.9268422123311,12.0123397937604));
#47337=CARTESIAN_POINT('Ctrl Pts',(53.0056202914725,28.9558672745944,12.0105042251296));
#47338=CARTESIAN_POINT('Ctrl Pts',(53.0052582589013,28.9775590614289,12.0091514244171));
#47339=CARTESIAN_POINT('Ctrl Pts',(53.0051991626429,29.1354634294638,11.999414201243));
#47340=CARTESIAN_POINT('Ctrl Pts',(53.0190996273219,29.2712417536779,11.9916209411359));
#47341=CARTESIAN_POINT('Ctrl Pts',(53.0466870113634,29.4044699382199,11.9837090255998));
#47342=CARTESIAN_POINT('Ctrl Pts',(53.0466869751866,29.4044697635106,11.8238528479472));
#47343=CARTESIAN_POINT('Ctrl Pts',(53.0419512156118,29.3815992755424,11.8252790508395));
#47344=CARTESIAN_POINT('Ctrl Pts',(53.037615893422,29.3586396669258,11.8267169431701));
#47345=CARTESIAN_POINT('Ctrl Pts',(53.0307704408819,29.3185315798298,11.8292425819739));
#47346=CARTESIAN_POINT('Ctrl Pts',(53.0280795442047,29.30142513244,11.830324114331));
#47347=CARTESIAN_POINT('Ctrl Pts',(53.0242942861441,29.2751362439084,11.8319937253997));
#47348=CARTESIAN_POINT('Ctrl Pts',(53.0230404475711,29.2659773372315,11.8325768036252));
#47349=CARTESIAN_POINT('Ctrl Pts',(53.0209591771938,29.2499457901447,11.8335999813272));
#47350=CARTESIAN_POINT('Ctrl Pts',(53.0201037655562,29.2430768915739,11.8340391966616));
#47351=CARTESIAN_POINT('Ctrl Pts',(53.0182496217826,29.2275287387491,11.8350353117973));
#47352=CARTESIAN_POINT('Ctrl Pts',(53.0172721282171,29.2188471407096,11.8355928665027));
#47353=CARTESIAN_POINT('Ctrl Pts',(53.0147764264254,29.1952907738518,11.8371095265229));
#47354=CARTESIAN_POINT('Ctrl Pts',(53.0133684061827,29.1804051379565,11.8380720434669));
#47355=CARTESIAN_POINT('Ctrl Pts',(53.0075080436848,29.1100167962154,11.8426437734471));
#47356=CARTESIAN_POINT('Ctrl Pts',(53.0052139371755,29.0543640789963,11.8463191563776));
#47357=CARTESIAN_POINT('Ctrl Pts',(53.0053217315665,28.8899112222531,11.8573648722136));
#47358=CARTESIAN_POINT('Ctrl Pts',(53.0142912576156,28.781329208358,11.8649080511666));
#47359=CARTESIAN_POINT('Ctrl Pts',(53.0505905309261,28.5621830167179,11.8803896986878));
#47360=CARTESIAN_POINT('Ctrl Pts',(53.0786206905866,28.4521064091951,11.8883022770975));
#47361=CARTESIAN_POINT('Ctrl Pts',(53.1211067553984,28.3298928969766,11.8968733832638));
#47362=CARTESIAN_POINT('Ctrl Pts',(53.1265401053883,28.3148493479945,11.8979243464688));
#47363=CARTESIAN_POINT('Ctrl Pts',(53.1344338257212,28.2937899722925,11.8993882463013));
#47364=CARTESIAN_POINT('Ctrl Pts',(53.1367433787841,28.2877187913659,11.8998094073322));
#47365=CARTESIAN_POINT('Ctrl Pts',(53.1405295564135,28.2779104094156,11.9004882930398));
#47366=CARTESIAN_POINT('Ctrl Pts',(53.1419878661865,28.2741662596018,11.9007470821577));
#47367=CARTESIAN_POINT('Ctrl Pts',(53.1451016006014,28.2662427531927,11.9012939350696));
#47368=CARTESIAN_POINT('Ctrl Pts',(53.1467598594749,28.2620645342128,11.9015818228112));
#47369=CARTESIAN_POINT('Ctrl Pts',(53.1509091233061,28.2517120757535,11.9022940238727));
#47370=CARTESIAN_POINT('Ctrl Pts',(53.1534169676304,28.2455445702882,11.9027173421247));
#47371=CARTESIAN_POINT('Ctrl Pts',(53.1629450897412,28.2224443337686,11.9042996105202));
#47372=CARTESIAN_POINT('Ctrl Pts',(53.1701680246017,28.2055954712677,11.9054470909592));
#47373=CARTESIAN_POINT('Ctrl Pts',(53.1890811128194,28.1631043211552,11.9083299580833));
#47374=CARTESIAN_POINT('Ctrl Pts',(53.2010845336275,28.1376051376242,11.9100497229659));
#47375=CARTESIAN_POINT('Ctrl Pts',(53.303190217923,27.9321157218,11.9238918679677));
#47376=CARTESIAN_POINT('Ctrl Pts',(53.4195222732825,27.7664501705442,11.9350644621512));
#47377=CARTESIAN_POINT('Ctrl Pts',(53.591511541332,27.5866913990487,11.9500752093234));
#47378=CARTESIAN_POINT('Ctrl Pts',(53.6255399602801,27.5535768267661,11.9529813306361));
#47379=CARTESIAN_POINT('Ctrl Pts',(53.6711831189628,27.5122255619556,11.9568202564802));
#47380=CARTESIAN_POINT('Ctrl Pts',(53.6817513418575,27.5028535338857,11.9577051740104));
#47381=CARTESIAN_POINT('Ctrl Pts',(53.6988785196684,27.4879868909286,11.9591335130573));
#47382=CARTESIAN_POINT('Ctrl Pts',(53.7053749676326,27.4824207531465,11.9596739807484));
#47383=CARTESIAN_POINT('Ctrl Pts',(53.7178032855557,27.4719100875166,11.9607055790849));
#47384=CARTESIAN_POINT('Ctrl Pts',(53.7237284702546,27.4669578692044,11.9611963838534));
#47385=CARTESIAN_POINT('Ctrl Pts',(53.7373167027513,27.4557343156967,11.9623197442445));
#47386=CARTESIAN_POINT('Ctrl Pts',(53.7449979445959,27.4494854247736,11.9629531855563));
#47387=CARTESIAN_POINT('Ctrl Pts',(53.7687893592911,27.4304231024851,11.9649105506074));
#47388=CARTESIAN_POINT('Ctrl Pts',(53.7850511834993,27.4178019719537,11.9662420142328));
#47389=CARTESIAN_POINT('Ctrl Pts',(53.8637276223799,27.3586677674977,11.9726555461709));
#47390=CARTESIAN_POINT('Ctrl Pts',(53.9286267770662,27.3155881631054,11.9778663714132));
#47391=CARTESIAN_POINT('Ctrl Pts',(54.0713039527384,27.2324670177253,11.9891448209487));
#47392=CARTESIAN_POINT('Ctrl Pts',(54.1495377513363,27.1935223697184,11.9952286001361));
#47393=CARTESIAN_POINT('Ctrl Pts',(54.325178939865,27.1200333978468,12.0084967750014));
#47394=CARTESIAN_POINT('Ctrl Pts',(54.4232447037284,27.0876675370054,12.0156629276098));
#47395=CARTESIAN_POINT('Ctrl Pts',(54.5389890551211,27.05918707542,12.0235598166266));
#47396=CARTESIAN_POINT('Ctrl Pts',(54.5546428189481,27.0555353127704,12.0246160802028));
#47397=CARTESIAN_POINT('Ctrl Pts',(54.5766955352554,27.0506710754432,12.0260860621106));
#47398=CARTESIAN_POINT('Ctrl Pts',(54.5830584099579,27.0493002180431,12.0265080937872));
#47399=CARTESIAN_POINT('Ctrl Pts',(54.5933623770618,27.0471329870347,12.027188004103));
#47400=CARTESIAN_POINT('Ctrl Pts',(54.5972993029406,27.0463173553511,12.0274469532736));
#47401=CARTESIAN_POINT('Ctrl Pts',(54.6056402678626,27.044615601903,12.0279937803656));
#47402=CARTESIAN_POINT('Ctrl Pts',(54.6100448875586,27.0437324432224,12.0282814839686));
#47403=CARTESIAN_POINT('Ctrl Pts',(54.6209706816359,27.0415801078761,12.028992600216));
#47404=CARTESIAN_POINT('Ctrl Pts',(54.6274953522048,27.040328601931,12.0294150244595));
#47405=CARTESIAN_POINT('Ctrl Pts',(54.6519458204627,27.0357652517017,12.0309900444762));
#47406=CARTESIAN_POINT('Ctrl Pts',(54.669911126967,27.032666462086,12.0321313059987));
#47407=CARTESIAN_POINT('Ctrl Pts',(54.7155410940459,27.0254385489766,12.0349952878808));
#47408=CARTESIAN_POINT('Ctrl Pts',(54.7432554469232,27.0216440702078,12.0367026451986));
#47409=CARTESIAN_POINT('Ctrl Pts',(54.8705082851564,27.0069407617222,12.0444324790711));
#47410=CARTESIAN_POINT('Ctrl Pts',(54.9707066919013,27.002952628509,12.0502184319241));
#47411=CARTESIAN_POINT('Ctrl Pts',(55.2020989685393,27.0111691653767,12.0636654421015));
#47412=CARTESIAN_POINT('Ctrl Pts',(55.3326122572786,27.0287933533485,12.071330909542));
#47413=CARTESIAN_POINT('Ctrl Pts',(55.4841150389246,27.0647345553516,12.0809165538984));
#47414=CARTESIAN_POINT('Ctrl Pts',(55.5076864227765,27.070784063731,12.0824272693655));
#47415=CARTESIAN_POINT('Ctrl Pts',(55.5405813134076,27.0798710103584,12.0845653123574));
#47416=CARTESIAN_POINT('Ctrl Pts',(55.5500026743539,27.0825484240716,12.085181116696));
#47417=CARTESIAN_POINT('Ctrl Pts',(55.5663382016336,27.0873210425458,12.086255025847));
#47418=CARTESIAN_POINT('Ctrl Pts',(55.573261467544,27.0893846434909,12.0867121043316));
#47419=CARTESIAN_POINT('Ctrl Pts',(55.587688354362,27.0937703035204,12.0876687001785));
#47420=CARTESIAN_POINT('Ctrl Pts',(55.5951897623571,27.0960991618526,12.088168431345));
#47421=CARTESIAN_POINT('Ctrl Pts',(55.6129472503702,27.1017272847668,12.0893570565879));
#47422=CARTESIAN_POINT('Ctrl Pts',(55.6231906580103,27.1050654287251,12.0900472074169));
#47423=CARTESIAN_POINT('Ctrl Pts',(55.6575150540122,27.1165595517097,12.0923752391267));
#47424=CARTESIAN_POINT('Ctrl Pts',(55.6814662270759,27.1250926285658,12.0940253832694));
#47425=CARTESIAN_POINT('Ctrl Pts',(55.7383164421377,27.1465798601157,12.0980056521678));
#47426=CARTESIAN_POINT('Ctrl Pts',(55.7710460736974,27.1599551409798,12.1003489849417));
#47427=CARTESIAN_POINT('Ctrl Pts',(55.8976860216487,27.2156799144859,12.1096214791105));
#47428=CARTESIAN_POINT('Ctrl Pts',(55.9886052921856,27.2644039644018,12.1167402977709));
#47429=CARTESIAN_POINT('Ctrl Pts',(56.1791081919703,27.3863368829186,12.1324957911777));
#47430=CARTESIAN_POINT('Ctrl Pts',(56.2765030712926,27.4622256391759,12.1411262917899));
#47431=CARTESIAN_POINT('Ctrl Pts',(56.3777562598497,27.5574108790346,12.1503290114144));
#47432=CARTESIAN_POINT('Ctrl Pts',(56.3891053221239,27.5683358898091,12.1513638446633));
#47433=CARTESIAN_POINT('Ctrl Pts',(56.4049214252137,27.5839261949023,12.1528092350562));
#47434=CARTESIAN_POINT('Ctrl Pts',(56.4094967138372,27.5884801634515,12.1532277484406));
#47435=CARTESIAN_POINT('Ctrl Pts',(56.4171601308041,27.5961822870067,12.1539292738617));
#47436=CARTESIAN_POINT('Ctrl Pts',(56.4202600458961,27.5993185904848,12.1542131948735));
#47437=CARTESIAN_POINT('Ctrl Pts',(56.4265703415529,27.6057454477852,12.1547914102444));
#47438=CARTESIAN_POINT('Ctrl Pts',(56.4297797855824,27.6090368583078,12.1550856333739));
#47439=CARTESIAN_POINT('Ctrl Pts',(56.4379389268974,27.6174624550732,12.1558340682869));
#47440=CARTESIAN_POINT('Ctrl Pts',(56.4428725726163,27.6226121956811,12.1562870579342));
#47441=CARTESIAN_POINT('Ctrl Pts',(56.462891721976,27.6437337888924,12.1581274586418));
#47442=CARTESIAN_POINT('Ctrl Pts',(56.4777411421276,27.6599285704001,12.159498010232));
#47443=CARTESIAN_POINT('Ctrl Pts',(56.5163113070324,27.7034142026811,12.1630830153467));
#47444=CARTESIAN_POINT('Ctrl Pts',(56.5395635825951,27.7311111189526,12.1652704749985));
#47445=CARTESIAN_POINT('Ctrl Pts',(56.6755312922512,27.9023130084241,12.1783302321244));
#47446=CARTESIAN_POINT('Ctrl Pts',(56.7688718930371,28.0600947716442,12.1885476842108));
#47447=CARTESIAN_POINT('Ctrl Pts',(56.8598050429194,28.2768692697035,12.2026782303178));
#47448=CARTESIAN_POINT('Ctrl Pts',(56.8782197384901,28.3261433816623,12.2058888243322));
#47449=CARTESIAN_POINT('Ctrl Pts',(56.8992433578435,28.3899865112696,12.2100754965742));
#47450=CARTESIAN_POINT('Ctrl Pts',(56.9036680884007,28.4039382749811,12.2109919623107));
#47451=CARTESIAN_POINT('Ctrl Pts',(56.9104678913919,28.426227291768,12.2124590853075));
#47452=CARTESIAN_POINT('Ctrl Pts',(56.9129428983815,28.4345336893609,12.2130064917863));
#47453=CARTESIAN_POINT('Ctrl Pts',(56.9172994802477,28.4495108520588,12.2139948045407));
#47454=CARTESIAN_POINT('Ctrl Pts',(56.9192005806321,28.4561758296227,12.2144350706508));
#47455=CARTESIAN_POINT('Ctrl Pts',(56.9235815537708,28.471843986474,12.2154711951535));
#47456=CARTESIAN_POINT('Ctrl Pts',(56.9260329978837,28.4808548807646,12.2160679590589));
#47457=CARTESIAN_POINT('Ctrl Pts',(56.9329647357412,28.5070592552695,12.2178061159177));
#47458=CARTESIAN_POINT('Ctrl Pts',(56.9372786033813,28.5242954418574,12.2189528017679));
#47459=CARTESIAN_POINT('Ctrl Pts',(56.9741730293097,28.6805417574891,12.2293808984508));
#47460=CARTESIAN_POINT('Ctrl Pts',(56.99196488151,28.8225912117635,12.2391445851376));
#47461=CARTESIAN_POINT('Ctrl Pts',(56.9967301029314,29.0964381919624,12.2582071533406));
#47462=CARTESIAN_POINT('Ctrl Pts',(56.9860720076567,29.2274971143795,12.2674223188148));
#47463=CARTESIAN_POINT('Ctrl Pts',(56.9598826317511,29.3716483979431,12.277118753755));
#47464=CARTESIAN_POINT('Ctrl Pts',(56.9569691736887,29.3866964562119,12.2781252115103));
#47465=CARTESIAN_POINT('Ctrl Pts',(56.95272378902,29.4073456389041,12.2794969838196));
#47466=CARTESIAN_POINT('Ctrl Pts',(56.9515407254034,29.4129763489545,12.2798700889732));
#47467=CARTESIAN_POINT('Ctrl Pts',(56.949473969176,29.422605696224,12.2805064249537));
#47468=CARTESIAN_POINT('Ctrl Pts',(56.9486023039066,29.426606836467,12.2807703201062));
#47469=CARTESIAN_POINT('Ctrl Pts',(56.9467642156186,29.4349208961341,12.2813175678194));
#47470=CARTESIAN_POINT('Ctrl Pts',(56.945795773709,29.4392333144551,12.2816007941594));
#47471=CARTESIAN_POINT('Ctrl Pts',(56.9434170715261,29.4496632751095,12.2822843594));
#47472=CARTESIAN_POINT('Ctrl Pts',(56.9419922333662,29.4557775147664,12.2826838765769));
#47473=CARTESIAN_POINT('Ctrl Pts',(56.9368837210311,29.4772401396713,12.2840823888012));
#47474=CARTESIAN_POINT('Ctrl Pts',(56.9330466530229,29.4925518992694,12.2850730853336));
#47475=CARTESIAN_POINT('Ctrl Pts',(56.9081058231038,29.5872938172732,12.2911684978436));
#47476=CARTESIAN_POINT('Ctrl Pts',(56.8822892840167,29.6654111490091,12.2960445877808));
#47477=CARTESIAN_POINT('Ctrl Pts',(56.8015962854423,29.8668632091009,12.3087435340589));
#47478=CARTESIAN_POINT('Ctrl Pts',(56.7389150577306,29.9865976090572,12.3164428204456));
#47479=CARTESIAN_POINT('Ctrl Pts',(56.6311141609693,30.1498677420976,12.3281376082845));
#47480=CARTESIAN_POINT('Ctrl Pts',(56.5952884820006,30.1990758151192,12.3318364687067));
#47481=CARTESIAN_POINT('Ctrl Pts',(56.547795852996,30.2584059508841,12.3365656426763));
#47482=CARTESIAN_POINT('Ctrl Pts',(56.5381843928376,30.2701363287175,12.3375144693885));
#47483=CARTESIAN_POINT('Ctrl Pts',(56.5227399730999,30.2885531559872,12.3390268337446));
#47484=CARTESIAN_POINT('Ctrl Pts',(56.5169944191003,30.2953123908205,12.3395868386569));
#47485=CARTESIAN_POINT('Ctrl Pts',(56.5061925278264,30.3078496014009,12.3406349531305));
#47486=CARTESIAN_POINT('Ctrl Pts',(56.5011475305854,30.3136371643264,12.341122592085));
#47487=CARTESIAN_POINT('Ctrl Pts',(56.4898413192851,30.3264573361728,12.3422113536783));
#47488=CARTESIAN_POINT('Ctrl Pts',(56.4835635006655,30.3334749925806,12.3428131593945));
#47489=CARTESIAN_POINT('Ctrl Pts',(56.4650446992758,30.3538835792914,12.3445806552348));
#47490=CARTESIAN_POINT('Ctrl Pts',(56.4526706912477,30.3671519828045,12.3457519162749));
#47491=CARTESIAN_POINT('Ctrl Pts',(56.4242266887403,30.3968297444831,12.3484232444066));
#47492=CARTESIAN_POINT('Ctrl Pts',(56.4080510403679,30.4131338195804,12.3499277312928));
#47493=CARTESIAN_POINT('Ctrl Pts',(56.353891399217,30.4658702123953,12.3549187738795));
#47494=CARTESIAN_POINT('Ctrl Pts',(56.3147493991992,30.501076493275,12.3584539259184));
#47495=CARTESIAN_POINT('Ctrl Pts',(56.1794946706626,30.6133793199982,12.3704263803881));
#47496=CARTESIAN_POINT('Ctrl Pts',(56.0776448662427,30.6831155136171,12.3790754108769));
#47497=CARTESIAN_POINT('Ctrl Pts',(55.898656786947,30.7827267944133,12.3932814793841));
#47498=CARTESIAN_POINT('Ctrl Pts',(55.8249058789421,30.8180297654826,12.3988794317685));
#47499=CARTESIAN_POINT('Ctrl Pts',(55.739385175626,30.8526869808828,12.4049397574574));
#47500=CARTESIAN_POINT('Ctrl Pts',(55.7295485465239,30.8565824562932,12.4056305384745));
#47501=CARTESIAN_POINT('Ctrl Pts',(55.7146332005614,30.8623523420861,12.4066680127006));
#47502=CARTESIAN_POINT('Ctrl Pts',(55.7095772648969,30.8642845716856,12.4070179715116));
#47503=CARTESIAN_POINT('Ctrl Pts',(55.7004879783124,30.8677158961167,12.4076439466111));
#47504=CARTESIAN_POINT('Ctrl Pts',(55.6964576013655,30.8692225354257,12.4079203999416));
#47505=CARTESIAN_POINT('Ctrl Pts',(55.6876258132563,30.8724915116391,12.4085237474727));
#47506=CARTESIAN_POINT('Ctrl Pts',(55.6828224951334,30.8742484258394,12.4088503215082));
#47507=CARTESIAN_POINT('Ctrl Pts',(55.6690897125291,30.8792116785985,12.409779679836));
#47508=CARTESIAN_POINT('Ctrl Pts',(55.6601439145152,30.8823728634177,12.4103798782418));
#47509=CARTESIAN_POINT('Ctrl Pts',(55.5992040329686,30.9034193749124,12.4144354161375));
#47510=CARTESIAN_POINT('Ctrl Pts',(55.5465071744757,30.9192138732791,12.4177794640655));
#47511=CARTESIAN_POINT('Ctrl Pts',(55.3009911366779,30.9818653087853,12.4329019155806));
#47512=CARTESIAN_POINT('Ctrl Pts',(55.1025220139745,31.0019699918356,12.4439664273347));
#47513=CARTESIAN_POINT('Ctrl Pts',(54.8658582572031,30.99060737848,12.4583638784567));
#47514=CARTESIAN_POINT('Ctrl Pts',(54.8274412590852,30.9876455727915,12.4607341798565));
#47515=CARTESIAN_POINT('Ctrl Pts',(54.7761289782824,30.9821908134408,12.4639554113397));
#47516=CARTESIAN_POINT('Ctrl Pts',(54.7631361902104,30.9806802311339,12.4647758093165));
#47517=CARTESIAN_POINT('Ctrl Pts',(54.7418994474283,30.9779992371245,12.4661249240122));
#47518=CARTESIAN_POINT('Ctrl Pts',(54.7336461694053,30.9769047804184,12.4666512581355));
#47519=CARTESIAN_POINT('Ctrl Pts',(54.7176821979909,30.9746860351847,12.4676733511091));
#47520=CARTESIAN_POINT('Ctrl Pts',(54.7099707539901,30.9735681676936,12.4681688997993));
#47521=CARTESIAN_POINT('Ctrl Pts',(54.6919822097886,30.9708528033732,12.4693292217248));
#47522=CARTESIAN_POINT('Ctrl Pts',(54.6817107357628,30.9692200662155,12.4699950907774));
#47523=CARTESIAN_POINT('Ctrl Pts',(54.6484996092183,30.9636742527576,12.4721590983502));
#47524=CARTESIAN_POINT('Ctrl Pts',(54.6256162328235,30.959440178979,12.4736672634306));
#47525=CARTESIAN_POINT('Ctrl Pts',(54.5058477989047,30.9351050527657,12.4816540133819));
#47526=CARTESIAN_POINT('Ctrl Pts',(54.4104971514521,30.9082188780357,12.4883446342128));
#47527=CARTESIAN_POINT('Ctrl Pts',(54.2188552461025,30.8384426630757,12.5024181705178));
#47528=CARTESIAN_POINT('Ctrl Pts',(54.1231601719404,30.7947728583041,12.5097970797009));
#47529=CARTESIAN_POINT('Ctrl Pts',(53.9711076309196,30.7103090387457,12.521806593635));
#47530=CARTESIAN_POINT('Ctrl Pts',(53.9126331261713,30.6737418787728,12.5264988281467));
#47531=CARTESIAN_POINT('Ctrl Pts',(53.8476891926842,30.6282857120999,12.5317028428716));
#47532=CARTESIAN_POINT('Ctrl Pts',(53.8392609786101,30.6222883504641,12.5323780232504));
#47533=CARTESIAN_POINT('Ctrl Pts',(53.8265351566805,30.613082940841,12.5333967410772));
#47534=CARTESIAN_POINT('Ctrl Pts',(53.8222033548238,30.6099227859656,12.5337433750676));
#47535=CARTESIAN_POINT('Ctrl Pts',(53.8145248190347,30.6042735280494,12.5343575044096));
#47536=CARTESIAN_POINT('Ctrl Pts',(53.811173117761,30.6017913729685,12.5346254616606));
#47537=CARTESIAN_POINT('Ctrl Pts',(53.8078084765724,30.5992832565342,12.5348943391444));
#47538=CARTESIAN_POINT('Ctrl Pts',(53.8077878272654,30.5992678632258,12.5348959892817));
#47539=CARTESIAN_POINT('Ctrl Pts',(53.807746700905,30.5992372037786,12.534899275783));
#47540=CARTESIAN_POINT('Ctrl Pts',(53.8077262236916,30.5992219375308,12.5349009121598));
#47541=CARTESIAN_POINT('Ctrl Pts',(53.8076854378746,30.599191529519,12.5349041714315));
#47542=CARTESIAN_POINT('Ctrl Pts',(53.8076651294104,30.599176387869,12.5349057943153));
#47543=CARTESIAN_POINT('Ctrl Pts',(53.8076246787578,30.5991462273426,12.5349090267877));
#47544=CARTESIAN_POINT('Ctrl Pts',(53.8076045363477,30.5991312083105,12.5349106363941));
#47545=CARTESIAN_POINT('Ctrl Pts',(53.8075644135963,30.5991012899123,12.534913842648));
#47546=CARTESIAN_POINT('Ctrl Pts',(53.8075444337523,30.5990863909264,12.5349154392559));
#47547=CARTESIAN_POINT('Ctrl Pts',(53.8075046343914,30.59905671135,12.5349186196521));
#47548=CARTESIAN_POINT('Ctrl Pts',(53.8074848145996,30.5990419305637,12.5349202034626));
#47549=CARTESIAN_POINT('Ctrl Pts',(53.8074453315781,30.5990124846063,12.534923358565));
#47550=CARTESIAN_POINT('Ctrl Pts',(53.8074256685349,30.5989978195833,12.5349249298422));
#47551=CARTESIAN_POINT('Ctrl Pts',(53.8073864977531,30.5989686042417,12.5349280599789));
#47552=CARTESIAN_POINT('Ctrl Pts',(53.8073669893436,30.5989540534315,12.5349296188921));
#47553=CARTESIAN_POINT('Ctrl Pts',(53.8032720508302,30.5958996297157,12.5352568438614));
#47554=CARTESIAN_POINT('Ctrl Pts',(53.7992082037635,30.5928441467766,12.5355814269861));
#47555=CARTESIAN_POINT('Ctrl Pts',(53.7907535307393,30.5864365898141,12.536256483283));
#47556=CARTESIAN_POINT('Ctrl Pts',(53.7863648497103,30.5830817416007,12.5366067655989));
#47557=CARTESIAN_POINT('Ctrl Pts',(53.7750381924555,30.5743484979265,12.5375106331926));
#47558=CARTESIAN_POINT('Ctrl Pts',(53.7681215993419,30.5689423938447,12.5380624123228));
#47559=CARTESIAN_POINT('Ctrl Pts',(53.7477544398615,30.5528054211746,12.5396874870066));
#47560=CARTESIAN_POINT('Ctrl Pts',(53.7344064362684,30.5419457164503,12.5407528524038));
#47561=CARTESIAN_POINT('Ctrl Pts',(53.6864631204206,30.5018978144699,12.5445876006126));
#47562=CARTESIAN_POINT('Ctrl Pts',(53.6527213766615,30.4717054839354,12.547302310406));
#47563=CARTESIAN_POINT('Ctrl Pts',(53.5095985960259,30.3345866168695,12.5590364742024));
#47564=CARTESIAN_POINT('Ctrl Pts',(53.4116969465367,30.2164349910421,12.5676929370378));
#47565=CARTESIAN_POINT('Ctrl Pts',(53.2920782945655,30.0326800778617,12.5807543067708));
#47566=CARTESIAN_POINT('Ctrl Pts',(53.2586986786024,29.9753425252075,12.5847747144192));
#47567=CARTESIAN_POINT('Ctrl Pts',(53.2210968400383,29.9026476104092,12.5898651574802));
#47568=CARTESIAN_POINT('Ctrl Pts',(53.2141174477524,29.8887590501956,12.5908372996373));
#47569=CARTESIAN_POINT('Ctrl Pts',(53.2033728835073,29.8667403337599,12.5923785544426));
#47570=CARTESIAN_POINT('Ctrl Pts',(53.1994988633785,29.8586637611448,12.5929439001637));
#47571=CARTESIAN_POINT('Ctrl Pts',(53.1924391459161,29.8436877789592,12.5939923305448));
#47572=CARTESIAN_POINT('Ctrl Pts',(53.1892382103987,29.8367957028458,12.5944748807675));
#47573=CARTESIAN_POINT('Ctrl Pts',(53.1822171173267,29.8214493417256,12.5955495608239));
#47574=CARTESIAN_POINT('Ctrl Pts',(53.1784164193892,29.8129863981877,12.5961423415963));
#47575=CARTESIAN_POINT('Ctrl Pts',(53.1676277042094,29.7885078691729,12.597857479758));
#47576=CARTESIAN_POINT('Ctrl Pts',(53.1607910554668,29.7724269003875,12.5989849167366));
#47577=CARTESIAN_POINT('Ctrl Pts',(53.1075557881091,29.6424932672407,12.6081024705636));
#47578=CARTESIAN_POINT('Ctrl Pts',(53.071588248345,29.5247259449193,12.6164396592281));
#47579=CARTESIAN_POINT('Ctrl Pts',(53.0466869618782,29.40446969924,12.6249522205985));
#47580=CARTESIAN_POINT('Origin',(55.,29.,3.45145488139523));
#47581=CARTESIAN_POINT('',(53.0466869980082,29.4044698737233,13.5836009930267));
#47582=CARTESIAN_POINT('',(53.04668699692,29.404469868468,13.4272582639285));
#47583=CARTESIAN_POINT('',(53.0466869980082,29.4044698737233,3.45145488139523));
#47584=CARTESIAN_POINT('',(53.0052507998914,29.001786383575,12.8095451186048));
#47585=CARTESIAN_POINT('Ctrl Pts',(53.0052507998914,29.001786383575,12.8095451186048));
#47586=CARTESIAN_POINT('Ctrl Pts',(53.0051890516009,28.9328357086924,12.8139430725437));
#47587=CARTESIAN_POINT('Ctrl Pts',(53.0087066016235,28.8638003853531,12.8183410264827));
#47588=CARTESIAN_POINT('Ctrl Pts',(53.0158030880324,28.7950849516546,12.8227389804216));
#47589=CARTESIAN_POINT('Ctrl Pts',(53.0228954791111,28.7264091731285,12.8271343963337));
#47590=CARTESIAN_POINT('Ctrl Pts',(53.0335626602207,28.6580534147751,12.8315298122457));
#47591=CARTESIAN_POINT('Ctrl Pts',(53.0477522628778,28.5904193175927,12.8359252281577));
#47592=CARTESIAN_POINT('Ctrl Pts',(53.0619387315161,28.5228001585686,12.8403196732662));
#47593=CARTESIAN_POINT('Ctrl Pts',(53.0796459745629,28.4559028336968,12.8447141183747));
#47594=CARTESIAN_POINT('Ctrl Pts',(53.1007704663719,28.3901190762986,12.8491085634832));
#47595=CARTESIAN_POINT('Ctrl Pts',(53.1223815493405,28.3228200258898,12.8536042322405));
#47596=CARTESIAN_POINT('Ctrl Pts',(53.1475691441378,28.256687014512,12.8580999009978));
#47597=CARTESIAN_POINT('Ctrl Pts',(53.1761690580459,28.1921211367596,12.8625955697552));
#47598=CARTESIAN_POINT('Ctrl Pts',(53.2041597928622,28.1289305142925,12.8669954806225));
#47599=CARTESIAN_POINT('Ctrl Pts',(53.2354186133925,28.067241345108,12.8713953914898));
#47600=CARTESIAN_POINT('Ctrl Pts',(53.269744656693,28.0074054153596,12.8757953023572));
#47601=CARTESIAN_POINT('Ctrl Pts',(53.3051912872886,27.9456161179573,12.8803388500595));
#47602=CARTESIAN_POINT('Ctrl Pts',(53.3439085797145,27.8858036579552,12.8848823977619));
#47603=CARTESIAN_POINT('Ctrl Pts',(53.3856280207344,27.828321428436,12.8894259454642));
#47604=CARTESIAN_POINT('Ctrl Pts',(53.4273474617544,27.7708391989169,12.8939694931665));
#47605=CARTESIAN_POINT('Ctrl Pts',(53.4720686272115,27.715687600944,12.8985130408689));
#47606=CARTESIAN_POINT('Ctrl Pts',(53.5194807316863,27.6631790476463,12.9030565885712));
#47607=CARTESIAN_POINT('Ctrl Pts',(53.5659798138644,27.6116816597558,12.9075126404662));
#47608=CARTESIAN_POINT('Ctrl Pts',(53.6152600337689,27.5625123993747,12.9119686923612));
#47609=CARTESIAN_POINT('Ctrl Pts',(53.6670591499095,27.515986437845,12.9164247442562));
#47610=CARTESIAN_POINT('Ctrl Pts',(53.7187809653277,27.4695299078173,12.9208741463074));
#47611=CARTESIAN_POINT('Ctrl Pts',(53.7730138550993,27.4257091713566,12.9253235483587));
#47612=CARTESIAN_POINT('Ctrl Pts',(53.8294571511627,27.3848043457414,12.9297729504099));
#47613=CARTESIAN_POINT('Ctrl Pts',(53.8858345639926,27.3439472661363,12.9342171589126));
#47614=CARTESIAN_POINT('Ctrl Pts',(53.9444168644604,27.3059996228174,12.9386613674154));
#47615=CARTESIAN_POINT('Ctrl Pts',(54.0048699297654,27.2712016584301,12.9431055759181));
#47616=CARTESIAN_POINT('Ctrl Pts',(54.0652853203789,27.2364253803305,12.9475470147651));
#47617=CARTESIAN_POINT('Ctrl Pts',(54.1275687400213,27.2047951304345,12.951988453612));
#47618=CARTESIAN_POINT('Ctrl Pts',(54.1913579525975,27.1765073069319,12.956429892459));
#47619=CARTESIAN_POINT('Ctrl Pts',(54.2551290295052,27.1482275258328,12.9608700685773));
#47620=CARTESIAN_POINT('Ctrl Pts',(54.3204046026038,27.1232884826883,12.9653102446956));
#47621=CARTESIAN_POINT('Ctrl Pts',(54.386800359913,27.1018393735257,12.969750420814));
#47622=CARTESIAN_POINT('Ctrl Pts',(54.4531997412496,27.0803890936233,12.9741908392869));
#47623=CARTESIAN_POINT('Ctrl Pts',(54.5207189620964,27.0624292738929,12.9786312577599));
#47624=CARTESIAN_POINT('Ctrl Pts',(54.5889580729728,27.0480594023573,12.9830716762329));
#47625=CARTESIAN_POINT('Ctrl Pts',(54.6572691170193,27.0336743830509,12.9875167755022));
#47626=CARTESIAN_POINT('Ctrl Pts',(54.7263010862091,27.0228869657343,12.9919618747714));
#47627=CARTESIAN_POINT('Ctrl Pts',(54.7956442995689,27.0157454018697,12.9964069740407));
#47628=CARTESIAN_POINT('Ctrl Pts',(54.8650282663177,27.0085996408686,13.0008546857193));
#47629=CARTESIAN_POINT('Ctrl Pts',(54.9347233528058,27.0051040226376,13.0053023973979));
#47630=CARTESIAN_POINT('Ctrl Pts',(55.0043180075572,27.0052546735709,13.0097501090766));
#47631=CARTESIAN_POINT('Ctrl Pts',(55.0740323330363,27.0054055835544,13.0142054687692));
#47632=CARTESIAN_POINT('Ctrl Pts',(55.1436453939375,27.0092152509383,13.0186608284618));
#47633=CARTESIAN_POINT('Ctrl Pts',(55.2127497158283,27.0166278410457,13.0231161881544));
#47634=CARTESIAN_POINT('Ctrl Pts',(55.2470960604591,27.0203120588699,13.0253305984151));
#47635=CARTESIAN_POINT('Ctrl Pts',(55.2813168731432,27.0248855094267,13.0275450086759));
#47636=CARTESIAN_POINT('Ctrl Pts',(55.3153632560029,27.0303366837799,13.0297594189366));
#47637=CARTESIAN_POINT('Ctrl Pts',(55.3838747019394,27.0413060674741,13.0342154708316));
#47638=CARTESIAN_POINT('Ctrl Pts',(55.4519473094091,27.0558757741474,13.0386715227266));
#47639=CARTESIAN_POINT('Ctrl Pts',(55.5191739402604,27.0739974085546,13.0431275746216));
#47640=CARTESIAN_POINT('Ctrl Pts',(55.5863002476406,27.0920919997314,13.0475769766729));
#47641=CARTESIAN_POINT('Ctrl Pts',(55.6525826157851,27.1137278715667,13.0520263787241));
#47642=CARTESIAN_POINT('Ctrl Pts',(55.7176223913188,27.1388053121777,13.0564757807753));
#47643=CARTESIAN_POINT('Ctrl Pts',(55.7825862494096,27.1638534812368,13.060919989278));
#47644=CARTESIAN_POINT('Ctrl Pts',(55.8463099415538,27.1923350651303,13.0653641977808));
#47645=CARTESIAN_POINT('Ctrl Pts',(55.9084100494376,27.2241005815135,13.0698084062836));
#47646=CARTESIAN_POINT('Ctrl Pts',(55.9704714561837,27.2558463014476,13.0742498451305));
#47647=CARTESIAN_POINT('Ctrl Pts',(56.030910851616,27.2908716715472,13.0786912839774));
#47648=CARTESIAN_POINT('Ctrl Pts',(56.0893662903561,27.3289797583704,13.0831327228244));
#47649=CARTESIAN_POINT('Ctrl Pts',(56.1478051098524,27.3670770108283,13.0875728989427));
#47650=CARTESIAN_POINT('Ctrl Pts',(56.2042606830138,27.4082549730815,13.092013075061));
#47651=CARTESIAN_POINT('Ctrl Pts',(56.2583986406965,27.4522724969836,13.0964532511794));
#47652=CARTESIAN_POINT('Ctrl Pts',(56.3125395533489,27.4962924234598,13.1008936696524));
#47653=CARTESIAN_POINT('Ctrl Pts',(56.3643622214861,27.5431519088996,13.1053340881254));
#47654=CARTESIAN_POINT('Ctrl Pts',(56.4135654592249,27.592569626949,13.1097745065984));
#47655=CARTESIAN_POINT('Ctrl Pts',(56.4628205637716,27.6420394378974,13.1142196058676));
#47656=CARTESIAN_POINT('Ctrl Pts',(56.5094503812403,27.6940725164669,13.1186647051369));
#47657=CARTESIAN_POINT('Ctrl Pts',(56.5531914064352,27.7483514800569,13.1231098044062));
#47658=CARTESIAN_POINT('Ctrl Pts',(56.5969581384719,27.8026623436931,13.1275575160848));
#47659=CARTESIAN_POINT('Ctrl Pts',(56.6378324125062,27.8592213230825,13.1320052277634));
#47660=CARTESIAN_POINT('Ctrl Pts',(56.6755934288613,27.9176810896704,13.1364529394421));
#47661=CARTESIAN_POINT('Ctrl Pts',(56.713419376759,27.9762413801108,13.1409082991347));
#47662=CARTESIAN_POINT('Ctrl Pts',(56.7481211381305,28.0367085577472,13.1453636588273));
#47663=CARTESIAN_POINT('Ctrl Pts',(56.7795237191017,28.0987104263032,13.1498190185199));
#47664=CARTESIAN_POINT('Ctrl Pts',(56.7951314819567,28.1295266978026,13.1520334287806));
#47665=CARTESIAN_POINT('Ctrl Pts',(56.8099249942695,28.1607217689548,13.1542478390414));
#47666=CARTESIAN_POINT('Ctrl Pts',(56.8238872899822,28.1922483575124,13.1564622493021));
#47667=CARTESIAN_POINT('Ctrl Pts',(56.8519835806166,28.2556892280575,13.1609183011971));
#47668=CARTESIAN_POINT('Ctrl Pts',(56.8768209254941,28.3207220085586,13.1653743530921));
#47669=CARTESIAN_POINT('Ctrl Pts',(56.8982182734294,28.3869788348524,13.1698304049871));
#47670=CARTESIAN_POINT('Ctrl Pts',(56.91958368973,28.4531367849315,13.1742798070383));
#47671=CARTESIAN_POINT('Ctrl Pts',(56.9375191492765,28.5205146935349,13.1787292090895));
#47672=CARTESIAN_POINT('Ctrl Pts',(56.951891265693,28.5887238769252,13.1831786111407));
#47673=CARTESIAN_POINT('Ctrl Pts',(56.9662466063086,28.6568534433929,13.1876228196435));
#47674=CARTESIAN_POINT('Ctrl Pts',(56.9770467646036,28.7258118811823,13.1920670281462));
#47675=CARTESIAN_POINT('Ctrl Pts',(56.9842083969008,28.7951961910305,13.196511236649));
#47676=CARTESIAN_POINT('Ctrl Pts',(56.9913655660283,28.8645372601852,13.2009526754959));
#47677=CARTESIAN_POINT('Ctrl Pts',(56.994888657593,28.934303189525,13.2053941143429));
#47678=CARTESIAN_POINT('Ctrl Pts',(56.994745820978,29.0040831594111,13.2098355531898));
#47679=CARTESIAN_POINT('Ctrl Pts',(56.9946030249724,29.0738432904193,13.2142757293081));
#47680=CARTESIAN_POINT('Ctrl Pts',(56.9907963709682,29.143616965266,13.2187159054265));
#47681=CARTESIAN_POINT('Ctrl Pts',(56.9833461092831,29.2129924254327,13.2231560815448));
#47682=CARTESIAN_POINT('Ctrl Pts',(56.9758954409461,29.2823716722658,13.2275965000178));
#47683=CARTESIAN_POINT('Ctrl Pts',(56.9648008247325,29.3513521753054,13.2320369184908));
#47684=CARTESIAN_POINT('Ctrl Pts',(56.9501342784475,29.4195281379407,13.2364773369638));
#47685=CARTESIAN_POINT('Ctrl Pts',(56.9354522716568,29.4877759671792,13.240922436233));
#47686=CARTESIAN_POINT('Ctrl Pts',(56.9171909229189,29.5552170843471,13.2453675355023));
#47687=CARTESIAN_POINT('Ctrl Pts',(56.8954730083251,29.6214576712948,13.2498126347716));
#47688=CARTESIAN_POINT('Ctrl Pts',(56.873742329993,29.6877371882009,13.2542603464502));
#47689=CARTESIAN_POINT('Ctrl Pts',(56.8485512189845,29.7528143143941,13.2587080581288));
#47690=CARTESIAN_POINT('Ctrl Pts',(56.8200708197311,29.8163147515899,13.2631557698074));
#47691=CARTESIAN_POINT('Ctrl Pts',(56.7915414473187,29.8799243802681,13.2676111295001));
#47692=CARTESIAN_POINT('Ctrl Pts',(56.7597117201564,29.9419514733999,13.2720664891927));
#47693=CARTESIAN_POINT('Ctrl Pts',(56.7247985790647,30.0020466177561,13.2765218488853));
#47694=CARTESIAN_POINT('Ctrl Pts',(56.7074459917984,30.0319152060329,13.278736259146));
#47695=CARTESIAN_POINT('Ctrl Pts',(56.6893323791755,30.0613069992499,13.2809506694068));
#47696=CARTESIAN_POINT('Ctrl Pts',(56.6704881664024,30.0901820253561,13.2831650796675));
#47697=CARTESIAN_POINT('Ctrl Pts',(56.6325680070147,30.1482871638118,13.2876211315625));
#47698=CARTESIAN_POINT('Ctrl Pts',(56.5915383406987,30.2045252534154,13.2920771834575));
#47699=CARTESIAN_POINT('Ctrl Pts',(56.5476091767831,30.2585441583181,13.2965332353525));
#47700=CARTESIAN_POINT('Ctrl Pts',(56.5037455691235,30.3124824498689,13.3009826374037));
#47701=CARTESIAN_POINT('Ctrl Pts',(56.4569913582548,30.3642077535697,13.305432039455));
#47702=CARTESIAN_POINT('Ctrl Pts',(56.407599966251,30.4133965818235,13.3098814415062));
#47703=CARTESIAN_POINT('Ctrl Pts',(56.3582662261708,30.4625279945953,13.3143256500089));
#47704=CARTESIAN_POINT('Ctrl Pts',(56.3063017637939,30.5091284689646,13.3187698585117));
#47705=CARTESIAN_POINT('Ctrl Pts',(56.2519992527036,30.5529087010284,13.3232140670144));
#47706=CARTESIAN_POINT('Ctrl Pts',(56.1977305832446,30.5966616490046,13.3276555058614));
#47707=CARTESIAN_POINT('Ctrl Pts',(56.141127135589,30.6375975352699,13.3320969447083));
#47708=CARTESIAN_POINT('Ctrl Pts',(56.0825161761122,30.6754659921811,13.3365383835553));
#47709=CARTESIAN_POINT('Ctrl Pts',(56.0239218800946,30.7133236828552,13.3409785596736));
#47710=CARTESIAN_POINT('Ctrl Pts',(55.9633216159151,30.7481154102871,13.3454187357919));
#47711=CARTESIAN_POINT('Ctrl Pts',(55.9010718012957,30.7796339992846,13.3498589119103));
#47712=CARTESIAN_POINT('Ctrl Pts',(55.838818588944,30.8111543086363,13.3542993303832));
#47713=CARTESIAN_POINT('Ctrl Pts',(55.7749160847834,30.839400906139,13.3587397488562));
#47714=CARTESIAN_POINT('Ctrl Pts',(55.7097438877997,30.8642132861427,13.3631801673292));
#47715=CARTESIAN_POINT('Ctrl Pts',(55.6445029905841,30.889051821721,13.3676252665984));
#47716=CARTESIAN_POINT('Ctrl Pts',(55.5779901871625,30.9104487402747,13.3720703658677));
#47717=CARTESIAN_POINT('Ctrl Pts',(55.510602661537,30.9282926345685,13.376515465137));
#47718=CARTESIAN_POINT('Ctrl Pts',(55.443175531891,30.9461470158175,13.3809631768156));
#47719=CARTESIAN_POINT('Ctrl Pts',(55.374873135569,30.9604441163661,13.3854108884943));
#47720=CARTESIAN_POINT('Ctrl Pts',(55.3061026145814,30.9711237281932,13.3898586001729));
#47721=CARTESIAN_POINT('Ctrl Pts',(55.2372138399965,30.9818217040302,13.3943139598655));
#47722=CARTESIAN_POINT('Ctrl Pts',(55.1678558203644,30.9888897254161,13.3987693195581));
#47723=CARTESIAN_POINT('Ctrl Pts',(55.0984397550739,30.9923195469405,13.4032246792507));
#47724=CARTESIAN_POINT('Ctrl Pts',(55.0639384672216,30.9940242425206,13.4054390895115));
#47725=CARTESIAN_POINT('Ctrl Pts',(55.029422824276,30.9948310032179,13.4076534997722));
#47726=CARTESIAN_POINT('Ctrl Pts',(54.9949429193088,30.9947435896463,13.409867910033));
#47727=CARTESIAN_POINT('Ctrl Pts',(54.9255590979858,30.9945676875479,13.414323961928));
#47728=CARTESIAN_POINT('Ctrl Pts',(54.8560485862619,30.9907670296928,13.418780013823));
#47729=CARTESIAN_POINT('Ctrl Pts',(54.7868210938184,30.9833260741641,13.423236065718));
#47730=CARTESIAN_POINT('Ctrl Pts',(54.7176969107666,30.9758962229028,13.4276854677692));
#47731=CARTESIAN_POINT('Ctrl Pts',(54.6488553910336,30.9648369083776,13.4321348698204));
#47732=CARTESIAN_POINT('Ctrl Pts',(54.5807058473582,30.9501846005085,13.4365842718716));
#47733=CARTESIAN_POINT('Ctrl Pts',(54.5126358509912,30.9355493954927,13.4410284803744));
#47734=CARTESIAN_POINT('Ctrl Pts',(54.4452567022659,30.9173296293411,13.4454726888771));
#47735=CARTESIAN_POINT('Ctrl Pts',(54.3789704083292,30.8956133067609,13.4499168973799));
#47736=CARTESIAN_POINT('Ctrl Pts',(54.312725424385,30.8739105179156,13.4543583362268));
#47737=CARTESIAN_POINT('Ctrl Pts',(54.2475724077383,30.8487156475518,13.4587997750738));
#47738=CARTESIAN_POINT('Ctrl Pts',(54.1838995371631,30.8201669146145,13.4632412139207));
#47739=CARTESIAN_POINT('Ctrl Pts',(54.1202447691797,30.791626298259,13.467681390039));
#47740=CARTESIAN_POINT('Ctrl Pts',(54.0580697578255,30.7597339123429,13.4721215661574));
#47741=CARTESIAN_POINT('Ctrl Pts',(53.9977423209735,30.7246759427012,13.4765617422757));
#47742=CARTESIAN_POINT('Ctrl Pts',(53.9374115913163,30.6896160595179,13.4810021607487));
#47743=CARTESIAN_POINT('Ctrl Pts',(53.8789290579547,30.6513904973879,13.4854425792217));
#47744=CARTESIAN_POINT('Ctrl Pts',(53.8226360110713,30.6102302941113,13.4898829976947));
#47745=CARTESIAN_POINT('Ctrl Pts',(53.7662836237708,30.5690267024633,13.4943280969639));
#47746=CARTESIAN_POINT('Ctrl Pts',(53.7121257248894,30.5248825847199,13.4987731962332));
#47747=CARTESIAN_POINT('Ctrl Pts',(53.6604719929179,30.478070458653,13.5032182955025));
#47748=CARTESIAN_POINT('Ctrl Pts',(53.608787903763,30.4312308208413,13.5076660071811));
#47749=CARTESIAN_POINT('Ctrl Pts',(53.5596112555166,30.3817204007798,13.5121137188597));
#47750=CARTESIAN_POINT('Ctrl Pts',(53.5132142006241,30.3298479421626,13.5165614305384));
#47751=CARTESIAN_POINT('Ctrl Pts',(53.4667373641832,30.2778862868264,13.521016790231));
#47752=CARTESIAN_POINT('Ctrl Pts',(53.4230499677281,30.223554866777,13.5254721499236));
#47753=CARTESIAN_POINT('Ctrl Pts',(53.3823827849961,30.167194117627,13.5299275096162));
#47754=CARTESIAN_POINT('Ctrl Pts',(53.3621703144147,30.1391816046469,13.532141919877));
#47755=CARTESIAN_POINT('Ctrl Pts',(53.3427032393411,30.1106682137782,13.5343563301377));
#47756=CARTESIAN_POINT('Ctrl Pts',(53.3240056759864,30.0816980116345,13.5365707403984));
#47757=CARTESIAN_POINT('Ctrl Pts',(53.2855729774195,30.0221499825526,13.5411224437642));
#47758=CARTESIAN_POINT('Ctrl Pts',(53.2502489871136,29.9604451874632,13.54567414713));
#47759=CARTESIAN_POINT('Ctrl Pts',(53.2182765830912,29.8969332350508,13.5502258504958));
#47760=CARTESIAN_POINT('Ctrl Pts',(53.1863531525859,29.8335185666491,13.5547705818203));
#47761=CARTESIAN_POINT('Ctrl Pts',(53.1577713218888,29.768302644132,13.5593153131447));
#47762=CARTESIAN_POINT('Ctrl Pts',(53.1327301960058,29.701663054173,13.5638600444692));
#47763=CARTESIAN_POINT('Ctrl Pts',(53.1077286374661,29.6351287610584,13.568397594689));
#47764=CARTESIAN_POINT('Ctrl Pts',(53.0862568201633,29.5671757024611,13.5729351449088));
#47765=CARTESIAN_POINT('Ctrl Pts',(53.0684666775928,29.4982033590118,13.5774726951287));
#47766=CARTESIAN_POINT('Ctrl Pts',(53.0604577088734,29.4671526049776,13.5795154610947));
#47767=CARTESIAN_POINT('Ctrl Pts',(53.0531942706169,29.4358955521725,13.5815582270607));
#47768=CARTESIAN_POINT('Ctrl Pts',(53.0466869980082,29.4044698737233,13.5836009930267));
#47769=CARTESIAN_POINT('Ctrl Pts',(53.0052508197207,29.0018083902244,12.809862253678));
#47770=CARTESIAN_POINT('Ctrl Pts',(53.0053734539764,29.1370804004845,12.8004754443569));
#47771=CARTESIAN_POINT('Ctrl Pts',(53.019255454431,29.2719942701512,12.7909324149165));
#47772=CARTESIAN_POINT('Ctrl Pts',(53.0466869981368,29.4044698743445,12.7818778464297));
#47773=CARTESIAN_POINT('',(53.0052496133582,28.9993761608918,12.6531293428976));
#47774=CARTESIAN_POINT('Ctrl Pts',(53.0466869618782,29.40446969924,12.6249522205985));
#47775=CARTESIAN_POINT('Ctrl Pts',(53.0420700593701,29.3821732061242,12.6265305192134));
#47776=CARTESIAN_POINT('Ctrl Pts',(53.0378335579175,29.3597910973607,12.6281140142711));
#47777=CARTESIAN_POINT('Ctrl Pts',(53.0148268141735,29.2257048289013,12.6375857831214));
#47778=CARTESIAN_POINT('Ctrl Pts',(53.0052148113952,29.1126451148838,12.6455257903824));
#47779=CARTESIAN_POINT('Ctrl Pts',(53.0052500967933,28.9993785847915,12.6531300191543));
#47780=CARTESIAN_POINT('Ctrl Pts',(53.0052500975323,28.9993762171256,12.6531301781092));
#47781=CARTESIAN_POINT('Ctrl Pts',(53.005258509644,28.9724757367139,12.6549361597253));
#47782=CARTESIAN_POINT('Ctrl Pts',(53.0058110777771,28.9455763451103,12.6567216238253));
#47783=CARTESIAN_POINT('Ctrl Pts',(53.0071539488144,28.9126576596725,12.6588751396755));
#47784=CARTESIAN_POINT('Ctrl Pts',(53.0074276493387,28.9066217491526,12.6592687057323));
#47785=CARTESIAN_POINT('Ctrl Pts',(53.0079488580194,28.8961765363347,12.6599474213631));
#47786=CARTESIAN_POINT('Ctrl Pts',(53.0081835894833,28.8917666799494,12.6602332408541));
#47787=CARTESIAN_POINT('Ctrl Pts',(53.0086619027922,28.8833098917081,12.6607799162569));
#47788=CARTESIAN_POINT('Ctrl Pts',(53.0089031819618,28.8792628435459,12.6610408976375));
#47789=CARTESIAN_POINT('Ctrl Pts',(53.0094096150325,28.8711830188659,12.6615606382477));
#47790=CARTESIAN_POINT('Ctrl Pts',(53.0096746881991,28.8671502756342,12.6618194020265));
#47791=CARTESIAN_POINT('Ctrl Pts',(53.0103328114064,28.8575821816223,12.6624318724954));
#47792=CARTESIAN_POINT('Ctrl Pts',(53.0107367097063,28.8520475752137,12.6627849819217));
#47793=CARTESIAN_POINT('Ctrl Pts',(53.0120197303878,28.8354224180735,12.6638423466634));
#47794=CARTESIAN_POINT('Ctrl Pts',(53.0129685598533,28.824337249783,12.664542917958));
#47795=CARTESIAN_POINT('Ctrl Pts',(53.0170786580199,28.780626063589,12.6672898950697));
#47796=CARTESIAN_POINT('Ctrl Pts',(53.0209513186601,28.7480703284126,12.6693016686706));
#47797=CARTESIAN_POINT('Ctrl Pts',(53.0462820404368,28.5722040552806,12.6800546980204));
#47798=CARTESIAN_POINT('Ctrl Pts',(53.082505936071,28.431451549809,12.6882737896722));
#47799=CARTESIAN_POINT('Ctrl Pts',(53.1666153451381,28.2085192389684,12.7022277418259));
#47800=CARTESIAN_POINT('Ctrl Pts',(53.2056524155551,28.1236126314987,12.7077818172185));
#47801=CARTESIAN_POINT('Ctrl Pts',(53.2613415874518,28.0219380941724,12.7149350482694));
#47802=CARTESIAN_POINT('Ctrl Pts',(53.2725321979323,28.002306111188,12.716340401782));
#47803=CARTESIAN_POINT('Ctrl Pts',(53.2892947868855,27.9740268563558,12.7184022950935));
#47804=CARTESIAN_POINT('Ctrl Pts',(53.294604209995,27.9652254299716,12.7190494100881));
#47805=CARTESIAN_POINT('Ctrl Pts',(53.3040479025908,27.9498407401896,12.7201902466597));
#47806=CARTESIAN_POINT('Ctrl Pts',(53.3081531055625,27.9432398234786,12.7206829029397));
#47807=CARTESIAN_POINT('Ctrl Pts',(53.3162167258366,27.9304414349278,12.7216443796122));
#47808=CARTESIAN_POINT('Ctrl Pts',(53.3201710430309,27.9242415180766,12.7221130437136));
#47809=CARTESIAN_POINT('Ctrl Pts',(53.3308642827153,27.9076784693703,12.7233729533457));
#47810=CARTESIAN_POINT('Ctrl Pts',(53.3376653196701,27.8973560102034,12.7241664895252));
#47811=CARTESIAN_POINT('Ctrl Pts',(53.3631498778221,27.8594478222072,12.727112100226));
#47812=CARTESIAN_POINT('Ctrl Pts',(53.3824268371305,27.8322695364704,12.7292862501438));
#47813=CARTESIAN_POINT('Ctrl Pts',(53.5326205455334,27.6313729350644,12.7458437135092));
#47814=CARTESIAN_POINT('Ctrl Pts',(53.6904841149691,27.4796474602261,12.7613830213825));
#47815=CARTESIAN_POINT('Ctrl Pts',(53.8936803471424,27.3398987856025,12.778164471115));
#47816=CARTESIAN_POINT('Ctrl Pts',(53.9180869401973,27.3238903594304,12.780131195552));
#47817=CARTESIAN_POINT('Ctrl Pts',(53.9536389455595,27.3016718947633,12.782917500711));
#47818=CARTESIAN_POINT('Ctrl Pts',(53.9645053554937,27.2950247306425,12.7837588542112));
#47819=CARTESIAN_POINT('Ctrl Pts',(53.981534268291,27.2848307231675,12.7850605566893));
#47820=CARTESIAN_POINT('Ctrl Pts',(53.9876531183372,27.2812120870877,12.7855249482218));
#47821=CARTESIAN_POINT('Ctrl Pts',(53.9991334821608,27.2745052723796,12.7863898430106));
#47822=CARTESIAN_POINT('Ctrl Pts',(54.0044902533456,27.2714091900203,12.7867908175676));
#47823=CARTESIAN_POINT('Ctrl Pts',(54.0136406767586,27.2661771139352,12.7874712508678));
#47824=CARTESIAN_POINT('Ctrl Pts',(54.0174270501321,27.2640285387459,12.7877515011323));
#47825=CARTESIAN_POINT('Ctrl Pts',(54.0247644428291,27.2598966372955,12.7882920144446));
#47826=CARTESIAN_POINT('Ctrl Pts',(54.0283145220785,27.2579117595308,12.7885523804664));
#47827=CARTESIAN_POINT('Ctrl Pts',(54.0368098159874,27.2531960201805,12.7891727445255));
#47828=CARTESIAN_POINT('Ctrl Pts',(54.0417606419014,27.2504752619845,12.7895321085822));
#47829=CARTESIAN_POINT('Ctrl Pts',(54.0595239779061,27.2408113294044,12.7908139930658));
#47830=CARTESIAN_POINT('Ctrl Pts',(54.0724012935901,27.2339873738655,12.7917293754081));
#47831=CARTESIAN_POINT('Ctrl Pts',(54.2109526135514,27.1624998425249,12.8014428298402));
#47832=CARTESIAN_POINT('Ctrl Pts',(54.3431035534356,27.1112169097634,12.809542835432));
#47833=CARTESIAN_POINT('Ctrl Pts',(54.6091972642971,27.0393042639946,12.825562867554));
#47834=CARTESIAN_POINT('Ctrl Pts',(54.7419984089862,27.0174554376566,12.8334384882912));
#47835=CARTESIAN_POINT('Ctrl Pts',(54.8933239499874,27.0080286570439,12.8428492364542));
#47836=CARTESIAN_POINT('Ctrl Pts',(54.9106827996876,27.0071748649683,12.8439346452484));
#47837=CARTESIAN_POINT('Ctrl Pts',(54.9373017051486,27.0062141066126,12.8456089950573));
#47838=CARTESIAN_POINT('Ctrl Pts',(54.9465553220098,27.0059446029238,12.8461928904665));
#47839=CARTESIAN_POINT('Ctrl Pts',(54.9627318041459,27.0055861577793,12.8472169549449));
#47840=CARTESIAN_POINT('Ctrl Pts',(54.9696539316157,27.0054688253542,12.8476562345475));
#47841=CARTESIAN_POINT('Ctrl Pts',(54.9853022799942,27.0052850604732,12.8486517628217));
#47842=CARTESIAN_POINT('Ctrl Pts',(54.9940285630985,27.0052398512805,12.8492086619283));
#47843=CARTESIAN_POINT('Ctrl Pts',(55.0176607716491,27.0052724873913,12.8507216949258));
#47844=CARTESIAN_POINT('Ctrl Pts',(55.0325657496042,27.0054601521964,12.8516812127403));
#47845=CARTESIAN_POINT('Ctrl Pts',(55.1025835820192,27.0071267623856,12.856214204079));
#47846=CARTESIAN_POINT('Ctrl Pts',(55.1576172690809,27.010723006665,12.8598524806449));
#47847=CARTESIAN_POINT('Ctrl Pts',(55.391093871695,27.0357288709439,12.8756180582932));
#47848=CARTESIAN_POINT('Ctrl Pts',(55.566348323001,27.0789199314493,12.8883765795719));
#47849=CARTESIAN_POINT('Ctrl Pts',(55.7832258921363,27.1646650176396,12.9043494143566));
#47850=CARTESIAN_POINT('Ctrl Pts',(55.8322349945113,27.1863618540079,12.9079636054641));
#47851=CARTESIAN_POINT('Ctrl Pts',(55.8887757539769,27.2141685095905,12.9120919796301));
#47852=CARTESIAN_POINT('Ctrl Pts',(55.8972067387195,27.2183893440583,12.9127064544593));
#47853=CARTESIAN_POINT('Ctrl Pts',(55.9101533827926,27.2249860816154,12.9136479498189));
#47854=CARTESIAN_POINT('Ctrl Pts',(55.9146902485402,27.2273197295348,12.9139774767896));
#47855=CARTESIAN_POINT('Ctrl Pts',(55.9230376726558,27.2316540103501,12.9145829700766));
#47856=CARTESIAN_POINT('Ctrl Pts',(55.9268506933373,27.2336495599271,12.9148592340194));
#47857=CARTESIAN_POINT('Ctrl Pts',(55.935458577342,27.2381900561372,12.9154821982093));
#47858=CARTESIAN_POINT('Ctrl Pts',(55.9402495222327,27.2407422400837,12.9158284399616));
#47859=CARTESIAN_POINT('Ctrl Pts',(55.954411980335,27.2483611022329,12.9168506984003));
#47860=CARTESIAN_POINT('Ctrl Pts',(55.9637535634786,27.2534834277916,12.9175233365335));
#47861=CARTESIAN_POINT('Ctrl Pts',(56.054349375983,27.3041086046727,12.9240349945454));
#47862=CARTESIAN_POINT('Ctrl Pts',(56.1323752267257,27.355180490015,12.9295537695112));
#47863=CARTESIAN_POINT('Ctrl Pts',(56.2944189346148,27.4782637066949,12.9414463241599));
#47864=CARTESIAN_POINT('Ctrl Pts',(56.3765925310782,27.5521759292839,12.9477758710708));
#47865=CARTESIAN_POINT('Ctrl Pts',(56.4888459720409,27.6713851064656,12.9574575690478));
#47866=CARTESIAN_POINT('Ctrl Pts',(56.5238804198786,27.7117190892901,12.9606546419061));
#47867=CARTESIAN_POINT('Ctrl Pts',(56.5717503339568,27.7715185701758,12.965327575746));
#47868=CARTESIAN_POINT('Ctrl Pts',(56.5859304580374,27.7898800669154,12.9667537405785));
#47869=CARTESIAN_POINT('Ctrl Pts',(56.6107108074562,27.8231513605512,12.9693258810721));
#47870=CARTESIAN_POINT('Ctrl Pts',(56.621432380324,27.8379677169106,12.9704671510169));
#47871=CARTESIAN_POINT('Ctrl Pts',(56.6373801969232,27.8606568225585,12.9722096803928));
#47872=CARTESIAN_POINT('Ctrl Pts',(56.6427569098827,27.8684229962685,12.9728052231761));
#47873=CARTESIAN_POINT('Ctrl Pts',(56.6524045956514,27.8825718856845,12.9738887424962));
#47874=CARTESIAN_POINT('Ctrl Pts',(56.6566942758634,27.8889416702826,12.9743760033577));
#47875=CARTESIAN_POINT('Ctrl Pts',(56.6658470247894,27.9027035299753,12.9754276608575));
#47876=CARTESIAN_POINT('Ctrl Pts',(56.6706978898526,27.91010348664,12.9759924984914));
#47877=CARTESIAN_POINT('Ctrl Pts',(56.6836740925846,27.9301887791068,12.9775239866285));
#47878=CARTESIAN_POINT('Ctrl Pts',(56.6917050952847,27.942934085098,12.9784940807524));
#47879=CARTESIAN_POINT('Ctrl Pts',(56.730807861266,28.0065777533603,12.9833307541744));
#47880=CARTESIAN_POINT('Ctrl Pts',(56.759727867836,28.058756025133,12.9872739281187));
#47881=CARTESIAN_POINT('Ctrl Pts',(56.8466202679737,28.2335742339024,13.0004206178233));
#47882=CARTESIAN_POINT('Ctrl Pts',(56.8944306704516,28.3608290766274,13.009919336971));
#47883=CARTESIAN_POINT('Ctrl Pts',(56.95003357156,28.5719329934062,13.025091233151));
#47884=CARTESIAN_POINT('Ctrl Pts',(56.9661105339601,28.6531794661694,13.0307895191124));
#47885=CARTESIAN_POINT('Ctrl Pts',(56.9791976622831,28.7508917520852,13.0373158786409));
#47886=CARTESIAN_POINT('Ctrl Pts',(56.9811128620717,28.7666115451036,13.0383557647059));
#47887=CARTESIAN_POINT('Ctrl Pts',(56.9835265916393,28.788601476027,13.0397948615663));
#47888=CARTESIAN_POINT('Ctrl Pts',(56.9841829229186,28.7948532070713,13.0402022425832));
#47889=CARTESIAN_POINT('Ctrl Pts',(56.9852505327707,28.8055072443768,13.0408933858884));
#47890=CARTESIAN_POINT('Ctrl Pts',(56.9856767446721,28.8099079776097,13.0411779660155));
#47891=CARTESIAN_POINT('Ctrl Pts',(56.9864693445362,28.8183854125024,13.041724393136));
#47892=CARTESIAN_POINT('Ctrl Pts',(56.9868378195759,28.8224618502742,13.0419863598279));
#47893=CARTESIAN_POINT('Ctrl Pts',(56.9876934405249,28.8322639896143,13.0426144517984));
#47894=CARTESIAN_POINT('Ctrl Pts',(56.9881684008509,28.8379907580309,13.0429799068639));
#47895=CARTESIAN_POINT('Ctrl Pts',(56.9898151031853,28.8589445216109,13.0443118553914));
#47896=CARTESIAN_POINT('Ctrl Pts',(56.9908367509594,28.8741832405085,13.0452704435188));
#47897=CARTESIAN_POINT('Ctrl Pts',(56.9990238046862,29.0216592298222,13.0544629434021));
#47898=CARTESIAN_POINT('Ctrl Pts',(56.993179481434,29.1543077908929,13.0620895835918));
#47899=CARTESIAN_POINT('Ctrl Pts',(56.9539738731566,29.4254964389924,13.078003732705));
#47900=CARTESIAN_POINT('Ctrl Pts',(56.9188740128804,29.563006623236,13.0862714786937));
#47901=CARTESIAN_POINT('Ctrl Pts',(56.8633221346202,29.7123021543208,13.0961539328045));
#47902=CARTESIAN_POINT('Ctrl Pts',(56.8568988089205,29.7288830619931,13.0972640425058));
#47903=CARTESIAN_POINT('Ctrl Pts',(56.8467642940753,29.7540400944956,13.0989685654779));
#47904=CARTESIAN_POINT('Ctrl Pts',(56.8432129795499,29.7626799651483,13.0995576412356));
#47905=CARTESIAN_POINT('Ctrl Pts',(56.8369211555333,29.7776864865177,13.1005873661059));
#47906=CARTESIAN_POINT('Ctrl Pts',(56.8342078830856,29.7840644377953,13.1010270920073));
#47907=CARTESIAN_POINT('Ctrl Pts',(56.8280277934161,29.7983840155855,13.1020191073718));
#47908=CARTESIAN_POINT('Ctrl Pts',(56.8245423738731,29.8063174138656,13.1025720199074));
#47909=CARTESIAN_POINT('Ctrl Pts',(56.8150347676198,29.827581000764,13.1040630300306));
#47910=CARTESIAN_POINT('Ctrl Pts',(56.8089175558138,29.8408678718873,13.1050043453805));
#47911=CARTESIAN_POINT('Ctrl Pts',(56.7801801493911,29.9015217495957,13.1093466980461));
#47912=CARTESIAN_POINT('Ctrl Pts',(56.7558437163744,29.9480479051199,13.1128061941598));
#47913=CARTESIAN_POINT('Ctrl Pts',(56.638753371119,30.1518927778984,13.128560038587));
#47914=CARTESIAN_POINT('Ctrl Pts',(56.5264955286858,30.2969822525403,13.1415268472822));
#47915=CARTESIAN_POINT('Ctrl Pts',(56.3702829227037,30.4500551217581,13.1565085240204));
#47916=CARTESIAN_POINT('Ctrl Pts',(56.3437703476986,30.4746581664952,13.1589607422659));
#47917=CARTESIAN_POINT('Ctrl Pts',(56.3000957447577,30.5130305330613,13.1628393331244));
#47918=CARTESIAN_POINT('Ctrl Pts',(56.2833501191642,30.5272599343804,13.1642903520899));
#47919=CARTESIAN_POINT('Ctrl Pts',(56.2608617180058,30.5457380609807,13.1661880040148));
#47920=CARTESIAN_POINT('Ctrl Pts',(56.2553271069651,30.5502362024321,13.1666510345344));
#47921=CARTESIAN_POINT('Ctrl Pts',(56.2461853697867,30.5575848999437,13.1674091235518));
#47922=CARTESIAN_POINT('Ctrl Pts',(56.242592359016,30.5604527954277,13.1677053884831));
#47923=CARTESIAN_POINT('Ctrl Pts',(56.235533522762,30.5660472284429,13.1682840760909));
#47924=CARTESIAN_POINT('Ctrl Pts',(56.2320685283388,30.5687747287695,13.1685665637616));
#47925=CARTESIAN_POINT('Ctrl Pts',(56.2235091673775,30.5754664536779,13.1692605834954));
#47926=CARTESIAN_POINT('Ctrl Pts',(56.2184044923577,30.5794175271527,13.1696711977433));
#47927=CARTESIAN_POINT('Ctrl Pts',(56.2007786930571,30.5929237794877,13.1710780737985));
#47928=CARTESIAN_POINT('Ctrl Pts',(56.1881632600141,30.6023556848185,13.172066193636));
#47929=CARTESIAN_POINT('Ctrl Pts',(56.0758778956707,30.6842502598361,13.1807093355327));
#47930=CARTESIAN_POINT('Ctrl Pts',(55.9697900866757,30.7474918441199,13.1878423757985));
#47931=CARTESIAN_POINT('Ctrl Pts',(55.7655791709926,30.844863256513,13.2009794451731));
#47932=CARTESIAN_POINT('Ctrl Pts',(55.6693393437374,30.8819178322031,13.2069567120401));
#47933=CARTESIAN_POINT('Ctrl Pts',(55.5368054123103,30.9214882141226,13.2152711386408));
#47934=CARTESIAN_POINT('Ctrl Pts',(55.5026740937519,30.9306982029106,13.2174183599116));
#47935=CARTESIAN_POINT('Ctrl Pts',(55.4436063777527,30.9449645767648,13.2211570884229));
#47936=CARTESIAN_POINT('Ctrl Pts',(55.4187843442119,30.9504597934128,13.2227349734993));
#47937=CARTESIAN_POINT('Ctrl Pts',(55.3833038700587,30.9576061315152,13.2250029049775));
#47938=CARTESIAN_POINT('Ctrl Pts',(55.3727259374319,30.9596476701852,13.2256806177267));
#47939=CARTESIAN_POINT('Ctrl Pts',(55.3544081283186,30.9630293260337,13.2268571351839));
#47940=CARTESIAN_POINT('Ctrl Pts',(55.346675843672,30.964409609232,13.2273546615312));
#47941=CARTESIAN_POINT('Ctrl Pts',(55.3318163495819,30.9669716989779,13.2283125837807));
#47942=CARTESIAN_POINT('Ctrl Pts',(55.3246904637155,30.9681605257084,13.2287727498787));
#47943=CARTESIAN_POINT('Ctrl Pts',(55.3078884230617,30.9708699146411,13.2298597078878));
#47944=CARTESIAN_POINT('Ctrl Pts',(55.2982072844609,30.9723579572064,13.2304875116423));
#47945=CARTESIAN_POINT('Ctrl Pts',(55.2644349807819,30.9772946102586,13.2326830646434));
#47946=CARTESIAN_POINT('Ctrl Pts',(55.2402927672055,30.9803734835933,13.2342622963263));
#47947=CARTESIAN_POINT('Ctrl Pts',(55.0855628378242,30.9972353825786,13.2444499901521));
#47948=CARTESIAN_POINT('Ctrl Pts',(54.9539612599652,30.9985343547,13.2534475445453));
#47949=CARTESIAN_POINT('Ctrl Pts',(54.7233996596851,30.9780193477641,13.2695567074557));
#47950=CARTESIAN_POINT('Ctrl Pts',(54.624398071639,30.9616302087489,13.2765791256516));
#47951=CARTESIAN_POINT('Ctrl Pts',(54.4998630576276,30.9312362421884,13.2852907805544));
#47952=CARTESIAN_POINT('Ctrl Pts',(54.4728230626734,30.9240309306456,13.2871741358083));
#47953=CARTESIAN_POINT('Ctrl Pts',(54.428425701111,30.9111940939926,13.2902434533576));
#47954=CARTESIAN_POINT('Ctrl Pts',(54.4109786290441,30.9058892740607,13.2914436637295));
#47955=CARTESIAN_POINT('Ctrl Pts',(54.3872762970908,30.8983259392221,13.2930637527363));
#47956=CARTESIAN_POINT('Ctrl Pts',(54.380956583815,30.8962744947742,13.2934946945814));
#47957=CARTESIAN_POINT('Ctrl Pts',(54.3703812385538,30.8927831251972,13.294213978301));
#47958=CARTESIAN_POINT('Ctrl Pts',(54.3661200539562,30.8913603461469,13.2945032979451));
#47959=CARTESIAN_POINT('Ctrl Pts',(54.3580545723318,30.8886370200833,13.2950499089708));
#47960=CARTESIAN_POINT('Ctrl Pts',(54.3542493509525,30.8873393509604,13.2953073704552));
#47961=CARTESIAN_POINT('Ctrl Pts',(54.3442946947251,30.8839109506206,13.2959798537793));
#47962=CARTESIAN_POINT('Ctrl Pts',(54.3381516571582,30.8817615925326,13.2963937935686));
#47963=CARTESIAN_POINT('Ctrl Pts',(54.3168780481539,30.8742012082629,13.2978239928542));
#47964=CARTESIAN_POINT('Ctrl Pts',(54.3018019589459,30.8686372852733,13.2988317452235));
#47965=CARTESIAN_POINT('Ctrl Pts',(54.1860727634522,30.8243305020476,13.3065347285346));
#47966=CARTESIAN_POINT('Ctrl Pts',(54.0886308192715,30.7776590132154,13.3128333253503));
#47967=CARTESIAN_POINT('Ctrl Pts',(53.8979549179244,30.666509646274,13.3256631051083));
#47968=CARTESIAN_POINT('Ctrl Pts',(53.8054813490004,30.6015246241497,13.3321739387852));
#47969=CARTESIAN_POINT('Ctrl Pts',(53.6897006446243,30.5045278471628,13.3412259813916));
#47970=CARTESIAN_POINT('Ctrl Pts',(53.6611149841582,30.4791467457248,13.3435419171897));
#47971=CARTESIAN_POINT('Ctrl Pts',(53.6136199231396,30.4344706888291,13.3475476030747));
#47972=CARTESIAN_POINT('Ctrl Pts',(53.5943406426183,30.4155838151899,13.3492208891125));
#47973=CARTESIAN_POINT('Ctrl Pts',(53.5677297540622,30.388434795049,13.3516019358723));
#47974=CARTESIAN_POINT('Ctrl Pts',(53.5600739781826,30.3804934919873,13.352295586868));
#47975=CARTESIAN_POINT('Ctrl Pts',(53.5470480865,30.3667555487657,13.353490986667));
#47976=CARTESIAN_POINT('Ctrl Pts',(53.5416457713439,30.3609896891154,13.353991343401));
#47977=CARTESIAN_POINT('Ctrl Pts',(53.5314056771144,30.3499295200854,13.3549486475392));
#47978=CARTESIAN_POINT('Ctrl Pts',(53.5265619050445,30.3446409084019,13.3554053302285));
#47979=CARTESIAN_POINT('Ctrl Pts',(53.5141061253413,30.3308931044141,13.356589806811));
#47980=CARTESIAN_POINT('Ctrl Pts',(53.5065378815352,30.3223947799361,13.3573194112538));
#47981=CARTESIAN_POINT('Ctrl Pts',(53.4851177927023,30.2979238985391,13.3594132423356));
#47982=CARTESIAN_POINT('Ctrl Pts',(53.4714469490872,30.2817956398368,13.3607847949351));
#47983=CARTESIAN_POINT('Ctrl Pts',(53.3550465780414,30.1399609332491,13.3727778801633));
#47984=CARTESIAN_POINT('Ctrl Pts',(53.2677810735677,30.0023872863944,13.384025521532));
#47985=CARTESIAN_POINT('Ctrl Pts',(53.1649050598222,29.7857873114781,13.4007345969455));
#47986=CARTESIAN_POINT('Ctrl Pts',(53.1357586664016,29.7138913589845,13.4061221151343));
#47987=CARTESIAN_POINT('Ctrl Pts',(53.103096413825,29.6175519029457,13.4130046660651));
#47988=CARTESIAN_POINT('Ctrl Pts',(53.0957414126947,29.5944854164993,13.4146277919164));
#47989=CARTESIAN_POINT('Ctrl Pts',(53.0841203307741,29.5556082578695,13.4173159677041));
#47990=CARTESIAN_POINT('Ctrl Pts',(53.0796258550381,29.5398690839979,13.4183913715069));
#47991=CARTESIAN_POINT('Ctrl Pts',(53.0736521685307,29.5179306490023,13.419870833062));
#47992=CARTESIAN_POINT('Ctrl Pts',(53.072008303696,29.5117774385784,13.4202836667103));
#47993=CARTESIAN_POINT('Ctrl Pts',(53.0692692431778,29.5013242407116,13.4209812808956));
#47994=CARTESIAN_POINT('Ctrl Pts',(53.0681588808038,29.4970283103165,13.4212669159244));
#47995=CARTESIAN_POINT('Ctrl Pts',(53.0660565420174,29.4887809941834,13.4218131973759));
#47996=CARTESIAN_POINT('Ctrl Pts',(53.06506232812,29.4848302441166,13.4220739757925));
#47997=CARTESIAN_POINT('Ctrl Pts',(53.0627123030393,29.4753694767777,13.4226963422761));
#47998=CARTESIAN_POINT('Ctrl Pts',(53.0613678764538,29.4698566288474,13.4230572870091));
#47999=CARTESIAN_POINT('Ctrl Pts',(53.0566159294787,29.4500035193902,13.4243512311863));
#48000=CARTESIAN_POINT('Ctrl Pts',(53.0533437522474,29.4356309171549,13.4252769140447));
#48001=CARTESIAN_POINT('Ctrl Pts',(53.0490256293916,29.4156430622009,13.4265506113638));
#48002=CARTESIAN_POINT('Ctrl Pts',(53.0478442633022,29.4100586740838,13.4269049972294));
#48003=CARTESIAN_POINT('Ctrl Pts',(53.04668699692,29.404469868468,13.4272582639285));
#48004=CARTESIAN_POINT('Origin',(55.,29.,3.45145488139523));
#48005=CARTESIAN_POINT('',(53.0466870452705,29.4044701019679,14.3843322575863));
#48006=CARTESIAN_POINT('',(53.0466869970967,29.4044698693216,14.2242573078582));
#48007=CARTESIAN_POINT('',(53.0466869980082,29.4044698737233,3.45145488139523));
#48008=CARTESIAN_POINT('',(53.0052501563995,28.9992103260818,13.6096063772323));
#48009=CARTESIAN_POINT('Ctrl Pts',(53.0466870452705,29.4044701019679,14.3843322575863));
#48010=CARTESIAN_POINT('Ctrl Pts',(53.0651942708541,29.4938472977425,14.3789669817368));
#48011=CARTESIAN_POINT('Ctrl Pts',(53.089821908192,29.5818877886488,14.3735004590224));
#48012=CARTESIAN_POINT('Ctrl Pts',(53.1256881001794,29.6828107362223,14.3668534278733));
#48013=CARTESIAN_POINT('Ctrl Pts',(53.1311373838443,29.6975873416164,14.3658705425979));
#48014=CARTESIAN_POINT('Ctrl Pts',(53.1402787406042,29.7214994452985,14.3642634905551));
#48015=CARTESIAN_POINT('Ctrl Pts',(53.1438645997717,29.7306750185046,14.3636428411623));
#48016=CARTESIAN_POINT('Ctrl Pts',(53.1503800876598,29.7469894802121,14.3625320028294));
#48017=CARTESIAN_POINT('Ctrl Pts',(53.1532834702555,29.7541386873287,14.3620426990456));
#48018=CARTESIAN_POINT('Ctrl Pts',(53.1595037545394,29.769204002796,14.3610061832558));
#48019=CARTESIAN_POINT('Ctrl Pts',(53.1628304062841,29.7771158907305,14.3604586512175));
#48020=CARTESIAN_POINT('Ctrl Pts',(53.1718166940001,29.7981080659995,14.3589972964518));
#48021=CARTESIAN_POINT('Ctrl Pts',(53.1775655484712,29.811149393054,14.3580804741788));
#48022=CARTESIAN_POINT('Ctrl Pts',(53.2061400163677,29.8741333785546,14.3536080789534));
#48023=CARTESIAN_POINT('Ctrl Pts',(53.2308796009079,29.923176502266,14.3499877399848));
#48024=CARTESIAN_POINT('Ctrl Pts',(53.3579669551592,30.1511945817571,14.332476096662));
#48025=CARTESIAN_POINT('Ctrl Pts',(53.4856042391137,30.314573690023,14.3177007073119));
#48026=CARTESIAN_POINT('Ctrl Pts',(53.6583134307999,30.4764287406221,14.3017586179392));
#48027=CARTESIAN_POINT('Ctrl Pts',(53.6811305092218,30.4968460794232,14.2997221901765));
#48028=CARTESIAN_POINT('Ctrl Pts',(53.7107698363668,30.5221639560008,14.297173626867));
#48029=CARTESIAN_POINT('Ctrl Pts',(53.717163959834,30.5275566188298,14.2966293847403));
#48030=CARTESIAN_POINT('Ctrl Pts',(53.7273345525257,30.5360253709058,14.2957727179552));
#48031=CARTESIAN_POINT('Ctrl Pts',(53.7310886056742,30.5391280505007,14.2954584358674));
#48032=CARTESIAN_POINT('Ctrl Pts',(53.738208769231,30.5449690224707,14.2948660328008));
#48033=CARTESIAN_POINT('Ctrl Pts',(53.741572414137,30.5477100509863,14.2945877242164));
#48034=CARTESIAN_POINT('Ctrl Pts',(53.7494405794122,30.5540791969193,14.2939402678272));
#48035=CARTESIAN_POINT('Ctrl Pts',(53.7539519628697,30.5576987211543,14.2935717310558));
#48036=CARTESIAN_POINT('Ctrl Pts',(53.7685545380172,30.5693104666846,14.2923872734525));
#48037=CARTESIAN_POINT('Ctrl Pts',(53.7787076100021,30.5772248365823,14.2915766322095));
#48038=CARTESIAN_POINT('Ctrl Pts',(53.8029823476145,30.5957721463632,14.2896669795025));
#48039=CARTESIAN_POINT('Ctrl Pts',(53.8171703356499,30.6063169157242,14.288573298804));
#48040=CARTESIAN_POINT('Ctrl Pts',(53.8696930583156,30.6442794398413,14.2845985610984));
#48041=CARTESIAN_POINT('Ctrl Pts',(53.9088580425179,30.6705264095227,14.2817765646807));
#48042=CARTESIAN_POINT('Ctrl Pts',(54.0859502996677,30.7803190623223,14.2694604641199));
#48043=CARTESIAN_POINT('Ctrl Pts',(54.2327738565179,30.8483477444895,14.2603476341313));
#48044=CARTESIAN_POINT('Ctrl Pts',(54.4400526960422,30.9153828242194,14.2472893587488));
#48045=CARTESIAN_POINT('Ctrl Pts',(54.4946295599682,30.9305004995872,14.2438403196924));
#48046=CARTESIAN_POINT('Ctrl Pts',(54.5642270961294,30.9466252096432,14.2393927256583));
#48047=CARTESIAN_POINT('Ctrl Pts',(54.5787188679156,30.9498127909308,14.2384640493554));
#48048=CARTESIAN_POINT('Ctrl Pts',(54.6018560005165,30.9546320094794,14.2369766658718));
#48049=CARTESIAN_POINT('Ctrl Pts',(54.6104791058872,30.9563686784118,14.2364212942788));
#48050=CARTESIAN_POINT('Ctrl Pts',(54.6266562736075,30.9595155201606,14.2353773536211));
#48051=CARTESIAN_POINT('Ctrl Pts',(54.6342075693632,30.9609391899764,14.2348892218689));
#48052=CARTESIAN_POINT('Ctrl Pts',(54.6511280164718,30.9640281194881,14.2337934991875));
#48053=CARTESIAN_POINT('Ctrl Pts',(54.6605011880695,30.9656700299328,14.2331851834562));
#48054=CARTESIAN_POINT('Ctrl Pts',(54.6882609692822,30.9703282723082,14.2313794558799));
#48055=CARTESIAN_POINT('Ctrl Pts',(54.70667808594,30.9731540588176,14.2301761004223));
#48056=CARTESIAN_POINT('Ctrl Pts',(54.8539410364848,30.9936417322771,14.220508702191));
#48057=CARTESIAN_POINT('Ctrl Pts',(54.9841705405366,30.9989193876083,14.2116517668491));
#48058=CARTESIAN_POINT('Ctrl Pts',(55.2573569930519,30.9832860576243,14.1926440728428));
#48059=CARTESIAN_POINT('Ctrl Pts',(55.3994516440834,30.9596173436848,14.1825093673263));
#48060=CARTESIAN_POINT('Ctrl Pts',(55.5517191505958,30.9169880287433,14.1720568930949));
#48061=CARTESIAN_POINT('Ctrl Pts',(55.5656169527115,30.9129335103937,14.1711070739291));
#48062=CARTESIAN_POINT('Ctrl Pts',(55.5848606013737,30.9070913397125,14.169798921699));
#48063=CARTESIAN_POINT('Ctrl Pts',(55.5902444712192,30.9054319109035,14.1694337027521));
#48064=CARTESIAN_POINT('Ctrl Pts',(55.5994991604183,30.9025364198383,14.168807313624));
#48065=CARTESIAN_POINT('Ctrl Pts',(55.6033733308077,30.9013113097393,14.1685455230875));
#48066=CARTESIAN_POINT('Ctrl Pts',(55.6114793866004,30.8987206995965,14.1679987041204));
#48067=CARTESIAN_POINT('Ctrl Pts',(55.6157104849498,30.8973528756005,14.1677138212604));
#48068=CARTESIAN_POINT('Ctrl Pts',(55.6260373096143,30.8939762516493,14.1670197493159));
#48069=CARTESIAN_POINT('Ctrl Pts',(55.6321280509547,30.8919521359551,14.1666114449781));
#48070=CARTESIAN_POINT('Ctrl Pts',(55.654021322371,30.884558891136,14.1651472453134));
#48071=CARTESIAN_POINT('Ctrl Pts',(55.6697666015426,30.8790207147876,14.164100719619));
#48072=CARTESIAN_POINT('Ctrl Pts',(55.7087729369854,30.8647481716934,14.1615200318356));
#48073=CARTESIAN_POINT('Ctrl Pts',(55.7319443247293,30.8557754283044,14.15999763892));
#48074=CARTESIAN_POINT('Ctrl Pts',(55.8299279452719,30.8157119594405,14.1535813619349));
#48075=CARTESIAN_POINT('Ctrl Pts',(55.9029815175782,30.7805102437794,14.1488492733601));
#48076=CARTESIAN_POINT('Ctrl Pts',(56.1108091448868,30.6642749660863,14.1350039842979));
#48077=CARTESIAN_POINT('Ctrl Pts',(56.2383666573575,30.5716711063742,14.125953151526));
#48078=CARTESIAN_POINT('Ctrl Pts',(56.3712962370987,30.4488429112459,14.1148004757563));
#48079=CARTESIAN_POINT('Ctrl Pts',(56.3885619678539,30.4323039960369,14.1133149742629));
#48080=CARTESIAN_POINT('Ctrl Pts',(56.4122406139927,30.4087915245124,14.1112229612347));
#48081=CARTESIAN_POINT('Ctrl Pts',(56.4189078774842,30.4020761540111,14.1106276554891));
#48082=CARTESIAN_POINT('Ctrl Pts',(56.4310237459086,30.3896979354768,14.1095341736236));
#48083=CARTESIAN_POINT('Ctrl Pts',(56.4364871788882,30.3840498167529,14.1090366547162));
#48084=CARTESIAN_POINT('Ctrl Pts',(56.4474848064315,30.372545162153,14.1080260519428));
#48085=CARTESIAN_POINT('Ctrl Pts',(56.4530171694596,30.3666870853055,14.1075129032463));
#48086=CARTESIAN_POINT('Ctrl Pts',(56.4665795690965,30.3521507761058,14.1062430040035));
#48087=CARTESIAN_POINT('Ctrl Pts',(56.4745681483055,30.3434344494269,14.1054845206256));
#48088=CARTESIAN_POINT('Ctrl Pts',(56.5040737073018,30.3106607382167,14.1026432068695));
#48089=CARTESIAN_POINT('Ctrl Pts',(56.5250823153939,30.2861543525517,14.1005395553245));
#48090=CARTESIAN_POINT('Ctrl Pts',(56.5761712050679,30.2235470815933,14.0952134833179));
#48091=CARTESIAN_POINT('Ctrl Pts',(56.6054713863942,30.184839286137,14.0919628863608));
#48092=CARTESIAN_POINT('Ctrl Pts',(56.6909706981619,30.0628865969941,14.0818539904205));
#48093=CARTESIAN_POINT('Ctrl Pts',(56.7423178351698,29.9764401368831,14.0748600572816));
#48094=CARTESIAN_POINT('Ctrl Pts',(56.8326119972608,29.7944332696938,14.0607016244154));
#48095=CARTESIAN_POINT('Ctrl Pts',(56.8711091598477,29.698960423908,14.0535589849105));
#48096=CARTESIAN_POINT('Ctrl Pts',(56.9069235399736,29.5856012709779,14.0456828312359));
#48097=CARTESIAN_POINT('Ctrl Pts',(56.9115833245341,29.5702065138135,14.0446258691389));
#48098=CARTESIAN_POINT('Ctrl Pts',(56.9178671854335,29.5485028785489,14.0431550855166));
#48099=CARTESIAN_POINT('Ctrl Pts',(56.9196472053074,29.5422403145689,14.0427329388972));
#48100=CARTESIAN_POINT('Ctrl Pts',(56.9224769082443,29.5320961065047,14.0420528931355));
#48101=CARTESIAN_POINT('Ctrl Pts',(56.9235455541656,29.5282198699761,14.0417939226578));
#48102=CARTESIAN_POINT('Ctrl Pts',(56.9257832120055,29.5200064995344,14.0412470983112));
#48103=CARTESIAN_POINT('Ctrl Pts',(56.9269493089306,29.5156685958802,14.0409594185336));
#48104=CARTESIAN_POINT('Ctrl Pts',(56.9298032364856,29.5049070625014,14.0402484436156));
#48105=CARTESIAN_POINT('Ctrl Pts',(56.9314736750158,29.4984788049915,14.0398261360066));
#48106=CARTESIAN_POINT('Ctrl Pts',(56.9376052688793,29.4743892912769,14.0382520609044));
#48107=CARTESIAN_POINT('Ctrl Pts',(56.9418567036914,29.4566749117992,14.0371116100608));
#48108=CARTESIAN_POINT('Ctrl Pts',(56.9520129039967,29.4116477696508,14.0342500877002));
#48109=CARTESIAN_POINT('Ctrl Pts',(56.957587712514,29.3842639307407,14.0325443456957));
#48110=CARTESIAN_POINT('Ctrl Pts',(56.9804611718324,29.2584376636158,14.0248269580536));
#48111=CARTESIAN_POINT('Ctrl Pts',(56.9909225705665,29.1588925964334,14.019051067913));
#48112=CARTESIAN_POINT('Ctrl Pts',(56.9977696671333,28.9274055886509,14.0056013002485));
#48113=CARTESIAN_POINT('Ctrl Pts',(56.9886291764605,28.7957891929518,13.9979230552837));
#48114=CARTESIAN_POINT('Ctrl Pts',(56.9625220767595,28.6420521826928,13.9883231958293));
#48115=CARTESIAN_POINT('Ctrl Pts',(56.958010266346,28.618142357595,13.986812694045));
#48116=CARTESIAN_POINT('Ctrl Pts',(56.9510706069042,28.5847326540622,13.9846749048522));
#48117=CARTESIAN_POINT('Ctrl Pts',(56.9490082401293,28.5751584340065,13.9840591369458));
#48118=CARTESIAN_POINT('Ctrl Pts',(56.9453022650103,28.5585491549572,13.9829852732039));
#48119=CARTESIAN_POINT('Ctrl Pts',(56.9436907758777,28.5515070609331,13.9825282034758));
#48120=CARTESIAN_POINT('Ctrl Pts',(56.9402473566488,28.536826755339,13.9815716081935));
#48121=CARTESIAN_POINT('Ctrl Pts',(56.9384084954687,28.5291903130069,13.9810718687408));
#48122=CARTESIAN_POINT('Ctrl Pts',(56.9339404194312,28.5111052241157,13.9798831912338));
#48123=CARTESIAN_POINT('Ctrl Pts',(56.9312715777554,28.5006667112456,13.9791929961317));
#48124=CARTESIAN_POINT('Ctrl Pts',(56.9220201957624,28.465666265351,13.9768646592819));
#48125=CARTESIAN_POINT('Ctrl Pts',(56.9150528139011,28.4412095254745,13.9752142498988));
#48126=CARTESIAN_POINT('Ctrl Pts',(56.8972836167096,28.3830779824912,13.9712332257385));
#48127=CARTESIAN_POINT('Ctrl Pts',(56.8860503800644,28.3495450753956,13.9688893963111));
#48128=CARTESIAN_POINT('Ctrl Pts',(56.8386151878298,28.2195256923073,13.9596138727579));
#48129=CARTESIAN_POINT('Ctrl Pts',(56.7958536810452,28.1256138335141,13.9524923847739));
#48130=CARTESIAN_POINT('Ctrl Pts',(56.6864896171579,27.9276452527475,13.9367378893781));
#48131=CARTESIAN_POINT('Ctrl Pts',(56.6170847408471,27.8255919943081,13.9281112117561));
#48132=CARTESIAN_POINT('Ctrl Pts',(56.5286799635785,27.7184332618856,13.9189118166904));
#48133=CARTESIAN_POINT('Ctrl Pts',(56.518510803645,27.7064000960918,13.9178768736967));
#48134=CARTESIAN_POINT('Ctrl Pts',(56.5039748214759,27.689607321279,13.9164313571804));
#48135=CARTESIAN_POINT('Ctrl Pts',(56.4997261206788,27.6847468677807,13.9160128256075));
#48136=CARTESIAN_POINT('Ctrl Pts',(56.4925355464219,27.6766010991317,13.9153112783626));
#48137=CARTESIAN_POINT('Ctrl Pts',(56.4896062637499,27.673304786914,13.9150273535929));
#48138=CARTESIAN_POINT('Ctrl Pts',(56.4836010006278,27.6665920481546,13.9144491389884));
#48139=CARTESIAN_POINT('Ctrl Pts',(56.4805241053374,27.6631765001843,13.9141549203355));
#48140=CARTESIAN_POINT('Ctrl Pts',(56.4726441312357,27.6544898073523,13.9134065112992));
#48141=CARTESIAN_POINT('Ctrl Pts',(56.4678244947929,27.6492336723389,13.9129535428838));
#48142=CARTESIAN_POINT('Ctrl Pts',(56.4480440695992,27.6278926889008,13.9111133418582));
#48143=CARTESIAN_POINT('Ctrl Pts',(56.4328456155094,27.6120289496164,13.9097429641106));
#48144=CARTESIAN_POINT('Ctrl Pts',(56.3919524378469,27.5707335288503,13.9061585261536));
#48145=CARTESIAN_POINT('Ctrl Pts',(56.3658223821017,27.5457428828289,13.9039714492178));
#48146=CARTESIAN_POINT('Ctrl Pts',(56.2038638338668,27.3990651491109,13.8909187544325));
#48147=CARTESIAN_POINT('Ctrl Pts',(56.0525544717185,27.2957648713558,13.8807073310655));
#48148=CARTESIAN_POINT('Ctrl Pts',(55.8421425156038,27.1909671641845,13.8665783800287));
#48149=CARTESIAN_POINT('Ctrl Pts',(55.7940697417436,27.169356305483,13.8633616022349));
#48150=CARTESIAN_POINT('Ctrl Pts',(55.7316148496795,27.1442031919948,13.8591678784783));
#48151=CARTESIAN_POINT('Ctrl Pts',(55.7179692857853,27.1388814740622,13.8582507974157));
#48152=CARTESIAN_POINT('Ctrl Pts',(55.696155441944,27.1306497590218,13.8567829176943));
#48153=CARTESIAN_POINT('Ctrl Pts',(55.6880244855881,27.1276418541832,13.856235375724));
#48154=CARTESIAN_POINT('Ctrl Pts',(55.6733587239375,27.1223249419516,13.8552469480946));
#48155=CARTESIAN_POINT('Ctrl Pts',(55.666830967928,27.1199967944287,13.8548067035874));
#48156=CARTESIAN_POINT('Ctrl Pts',(55.6514822166297,27.1146126041592,13.8537708004094));
#48157=CARTESIAN_POINT('Ctrl Pts',(55.642651696652,27.1115843934909,13.8531742374692));
#48158=CARTESIAN_POINT('Ctrl Pts',(55.6169676863278,27.1029777038107,13.8514372466277));
#48159=CARTESIAN_POINT('Ctrl Pts',(55.6000609227542,27.0975622024356,13.8502915367412));
#48160=CARTESIAN_POINT('Ctrl Pts',(55.444625152373,27.0500517563864,13.8397342686215));
#48161=CARTESIAN_POINT('Ctrl Pts',(55.3019966260477,27.0229384485427,13.8298256084381));
#48162=CARTESIAN_POINT('Ctrl Pts',(55.0291351005587,27.0012962381262,13.8107699328795));
#48163=CARTESIAN_POINT('Ctrl Pts',(54.8998543217901,27.0035927520551,13.8017145598568));
#48164=CARTESIAN_POINT('Ctrl Pts',(54.7563237048571,27.0201291054974,13.7921506511831));
#48165=CARTESIAN_POINT('Ctrl Pts',(54.7409755193925,27.0220785533364,13.7911345961937));
#48166=CARTESIAN_POINT('Ctrl Pts',(54.7199326459483,27.025000463303,13.7897520890081));
#48167=CARTESIAN_POINT('Ctrl Pts',(54.7142176621014,27.0258193218226,13.7893776877286));
#48168=CARTESIAN_POINT('Ctrl Pts',(54.7044500361928,27.0272621580412,13.7887397132935));
#48169=CARTESIAN_POINT('Ctrl Pts',(54.700395655348,27.0278738347646,13.7884754685129));
#48170=CARTESIAN_POINT('Ctrl Pts',(54.6919788284793,27.0291702205632,13.787928121352));
#48171=CARTESIAN_POINT('Ctrl Pts',(54.6876167445176,27.0298569179614,13.787645142103));
#48172=CARTESIAN_POINT('Ctrl Pts',(54.677080001698,27.0315515300813,13.7869631880806));
#48173=CARTESIAN_POINT('Ctrl Pts',(54.6709076673694,27.0325740310885,13.78656502541));
#48174=CARTESIAN_POINT('Ctrl Pts',(54.6493148870433,27.0362555234082,13.7851764295812));
#48175=CARTESIAN_POINT('Ctrl Pts',(54.6339205443326,27.0390669859573,13.7841941392111));
#48176=CARTESIAN_POINT('Ctrl Pts',(54.5393207514004,27.0574966126828,13.7781964887587));
#48177=CARTESIAN_POINT('Ctrl Pts',(54.4610819511533,27.0777317899205,13.7734019205983));
#48178=CARTESIAN_POINT('Ctrl Pts',(54.2899824146538,27.1332567081432,13.7628691405398));
#48179=CARTESIAN_POINT('Ctrl Pts',(54.1981001170324,27.1708438163722,13.7571753820321));
#48180=CARTESIAN_POINT('Ctrl Pts',(54.0244365034281,27.2574966584921,13.7457803729509));
#48181=CARTESIAN_POINT('Ctrl Pts',(53.9426256203644,27.3058931363041,13.7401039602952));
#48182=CARTESIAN_POINT('Ctrl Pts',(53.851878610867,27.3687172585093,13.7332514870052));
#48183=CARTESIAN_POINT('Ctrl Pts',(53.8392827210759,27.3776555592461,13.732287294808));
#48184=CARTESIAN_POINT('Ctrl Pts',(53.8188989617653,27.392479190798,13.7307047886843));
#48185=CARTESIAN_POINT('Ctrl Pts',(53.8110481068422,27.3982771135814,13.7300898140024));
#48186=CARTESIAN_POINT('Ctrl Pts',(53.7972281024202,27.4086408960748,13.7289973695291));
#48187=CARTESIAN_POINT('Ctrl Pts',(53.7912415726967,27.4131833448164,13.7285208139995));
#48188=CARTESIAN_POINT('Ctrl Pts',(53.7850295944423,27.4179524101621,13.7280227860304));
#48189=CARTESIAN_POINT('Ctrl Pts',(53.7847783156711,27.4181454172935,13.7280026344184));
#48190=CARTESIAN_POINT('Ctrl Pts',(53.7843290172851,27.4184906934568,13.7279665915702));
#48191=CARTESIAN_POINT('Ctrl Pts',(53.7841309802507,27.418642939842,13.7279507012242));
#48192=CARTESIAN_POINT('Ctrl Pts',(53.7837751966178,27.4189165645815,13.7279221466534));
#48193=CARTESIAN_POINT('Ctrl Pts',(53.7836174395383,27.4190379293856,13.7279094829599));
#48194=CARTESIAN_POINT('Ctrl Pts',(53.7833329639721,27.4192568483408,13.7278866428393));
#48195=CARTESIAN_POINT('Ctrl Pts',(53.7832062390315,27.4193543941343,13.7278764667405));
#48196=CARTESIAN_POINT('Ctrl Pts',(53.7829770460267,27.4195308580267,13.7278580595973));
#48197=CARTESIAN_POINT('Ctrl Pts',(53.7828745739527,27.419609770817,13.7278498287644));
#48198=CARTESIAN_POINT('Ctrl Pts',(53.7826888056261,27.4197528580603,13.7278349055229));
#48199=CARTESIAN_POINT('Ctrl Pts',(53.7826055066662,27.4198170292156,13.7278282132389));
#48200=CARTESIAN_POINT('Ctrl Pts',(53.7823839664693,27.4199877254125,13.7278104128041));
#48201=CARTESIAN_POINT('Ctrl Pts',(53.7822457341113,27.4200942620307,13.7277993041961));
#48202=CARTESIAN_POINT('Ctrl Pts',(53.7819749860418,27.4203029860524,13.7277775427791));
#48203=CARTESIAN_POINT('Ctrl Pts',(53.7818424692788,27.420405171935,13.7277668900339));
#48204=CARTESIAN_POINT('Ctrl Pts',(53.7815827204365,27.4206055207184,13.7277460060535));
#48205=CARTESIAN_POINT('Ctrl Pts',(53.7814554872659,27.4207036823922,13.7277357748621));
#48206=CARTESIAN_POINT('Ctrl Pts',(53.7812059146623,27.4208962782861,13.7277157029389));
#48207=CARTESIAN_POINT('Ctrl Pts',(53.7810835744424,27.4209907112716,13.7277058622609));
#48208=CARTESIAN_POINT('Ctrl Pts',(53.7808434341293,27.4211761173116,13.7276865432656));
#48209=CARTESIAN_POINT('Ctrl Pts',(53.7807256331334,27.4212670894179,13.7276770649804));
#48210=CARTESIAN_POINT('Ctrl Pts',(53.7804942496461,27.4214458172252,13.7276584452005));
#48211=CARTESIAN_POINT('Ctrl Pts',(53.780380666441,27.4215335720038,13.7276493037423));
#48212=CARTESIAN_POINT('Ctrl Pts',(53.7801574257056,27.4217060870522,13.727631334325));
#48213=CARTESIAN_POINT('Ctrl Pts',(53.7800477675759,27.4217908464616,13.7276225064019));
#48214=CARTESIAN_POINT('Ctrl Pts',(53.7798321099569,27.4219575732693,13.7276051428055));
#48215=CARTESIAN_POINT('Ctrl Pts',(53.7797261098431,27.422039539958,13.7275966071578));
#48216=CARTESIAN_POINT('Ctrl Pts',(53.7795175236842,27.4222008669263,13.7275798086416));
#48217=CARTESIAN_POINT('Ctrl Pts',(53.7794149371728,27.4222802264898,13.7275715458042));
#48218=CARTESIAN_POINT('Ctrl Pts',(53.779212954302,27.4224365092483,13.7275552750751));
#48219=CARTESIAN_POINT('Ctrl Pts',(53.7791135574443,27.4225134318541,13.7275472672055));
#48220=CARTESIAN_POINT('Ctrl Pts',(53.7715419549009,27.4283741919388,13.7269371910812));
#48221=CARTESIAN_POINT('Ctrl Pts',(53.7641110412985,27.4342109574254,13.726333042846));
#48222=CARTESIAN_POINT('Ctrl Pts',(53.7486875278689,27.4465038722832,13.7250676024798));
#48223=CARTESIAN_POINT('Ctrl Pts',(53.740702795094,27.4529694040054,13.7244059474242));
#48224=CARTESIAN_POINT('Ctrl Pts',(53.7199595064664,27.4700330098056,13.7226696883172));
#48225=CARTESIAN_POINT('Ctrl Pts',(53.7072827697899,27.4807288617268,13.721591190327));
#48226=CARTESIAN_POINT('Ctrl Pts',(53.6697467192044,27.513209405967,13.7183444825198));
#48227=CARTESIAN_POINT('Ctrl Pts',(53.6452949459689,27.5354543127234,13.7161579741097));
#48228=CARTESIAN_POINT('Ctrl Pts',(53.509867458539,27.6649532553078,13.703631876999));
#48229=CARTESIAN_POINT('Ctrl Pts',(53.4110929036486,27.78418493134,13.6928006453438));
#48230=CARTESIAN_POINT('Ctrl Pts',(53.2813515487948,27.9839689921873,13.6762697187608));
#48231=CARTESIAN_POINT('Ctrl Pts',(53.2401232236364,28.0571805440688,13.6705112347364));
#48232=CARTESIAN_POINT('Ctrl Pts',(53.1990242983824,28.1423134841901,13.6643025314381));
#48233=CARTESIAN_POINT('Ctrl Pts',(53.1944976359306,28.1518839334948,13.6636112806525));
#48234=CARTESIAN_POINT('Ctrl Pts',(53.1877714475442,28.1664026466545,13.6625732420881));
#48235=CARTESIAN_POINT('Ctrl Pts',(53.1855156060419,28.1713243942352,13.6622231835562));
#48236=CARTESIAN_POINT('Ctrl Pts',(53.1815029059856,28.1801741671808,13.6615971028701));
#48237=CARTESIAN_POINT('Ctrl Pts',(53.1797387002814,28.1840987321243,13.661320643007));
#48238=CARTESIAN_POINT('Ctrl Pts',(53.1759057898713,28.192699547708,13.6607173661997));
#48239=CARTESIAN_POINT('Ctrl Pts',(53.1738423640646,28.1973780480107,13.660390868863));
#48240=CARTESIAN_POINT('Ctrl Pts',(53.1680040285132,28.210754646661,13.6594619496137));
#48241=CARTESIAN_POINT('Ctrl Pts',(53.1642730549121,28.2194719359409,13.6588621097547));
#48242=CARTESIAN_POINT('Ctrl Pts',(53.139384588578,28.2787886881304,13.6548156630093));
#48243=CARTESIAN_POINT('Ctrl Pts',(53.120257471211,28.3302204271598,13.651479776779));
#48244=CARTESIAN_POINT('Ctrl Pts',(53.0384007306736,28.5816045754939,13.6356996351405));
#48245=CARTESIAN_POINT('Ctrl Pts',(53.005322673042,28.7897894775224,13.6240476812006));
#48246=CARTESIAN_POINT('Ctrl Pts',(53.0052501195981,28.9993092490871,13.6112224443046));
#48247=CARTESIAN_POINT('Ctrl Pts',(53.0466869980082,29.4044698737233,13.5836009930267));
#48248=CARTESIAN_POINT('Ctrl Pts',(53.0322541803675,29.3347692305246,13.5881317496805));
#48249=CARTESIAN_POINT('Ctrl Pts',(53.0215445661767,29.2642383494607,13.5926625063343));
#48250=CARTESIAN_POINT('Ctrl Pts',(53.0146376983758,29.1932979404689,13.5971932629881));
#48251=CARTESIAN_POINT('Ctrl Pts',(53.0083611430925,29.1288314685893,13.6013105481937));
#48252=CARTESIAN_POINT('Ctrl Pts',(53.0052243749933,29.0640272252075,13.6054278333992));
#48253=CARTESIAN_POINT('Ctrl Pts',(53.0052501577945,28.9992065763071,13.6095451186048));
#48254=CARTESIAN_POINT('Ctrl Pts',(53.04668699692,29.404469868468,13.4272582639285));
#48255=CARTESIAN_POINT('Ctrl Pts',(53.0192622797945,29.2720272299845,13.4356299227296));
#48256=CARTESIAN_POINT('Ctrl Pts',(53.0053718659343,29.1371047871859,13.4433896989916));
#48257=CARTESIAN_POINT('Ctrl Pts',(53.0051306974257,28.8675449949671,13.4590561681005));
#48258=CARTESIAN_POINT('Ctrl Pts',(53.018560705128,28.7336554613748,13.4669297628423));
#48259=CARTESIAN_POINT('Ctrl Pts',(53.0484658429314,28.5867336035516,13.4762350552335));
#48260=CARTESIAN_POINT('Ctrl Pts',(53.0517831798354,28.5713674296968,13.4772161475346));
#48261=CARTESIAN_POINT('Ctrl Pts',(53.0574723139598,28.5464466642276,13.47882084617));
#48262=CARTESIAN_POINT('Ctrl Pts',(53.0597338740793,28.5368674115602,13.4794409523941));
#48263=CARTESIAN_POINT('Ctrl Pts',(53.0638944896611,28.5198098907924,13.4805511858727));
#48264=CARTESIAN_POINT('Ctrl Pts',(53.0657662261264,28.5123251150224,13.4810404316407));
#48265=CARTESIAN_POINT('Ctrl Pts',(53.0698130200128,28.4965324892311,13.4820772087865));
#48266=CARTESIAN_POINT('Ctrl Pts',(53.0719983959439,28.4882274693868,13.4826250625314));
#48267=CARTESIAN_POINT('Ctrl Pts',(53.077958904894,28.4661560585519,13.4840881899181));
#48268=CARTESIAN_POINT('Ctrl Pts',(53.0818282409135,28.4524158418302,13.4850064759762));
#48269=CARTESIAN_POINT('Ctrl Pts',(53.1013726919866,28.3857627910998,13.4894981975022));
#48270=CARTESIAN_POINT('Ctrl Pts',(53.1190902137219,28.3334788812946,13.4931370802024));
#48271=CARTESIAN_POINT('Ctrl Pts',(53.2144773091795,28.0862362499409,13.5109178671461));
#48272=CARTESIAN_POINT('Ctrl Pts',(53.3203980659002,27.9036564916009,13.5259805171546));
#48273=CARTESIAN_POINT('Ctrl Pts',(53.4700172669804,27.7197952147096,13.5418939049268));
#48274=CARTESIAN_POINT('Ctrl Pts',(53.4876654878434,27.6989942525256,13.5437037653887));
#48275=CARTESIAN_POINT('Ctrl Pts',(53.511049054234,27.67255245965,13.5460098610623));
#48276=CARTESIAN_POINT('Ctrl Pts',(53.5163986154985,27.6665762757419,13.5465314356923));
#48277=CARTESIAN_POINT('Ctrl Pts',(53.525003110516,27.6570797785728,13.5473606073883));
#48278=CARTESIAN_POINT('Ctrl Pts',(53.5282348740401,27.6535387267781,13.5476698696107));
#48279=CARTESIAN_POINT('Ctrl Pts',(53.5344311426885,27.6467984224367,13.548258638127));
#48280=CARTESIAN_POINT('Ctrl Pts',(53.537393388527,27.6435972259601,13.5485382981469));
#48281=CARTESIAN_POINT('Ctrl Pts',(53.5444140103239,27.6360600234444,13.5491968940579));
#48282=CARTESIAN_POINT('Ctrl Pts',(53.5484813299337,27.6317323413894,13.549575156563));
#48283=CARTESIAN_POINT('Ctrl Pts',(53.5620244630688,27.6174506201933,13.5508240906368));
#48284=CARTESIAN_POINT('Ctrl Pts',(53.5715840587647,27.6075760861822,13.5516886481452));
#48285=CARTESIAN_POINT('Ctrl Pts',(53.6249367112101,27.5535935064197,13.556426194913));
#48286=CARTESIAN_POINT('Ctrl Pts',(53.6706750253964,27.5114478695419,13.5601670286191));
#48287=CARTESIAN_POINT('Ctrl Pts',(53.8394122124819,27.369956842267,13.5731934873786));
#48288=CARTESIAN_POINT('Ctrl Pts',(53.9721501891463,27.2831621438011,13.582129913193));
#48289=CARTESIAN_POINT('Ctrl Pts',(54.1680317258645,27.186018662626,13.5952015002929));
#48290=CARTESIAN_POINT('Ctrl Pts',(54.223512991292,27.1615859118838,13.5988859279352));
#48291=CARTESIAN_POINT('Ctrl Pts',(54.2941428846151,27.1342500855928,13.6035988951816));
#48292=CARTESIAN_POINT('Ctrl Pts',(54.3083308202188,27.1289439515654,13.6045466458279));
#48293=CARTESIAN_POINT('Ctrl Pts',(54.3309177685287,27.1207886872144,13.6060576764053));
#48294=CARTESIAN_POINT('Ctrl Pts',(54.3392779023909,27.1178330317896,13.6066174342552));
#48295=CARTESIAN_POINT('Ctrl Pts',(54.3541876162418,27.1126734043429,13.6076166906297));
#48296=CARTESIAN_POINT('Ctrl Pts',(54.3607295054006,27.1104475274632,13.6080554605506));
#48297=CARTESIAN_POINT('Ctrl Pts',(54.3758990358787,27.1053738906735,13.6090737192456));
#48298=CARTESIAN_POINT('Ctrl Pts',(54.3845347784986,27.1025510114365,13.6096540116386));
#48299=CARTESIAN_POINT('Ctrl Pts',(54.4089693702275,27.0947481116549,13.611297824848));
#48300=CARTESIAN_POINT('Ctrl Pts',(54.4248111023746,27.089905848361,13.6123657909032));
#48301=CARTESIAN_POINT('Ctrl Pts',(54.5340505284384,27.0579973552965,13.6197471721428));
#48302=CARTESIAN_POINT('Ctrl Pts',(54.6292445131402,27.0375987859738,13.6262743641295));
#48303=CARTESIAN_POINT('Ctrl Pts',(54.8431431712336,27.0078849615611,13.641107386835));
#48304=CARTESIAN_POINT('Ctrl Pts',(54.9619691336942,27.0020815866556,13.6494632201937));
#48305=CARTESIAN_POINT('Ctrl Pts',(55.1068628280687,27.0079411007819,13.6594701311226));
#48306=CARTESIAN_POINT('Ctrl Pts',(55.1331009846328,27.0095220325701,13.6612740240867));
#48307=CARTESIAN_POINT('Ctrl Pts',(55.2022938617599,27.0150654913943,13.6659980517488));
#48308=CARTESIAN_POINT('Ctrl Pts',(55.2451674067815,27.019903695524,13.6688915489856));
#48309=CARTESIAN_POINT('Ctrl Pts',(55.2961918153411,27.0273446895328,13.672269569159));
#48310=CARTESIAN_POINT('Ctrl Pts',(55.3045223271595,27.0286135022251,13.6728189731656));
#48311=CARTESIAN_POINT('Ctrl Pts',(55.3181553356886,27.0307784130053,13.6737143493731));
#48312=CARTESIAN_POINT('Ctrl Pts',(55.3234625934568,27.0316432161366,13.6740619860121));
#48313=CARTESIAN_POINT('Ctrl Pts',(55.3330086123248,27.0332383657885,13.6746855192151));
#48314=CARTESIAN_POINT('Ctrl Pts',(55.3372485439355,27.0339609662236,13.67496183725));
#48315=CARTESIAN_POINT('Ctrl Pts',(55.3465541257768,27.0355778815793,13.6755669026442));
#48316=CARTESIAN_POINT('Ctrl Pts',(55.3516186586799,27.0364780770946,13.6758953165495));
#48317=CARTESIAN_POINT('Ctrl Pts',(55.366150214895,27.0391190155327,13.676835214478));
#48318=CARTESIAN_POINT('Ctrl Pts',(55.3756083509271,27.0409087334696,13.6774440198634));
#48319=CARTESIAN_POINT('Ctrl Pts',(55.4424588569501,27.0540604696559,13.6817285841596));
#48320=CARTESIAN_POINT('Ctrl Pts',(55.4993457718579,27.0678753394493,13.6852781593405));
#48321=CARTESIAN_POINT('Ctrl Pts',(55.6460229120549,27.1104085328351,13.6943691825458));
#48322=CARTESIAN_POINT('Ctrl Pts',(55.7345296956808,27.1430214324681,13.6997974645792));
#48323=CARTESIAN_POINT('Ctrl Pts',(55.9394549824077,27.2354857316176,13.712869705305));
#48324=CARTESIAN_POINT('Ctrl Pts',(56.0529258671097,27.3007569638729,13.7205440317705));
#48325=CARTESIAN_POINT('Ctrl Pts',(56.1720307479055,27.385806650501,13.7296264899733));
#48326=CARTESIAN_POINT('Ctrl Pts',(56.184754887258,27.3951224100962,13.7306106306991));
#48327=CARTESIAN_POINT('Ctrl Pts',(56.2052510559006,27.4105049149619,13.7322193300444));
#48328=CARTESIAN_POINT('Ctrl Pts',(56.2130910667286,27.4164802523002,13.7328403591743));
#48329=CARTESIAN_POINT('Ctrl Pts',(56.2269891012955,27.4272365531428,13.7339516201237));
#48330=CARTESIAN_POINT('Ctrl Pts',(56.2330643162668,27.4319950562254,13.734440964218));
#48331=CARTESIAN_POINT('Ctrl Pts',(56.2458350416459,27.4421180348539,13.735477297017));
#48332=CARTESIAN_POINT('Ctrl Pts',(56.2525238451077,27.4474906821569,13.7360246041238));
#48333=CARTESIAN_POINT('Ctrl Pts',(56.2702192578666,27.4618929567417,13.7374847216203));
#48334=CARTESIAN_POINT('Ctrl Pts',(56.2811640520132,27.4709974185492,13.7384005225917));
#48335=CARTESIAN_POINT('Ctrl Pts',(56.3337016055214,27.5156611000157,13.7428595047627));
#48336=CARTESIAN_POINT('Ctrl Pts',(56.3739132129935,27.5528015091451,13.7464669815222));
#48337=CARTESIAN_POINT('Ctrl Pts',(56.556403682939,27.7358218331011,13.763802763068));
#48338=CARTESIAN_POINT('Ctrl Pts',(56.6772807696819,27.9012527193196,13.7783918612653));
#48339=CARTESIAN_POINT('Ctrl Pts',(56.7861187992832,28.1112451127015,13.794354833922));
#48340=CARTESIAN_POINT('Ctrl Pts',(56.8005066069445,28.1407666972846,13.7965425201784));
#48341=CARTESIAN_POINT('Ctrl Pts',(56.8176827240047,28.1783377419043,13.7992446313139));
#48342=CARTESIAN_POINT('Ctrl Pts',(56.8211564665033,28.186066045576,13.7997961540347));
#48343=CARTESIAN_POINT('Ctrl Pts',(56.8265787406386,28.1983379128634,13.80066486956));
#48344=CARTESIAN_POINT('Ctrl Pts',(56.8285597596163,28.202866884079,13.8009839597641));
#48345=CARTESIAN_POINT('Ctrl Pts',(56.8320695862194,28.2109729247638,13.8015523151733));
#48346=CARTESIAN_POINT('Ctrl Pts',(56.8336047561259,28.2145470778719,13.8018019570369));
#48347=CARTESIAN_POINT('Ctrl Pts',(56.837253417559,28.2231108163822,13.802397834299));
#48348=CARTESIAN_POINT('Ctrl Pts',(56.839357041771,28.2281045417277,13.8027434733792));
#48349=CARTESIAN_POINT('Ctrl Pts',(56.8456536612356,28.2432237912973,13.8037846017817));
#48350=CARTESIAN_POINT('Ctrl Pts',(56.8497836678832,28.2533755548553,13.8044764418035));
#48351=CARTESIAN_POINT('Ctrl Pts',(56.859138853412,28.2769252653885,13.8060658507437));
#48352=CARTESIAN_POINT('Ctrl Pts',(56.8643032978211,28.2903468541546,13.8069601953942));
#48353=CARTESIAN_POINT('Ctrl Pts',(56.8814524795775,28.3363945866847,13.8099932493751));
#48354=CARTESIAN_POINT('Ctrl Pts',(56.8927300162752,28.3692790308099,13.8120991616735));
#48355=CARTESIAN_POINT('Ctrl Pts',(56.9515715872095,28.5566820118012,13.8238511790861));
#48356=CARTESIAN_POINT('Ctrl Pts',(56.9810729004658,28.7162409482339,13.832959407114));
#48357=CARTESIAN_POINT('Ctrl Pts',(56.9928851853073,28.9084136673114,13.8443856836901));
#48358=CARTESIAN_POINT('Ctrl Pts',(56.9940632644929,28.9392464334113,13.8462308312626));
#48359=CARTESIAN_POINT('Ctrl Pts',(56.9952141605428,29.0160012475613,13.8508679486389));
#48360=CARTESIAN_POINT('Ctrl Pts',(56.9943172901175,29.0619163826329,13.8536811574656));
#48361=CARTESIAN_POINT('Ctrl Pts',(56.9910834041304,29.1216931360445,13.8574134479113));
#48362=CARTESIAN_POINT('Ctrl Pts',(56.9901832593468,29.1356205006884,13.8582879469259));
#48363=CARTESIAN_POINT('Ctrl Pts',(56.9884985263497,29.1580307726393,13.8597034805317));
#48364=CARTESIAN_POINT('Ctrl Pts',(56.9878056026295,29.1665202598075,13.8602416567928));
#48365=CARTESIAN_POINT('Ctrl Pts',(56.9863800870205,29.1827059892552,13.8612715399131));
#48366=CARTESIAN_POINT('Ctrl Pts',(56.9856570820741,29.1904029366585,13.861762938823));
#48367=CARTESIAN_POINT('Ctrl Pts',(56.9838990273516,29.2080184094293,13.862891435862));
#48368=CARTESIAN_POINT('Ctrl Pts',(56.9828343110241,29.217933702026,13.8635294490617));
#48369=CARTESIAN_POINT('Ctrl Pts',(56.9793022726372,29.2486544276286,13.865515160001));
#48370=CARTESIAN_POINT('Ctrl Pts',(56.9765815480504,29.269428728191,13.8668707172512));
#48371=CARTESIAN_POINT('Ctrl Pts',(56.9618187864692,29.3698397011017,13.873486858702));
#48372=CARTESIAN_POINT('Ctrl Pts',(56.9452896746838,29.4487310778269,13.8788856539736));
#48373=CARTESIAN_POINT('Ctrl Pts',(56.8886021908327,29.655929187901,13.893580012467));
#48374=CARTESIAN_POINT('Ctrl Pts',(56.8401780429224,29.7815385032808,13.9030534175969));
#48375=CARTESIAN_POINT('Ctrl Pts',(56.7734796273103,29.9132225485684,13.9132134275387));
#48376=CARTESIAN_POINT('Ctrl Pts',(56.7673345101703,29.9250589994415,13.9141285064394));
#48377=CARTESIAN_POINT('Ctrl Pts',(56.7378299908922,29.980521977619,13.9184224612474));
#48378=CARTESIAN_POINT('Ctrl Pts',(56.7129689835823,30.0233350305033,13.9217553112083));
#48379=CARTESIAN_POINT('Ctrl Pts',(56.6818623218586,30.0725872427281,13.9255742071527));
#48380=CARTESIAN_POINT('Ctrl Pts',(56.6771368589783,30.079961214984,13.9261455423294));
#48381=CARTESIAN_POINT('Ctrl Pts',(56.6693770470305,30.0918964434607,13.9270692865281));
#48382=CARTESIAN_POINT('Ctrl Pts',(56.6663722647528,30.096476650632,13.9274235372464));
#48383=CARTESIAN_POINT('Ctrl Pts',(56.660971340531,30.1046358303036,13.9280540850271));
#48384=CARTESIAN_POINT('Ctrl Pts',(56.6585824444064,30.1082194673971,13.9283308477906));
#48385=CARTESIAN_POINT('Ctrl Pts',(56.6533596955507,30.1159995154923,13.928931288231));
#48386=CARTESIAN_POINT('Ctrl Pts',(56.6505214688519,30.1201928778897,13.9292546690646));
#48387=CARTESIAN_POINT('Ctrl Pts',(56.642453529663,30.1320156897458,13.930165841753));
#48388=CARTESIAN_POINT('Ctrl Pts',(56.6371865936775,30.1396197542288,13.9307512041576));
#48389=CARTESIAN_POINT('Ctrl Pts',(56.6033230585753,30.1877904326045,13.9344569672262));
#48390=CARTESIAN_POINT('Ctrl Pts',(56.5732711193595,30.2273181466497,13.9374869289217));
#48391=CARTESIAN_POINT('Ctrl Pts',(56.4502927154589,30.3771220173194,13.9491032961354));
#48392=CARTESIAN_POINT('Ctrl Pts',(56.3469964045756,30.4783166965125,13.9572751912039));
#48393=CARTESIAN_POINT('Ctrl Pts',(56.1621380870861,30.6238081508515,13.9711097313542));
#48394=CARTESIAN_POINT('Ctrl Pts',(56.0868261923672,30.6751488308281,13.976563788154));
#48395=CARTESIAN_POINT('Ctrl Pts',(55.9950733333197,30.7288987283495,13.9831670697934));
#48396=CARTESIAN_POINT('Ctrl Pts',(55.9817807042995,30.7364816094512,13.9841225584316));
#48397=CARTESIAN_POINT('Ctrl Pts',(55.9599074599513,30.7486279330233,13.9856936264227));
#48398=CARTESIAN_POINT('Ctrl Pts',(55.9513782630393,30.7532830276627,13.986305948046));
#48399=CARTESIAN_POINT('Ctrl Pts',(55.9360282549451,30.761515820783,13.987407576762));
#48400=CARTESIAN_POINT('Ctrl Pts',(55.9292200480779,30.765116704491,13.9878960549306));
#48401=CARTESIAN_POINT('Ctrl Pts',(55.9147108471562,30.7726834631291,13.9889368796685));
#48402=CARTESIAN_POINT('Ctrl Pts',(55.9070045519298,30.7766387739934,13.9894895833196));
#48403=CARTESIAN_POINT('Ctrl Pts',(55.886229306153,30.7871314196129,13.990979440889));
#48404=CARTESIAN_POINT('Ctrl Pts',(55.8731140758901,30.7935754474795,13.9919198039706));
#48405=CARTESIAN_POINT('Ctrl Pts',(55.8062178986304,30.8255365602756,13.9967163606685));
#48406=CARTESIAN_POINT('Ctrl Pts',(55.7513897082779,30.8487788723939,14.0006492634164));
#48407=CARTESIAN_POINT('Ctrl Pts',(55.5783829187453,30.9131505817495,14.0130711142128));
#48408=CARTESIAN_POINT('Ctrl Pts',(55.457325362907,30.9456410000043,14.0217995351282));
#48409=CARTESIAN_POINT('Ctrl Pts',(55.3065832885331,30.9712457652461,14.0324465720854));
#48410=CARTESIAN_POINT('Ctrl Pts',(55.2790315711577,30.9753340498615,14.0343825333049));
#48411=CARTESIAN_POINT('Ctrl Pts',(55.235974155518,30.980804293473,14.0373856139143));
#48412=CARTESIAN_POINT('Ctrl Pts',(55.2205227664561,30.9825839642448,14.0384588020913));
#48413=CARTESIAN_POINT('Ctrl Pts',(55.1932647908902,30.9854008923412,14.040342648024));
#48414=CARTESIAN_POINT('Ctrl Pts',(55.1814668635183,30.9865139739101,14.0411549362191));
#48415=CARTESIAN_POINT('Ctrl Pts',(55.1213401029865,30.9916465357524,14.0452769500359));
#48416=CARTESIAN_POINT('Ctrl Pts',(55.0728817523399,30.9940081356515,14.0485411204418));
#48417=CARTESIAN_POINT('Ctrl Pts',(55.0156722412972,30.9947074484053,14.0522915149576));
#48418=CARTESIAN_POINT('Ctrl Pts',(55.0069622553196,30.9947568667458,14.0528596719106));
#48419=CARTESIAN_POINT('Ctrl Pts',(54.9927887817969,30.9947444467984,14.0537793105317));
#48420=CARTESIAN_POINT('Ctrl Pts',(54.9873254888367,30.9947172150906,14.0541326077435));
#48421=CARTESIAN_POINT('Ctrl Pts',(54.9775566148965,30.9946283857934,14.0547621333201));
#48422=CARTESIAN_POINT('Ctrl Pts',(54.9732510681428,30.9945752928206,14.0550388210311));
#48423=CARTESIAN_POINT('Ctrl Pts',(54.9638717464374,30.9944292572019,14.0556398788227));
#48424=CARTESIAN_POINT('Ctrl Pts',(54.9587981493436,30.9943308957053,14.0559639470099));
#48425=CARTESIAN_POINT('Ctrl Pts',(54.9444267149429,30.9939974111246,14.0568790233002));
#48426=CARTESIAN_POINT('Ctrl Pts',(54.9351299238276,30.9937166164576,14.0574675687562));
#48427=CARTESIAN_POINT('Ctrl Pts',(54.8751566660358,30.9914852688371,14.0612441873773));
#48428=CARTESIAN_POINT('Ctrl Pts',(54.8245635905017,30.9876675931011,14.0643377812585));
#48429=CARTESIAN_POINT('Ctrl Pts',(54.6226861112882,30.9646643647558,14.0765048208363));
#48430=CARTESIAN_POINT('Ctrl Pts',(54.4736773815441,30.9300938729643,14.0851209043516));
#48431=CARTESIAN_POINT('Ctrl Pts',(54.2526950064088,30.8512990205875,14.0989745782191));
#48432=CARTESIAN_POINT('Ctrl Pts',(54.1771218585655,30.818967290988,14.103915184312));
#48433=CARTESIAN_POINT('Ctrl Pts',(54.0903332878911,30.7753196808222,14.1099499694336));
#48434=CARTESIAN_POINT('Ctrl Pts',(54.0769818442792,30.7684148159326,14.1108887313059));
#48435=CARTESIAN_POINT('Ctrl Pts',(54.0552030109209,30.756837792662,14.1124378017198));
#48436=CARTESIAN_POINT('Ctrl Pts',(54.0467290286795,30.7522542139551,14.1130450066679));
#48437=CARTESIAN_POINT('Ctrl Pts',(54.0322029104018,30.7442604761362,14.1140937577726));
#48438=CARTESIAN_POINT('Ctrl Pts',(54.0261347194341,30.7408797283479,14.11453425608));
#48439=CARTESIAN_POINT('Ctrl Pts',(54.0128680127404,30.7333974277856,14.1155026228115));
#48440=CARTESIAN_POINT('Ctrl Pts',(54.0056771701003,30.7292825996562,14.1160309592713));
#48441=CARTESIAN_POINT('Ctrl Pts',(53.991026900061,30.7207776613804,14.1171145565142));
#48442=CARTESIAN_POINT('Ctrl Pts',(53.9835700034755,30.7163835627802,14.1176699529132));
#48443=CARTESIAN_POINT('Ctrl Pts',(53.9652660689358,30.705436557167,14.1190428794947));
#48444=CARTESIAN_POINT('Ctrl Pts',(53.954452547315,30.698828617189,14.1198623862227));
#48445=CARTESIAN_POINT('Ctrl Pts',(53.9245763020348,30.6801785073752,14.1221503794187));
#48446=CARTESIAN_POINT('Ctrl Pts',(53.9056541627246,30.6679157854479,14.1236267852478));
#48447=CARTESIAN_POINT('Ctrl Pts',(53.8444220468922,30.6267430168411,14.1284957860482));
#48448=CARTESIAN_POINT('Ctrl Pts',(53.8030202578763,30.5965249831906,14.1319343696131));
#48449=CARTESIAN_POINT('Ctrl Pts',(53.6628183512369,30.485674246185,14.1440927774701));
#48450=CARTESIAN_POINT('Ctrl Pts',(53.5706230262519,30.3971969852112,14.1530507991673));
#48451=CARTESIAN_POINT('Ctrl Pts',(53.4355569263155,30.2401190356787,14.1674093788836));
#48452=CARTESIAN_POINT('Ctrl Pts',(53.3872642776358,30.1766323853783,14.1728652343878));
#48453=CARTESIAN_POINT('Ctrl Pts',(53.3370318731402,30.1016694239624,14.1787911452356));
#48454=CARTESIAN_POINT('Ctrl Pts',(53.3312375955971,30.092872618301,14.1794788637904));
#48455=CARTESIAN_POINT('Ctrl Pts',(53.3225771294647,30.0794949114825,14.1805126591863));
#48456=CARTESIAN_POINT('Ctrl Pts',(53.3196595307607,30.0749477473832,14.1808619681279));
#48457=CARTESIAN_POINT('Ctrl Pts',(53.3144517963359,30.0667583255159,14.1814872574659));
#48458=CARTESIAN_POINT('Ctrl Pts',(53.3121549471321,30.0631204778881,14.1817636705519));
#48459=CARTESIAN_POINT('Ctrl Pts',(53.3071490676496,30.0551348367984,14.1823674880994));
#48460=CARTESIAN_POINT('Ctrl Pts',(53.3044450126459,30.0507840354969,14.1826945687266));
#48461=CARTESIAN_POINT('Ctrl Pts',(53.2967607423014,30.0383132132239,14.1836268244172));
#48462=CARTESIAN_POINT('Ctrl Pts',(53.2918218084368,30.0301677397863,14.1842293882498));
#48463=CARTESIAN_POINT('Ctrl Pts',(53.2582925747111,29.9739659044742,14.1883457272394));
#48464=CARTESIAN_POINT('Ctrl Pts',(53.2316728004694,29.9247564554568,14.1917443531438));
#48465=CARTESIAN_POINT('Ctrl Pts',(53.1342445573405,29.7250124835798,14.2049986892035));
#48466=CARTESIAN_POINT('Ctrl Pts',(53.0803647391669,29.5671103438876,14.214353633724));
#48467=CARTESIAN_POINT('Ctrl Pts',(53.0466869970968,29.404469869322,14.2242573078582));
#48468=CARTESIAN_POINT('Origin',(55.,29.,3.45145488139523));
#48469=CARTESIAN_POINT('',(53.0466869980082,29.4044698737233,15.1816708487869));
#48470=CARTESIAN_POINT('',(53.0466869327998,29.4044695588112,15.0243707259923));
#48471=CARTESIAN_POINT('',(53.0466869980082,29.4044698737233,3.45145488139523));
#48472=CARTESIAN_POINT('Ctrl Pts',(53.0466869980082,29.4044698737233,15.1816708487869));
#48473=CARTESIAN_POINT('Ctrl Pts',(53.0470224670368,29.4060899598109,15.1815647121178));
#48474=CARTESIAN_POINT('Ctrl Pts',(53.0473599534689,29.4077096374892,15.181458690835));
#48475=CARTESIAN_POINT('Ctrl Pts',(53.048812389329,29.4146370526371,15.181005606289));
#48476=CARTESIAN_POINT('Ctrl Pts',(53.0499469795097,29.4199407058099,15.1806596578178));
#48477=CARTESIAN_POINT('Ctrl Pts',(53.053369592957,29.4356267288989,15.1796390761652));
#48478=CARTESIAN_POINT('Ctrl Pts',(53.055719044283,29.4459957011679,15.1789678051049));
#48479=CARTESIAN_POINT('Ctrl Pts',(53.0797470144503,29.5482398675821,15.1723775328184));
#48480=CARTESIAN_POINT('Ctrl Pts',(53.1078416497406,29.6384982890581,15.1667878124747));
#48481=CARTESIAN_POINT('Ctrl Pts',(53.1638986225485,29.7818569058069,15.1577953700304));
#48482=CARTESIAN_POINT('Ctrl Pts',(53.188038245344,29.8362793946939,15.1543534888154));
#48483=CARTESIAN_POINT('Ctrl Pts',(53.2380289368913,29.9366171738472,15.1478322163256));
#48484=CARTESIAN_POINT('Ctrl Pts',(53.2633349986028,29.9827451920892,15.1447598892344));
#48485=CARTESIAN_POINT('Ctrl Pts',(53.3232484735195,30.0823990999518,15.13787460351));
#48486=CARTESIAN_POINT('Ctrl Pts',(53.3586559090021,30.1353730470149,15.1340456154438));
#48487=CARTESIAN_POINT('Ctrl Pts',(53.4110610019801,30.2061910497867,15.128621603843));
#48488=CARTESIAN_POINT('Ctrl Pts',(53.4259468885532,30.2255532260649,15.1271052657307));
#48489=CARTESIAN_POINT('Ctrl Pts',(53.4479212305432,30.2530744765511,15.1248985445183));
#48490=CARTESIAN_POINT('Ctrl Pts',(53.4547267438086,30.261457374144,15.1242193182452));
#48491=CARTESIAN_POINT('Ctrl Pts',(53.4666025441957,30.275845432215,15.1230410148455));
#48492=CARTESIAN_POINT('Ctrl Pts',(53.4716409286319,30.2818766986242,15.1225432267889));
#48493=CARTESIAN_POINT('Ctrl Pts',(53.4813756062181,30.2933907481243,15.121585394034));
#48494=CARTESIAN_POINT('Ctrl Pts',(53.4860662890743,30.2988781287734,15.12112558254));
#48495=CARTESIAN_POINT('Ctrl Pts',(53.4971772144188,30.3117342545164,15.120040376206));
#48496=CARTESIAN_POINT('Ctrl Pts',(53.5036219846617,30.3190814641071,15.1194139775259));
#48497=CARTESIAN_POINT('Ctrl Pts',(53.5262921221019,30.344546076252,15.1172209308533));
#48498=CARTESIAN_POINT('Ctrl Pts',(53.5427940905725,30.3624132676657,15.1156428080782));
#48499=CARTESIAN_POINT('Ctrl Pts',(53.6537600583608,30.4782367687602,15.1051444187163));
#48500=CARTESIAN_POINT('Ctrl Pts',(53.7576937575479,30.5665915035616,15.0958034167235));
#48501=CARTESIAN_POINT('Ctrl Pts',(53.9492604224329,30.6983156180562,15.079614273548));
#48502=CARTESIAN_POINT('Ctrl Pts',(54.0325944635387,30.7471284376168,15.0728630546955));
#48503=CARTESIAN_POINT('Ctrl Pts',(54.1559212260418,30.8078272938131,15.0635277169891));
#48504=CARTESIAN_POINT('Ctrl Pts',(54.1932589666301,30.8247953180536,15.0607826245665));
#48505=CARTESIAN_POINT('Ctrl Pts',(54.2390008357661,30.8439038001829,15.0575384920683));
#48506=CARTESIAN_POINT('Ctrl Pts',(54.2469269658911,30.8471551001205,15.0569805903791));
#48507=CARTESIAN_POINT('Ctrl Pts',(54.2587483829884,30.8519155078261,15.0561550606406));
#48508=CARTESIAN_POINT('Ctrl Pts',(54.262627734672,30.8534635553317,15.0558851965462));
#48509=CARTESIAN_POINT('Ctrl Pts',(54.270131840966,30.8564307649859,15.0553652338167));
#48510=CARTESIAN_POINT('Ctrl Pts',(54.2737559163352,30.8578515136133,15.0551150456948));
#48511=CARTESIAN_POINT('Ctrl Pts',(54.2819766427312,30.8610465596035,15.0545496354718));
#48512=CARTESIAN_POINT('Ctrl Pts',(54.2865757182341,30.8628144389725,15.0542347968642));
#48513=CARTESIAN_POINT('Ctrl Pts',(54.2990359684272,30.8675512308249,15.0533856816806));
#48514=CARTESIAN_POINT('Ctrl Pts',(54.3069095339833,30.8704875795197,15.0528532906089));
#48515=CARTESIAN_POINT('Ctrl Pts',(54.3449108715701,30.8843868085517,15.0503026453744));
#48516=CARTESIAN_POINT('Ctrl Pts',(54.3752832874809,30.8946727184954,15.0483210694459));
#48517=CARTESIAN_POINT('Ctrl Pts',(54.6011299184018,30.9651356977874,15.0339125865283));
#48518=CARTESIAN_POINT('Ctrl Pts',(54.8045874155427,30.9956676910153,15.0225965721283));
#48519=CARTESIAN_POINT('Ctrl Pts',(55.063939897846,30.9944775996404,15.0070201188638));
#48520=CARTESIAN_POINT('Ctrl Pts',(55.118688714962,30.9919692218243,15.0036763476619));
#48521=CARTESIAN_POINT('Ctrl Pts',(55.1874496559725,30.9859740740519,14.9993748379639));
#48522=CARTESIAN_POINT('Ctrl Pts',(55.2016238507265,30.9845851462249,14.9984827100107));
#48523=CARTESIAN_POINT('Ctrl Pts',(55.2243119224057,30.9821163817143,14.9970455071506));
#48524=CARTESIAN_POINT('Ctrl Pts',(55.2328359829634,30.9811331582019,14.9965034529015));
#48525=CARTESIAN_POINT('Ctrl Pts',(55.2490133844807,30.9791612983959,14.995470633942));
#48526=CARTESIAN_POINT('Ctrl Pts',(55.2566678686109,30.9781831849489,14.9949802073708));
#48527=CARTESIAN_POINT('Ctrl Pts',(55.2740848560142,30.9758547978881,14.9938602427892));
#48528=CARTESIAN_POINT('Ctrl Pts',(55.2838433546837,30.9744765470646,14.9932298385799));
#48529=CARTESIAN_POINT('Ctrl Pts',(55.3091818810254,30.9707061124449,14.9915852238612));
#48530=CARTESIAN_POINT('Ctrl Pts',(55.3247442363619,30.9682015076241,14.9905675160397));
#48531=CARTESIAN_POINT('Ctrl Pts',(55.4692664154368,30.9431814353208,14.9810433865531));
#48532=CARTESIAN_POINT('Ctrl Pts',(55.5957222696909,30.9082107956794,14.9721351533866));
#48533=CARTESIAN_POINT('Ctrl Pts',(55.8062786988101,30.8270005304312,14.9564621732478));
#48534=CARTESIAN_POINT('Ctrl Pts',(55.8921918203495,30.7866198611483,14.9498115676859));
#48535=CARTESIAN_POINT('Ctrl Pts',(56.02522746143,30.7120931189279,14.9393431915314));
#48536=CARTESIAN_POINT('Ctrl Pts',(56.0743057259755,30.6817320689865,14.9354426665937));
#48537=CARTESIAN_POINT('Ctrl Pts',(56.1299361369377,30.6438868393105,14.9310328157275));
#48538=CARTESIAN_POINT('Ctrl Pts',(56.1378300131961,30.6384329354282,14.9304073600285));
#48539=CARTESIAN_POINT('Ctrl Pts',(56.1498897723805,30.6299716146594,14.9294526632382));
#48540=CARTESIAN_POINT('Ctrl Pts',(56.1540837705836,30.6270047956683,14.9291208068982));
#48541=CARTESIAN_POINT('Ctrl Pts',(56.1617683302979,30.6215241014703,14.9285131135054));
#48542=CARTESIAN_POINT('Ctrl Pts',(56.1652622123637,30.6190151457151,14.928236962584));
#48543=CARTESIAN_POINT('Ctrl Pts',(56.1731119339761,30.6133396887155,14.9276168401683));
#48544=CARTESIAN_POINT('Ctrl Pts',(56.1774630757785,30.6101668446562,14.9272733084638));
#48545=CARTESIAN_POINT('Ctrl Pts',(56.1902208486627,30.6007845327608,14.9262664887576));
#48546=CARTESIAN_POINT('Ctrl Pts',(56.1985917433874,30.5945264603346,14.9256064295306));
#48547=CARTESIAN_POINT('Ctrl Pts',(56.2640150478082,30.5448097249438,14.9204487135644));
#48548=CARTESIAN_POINT('Ctrl Pts',(56.318741931028,30.4983635156922,14.916139683763));
#48549=CARTESIAN_POINT('Ctrl Pts',(56.4978979214821,30.3288772682684,14.9015893367329));
#48550=CARTESIAN_POINT('Ctrl Pts',(56.6085814031798,30.1925102403982,14.891723002521));
#48551=CARTESIAN_POINT('Ctrl Pts',(56.722676280292,30.0066191030003,14.8785112448309));
#48552=CARTESIAN_POINT('Ctrl Pts',(56.7440804584488,29.9690606385643,14.8758572313731));
#48553=CARTESIAN_POINT('Ctrl Pts',(56.770387149474,29.9192007653189,14.87233846652));
#48554=CARTESIAN_POINT('Ctrl Pts',(56.7764120171962,29.9075026380439,14.8715132401188));
#48555=CARTESIAN_POINT('Ctrl Pts',(56.7860668617947,29.8882918027939,14.8701582055884));
#48556=CARTESIAN_POINT('Ctrl Pts',(56.7897662804536,29.8808142935112,14.8696308211571));
#48557=CARTESIAN_POINT('Ctrl Pts',(56.7968271033006,29.866314339404,14.8686081224534));
#48558=CARTESIAN_POINT('Ctrl Pts',(56.8001945202945,29.8592949785211,14.8681130274366));
#48559=CARTESIAN_POINT('Ctrl Pts',(56.8078698867733,29.8430525820942,14.866967290632));
#48560=CARTESIAN_POINT('Ctrl Pts',(56.8121484703279,29.8338159862046,14.8663156563821));
#48561=CARTESIAN_POINT('Ctrl Pts',(56.8257232313318,29.8039127854338,14.8642054954654));
#48562=CARTESIAN_POINT('Ctrl Pts',(56.8347377230418,29.7831210007921,14.8627374827386));
#48563=CARTESIAN_POINT('Ctrl Pts',(56.9084418751415,29.6048615727444,14.8501397812045));
#48564=CARTESIAN_POINT('Ctrl Pts',(56.9530696874973,29.4398905981779,14.8383145967836));
#48565=CARTESIAN_POINT('Ctrl Pts',(56.990086119627,29.1702572158588,14.8193602346738));
#48566=CARTESIAN_POINT('Ctrl Pts',(56.9961894599312,29.0682839503516,14.8122975621214));
#48567=CARTESIAN_POINT('Ctrl Pts',(56.994269453784,28.9547150492043,14.8048267434208));
#48568=CARTESIAN_POINT('Ctrl Pts',(56.9939732964893,28.943150293604,14.8040706430821));
#48569=CARTESIAN_POINT('Ctrl Pts',(56.9933865923527,28.9260531873612,14.8029603609363));
#48570=CARTESIAN_POINT('Ctrl Pts',(56.9931735891566,28.9205186629455,14.8026021164631));
#48571=CARTESIAN_POINT('Ctrl Pts',(56.9927554370513,28.9107162610247,14.8019697674695));
#48572=CARTESIAN_POINT('Ctrl Pts',(56.9925596248488,28.9064480862396,14.8016951563733));
#48573=CARTESIAN_POINT('Ctrl Pts',(56.9921047054893,28.8971824680362,14.8011006065749));
#48574=CARTESIAN_POINT('Ctrl Pts',(56.9918405076977,28.8921853640459,14.8007809519491));
#48575=CARTESIAN_POINT('Ctrl Pts',(56.9910633811949,28.8784659977468,14.7999059583668));
#48576=CARTESIAN_POINT('Ctrl Pts',(56.9905119389645,28.8697459056586,14.7993527026527));
#48577=CARTESIAN_POINT('Ctrl Pts',(56.9873980599879,28.8251586075112,14.7965373413393));
#48578=CARTESIAN_POINT('Ctrl Pts',(56.9839232481805,28.789359360743,14.7943216636943));
#48579=CARTESIAN_POINT('Ctrl Pts',(56.9570975552413,28.5737898798137,14.7811460681651));
#48580=CARTESIAN_POINT('Ctrl Pts',(56.9102979242465,28.3977864552719,14.7710179168197));
#48581=CARTESIAN_POINT('Ctrl Pts',(56.8128589983795,28.1647445950081,14.7560057494288));
#48582=CARTESIAN_POINT('Ctrl Pts',(56.7818567324052,28.1005033283168,14.7516908206727));
#48583=CARTESIAN_POINT('Ctrl Pts',(56.7400643474081,28.0245819070587,14.7462981885722));
#48584=CARTESIAN_POINT('Ctrl Pts',(56.7324875679599,28.0111869765984,14.7453353145438));
#48585=CARTESIAN_POINT('Ctrl Pts',(56.7203197491604,27.9902448185969,14.7438111552698));
#48586=CARTESIAN_POINT('Ctrl Pts',(56.7158321648822,27.9826379485921,14.743253579194));
#48587=CARTESIAN_POINT('Ctrl Pts',(56.707347649005,27.9684717332072,14.742207669382));
#48588=CARTESIAN_POINT('Ctrl Pts',(56.7033630471215,27.9619051648476,14.7417197888606));
#48589=CARTESIAN_POINT('Ctrl Pts',(56.694382684137,27.9472965695562,14.7406274589596));
#48590=CARTESIAN_POINT('Ctrl Pts',(56.6893674205685,27.9392668073359,14.7400223050317));
#48591=CARTESIAN_POINT('Ctrl Pts',(56.6765342626566,27.9190419694735,14.7384858723168));
#48592=CARTESIAN_POINT('Ctrl Pts',(56.6686404410841,27.9068959529194,14.7375518152628));
#48593=CARTESIAN_POINT('Ctrl Pts',(56.6210719546175,27.8354196463711,14.731986339785));
#48594=CARTESIAN_POINT('Ctrl Pts',(56.5783728242281,27.7781739700948,14.7272423631001));
#48595=CARTESIAN_POINT('Ctrl Pts',(56.4283787549943,27.5980969860731,14.7113443557333));
#48596=CARTESIAN_POINT('Ctrl Pts',(56.3091114502449,27.4861254197318,14.6997853696989));
#48597=CARTESIAN_POINT('Ctrl Pts',(56.1356396186382,27.3592538635945,14.6850801299537));
#48598=CARTESIAN_POINT('Ctrl Pts',(56.092530704955,27.3302386652636,14.6815793239745));
#48599=CARTESIAN_POINT('Ctrl Pts',(56.0403740439414,27.2980196950469,14.6775630778841));
#48600=CARTESIAN_POINT('Ctrl Pts',(56.0323790324984,27.2931582817371,14.6769533273823));
#48601=CARTESIAN_POINT('Ctrl Pts',(56.0199853427721,27.2857411702807,14.6760175170521));
#48602=CARTESIAN_POINT('Ctrl Pts',(56.0156107266987,27.2831458163414,14.6756889969856));
#48603=CARTESIAN_POINT('Ctrl Pts',(56.0075154551249,27.2783848565416,14.6750844408483));
#48604=CARTESIAN_POINT('Ctrl Pts',(56.0037977354804,27.2762145721247,14.6748081142109));
#48605=CARTESIAN_POINT('Ctrl Pts',(55.99535933784,27.2713250657538,14.6741838596373));
#48606=CARTESIAN_POINT('Ctrl Pts',(55.9906345346999,27.2686131396879,14.673836398588));
#48607=CARTESIAN_POINT('Ctrl Pts',(55.978371738512,27.2616412135329,14.6729397845214));
#48608=CARTESIAN_POINT('Ctrl Pts',(55.9708169210206,27.257410822533,14.6723924523817));
#48609=CARTESIAN_POINT('Ctrl Pts',(55.9216739961126,27.2303115716273,14.6688631748919));
#48610=CARTESIAN_POINT('Ctrl Pts',(55.8793049003513,27.2088819757356,14.6659636077121));
#48611=CARTESIAN_POINT('Ctrl Pts',(55.8193476125214,27.1811976653523,14.6620007681012));
#48612=CARTESIAN_POINT('Ctrl Pts',(55.802378914537,27.1736482946895,14.6608944315436));
#48613=CARTESIAN_POINT('Ctrl Pts',(55.6639361306865,27.1143571042289,14.6519720393256));
#48614=CARTESIAN_POINT('Ctrl Pts',(55.5377023741406,27.0745548605659,14.6444580527923));
#48615=CARTESIAN_POINT('Ctrl Pts',(55.3302621046573,27.0311585553832,14.6319688700782));
#48616=CARTESIAN_POINT('Ctrl Pts',(55.2511625191969,27.0195139544978,14.6271798609614));
#48617=CARTESIAN_POINT('Ctrl Pts',(55.1507973913819,27.0108486752994,14.6209522199962));
#48618=CARTESIAN_POINT('Ctrl Pts',(55.1299850358691,27.0093803262718,14.6196529582574));
#48619=CARTESIAN_POINT('Ctrl Pts',(55.0992133985729,27.0076939548044,14.617718768137));
#48620=CARTESIAN_POINT('Ctrl Pts',(55.08926893795,27.0072236133591,14.6170916676523));
#48621=CARTESIAN_POINT('Ctrl Pts',(55.071598864522,27.006520404196,14.6159736114701));
#48622=CARTESIAN_POINT('Ctrl Pts',(55.0638745826813,27.0062579576968,14.6154835845938));
#48623=CARTESIAN_POINT('Ctrl Pts',(55.0476260098276,27.0058004047641,14.6144500005336));
#48624=CARTESIAN_POINT('Ctrl Pts',(55.039101621038,27.005615051705,14.6139061503018));
#48625=CARTESIAN_POINT('Ctrl Pts',(55.0165822687428,27.0052698245226,14.6124650602729));
#48626=CARTESIAN_POINT('Ctrl Pts',(55.002586557658,27.0052025822507,14.6115649664495));
#48627=CARTESIAN_POINT('Ctrl Pts',(54.9423175960707,27.0055472793374,14.60766900895));
#48628=CARTESIAN_POINT('Ctrl Pts',(54.8960702830593,27.0074220349251,14.6046283759));
#48629=CARTESIAN_POINT('Ctrl Pts',(54.6809195074619,27.0236540446459,14.5902348815082));
#48630=CARTESIAN_POINT('Ctrl Pts',(54.5142360685767,27.0578948832675,14.5782882415939));
#48631=CARTESIAN_POINT('Ctrl Pts',(54.3066928393707,27.1289454451837,14.5631209403966));
#48632=CARTESIAN_POINT('Ctrl Pts',(54.2600803563821,27.1468838258741,14.5597009203411));
#48633=CARTESIAN_POINT('Ctrl Pts',(54.1973096322782,27.1737872746396,14.5551176632957));
#48634=CARTESIAN_POINT('Ctrl Pts',(54.1805320085016,27.1812540014247,14.5538949244316));
#48635=CARTESIAN_POINT('Ctrl Pts',(54.1518227375656,27.1945087500848,14.5518094447632));
#48636=CARTESIAN_POINT('Ctrl Pts',(54.1398415253075,27.2001859143369,14.550941194762));
#48637=CARTESIAN_POINT('Ctrl Pts',(54.1226532505167,27.2085412359049,14.5496995451603));
#48638=CARTESIAN_POINT('Ctrl Pts',(54.1174002805988,27.2111233805302,14.549320616206));
#48639=CARTESIAN_POINT('Ctrl Pts',(54.108264524747,27.2156641808923,14.5486626326446));
#48640=CARTESIAN_POINT('Ctrl Pts',(54.1043766705967,27.2176124645689,14.5483829491101));
#48641=CARTESIAN_POINT('Ctrl Pts',(54.0961799444754,27.2217536044502,14.5477940257345));
#48642=CARTESIAN_POINT('Ctrl Pts',(54.0918726588997,27.2239494180637,14.5474849721714));
#48643=CARTESIAN_POINT('Ctrl Pts',(54.0802783229576,27.2299133080003,14.5466540801106));
#48644=CARTESIAN_POINT('Ctrl Pts',(54.0730063696024,27.23371076119,14.5461340336098));
#48645=CARTESIAN_POINT('Ctrl Pts',(54.0401312137691,27.2511373024455,14.5437870080365));
#48646=CARTESIAN_POINT('Ctrl Pts',(54.0148022803011,27.2652797114822,14.5419897966795));
#48647=CARTESIAN_POINT('Ctrl Pts',(53.8105682327205,27.3852307943931,14.5275153567077));
#48648=CARTESIAN_POINT('Ctrl Pts',(53.6488833095392,27.5178618052388,14.5160367210116));
#48649=CARTESIAN_POINT('Ctrl Pts',(53.4739728698963,27.7141933839252,14.5002475205211));
#48650=CARTESIAN_POINT('Ctrl Pts',(53.4390770486406,27.7567879622548,14.4968884947703));
#48651=CARTESIAN_POINT('Ctrl Pts',(53.3974142753498,27.8121658395127,14.4925697712738));
#48652=CARTESIAN_POINT('Ctrl Pts',(53.3889620749612,27.8236549038843,14.4916763415755));
#48653=CARTESIAN_POINT('Ctrl Pts',(53.3756209184998,27.8422030106943,14.4902375384475));
#48654=CARTESIAN_POINT('Ctrl Pts',(53.3706529698515,27.8492048312158,14.4896951978067));
#48655=CARTESIAN_POINT('Ctrl Pts',(53.3613063049198,27.8625598609991,14.4886621558874));
#48656=CARTESIAN_POINT('Ctrl Pts',(53.3569189387276,27.8689068475726,14.4881717949501));
#48657=CARTESIAN_POINT('Ctrl Pts',(53.3470163653832,27.8834116105564,14.4870524304576));
#48658=CARTESIAN_POINT('Ctrl Pts',(53.3415245540366,27.8915850428766,14.4864225641524));
#48659=CARTESIAN_POINT('Ctrl Pts',(53.3274149942888,27.9129238532495,14.4847802759296));
#48660=CARTESIAN_POINT('Ctrl Pts',(53.3188922402634,27.9261509291702,14.4837643729607));
#48661=CARTESIAN_POINT('Ctrl Pts',(53.2398224855917,28.0521135241842,14.474107398011));
#48662=CARTESIAN_POINT('Ctrl Pts',(53.1805722656838,28.1715168978081,14.4650506855469));
#48663=CARTESIAN_POINT('Ctrl Pts',(53.0959067780878,28.3959401859881,14.4483853649842));
#48664=CARTESIAN_POINT('Ctrl Pts',(53.066270254425,28.4988515215815,14.4408763443914));
#48665=CARTESIAN_POINT('Ctrl Pts',(53.0361616183748,28.6473587463756,14.4305583528831));
#48666=CARTESIAN_POINT('Ctrl Pts',(53.0287668261489,28.691361855593,14.4275653105527));
#48667=CARTESIAN_POINT('Ctrl Pts',(53.0216615227814,28.7444902083758,14.4240563189061));
#48668=CARTESIAN_POINT('Ctrl Pts',(53.0205300394347,28.7534091109344,14.4234707796412));
#48669=CARTESIAN_POINT('Ctrl Pts',(53.0188622654596,28.7673072562234,14.4225641552479));
#48670=CARTESIAN_POINT('Ctrl Pts',(53.0182843774749,28.772281250233,14.4222408408804));
#48671=CARTESIAN_POINT('Ctrl Pts',(53.0172435746198,28.7815437692101,14.4216409861906));
#48672=CARTESIAN_POINT('Ctrl Pts',(53.0167758427499,28.7858315855335,14.4213641922033));
#48673=CARTESIAN_POINT('Ctrl Pts',(53.0157374101552,28.7956463645899,14.4207326196536));
#48674=CARTESIAN_POINT('Ctrl Pts',(53.0151758913133,28.80117421414,14.4203783546339));
#48675=CARTESIAN_POINT('Ctrl Pts',(53.0137635028851,28.8156810281445,14.4194522778057));
#48676=CARTESIAN_POINT('Ctrl Pts',(53.0129504080065,28.8246636604479,14.4188824905126));
#48677=CARTESIAN_POINT('Ctrl Pts',(53.0076044433637,28.8885459938445,14.4148541971869));
#48678=CARTESIAN_POINT('Ctrl Pts',(53.0052860625162,28.9436125615935,14.4115069438421));
#48679=CARTESIAN_POINT('Ctrl Pts',(53.0051882323728,29.0948294972808,14.4024882069693));
#48680=CARTESIAN_POINT('Ctrl Pts',(53.0120736301616,29.1908332932345,14.3969496620502));
#48681=CARTESIAN_POINT('Ctrl Pts',(53.0316091386433,29.3256930481689,14.3890273030344));
#48682=CARTESIAN_POINT('Ctrl Pts',(53.0385576087489,29.3652105038048,14.386688994918));
#48683=CARTESIAN_POINT('Ctrl Pts',(53.0466870452705,29.4044701019679,14.3843322575863));
#48684=CARTESIAN_POINT('',(53.0052501615731,28.9991971327588,14.249733584776));
#48685=CARTESIAN_POINT('Ctrl Pts',(53.0466869970968,29.404469869322,14.2242573078582));
#48686=CARTESIAN_POINT('Ctrl Pts',(53.040725367752,29.375679274519,14.2260104549135));
#48687=CARTESIAN_POINT('Ctrl Pts',(53.0353967871213,29.3467400824718,14.2277788712771));
#48688=CARTESIAN_POINT('Ctrl Pts',(53.0243618871024,29.2783333519043,14.231984850153));
#48689=CARTESIAN_POINT('Ctrl Pts',(53.019196515761,29.2388150623199,14.2344347376859));
#48690=CARTESIAN_POINT('Ctrl Pts',(53.0138972638999,29.1860067588108,14.2377471311623));
#48691=CARTESIAN_POINT('Ctrl Pts',(53.0127073123571,29.1728304169053,14.2385767742036));
#48692=CARTESIAN_POINT('Ctrl Pts',(53.0109796151204,29.1513120324257,14.2399372250438));
#48693=CARTESIAN_POINT('Ctrl Pts',(53.0103630697111,29.1429765883835,14.2404655713147));
#48694=CARTESIAN_POINT('Ctrl Pts',(53.0092998729139,29.1272605095596,14.2414644008461));
#48695=CARTESIAN_POINT('Ctrl Pts',(53.0088418363709,29.1198807669603,14.2419345208487));
#48696=CARTESIAN_POINT('Ctrl Pts',(53.0079989932211,29.1049598385266,14.2428873418051));
#48697=CARTESIAN_POINT('Ctrl Pts',(53.0076159563652,29.09741867791,14.2433700899416));
#48698=CARTESIAN_POINT('Ctrl Pts',(53.0066687223206,29.0764165808719,14.244717925102));
#48699=CARTESIAN_POINT('Ctrl Pts',(53.0061980781166,29.0629520294684,14.2455858999131));
#48700=CARTESIAN_POINT('Ctrl Pts',(53.005447988207,29.0327244597251,14.2475434846741));
#48701=CARTESIAN_POINT('Ctrl Pts',(53.0052434143432,29.0159608454436,14.2486353362988));
#48702=CARTESIAN_POINT('Ctrl Pts',(53.0052501615731,28.9991971327588,14.249733584776));
#48703=CARTESIAN_POINT('Ctrl Pts',(53.0052501609099,28.9991987822212,14.2497334767141));
#48704=CARTESIAN_POINT('Ctrl Pts',(53.0053246644065,28.8137113382107,14.2618853925284));
#48705=CARTESIAN_POINT('Ctrl Pts',(53.0312721441039,28.6291575593077,14.2748853711652));
#48706=CARTESIAN_POINT('Ctrl Pts',(53.1040908771866,28.3748505603294,14.2932407346553));
#48707=CARTESIAN_POINT('Ctrl Pts',(53.1303690160143,28.3001672407954,14.2986699861498));
#48708=CARTESIAN_POINT('Ctrl Pts',(53.1663243404648,28.2146027170922,14.3047952468782));
#48709=CARTESIAN_POINT('Ctrl Pts',(53.1717628123662,28.2020249835474,14.305693077749));
#48710=CARTESIAN_POINT('Ctrl Pts',(53.1797408127415,28.1840838033772,14.3069690547199));
#48711=CARTESIAN_POINT('Ctrl Pts',(53.1821751904497,28.1786744173794,14.3073531513019));
#48712=CARTESIAN_POINT('Ctrl Pts',(53.1864408348969,28.1693076805571,14.3080170638155));
#48713=CARTESIAN_POINT('Ctrl Pts',(53.1882610004978,28.1653453564037,14.3082975427918));
#48714=CARTESIAN_POINT('Ctrl Pts',(53.1918573983875,28.1575835444411,14.3088462156829));
#48715=CARTESIAN_POINT('Ctrl Pts',(53.1936326222042,28.1537836862946,14.3091144716429));
#48716=CARTESIAN_POINT('Ctrl Pts',(53.1985749526546,28.1432910740531,14.3098543151022));
#48717=CARTESIAN_POINT('Ctrl Pts',(53.2017673977033,28.1366102287286,14.3103243759331));
#48718=CARTESIAN_POINT('Ctrl Pts',(53.2146432621076,28.1100460769859,14.3121899812013));
#48719=CARTESIAN_POINT('Ctrl Pts',(53.2246202659834,28.090305786585,14.3135686415586));
#48720=CARTESIAN_POINT('Ctrl Pts',(53.3354139651265,27.8798607475237,14.3282262007319));
#48721=CARTESIAN_POINT('Ctrl Pts',(53.4662080156965,27.7065280515995,14.3400863159308));
#48722=CARTESIAN_POINT('Ctrl Pts',(53.6487888635769,27.5321433858319,14.3552415069585));
#48723=CARTESIAN_POINT('Ctrl Pts',(53.6760230284697,27.5075324732154,14.3574683069494));
#48724=CARTESIAN_POINT('Ctrl Pts',(53.7174944090601,27.4720844625924,14.3608225240116));
#48725=CARTESIAN_POINT('Ctrl Pts',(53.7312242632586,27.4606642409316,14.3619272588977));
#48726=CARTESIAN_POINT('Ctrl Pts',(53.7534974503018,27.4426382840054,14.3637115088071));
#48727=CARTESIAN_POINT('Ctrl Pts',(53.7619444950756,27.435914746434,14.3643863979676));
#48728=CARTESIAN_POINT('Ctrl Pts',(53.777834958953,27.4234759005362,14.3656529456451));
#48729=CARTESIAN_POINT('Ctrl Pts',(53.7852649646029,27.4177438852326,14.366243930374));
#48730=CARTESIAN_POINT('Ctrl Pts',(53.7987118637462,27.4075205663011,14.3673114594031));
#48731=CARTESIAN_POINT('Ctrl Pts',(53.8047142283885,27.4030103773841,14.3677872559044));
#48732=CARTESIAN_POINT('Ctrl Pts',(53.8174100215412,27.3935824046972,14.3687921926577));
#48733=CARTESIAN_POINT('Ctrl Pts',(53.824108975014,27.3886723357454,14.3693216184123));
#48734=CARTESIAN_POINT('Ctrl Pts',(53.8413625459517,27.3761910414697,14.3706831822829));
#48735=CARTESIAN_POINT('Ctrl Pts',(53.8519606769851,27.3686809069383,14.3715176305469));
#48736=CARTESIAN_POINT('Ctrl Pts',(53.8937067553167,27.3397067435328,14.3747976821944));
#48737=CARTESIAN_POINT('Ctrl Pts',(53.9253876418756,27.319028138314,14.3772723654842));
#48738=CARTESIAN_POINT('Ctrl Pts',(54.1275229559937,27.195141398671,14.3929823955489));
#48739=CARTESIAN_POINT('Ctrl Pts',(54.3120421664303,27.1170725062956,14.4071372283339));
#48740=CARTESIAN_POINT('Ctrl Pts',(54.5583117727563,27.0539865963618,14.4245638823944));
#48741=CARTESIAN_POINT('Ctrl Pts',(54.6121753874919,27.0425399306265,14.4282802423395));
#48742=CARTESIAN_POINT('Ctrl Pts',(54.6758045606403,27.0317482541399,14.4325093229748));
#48743=CARTESIAN_POINT('Ctrl Pts',(54.6851721342161,27.0302281752847,14.4331278668094));
#48744=CARTESIAN_POINT('Ctrl Pts',(54.6996050249004,27.0279917383704,14.4340742560793));
#48745=CARTESIAN_POINT('Ctrl Pts',(54.704662693833,27.0272279396747,14.4344046480424));
#48746=CARTESIAN_POINT('Ctrl Pts',(54.7139802870532,27.0258574519073,14.4350109532414));
#48747=CARTESIAN_POINT('Ctrl Pts',(54.7182392201102,27.0252450937009,14.4352871701495));
#48748=CARTESIAN_POINT('Ctrl Pts',(54.7278595110274,27.0238936249648,14.4359090563574));
#48749=CARTESIAN_POINT('Ctrl Pts',(54.7332219071396,27.0231625504315,14.4362542742205));
#48750=CARTESIAN_POINT('Ctrl Pts',(54.7490728202296,27.0210672117067,14.4372706869758));
#48751=CARTESIAN_POINT('Ctrl Pts',(54.7595694807707,27.0197645071737,14.4379385604191));
#48752=CARTESIAN_POINT('Ctrl Pts',(54.868931029553,27.0070744290167,14.4448474175373));
#48753=CARTESIAN_POINT('Ctrl Pts',(54.9685201262177,27.0030157942425,14.450721636958));
#48754=CARTESIAN_POINT('Ctrl Pts',(55.1716179412225,27.009944127616,14.4625753700099));
#48755=CARTESIAN_POINT('Ctrl Pts',(55.2747921886321,27.0215501178099,14.4685348556598));
#48756=CARTESIAN_POINT('Ctrl Pts',(55.4292858191351,27.0512516705974,14.4778352207209));
#48757=CARTESIAN_POINT('Ctrl Pts',(55.4815419551017,27.0635023678334,14.4810465237869));
#48758=CARTESIAN_POINT('Ctrl Pts',(55.5556634637849,27.0840649084069,14.4857385798045));
#48759=CARTESIAN_POINT('Ctrl Pts',(55.5779774706556,27.0906778329818,14.4871691596413));
#48760=CARTESIAN_POINT('Ctrl Pts',(55.6176548622142,27.103195797205,14.4897485847687));
#48761=CARTESIAN_POINT('Ctrl Pts',(55.6350623518291,27.1089528067584,14.4908926849355));
#48762=CARTESIAN_POINT('Ctrl Pts',(55.6613228049286,27.118041150515,14.4926386631151));
#48763=CARTESIAN_POINT('Ctrl Pts',(55.6702358105484,27.1211969457125,14.4932347894402));
#48764=CARTESIAN_POINT('Ctrl Pts',(55.6863472835309,27.1270307119562,14.4943189270248));
#48765=CARTESIAN_POINT('Ctrl Pts',(55.6935534003728,27.1296871315962,14.4948062186628));
#48766=CARTESIAN_POINT('Ctrl Pts',(55.7090214788684,27.1354908771771,14.4958574438798));
#48767=CARTESIAN_POINT('Ctrl Pts',(55.7172781907303,27.1386516393852,14.4964218152924));
#48768=CARTESIAN_POINT('Ctrl Pts',(55.73951709598,27.1473348862068,14.4979508167069));
#48769=CARTESIAN_POINT('Ctrl Pts',(55.7534580969242,27.1529606298484,14.4989188715005));
#48770=CARTESIAN_POINT('Ctrl Pts',(55.8219923878431,27.1815219284064,14.5037262846639));
#48771=CARTESIAN_POINT('Ctrl Pts',(55.8756042850608,27.2067209030127,14.5076411152743));
#48772=CARTESIAN_POINT('Ctrl Pts',(56.0482596555304,27.2974628405327,14.520772528181));
#48773=CARTESIAN_POINT('Ctrl Pts',(56.1617265122295,27.3727739338602,14.5302875380155));
#48774=CARTESIAN_POINT('Ctrl Pts',(56.330718030919,27.5116801609606,14.5454914255561));
#48775=CARTESIAN_POINT('Ctrl Pts',(56.3914499721474,27.5682960389631,14.5512045018767));
#48776=CARTESIAN_POINT('Ctrl Pts',(56.4593854929884,27.6400467315979,14.557745936076));
#48777=CARTESIAN_POINT('Ctrl Pts',(56.4701484411296,27.6516890165338,14.5587870933634));
#48778=CARTESIAN_POINT('Ctrl Pts',(56.4849856181495,27.6681273231459,14.5602276376931));
#48779=CARTESIAN_POINT('Ctrl Pts',(56.4891773707381,27.6728158098745,14.5606352162866));
#48780=CARTESIAN_POINT('Ctrl Pts',(56.49627850638,27.6808344508043,14.5613265935474));
#48781=CARTESIAN_POINT('Ctrl Pts',(56.4991990986591,27.684154576377,14.561611211378));
#48782=CARTESIAN_POINT('Ctrl Pts',(56.504801347771,27.6905660715276,14.5621576310641));
#48783=CARTESIAN_POINT('Ctrl Pts',(56.5074845491426,27.6936560008499,14.5624195530706));
#48784=CARTESIAN_POINT('Ctrl Pts',(56.5139107807156,27.7011025060543,14.5630474306968));
#48785=CARTESIAN_POINT('Ctrl Pts',(56.5176445666459,27.7054670637592,14.5634127171132));
#48786=CARTESIAN_POINT('Ctrl Pts',(56.5312236968103,27.7214797000593,14.5647432072247));
#48787=CARTESIAN_POINT('Ctrl Pts',(56.5409545136199,27.733224808045,14.5657005286848));
#48788=CARTESIAN_POINT('Ctrl Pts',(56.6342286097396,27.8484721863339,14.5749281809192));
#48789=CARTESIAN_POINT('Ctrl Pts',(56.707368598885,27.9599893859013,14.5825857304154));
#48790=CARTESIAN_POINT('Ctrl Pts',(56.8340411388648,28.2030047558217,14.5985027339655));
#48791=CARTESIAN_POINT('Ctrl Pts',(56.8857658330866,28.3345765345478,14.6067412839686));
#48792=CARTESIAN_POINT('Ctrl Pts',(56.9279053956793,28.4876287967668,14.616589803726));
#48793=CARTESIAN_POINT('Ctrl Pts',(56.9323940524154,28.5048266373916,14.6176994434686));
#48794=CARTESIAN_POINT('Ctrl Pts',(56.9388898675969,28.531149412194,14.6194033927348));
#48795=CARTESIAN_POINT('Ctrl Pts',(56.9410638034397,28.540232560335,14.6199923703701));
#48796=CARTESIAN_POINT('Ctrl Pts',(56.9449075838716,28.5568059780862,14.621069000158));
#48797=CARTESIAN_POINT('Ctrl Pts',(56.9465981536306,28.5642912940174,14.6215559811152));
#48798=CARTESIAN_POINT('Ctrl Pts',(56.9501630308908,28.5805104216208,14.6226128199122));
#48799=CARTESIAN_POINT('Ctrl Pts',(56.9520219416241,28.5892474119579,14.623183155736));
#48800=CARTESIAN_POINT('Ctrl Pts',(56.9569323960075,28.6131132581165,14.6247440374216));
#48801=CARTESIAN_POINT('Ctrl Pts',(56.9598670916731,28.6282652632737,14.6257382528747));
#48802=CARTESIAN_POINT('Ctrl Pts',(56.9741944138705,28.7071297318096,14.6309309320337));
#48803=CARTESIAN_POINT('Ctrl Pts',(56.982655906263,28.771328660021,14.6352203386183));
#48804=CARTESIAN_POINT('Ctrl Pts',(57.0019543244248,29.0050041288652,14.6510615840544));
#48805=CARTESIAN_POINT('Ctrl Pts',(56.9942720472674,29.1752527466829,14.6631062258711));
#48806=CARTESIAN_POINT('Ctrl Pts',(56.9560955699289,29.3943209878762,14.6783280036037));
#48807=CARTESIAN_POINT('Ctrl Pts',(56.9450072694434,29.445810169866,14.6818777778332));
#48808=CARTESIAN_POINT('Ctrl Pts',(56.9295553825495,29.5058969481292,14.6859424971687));
#48809=CARTESIAN_POINT('Ctrl Pts',(56.9271530388352,29.5149726882374,14.6865543155088));
#48810=CARTESIAN_POINT('Ctrl Pts',(56.9233486493168,29.5289456268321,14.6874926144979));
#48811=CARTESIAN_POINT('Ctrl Pts',(56.9219918097328,29.5338548376574,14.6878215755629));
#48812=CARTESIAN_POINT('Ctrl Pts',(56.9194536113817,29.5429032359507,14.6884265409755));
#48813=CARTESIAN_POINT('Ctrl Pts',(56.9182776640426,29.5470437771399,14.6887028389852));
#48814=CARTESIAN_POINT('Ctrl Pts',(56.9155853791141,29.5564079453343,14.6893265232576));
#48815=CARTESIAN_POINT('Ctrl Pts',(56.914061075659,29.5616291896187,14.6896734463339));
#48816=CARTESIAN_POINT('Ctrl Pts',(56.9100630397513,29.5751184432691,14.6905677432495));
#48817=CARTESIAN_POINT('Ctrl Pts',(56.9075569439705,29.5833768519755,14.6911133117998));
#48818=CARTESIAN_POINT('Ctrl Pts',(56.891085870825,29.6364132728549,14.6946060667833));
#48819=CARTESIAN_POINT('Ctrl Pts',(56.8755975894105,29.6807070429271,14.6974728144533));
#48820=CARTESIAN_POINT('Ctrl Pts',(56.851433863643,29.7427013622904,14.7014673662404));
#48821=CARTESIAN_POINT('Ctrl Pts',(56.8440375626336,29.7608798654152,14.7026364426345));
#48822=CARTESIAN_POINT('Ctrl Pts',(56.8165545793273,29.8256712537723,14.7068048569867));
#48823=CARTESIAN_POINT('Ctrl Pts',(56.7949583681512,29.8716239774689,14.7097646614618));
#48824=CARTESIAN_POINT('Ctrl Pts',(56.7277345569171,30.0015414198841,14.7182687370513));
#48825=CARTESIAN_POINT('Ctrl Pts',(56.6778005400033,30.0831141937596,14.7237844735192));
#48826=CARTESIAN_POINT('Ctrl Pts',(56.593791004895,30.2005182071573,14.7323514863034));
#48827=CARTESIAN_POINT('Ctrl Pts',(56.5639169876408,30.2391839609559,14.73528577473));
#48828=CARTESIAN_POINT('Ctrl Pts',(56.5118993934418,30.3016295410715,14.7402533278628));
#48829=CARTESIAN_POINT('Ctrl Pts',(56.4905397403674,30.326035571464,14.7422571011955));
#48830=CARTESIAN_POINT('Ctrl Pts',(56.4605798585478,30.3586295807714,14.7450260981036));
#48831=CARTESIAN_POINT('Ctrl Pts',(56.4524867667053,30.3672783344635,14.7457701213043));
#48832=CARTESIAN_POINT('Ctrl Pts',(56.4387566114817,30.3816917061996,14.7470260632406));
#48833=CARTESIAN_POINT('Ctrl Pts',(56.4331606877759,30.3874952244938,14.7475362157439));
#48834=CARTESIAN_POINT('Ctrl Pts',(56.4220436102186,30.3988857095545,14.7485464149961));
#48835=CARTESIAN_POINT('Ctrl Pts',(56.4165243300478,30.4044743063722,14.7490463754638));
#48836=CARTESIAN_POINT('Ctrl Pts',(56.4042928118695,30.4167139974182,14.75015100402));
#48837=CARTESIAN_POINT('Ctrl Pts',(56.3975660605672,30.423350256699,14.7507563057259));
#48838=CARTESIAN_POINT('Ctrl Pts',(56.3737162199602,30.4465471860753,14.7528949600637));
#48839=CARTESIAN_POINT('Ctrl Pts',(56.3563444342309,30.4628481497572,14.7544393821512));
#48840=CARTESIAN_POINT('Ctrl Pts',(56.2213538722951,30.5850457478265,14.766345224979));
#48841=CARTESIAN_POINT('Ctrl Pts',(56.091819722919,30.6768978488232,14.777295261799));
#48842=CARTESIAN_POINT('Ctrl Pts',(55.8823443019209,30.7907911426206,14.7939126937327));
#48843=CARTESIAN_POINT('Ctrl Pts',(55.8096070013011,30.8248294247372,14.7994956919807));
#48844=CARTESIAN_POINT('Ctrl Pts',(55.712047432857,30.8634984069749,14.8066003386343));
#48845=CARTESIAN_POINT('Ctrl Pts',(55.6889132402556,30.8721742767818,14.8082576532146));
#48846=CARTESIAN_POINT('Ctrl Pts',(55.6499565973372,30.8859639884705,14.810996342969));
#48847=CARTESIAN_POINT('Ctrl Pts',(55.6342210924585,30.8913136686688,14.8120885510323));
#48848=CARTESIAN_POINT('Ctrl Pts',(55.6123282979792,30.8984527047916,14.8135870550372));
#48849=CARTESIAN_POINT('Ctrl Pts',(55.6062269937731,30.9004098114821,14.8140024204481));
#48850=CARTESIAN_POINT('Ctrl Pts',(55.5958776648937,30.9036746372742,14.8147030487002));
#48851=CARTESIAN_POINT('Ctrl Pts',(55.5916345383749,30.9049976090554,14.8149891831189));
#48852=CARTESIAN_POINT('Ctrl Pts',(55.5835017130842,30.9075035626529,14.815535437933));
#48853=CARTESIAN_POINT('Ctrl Pts',(55.5796127869433,30.9086888454212,14.8157956958974));
#48854=CARTESIAN_POINT('Ctrl Pts',(55.5692577525946,30.9118103285,14.8164862310585));
#48855=CARTESIAN_POINT('Ctrl Pts',(55.5627853258593,30.9137256337259,14.8169153115698));
#48856=CARTESIAN_POINT('Ctrl Pts',(55.5394624277458,30.9204987324453,14.8184527635663));
#48857=CARTESIAN_POINT('Ctrl Pts',(55.5225572277172,30.925167287593,14.8195508502358));
#48858=CARTESIAN_POINT('Ctrl Pts',(55.2914919004626,30.9857104175249,14.8343660863571));
#48859=CARTESIAN_POINT('Ctrl Pts',(55.0695206893635,31.0057952110265,14.846496059263));
#48860=CARTESIAN_POINT('Ctrl Pts',(54.8119480454818,30.9862090764469,14.8619981961419));
#48861=CARTESIAN_POINT('Ctrl Pts',(54.7752291828745,30.9823894354443,14.8642373229086));
#48862=CARTESIAN_POINT('Ctrl Pts',(54.7125864811099,30.9741103358519,14.8681217300302));
#48863=CARTESIAN_POINT('Ctrl Pts',(54.6866056030445,30.9701527862442,14.869751877021));
#48864=CARTESIAN_POINT('Ctrl Pts',(54.6499549078552,30.9638266585787,14.8720818428361));
#48865=CARTESIAN_POINT('Ctrl Pts',(54.6392140216405,30.9618817960723,14.8727683699272));
#48866=CARTESIAN_POINT('Ctrl Pts',(54.6207475921886,30.9583812880662,14.8739553091861));
#48867=CARTESIAN_POINT('Ctrl Pts',(54.6130142345525,30.9568678219887,14.8744543803629));
#48868=CARTESIAN_POINT('Ctrl Pts',(54.5982382282599,30.9538850521817,14.8754118726171));
#48869=CARTESIAN_POINT('Ctrl Pts',(54.5911941495911,30.9524233897456,14.8758700443441));
#48870=CARTESIAN_POINT('Ctrl Pts',(54.5746980224023,30.9489072198302,14.876947098327));
#48871=CARTESIAN_POINT('Ctrl Pts',(54.5652527704239,30.9468220166742,14.8775669473071));
#48872=CARTESIAN_POINT('Ctrl Pts',(54.5327938568077,30.939408157388,14.8797081708378));
#48873=CARTESIAN_POINT('Ctrl Pts',(54.5098606333127,30.9337396162421,14.8812402928767));
#48874=CARTESIAN_POINT('Ctrl Pts',(54.3382652637259,30.8880768436519,14.8928542988055));
#48875=CARTESIAN_POINT('Ctrl Pts',(54.1946057359321,30.8314065391958,14.9034896723543));
#48876=CARTESIAN_POINT('Ctrl Pts',(53.95550996692,30.7034737471099,14.9223898720556));
#48877=CARTESIAN_POINT('Ctrl Pts',(53.8571713263389,30.6391250578482,14.9305621243993));
#48878=CARTESIAN_POINT('Ctrl Pts',(53.7565545725706,30.5598038464128,14.9389783200573));
#48879=CARTESIAN_POINT('Ctrl Pts',(53.7481142292371,30.5530378616514,14.9396846612649));
#48880=CARTESIAN_POINT('Ctrl Pts',(53.7355510532793,30.5427979378009,14.9407360123452));
#48881=CARTESIAN_POINT('Ctrl Pts',(53.7313867463494,30.5393755324979,14.9410845003608));
#48882=CARTESIAN_POINT('Ctrl Pts',(53.7242434772513,30.5334562154517,14.941682201046));
#48883=CARTESIAN_POINT('Ctrl Pts',(53.7212578981565,30.5309674418176,14.9419319864272));
#48884=CARTESIAN_POINT('Ctrl Pts',(53.714476488922,30.5252807933089,14.9424992727809));
#48885=CARTESIAN_POINT('Ctrl Pts',(53.7106853119231,30.5220774725254,14.9428163734158));
#48886=CARTESIAN_POINT('Ctrl Pts',(53.7003885010503,30.5133111980925,14.9436776235038));
#48887=CARTESIAN_POINT('Ctrl Pts',(53.6939065657217,30.5077203910676,14.9442197957987));
#48888=CARTESIAN_POINT('Ctrl Pts',(53.6619900706613,30.4798314411295,14.9468906122155));
#48889=CARTESIAN_POINT('Ctrl Pts',(53.6370879056476,30.4569291686295,14.9489783049751));
#48890=CARTESIAN_POINT('Ctrl Pts',(53.4671678835173,30.2924836710184,14.96335221065));
#48891=CARTESIAN_POINT('Ctrl Pts',(53.3438682042306,30.130192216475,14.9745757778029));
#48892=CARTESIAN_POINT('Ctrl Pts',(53.2210529777984,29.9040795709367,14.9900312903674));
#48893=CARTESIAN_POINT('Ctrl Pts',(53.1969619226494,29.8550235447499,14.9933659389943));
#48894=CARTESIAN_POINT('Ctrl Pts',(53.1691731835517,29.7920247493577,14.9976571524138));
#48895=CARTESIAN_POINT('Ctrl Pts',(53.1635700945524,29.7789449411288,14.9985484981535));
#48896=CARTESIAN_POINT('Ctrl Pts',(53.1548144174318,29.757886077951,14.9999847391649));
#48897=CARTESIAN_POINT('Ctrl Pts',(53.151572468519,29.7499445302369,15.0005266210572));
#48898=CARTESIAN_POINT('Ctrl Pts',(53.1455112899721,29.7348188510598,15.0015593057555));
#48899=CARTESIAN_POINT('Ctrl Pts',(53.1426823269921,29.727638769101,15.0020497717463));
#48900=CARTESIAN_POINT('Ctrl Pts',(53.1363338799046,29.711247763869,15.0031700976402));
#48901=CARTESIAN_POINT('Ctrl Pts',(53.1328409068122,29.7020268540378,15.0038008258223));
#48902=CARTESIAN_POINT('Ctrl Pts',(53.1239363997985,29.6779837083138,15.0054468430742));
#48903=CARTESIAN_POINT('Ctrl Pts',(53.1186322052068,29.663122717046,15.0064656392795));
#48904=CARTESIAN_POINT('Ctrl Pts',(53.0860852110435,29.5683993679536,15.0129695959839));
#48905=CARTESIAN_POINT('Ctrl Pts',(53.0637744386948,29.4869905985863,15.0186105520578));
#48906=CARTESIAN_POINT('Ctrl Pts',(53.0466869327998,29.4044695588112,15.0243707259923));
#48907=CARTESIAN_POINT('Origin',(55.,29.,3.45145488139523));
#48908=CARTESIAN_POINT('',(53.0466870408509,29.4044700806242,15.9845144320741));
#48909=CARTESIAN_POINT('',(53.0466869980082,29.4044698737233,15.8273167122946));
#48910=CARTESIAN_POINT('',(53.0466869980082,29.4044698737233,3.45145488139523));
#48911=CARTESIAN_POINT('',(53.0052506493574,29.0017284253212,15.2092031079544));
#48912=CARTESIAN_POINT('Ctrl Pts',(53.0466870408509,29.4044700806242,15.9845144320741));
#48913=CARTESIAN_POINT('Ctrl Pts',(53.0534501350343,29.4371311849806,15.9822259750689));
#48914=CARTESIAN_POINT('Ctrl Pts',(53.0610339691148,29.4696302032199,15.9799208471347));
#48915=CARTESIAN_POINT('Ctrl Pts',(53.1040382957387,29.6350350901668,15.9680638067916));
#48916=CARTESIAN_POINT('Ctrl Pts',(53.1523155091381,29.7642026943096,15.9583574580738));
#48917=CARTESIAN_POINT('Ctrl Pts',(53.2238469535253,29.908211952473,15.9476090852829));
#48918=CARTESIAN_POINT('Ctrl Pts',(53.2345585205531,29.9288622557103,15.9460705215691));
#48919=CARTESIAN_POINT('Ctrl Pts',(53.2492230067567,29.9559626042592,15.9440595427439));
#48920=CARTESIAN_POINT('Ctrl Pts',(53.2528543757088,29.9625833744256,15.943568904757));
#48921=CARTESIAN_POINT('Ctrl Pts',(53.2588018968879,29.9732824469627,15.9427773021417));
#48922=CARTESIAN_POINT('Ctrl Pts',(53.2610949478323,29.9773734068887,15.9424749214682));
#48923=CARTESIAN_POINT('Ctrl Pts',(53.2655699058029,29.9852914376546,15.9418903069871));
#48924=CARTESIAN_POINT('Ctrl Pts',(53.2677500801846,29.9891193984707,15.9416079745063));
#48925=CARTESIAN_POINT('Ctrl Pts',(53.2730285419103,29.9983163678438,15.9409302996695));
#48926=CARTESIAN_POINT('Ctrl Pts',(53.2761392426007,30.0036782746023,15.9405357439184));
#48927=CARTESIAN_POINT('Ctrl Pts',(53.2870089281247,30.0222147109915,15.9391732866053));
#48928=CARTESIAN_POINT('Ctrl Pts',(53.2948945772483,30.0353148595139,15.938213124837));
#48929=CARTESIAN_POINT('Ctrl Pts',(53.343389813394,30.1138209627918,15.9324675225151));
#48930=CARTESIAN_POINT('Ctrl Pts',(53.3876118386438,30.1769288407111,15.9278833103945));
#48931=CARTESIAN_POINT('Ctrl Pts',(53.486728981154,30.3022642533455,15.9185110263194));
#48932=CARTESIAN_POINT('Ctrl Pts',(53.542074866669,30.3639413888214,15.913741320745));
#48933=CARTESIAN_POINT('Ctrl Pts',(53.6829839979068,30.5025619302817,15.9022121878352));
#48934=CARTESIAN_POINT('Ctrl Pts',(53.7716685449202,30.5758871146582,15.8954103428522));
#48935=CARTESIAN_POINT('Ctrl Pts',(53.8791629502807,30.6501519871727,15.8873025739885));
#48936=CARTESIAN_POINT('Ctrl Pts',(53.8922701190462,30.6589791322843,15.8863164312488));
#48937=CARTESIAN_POINT('Ctrl Pts',(53.9137297484089,30.6730636170399,15.8847051046488));
#48938=CARTESIAN_POINT('Ctrl Pts',(53.9220189414534,30.6784164435489,15.8840834696314));
#48939=CARTESIAN_POINT('Ctrl Pts',(53.9368620272109,30.687846196439,15.8829715330225));
#48940=CARTESIAN_POINT('Ctrl Pts',(53.9434005540701,30.6919470264057,15.8824821232514));
#48941=CARTESIAN_POINT('Ctrl Pts',(53.9572525233911,30.70052308865,15.8814460772464));
#48942=CARTESIAN_POINT('Ctrl Pts',(53.9645713334985,30.7049893101813,15.8808991251948));
#48943=CARTESIAN_POINT('Ctrl Pts',(53.9840974056889,30.7167327848268,15.8794409636563));
#48944=CARTESIAN_POINT('Ctrl Pts',(53.9963538553849,30.7239268936921,15.8785267777463));
#48945=CARTESIAN_POINT('Ctrl Pts',(54.0559112429152,30.7580346033474,15.8740889179072));
#48946=CARTESIAN_POINT('Ctrl Pts',(54.1042194388631,30.7831336168473,15.8705016855517));
#48947=CARTESIAN_POINT('Ctrl Pts',(54.3347580624309,30.891178503412,15.8534279706695));
#48948=CARTESIAN_POINT('Ctrl Pts',(54.5277408838768,30.9483460970599,15.8391144621655));
#48949=CARTESIAN_POINT('Ctrl Pts',(54.7618318124214,30.980811382159,15.8231176007144));
#48950=CARTESIAN_POINT('Ctrl Pts',(54.7978175241762,30.9848074088325,15.8207001693762));
#48951=CARTESIAN_POINT('Ctrl Pts',(54.8426205144947,30.9885512147939,15.8177577070384));
#48952=CARTESIAN_POINT('Ctrl Pts',(54.8513513611765,30.9892229199449,15.817187470535));
#48953=CARTESIAN_POINT('Ctrl Pts',(54.8650825849914,30.9901884175931,15.8162959156915));
#48954=CARTESIAN_POINT('Ctrl Pts',(54.8700800040111,30.9905208972444,15.8159725345064));
#48955=CARTESIAN_POINT('Ctrl Pts',(54.87934240885,30.9911020966014,15.815375264312));
#48956=CARTESIAN_POINT('Ctrl Pts',(54.8836069091706,30.9913559356111,15.8151011059494));
#48957=CARTESIAN_POINT('Ctrl Pts',(54.8933957273366,30.9919070501149,15.8144736724289));
#48958=CARTESIAN_POINT('Ctrl Pts',(54.8989204853775,30.9921950458559,15.8141209145496));
#48959=CARTESIAN_POINT('Ctrl Pts',(54.9159684543779,30.9930126250906,15.8130364009741));
#48960=CARTESIAN_POINT('Ctrl Pts',(54.9274953565567,30.993465253249,15.8123087558535));
#48961=CARTESIAN_POINT('Ctrl Pts',(55.0374492139618,30.9968278183815,15.805416124932));
#48962=CARTESIAN_POINT('Ctrl Pts',(55.1359744870044,30.9925461058079,15.7996054702781));
#48963=CARTESIAN_POINT('Ctrl Pts',(55.4071790849199,30.9605393757481,15.7836772705975));
#48964=CARTESIAN_POINT('Ctrl Pts',(55.5771099911548,30.9174066372552,15.7737027239332));
#48965=CARTESIAN_POINT('Ctrl Pts',(55.7598115976644,30.8445063784477,15.7615588943813));
#48966=CARTESIAN_POINT('Ctrl Pts',(55.7802302008728,30.8359624770948,15.7601818824313));
#48967=CARTESIAN_POINT('Ctrl Pts',(55.8097383194006,30.8230340387689,15.7581609173275));
#48968=CARTESIAN_POINT('Ctrl Pts',(55.8189438780761,30.8189173073606,15.7575259989864));
#48969=CARTESIAN_POINT('Ctrl Pts',(55.8351867585324,30.8115051803805,15.7563976322834));
#48970=CARTESIAN_POINT('Ctrl Pts',(55.8422368318634,30.8082381083408,15.7559051576322));
#48971=CARTESIAN_POINT('Ctrl Pts',(55.85685327556,30.8013606828087,15.7548783926994));
#48972=CARTESIAN_POINT('Ctrl Pts',(55.8644163210114,30.7977436596643,15.7543438807363));
#48973=CARTESIAN_POINT('Ctrl Pts',(55.8839589700011,30.7882455640918,15.7529542086075));
#48974=CARTESIAN_POINT('Ctrl Pts',(55.8959026011397,30.7822918316445,15.7520965508992));
#48975=CARTESIAN_POINT('Ctrl Pts',(55.9478661968136,30.7557344104761,15.748327764671));
#48976=CARTESIAN_POINT('Ctrl Pts',(55.9872392887986,30.7339007171338,15.7453740607433));
#48977=CARTESIAN_POINT('Ctrl Pts',(56.1613594710533,30.6294912511017,15.7318519517475));
#48978=CARTESIAN_POINT('Ctrl Pts',(56.2867291783249,30.5324199910015,15.7207727388125));
#48979=CARTESIAN_POINT('Ctrl Pts',(56.460691935294,30.3611849223542,15.703823897267));
#48980=CARTESIAN_POINT('Ctrl Pts',(56.518102047975,30.2968480913344,15.6979082115625));
#48981=CARTESIAN_POINT('Ctrl Pts',(56.5777142852303,30.2206382502073,15.6915534019287));
#48982=CARTESIAN_POINT('Ctrl Pts',(56.5841837717373,30.212230131959,15.6908606936952));
#48983=CARTESIAN_POINT('Ctrl Pts',(56.5938560517245,30.1994497951508,15.6898209049963));
#48984=CARTESIAN_POINT('Ctrl Pts',(56.5971084927256,30.1951156382712,15.6894705377689));
#48985=CARTESIAN_POINT('Ctrl Pts',(56.6029120278979,30.18731592684,15.6888441305743));
#48986=CARTESIAN_POINT('Ctrl Pts',(56.605469596442,30.1838553354578,15.6885676508327));
#48987=CARTESIAN_POINT('Ctrl Pts',(56.611039517791,30.1762675465147,15.6879645938516));
#48988=CARTESIAN_POINT('Ctrl Pts',(56.614047214767,30.1721370477773,15.6876383344927));
#48989=CARTESIAN_POINT('Ctrl Pts',(56.6225805559452,30.1603230022554,15.6867107748798));
#48990=CARTESIAN_POINT('Ctrl Pts',(56.6280675237954,30.1526115028084,15.6861120448344));
#48991=CARTESIAN_POINT('Ctrl Pts',(56.6647310587047,30.100299594614,15.6820934982729));
#48992=CARTESIAN_POINT('Ctrl Pts',(56.6941292149109,30.0544743047909,15.6787826600966));
#48993=CARTESIAN_POINT('Ctrl Pts',(56.8176808598636,29.8433488409794,15.6641769424767));
#48994=CARTESIAN_POINT('Ctrl Pts',(56.8897746777335,29.6663039204156,15.6535483530655));
#48995=CARTESIAN_POINT('Ctrl Pts',(56.9467241252387,29.4374617147852,15.6392995017148));
#48996=CARTESIAN_POINT('Ctrl Pts',(56.9562161822891,29.3928426336596,15.6365045817793));
#48997=CARTESIAN_POINT('Ctrl Pts',(56.9665989153019,29.3342306254704,15.6327932903754));
#48998=CARTESIAN_POINT('Ctrl Pts',(56.9688837792124,29.3204965727755,15.6319208657096));
#48999=CARTESIAN_POINT('Ctrl Pts',(56.9723333091103,29.2983308672023,15.6305078811102));
#49000=CARTESIAN_POINT('Ctrl Pts',(56.9735881319035,29.2899135570232,15.6299701606428));
#49001=CARTESIAN_POINT('Ctrl Pts',(56.9758802335732,29.2738332695984,15.6289406112517));
#49002=CARTESIAN_POINT('Ctrl Pts',(56.9769268937505,29.2661717697013,15.6284490866766));
#49003=CARTESIAN_POINT('Ctrl Pts',(56.9792231719078,29.248601956768,15.6273195320291));
#49004=CARTESIAN_POINT('Ctrl Pts',(56.9804429719575,29.2386900207149,15.6266805808522));
#49005=CARTESIAN_POINT('Ctrl Pts',(56.9839997451104,29.2078814544076,15.6246890254546));
#49006=CARTESIAN_POINT('Ctrl Pts',(56.9860807145653,29.1869572869407,15.6233284949867));
#49007=CARTESIAN_POINT('Ctrl Pts',(56.9945800824859,29.0851812835282,15.6166700943837));
#49008=CARTESIAN_POINT('Ctrl Pts',(56.996393345391,29.004031556856,15.6112319951362));
#49009=CARTESIAN_POINT('Ctrl Pts',(56.9880004560141,28.7867542701175,15.5963534135569));
#49010=CARTESIAN_POINT('Ctrl Pts',(56.9687821502761,28.6514132046081,15.5867284902775));
#49011=CARTESIAN_POINT('Ctrl Pts',(56.9330922752534,28.5077412321302,15.5765523338113));
#49012=CARTESIAN_POINT('Ctrl Pts',(56.9301718377433,28.4964117514736,15.575750404459));
#49013=CARTESIAN_POINT('Ctrl Pts',(56.9146388582822,28.4382744397134,15.5716399734323));
#49014=CARTESIAN_POINT('Ctrl Pts',(56.9004215788212,28.3919077080542,15.5683770756143));
#49015=CARTESIAN_POINT('Ctrl Pts',(56.8816726531832,28.3378735509759,15.5646279514439));
#49016=CARTESIAN_POINT('Ctrl Pts',(56.8787638608648,28.3296644348544,15.5640598538804));
#49017=CARTESIAN_POINT('Ctrl Pts',(56.8739430684001,28.3163372299478,15.5631402918558));
#49018=CARTESIAN_POINT('Ctrl Pts',(56.8720636785446,28.3112075842859,15.5627870123391));
#49019=CARTESIAN_POINT('Ctrl Pts',(56.8686653355209,28.3020487362003,15.5621575055048));
#49020=CARTESIAN_POINT('Ctrl Pts',(56.8671543920099,28.2980166808585,15.5618808189604));
#49021=CARTESIAN_POINT('Ctrl Pts',(56.8638342554452,28.2892432321268,15.5612797489023));
#49022=CARTESIAN_POINT('Ctrl Pts',(56.8620200237999,28.2845038454396,15.5609556673785));
#49023=CARTESIAN_POINT('Ctrl Pts',(56.8568292159944,28.2710971625509,15.5600405159956));
#49024=CARTESIAN_POINT('Ctrl Pts',(56.8534100218288,28.262446352638,15.5594519094221));
#49025=CARTESIAN_POINT('Ctrl Pts',(56.8309519575169,28.2067683237267,15.5556739162163));
#49026=CARTESIAN_POINT('Ctrl Pts',(56.8101835803972,28.1604537358058,15.5525790881391));
#49027=CARTESIAN_POINT('Ctrl Pts',(56.7199514788576,27.978192611782,15.5404008722918));
#49028=CARTESIAN_POINT('Ctrl Pts',(56.6367555386292,27.849625815281,15.5317757344369));
#49029=CARTESIAN_POINT('Ctrl Pts',(56.4875525998059,27.6684805830844,15.517916657112));
#49030=CARTESIAN_POINT('Ctrl Pts',(56.4315492555174,27.6084465321837,15.5129814421806));
#49031=CARTESIAN_POINT('Ctrl Pts',(56.3611385516219,27.5417291466275,15.506955369004));
#49032=CARTESIAN_POINT('Ctrl Pts',(56.3501473945844,27.5315470615806,15.5060195929095));
#49033=CARTESIAN_POINT('Ctrl Pts',(56.3319128979894,27.5150326173022,15.5044744510278));
#49034=CARTESIAN_POINT('Ctrl Pts',(56.3247364724658,27.5086270188727,15.5038681616673));
#49035=CARTESIAN_POINT('Ctrl Pts',(56.3117381518173,27.4971927065506,15.5027731176742));
#49036=CARTESIAN_POINT('Ctrl Pts',(56.3059329314384,27.4921452602886,15.5022851512732));
#49037=CARTESIAN_POINT('Ctrl Pts',(56.2934817572786,27.4814452182999,15.5012407892012));
#49038=CARTESIAN_POINT('Ctrl Pts',(56.2868276418939,27.4758024086326,15.5006840078356));
#49039=CARTESIAN_POINT('Ctrl Pts',(56.2687115359405,27.4606428144417,15.499171627257));
#49040=CARTESIAN_POINT('Ctrl Pts',(56.2571797806631,27.4512106387898,15.4982126490977));
#49041=CARTESIAN_POINT('Ctrl Pts',(56.1959274170714,27.4022452814668,15.4931372888402));
#49042=CARTESIAN_POINT('Ctrl Pts',(56.1444500015157,27.3649785179587,15.4889330350341));
#49043=CARTESIAN_POINT('Ctrl Pts',(55.9714154918429,27.2518906334691,15.4749868454011));
#49044=CARTESIAN_POINT('Ctrl Pts',(55.843464214561,27.1866897421248,15.4649205047184));
#49045=CARTESIAN_POINT('Ctrl Pts',(55.6353437436458,27.1074649680234,15.4494865270663));
#49046=CARTESIAN_POINT('Ctrl Pts',(55.5593948870377,27.0836412670851,15.4440426721734));
#49047=CARTESIAN_POINT('Ctrl Pts',(55.4720000030585,27.0618683069888,15.4381280082817));
#49048=CARTESIAN_POINT('Ctrl Pts',(55.4617611815757,27.0594034203216,15.4374404415707));
#49049=CARTESIAN_POINT('Ctrl Pts',(55.4462411529914,27.0557969296875,15.4364068284634));
#49050=CARTESIAN_POINT('Ctrl Pts',(55.4409742285562,27.0545955493417,15.4360575516247));
#49051=CARTESIAN_POINT('Ctrl Pts',(55.4315040594452,27.0524758490768,15.4354322959159));
#49052=CARTESIAN_POINT('Ctrl Pts',(55.4273026843721,27.0515497212559,15.4351558845729));
#49053=CARTESIAN_POINT('Ctrl Pts',(55.418091824202,27.0495505559698,15.4345520429127));
#49054=CARTESIAN_POINT('Ctrl Pts',(55.4130811973027,27.0484832224577,15.4342249366142));
#49055=CARTESIAN_POINT('Ctrl Pts',(55.3987405173231,27.0454861642834,15.4332925347245));
#49056=CARTESIAN_POINT('Ctrl Pts',(55.3894005251443,27.0436039323051,15.4326898516438));
#49057=CARTESIAN_POINT('Ctrl Pts',(55.325107144906,27.0311259542079,15.4285704144821));
#49058=CARTESIAN_POINT('Ctrl Pts',(55.269737052041,27.0227790114455,15.4251690080409));
#49059=CARTESIAN_POINT('Ctrl Pts',(55.0042995182457,26.9941257679317,15.4092468672784));
#49060=CARTESIAN_POINT('Ctrl Pts',(54.7922557163921,27.0049055286503,15.3975101998206));
#49061=CARTESIAN_POINT('Ctrl Pts',(54.5582014891221,27.0545850658182,15.382836870463));
#49062=CARTESIAN_POINT('Ctrl Pts',(54.530703447624,27.0610348601485,15.3810881705825));
#49063=CARTESIAN_POINT('Ctrl Pts',(54.4921638618881,27.0709423334816,15.3785980930345));
#49064=CARTESIAN_POINT('Ctrl Pts',(54.4810004990371,27.0739157513201,15.3778721463226));
#49065=CARTESIAN_POINT('Ctrl Pts',(54.4629202958088,27.0789000989385,15.376688541359));
#49066=CARTESIAN_POINT('Ctrl Pts',(54.4559873073951,27.0808518487103,15.3762327931316));
#49067=CARTESIAN_POINT('Ctrl Pts',(54.4414986093018,27.0850154728945,15.3752763365451));
#49068=CARTESIAN_POINT('Ctrl Pts',(54.4339451336591,27.0872346124377,15.374775400383));
#49069=CARTESIAN_POINT('Ctrl Pts',(54.4159893938189,27.0926255113846,15.373579016903));
#49070=CARTESIAN_POINT('Ctrl Pts',(54.4055996284835,27.095837712119,15.3728822684409));
#49071=CARTESIAN_POINT('Ctrl Pts',(54.371265208435,27.1067612598061,15.3705645862299));
#49072=CARTESIAN_POINT('Ctrl Pts',(54.3474409678094,27.1148403304547,15.3689317570972));
#49073=CARTESIAN_POINT('Ctrl Pts',(54.2905365306493,27.135345199287,15.3649704802703));
#49074=CARTESIAN_POINT('Ctrl Pts',(54.2576222284266,27.1482033232074,15.3626285420471));
#49075=CARTESIAN_POINT('Ctrl Pts',(54.130245812673,27.201905258266,15.3533645567618));
#49076=CARTESIAN_POINT('Ctrl Pts',(54.0386690722697,27.2491557563958,15.3462532360143));
#49077=CARTESIAN_POINT('Ctrl Pts',(53.8752255940669,27.3501883854994,15.3328686656728));
#49078=CARTESIAN_POINT('Ctrl Pts',(53.8025292375411,27.4021699292104,15.3266267412755));
#49079=CARTESIAN_POINT('Ctrl Pts',(53.6995333120882,27.4868069335144,15.3175483810126));
#49080=CARTESIAN_POINT('Ctrl Pts',(53.6664419616967,27.5158873090291,15.3145923673441));
#49081=CARTESIAN_POINT('Ctrl Pts',(53.6281598744205,27.5518445960922,15.3111513013047));
#49082=CARTESIAN_POINT('Ctrl Pts',(53.6220187445413,27.5576869030329,15.3105986162566));
#49083=CARTESIAN_POINT('Ctrl Pts',(53.6120318939036,27.5673098116783,15.3096989903351));
#49084=CARTESIAN_POINT('Ctrl Pts',(53.6081640073724,27.5710671077591,15.3093503589827));
#49085=CARTESIAN_POINT('Ctrl Pts',(53.601237937294,27.5778499518201,15.3087257825006));
#49086=CARTESIAN_POINT('Ctrl Pts',(53.5981742763906,27.5808697349148,15.308449409225));
#49087=CARTESIAN_POINT('Ctrl Pts',(53.5914776804509,27.5875132687538,15.3078450921271));
#49088=CARTESIAN_POINT('Ctrl Pts',(53.5878489549749,27.5911411291165,15.3075174760076));
#49089=CARTESIAN_POINT('Ctrl Pts',(53.5782661296107,27.600795891496,15.3066517625548));
#49090=CARTESIAN_POINT('Ctrl Pts',(53.572336281025,27.6068468687897,15.3061155051506));
#49091=CARTESIAN_POINT('Ctrl Pts',(53.5362854811462,27.6441059908498,15.3028504882215));
#49092=CARTESIAN_POINT('Ctrl Pts',(53.5071480075697,27.6762544377816,15.3001907736147));
#49093=CARTESIAN_POINT('Ctrl Pts',(53.4119825141931,27.7883970691601,15.2913279090634));
#49094=CARTESIAN_POINT('Ctrl Pts',(53.3511480315519,27.87258188765,15.285348102138));
#49095=CARTESIAN_POINT('Ctrl Pts',(53.2314424707286,28.068795988012,15.2719943369466));
#49096=CARTESIAN_POINT('Ctrl Pts',(53.1761208474975,28.182444958832,15.2646170027063));
#49097=CARTESIAN_POINT('Ctrl Pts',(53.1233638528613,28.3233486405983,15.2553547423411));
#49098=CARTESIAN_POINT('Ctrl Pts',(53.1152454490691,28.34630244452,15.2538433016772));
#49099=CARTESIAN_POINT('Ctrl Pts',(53.10445248795,28.3786923770328,15.2517043961847));
#49100=CARTESIAN_POINT('Ctrl Pts',(53.1014240848476,28.3880089692199,15.2510884670508));
#49101=CARTESIAN_POINT('Ctrl Pts',(53.0962817208661,28.4042345478716,15.250014401317));
#49102=CARTESIAN_POINT('Ctrl Pts',(53.0941364250883,28.411133468548,15.2495572917936));
#49103=CARTESIAN_POINT('Ctrl Pts',(53.0897372543244,28.4255563614228,15.2486006907876));
#49104=CARTESIAN_POINT('Ctrl Pts',(53.087490248292,28.4330822827254,15.2481009858164));
#49105=CARTESIAN_POINT('Ctrl Pts',(53.0822672106087,28.4509603538222,15.2469125324399));
#49106=CARTESIAN_POINT('Ctrl Pts',(53.0793304922248,28.4613236416942,15.2462225282671));
#49107=CARTESIAN_POINT('Ctrl Pts',(53.0733145933244,28.4832277387007,15.2447616236886));
#49108=CARTESIAN_POINT('Ctrl Pts',(53.0702548607665,28.4947734035954,15.24399012784));
#49109=CARTESIAN_POINT('Ctrl Pts',(53.0579613454037,28.5429036158068,15.2407676024948));
#49110=CARTESIAN_POINT('Ctrl Pts',(53.0496633357835,28.579716974646,15.238287252437));
#49111=CARTESIAN_POINT('Ctrl Pts',(53.0175812102494,28.7435842007438,15.2271734272461));
#49112=CARTESIAN_POINT('Ctrl Pts',(53.0051388531737,28.872519698558,15.2182084608135));
#49113=CARTESIAN_POINT('Ctrl Pts',(53.005250747999,29.0017274667166,15.2092030022871));
#49114=CARTESIAN_POINT('Ctrl Pts',(53.0052507488189,29.0017284132713,15.2092029363146));
#49115=CARTESIAN_POINT('Ctrl Pts',(53.0053490353139,29.1151601460515,15.2012970280619));
#49116=CARTESIAN_POINT('Ctrl Pts',(53.0151226269909,29.2283926494983,15.1933979671947));
#49117=CARTESIAN_POINT('Ctrl Pts',(53.0359402980613,29.3486704232499,15.185359270907));
#49118=CARTESIAN_POINT('Ctrl Pts',(53.0374623744913,29.3571381404936,15.1847953083819));
#49119=CARTESIAN_POINT('Ctrl Pts',(53.0400384497655,29.3709555337908,15.1838785633237));
#49120=CARTESIAN_POINT('Ctrl Pts',(53.0410596639462,29.3763111051693,15.1835241010534));
#49121=CARTESIAN_POINT('Ctrl Pts',(53.0430796951611,29.3866736988947,15.1828400092167));
#49122=CARTESIAN_POINT('Ctrl Pts',(53.0440758022868,29.3916812008686,15.1825102357848));
#49123=CARTESIAN_POINT('Ctrl Pts',(53.045617923212,29.3992809505369,15.1820110196316));
#49124=CARTESIAN_POINT('Ctrl Pts',(53.0461498747513,29.4018759355602,15.1818407854086));
#49125=CARTESIAN_POINT('Ctrl Pts',(53.0466869980082,29.4044698737233,15.1816708487869));
#49126=CARTESIAN_POINT('Ctrl Pts',(53.0466869327998,29.4044695588112,15.0243707259923));
#49127=CARTESIAN_POINT('Ctrl Pts',(53.0376291222587,29.360726490131,15.0274241010433));
#49128=CARTESIAN_POINT('Ctrl Pts',(53.0300389624832,29.3166708117229,15.0305098276839));
#49129=CARTESIAN_POINT('Ctrl Pts',(53.0114370908261,29.1817155653926,15.0399673408109));
#49130=CARTESIAN_POINT('Ctrl Pts',(53.0051945752177,29.0903027661733,15.0463852547253));
#49131=CARTESIAN_POINT('Ctrl Pts',(53.005258330144,28.9857281837005,15.0535820183753));
#49132=CARTESIAN_POINT('Ctrl Pts',(53.0053944644802,28.9726726926802,15.0544777782754));
#49133=CARTESIAN_POINT('Ctrl Pts',(53.0066601161836,28.9101641215504,15.0587510993224));
#49134=CARTESIAN_POINT('Ctrl Pts',(53.0095007899479,28.8607585952538,15.0620825136977));
#49135=CARTESIAN_POINT('Ctrl Pts',(53.015003364643,28.8027879233336,15.06589997914));
#49136=CARTESIAN_POINT('Ctrl Pts',(53.0158882634707,28.7940755740842,15.0664712486255));
#49137=CARTESIAN_POINT('Ctrl Pts',(53.0174198902035,28.7799234829607,15.067394907984));
#49138=CARTESIAN_POINT('Ctrl Pts',(53.0180316898803,28.7744801904085,15.0677491390117));
#49139=CARTESIAN_POINT('Ctrl Pts',(53.0191645775542,28.7647615238637,15.0683796656477));
#49140=CARTESIAN_POINT('Ctrl Pts',(53.0196770963515,28.7604852615998,15.0686564268264));
#49141=CARTESIAN_POINT('Ctrl Pts',(53.02082234174,28.7511848059899,15.0692568798577));
#49142=CARTESIAN_POINT('Ctrl Pts',(53.0214603495527,28.7461613569629,15.0695802747634));
#49143=CARTESIAN_POINT('Ctrl Pts',(53.0233179578874,28.7319678328385,15.0704915273097));
#49144=CARTESIAN_POINT('Ctrl Pts',(53.0245822472553,28.7228035927355,15.0710769548237));
#49145=CARTESIAN_POINT('Ctrl Pts',(53.0330382705838,28.6645083316185,15.0747841463435));
#49146=CARTESIAN_POINT('Ctrl Pts',(53.0419992811613,28.6156470413761,15.0778153908479));
#49147=CARTESIAN_POINT('Ctrl Pts',(53.0840940814233,28.4262714373364,15.0894423992174));
#49148=CARTESIAN_POINT('Ctrl Pts',(53.1306133781078,28.2891841467318,15.0976228415291));
#49149=CARTESIAN_POINT('Ctrl Pts',(53.2298702494432,28.0759181891185,15.1114576526866));
#49150=CARTESIAN_POINT('Ctrl Pts',(53.2737978282334,27.9962522544171,15.1169018513406));
#49151=CARTESIAN_POINT('Ctrl Pts',(53.3312822318091,27.9070029308792,15.123494153909));
#49152=CARTESIAN_POINT('Ctrl Pts',(53.3397132761916,27.8942380195203,15.1244493039887));
#49153=CARTESIAN_POINT('Ctrl Pts',(53.3537372969032,27.8735271597694,15.1260199269429));
#49154=CARTESIAN_POINT('Ctrl Pts',(53.3592430846853,27.8655227252657,15.1266321452406));
#49155=CARTESIAN_POINT('Ctrl Pts',(53.3692179839382,27.8512455029686,15.1277336605262));
#49156=CARTESIAN_POINT('Ctrl Pts',(53.3736653957638,27.8449577363907,15.1282221292872));
#49157=CARTESIAN_POINT('Ctrl Pts',(53.38319256003,27.8316523144574,15.1292630115287));
#49158=CARTESIAN_POINT('Ctrl Pts',(53.3882818263358,27.8246416984359,15.1298157825676));
#49159=CARTESIAN_POINT('Ctrl Pts',(53.4020806255106,27.8058915860757,15.1313060119466));
#49160=CARTESIAN_POINT('Ctrl Pts',(53.4108736669392,27.7942144840833,15.1322466822229));
#49161=CARTESIAN_POINT('Ctrl Pts',(53.4561611198195,27.7354288929138,15.1370476690013));
#49162=CARTESIAN_POINT('Ctrl Pts',(53.4946217080038,27.6898803311271,15.1409848655225));
#49163=CARTESIAN_POINT('Ctrl Pts',(53.6201292770321,27.5540767633319,15.1534290333));
#49164=CARTESIAN_POINT('Ctrl Pts',(53.7136770413483,27.4702601931502,15.1621765930002));
#49165=CARTESIAN_POINT('Ctrl Pts',(53.8321937887245,27.3826742081028,15.1724379731407));
#49166=CARTESIAN_POINT('Ctrl Pts',(53.8501486889396,27.3698601140367,15.173971687895));
#49167=CARTESIAN_POINT('Ctrl Pts',(53.9339655076504,27.3121154789667,15.1810263965228));
#49168=CARTESIAN_POINT('Ctrl Pts',(54.0022790661451,27.270855829103,15.1864850847642));
#49169=CARTESIAN_POINT('Ctrl Pts',(54.082213250937,27.2288969523772,15.1924136502432));
#49170=CARTESIAN_POINT('Ctrl Pts',(54.0915789911015,27.2240749440972,15.1931014046576));
#49171=CARTESIAN_POINT('Ctrl Pts',(54.1058056185925,27.2168922747006,15.1941352431392));
#49172=CARTESIAN_POINT('Ctrl Pts',(54.1106384482421,27.2144768879472,15.1944845596983));
#49173=CARTESIAN_POINT('Ctrl Pts',(54.1193372725627,27.2101734071464,15.1951098570643));
#49174=CARTESIAN_POINT('Ctrl Pts',(54.1231995988337,27.2082781662431,15.1953862706113));
#49175=CARTESIAN_POINT('Ctrl Pts',(54.1316740624742,27.204153718096,15.1959900826017));
#49176=CARTESIAN_POINT('Ctrl Pts',(54.1362886588485,27.2019297781827,15.196317157254));
#49177=CARTESIAN_POINT('Ctrl Pts',(54.1495082651488,27.1956214094208,15.1972493787525));
#49178=CARTESIAN_POINT('Ctrl Pts',(54.158134171207,27.1915807388752,15.1978519146674));
#49179=CARTESIAN_POINT('Ctrl Pts',(54.2175845710579,27.164249693858,15.2019675270229));
#49180=CARTESIAN_POINT('Ctrl Pts',(54.2693447546239,27.1430408594128,15.2053655007225));
#49181=CARTESIAN_POINT('Ctrl Pts',(54.4123228501189,27.0913614894308,15.2144327433584));
#49182=CARTESIAN_POINT('Ctrl Pts',(54.5049609822851,27.0652639078608,15.2199709222166));
#49183=CARTESIAN_POINT('Ctrl Pts',(54.7279497816268,27.0195175219057,15.2332051288297));
#49184=CARTESIAN_POINT('Ctrl Pts',(54.8590548620189,27.0058961729545,15.2409290077794));
#49185=CARTESIAN_POINT('Ctrl Pts',(55.0062864408515,27.0051977337203,15.2500662951122));
#49186=CARTESIAN_POINT('Ctrl Pts',(55.0220354675471,27.0053095435629,15.2510491834752));
#49187=CARTESIAN_POINT('Ctrl Pts',(55.0476308021818,27.0057944140287,15.2526562393269));
#49188=CARTESIAN_POINT('Ctrl Pts',(55.0574787656746,27.0060539630259,15.2532768894091));
#49189=CARTESIAN_POINT('Ctrl Pts',(55.0750361561066,27.0066468755158,15.2543877281854));
#49190=CARTESIAN_POINT('Ctrl Pts',(55.0827463833307,27.0069520485085,15.2548770317168));
#49191=CARTESIAN_POINT('Ctrl Pts',(55.099028542845,27.0076911447072,15.2559135461434));
#49192=CARTESIAN_POINT('Ctrl Pts',(55.107599813629,27.0081356714095,15.2564610770654));
#49193=CARTESIAN_POINT('Ctrl Pts',(55.1303957097441,27.0094654882322,15.2579224268753));
#49194=CARTESIAN_POINT('Ctrl Pts',(55.144613961042,27.010447922634,15.2588392452766));
#49195=CARTESIAN_POINT('Ctrl Pts',(55.2135564245036,27.0159545398855,15.2633115950144));
#49196=CARTESIAN_POINT('Ctrl Pts',(55.26808394779,27.0225843209741,15.2669318907946));
#49197=CARTESIAN_POINT('Ctrl Pts',(55.525689021111,27.0647560464535,15.2844429337309));
#49198=CARTESIAN_POINT('Ctrl Pts',(55.7226781541907,27.1293767307577,15.2992176856752));
#49199=CARTESIAN_POINT('Ctrl Pts',(55.9335362417546,27.2369131548663,15.3151598451062));
#49200=CARTESIAN_POINT('Ctrl Pts',(55.9604914490807,27.2514515855585,15.3171967860309));
#49201=CARTESIAN_POINT('Ctrl Pts',(55.9943719038012,27.2707452319232,15.319745894495));
#49202=CARTESIAN_POINT('Ctrl Pts',(56.0016149641621,27.2749304346016,15.3202901847875));
#49203=CARTESIAN_POINT('Ctrl Pts',(56.0130332067034,27.2816243120533,15.3211469098));
#49204=CARTESIAN_POINT('Ctrl Pts',(56.0172257990867,27.2841028708837,15.3214612023679));
#49205=CARTESIAN_POINT('Ctrl Pts',(56.0251364000081,27.2888186094297,15.3220536131763));
#49206=CARTESIAN_POINT('Ctrl Pts',(56.0288561464624,27.2910525402203,15.3223319191023));
#49207=CARTESIAN_POINT('Ctrl Pts',(56.0375170010559,27.2962924301282,15.3229793531829));
#49208=CARTESIAN_POINT('Ctrl Pts',(56.0424523559679,27.299307758982,15.3233478704364));
#49209=CARTESIAN_POINT('Ctrl Pts',(56.0583285469679,27.3091026318202,15.3245322018731));
#49210=CARTESIAN_POINT('Ctrl Pts',(56.0692171646043,27.3159667763766,15.3253427380342));
#49211=CARTESIAN_POINT('Ctrl Pts',(56.0948972803195,27.3325049197619,15.3272521025473));
#49212=CARTESIAN_POINT('Ctrl Pts',(56.1096283706402,27.3422711857799,15.328345602296));
#49213=CARTESIAN_POINT('Ctrl Pts',(56.1631489071019,27.3787868295846,15.3323194392121));
#49214=CARTESIAN_POINT('Ctrl Pts',(56.2011192174906,27.4067138528786,15.3351407445395));
#49215=CARTESIAN_POINT('Ctrl Pts',(56.3644628416342,27.5360139565463,15.3474546357497));
#49216=CARTESIAN_POINT('Ctrl Pts',(56.478262811641,27.6510168399532,15.3565659347542));
#49217=CARTESIAN_POINT('Ctrl Pts',(56.6116750995397,27.8232501927843,15.3696245467974));
#49218=CARTESIAN_POINT('Ctrl Pts',(56.6444395921615,27.8694893740611,15.3730758778743));
#49219=CARTESIAN_POINT('Ctrl Pts',(56.6832475001944,27.9295208172102,15.3775260676406));
#49220=CARTESIAN_POINT('Ctrl Pts',(56.6911652830976,27.9420738237988,15.3784549456834));
#49221=CARTESIAN_POINT('Ctrl Pts',(56.7035518898214,27.9622062301939,15.3799425790555));
#49222=CARTESIAN_POINT('Ctrl Pts',(56.7081120149612,27.9697290209262,15.3804979968454));
#49223=CARTESIAN_POINT('Ctrl Pts',(56.716561936661,27.9838790780014,15.3815419780149));
#49224=CARTESIAN_POINT('Ctrl Pts',(56.7204634999068,27.9904991563575,15.3820301037449));
#49225=CARTESIAN_POINT('Ctrl Pts',(56.7291102541959,28.0053664876959,15.3831257522241));
#49226=CARTESIAN_POINT('Ctrl Pts',(56.7338348578466,28.0136254385232,15.3837339993377));
#49227=CARTESIAN_POINT('Ctrl Pts',(56.7476335180598,28.03815197783,15.3855393231576));
#49228=CARTESIAN_POINT('Ctrl Pts',(56.7565388008986,28.0545128592441,15.3867423394837));
#49229=CARTESIAN_POINT('Ctrl Pts',(56.825706938564,28.185940143541,15.3963990124893));
#49230=CARTESIAN_POINT('Ctrl Pts',(56.8748178513817,28.3064972601989,15.4052445394534));
#49231=CARTESIAN_POINT('Ctrl Pts',(56.9528892802432,28.5687966936549,15.4242542246605));
#49232=CARTESIAN_POINT('Ctrl Pts',(56.9788923783932,28.7106847281869,15.4344034918505));
#49233=CARTESIAN_POINT('Ctrl Pts',(56.9904672661758,28.8685595625478,15.444867303577));
#49234=CARTESIAN_POINT('Ctrl Pts',(56.9913675577762,28.8829880137083,15.4458157475121));
#49235=CARTESIAN_POINT('Ctrl Pts',(56.9924004720642,28.9030483516967,15.4471223244563));
#49236=CARTESIAN_POINT('Ctrl Pts',(56.9926661930258,28.9086725221637,15.4474873222747));
#49237=CARTESIAN_POINT('Ctrl Pts',(56.9930826344096,28.9183564000096,15.4481134330865));
#49238=CARTESIAN_POINT('Ctrl Pts',(56.9932447712145,28.9224155444112,15.4483751652129));
#49239=CARTESIAN_POINT('Ctrl Pts',(56.9935584386156,28.9309196528592,15.4489219764759));
#49240=CARTESIAN_POINT('Ctrl Pts',(56.993707505286,28.9353646658576,15.4492069094866));
#49241=CARTESIAN_POINT('Ctrl Pts',(56.9940354922301,28.9462295261276,15.4499012935754));
#49242=CARTESIAN_POINT('Ctrl Pts',(56.994198279306,28.9526498821564,15.4503098580233));
#49243=CARTESIAN_POINT('Ctrl Pts',(56.9946730631908,28.9757844855206,15.4517760403744));
#49244=CARTESIAN_POINT('Ctrl Pts',(56.9948059672532,28.9925022509453,15.4528242552352));
#49245=CARTESIAN_POINT('Ctrl Pts',(56.9946135989172,29.0341191891389,15.4554099233105));
#49246=CARTESIAN_POINT('Ctrl Pts',(56.9940323189497,29.0590148665882,15.4569355487784));
#49247=CARTESIAN_POINT('Ctrl Pts',(56.9895650880044,29.165138032552,15.4633730860939));
#49248=CARTESIAN_POINT('Ctrl Pts',(56.981180216457,29.2461032509164,15.4681220971931));
#49249=CARTESIAN_POINT('Ctrl Pts',(56.9422466077599,29.4808812464962,15.4819584700742));
#49250=CARTESIAN_POINT('Ctrl Pts',(56.8985065291685,29.6318508819898,15.4909856366232));
#49251=CARTESIAN_POINT('Ctrl Pts',(56.8283669327761,29.7979098839537,15.5020932747695));
#49252=CARTESIAN_POINT('Ctrl Pts',(56.8187879330774,29.8195097346748,15.50356116403));
#49253=CARTESIAN_POINT('Ctrl Pts',(56.80479022424,29.8496184656033,15.5056422782307));
#49254=CARTESIAN_POINT('Ctrl Pts',(56.8006901748169,29.8582739538353,15.5062446638891));
#49255=CARTESIAN_POINT('Ctrl Pts',(56.7934115569063,29.8733578724643,15.5073018244246));
#49256=CARTESIAN_POINT('Ctrl Pts',(56.7902603349002,29.8797993617595,15.507755652913));
#49257=CARTESIAN_POINT('Ctrl Pts',(56.7835638454093,29.8933028667214,15.5087121037417));
#49258=CARTESIAN_POINT('Ctrl Pts',(56.7800112178942,29.9003610740036,15.5092149751998));
#49259=CARTESIAN_POINT('Ctrl Pts',(56.7713975869396,29.9172240164427,15.5104235594198));
#49260=CARTESIAN_POINT('Ctrl Pts',(56.766297028686,29.9270081476235,15.5111306434992));
#49261=CARTESIAN_POINT('Ctrl Pts',(56.748432962206,29.960593106725,15.5135783306971));
#49262=CARTESIAN_POINT('Ctrl Pts',(56.7352679005363,29.9841758661671,15.5153329787346));
#49263=CARTESIAN_POINT('Ctrl Pts',(56.7023055933076,30.0405032114287,15.5196137407792));
#49264=CARTESIAN_POINT('Ctrl Pts',(56.6820377059062,30.0729585755317,15.5221558557782));
#49265=CARTESIAN_POINT('Ctrl Pts',(56.5982478551581,30.1989191153789,15.5323255567253));
#49266=CARTESIAN_POINT('Ctrl Pts',(56.5277661155212,30.2875281498299,15.5401781797339));
#49267=CARTESIAN_POINT('Ctrl Pts',(56.3762794460756,30.4479167359367,15.5555547476907));
#49268=CARTESIAN_POINT('Ctrl Pts',(56.2961709985651,30.520050409855,15.5630480774395));
#49269=CARTESIAN_POINT('Ctrl Pts',(56.1978656022446,30.5951186077054,15.5712424467446));
#49270=CARTESIAN_POINT('Ctrl Pts',(56.1849866435476,30.6047093404324,15.572297617456));
#49271=CARTESIAN_POINT('Ctrl Pts',(56.1667281799059,30.6179663917015,15.5737663453386));
#49272=CARTESIAN_POINT('Ctrl Pts',(56.1614447964174,30.6217632004028,15.5741881974828));
#49273=CARTESIAN_POINT('Ctrl Pts',(56.1528669377008,30.6278641057177,15.5748678964775));
#49274=CARTESIAN_POINT('Ctrl Pts',(56.1495839610035,30.630184173653,15.5751268126029));
#49275=CARTESIAN_POINT('Ctrl Pts',(56.1426170368713,30.6350761618882,15.5756736447723));
#49276=CARTESIAN_POINT('Ctrl Pts',(56.1389313692111,30.637645592038,15.5759613861409));
#49277=CARTESIAN_POINT('Ctrl Pts',(56.1297719580966,30.6439851154093,15.5766727251106));
#49278=CARTESIAN_POINT('Ctrl Pts',(56.1242879366608,30.6477403847283,15.577095332943));
#49279=CARTESIAN_POINT('Ctrl Pts',(56.1036760748113,30.6617038655529,15.5786718391155));
#49280=CARTESIAN_POINT('Ctrl Pts',(56.0884266084257,30.6717320922745,15.5798143755022));
#49281=CARTESIAN_POINT('Ctrl Pts',(56.0494277507255,30.6966182829233,15.5826822258811));
#49282=CARTESIAN_POINT('Ctrl Pts',(56.0254984834328,30.7111882481179,15.5843921240233));
#49283=CARTESIAN_POINT('Ctrl Pts',(55.9144181694639,30.7756550107634,15.5921415723413));
#49284=CARTESIAN_POINT('Ctrl Pts',(55.8238783142742,30.8194336799641,15.5979433860182));
#49285=CARTESIAN_POINT('Ctrl Pts',(55.6084960152647,30.9041868501124,15.6113859764733));
#49286=CARTESIAN_POINT('Ctrl Pts',(55.4821567912092,30.940029454509,15.6190312079532));
#49287=CARTESIAN_POINT('Ctrl Pts',(55.3292675381673,30.9675372734213,15.6285944111241));
#49288=CARTESIAN_POINT('Ctrl Pts',(55.3052354230689,30.9714084535927,15.6301055298876));
#49289=CARTESIAN_POINT('Ctrl Pts',(55.2714415011369,30.9762193771607,15.6322440523846));
#49290=CARTESIAN_POINT('Ctrl Pts',(55.2617338360955,30.9775284849541,15.6328599259822));
#49291=CARTESIAN_POINT('Ctrl Pts',(55.2448503756882,30.9796787745711,15.6339339219029));
#49292=CARTESIAN_POINT('Ctrl Pts',(55.2376788645123,30.9805525774661,15.6343910174821));
#49293=CARTESIAN_POINT('Ctrl Pts',(55.2227010559496,30.9822950067479,15.6353476157858));
#49294=CARTESIAN_POINT('Ctrl Pts',(55.214894071865,30.9831565215827,15.6358473321383));
#49295=CARTESIAN_POINT('Ctrl Pts',(55.1963681511624,30.9850902133622,15.6370358610923));
#49296=CARTESIAN_POINT('Ctrl Pts',(55.1856453028863,30.9861217032208,15.6377259298965));
#49297=CARTESIAN_POINT('Ctrl Pts',(55.149595684472,30.9892950305221,15.6400533929149));
#49298=CARTESIAN_POINT('Ctrl Pts',(55.1242373064698,30.9910395728451,15.6417030422273));
#49299=CARTESIAN_POINT('Ctrl Pts',(55.0635576408155,30.9940503629637,15.6456819013906));
#49300=CARTESIAN_POINT('Ctrl Pts',(55.0282234420616,30.9948633057558,15.648024306871));
#49301=CARTESIAN_POINT('Ctrl Pts',(54.8899487516295,30.9943703041964,15.6572911436484));
#49302=CARTESIAN_POINT('Ctrl Pts',(54.7872033187004,30.9860356059246,15.6644049771679));
#49303=CARTESIAN_POINT('Ctrl Pts',(54.563776474529,30.9503713726648,15.6801653432667));
#49304=CARTESIAN_POINT('Ctrl Pts',(54.4440370191278,30.9196744314123,15.6888060340609));
#49305=CARTESIAN_POINT('Ctrl Pts',(54.3130936552536,30.8728145338205,15.6980153577458));
#49306=CARTESIAN_POINT('Ctrl Pts',(54.2983576958312,30.8673437600483,15.6990479028453));
#49307=CARTESIAN_POINT('Ctrl Pts',(54.2776680678751,30.8593831608111,15.7004906675542));
#49308=CARTESIAN_POINT('Ctrl Pts',(54.2716598962553,30.8570379250098,15.7009088056684));
#49309=CARTESIAN_POINT('Ctrl Pts',(54.2615641560586,30.853040609973,15.7016098840766));
#49310=CARTESIAN_POINT('Ctrl Pts',(54.2574705332348,30.851404059111,15.7018937307964));
#49311=CARTESIAN_POINT('Ctrl Pts',(54.2491178855321,30.8480326730328,15.7024719721427));
#49312=CARTESIAN_POINT('Ctrl Pts',(54.2448593842566,30.8462966614054,15.7027662945351));
#49313=CARTESIAN_POINT('Ctrl Pts',(54.2343542928674,30.8419717518811,15.7034912290836));
#49314=CARTESIAN_POINT('Ctrl Pts',(54.2281147350903,30.8393657669244,15.7039208307253));
#49315=CARTESIAN_POINT('Ctrl Pts',(54.2033444814168,30.8288720955499,15.7056228612084));
#49316=CARTESIAN_POINT('Ctrl Pts',(54.1849197152366,30.8207353898419,15.7068812054709));
#49317=CARTESIAN_POINT('Ctrl Pts',(54.0365231350092,30.7524965475627,15.7169783921562));
#49318=CARTESIAN_POINT('Ctrl Pts',(53.9132279582904,30.6788297710545,15.7251526225547));
#49319=CARTESIAN_POINT('Ctrl Pts',(53.7829812108933,30.5805976911614,15.734646900052));
#49320=CARTESIAN_POINT('Ctrl Pts',(53.7672692879489,30.5683745638605,15.7358074220821));
#49321=CARTESIAN_POINT('Ctrl Pts',(53.6696529324222,30.4900605023783,15.743127462459));
#49322=CARTESIAN_POINT('Ctrl Pts',(53.5929139277952,30.417818086796,15.7493881697009));
#49323=CARTESIAN_POINT('Ctrl Pts',(53.5116934176174,30.3282384734495,15.7568929020904));
#49324=CARTESIAN_POINT('Ctrl Pts',(53.5012883543632,30.3164867287231,15.757872518066));
#49325=CARTESIAN_POINT('Ctrl Pts',(53.4845907105408,30.2971734589775,15.7594752789262));
#49326=CARTESIAN_POINT('Ctrl Pts',(53.4782133472366,30.2896858823703,15.7600949378891));
#49327=CARTESIAN_POINT('Ctrl Pts',(53.4669331329581,30.2762417704714,15.7612046739681));
#49328=CARTESIAN_POINT('Ctrl Pts',(53.4620089404592,30.2703033391976,15.7616938726205));
#49329=CARTESIAN_POINT('Ctrl Pts',(53.4516735838924,30.2576910159417,15.7627308677088));
#49330=CARTESIAN_POINT('Ctrl Pts',(53.4462708571174,30.2510104432699,15.7632789884445));
#49331=CARTESIAN_POINT('Ctrl Pts',(53.4319956777335,30.2331237982327,15.7647435861003));
#49332=CARTESIAN_POINT('Ctrl Pts',(53.4232003557133,30.221857078656,15.765663086126));
#49333=CARTESIAN_POINT('Ctrl Pts',(53.3812305055252,30.1668862202387,15.7701356318137));
#49334=CARTESIAN_POINT('Ctrl Pts',(53.3497504438594,30.121924047546,15.7737533029853));
#49335=CARTESIAN_POINT('Ctrl Pts',(53.2816383736695,30.0155613755344,15.78222626844));
#49336=CARTESIAN_POINT('Ctrl Pts',(53.2463742546062,29.9533764934821,15.7871201842216));
#49337=CARTESIAN_POINT('Ctrl Pts',(53.1838448417862,29.8278538269155,15.7968350799041));
#49338=CARTESIAN_POINT('Ctrl Pts',(53.1563731239664,29.7647229573151,15.801645506378));
#49339=CARTESIAN_POINT('Ctrl Pts',(53.0999240048787,29.6141667059374,15.8128243982356));
#49340=CARTESIAN_POINT('Ctrl Pts',(53.0736221236358,29.5258914375472,15.8191605622914));
#49341=CARTESIAN_POINT('Ctrl Pts',(53.0511813086901,29.4257303638222,15.8259024611584));
#49342=CARTESIAN_POINT('Ctrl Pts',(53.0489394772819,29.4153353859556,15.8265968235746));
#49343=CARTESIAN_POINT('Ctrl Pts',(53.0467495290295,29.4047717676867,15.8272967139322));
#49344=CARTESIAN_POINT('Ctrl Pts',(53.0467182547747,29.4046208225388,15.8273067135856));
#49345=CARTESIAN_POINT('Ctrl Pts',(53.0466869980082,29.4044698737233,15.8273167122946));
#49346=CARTESIAN_POINT('Origin',(55.,29.,3.45145488139523));
#49347=CARTESIAN_POINT('',(53.046686998698,29.4044698770549,16.7848524498588));
#49348=CARTESIAN_POINT('',(53.0466869925414,29.4044698473222,16.6248055079682));
#49349=CARTESIAN_POINT('',(53.0466869980082,29.4044698737233,3.45145488139523));
#49350=CARTESIAN_POINT('Ctrl Pts',(53.046686998698,29.4044698770549,16.7848524498588));
#49351=CARTESIAN_POINT('Ctrl Pts',(53.0473705149442,29.4077707932567,16.7846504639398));
#49352=CARTESIAN_POINT('Ctrl Pts',(53.048062443288,29.4110701929009,16.7844482656876));
#49353=CARTESIAN_POINT('Ctrl Pts',(53.0602391405275,29.4684096166467,16.7809288766104));
#49354=CARTESIAN_POINT('Ctrl Pts',(53.0739547274212,29.5219468704672,16.7775578590536));
#49355=CARTESIAN_POINT('Ctrl Pts',(53.093988482993,29.5885164108423,16.7732256058865));
#49356=CARTESIAN_POINT('Ctrl Pts',(53.098250161206,29.602145333603,16.7723311577031));
#49357=CARTESIAN_POINT('Ctrl Pts',(53.1053088717664,29.6238965137048,16.770891102513));
#49358=CARTESIAN_POINT('Ctrl Pts',(53.1080127330734,29.6320486605423,16.7703485378006));
#49359=CARTESIAN_POINT('Ctrl Pts',(53.1132451521605,29.647489945067,16.7693153208745));
#49360=CARTESIAN_POINT('Ctrl Pts',(53.1157635219392,29.654782388912,16.7688250107219));
#49361=CARTESIAN_POINT('Ctrl Pts',(53.1215902313444,29.6713427903041,16.767706112983));
#49362=CARTESIAN_POINT('Ctrl Pts',(53.1249249564342,29.6806011874579,16.7670766653315));
#49363=CARTESIAN_POINT('Ctrl Pts',(53.1337621247913,29.7045783631893,16.7654361871325));
#49364=CARTESIAN_POINT('Ctrl Pts',(53.1393701416055,29.7192572443075,16.7644216881598));
#49365=CARTESIAN_POINT('Ctrl Pts',(53.1929729923203,29.8547382862848,16.7549613145506));
#49366=CARTESIAN_POINT('Ctrl Pts',(53.2524860251078,29.9706223155998,16.7461195822069));
#49367=CARTESIAN_POINT('Ctrl Pts',(53.3610768887371,30.1392758471369,16.7321918515968));
#49368=CARTESIAN_POINT('Ctrl Pts',(53.4024499896321,30.1966003254097,16.727249496158));
#49369=CARTESIAN_POINT('Ctrl Pts',(53.4819910523746,30.295309292532,16.7184595056697));
#49370=CARTESIAN_POINT('Ctrl Pts',(53.5190364879144,30.337507107203,16.7146000730754));
#49371=CARTESIAN_POINT('Ctrl Pts',(53.5715054469016,30.3924164580435,16.7094920025527));
#49372=CARTESIAN_POINT('Ctrl Pts',(53.5854095794868,30.406539827671,16.7081699822837));
#49373=CARTESIAN_POINT('Ctrl Pts',(53.6093822823076,30.4301753892688,16.7059470282432));
#49374=CARTESIAN_POINT('Ctrl Pts',(53.6193434194752,30.43979398281,16.7050393147285));
#49375=CARTESIAN_POINT('Ctrl Pts',(53.6337679137596,30.4534350760634,16.7037485930727));
#49376=CARTESIAN_POINT('Ctrl Pts',(53.6381502808744,30.4575421018179,16.7033595348484));
#49377=CARTESIAN_POINT('Ctrl Pts',(53.6457699642133,30.464618677093,16.7026884921108));
#49378=CARTESIAN_POINT('Ctrl Pts',(53.6489986463229,30.4675974253779,16.7024058199935));
#49379=CARTESIAN_POINT('Ctrl Pts',(53.6557133918333,30.4737514414887,16.7018214317487));
#49380=CARTESIAN_POINT('Ctrl Pts',(53.6592008959342,30.4769250352797,16.7015198380407));
#49381=CARTESIAN_POINT('Ctrl Pts',(53.6683878641594,30.4852257241798,16.7007303010491));
#49382=CARTESIAN_POINT('Ctrl Pts',(53.6741057542279,30.490332441318,16.7002438537992));
#49383=CARTESIAN_POINT('Ctrl Pts',(53.6979893345979,30.5114169041511,16.6982317444918));
#49384=CARTESIAN_POINT('Ctrl Pts',(53.7164163415951,30.5270972286205,16.6967264770743));
#49385=CARTESIAN_POINT('Ctrl Pts',(53.8644110482558,30.6484600670704,16.6849622493311));
#49386=CARTESIAN_POINT('Ctrl Pts',(54.0065288925773,30.7378183482786,16.6755522791111));
#49387=CARTESIAN_POINT('Ctrl Pts',(54.2167920207878,30.8357007838572,16.6619415093971));
#49388=CARTESIAN_POINT('Ctrl Pts',(54.2767260802871,30.8601306304453,16.6580998674304));
#49389=CARTESIAN_POINT('Ctrl Pts',(54.3626510169625,30.8903733480591,16.6525663728397));
#49390=CARTESIAN_POINT('Ctrl Pts',(54.3877350558922,30.898646008298,16.6509482132753));
#49391=CARTESIAN_POINT('Ctrl Pts',(54.4323406533457,30.9123809793309,16.6480610175726));
#49392=CARTESIAN_POINT('Ctrl Pts',(54.4517953380515,30.9180484211611,16.6467985681853));
#49393=CARTESIAN_POINT('Ctrl Pts',(54.4808204171494,30.9260262058763,16.6449088762474));
#49394=CARTESIAN_POINT('Ctrl Pts',(54.4903274158068,30.9285637755451,16.6442889412856));
#49395=CARTESIAN_POINT('Ctrl Pts',(54.5073212005192,30.9329652567805,16.643178897985));
#49396=CARTESIAN_POINT('Ctrl Pts',(54.5148008080795,30.9348562801469,16.6426896699732));
#49397=CARTESIAN_POINT('Ctrl Pts',(54.5306305026254,30.9387608449992,16.6416528085416));
#49398=CARTESIAN_POINT('Ctrl Pts',(54.5389829822338,30.940763933279,16.6411048520127));
#49399=CARTESIAN_POINT('Ctrl Pts',(54.5612571514811,30.9459538128896,16.6396411598183));
#49400=CARTESIAN_POINT('Ctrl Pts',(54.5752003659685,30.949045095031,16.6387224076357));
#49401=CARTESIAN_POINT('Ctrl Pts',(54.637039086391,30.9620599787507,16.6346358467582));
#49402=CARTESIAN_POINT('Ctrl Pts',(54.6852534319062,30.9703689751216,16.6314176886647));
#49403=CARTESIAN_POINT('Ctrl Pts',(54.7567159234007,30.9799946399306,16.6265978493644));
#49404=CARTESIAN_POINT('Ctrl Pts',(54.7797622740632,30.9826903931219,16.6250360001261));
#49405=CARTESIAN_POINT('Ctrl Pts',(54.8211578790237,30.9868018404937,16.6222179346312));
#49406=CARTESIAN_POINT('Ctrl Pts',(54.8394899157393,30.9883668026405,16.6209655201859));
#49407=CARTESIAN_POINT('Ctrl Pts',(54.9847570689201,30.9987459156168,16.611008911908));
#49408=CARTESIAN_POINT('Ctrl Pts',(55.1122469751788,30.9956489301273,16.6020502653037));
#49409=CARTESIAN_POINT('Ctrl Pts',(55.3026256359539,30.9727162131075,16.5888054589628));
#49410=CARTESIAN_POINT('Ctrl Pts',(55.366285797496,30.9618939551428,16.5844048501245));
#49411=CARTESIAN_POINT('Ctrl Pts',(55.4429918157718,30.944988935424,16.5792186881644));
#49412=CARTESIAN_POINT('Ctrl Pts',(55.4566371335069,30.9418306472086,16.5783007095968));
#49413=CARTESIAN_POINT('Ctrl Pts',(55.4760641829041,30.9371180316722,16.5770014254847));
#49414=CARTESIAN_POINT('Ctrl Pts',(55.4818735736244,30.9356810781081,16.5766138744825));
#49415=CARTESIAN_POINT('Ctrl Pts',(55.4919124966708,30.9331499534369,16.5759459715793));
#49416=CARTESIAN_POINT('Ctrl Pts',(55.4961450336239,30.9320679993103,16.575664933799));
#49417=CARTESIAN_POINT('Ctrl Pts',(55.5049953147444,30.9297746200873,16.5750784867965));
#49418=CARTESIAN_POINT('Ctrl Pts',(55.5096122862517,30.9285605178737,16.574773232089));
#49419=CARTESIAN_POINT('Ctrl Pts',(55.5218866767057,30.9252856257193,16.5739634037597));
#49420=CARTESIAN_POINT('Ctrl Pts',(55.5295363350761,30.9231957047473,16.5734604687426));
#49421=CARTESIAN_POINT('Ctrl Pts',(55.5626493230453,30.9139365367559,16.5712902806018));
#49422=CARTESIAN_POINT('Ctrl Pts',(55.5879823938107,30.9063064260557,16.5696476104942));
#49423=CARTESIAN_POINT('Ctrl Pts',(55.8136501057351,30.8334101305179,16.5551114939945));
#49424=CARTESIAN_POINT('Ctrl Pts',(56.0026354425854,30.7372869754487,16.5434942664095));
#49425=CARTESIAN_POINT('Ctrl Pts',(56.2177767877406,30.580854148709,16.5275237372436));
#49426=CARTESIAN_POINT('Ctrl Pts',(56.2610902157996,30.5465221558145,16.524152513996));
#49427=CARTESIAN_POINT('Ctrl Pts',(56.3137331457803,30.5011118207985,16.5198200287775));
#49428=CARTESIAN_POINT('Ctrl Pts',(56.3244452608945,30.4916689348158,16.5189255631614));
#49429=CARTESIAN_POINT('Ctrl Pts',(56.3414364869799,30.4763636014501,16.5174854865406));
#49430=CARTESIAN_POINT('Ctrl Pts',(56.3477808443583,30.4705740797913,16.5169429179931));
#49431=CARTESIAN_POINT('Ctrl Pts',(56.3597526978606,30.4595066581819,16.515909698067));
#49432=CARTESIAN_POINT('Ctrl Pts',(56.3653873633034,30.4542367173274,16.5154193887792));
#49433=CARTESIAN_POINT('Ctrl Pts',(56.3781391693547,30.4421708736491,16.5143004990087));
#49434=CARTESIAN_POINT('Ctrl Pts',(56.385236833727,30.4353547671904,16.5136710585063));
#49435=CARTESIAN_POINT('Ctrl Pts',(56.4035362126393,30.4175191586215,16.5120306112103));
#49436=CARTESIAN_POINT('Ctrl Pts',(56.4146584978254,30.4064194880906,16.5110161362069));
#49437=CARTESIAN_POINT('Ctrl Pts',(56.5165894435594,30.3022632870349,16.5015535272999));
#49438=CARTESIAN_POINT('Ctrl Pts',(56.5982104028425,30.2006853610274,16.4927093080987));
#49439=CARTESIAN_POINT('Ctrl Pts',(56.7292230403294,30.0003875490554,16.4760908341323));
#49440=CARTESIAN_POINT('Ctrl Pts',(56.7814598942167,29.9040958844398,16.4684053515834));
#49441=CARTESIAN_POINT('Ctrl Pts',(56.8437258272161,29.7627175415939,16.4578824112201));
#49442=CARTESIAN_POINT('Ctrl Pts',(56.8605058075648,29.7208202428746,16.4548540523711));
#49443=CARTESIAN_POINT('Ctrl Pts',(56.8789186336949,29.6699057098751,16.451309489791));
#49444=CARTESIAN_POINT('Ctrl Pts',(56.8819281517953,29.6614040603197,16.4507220875718));
#49445=CARTESIAN_POINT('Ctrl Pts',(56.8865208927137,29.6481447515475,16.4498132145359));
#49446=CARTESIAN_POINT('Ctrl Pts',(56.8881439659113,29.6434011679587,16.4494894970489));
#49447=CARTESIAN_POINT('Ctrl Pts',(56.8911298792098,29.6345659463069,16.4488892876068));
#49448=CARTESIAN_POINT('Ctrl Pts',(56.8924973247266,29.6304760397204,16.4486125391023));
#49449=CARTESIAN_POINT('Ctrl Pts',(56.8955934637248,29.6211149289821,16.4479815751847));
#49450=CARTESIAN_POINT('Ctrl Pts',(56.8973134387888,29.6158409303445,16.4476278694876));
#49451=CARTESIAN_POINT('Ctrl Pts',(56.9017628670033,29.6020019653963,16.4467042255336));
#49452=CARTESIAN_POINT('Ctrl Pts',(56.90445650002,29.5934254926012,16.4461362945954));
#49453=CARTESIAN_POINT('Ctrl Pts',(56.9230274567938,29.5328669202895,16.4421557205374));
#49454=CARTESIAN_POINT('Ctrl Pts',(56.9368338632843,29.4802681401315,16.4388513616038));
#49455=CARTESIAN_POINT('Ctrl Pts',(56.959416274603,29.3772607638437,16.4325585114556));
#49456=CARTESIAN_POINT('Ctrl Pts',(56.9684362348361,29.3269511541557,16.4295652887979));
#49457=CARTESIAN_POINT('Ctrl Pts',(56.9869603761347,29.1945289522752,16.4217753928369));
#49458=CARTESIAN_POINT('Ctrl Pts',(56.9933116541355,29.1120782333297,16.4170105030146));
#49459=CARTESIAN_POINT('Ctrl Pts',(56.9958274017511,28.9418224076345,16.4070142896063));
#49460=CARTESIAN_POINT('Ctrl Pts',(56.991343565272,28.8541924701125,16.4017821409044));
#49461=CARTESIAN_POINT('Ctrl Pts',(56.9785580648322,28.7454131546871,16.395018614302));
#49462=CARTESIAN_POINT('Ctrl Pts',(56.9756460596507,28.7237228452262,16.393656848677));
#49463=CARTESIAN_POINT('Ctrl Pts',(56.9708622998961,28.6920514054342,16.3916473262227));
#49464=CARTESIAN_POINT('Ctrl Pts',(56.9692701960676,28.6820291981181,16.3910083205457));
#49465=CARTESIAN_POINT('Ctrl Pts',(56.9663267336948,28.6643709363987,16.389876777756));
#49466=CARTESIAN_POINT('Ctrl Pts',(56.9650071801711,28.6567297404387,16.3893852504248));
#49467=CARTESIAN_POINT('Ctrl Pts',(56.962342135679,28.6418162483501,16.3884221710889));
#49468=CARTESIAN_POINT('Ctrl Pts',(56.9610006864978,28.6345433506538,16.3879507540536));
#49469=CARTESIAN_POINT('Ctrl Pts',(56.9572683841659,28.6149204330259,16.3866740134778));
#49470=CARTESIAN_POINT('Ctrl Pts',(56.9548011327827,28.6025854558701,16.3858662875173));
#49471=CARTESIAN_POINT('Ctrl Pts',(56.9450646693022,28.5561941261973,16.3828084782362));
#49472=CARTESIAN_POINT('Ctrl Pts',(56.9370210980891,28.5223084300253,16.380534086293));
#49473=CARTESIAN_POINT('Ctrl Pts',(56.881347545963,28.3123849184692,16.3661792143959));
#49474=CARTESIAN_POINT('Ctrl Pts',(56.8106530116329,28.1433817345567,16.3533360541871));
#49475=CARTESIAN_POINT('Ctrl Pts',(56.6833842180433,27.9276702164961,16.3360099263615));
#49476=CARTESIAN_POINT('Ctrl Pts',(56.6457581492161,27.8707721356431,16.3313518807412));
#49477=CARTESIAN_POINT('Ctrl Pts',(56.5967439052245,27.8043229189547,16.3258968957257));
#49478=CARTESIAN_POINT('Ctrl Pts',(56.5880734703435,27.7928308062458,16.3249529657946));
#49479=CARTESIAN_POINT('Ctrl Pts',(56.5755827017754,27.7766426011678,16.3236237470804));
#49480=CARTESIAN_POINT('Ctrl Pts',(56.5718644731194,27.7718687953404,16.3232318231915));
#49481=CARTESIAN_POINT('Ctrl Pts',(56.5654177367583,27.7636691173335,16.3225588413691));
#49482=CARTESIAN_POINT('Ctrl Pts',(56.5626995809244,27.7602351984057,16.3222770686008));
#49483=CARTESIAN_POINT('Ctrl Pts',(56.5570122738429,27.7530986946551,16.3216916482766));
#49484=CARTESIAN_POINT('Ctrl Pts',(56.5540412023467,27.7493977336054,16.3213881401283));
#49485=CARTESIAN_POINT('Ctrl Pts',(56.5461497599975,27.7396391845484,16.3205879897887));
#49486=CARTESIAN_POINT('Ctrl Pts',(56.5412069421259,27.7335997347668,16.3200929175765));
#49487=CARTESIAN_POINT('Ctrl Pts',(56.5200570009195,27.7080646243609,16.3179995269098));
#49488=CARTESIAN_POINT('Ctrl Pts',(56.5035136476127,27.6888489208012,16.3164237044337));
#49489=CARTESIAN_POINT('Ctrl Pts',(56.3452890152304,27.51199960473,16.3018588965334));
#49490=CARTESIAN_POINT('Ctrl Pts',(56.1796882752731,27.3775607955234,16.2901809722933));
#49491=CARTESIAN_POINT('Ctrl Pts',(55.9643419860151,27.2534584359322,16.2752593322375));
#49492=CARTESIAN_POINT('Ctrl Pts',(55.9321870505075,27.2360867449525,16.2730418908035));
#49493=CARTESIAN_POINT('Ctrl Pts',(55.8762991378782,27.2078483797508,16.269191800827));
#49494=CARTESIAN_POINT('Ctrl Pts',(55.8527962931578,27.1965460932352,16.2675739211466));
#49495=CARTESIAN_POINT('Ctrl Pts',(55.8191815357387,27.1811851108778,16.2652585011433));
#49496=CARTESIAN_POINT('Ctrl Pts',(55.8092469305589,27.1767431921701,16.2645740244299));
#49497=CARTESIAN_POINT('Ctrl Pts',(55.79206229399,27.169227789693,16.2633895139526));
#49498=CARTESIAN_POINT('Ctrl Pts',(55.7848294240865,27.1661155064174,16.2628908065538));
#49499=CARTESIAN_POINT('Ctrl Pts',(55.7709470783642,27.1602391409029,16.2619332337006));
#49500=CARTESIAN_POINT('Ctrl Pts',(55.7643006779694,27.1574680768745,16.2614746131039));
#49501=CARTESIAN_POINT('Ctrl Pts',(55.748666045773,27.1510487265375,16.260395318362));
#49502=CARTESIAN_POINT('Ctrl Pts',(55.7396659794475,27.1474299222136,16.2597736673114));
#49503=CARTESIAN_POINT('Ctrl Pts',(55.7085098296015,27.135165687043,16.2576202161656));
#49504=CARTESIAN_POINT('Ctrl Pts',(55.6862264610941,27.1268512186896,16.2560775054092));
#49505=CARTESIAN_POINT('Ctrl Pts',(55.5213574464728,27.0686712615615,16.2446404063663));
#49506=CARTESIAN_POINT('Ctrl Pts',(55.3736910792937,27.0347562595619,16.2342156075911));
#49507=CARTESIAN_POINT('Ctrl Pts',(55.1389188332706,27.0082673285828,16.2177487144301));
#49508=CARTESIAN_POINT('Ctrl Pts',(55.0536621031402,27.0041494343057,16.2118036362858));
#49509=CARTESIAN_POINT('Ctrl Pts',(54.9428131343688,27.0059057067328,16.2042901932319));
#49510=CARTESIAN_POINT('Ctrl Pts',(54.9172356810205,27.0068034259631,16.2025718680887));
#49511=CARTESIAN_POINT('Ctrl Pts',(54.8746436909906,27.0091196670412,16.1997433742915));
#49512=CARTESIAN_POINT('Ctrl Pts',(54.8576178844072,27.0102648206072,16.1986214931631));
#49513=CARTESIAN_POINT('Ctrl Pts',(54.8341546733036,27.0121456779245,16.1970894477872));
#49514=CARTESIAN_POINT('Ctrl Pts',(54.8277035914137,27.012694429995,16.1966696847085));
#49515=CARTESIAN_POINT('Ctrl Pts',(54.8168154048531,27.0136740353514,16.195963807799));
#49516=CARTESIAN_POINT('Ctrl Pts',(54.8123769013735,27.0140883685486,16.1956767926037));
#49517=CARTESIAN_POINT('Ctrl Pts',(54.8039069002132,27.0149076911272,16.195130523713));
#49518=CARTESIAN_POINT('Ctrl Pts',(54.7998752084606,27.0153100879351,16.1948711229679));
#49519=CARTESIAN_POINT('Ctrl Pts',(54.7902848010281,27.0162968120632,16.1942554916693));
#49520=CARTESIAN_POINT('Ctrl Pts',(54.7847272240995,27.0168922277757,16.1938998730537));
#49521=CARTESIAN_POINT('Ctrl Pts',(54.7650467696054,27.0190844177865,16.1926443511984));
#49522=CARTESIAN_POINT('Ctrl Pts',(54.750938143285,27.0208088059089,16.191751210422));
#49523=CARTESIAN_POINT('Ctrl Pts',(54.5920295626162,27.0419571703747,16.1817575986078));
#49524=CARTESIAN_POINT('Ctrl Pts',(54.4497435299318,27.0770849236533,16.1734064550476));
#49525=CARTESIAN_POINT('Ctrl Pts',(54.1923503502196,27.1715781825362,16.1574616719917));
#49526=CARTESIAN_POINT('Ctrl Pts',(54.0766900076913,27.2271726503802,16.1499362229217));
#49527=CARTESIAN_POINT('Ctrl Pts',(53.9512779231385,27.3030750479341,16.1408503125363));
#49528=CARTESIAN_POINT('Ctrl Pts',(53.9355292029729,27.3129095538098,16.1396919383558));
#49529=CARTESIAN_POINT('Ctrl Pts',(53.9119313723182,27.3281075024208,16.1379285744878));
#49530=CARTESIAN_POINT('Ctrl Pts',(53.9039792688119,27.3333097426913,16.1373295147433));
#49531=CARTESIAN_POINT('Ctrl Pts',(53.8896652359821,27.3428206769313,16.136242255194));
#49532=CARTESIAN_POINT('Ctrl Pts',(53.883290418788,27.3471097115843,16.1357547948308));
#49533=CARTESIAN_POINT('Ctrl Pts',(53.8696629597413,27.3563932094912,16.1347056759883));
#49534=CARTESIAN_POINT('Ctrl Pts',(53.8624183148006,27.3613990687755,16.134143595276));
#49535=CARTESIAN_POINT('Ctrl Pts',(53.8430215607499,27.3749923482477,16.1326268013637));
#49536=CARTESIAN_POINT('Ctrl Pts',(53.8309321913598,27.3836679127855,16.1316687551628));
#49537=CARTESIAN_POINT('Ctrl Pts',(53.7728269335032,27.4263582834322,16.1270012236523));
#49538=CARTESIAN_POINT('Ctrl Pts',(53.7281960716767,27.4622042819646,16.1232215057134));
#49539=CARTESIAN_POINT('Ctrl Pts',(53.564243397828,27.6059094000608,16.108563118275));
#49540=CARTESIAN_POINT('Ctrl Pts',(53.456585018566,27.7261304637871,16.0972139560425));
#49541=CARTESIAN_POINT('Ctrl Pts',(53.3283951179911,27.9097016548184,16.0817586892576));
#49542=CARTESIAN_POINT('Ctrl Pts',(53.2947233113002,27.9631555857376,16.077456762131));
#49543=CARTESIAN_POINT('Ctrl Pts',(53.2568228139543,28.0301790206476,16.0723740707819));
#49544=CARTESIAN_POINT('Ctrl Pts',(53.2501300884162,28.0423075900775,16.0714662997064));
#49545=CARTESIAN_POINT('Ctrl Pts',(53.2407400725064,28.0597513277486,16.0701788162971));
#49546=CARTESIAN_POINT('Ctrl Pts',(53.2379395876584,28.0650100729875,16.069793008775));
#49547=CARTESIAN_POINT('Ctrl Pts',(53.2331285073647,28.0741427006845,16.0691271223121));
#49548=CARTESIAN_POINT('Ctrl Pts',(53.2311070019716,28.0780107521239,16.0688463690211));
#49549=CARTESIAN_POINT('Ctrl Pts',(53.226895548703,28.0861339986264,16.0682594717182));
#49550=CARTESIAN_POINT('Ctrl Pts',(53.2247082082337,28.0903904579852,16.0679534884231));
#49551=CARTESIAN_POINT('Ctrl Pts',(53.2189133266554,28.1017675463824,16.0671396226325));
#49552=CARTESIAN_POINT('Ctrl Pts',(53.2153331281141,28.1089021152602,16.0666334077133));
#49553=CARTESIAN_POINT('Ctrl Pts',(53.1998643606763,28.1401952533789,16.0644303853692));
#49554=CARTESIAN_POINT('Ctrl Pts',(53.1884221764369,28.1645728772,16.0627590835511));
#49555=CARTESIAN_POINT('Ctrl Pts',(53.09912068626,28.3652996467371,16.0493004481448));
#49556=CARTESIAN_POINT('Ctrl Pts',(53.0466992427891,28.5518680042743,16.0385865915237));
#49557=CARTESIAN_POINT('Ctrl Pts',(53.0127802526994,28.8130240365448,16.0229282389335));
#49558=CARTESIAN_POINT('Ctrl Pts',(53.0074127724654,28.883394428305,16.0186573924036));
#49559=CARTESIAN_POINT('Ctrl Pts',(53.005428202742,28.9692368710182,16.0133141479646));
#49560=CARTESIAN_POINT('Ctrl Pts',(53.0052505792685,28.9845807777245,16.0123540104904));
#49561=CARTESIAN_POINT('Ctrl Pts',(53.0052496691705,29.0087471519639,16.0108332130472));
#49562=CARTESIAN_POINT('Ctrl Pts',(53.0053078649336,29.017569214441,16.010276234499));
#49563=CARTESIAN_POINT('Ctrl Pts',(53.0055262108525,29.0340716527731,16.0092308615406));
#49564=CARTESIAN_POINT('Ctrl Pts',(53.0056722098719,29.0417520772478,16.0087429160464));
#49565=CARTESIAN_POINT('Ctrl Pts',(53.0060974962549,29.0589087799409,16.0076496815384));
#49566=CARTESIAN_POINT('Ctrl Pts',(53.0063999828318,29.0683842470709,16.0070436825613));
#49567=CARTESIAN_POINT('Ctrl Pts',(53.0074904048594,29.0963002992091,16.005251607672));
#49568=CARTESIAN_POINT('Ctrl Pts',(53.0084667367059,29.114732113191,16.0040597225994));
#49569=CARTESIAN_POINT('Ctrl Pts',(53.0158019178629,29.2243793139538,15.9969158706723));
#49570=CARTESIAN_POINT('Ctrl Pts',(53.0281673395051,29.3150326305598,15.9907810223551));
#49571=CARTESIAN_POINT('Ctrl Pts',(53.0466870408509,29.4044700806242,15.9845144320741));
#49572=CARTESIAN_POINT('',(53.0052507646772,29.0017466193016,15.8519165719564));
#49573=CARTESIAN_POINT('Ctrl Pts',(53.0466869980082,29.4044698737233,15.8273167122946));
#49574=CARTESIAN_POINT('Ctrl Pts',(53.0456184424675,29.3993094809065,15.82765853191));
#49575=CARTESIAN_POINT('Ctrl Pts',(53.0445703257718,29.3941448016429,15.8279992478323));
#49576=CARTESIAN_POINT('Ctrl Pts',(53.0427035097501,29.3847551573521,15.8286160926387));
#49577=CARTESIAN_POINT('Ctrl Pts',(53.0418780067912,29.3805316578891,15.8288925951965));
#49578=CARTESIAN_POINT('Ctrl Pts',(53.0401030767234,29.3712919003011,15.8294954045698));
#49579=CARTESIAN_POINT('Ctrl Pts',(53.0391592372855,29.3662746643889,15.8298213954536));
#49580=CARTESIAN_POINT('Ctrl Pts',(53.0372473892707,29.3558924974828,15.8304933076919));
#49581=CARTESIAN_POINT('Ctrl Pts',(53.0362820895715,29.3505271039116,15.8308390787137));
#49582=CARTESIAN_POINT('Ctrl Pts',(53.0338503748553,29.3366856194693,15.8317274689985));
#49583=CARTESIAN_POINT('Ctrl Pts',(53.0324167517075,29.3282037809664,15.8322683670757));
#49584=CARTESIAN_POINT('Ctrl Pts',(53.013969231259,29.2145940953637,15.8394699185221));
#49585=CARTESIAN_POINT('Ctrl Pts',(53.0053440331463,29.10826508465,15.8457172851574));
#49586=CARTESIAN_POINT('Ctrl Pts',(53.0052507646772,29.0017466193016,15.8519165719564));
#49587=CARTESIAN_POINT('Ctrl Pts',(53.0052507657883,29.0017478878248,15.8519164981294));
#49588=CARTESIAN_POINT('Ctrl Pts',(53.0051093436462,28.8403521130213,15.8613095998475));
#49589=CARTESIAN_POINT('Ctrl Pts',(53.0245544374861,28.6795460303851,15.870580099587));
#49590=CARTESIAN_POINT('Ctrl Pts',(53.0672282899422,28.5063299825751,15.8815629752095));
#49591=CARTESIAN_POINT('Ctrl Pts',(53.0715056526317,28.4898763927981,15.8826157811221));
#49592=CARTESIAN_POINT('Ctrl Pts',(53.0797596380104,28.4597147202466,15.8845645221717));
#49593=CARTESIAN_POINT('Ctrl Pts',(53.0836741129222,28.4459906957321,15.8854584571496));
#49594=CARTESIAN_POINT('Ctrl Pts',(53.0901792353015,28.4240781767898,15.8868978811729));
#49595=CARTESIAN_POINT('Ctrl Pts',(53.0926761362893,28.4158621952565,15.8874403327134));
#49596=CARTESIAN_POINT('Ctrl Pts',(53.0975170602289,28.4002952774349,15.8884734607162));
#49597=CARTESIAN_POINT('Ctrl Pts',(53.0998508416654,28.3929413012384,15.8889637959835));
#49598=CARTESIAN_POINT('Ctrl Pts',(53.1052591967136,28.3762358194421,15.8900829274264));
#49599=CARTESIAN_POINT('Ctrl Pts',(53.1083604298594,28.3668932194674,15.8907125850152));
#49600=CARTESIAN_POINT('Ctrl Pts',(53.1165947697249,28.3426876288607,15.8923539716098));
#49601=CARTESIAN_POINT('Ctrl Pts',(53.1218346171657,28.3278619293213,15.8933691753787));
#49602=CARTESIAN_POINT('Ctrl Pts',(53.1721208950162,28.190762376242,15.9028511894069));
#49603=CARTESIAN_POINT('Ctrl Pts',(53.2288636056454,28.0731386423043,15.9117159283036));
#49604=CARTESIAN_POINT('Ctrl Pts',(53.3351842360839,27.8986837442372,15.9259023947575));
#49605=CARTESIAN_POINT('Ctrl Pts',(53.37720369887,27.8376570293225,15.931083915525));
#49606=CARTESIAN_POINT('Ctrl Pts',(53.4552514148529,27.7368137124046,15.9399158919349));
#49607=CARTESIAN_POINT('Ctrl Pts',(53.489674658915,27.6958504963349,15.9435878306713));
#49608=CARTESIAN_POINT('Ctrl Pts',(53.5450073275289,27.6351391981811,15.9491076753616));
#49609=CARTESIAN_POINT('Ctrl Pts',(53.5647651062883,27.6143775087489,15.9510102321847));
#49610=CARTESIAN_POINT('Ctrl Pts',(53.5903604319765,27.588616827809,15.9533821248557));
#49611=CARTESIAN_POINT('Ctrl Pts',(53.5957876145509,27.5832171120518,15.9538799431939));
#49612=CARTESIAN_POINT('Ctrl Pts',(53.6041624457859,27.5749800632388,15.9546401466377));
#49613=CARTESIAN_POINT('Ctrl Pts',(53.6070878870238,27.5721204027751,15.9549042168737));
#49614=CARTESIAN_POINT('Ctrl Pts',(53.6131082598438,27.5662715120836,15.9554445913871));
#49615=CARTESIAN_POINT('Ctrl Pts',(53.6162040351187,27.5632833250053,15.9557208058892));
#49616=CARTESIAN_POINT('Ctrl Pts',(53.6232149086716,27.5565597851309,15.9563426337679));
#49617=CARTESIAN_POINT('Ctrl Pts',(53.6271355454588,27.5528303372736,15.956687796091));
#49618=CARTESIAN_POINT('Ctrl Pts',(53.6387613556214,27.541861222155,15.9577038922058));
#49619=CARTESIAN_POINT('Ctrl Pts',(53.6465091073372,27.5346666736312,15.9583715076284));
#49620=CARTESIAN_POINT('Ctrl Pts',(53.7153705472041,27.4717342354335,15.9642256051505));
#49621=CARTESIAN_POINT('Ctrl Pts',(53.7798468220845,27.419778895783,15.9691601250023));
#49622=CARTESIAN_POINT('Ctrl Pts',(53.9620610243514,27.2907728495076,15.9822610241051));
#49623=CARTESIAN_POINT('Ctrl Pts',(54.0850066333442,27.2219218087822,15.9902650108258));
#49624=CARTESIAN_POINT('Ctrl Pts',(54.2719581495117,27.1417922956407,16.0024145830526));
#49625=CARTESIAN_POINT('Ctrl Pts',(54.3308821238767,27.1197710539724,16.0062359469742));
#49626=CARTESIAN_POINT('Ctrl Pts',(54.4049500821644,27.0960131957975,16.0110790991412));
#49627=CARTESIAN_POINT('Ctrl Pts',(54.4192070524495,27.091615948398,16.012013022368));
#49628=CARTESIAN_POINT('Ctrl Pts',(54.4418816802873,27.0849000794189,16.013501605518));
#49629=CARTESIAN_POINT('Ctrl Pts',(54.4502677242869,27.0824760273333,16.0140528452591));
#49630=CARTESIAN_POINT('Ctrl Pts',(54.4660727150047,27.0780196710631,16.0150931841408));
#49631=CARTESIAN_POINT('Ctrl Pts',(54.4734880532289,27.075975078724,16.0155818761158));
#49632=CARTESIAN_POINT('Ctrl Pts',(54.4901960317847,27.0714720972271,16.0166843881663));
#49633=CARTESIAN_POINT('Ctrl Pts',(54.4994949381191,27.0690378989992,16.0172989731665));
#49634=CARTESIAN_POINT('Ctrl Pts',(54.5233093838449,27.0629875085177,16.0188755775652));
#49635=CARTESIAN_POINT('Ctrl Pts',(54.537848464713,27.0594672705629,16.0198406334626));
#49636=CARTESIAN_POINT('Ctrl Pts',(54.6317880676586,27.0378379617853,16.0260933976371));
#49637=CARTESIAN_POINT('Ctrl Pts',(54.7121849052481,27.0244445475794,16.031529174913));
#49638=CARTESIAN_POINT('Ctrl Pts',(54.9455556621049,27.0001154572308,16.0475336698631));
#49639=CARTESIAN_POINT('Ctrl Pts',(55.0992520022739,27.0018393962555,16.0583875260599));
#49640=CARTESIAN_POINT('Ctrl Pts',(55.3016285231695,27.0275322873061,16.0723361147082));
#49641=CARTESIAN_POINT('Ctrl Pts',(55.3517704300118,27.0358545932164,16.075758134992));
#49642=CARTESIAN_POINT('Ctrl Pts',(55.410658578202,27.0479565383794,16.0796962343169));
#49643=CARTESIAN_POINT('Ctrl Pts',(55.4197600113891,27.0498934170656,16.0803025657274));
#49644=CARTESIAN_POINT('Ctrl Pts',(55.4338044568427,27.0529851014715,16.0812342593709));
#49645=CARTESIAN_POINT('Ctrl Pts',(55.4387570307523,27.0540951741629,16.0815620486359));
#49646=CARTESIAN_POINT('Ctrl Pts',(55.4479033307149,27.0561819249338,16.0821659295712));
#49647=CARTESIAN_POINT('Ctrl Pts',(55.4520981085789,27.0571532733041,16.082442306671));
#49648=CARTESIAN_POINT('Ctrl Pts',(55.4616070913419,27.0593876507695,16.0830675204893));
#49649=CARTESIAN_POINT('Ctrl Pts',(55.4669192678329,27.0606589274221,16.0834158841143));
#49650=CARTESIAN_POINT('Ctrl Pts',(55.4806846852887,27.0640130194205,16.0843163907903));
#49651=CARTESIAN_POINT('Ctrl Pts',(55.4891297367667,27.0661294090049,16.084866686632));
#49652=CARTESIAN_POINT('Ctrl Pts',(55.5444459598084,27.0803775850238,16.0884586122785));
#49653=CARTESIAN_POINT('Ctrl Pts',(55.590880168795,27.0941581688365,16.0914144803056));
#49654=CARTESIAN_POINT('Ctrl Pts',(55.6476450413812,27.113279265236,16.0950059125877));
#49655=CARTESIAN_POINT('Ctrl Pts',(55.6584877042439,27.1170360647042,16.0956908919734));
#49656=CARTESIAN_POINT('Ctrl Pts',(55.711955962851,27.1360802402875,16.0990663431069));
#49657=CARTESIAN_POINT('Ctrl Pts',(55.7540862625891,27.1527229855558,16.1017187435115));
#49658=CARTESIAN_POINT('Ctrl Pts',(55.9092876909186,27.2202276968184,16.1115807550486));
#49659=CARTESIAN_POINT('Ctrl Pts',(56.0180984212386,27.2801547622904,16.1186983446739));
#49660=CARTESIAN_POINT('Ctrl Pts',(56.1696622857658,27.3830804485953,16.1296682968205));
#49661=CARTESIAN_POINT('Ctrl Pts',(56.2171706859668,27.4185344742452,16.1332765141344));
#49662=CARTESIAN_POINT('Ctrl Pts',(56.2743224744466,27.4652874101441,16.1378760007654));
#49663=CARTESIAN_POINT('Ctrl Pts',(56.2855151809648,27.4746504649457,16.1387897517996));
#49664=CARTESIAN_POINT('Ctrl Pts',(56.3031831038444,27.4897628281704,16.1402535373996));
#49665=CARTESIAN_POINT('Ctrl Pts',(56.3097254916999,27.495433068983,16.1408003472013));
#49666=CARTESIAN_POINT('Ctrl Pts',(56.3220183844732,27.5062281689726,16.1418369683236));
#49667=CARTESIAN_POINT('Ctrl Pts',(56.3277765366456,27.5113441102529,16.142326405381));
#49668=CARTESIAN_POINT('Ctrl Pts',(56.3407366928316,27.5229938251691,16.1434368923207));
#49669=CARTESIAN_POINT('Ctrl Pts',(56.3479207984152,27.5295471324476,16.1440587536812));
#49670=CARTESIAN_POINT('Ctrl Pts',(56.3663043556554,27.5465644531971,16.1456665381532));
#49671=CARTESIAN_POINT('Ctrl Pts',(56.3774314693018,27.5571053376125,16.1466557053096));
#49672=CARTESIAN_POINT('Ctrl Pts',(56.45435191277,27.6316738985952,16.1536082345949));
#49673=CARTESIAN_POINT('Ctrl Pts',(56.5157686080941,27.7000395847004,16.1597616422413));
#49674=CARTESIAN_POINT('Ctrl Pts',(56.6605648876017,27.8854852918218,16.1758908241453));
#49675=CARTESIAN_POINT('Ctrl Pts',(56.7364082231354,28.0077791680692,16.186043299444));
#49676=CARTESIAN_POINT('Ctrl Pts',(56.8199025109903,28.181809117412,16.1992306266099));
#49677=CARTESIAN_POINT('Ctrl Pts',(56.8396612364857,28.2272588317221,16.2025647506368));
#49678=CARTESIAN_POINT('Ctrl Pts',(56.8610762565936,28.2820110019831,16.2064154335477));
#49679=CARTESIAN_POINT('Ctrl Pts',(56.8643840125117,28.2906444502721,16.2070178130887));
#49680=CARTESIAN_POINT('Ctrl Pts',(56.8694100149325,28.3040406710662,16.2079447466192));
#49681=CARTESIAN_POINT('Ctrl Pts',(56.8711703030554,28.3087873772885,16.2082716894991));
#49682=CARTESIAN_POINT('Ctrl Pts',(56.8743947095208,28.3175847409548,16.2088747945427));
#49683=CARTESIAN_POINT('Ctrl Pts',(56.8758637714997,28.3216334145851,16.2091512361691));
#49684=CARTESIAN_POINT('Ctrl Pts',(56.879171923112,28.3308434665858,16.2097775881101));
#49685=CARTESIAN_POINT('Ctrl Pts',(56.8810028658543,28.3360076783692,16.2101270180079));
#49686=CARTESIAN_POINT('Ctrl Pts',(56.8857065035791,28.3494499851625,16.2110321289913));
#49687=CARTESIAN_POINT('Ctrl Pts',(56.8885460101602,28.357739683981,16.2115859314993));
#49688=CARTESIAN_POINT('Ctrl Pts',(56.9069535038081,28.4126565560172,16.2152275790398));
#49689=CARTESIAN_POINT('Ctrl Pts',(56.9208493730226,28.4598310005638,16.2182270273091));
#49690=CARTESIAN_POINT('Ctrl Pts',(56.9360826378166,28.5196162287657,16.2219237973167));
#49691=CARTESIAN_POINT('Ctrl Pts',(56.9390618649206,28.5317867559535,16.2226709879493));
#49692=CARTESIAN_POINT('Ctrl Pts',(56.9728129473247,28.6755146481478,16.2314401926524));
#49693=CARTESIAN_POINT('Ctrl Pts',(56.9902577892416,28.8098454730723,16.2391210105582));
#49694=CARTESIAN_POINT('Ctrl Pts',(56.9962201969134,29.0256685820198,16.2518384705449));
#49695=CARTESIAN_POINT('Ctrl Pts',(56.993543213177,29.1064765045103,16.2566788736578));
#49696=CARTESIAN_POINT('Ctrl Pts',(56.9840093091887,29.2077858605768,16.2629686432462));
#49697=CARTESIAN_POINT('Ctrl Pts',(56.9817137466075,29.2286448722807,16.2642753085243));
#49698=CARTESIAN_POINT('Ctrl Pts',(56.9778416813111,29.2593634888168,16.2662184359281));
#49699=CARTESIAN_POINT('Ctrl Pts',(56.9765195019449,29.2692541333232,16.266846963416));
#49700=CARTESIAN_POINT('Ctrl Pts',(56.9740412621945,29.2867898815336,16.2679666249332));
#49701=CARTESIAN_POINT('Ctrl Pts',(56.9729148491761,29.2944390194358,16.2684568204636));
#49702=CARTESIAN_POINT('Ctrl Pts',(56.9704545903423,29.3104976107706,16.2694897990369));
#49703=CARTESIAN_POINT('Ctrl Pts',(56.969111315947,29.3189054415072,16.2700328693401));
#49704=CARTESIAN_POINT('Ctrl Pts',(56.9654267056438,29.3410568769526,16.2714696689978));
#49705=CARTESIAN_POINT('Ctrl Pts',(56.9629950755614,29.3547847877656,16.2723662219427));
#49706=CARTESIAN_POINT('Ctrl Pts',(56.9519632366188,29.4134764264499,16.276226299209));
#49707=CARTESIAN_POINT('Ctrl Pts',(56.9419610538658,29.4581592889818,16.2792335787092));
#49708=CARTESIAN_POINT('Ctrl Pts',(56.8825649743854,29.6863586175012,16.2949580354118));
#49709=CARTESIAN_POINT('Ctrl Pts',(56.8086646675245,29.8624666252785,16.3084558762451));
#49710=CARTESIAN_POINT('Ctrl Pts',(56.6830430005983,30.0720790042431,16.3252012724145));
#49711=CARTESIAN_POINT('Ctrl Pts',(56.6531771657305,30.1175838011226,16.3288733808365));
#49712=CARTESIAN_POINT('Ctrl Pts',(56.61597346764,30.169507105781,16.3330588810635));
#49713=CARTESIAN_POINT('Ctrl Pts',(56.6104068330511,30.1771605494221,16.3336756838335));
#49714=CARTESIAN_POINT('Ctrl Pts',(56.601751158043,30.1888847274772,16.3346199793788));
#49715=CARTESIAN_POINT('Ctrl Pts',(56.5987006816378,30.1929835704907,16.3349500014956));
#49716=CARTESIAN_POINT('Ctrl Pts',(56.5930520797948,30.200512869864,16.335555958806));
#49717=CARTESIAN_POINT('Ctrl Pts',(56.590458613593,30.2039466262005,16.335832195089));
#49718=CARTESIAN_POINT('Ctrl Pts',(56.5845740858773,30.2116855585267,16.3364545388998));
#49719=CARTESIAN_POINT('Ctrl Pts',(56.5812765859484,30.215985726383,16.3368001919897));
#49720=CARTESIAN_POINT('Ctrl Pts',(56.5714714149679,30.2286650118085,16.3378190876345));
#49721=CARTESIAN_POINT('Ctrl Pts',(56.564914253742,30.2370058647142,16.3384889845447));
#49722=CARTESIAN_POINT('Ctrl Pts',(56.5044820789306,30.3126272672709,16.3445632649717));
#49723=CARTESIAN_POINT('Ctrl Pts',(56.4463585816557,30.3764110358905,16.3496937990699));
#49724=CARTESIAN_POINT('Ctrl Pts',(56.2851697870585,30.5317686743795,16.3628112542214));
#49725=CARTESIAN_POINT('Ctrl Pts',(56.1764379899719,30.6167776780792,16.3706626054413));
#49726=CARTESIAN_POINT('Ctrl Pts',(56.0069665063753,30.7230606888814,16.3826161142804));
#49727=CARTESIAN_POINT('Ctrl Pts',(55.9525922704674,30.7537064993419,16.3864090681107));
#49728=CARTESIAN_POINT('Ctrl Pts',(55.8836384871072,30.7884155547747,16.3912162481201));
#49729=CARTESIAN_POINT('Ctrl Pts',(55.8703280790984,30.7949306918662,16.3921439862725));
#49730=CARTESIAN_POINT('Ctrl Pts',(55.8490836385608,30.8050374943899,16.3936249666681));
#49731=CARTESIAN_POINT('Ctrl Pts',(55.8411963801974,30.8087266315008,16.3941748491635));
#49732=CARTESIAN_POINT('Ctrl Pts',(55.8262938681619,30.815578480666,16.3952140323911));
#49733=CARTESIAN_POINT('Ctrl Pts',(55.8192839551839,30.8187524774128,16.3957029359699));
#49734=CARTESIAN_POINT('Ctrl Pts',(55.803446289644,30.8258134237068,16.396807810897));
#49735=CARTESIAN_POINT('Ctrl Pts',(55.7946084056116,30.8296770411454,16.3974245610209));
#49736=CARTESIAN_POINT('Ctrl Pts',(55.7718929435755,30.8394118351872,16.3990104255696));
#49737=CARTESIAN_POINT('Ctrl Pts',(55.7579764276244,30.8451900526467,16.3999826374789));
#49738=CARTESIAN_POINT('Ctrl Pts',(55.6658497387135,30.8822235133429,16.4064240857066));
#49739=CARTESIAN_POINT('Ctrl Pts',(55.5858028016728,30.9086521379401,16.412052121815));
#49740=CARTESIAN_POINT('Ctrl Pts',(55.3847268201818,30.961197526918,16.4262481425568));
#49741=CARTESIAN_POINT('Ctrl Pts',(55.2624764953858,30.9812654972897,16.434941119093));
#49742=CARTESIAN_POINT('Ctrl Pts',(55.0700453721811,30.9947236744574,16.4482915915325));
#49743=CARTESIAN_POINT('Ctrl Pts',(55.0007102877229,30.995953487212,16.4530298627083));
#49744=CARTESIAN_POINT('Ctrl Pts',(54.9169405620533,30.9930728381702,16.4585683039943));
#49745=CARTESIAN_POINT('Ctrl Pts',(54.9024408539262,30.992415732405,16.4595201282042));
#49746=CARTESIAN_POINT('Ctrl Pts',(54.8818878658535,30.9912593857453,16.460858433786));
#49747=CARTESIAN_POINT('Ctrl Pts',(54.8758281075853,30.9908906953949,16.461251670957));
#49748=CARTESIAN_POINT('Ctrl Pts',(54.8653965885547,30.9902082034325,16.4619261835779));
#49749=CARTESIAN_POINT('Ctrl Pts',(54.8610240334727,30.9899076495183,16.4622081825729));
#49750=CARTESIAN_POINT('Ctrl Pts',(54.8519267968819,30.9892522052942,16.462793321303));
#49751=CARTESIAN_POINT('Ctrl Pts',(54.8472023621686,30.9888948923337,16.46309632605));
#49752=CARTESIAN_POINT('Ctrl Pts',(54.8347356467625,30.987907340576,16.4638936871355));
#49753=CARTESIAN_POINT('Ctrl Pts',(54.8269956053571,30.9872486973983,16.4643864930584));
#49754=CARTESIAN_POINT('Ctrl Pts',(54.7943196443121,30.9842757612931,16.4664582354515));
#49755=CARTESIAN_POINT('Ctrl Pts',(54.7694234152813,30.9815371002198,16.468015246375));
#49756=CARTESIAN_POINT('Ctrl Pts',(54.5340336729235,30.9511466752183,16.4825883654055));
#49757=CARTESIAN_POINT('Ctrl Pts',(54.3291516015137,30.8905254229942,16.4942834611104));
#49758=CARTESIAN_POINT('Ctrl Pts',(54.1046961950376,30.7829175919944,16.5092270911453));
#49759=CARTESIAN_POINT('Ctrl Pts',(54.0721731723033,30.7662109692837,16.5114454499886));
#49760=CARTESIAN_POINT('Ctrl Pts',(54.0172613934515,30.7360682258792,16.515296992248));
#49761=CARTESIAN_POINT('Ctrl Pts',(53.9946432127787,30.7230686830316,16.5169153914755));
#49762=CARTESIAN_POINT('Ctrl Pts',(53.9629591009696,30.7040223571419,16.519231427417));
#49763=CARTESIAN_POINT('Ctrl Pts',(53.9536771687933,30.6983387604725,16.5199159908968));
#49764=CARTESIAN_POINT('Ctrl Pts',(53.9377608565675,30.6884127367668,16.5211006038205));
#49765=CARTESIAN_POINT('Ctrl Pts',(53.931104166181,30.6842064187867,16.5215993262792));
#49766=CARTESIAN_POINT('Ctrl Pts',(53.9184082989524,30.676078400386,16.522556894751));
#49767=CARTESIAN_POINT('Ctrl Pts',(53.9123650988404,30.6721631892768,16.5230154957149));
#49768=CARTESIAN_POINT('Ctrl Pts',(53.8982318417188,30.6628976402545,16.524094693499));
#49769=CARTESIAN_POINT('Ctrl Pts',(53.890159403155,30.6575208839386,16.5247162667857));
#49770=CARTESIAN_POINT('Ctrl Pts',(53.8624348668058,30.6387612492481,16.5268691908446));
#49771=CARTESIAN_POINT('Ctrl Pts',(53.8429836575419,30.6250864491029,16.5284114452237));
#49772=CARTESIAN_POINT('Ctrl Pts',(53.701675760247,30.5219195468145,16.5398568095811));
#49773=CARTESIAN_POINT('Ctrl Pts',(53.5901219031113,30.4191942603955,16.5502913885636));
#49774=CARTESIAN_POINT('Ctrl Pts',(53.4355440712499,30.2404671346425,16.5667609675963));
#49775=CARTESIAN_POINT('Ctrl Pts',(53.3840105141943,30.1725445283333,16.5726991143893));
#49776=CARTESIAN_POINT('Ctrl Pts',(53.3228525960863,30.0802120750893,16.5802047619668));
#49777=CARTESIAN_POINT('Ctrl Pts',(53.3091413713342,30.0586211628707,16.5819219463752));
#49778=CARTESIAN_POINT('Ctrl Pts',(53.2869843573526,30.0222014629899,16.5847487648326));
#49779=CARTESIAN_POINT('Ctrl Pts',(53.2783070726536,30.0075177086968,16.5858700946251));
#49780=CARTESIAN_POINT('Ctrl Pts',(53.2665974380612,29.9871094268052,16.5874015175642));
#49781=CARTESIAN_POINT('Ctrl Pts',(53.2634033247451,29.9814792165496,16.5878211995808));
#49782=CARTESIAN_POINT('Ctrl Pts',(53.2580560243589,29.971945789255,16.588526979446));
#49783=CARTESIAN_POINT('Ctrl Pts',(53.2558884291839,29.9680507535276,16.58881397811));
#49784=CARTESIAN_POINT('Ctrl Pts',(53.2517754072555,29.9606012460005,16.5893602456651));
#49785=CARTESIAN_POINT('Ctrl Pts',(53.2498277351428,29.9570480784841,16.589619661434));
#49786=CARTESIAN_POINT('Ctrl Pts',(53.2452187597631,29.9485787326357,16.5902353674182));
#49787=CARTESIAN_POINT('Ctrl Pts',(53.2425672520202,29.9436572212489,16.590591045347));
#49788=CARTESIAN_POINT('Ctrl Pts',(53.2332452772804,29.926178965255,16.5918469836628));
#49789=CARTESIAN_POINT('Ctrl Pts',(53.2266882273536,29.9135617712372,16.5927404757286));
#49790=CARTESIAN_POINT('Ctrl Pts',(53.1543099606901,29.770574106496,16.6027310574458));
#49791=CARTESIAN_POINT('Ctrl Pts',(53.1028523696274,29.6334035079832,16.6110794161731));
#49792=CARTESIAN_POINT('Ctrl Pts',(53.0594626196383,29.4628561496766,16.6213130063293));
#49793=CARTESIAN_POINT('Ctrl Pts',(53.0527458528725,29.4337300029892,16.6230547010837));
#49794=CARTESIAN_POINT('Ctrl Pts',(53.0466869925414,29.4044698473222,16.6248055079682));
#49795=CARTESIAN_POINT('Origin',(55.,29.,3.45145488139523));
#49796=CARTESIAN_POINT('',(53.0466869985623,29.4044698763992,17.581803907097));
#49797=CARTESIAN_POINT('',(53.0466869493682,29.4044696388253,17.4239266846335));
#49798=CARTESIAN_POINT('',(53.0466869980082,29.4044698737233,3.45145488139523));
#49799=CARTESIAN_POINT('',(53.0052506867316,28.9983447914819,16.808800702469));
#49800=CARTESIAN_POINT('Ctrl Pts',(53.0466869985623,29.4044698763992,17.581803907097));
#49801=CARTESIAN_POINT('Ctrl Pts',(53.0535381681538,29.4375563419659,17.5797310997435));
#49802=CARTESIAN_POINT('Ctrl Pts',(53.0612300479194,29.4704689730775,17.5776932705287));
#49803=CARTESIAN_POINT('Ctrl Pts',(53.0938908516641,29.5957598515763,17.5699744739283));
#49804=CARTESIAN_POINT('Ctrl Pts',(53.1246568243288,29.686492379341,17.5644613216537));
#49805=CARTESIAN_POINT('Ctrl Pts',(53.2128129037564,29.895674240343,17.5512636247914));
#49806=CARTESIAN_POINT('Ctrl Pts',(53.2756234352799,30.0113303012941,17.543550655876));
#49807=CARTESIAN_POINT('Ctrl Pts',(53.3581799806064,30.133006073438,17.5344254532823));
#49808=CARTESIAN_POINT('Ctrl Pts',(53.3671788955301,30.1459367160742,17.5334422965875));
#49809=CARTESIAN_POINT('Ctrl Pts',(53.3820533089232,30.1667789607287,17.5318348883462));
#49810=CARTESIAN_POINT('Ctrl Pts',(53.3878360472386,30.1747561543626,17.5312141567916));
#49811=CARTESIAN_POINT('Ctrl Pts',(53.3982526552653,30.1889039278494,17.5301032269704));
#49812=CARTESIAN_POINT('Ctrl Pts',(53.4028637108962,30.1950911167491,17.5296139144155));
#49813=CARTESIAN_POINT('Ctrl Pts',(53.4126786850509,30.2081027513415,17.5285774380986));
#49814=CARTESIAN_POINT('Ctrl Pts',(53.417890966705,30.2149206631241,17.5280299546567));
#49815=CARTESIAN_POINT('Ctrl Pts',(53.4318737956573,30.2329682867523,17.5265688674668));
#49816=CARTESIAN_POINT('Ctrl Pts',(53.4407208178199,30.2441378555194,17.5256522661133));
#49817=CARTESIAN_POINT('Ctrl Pts',(53.4842138998157,30.2978562227251,17.5211827777587));
#49818=CARTESIAN_POINT('Ctrl Pts',(53.5204830046658,30.3390544333428,17.5175652268632));
#49819=CARTESIAN_POINT('Ctrl Pts',(53.7005121844257,30.5272965410038,17.5000923933763));
#49820=CARTESIAN_POINT('Ctrl Pts',(53.8647087262536,30.6529955110114,17.4853582103319));
#49821=CARTESIAN_POINT('Ctrl Pts',(54.0724913873703,30.7662736313456,17.4694116497016));
#49822=CARTESIAN_POINT('Ctrl Pts',(54.100143311368,30.7805204186495,17.4673420523021));
#49823=CARTESIAN_POINT('Ctrl Pts',(54.1356841566394,30.7977921003784,17.4647582678335));
#49824=CARTESIAN_POINT('Ctrl Pts',(54.1432728207524,30.8014207891586,17.4642109214754));
#49825=CARTESIAN_POINT('Ctrl Pts',(54.1553006938363,30.807078986864,17.4633504928221));
#49826=CARTESIAN_POINT('Ctrl Pts',(54.1597246844119,30.8091403422196,17.4630355261175));
#49827=CARTESIAN_POINT('Ctrl Pts',(54.1680937508903,30.8130025816279,17.4624425959009));
#49828=CARTESIAN_POINT('Ctrl Pts',(54.1720370909655,30.8148068188967,17.4621644396664));
#49829=CARTESIAN_POINT('Ctrl Pts',(54.1812359971743,30.8189794662923,17.4615183580629));
#49830=CARTESIAN_POINT('Ctrl Pts',(54.1864959767656,30.8213379689892,17.4611510354285));
#49831=CARTESIAN_POINT('Ctrl Pts',(54.2034378144508,30.8288464209236,17.4599744664441));
#49832=CARTESIAN_POINT('Ctrl Pts',(54.2151591899121,30.8339071594355,17.4591704019459));
#49833=CARTESIAN_POINT('Ctrl Pts',(54.2430500915498,30.8456327461047,17.4572787816351));
#49834=CARTESIAN_POINT('Ctrl Pts',(54.25926050137,30.8521982714125,17.4561964220564));
#49835=CARTESIAN_POINT('Ctrl Pts',(54.3187665994462,30.8753931554573,17.4522779180653));
#49836=CARTESIAN_POINT('Ctrl Pts',(54.3625547026584,30.890725390171,17.4494990516173));
#49837=CARTESIAN_POINT('Ctrl Pts',(54.5585261018975,30.9517604376265,17.4373591276503));
#49838=CARTESIAN_POINT('Ctrl Pts',(54.7153106748265,30.9807126760047,17.4283769401918));
#49839=CARTESIAN_POINT('Ctrl Pts',(54.9333902267673,30.9945293017382,17.4153048114855));
#49840=CARTESIAN_POINT('Ctrl Pts',(54.9930409514654,30.9956288600365,17.4116769903123));
#49841=CARTESIAN_POINT('Ctrl Pts',(55.0677068979847,30.9936575140025,17.4070284306335));
#49842=CARTESIAN_POINT('Ctrl Pts',(55.082761010887,30.9930893363719,17.406085786113));
#49843=CARTESIAN_POINT('Ctrl Pts',(55.1066445569654,30.9919168639485,17.4045810847275));
#49844=CARTESIAN_POINT('Ctrl Pts',(55.1154790846982,30.9914242218461,17.4040224995904));
#49845=CARTESIAN_POINT('Ctrl Pts',(55.1319745795703,30.9903942445524,17.4029756780733));
#49846=CARTESIAN_POINT('Ctrl Pts',(55.1396363132616,30.9898714118591,17.4024879021486));
#49847=CARTESIAN_POINT('Ctrl Pts',(55.1567146650854,30.9886068735467,17.4013970752679));
#49848=CARTESIAN_POINT('Ctrl Pts',(55.166129370669,30.9878425015409,17.4007933287865));
#49849=CARTESIAN_POINT('Ctrl Pts',(55.1937551486907,30.9854019626926,17.3990144784027));
#49850=CARTESIAN_POINT('Ctrl Pts',(55.2119486220281,30.9835422244071,17.3978336941341));
#49851=CARTESIAN_POINT('Ctrl Pts',(55.2531565645805,30.978756544452,17.3951373853378));
#49852=CARTESIAN_POINT('Ctrl Pts',(55.2761503950709,30.9756787678862,17.3936173216041));
#49853=CARTESIAN_POINT('Ctrl Pts',(55.3518863522303,30.9641933982191,17.3885581173148));
#49854=CARTESIAN_POINT('Ctrl Pts',(55.4043411466839,30.9540693785939,17.3849688916255));
#49855=CARTESIAN_POINT('Ctrl Pts',(55.5638922877239,30.9165758966246,17.3738002372527));
#49856=CARTESIAN_POINT('Ctrl Pts',(55.6691691546217,30.8824045962201,17.366065227641));
#49857=CARTESIAN_POINT('Ctrl Pts',(55.8568452662251,30.8037445639532,17.351914665903));
#49858=CARTESIAN_POINT('Ctrl Pts',(55.9400158894148,30.7618321367739,17.3455051536004));
#49859=CARTESIAN_POINT('Ctrl Pts',(56.0291031993863,30.7088262697652,17.3386962997571));
#49860=CARTESIAN_POINT('Ctrl Pts',(56.0381973701369,30.7033164261879,17.3380019966732));
#49861=CARTESIAN_POINT('Ctrl Pts',(56.0518635063517,30.6948864694617,17.33696029324));
#49862=CARTESIAN_POINT('Ctrl Pts',(56.0564681614387,30.6920200961869,17.3366095885707));
#49863=CARTESIAN_POINT('Ctrl Pts',(56.0647052140231,30.6868458403245,17.335982824003));
#49864=CARTESIAN_POINT('Ctrl Pts',(56.0683418732225,30.6845449607527,17.3357063220728));
#49865=CARTESIAN_POINT('Ctrl Pts',(56.0762766320209,30.6794886835234,17.3351035033189));
#49866=CARTESIAN_POINT('Ctrl Pts',(56.0805716037684,30.6767285520455,17.3347775024975));
#49867=CARTESIAN_POINT('Ctrl Pts',(56.0927817748795,30.6688153754126,17.3338514191313));
#49868=CARTESIAN_POINT('Ctrl Pts',(56.1006711648465,30.663622481183,17.333253893963));
#49869=CARTESIAN_POINT('Ctrl Pts',(56.1533820446094,30.6283884115258,17.3292652751113));
#49870=CARTESIAN_POINT('Ctrl Pts',(56.1970099180198,30.5965924183431,17.3259813070043));
#49871=CARTESIAN_POINT('Ctrl Pts',(56.3836949436426,30.4485763496265,17.3117513026923));
#49872=CARTESIAN_POINT('Ctrl Pts',(56.5115330081187,30.3146334040807,17.3014375781602));
#49873=CARTESIAN_POINT('Ctrl Pts',(56.6489110046309,30.123704920779,17.2872816866688));
#49874=CARTESIAN_POINT('Ctrl Pts',(56.6770544045998,30.0812530293964,17.2841701925491));
#49875=CARTESIAN_POINT('Ctrl Pts',(56.7110752607927,30.0254066092997,17.2800961808225));
#49876=CARTESIAN_POINT('Ctrl Pts',(56.7184739950843,30.012958228827,17.2791893039776));
#49877=CARTESIAN_POINT('Ctrl Pts',(56.730066196122,29.9929617571221,17.2777339692156));
#49878=CARTESIAN_POINT('Ctrl Pts',(56.7343474153583,29.9854649324761,17.2771886705749));
#49879=CARTESIAN_POINT('Ctrl Pts',(56.7419801946523,29.9718954016438,17.2762021199146));
#49880=CARTESIAN_POINT('Ctrl Pts',(56.7453490196844,29.9658325257545,17.2757614926161));
#49881=CARTESIAN_POINT('Ctrl Pts',(56.7532029653917,29.9515224935127,17.2747218119821));
#49882=CARTESIAN_POINT('Ctrl Pts',(56.7576615909594,29.9432610562505,17.2741218332623));
#49883=CARTESIAN_POINT('Ctrl Pts',(56.7705014750913,29.9190627372125,17.2723649969866));
#49884=CARTESIAN_POINT('Ctrl Pts',(56.7787252845113,29.9030438059255,17.2712026703299));
#49885=CARTESIAN_POINT('Ctrl Pts',(56.7968455484423,29.8665397520384,17.2685547410683));
#49886=CARTESIAN_POINT('Ctrl Pts',(56.8066105386457,29.8459925288005,17.2670648289233));
#49887=CARTESIAN_POINT('Ctrl Pts',(56.8374970839021,29.7780272323461,17.2621372635663));
#49888=CARTESIAN_POINT('Ctrl Pts',(56.8571181352503,29.7299543749127,17.258652379659));
#49889=CARTESIAN_POINT('Ctrl Pts',(56.9184682066805,29.5610965237657,17.246424303392));
#49890=CARTESIAN_POINT('Ctrl Pts',(56.9504561619717,29.4371105736198,17.2374449395276));
#49891=CARTESIAN_POINT('Ctrl Pts',(56.9825844734383,29.2335147737168,17.2231647760945));
#49892=CARTESIAN_POINT('Ctrl Pts',(56.9902294348302,29.1554347421957,17.2178021227409));
#49893=CARTESIAN_POINT('Ctrl Pts',(56.9936658735568,29.0665921570856,17.2119636188883));
#49894=CARTESIAN_POINT('Ctrl Pts',(56.9939892182602,29.056081545185,17.211277095355));
#49895=CARTESIAN_POINT('Ctrl Pts',(56.9943527715682,29.0401712751975,17.2102447357551));
#49896=CARTESIAN_POINT('Ctrl Pts',(56.9944541913453,29.0347733963088,17.2098956806203));
#49897=CARTESIAN_POINT('Ctrl Pts',(56.9945970495816,29.0250734938898,17.2092706584106));
#49898=CARTESIAN_POINT('Ctrl Pts',(56.9946464868534,29.0207717076191,17.2089942603481));
#49899=CARTESIAN_POINT('Ctrl Pts',(56.9947243286119,29.0113440975971,17.2083902563178));
#49900=CARTESIAN_POINT('Ctrl Pts',(56.9947468936236,29.0062183196711,17.2080629756295));
#49901=CARTESIAN_POINT('Ctrl Pts',(56.9947549257927,28.9915519540209,17.2071295754828));
#49902=CARTESIAN_POINT('Ctrl Pts',(56.9946917054074,28.9820113263388,17.2065260772961));
#49903=CARTESIAN_POINT('Ctrl Pts',(56.993783157081,28.9161835186509,17.2023852998064));
#49904=CARTESIAN_POINT('Ctrl Pts',(56.9906238214904,28.8599480384416,17.198964739783));
#49905=CARTESIAN_POINT('Ctrl Pts',(56.975669469355,28.7085549220737,17.1898942195664));
#49906=CARTESIAN_POINT('Ctrl Pts',(56.9593900436916,28.6139913383113,17.1843726036092));
#49907=CARTESIAN_POINT('Ctrl Pts',(56.9048245527289,28.3934266316467,17.1711625266656));
#49908=CARTESIAN_POINT('Ctrl Pts',(56.8607571770135,28.2693400215482,17.1634458349897));
#49909=CARTESIAN_POINT('Ctrl Pts',(56.7981092238956,28.1362414063239,17.1543165136526));
#49910=CARTESIAN_POINT('Ctrl Pts',(56.7912324572086,28.1220695065229,17.1533334531046));
#49911=CARTESIAN_POINT('Ctrl Pts',(56.77978296218,28.0991685858964,17.1517261710412));
#49912=CARTESIAN_POINT('Ctrl Pts',(56.7753120427761,28.0903892182327,17.1511054685904));
#49913=CARTESIAN_POINT('Ctrl Pts',(56.76722380808,28.0747934731403,17.1499945711783));
#49914=CARTESIAN_POINT('Ctrl Pts',(56.7636316076198,28.0679642415244,17.1495052617317));
#49915=CARTESIAN_POINT('Ctrl Pts',(56.7559605674234,28.0535837570758,17.148468771439));
#49916=CARTESIAN_POINT('Ctrl Pts',(56.7518724462376,28.0460376592555,17.1479212707881));
#49917=CARTESIAN_POINT('Ctrl Pts',(56.740867253046,28.0260329418747,17.1464600888447));
#49918=CARTESIAN_POINT('Ctrl Pts',(56.7338652603423,28.0136218450065,17.1455434092596));
#49919=CARTESIAN_POINT('Ctrl Pts',(56.6992519433195,27.9537769300455,17.1410728918009));
#49920=CARTESIAN_POINT('Ctrl Pts',(56.6698261923115,27.9074253324099,17.1374543538894));
#49921=CARTESIAN_POINT('Ctrl Pts',(56.5211582989487,27.6933027768657,17.1199678266363));
#49922=CARTESIAN_POINT('Ctrl Pts',(56.3783633923795,27.5434727421367,17.1052191104057));
#49923=CARTESIAN_POINT('Ctrl Pts',(56.1906809541047,27.3992929842158,17.089274136507));
#49924=CARTESIAN_POINT('Ctrl Pts',(56.1657183216661,27.3810234314543,17.0872162566158));
#49925=CARTESIAN_POINT('Ctrl Pts',(56.1334515375371,27.3585416095927,17.0846449066322));
#49926=CARTESIAN_POINT('Ctrl Pts',(56.1265333593992,27.3537859703194,17.0840986509278));
#49927=CARTESIAN_POINT('Ctrl Pts',(56.1155488961026,27.3463367914275,17.0832395438774));
#49928=CARTESIAN_POINT('Ctrl Pts',(56.1115024952881,27.3436143108617,17.0829248176192));
#49929=CARTESIAN_POINT('Ctrl Pts',(56.1038385121663,27.3384985961421,17.0823320733395));
#49930=CARTESIAN_POINT('Ctrl Pts',(56.1002231481101,27.3361023466941,17.0820538643899));
#49931=CARTESIAN_POINT('Ctrl Pts',(56.0917790326205,27.3305451749219,17.0814073035615));
#49932=CARTESIAN_POINT('Ctrl Pts',(56.0869443507301,27.327393396685,17.0810395573126));
#49933=CARTESIAN_POINT('Ctrl Pts',(56.0713401172818,27.3173170694722,17.0798602398985));
#49934=CARTESIAN_POINT('Ctrl Pts',(56.0605172982703,27.3104750455651,17.0790538845301));
#49935=CARTESIAN_POINT('Ctrl Pts',(55.9651537695647,27.2514651179554,17.0720428720727));
#49936=CARTESIAN_POINT('Ctrl Pts',(55.8768797952597,27.2055688613344,17.0661920095469));
#49937=CARTESIAN_POINT('Ctrl Pts',(55.6282143070381,27.099034524664,17.0504248779519));
#49938=CARTESIAN_POINT('Ctrl Pts',(55.4628842776193,27.0521664452302,17.0406303679596));
#49939=CARTESIAN_POINT('Ctrl Pts',(55.2712991874232,27.0236566834948,17.0286779132244));
#49940=CARTESIAN_POINT('Ctrl Pts',(55.2489388964172,27.0207159082614,17.027275287131));
#49941=CARTESIAN_POINT('Ctrl Pts',(55.2164400850321,27.0170011409015,17.0252236209845));
#49942=CARTESIAN_POINT('Ctrl Pts',(55.2063374220252,27.0159244853656,17.0245840145233));
#49943=CARTESIAN_POINT('Ctrl Pts',(55.1884826768431,27.0141595216324,17.0234502209378));
#49944=CARTESIAN_POINT('Ctrl Pts',(55.1807339086403,27.0134393096412,17.0229570389746));
#49945=CARTESIAN_POINT('Ctrl Pts',(55.1646618709513,27.0120403005558,17.0219316872968));
#49946=CARTESIAN_POINT('Ctrl Pts',(55.1563381695954,27.0113683921812,17.0213993129675));
#49947=CARTESIAN_POINT('Ctrl Pts',(55.134851106143,27.0097696433391,17.0200214397622));
#49948=CARTESIAN_POINT('Ctrl Pts',(55.1216824918756,27.0089211339618,17.0191735226355));
#49949=CARTESIAN_POINT('Ctrl Pts',(55.0649970952024,27.005833095605,17.0155080491662));
#49950=CARTESIAN_POINT('Ctrl Pts',(55.0214245833406,27.0048892852,17.0126507552212));
#49951=CARTESIAN_POINT('Ctrl Pts',(54.8190704443571,27.0071355050272,16.9991873921537));
#49952=CARTESIAN_POINT('Ctrl Pts',(54.6610791641538,27.0278534440817,16.9880583516065));
#49953=CARTESIAN_POINT('Ctrl Pts',(54.4228685544033,27.0885791987382,16.970985457503));
#49954=CARTESIAN_POINT('Ctrl Pts',(54.3399775022593,27.1155945106876,16.9650016216296));
#49955=CARTESIAN_POINT('Ctrl Pts',(54.2492525370051,27.1518878508919,16.9585836787932));
#49956=CARTESIAN_POINT('Ctrl Pts',(54.2394270271168,27.15590970026,16.9578904551627));
#49957=CARTESIAN_POINT('Ctrl Pts',(54.2246340220044,27.1621032284541,16.9568500476466));
#49958=CARTESIAN_POINT('Ctrl Pts',(54.2196426841745,27.164216950726,16.9564995713297));
#49959=CARTESIAN_POINT('Ctrl Pts',(54.2107042831989,27.1680452102899,16.9558730486546));
#49960=CARTESIAN_POINT('Ctrl Pts',(54.206754110838,27.1697521915009,16.9555965617919));
#49961=CARTESIAN_POINT('Ctrl Pts',(54.2027934097233,27.1714789541209,16.9553197365329));
#49962=CARTESIAN_POINT('Ctrl Pts',(54.2027774475001,27.1714859134837,16.9553186208917));
#49963=CARTESIAN_POINT('Ctrl Pts',(54.2027457625764,27.1714997282734,16.9553164063629));
#49964=CARTESIAN_POINT('Ctrl Pts',(54.2027300387601,27.1715065841795,16.955315307397));
#49965=CARTESIAN_POINT('Ctrl Pts',(54.2026988231264,27.1715201953148,16.9553131256925));
#49966=CARTESIAN_POINT('Ctrl Pts',(54.2026833324532,27.1715269500379,16.9553120430336));
#49967=CARTESIAN_POINT('Ctrl Pts',(54.2026525813444,27.1715403595539,16.9553098938193));
#49968=CARTESIAN_POINT('Ctrl Pts',(54.2026373204142,27.1715470145555,16.9553088272291));
#49969=CARTESIAN_POINT('Ctrl Pts',(54.2026070256313,27.171560225986,16.9553067099308));
#49970=CARTESIAN_POINT('Ctrl Pts',(54.2025919911115,27.171566782699,16.9553056591759));
#49971=CARTESIAN_POINT('Ctrl Pts',(54.2025621435818,27.1715797999605,16.9553035731585));
#49972=CARTESIAN_POINT('Ctrl Pts',(54.202547331179,27.1715862602377,16.9553025379383));
#49973=CARTESIAN_POINT('Ctrl Pts',(54.2025179247056,27.1715990859941,16.9553004827678));
#49974=CARTESIAN_POINT('Ctrl Pts',(54.2025033308667,27.1716054513659,16.9552994628335));
#49975=CARTESIAN_POINT('Ctrl Pts',(54.2024743579551,27.1716180888482,16.9552974379851));
#49976=CARTESIAN_POINT('Ctrl Pts',(54.2024599790974,27.1716243608588,16.9552964330859));
#49977=CARTESIAN_POINT('Ctrl Pts',(54.2024314323554,27.171636813255,16.955294438042));
#49978=CARTESIAN_POINT('Ctrl Pts',(54.2024172647329,27.1716429935205,16.9552934479155));
#49979=CARTESIAN_POINT('Ctrl Pts',(54.2023891377923,27.171655263573,16.9552914822301));
#49980=CARTESIAN_POINT('Ctrl Pts',(54.2023751781523,27.1716613534948,16.9552905066487));
#49981=CARTESIAN_POINT('Ctrl Pts',(54.2023474637385,27.1716734443429,16.9552885698126));
#49982=CARTESIAN_POINT('Ctrl Pts',(54.2023337087108,27.1716794453745,16.9552876085402));
#49983=CARTESIAN_POINT('Ctrl Pts',(54.202306399932,27.1716913599916,16.9552857000709));
#49984=CARTESIAN_POINT('Ctrl Pts',(54.2022928460989,27.1716972736077,16.9552847528682));
#49985=CARTESIAN_POINT('Ctrl Pts',(54.2022659365562,27.1717090147535,16.9552828723178));
#49986=CARTESIAN_POINT('Ctrl Pts',(54.2022525807084,27.1717148423384,16.9552819389602));
#49987=CARTESIAN_POINT('Ctrl Pts',(54.2022260638523,27.1717264128393,16.95528008587));
#49988=CARTESIAN_POINT('Ctrl Pts',(54.2022129028588,27.1717321557438,16.9552791661382));
#49989=CARTESIAN_POINT('Ctrl Pts',(54.2021867718216,27.1717435585663,16.9552773400276));
#49990=CARTESIAN_POINT('Ctrl Pts',(54.2021738022083,27.1717492182916,16.9552764336786));
#49991=CARTESIAN_POINT('Ctrl Pts',(54.2021477040113,27.1717606074448,16.9552746098798));
#49992=CARTESIAN_POINT('Ctrl Pts',(54.202134575331,27.1717663369189,16.9552736924234));
#49993=CARTESIAN_POINT('Ctrl Pts',(54.2021083594329,27.1717777781088,16.9552718604166));
#49994=CARTESIAN_POINT('Ctrl Pts',(54.2020952722161,27.1717834898229,16.9552709458663));
#49995=CARTESIAN_POINT('Ctrl Pts',(54.2020691376536,27.1717948961843,16.9552691195604));
#49996=CARTESIAN_POINT('Ctrl Pts',(54.2020560909416,27.1718005905539,16.9552682078491));
#49997=CARTESIAN_POINT('Ctrl Pts',(54.2020300393818,27.1718119613529,16.9552663873605));
#49998=CARTESIAN_POINT('Ctrl Pts',(54.2020170336725,27.1718176381574,16.955265478523));
#49999=CARTESIAN_POINT('Ctrl Pts',(54.2019910627921,27.1718289744019,16.9552636636891));
#50000=CARTESIAN_POINT('Ctrl Pts',(54.2019780975008,27.1718346338934,16.9552627576844));
#50001=CARTESIAN_POINT('Ctrl Pts',(54.2019522079513,27.1718459352929,16.9552609485507));
#50002=CARTESIAN_POINT('Ctrl Pts',(54.2019392832992,27.1718515773718,16.9552600453941));
#50003=CARTESIAN_POINT('Ctrl Pts',(54.2019134729174,27.1718628448645,16.9552582418092));
#50004=CARTESIAN_POINT('Ctrl Pts',(54.201900587917,27.1718684699589,16.9552573414317));
#50005=CARTESIAN_POINT('Ctrl Pts',(54.2018748580515,27.17187970295,16.9552555434897));
#50006=CARTESIAN_POINT('Ctrl Pts',(54.2018620128074,27.1718853110112,16.9552546458986));
#50007=CARTESIAN_POINT('Ctrl Pts',(54.2018363625221,27.1718965099035,16.9552528535338));
#50008=CARTESIAN_POINT('Ctrl Pts',(54.2018235570324,27.1719021009293,16.9552519587288));
#50009=CARTESIAN_POINT('Ctrl Pts',(54.2017979855248,27.171913266067,16.9552501718851));
#50010=CARTESIAN_POINT('Ctrl Pts',(54.2017852197049,27.1719188400915,16.9552492798603));
#50011=CARTESIAN_POINT('Ctrl Pts',(54.2017597250103,27.1719299723268,16.9552474984002));
#50012=CARTESIAN_POINT('Ctrl Pts',(54.2017469974417,27.1719355299664,16.9552466090563));
#50013=CARTESIAN_POINT('Ctrl Pts',(54.201721582803,27.1719466278773,16.9552448332063));
#50014=CARTESIAN_POINT('Ctrl Pts',(54.2017088946066,27.1719521686396,16.9552439466216));
#50015=CARTESIAN_POINT('Ctrl Pts',(54.201683555894,27.1719632340239,16.955242176093));
#50016=CARTESIAN_POINT('Ctrl Pts',(54.2016709058875,27.1719687584223,16.9552412921847));
#50017=CARTESIAN_POINT('Ctrl Pts',(54.2016456455027,27.1719797902253,16.9552395271451));
#50018=CARTESIAN_POINT('Ctrl Pts',(54.2016330344284,27.1719852979329,16.9552386459652));
#50019=CARTESIAN_POINT('Ctrl Pts',(54.2016078487016,27.1719962977517,16.9552368861581));
#50020=CARTESIAN_POINT('Ctrl Pts',(54.2015952750726,27.1720017894151,16.9552360076024));
#50021=CARTESIAN_POINT('Ctrl Pts',(54.2015701672082,27.1720127558445,16.9552342532515));
#50022=CARTESIAN_POINT('Ctrl Pts',(54.2015576319523,27.1720182310555,16.9552333773849));
#50023=CARTESIAN_POINT('Ctrl Pts',(54.1967690964865,27.1741098498789,16.9548987931142));
#50024=CARTESIAN_POINT('Ctrl Pts',(54.192001225686,27.176214731155,16.9545662203758));
#50025=CARTESIAN_POINT('Ctrl Pts',(54.1781245656607,27.1824059861494,16.953599785945));
#50026=CARTESIAN_POINT('Ctrl Pts',(54.1690379795318,27.1865421540539,16.9529688485702));
#50027=CARTESIAN_POINT('Ctrl Pts',(54.1482171172537,27.1962090614782,16.9515266383903));
#50028=CARTESIAN_POINT('Ctrl Pts',(54.1365048537253,27.2017864474003,16.9507179441833));
#50029=CARTESIAN_POINT('Ctrl Pts',(54.0119497578688,27.2625972458452,16.9421368224733));
#50030=CARTESIAN_POINT('Ctrl Pts',(53.9044964916336,27.3282667851673,16.9348896110096));
#50031=CARTESIAN_POINT('Ctrl Pts',(53.6977385654398,27.4831782467005,16.9198861400974));
#50032=CARTESIAN_POINT('Ctrl Pts',(53.5997672214793,27.5731238130959,16.9121501946306));
#50033=CARTESIAN_POINT('Ctrl Pts',(53.4952419008201,27.6902963111776,16.9024836744009));
#50034=CARTESIAN_POINT('Ctrl Pts',(53.4793644126827,27.7087649244213,16.9009716779454));
#50035=CARTESIAN_POINT('Ctrl Pts',(53.4575913232255,27.7350499350715,16.898833272468));
#50036=CARTESIAN_POINT('Ctrl Pts',(53.4514086539015,27.7426265350641,16.8982184170669));
#50037=CARTESIAN_POINT('Ctrl Pts',(53.440758260902,27.7558758515742,16.897145696228));
#50038=CARTESIAN_POINT('Ctrl Pts',(53.4362651284139,27.761527978995,16.8966888514168));
#50039=CARTESIAN_POINT('Ctrl Pts',(53.4269466128665,27.7733817435062,16.8957322868379));
#50040=CARTESIAN_POINT('Ctrl Pts',(53.4221269977021,27.7795877370038,16.8952323508454));
#50041=CARTESIAN_POINT('Ctrl Pts',(53.4107759066309,27.7943836477883,16.894042398161));
#50042=CARTESIAN_POINT('Ctrl Pts',(53.4042772726416,27.8029983385437,16.893351117135));
#50043=CARTESIAN_POINT('Ctrl Pts',(53.3826411528737,27.8321688481488,16.8910152409741));
#50044=CARTESIAN_POINT('Ctrl Pts',(53.3678289568953,27.8529617155225,16.8893582696848));
#50045=CARTESIAN_POINT('Ctrl Pts',(53.3139491573439,27.9317538349862,16.8831062916893));
#50046=CARTESIAN_POINT('Ctrl Pts',(53.2775445556309,27.9915047351612,16.8784161761032));
#50047=CARTESIAN_POINT('Ctrl Pts',(53.2164548514914,28.1047635971426,16.8696291260683));
#50048=CARTESIAN_POINT('Ctrl Pts',(53.1908559343621,28.1576944646641,16.8655616077109));
#50049=CARTESIAN_POINT('Ctrl Pts',(53.1427675624629,28.2694702538247,16.8570952172123));
#50050=CARTESIAN_POINT('Ctrl Pts',(53.1206511797414,28.3284092350215,16.8526976972126));
#50051=CARTESIAN_POINT('Ctrl Pts',(53.0775342578781,28.4622378848971,16.8429585405376));
#50052=CARTESIAN_POINT('Ctrl Pts',(53.0580484270442,28.5375181385459,16.8376449679266));
#50053=CARTESIAN_POINT('Ctrl Pts',(53.040968361574,28.6240572391024,16.8318525687653));
#50054=CARTESIAN_POINT('Ctrl Pts',(53.0390156215005,28.6343797071378,16.8311667096999));
#50055=CARTESIAN_POINT('Ctrl Pts',(53.0361832923671,28.6500276804763,16.8301351486327));
#50056=CARTESIAN_POINT('Ctrl Pts',(53.03524365311,28.655341930869,16.8297862347986));
#50057=CARTESIAN_POINT('Ctrl Pts',(53.0335937438138,28.6648992613888,16.8291613612945));
#50058=CARTESIAN_POINT('Ctrl Pts',(53.0328756258493,28.6691408652251,16.8288849715844));
#50059=CARTESIAN_POINT('Ctrl Pts',(53.0315009213921,28.6774233448767,16.828347095018));
#50060=CARTESIAN_POINT('Ctrl Pts',(53.030843055287,28.6814638973008,16.8280855343157));
#50061=CARTESIAN_POINT('Ctrl Pts',(53.0293981313878,28.6905140507565,16.8275015017758));
#50062=CARTESIAN_POINT('Ctrl Pts',(53.0286177249731,28.6955247064408,16.8271793958916));
#50063=CARTESIAN_POINT('Ctrl Pts',(53.0267038510002,28.7081287718775,16.8263721617139));
#50064=CARTESIAN_POINT('Ctrl Pts',(53.0255950869262,28.7157259262221,16.8258883385404));
#50065=CARTESIAN_POINT('Ctrl Pts',(53.0117703005564,28.8144369969873,16.8196352878344));
#50066=CARTESIAN_POINT('Ctrl Pts',(53.0053270402533,28.9063285088114,16.8141802815779));
#50067=CARTESIAN_POINT('Ctrl Pts',(53.0052506867316,28.9983447914819,16.808800702469));
#50068=CARTESIAN_POINT('Ctrl Pts',(53.0052506883683,28.9983428202296,16.808800817715));
#50069=CARTESIAN_POINT('Ctrl Pts',(53.0051373356856,29.1347855826284,16.8008239164537));
#50070=CARTESIAN_POINT('Ctrl Pts',(53.0190227966867,29.2708706932225,16.793027499536));
#50071=CARTESIAN_POINT('Ctrl Pts',(53.046686998698,29.4044698770549,16.7848524498588));
#50072=CARTESIAN_POINT('Ctrl Pts',(53.0466869925414,29.4044698473222,16.6248055079682));
#50073=CARTESIAN_POINT('Ctrl Pts',(53.0380141080535,29.3625857410172,16.627311679928));
#50074=CARTESIAN_POINT('Ctrl Pts',(53.0306892831047,29.3204270586987,16.6298366943859));
#50075=CARTESIAN_POINT('Ctrl Pts',(53.016097694892,29.216771308831,16.6360937083062));
#50076=CARTESIAN_POINT('Ctrl Pts',(53.0103280254816,29.155120766903,16.6398574975813));
#50077=CARTESIAN_POINT('Ctrl Pts',(53.0067418712798,29.0785377137215,16.644631910438));
#50078=CARTESIAN_POINT('Ctrl Pts',(53.0062145424458,29.0637626142266,16.6455574981895));
#50079=CARTESIAN_POINT('Ctrl Pts',(53.0056378785134,29.0402861853452,16.6470358351619));
#50080=CARTESIAN_POINT('Ctrl Pts',(53.0054811477803,29.0315878557825,16.6475852455396));
#50081=CARTESIAN_POINT('Ctrl Pts',(53.0052930147921,29.0151932821328,16.6486240301248));
#50082=CARTESIAN_POINT('Ctrl Pts',(53.0052492435961,29.0074973183083,16.6491130106753));
#50083=CARTESIAN_POINT('Ctrl Pts',(53.0052509714746,28.9901440891952,16.6502187237599));
#50084=CARTESIAN_POINT('Ctrl Pts',(53.0053220645592,28.9804870745547,16.6508362399704));
#50085=CARTESIAN_POINT('Ctrl Pts',(53.0057460131162,28.9514979524699,16.6526967159222));
#50086=CARTESIAN_POINT('Ctrl Pts',(53.0063098203821,28.9321705291095,16.653946173717));
#50087=CARTESIAN_POINT('Ctrl Pts',(53.0082417662792,28.8879905375205,16.6568238571183));
#50088=CARTESIAN_POINT('Ctrl Pts',(53.0097942630168,28.8631496622685,16.6584575425616));
#50089=CARTESIAN_POINT('Ctrl Pts',(53.0166096057066,28.7793278987833,16.6640243318593));
#50090=CARTESIAN_POINT('Ctrl Pts',(53.0240331458528,28.7205585069491,16.6680193413029));
#50091=CARTESIAN_POINT('Ctrl Pts',(53.0573871997508,28.5264372437851,16.6814992160782));
#50092=CARTESIAN_POINT('Ctrl Pts',(53.0947158109967,28.3934567608155,16.6912276925873));
#50093=CARTESIAN_POINT('Ctrl Pts',(53.1496828980849,28.2546902706706,16.7014785847141));
#50094=CARTESIAN_POINT('Ctrl Pts',(53.1540131117373,28.2440288454328,16.7022665855961));
#50095=CARTESIAN_POINT('Ctrl Pts',(53.1765098094134,28.189985784901,16.7062613026342));
#50096=CARTESIAN_POINT('Ctrl Pts',(53.1961158324718,28.1472150338447,16.7094241255423));
#50097=CARTESIAN_POINT('Ctrl Pts',(53.2210916112852,28.0974552110499,16.7130731610436));
#50098=CARTESIAN_POINT('Ctrl Pts',(53.225016031919,28.0897615307207,16.7136364654033));
#50099=CARTESIAN_POINT('Ctrl Pts',(53.2314941476769,28.0772626495191,16.7145498319228));
#50100=CARTESIAN_POINT('Ctrl Pts',(53.2340177048106,28.072442075964,16.7149016699997));
#50101=CARTESIAN_POINT('Ctrl Pts',(53.2385729259767,28.0638265366592,16.7155296381796));
#50102=CARTESIAN_POINT('Ctrl Pts',(53.2405971714556,28.0600277777576,16.7158062178911));
#50103=CARTESIAN_POINT('Ctrl Pts',(53.2450427364248,28.051749774431,16.7164082513786));
#50104=CARTESIAN_POINT('Ctrl Pts',(53.2474689113033,28.0472732438913,16.7167333953908));
#50105=CARTESIAN_POINT('Ctrl Pts',(53.2544136559397,28.0345758047717,16.7176545933729));
#50106=CARTESIAN_POINT('Ctrl Pts',(53.2589731841233,28.0263772825995,16.7182481322152));
#50107=CARTESIAN_POINT('Ctrl Pts',(53.2894205873233,27.9725274605633,16.7221403205046));
#50108=CARTESIAN_POINT('Ctrl Pts',(53.3170460216686,27.9278765433461,16.7253377004572));
#50109=CARTESIAN_POINT('Ctrl Pts',(53.4404256656817,27.7450032083083,16.7385291408264));
#50110=CARTESIAN_POINT('Ctrl Pts',(53.5516896782469,27.6180835154592,16.7479816178534));
#50111=CARTESIAN_POINT('Ctrl Pts',(53.7272075343015,27.4626567812544,16.7619475594429));
#50112=CARTESIAN_POINT('Ctrl Pts',(53.779009037906,27.4212015512862,16.7659680280247));
#50113=CARTESIAN_POINT('Ctrl Pts',(53.8453794138403,27.3733099664234,16.7710585396867));
#50114=CARTESIAN_POINT('Ctrl Pts',(53.8580896429777,27.3643625467501,16.7720306862463));
#50115=CARTESIAN_POINT('Ctrl Pts',(53.8782873935378,27.3504944284185,16.7735719465051));
#50116=CARTESIAN_POINT('Ctrl Pts',(53.8857058947758,27.3454739515399,16.7741372932323));
#50117=CARTESIAN_POINT('Ctrl Pts',(53.8994798388177,27.3362870787299,16.7751857245628));
#50118=CARTESIAN_POINT('Ctrl Pts',(53.9058257852833,27.3321066896175,16.7756682747216));
#50119=CARTESIAN_POINT('Ctrl Pts',(53.9199717302421,27.3229035311781,16.7767429534923));
#50120=CARTESIAN_POINT('Ctrl Pts',(53.9277831567242,27.3178987350833,16.777335733035));
#50121=CARTESIAN_POINT('Ctrl Pts',(53.9504072728413,27.3036250431982,16.7790508641112));
#50122=CARTESIAN_POINT('Ctrl Pts',(53.9653069096655,27.2944962434085,16.780178295169));
#50123=CARTESIAN_POINT('Ctrl Pts',(54.1055675975932,27.2110749415363,16.7907748335484));
#50124=CARTESIAN_POINT('Ctrl Pts',(54.2385716978849,27.1505477905933,16.8007485881494));
#50125=CARTESIAN_POINT('Ctrl Pts',(54.3842491664793,27.1026498761366,16.8114250724037));
#50126=CARTESIAN_POINT('Ctrl Pts',(54.3915609796176,27.1002925121066,16.811960178837));
#50127=CARTESIAN_POINT('Ctrl Pts',(54.5136213425887,27.0617166462131,16.8208791403012));
#50128=CARTESIAN_POINT('Ctrl Pts',(54.631412340556,27.0359086378257,16.8292996491075));
#50129=CARTESIAN_POINT('Ctrl Pts',(54.7665220858822,27.0188977578712,16.8383183593856));
#50130=CARTESIAN_POINT('Ctrl Pts',(54.7822478558811,27.0171076501075,16.8393581526558));
#50131=CARTESIAN_POINT('Ctrl Pts',(54.8044281941343,27.01484986433,16.8408092347665));
#50132=CARTESIAN_POINT('Ctrl Pts',(54.8108658040319,27.0142261832951,16.8412285619085));
#50133=CARTESIAN_POINT('Ctrl Pts',(54.8216999854387,27.013229722933,16.8419310570466));
#50134=CARTESIAN_POINT('Ctrl Pts',(54.8260949280315,27.0128402036477,16.8422151395493));
#50135=CARTESIAN_POINT('Ctrl Pts',(54.835068249673,27.0120749053375,16.8427933006729));
#50136=CARTESIAN_POINT('Ctrl Pts',(54.8396466892665,27.0117003543164,16.8430873102334));
#50137=CARTESIAN_POINT('Ctrl Pts',(54.8513205337262,27.0107859306266,16.8438345433273));
#50138=CARTESIAN_POINT('Ctrl Pts',(54.8584176801825,27.0102681970044,16.8442865524473));
#50139=CARTESIAN_POINT('Ctrl Pts',(54.8873077878004,27.0083160368007,16.8461178346457));
#50140=CARTESIAN_POINT('Ctrl Pts',(54.9091217760328,27.0072015192836,16.8474804575923));
#50141=CARTESIAN_POINT('Ctrl Pts',(54.9667850861947,27.0052042773022,16.8510396497858));
#50142=CARTESIAN_POINT('Ctrl Pts',(55.0026485633602,27.0049294518526,16.853209704663));
#50143=CARTESIAN_POINT('Ctrl Pts',(55.2159691986194,27.0090476576258,16.8659591569947));
#50144=CARTESIAN_POINT('Ctrl Pts',(55.3921880979826,27.036144128805,16.8759121178361));
#50145=CARTESIAN_POINT('Ctrl Pts',(55.6173965315011,27.1023376317224,16.8899769536234));
#50146=CARTESIAN_POINT('Ctrl Pts',(55.6715641306788,27.1208242106551,16.8934616717058));
#50147=CARTESIAN_POINT('Ctrl Pts',(55.7387211851653,27.1470186274005,16.8979490914754));
#50148=CARTESIAN_POINT('Ctrl Pts',(55.7525221132542,27.1525803381787,16.8988803109771));
#50149=CARTESIAN_POINT('Ctrl Pts',(55.7743893686359,27.1616784260374,16.9003708475851));
#50150=CARTESIAN_POINT('Ctrl Pts',(55.7824968994221,27.1651147987,16.9009268044888));
#50151=CARTESIAN_POINT('Ctrl Pts',(55.7976354968249,27.171649866317,16.9019712644512));
#50152=CARTESIAN_POINT('Ctrl Pts',(55.8046719505285,27.1747357324274,16.902459325961));
#50153=CARTESIAN_POINT('Ctrl Pts',(55.8203708224177,27.1817289587022,16.9035541313588));
#50154=CARTESIAN_POINT('Ctrl Pts',(55.8290234549913,27.1856577026814,16.9041615945916));
#50155=CARTESIAN_POINT('Ctrl Pts',(55.8544989369083,27.197445176146,16.905962293666));
#50156=CARTESIAN_POINT('Ctrl Pts',(55.871240131674,27.20547696568,16.9071614234284));
#50157=CARTESIAN_POINT('Ctrl Pts',(56.0025668246039,27.2707533622711,16.9166963644473));
#50158=CARTESIAN_POINT('Ctrl Pts',(56.1114885289116,27.3386702315731,16.9254125530072));
#50159=CARTESIAN_POINT('Ctrl Pts',(56.3290853987426,27.5053776099329,16.9444453797473));
#50160=CARTESIAN_POINT('Ctrl Pts',(56.434935636503,27.6066840579594,16.9547608188785));
#50161=CARTESIAN_POINT('Ctrl Pts',(56.5379106090545,27.729543130681,16.9653535960946));
#50162=CARTESIAN_POINT('Ctrl Pts',(56.5469269254191,27.7405370934029,16.9662861729264));
#50163=CARTESIAN_POINT('Ctrl Pts',(56.5593236484277,27.7559869089346,16.9675744729361));
#50164=CARTESIAN_POINT('Ctrl Pts',(56.5628037806768,27.7603616833135,16.9679368207702));
#50165=CARTESIAN_POINT('Ctrl Pts',(56.568774647179,27.7679325965983,16.9685596016942));
#50166=CARTESIAN_POINT('Ctrl Pts',(56.5712740958414,27.7711217730762,16.9688206393008));
#50167=CARTESIAN_POINT('Ctrl Pts',(56.5765027963279,27.7778353771084,16.9693673855857));
#50168=CARTESIAN_POINT('Ctrl Pts',(56.5792299773671,27.7813613696304,16.9696529414121));
#50169=CARTESIAN_POINT('Ctrl Pts',(56.5858884975803,27.7900301085702,16.9703511633553));
#50170=CARTESIAN_POINT('Ctrl Pts',(56.5898067105022,27.7951829637067,16.9707629196622));
#50171=CARTESIAN_POINT('Ctrl Pts',(56.6039573566964,27.8139817586543,16.9722535952883));
#50172=CARTESIAN_POINT('Ctrl Pts',(56.6140400860481,27.8277401665352,16.973322693676));
#50173=CARTESIAN_POINT('Ctrl Pts',(56.6387976632642,27.8624482846744,16.9759701419054));
#50174=CARTESIAN_POINT('Ctrl Pts',(56.6532487273545,27.8835545442302,16.9775359238579));
#50175=CARTESIAN_POINT('Ctrl Pts',(56.7140531491889,27.9761321829212,16.9842421093809));
#50176=CARTESIAN_POINT('Ctrl Pts',(56.7562109410883,28.0502585149894,16.9892053458231));
#50177=CARTESIAN_POINT('Ctrl Pts',(56.8596637001564,28.2627587233095,17.0029379060831));
#50178=CARTESIAN_POINT('Ctrl Pts',(56.9101571472269,28.4057211532166,17.011671141));
#50179=CARTESIAN_POINT('Ctrl Pts',(56.9493510762836,28.5761800975825,17.0224449343882));
#50180=CARTESIAN_POINT('Ctrl Pts',(56.9542642902374,28.5994454620733,17.0239216831063));
#50181=CARTESIAN_POINT('Ctrl Pts',(56.960594471874,28.6323167694341,17.026019305295));
#50182=CARTESIAN_POINT('Ctrl Pts',(56.9623591145657,28.6418543014683,17.0266292333191));
#50183=CARTESIAN_POINT('Ctrl Pts',(56.9653124779692,28.6584941042941,17.0276957920694));
#50184=CARTESIAN_POINT('Ctrl Pts',(56.9665324386422,28.6655907022316,17.0281514316468));
#50185=CARTESIAN_POINT('Ctrl Pts',(56.9690059772508,28.6804612257381,17.0291078807471));
#50186=CARTESIAN_POINT('Ctrl Pts',(56.9702519985466,28.6882362656963,17.0296089192385));
#50187=CARTESIAN_POINT('Ctrl Pts',(56.9731104881044,28.7067748041533,17.03080595699));
#50188=CARTESIAN_POINT('Ctrl Pts',(56.9746809510815,28.7175444327702,17.0315032611491));
#50189=CARTESIAN_POINT('Ctrl Pts',(56.9797157501852,28.7541677090476,17.0338812872322));
#50190=CARTESIAN_POINT('Ctrl Pts',(56.9827609556198,28.7800753459827,17.0355750013085));
#50191=CARTESIAN_POINT('Ctrl Pts',(56.9888517118132,28.8424160542129,17.0396798796929));
#50192=CARTESIAN_POINT('Ctrl Pts',(56.991405309247,28.8788866331893,17.0421053732857));
#50193=CARTESIAN_POINT('Ctrl Pts',(57.0019582336632,29.1275005846225,17.0588033690762));
#50194=CARTESIAN_POINT('Ctrl Pts',(56.9770490507329,29.3396262579937,17.0740579853184));
#50195=CARTESIAN_POINT('Ctrl Pts',(56.9123455908051,29.5679720353296,17.0899547757384));
#50196=CARTESIAN_POINT('Ctrl Pts',(56.9050451818364,29.5919973700519,17.09161794996));
#50197=CARTESIAN_POINT('Ctrl Pts',(56.8948921114606,29.6232751424958,17.0937651781727));
#50198=CARTESIAN_POINT('Ctrl Pts',(56.8924482274647,29.6306565852133,17.094270588738));
#50199=CARTESIAN_POINT('Ctrl Pts',(56.8884452571021,29.6425142305224,17.0950801340207));
#50200=CARTESIAN_POINT('Ctrl Pts',(56.8869132979433,29.6469994070125,17.0953858018368));
#50201=CARTESIAN_POINT('Ctrl Pts',(56.8839341483183,29.6556209961786,17.0959722624333));
#50202=CARTESIAN_POINT('Ctrl Pts',(56.8824893043134,29.6597581263541,17.0962531807272));
#50203=CARTESIAN_POINT('Ctrl Pts',(56.8790117196527,29.6696113234977,17.0969211022267));
#50204=CARTESIAN_POINT('Ctrl Pts',(56.8769664933563,29.6753229984733,17.0973073767489));
#50205=CARTESIAN_POINT('Ctrl Pts',(56.8699485518084,29.694643725852,17.0986112321948));
#50206=CARTESIAN_POINT('Ctrl Pts',(56.8648534961166,29.7082082736441,17.0995219376815));
#50207=CARTESIAN_POINT('Ctrl Pts',(56.8346262951967,29.7860931888906,17.1047304345441));
#50208=CARTESIAN_POINT('Ctrl Pts',(56.8063128411885,29.8491360751404,17.1088656295736));
#50209=CARTESIAN_POINT('Ctrl Pts',(56.7364732628164,29.9852568689812,17.1178768485602));
#50210=CARTESIAN_POINT('Ctrl Pts',(56.6934886235885,30.0574344048988,17.1227136889816));
#50211=CARTESIAN_POINT('Ctrl Pts',(56.5767644940927,30.2279671591395,17.1347455847663));
#50212=CARTESIAN_POINT('Ctrl Pts',(56.4982561847613,30.3226156610323,17.1419845196874));
#50213=CARTESIAN_POINT('Ctrl Pts',(56.4003615471259,30.420656935306,17.1505816892507));
#50214=CARTESIAN_POINT('Ctrl Pts',(56.3890337108705,30.4317345836828,17.1515703891042));
#50215=CARTESIAN_POINT('Ctrl Pts',(56.3704299436187,30.4494988590162,17.1531850703969));
#50216=CARTESIAN_POINT('Ctrl Pts',(56.3632340364831,30.4562685634234,17.1538074781997));
#50217=CARTESIAN_POINT('Ctrl Pts',(56.3503265620258,30.4682320424015,17.1549202767601));
#50218=CARTESIAN_POINT('Ctrl Pts',(56.344634537416,30.4734466778667,17.1554097704689));
#50219=CARTESIAN_POINT('Ctrl Pts',(56.3325620530644,30.4843784326484,17.1564454527626));
#50220=CARTESIAN_POINT('Ctrl Pts',(56.3261747582456,30.4900877368197,17.1569919538823));
#50221=CARTESIAN_POINT('Ctrl Pts',(56.3091178883716,30.5051375349052,17.1584476342307));
#50222=CARTESIAN_POINT('Ctrl Pts',(56.298385306972,30.5144055672629,17.1593597719696));
#50223=CARTESIAN_POINT('Ctrl Pts',(56.2462767921634,30.558442337052,17.1637710365687));
#50224=CARTESIAN_POINT('Ctrl Pts',(56.2036015295455,30.5916314897093,17.1673328003718));
#50225=CARTESIAN_POINT('Ctrl Pts',(56.0743789040041,30.6839586024112,17.177980366284));
#50226=CARTESIAN_POINT('Ctrl Pts',(55.9844651183941,30.7380536603584,17.1852276320582));
#50227=CARTESIAN_POINT('Ctrl Pts',(55.7827564792034,30.8387174118643,17.2009338169644));
#50228=CARTESIAN_POINT('Ctrl Pts',(55.6701064714993,30.8826980467667,17.2093796052857));
#50229=CARTESIAN_POINT('Ctrl Pts',(55.5389408728829,30.9206304706546,17.2184226765959));
#50230=CARTESIAN_POINT('Ctrl Pts',(55.523665809749,30.9248513777666,17.2194638168261));
#50231=CARTESIAN_POINT('Ctrl Pts',(55.5020841950951,30.9305390171978,17.220916444607));
#50232=CARTESIAN_POINT('Ctrl Pts',(55.4958187876428,30.9321576458734,17.2213359928051));
#50233=CARTESIAN_POINT('Ctrl Pts',(55.4852677142603,30.9348287470336,17.2220387514561));
#50234=CARTESIAN_POINT('Ctrl Pts',(55.4809862693466,30.9358975295233,17.2223228779195));
#50235=CARTESIAN_POINT('Ctrl Pts',(55.4722415763028,30.9380496767025,17.2229010247945));
#50236=CARTESIAN_POINT('Ctrl Pts',(55.4677780796463,30.9391318482742,17.2231949767329));
#50237=CARTESIAN_POINT('Ctrl Pts',(55.4563937166237,30.941850383721,17.2239418854143));
#50238=CARTESIAN_POINT('Ctrl Pts',(55.4494676940967,30.9434651869639,17.2243936298259));
#50239=CARTESIAN_POINT('Ctrl Pts',(55.4212714050009,30.9498803615555,17.2262224577608));
#50240=CARTESIAN_POINT('Ctrl Pts',(55.3999308277264,30.954369065977,17.2275829472569));
#50241=CARTESIAN_POINT('Ctrl Pts',(55.3433942240956,30.9652958736434,17.2311352048808));
#50242=CARTESIAN_POINT('Ctrl Pts',(55.3080901475351,30.9711388141247,17.2333005866451));
#50243=CARTESIAN_POINT('Ctrl Pts',(55.0980752267453,31.0001159847246,17.245970158376));
#50244=CARTESIAN_POINT('Ctrl Pts',(54.9210794676328,31.0009651764872,17.2558551631142));
#50245=CARTESIAN_POINT('Ctrl Pts',(54.6883084873651,30.9711139540399,17.2699051524524));
#50246=CARTESIAN_POINT('Ctrl Pts',(54.6307107926752,30.9611390398661,17.2734618740002));
#50247=CARTESIAN_POINT('Ctrl Pts',(54.5590096546041,30.9454509240181,17.2780304184129));
#50248=CARTESIAN_POINT('Ctrl Pts',(54.5444185502863,30.9420858132495,17.2789674725467));
#50249=CARTESIAN_POINT('Ctrl Pts',(54.5212882255149,30.9364763163197,17.2804652431872));
#50250=CARTESIAN_POINT('Ctrl Pts',(54.5127234497355,30.9343389171067,17.2810225427306));
#50251=CARTESIAN_POINT('Ctrl Pts',(54.4967329731218,30.9302354430042,17.2820682033866));
#50252=CARTESIAN_POINT('Ctrl Pts',(54.4893038707121,30.9282831811266,17.2825561132701));
#50253=CARTESIAN_POINT('Ctrl Pts',(54.4727381446291,30.923827497939,17.2836488589577));
#50254=CARTESIAN_POINT('Ctrl Pts',(54.4636077529387,30.9213018133975,17.2842544018042));
#50255=CARTESIAN_POINT('Ctrl Pts',(54.4367751356201,30.9136730964898,17.2860437961668));
#50256=CARTESIAN_POINT('Ctrl Pts',(54.4191256025028,30.9083898618668,17.2872334306284));
#50257=CARTESIAN_POINT('Ctrl Pts',(54.3792166735737,30.8958385601036,17.2899529923729));
#50258=CARTESIAN_POINT('Ctrl Pts',(54.3570073171438,30.8884215944177,17.2914875716143));
#50259=CARTESIAN_POINT('Ctrl Pts',(54.2838986651823,30.8625672691579,17.2966105974432));
#50260=CARTESIAN_POINT('Ctrl Pts',(54.2336227992142,30.8424502972793,17.300250544259));
#50261=CARTESIAN_POINT('Ctrl Pts',(54.0305841217449,30.7514590585834,17.3154208767061));
#50262=CARTESIAN_POINT('Ctrl Pts',(53.8862893248748,30.6634355972053,17.3273994342522));
#50263=CARTESIAN_POINT('Ctrl Pts',(53.7257187867043,30.535127955614,17.3413232523151));
#50264=CARTESIAN_POINT('Ctrl Pts',(53.6973199133797,30.5111040529081,17.3438084178473));
#50265=CARTESIAN_POINT('Ctrl Pts',(53.6630297473393,30.4804107658478,17.3468207886061));
#50266=CARTESIAN_POINT('Ctrl Pts',(53.6564911355618,30.4744793759891,17.3473957404883));
#50267=CARTESIAN_POINT('Ctrl Pts',(53.6462928511885,30.4651040118555,17.3482930432789));
#50268=CARTESIAN_POINT('Ctrl Pts',(53.6426065425826,30.4616893696684,17.3486174996186));
#50269=CARTESIAN_POINT('Ctrl Pts',(53.6357814944816,30.4553192149326,17.349218363294));
#50270=CARTESIAN_POINT('Ctrl Pts',(53.6326394562746,30.4523674783387,17.3494950324541));
#50271=CARTESIAN_POINT('Ctrl Pts',(53.6264534166954,30.4465182356605,17.3500398643856));
#50272=CARTESIAN_POINT('Ctrl Pts',(53.6234090136276,30.443621307553,17.3503080637695));
#50273=CARTESIAN_POINT('Ctrl Pts',(53.6142464033956,30.4348472059722,17.3511155340885));
#50274=CARTESIAN_POINT('Ctrl Pts',(53.6081564176096,30.4289405107245,17.3516526061822));
#50275=CARTESIAN_POINT('Ctrl Pts',(53.5718989645209,30.3933225769464,17.3548538075152));
#50276=CARTESIAN_POINT('Ctrl Pts',(53.5426436525828,30.3626934488702,17.3574522319262));
#50277=CARTESIAN_POINT('Ctrl Pts',(53.4497529135049,30.259023961256,17.3658480041075));
#50278=CARTESIAN_POINT('Ctrl Pts',(53.390456506765,30.1822774291885,17.3714513667412));
#50279=CARTESIAN_POINT('Ctrl Pts',(53.2628713442118,29.9896545022768,17.3848682233645));
#50280=CARTESIAN_POINT('Ctrl Pts',(53.2002604625237,29.8706112451632,17.3926855861683));
#50281=CARTESIAN_POINT('Ctrl Pts',(53.1460897707639,29.7363137123425,17.401600684779));
#50282=CARTESIAN_POINT('Ctrl Pts',(53.1421844534187,29.7264037509495,17.4022588758078));
#50283=CARTESIAN_POINT('Ctrl Pts',(53.1325798627255,29.7014474042068,17.4039176519475));
#50284=CARTESIAN_POINT('Ctrl Pts',(53.1269829963,29.6863626667633,17.4049214253623));
#50285=CARTESIAN_POINT('Ctrl Pts',(53.1182202001915,29.6618394167378,17.4065558724073));
#50286=CARTESIAN_POINT('Ctrl Pts',(53.1149413045205,29.6524418268117,17.407182824668));
#50287=CARTESIAN_POINT('Ctrl Pts',(53.1092416056515,29.6357043226245,17.4083007139324));
#50288=CARTESIAN_POINT('Ctrl Pts',(53.106792854804,29.6283740878282,17.4087907231174));
#50289=CARTESIAN_POINT('Ctrl Pts',(53.1017318540653,29.6129260393603,17.4098243698434));
#50290=CARTESIAN_POINT('Ctrl Pts',(53.099128945284,29.6048053515303,17.4103683010345));
#50291=CARTESIAN_POINT('Ctrl Pts',(53.0923901178946,29.5833079294571,17.4118098377418));
#50292=CARTESIAN_POINT('Ctrl Pts',(53.0883428903512,29.5699040985341,17.4127103004647));
#50293=CARTESIAN_POINT('Ctrl Pts',(53.0798065221263,29.5405183789881,17.4146883867922));
#50294=CARTESIAN_POINT('Ctrl Pts',(53.0753751359511,29.5245209393451,17.415767794003));
#50295=CARTESIAN_POINT('Ctrl Pts',(53.0620579705738,29.4740029708086,17.419185008074));
#50296=CARTESIAN_POINT('Ctrl Pts',(53.0539040381943,29.439323265497,17.4215435341112));
#50297=CARTESIAN_POINT('Ctrl Pts',(53.0466869493682,29.4044696388254,17.4239266846335));
#50298=CARTESIAN_POINT('Origin',(55.,29.,3.45145488139523));
#50299=CARTESIAN_POINT('',(53.0466869980087,29.4044698737256,18.3839095910714));
#50300=CARTESIAN_POINT('',(53.0466869962288,29.4044698651299,18.2270410618393));
#50301=CARTESIAN_POINT('',(53.0466869980082,29.4044698737233,3.45145488139523));
#50302=CARTESIAN_POINT('Ctrl Pts',(53.0466869980087,29.4044698737256,18.3839095910714));
#50303=CARTESIAN_POINT('Ctrl Pts',(53.0663282740129,29.4993238104147,18.3771815173166));
#50304=CARTESIAN_POINT('Ctrl Pts',(53.0928528261563,29.5926220832049,18.3703852673977));
#50305=CARTESIAN_POINT('Ctrl Pts',(53.1449829312298,29.7355207600424,18.3599570166841));
#50306=CARTESIAN_POINT('Ctrl Pts',(53.1660641757064,29.7866128105735,18.356226466279));
#50307=CARTESIAN_POINT('Ctrl Pts',(53.1932258003383,29.8453903051281,18.3519834221063));
#50308=CARTESIAN_POINT('Ctrl Pts',(53.1972717429001,29.853983967166,18.3513643263843));
#50309=CARTESIAN_POINT('Ctrl Pts',(53.203591523263,29.8671622270098,18.350417273382));
#50310=CARTESIAN_POINT('Ctrl Pts',(53.2058218110092,29.8717673834286,18.3500867641168));
#50311=CARTESIAN_POINT('Ctrl Pts',(53.2099601354037,29.8802291511687,18.3494803481231));
#50312=CARTESIAN_POINT('Ctrl Pts',(53.2118629226712,29.884088156661,18.3492041369051));
#50313=CARTESIAN_POINT('Ctrl Pts',(53.216186318876,29.8927852925755,18.3485823939949));
#50314=CARTESIAN_POINT('Ctrl Pts',(53.218614127881,29.8976197434721,18.3482373127953));
#50315=CARTESIAN_POINT('Ctrl Pts',(53.2258420108211,29.9118676677859,18.3472216798123));
#50316=CARTESIAN_POINT('Ctrl Pts',(53.2306973362416,29.9212531191818,18.3465544418942));
#50317=CARTESIAN_POINT('Ctrl Pts',(53.2739837314391,30.0033220625778,18.3407317648595));
#50318=CARTESIAN_POINT('Ctrl Pts',(53.3168048136082,30.0736129052864,18.3358252444211));
#50319=CARTESIAN_POINT('Ctrl Pts',(53.4522314216923,30.2677982394056,18.3219299186714));
#50320=CARTESIAN_POINT('Ctrl Pts',(53.5550348327484,30.3838263831878,18.3131513860552));
#50321=CARTESIAN_POINT('Ctrl Pts',(53.7084272785613,30.5210186831608,18.3007611623597));
#50322=CARTESIAN_POINT('Ctrl Pts',(53.7479567672762,30.553719728598,18.2976253393918));
#50323=CARTESIAN_POINT('Ctrl Pts',(53.7968390382002,30.591080200683,18.2937894523554));
#50324=CARTESIAN_POINT('Ctrl Pts',(53.8050258461031,30.5972380130678,18.2931483975018));
#50325=CARTESIAN_POINT('Ctrl Pts',(53.8205970758861,30.608763388188,18.2919314856081));
#50326=CARTESIAN_POINT('Ctrl Pts',(53.8279716426294,30.6141438664713,18.2913561426259));
#50327=CARTESIAN_POINT('Ctrl Pts',(53.8355043801587,30.6195609084879,18.2907693836756));
#50328=CARTESIAN_POINT('Ctrl Pts',(53.8356259854771,30.6196483381388,18.2907599115318));
#50329=CARTESIAN_POINT('Ctrl Pts',(53.8358714539326,30.6198247787943,18.2907407918683));
#50330=CARTESIAN_POINT('Ctrl Pts',(53.8359953173427,30.6199137892236,18.2907311443365));
#50331=CARTESIAN_POINT('Ctrl Pts',(53.8362455233502,30.6200935481556,18.2907116566818));
#50332=CARTESIAN_POINT('Ctrl Pts',(53.836371866466,30.6201842961669,18.2907018165287));
#50333=CARTESIAN_POINT('Ctrl Pts',(53.8366272725509,30.6203677004834,18.2906819249176));
#50334=CARTESIAN_POINT('Ctrl Pts',(53.8367563359285,30.6204603561149,18.2906718734391));
#50335=CARTESIAN_POINT('Ctrl Pts',(53.8370174443922,30.620647760701,18.2906515388179));
#50336=CARTESIAN_POINT('Ctrl Pts',(53.8371494899267,30.6207425088938,18.2906412556528));
#50337=CARTESIAN_POINT('Ctrl Pts',(53.842977443031,30.624923230096,18.2901874111216));
#50338=CARTESIAN_POINT('Ctrl Pts',(53.8486947778472,30.6289791233919,18.2897427105465));
#50339=CARTESIAN_POINT('Ctrl Pts',(53.8615194070074,30.6379757095229,18.2887463094328));
#50340=CARTESIAN_POINT('Ctrl Pts',(53.8686376875887,30.6429004229695,18.2881940154142));
#50341=CARTESIAN_POINT('Ctrl Pts',(53.8873387805978,30.6556594179283,18.2867448721204));
#50342=CARTESIAN_POINT('Ctrl Pts',(53.8989721552239,30.6634183977424,18.2858452293157));
#50343=CARTESIAN_POINT('Ctrl Pts',(53.9515517668399,30.6976935934691,18.2817864778678));
#50344=CARTESIAN_POINT('Ctrl Pts',(53.9933778498125,30.7228228005966,18.2785771149641));
#50345=CARTESIAN_POINT('Ctrl Pts',(54.1823294197327,30.8271144889793,18.2641524755469));
#50346=CARTESIAN_POINT('Ctrl Pts',(54.3381275678869,30.8891378566349,18.2523757746302));
#50347=CARTESIAN_POINT('Ctrl Pts',(54.5477227223439,30.9434310501543,18.2374091253044));
#50348=CARTESIAN_POINT('Ctrl Pts',(54.5961015743428,30.9540587759604,18.2340182522851));
#50349=CARTESIAN_POINT('Ctrl Pts',(54.6627994641184,30.966127381721,18.2294700722904));
#50350=CARTESIAN_POINT('Ctrl Pts',(54.6808146832369,30.9691322624609,18.2282541488075));
#50351=CARTESIAN_POINT('Ctrl Pts',(54.7119196652734,30.9738823589965,18.2261791212927));
#50352=CARTESIAN_POINT('Ctrl Pts',(54.7249899163165,30.9757457636343,18.2253145780033));
#50353=CARTESIAN_POINT('Ctrl Pts',(54.7438707322264,30.9782465730511,18.2240772391273));
#50354=CARTESIAN_POINT('Ctrl Pts',(54.7496667828406,30.9789883749192,18.2236989659522));
#50355=CARTESIAN_POINT('Ctrl Pts',(54.7597805253145,30.980237628361,18.223041731113));
#50356=CARTESIAN_POINT('Ctrl Pts',(54.7640967337669,30.9807564492455,18.2227621448487));
#50357=CARTESIAN_POINT('Ctrl Pts',(54.7732215723239,30.9818230316452,18.2221730061112));
#50358=CARTESIAN_POINT('Ctrl Pts',(54.7780305150069,30.982367406146,18.2218636424506));
#50359=CARTESIAN_POINT('Ctrl Pts',(54.7910184728013,30.983789794659,18.2210310289626));
#50360=CARTESIAN_POINT('Ctrl Pts',(54.799201122105,30.9846347382581,18.2205095839159));
#50361=CARTESIAN_POINT('Ctrl Pts',(54.8364755475044,30.9882508165458,18.2181474714516));
#50362=CARTESIAN_POINT('Ctrl Pts',(54.8656224576978,30.9904332295135,18.2163370387361));
#50363=CARTESIAN_POINT('Ctrl Pts',(55.1021246800094,31.0029223530592,18.2018675931434));
#50364=CARTESIAN_POINT('Ctrl Pts',(55.3098961404352,30.9814424099518,18.1904007120756));
#50365=CARTESIAN_POINT('Ctrl Pts',(55.5638283585736,30.9141977573769,18.1746268899483));
#50366=CARTESIAN_POINT('Ctrl Pts',(55.6164115195397,30.897917671219,18.1712689328064));
#50367=CARTESIAN_POINT('Ctrl Pts',(55.6816887888239,30.8747083375326,18.1669514150592));
#50368=CARTESIAN_POINT('Ctrl Pts',(55.6950743901197,30.8697867608963,18.1660580763259));
#50369=CARTESIAN_POINT('Ctrl Pts',(55.7164311082431,30.8616733683527,18.1646193850239));
#50370=CARTESIAN_POINT('Ctrl Pts',(55.7244365482176,30.8585728253661,18.1640770643958));
#50371=CARTESIAN_POINT('Ctrl Pts',(55.7395985550381,30.852587669857,18.1630440380833));
#50372=CARTESIAN_POINT('Ctrl Pts',(55.7467589034668,30.8497130140884,18.1625536725862));
#50373=CARTESIAN_POINT('Ctrl Pts',(55.7630195683498,30.843075060168,18.1614342662883));
#50374=CARTESIAN_POINT('Ctrl Pts',(55.7721090007092,30.8392857919333,18.1608043624977));
#50375=CARTESIAN_POINT('Ctrl Pts',(55.7956498067761,30.8292666824433,18.1591619121793));
#50376=CARTESIAN_POINT('Ctrl Pts',(55.8100559535118,30.8229329497533,18.1581458834684));
#50377=CARTESIAN_POINT('Ctrl Pts',(55.9440632616849,30.7621138246413,18.1485901995602));
#50378=CARTESIAN_POINT('Ctrl Pts',(56.0580579763213,30.6961138418899,18.139645289434));
#50379=CARTESIAN_POINT('Ctrl Pts',(56.2425369075894,30.5634314574486,18.123862179558));
#50380=CARTESIAN_POINT('Ctrl Pts',(56.3162207716959,30.5019252089318,18.1171375627799));
#50381=CARTESIAN_POINT('Ctrl Pts',(56.4256787563422,30.3962924303059,18.1067029141482));
#50382=CARTESIAN_POINT('Ctrl Pts',(56.4644933032787,30.355526870813,18.1029014780861));
#50383=CARTESIAN_POINT('Ctrl Pts',(56.5078154723697,30.3059904508371,18.0985887702237));
#50384=CARTESIAN_POINT('Ctrl Pts',(56.51404373589,30.2987648481809,18.0979669675616));
#50385=CARTESIAN_POINT('Ctrl Pts',(56.5235385212463,30.2875885239057,18.0970166604509));
#50386=CARTESIAN_POINT('Ctrl Pts',(56.5268419478216,30.2836695448633,18.0966855771727));
#50387=CARTESIAN_POINT('Ctrl Pts',(56.5328903130045,30.27643776151,18.0960786185718));
#50388=CARTESIAN_POINT('Ctrl Pts',(56.5356396308803,30.273128821231,18.0958024347583));
#50389=CARTESIAN_POINT('Ctrl Pts',(56.5418152450407,30.2656470530566,18.095181390067));
#50390=CARTESIAN_POINT('Ctrl Pts',(56.5452353123318,30.2614692005419,18.094836975083));
#50391=CARTESIAN_POINT('Ctrl Pts',(56.5552671223081,30.2491126229863,18.0938251358267));
#50392=CARTESIAN_POINT('Ctrl Pts',(56.5618313171359,30.2408952875882,18.0931609886581));
#50393=CARTESIAN_POINT('Ctrl Pts',(56.6168362436764,30.1709098397934,18.0875744094962));
#50394=CARTESIAN_POINT('Ctrl Pts',(56.6616630319082,30.106376186782,18.0828786364954));
#50395=CARTESIAN_POINT('Ctrl Pts',(56.7691977368114,29.930223931931,18.0707445326249));
#50396=CARTESIAN_POINT('Ctrl Pts',(56.8251736495254,29.8149350803117,18.0634500423054));
#50397=CARTESIAN_POINT('Ctrl Pts',(56.8877653171004,29.6465666997486,18.0528156418698));
#50398=CARTESIAN_POINT('Ctrl Pts',(56.9039043478081,29.5973726190831,18.0497134993359));
#50399=CARTESIAN_POINT('Ctrl Pts',(56.9243442566134,29.5257777117091,18.045168280225));
#50400=CARTESIAN_POINT('Ctrl Pts',(56.9302036231324,29.5038421694369,18.0437717783187));
#50401=CARTESIAN_POINT('Ctrl Pts',(56.9400295493195,29.4643663619956,18.0412486308567));
#50402=CARTESIAN_POINT('Ctrl Pts',(56.9441357918232,29.4468632458685,18.040126430872));
#50403=CARTESIAN_POINT('Ctrl Pts',(56.9500239701917,29.4201453316535,18.0384071533119));
#50404=CARTESIAN_POINT('Ctrl Pts',(56.951978455162,29.4109692078438,18.0378155589075));
#50405=CARTESIAN_POINT('Ctrl Pts',(56.9552650180717,29.3949865450273,18.0367830588096));
#50406=CARTESIAN_POINT('Ctrl Pts',(56.956626475505,29.388186160273,18.0363430927333));
#50407=CARTESIAN_POINT('Ctrl Pts',(56.9596037717126,29.3729010865599,18.0353526619981));
#50408=CARTESIAN_POINT('Ctrl Pts',(56.9612000139744,29.3644127657066,18.0348015869995));
#50409=CARTESIAN_POINT('Ctrl Pts',(56.9653280602459,29.3416480653089,18.0333207129244));
#50410=CARTESIAN_POINT('Ctrl Pts',(56.9677593816375,29.3273542157921,18.0323877713829));
#50411=CARTESIAN_POINT('Ctrl Pts',(56.9780576131325,29.2625440692861,18.0281428204872));
#50412=CARTESIAN_POINT('Ctrl Pts',(56.9841358885803,29.2117671008798,18.0247755197651));
#50413=CARTESIAN_POINT('Ctrl Pts',(57.0030975515834,28.9773340406004,18.0090290832544));
#50414=CARTESIAN_POINT('Ctrl Pts',(56.9924650169005,28.7926890268494,17.9959561601167));
#50415=CARTESIAN_POINT('Ctrl Pts',(56.9461977734431,28.5592605768878,17.9796539652705));
#50416=CARTESIAN_POINT('Ctrl Pts',(56.9335677674824,28.5067922991434,17.9760140646675));
#50417=CARTESIAN_POINT('Ctrl Pts',(56.9162441932175,28.4458114560922,17.9718603196061));
#50418=CARTESIAN_POINT('Ctrl Pts',(56.9135989145825,28.4367452150573,17.9712448041018));
#50419=CARTESIAN_POINT('Ctrl Pts',(56.9094245963475,28.422807366722,17.9703020567034));
#50420=CARTESIAN_POINT('Ctrl Pts',(56.9079411188841,28.4179224164041,17.9699723081431));
#50421=CARTESIAN_POINT('Ctrl Pts',(56.9051725899797,28.4089302202114,17.9693666072098));
#50422=CARTESIAN_POINT('Ctrl Pts',(56.9038930070097,28.404821454783,17.9690903556613));
#50423=CARTESIAN_POINT('Ctrl Pts',(56.9009705559212,28.3955432785602,17.9684676693866));
#50424=CARTESIAN_POINT('Ctrl Pts',(56.8993198965764,28.3903764155592,17.968121691337));
#50425=CARTESIAN_POINT('Ctrl Pts',(56.8943708786245,28.3751003201572,17.9671009407073));
#50426=CARTESIAN_POINT('Ctrl Pts',(56.891012676707,28.36501046949,17.9664295319024));
#50427=CARTESIAN_POINT('Ctrl Pts',(56.8557710997816,28.2618853752652,17.959591379748));
#50428=CARTESIAN_POINT('Ctrl Pts',(56.8171248640251,28.1712888741321,17.9537823998474));
#50429=CARTESIAN_POINT('Ctrl Pts',(56.7131989377843,27.9702717075897,17.9405785148102));
#50430=CARTESIAN_POINT('Ctrl Pts',(56.6436605211539,27.8625599789595,17.9332479119037));
#50431=CARTESIAN_POINT('Ctrl Pts',(56.5269289198295,27.715032772372,17.9219907115163));
#50432=CARTESIAN_POINT('Ctrl Pts',(56.4874534903524,27.6695362610519,17.9183261496486));
#50433=CARTESIAN_POINT('Ctrl Pts',(56.4358830446294,27.6152680936827,17.9136632802926));
#50434=CARTESIAN_POINT('Ctrl Pts',(56.4256655237052,27.6047507868735,17.9127451694339));
#50435=CARTESIAN_POINT('Ctrl Pts',(56.4092214157461,27.5881934311821,17.9112760237213));
#50436=CARTESIAN_POINT('Ctrl Pts',(56.4030696495878,27.5820795717187,17.9107282554543));
#50437=CARTESIAN_POINT('Ctrl Pts',(56.3913814106349,27.5706138995664,17.9096908430322));
#50438=CARTESIAN_POINT('Ctrl Pts',(56.3858534243918,27.5652536330882,17.9092015803126));
#50439=CARTESIAN_POINT('Ctrl Pts',(56.3732925193085,27.5532141515733,17.9080928827734));
#50440=CARTESIAN_POINT('Ctrl Pts',(56.3662416824886,27.5465539933079,17.9074726468792));
#50441=CARTESIAN_POINT('Ctrl Pts',(56.3479843856686,27.529558550433,17.9058718433426));
#50442=CARTESIAN_POINT('Ctrl Pts',(56.3367076744035,27.5192999856403,17.904888078671));
#50443=CARTESIAN_POINT('Ctrl Pts',(56.2586290539391,27.449889738141,17.8981090283514));
#50444=CARTESIAN_POINT('Ctrl Pts',(56.1880504229011,27.3951569569671,17.8921346619723));
#50445=CARTESIAN_POINT('Ctrl Pts',(55.993042080647,27.2638613975576,17.8760376483664));
#50446=CARTESIAN_POINT('Ctrl Pts',(55.8634668076913,27.1959126267061,17.8657127289931));
#50447=CARTESIAN_POINT('Ctrl Pts',(55.6812203591201,27.1245127056362,17.8523373866328));
#50448=CARTESIAN_POINT('Ctrl Pts',(55.6341241274545,27.1080694293651,17.8489807377694));
#50449=CARTESIAN_POINT('Ctrl Pts',(55.5776056576967,27.0906846708512,17.8451076288189));
#50450=CARTESIAN_POINT('Ctrl Pts',(55.5687352309557,27.0880236489581,17.8445042220343));
#50451=CARTESIAN_POINT('Ctrl Pts',(55.5549841471116,27.0840026560994,17.8435760507969));
#50452=CARTESIAN_POINT('Ctrl Pts',(55.550116439522,27.0825993820483,17.8432488875649));
#50453=CARTESIAN_POINT('Ctrl Pts',(55.5411006858606,27.0800374592453,17.8426455808977));
#50454=CARTESIAN_POINT('Ctrl Pts',(55.5369542575908,27.0788737063963,17.842369156446));
#50455=CARTESIAN_POINT('Ctrl Pts',(55.5275282421993,27.0762610655953,17.8417431027127));
#50456=CARTESIAN_POINT('Ctrl Pts',(55.5222464449193,27.0748204793991,17.8413939519305));
#50457=CARTESIAN_POINT('Ctrl Pts',(55.5085100860416,27.0711346409395,17.8404900473232));
#50458=CARTESIAN_POINT('Ctrl Pts',(55.500046462024,27.0689231958935,17.8399371638316));
#50459=CARTESIAN_POINT('Ctrl Pts',(55.4438182761371,27.0546258996368,17.8362892556665));
#50460=CARTESIAN_POINT('Ctrl Pts',(55.3956302804157,27.0442565059558,17.8332830769496));
#50461=CARTESIAN_POINT('Ctrl Pts',(55.3330029806956,27.0331899908629,17.8294725779965));
#50462=CARTESIAN_POINT('Ctrl Pts',(55.3188757268696,27.0308502133203,17.8286192969761));
#50463=CARTESIAN_POINT('Ctrl Pts',(55.2641450783895,27.0223900899969,17.8253337585803));
#50464=CARTESIAN_POINT('Ctrl Pts',(55.223380569697,27.0173717162484,17.8229292921772));
#50465=CARTESIAN_POINT('Ctrl Pts',(55.0762660196611,27.0038563116771,17.8143198635165));
#50466=CARTESIAN_POINT('Ctrl Pts',(54.9694349096605,27.0026339342132,17.8081854199797));
#50467=CARTESIAN_POINT('Ctrl Pts',(54.813507427528,27.0133668790575,17.7989163739121));
#50468=CARTESIAN_POINT('Ctrl Pts',(54.7641426116709,27.0186213362915,17.7959369671255));
#50469=CARTESIAN_POINT('Ctrl Pts',(54.6931983924026,27.0288615539455,17.7915572649534));
#50470=CARTESIAN_POINT('Ctrl Pts',(54.671423722046,27.032374127849,17.7901996637063));
#50471=CARTESIAN_POINT('Ctrl Pts',(54.6324166209569,27.0393320822694,17.7877409009367));
#50472=CARTESIAN_POINT('Ctrl Pts',(54.6151628181644,27.0426455259808,17.7866438559577));
#50473=CARTESIAN_POINT('Ctrl Pts',(54.5888491503543,27.0480602014071,17.7849552869356));
#50474=CARTESIAN_POINT('Ctrl Pts',(54.5797561876686,27.0499976584629,17.7843689450596));
#50475=CARTESIAN_POINT('Ctrl Pts',(54.5639127651605,27.0534894126746,17.7833422152924));
#50476=CARTESIAN_POINT('Ctrl Pts',(54.5571561889739,27.0550154499253,17.7829027328036));
#50477=CARTESIAN_POINT('Ctrl Pts',(54.5419345314749,27.0585368334298,17.781908906117));
#50478=CARTESIAN_POINT('Ctrl Pts',(54.5334743185896,27.0605524020323,17.7813539246064));
#50479=CARTESIAN_POINT('Ctrl Pts',(54.5106806898762,27.066140547341,17.7798514926926));
#50480=CARTESIAN_POINT('Ctrl Pts',(54.4963735567035,27.06981706666,17.7789007387953));
#50481=CARTESIAN_POINT('Ctrl Pts',(54.4299525752821,27.0876740879398,17.774449977846));
#50482=CARTESIAN_POINT('Ctrl Pts',(54.3783918026737,27.1038072900062,17.7708878935433));
#50483=CARTESIAN_POINT('Ctrl Pts',(54.1571936289104,27.1830112142003,17.7551258569955));
#50484=CARTESIAN_POINT('Ctrl Pts',(53.9959348693765,27.2669082743935,17.742276924179));
#50485=CARTESIAN_POINT('Ctrl Pts',(53.8187888844234,27.3921851855131,17.7274157489341));
#50486=CARTESIAN_POINT('Ctrl Pts',(53.789912274838,27.413804493902,17.7249702690597));
#50487=CARTESIAN_POINT('Ctrl Pts',(53.744443646218,27.4498107388722,17.7211010926532));
#50488=CARTESIAN_POINT('Ctrl Pts',(53.7274759499059,27.4637086408299,17.719652887236));
#50489=CARTESIAN_POINT('Ctrl Pts',(53.7053019398326,27.4824904328981,17.7177583153406));
#50490=CARTESIAN_POINT('Ctrl Pts',(53.6998884102839,27.4871258442155,17.71729561654));
#50491=CARTESIAN_POINT('Ctrl Pts',(53.691024708216,27.4947982288816,17.7165379296553));
#50492=CARTESIAN_POINT('Ctrl Pts',(53.6875600375025,27.4978182426359,17.7162417375863));
#50493=CARTESIAN_POINT('Ctrl Pts',(53.6807911391025,27.503759713218,17.7156630739839));
#50494=CARTESIAN_POINT('Ctrl Pts',(53.6774861213605,27.5066801896993,17.7153805381141));
#50495=CARTESIAN_POINT('Ctrl Pts',(53.6693649423274,27.5139045710416,17.7146862191356));
#50496=CARTESIAN_POINT('Ctrl Pts',(53.6645598936171,27.5182209997099,17.7142753556603));
#50497=CARTESIAN_POINT('Ctrl Pts',(53.6480923970351,27.5331591011247,17.7128667310573));
#50498=CARTESIAN_POINT('Ctrl Pts',(53.6365346767694,27.5438960414061,17.7118771390249));
#50499=CARTESIAN_POINT('Ctrl Pts',(53.5367996368861,27.6387772250574,17.7033164147693));
#50500=CARTESIAN_POINT('Ctrl Pts',(53.4563667974212,27.7307138097244,17.696255679928));
#50501=CARTESIAN_POINT('Ctrl Pts',(53.3238248941312,27.9135978507516,17.6831400840354));
#50502=CARTESIAN_POINT('Ctrl Pts',(53.2695009990644,28.0024009818177,17.6771096479169));
#50503=CARTESIAN_POINT('Ctrl Pts',(53.1979406496193,28.1429680853764,17.6676298571703));
#50504=CARTESIAN_POINT('Ctrl Pts',(53.1754856925313,28.1918735416007,17.6643448911918));
#50505=CARTESIAN_POINT('Ctrl Pts',(53.1496525329729,28.2547199801584,17.6601097714238));
#50506=CARTESIAN_POINT('Ctrl Pts',(53.1444089602304,28.2678730072018,17.6592227268509));
#50507=CARTESIAN_POINT('Ctrl Pts',(53.1362199996939,28.2890675215343,17.657791772915));
#50508=CARTESIAN_POINT('Ctrl Pts',(53.1331855319149,28.297074245353,17.6572508370274));
#50509=CARTESIAN_POINT('Ctrl Pts',(53.1275131744374,28.3123371045532,17.6562188808308));
#50510=CARTESIAN_POINT('Ctrl Pts',(53.1248656726683,28.3195895199137,17.6557281900277));
#50511=CARTESIAN_POINT('Ctrl Pts',(53.1189235527814,28.3361651281563,17.6546058435977));
#50512=CARTESIAN_POINT('Ctrl Pts',(53.1156560433519,28.3454977581284,17.6539733080981));
#50513=CARTESIAN_POINT('Ctrl Pts',(53.1073248611403,28.3698727978348,17.6523194652743));
#50514=CARTESIAN_POINT('Ctrl Pts',(53.1023711758809,28.3849517953617,17.6512945957911));
#50515=CARTESIAN_POINT('Ctrl Pts',(53.0611082639427,28.5158020475714,17.6423840984435));
#50516=CARTESIAN_POINT('Ctrl Pts',(53.0352582612837,28.6345833017177,17.6341569402808));
#50517=CARTESIAN_POINT('Ctrl Pts',(53.0102373548337,28.8367212287986,17.6200434124739));
#50518=CARTESIAN_POINT('Ctrl Pts',(53.0051918952654,28.9190324141993,17.6142722512882));
#50519=CARTESIAN_POINT('Ctrl Pts',(53.0053057996264,29.0791465571617,17.6031814545234));
#50520=CARTESIAN_POINT('Ctrl Pts',(53.0099041912835,29.1568137953276,17.597864905554));
#50521=CARTESIAN_POINT('Ctrl Pts',(53.0202577197349,29.2444553877004,17.5920697090153));
#50522=CARTESIAN_POINT('Ctrl Pts',(53.0215726775749,29.2548789402342,17.5913838089206));
#50523=CARTESIAN_POINT('Ctrl Pts',(53.023687696584,29.2706406591957,17.5903521985442));
#50524=CARTESIAN_POINT('Ctrl Pts',(53.0244271467207,29.2759865759061,17.5900032759831));
#50525=CARTESIAN_POINT('Ctrl Pts',(53.0257950220923,29.2855884707871,17.5893783932969));
#50526=CARTESIAN_POINT('Ctrl Pts',(53.0264155245548,29.2898454567165,17.5891020030736));
#50527=CARTESIAN_POINT('Ctrl Pts',(53.0278057847463,29.2991719073525,17.5884979014875));
#50528=CARTESIAN_POINT('Ctrl Pts',(53.0285813170688,29.304240416175,17.5881705161606));
#50529=CARTESIAN_POINT('Ctrl Pts',(53.0308569600119,29.3187387979668,17.5872365168331));
#50530=CARTESIAN_POINT('Ctrl Pts',(53.0324052699432,29.3281611190893,17.5866325293694));
#50531=CARTESIAN_POINT('Ctrl Pts',(53.0378624988456,29.3599433479304,17.5846042947244));
#50532=CARTESIAN_POINT('Ctrl Pts',(53.0420850947042,29.3822458266942,17.5831962037013));
#50533=CARTESIAN_POINT('Ctrl Pts',(53.0466869985623,29.4044698763992,17.581803907097));
#50534=CARTESIAN_POINT('',(53.0052506561638,28.9983820491308,17.4520829507836));
#50535=CARTESIAN_POINT('Ctrl Pts',(53.0466869493682,29.4044696388254,17.4239266846335));
#50536=CARTESIAN_POINT('Ctrl Pts',(53.0190383160083,29.2709455589196,17.4330565230793));
#50537=CARTESIAN_POINT('Ctrl Pts',(53.0051399492086,29.1348711355884,17.4425822687156));
#50538=CARTESIAN_POINT('Ctrl Pts',(53.0052506561637,28.9983820492037,17.4520829507785));
#50539=CARTESIAN_POINT('Ctrl Pts',(53.0052506575382,28.9983803554686,17.4520830686754));
#50540=CARTESIAN_POINT('Ctrl Pts',(53.0053310699018,28.8993447299746,17.4589767034832));
#50541=CARTESIAN_POINT('Ctrl Pts',(53.012786828428,28.800437688623,17.4658212023425));
#50542=CARTESIAN_POINT('Ctrl Pts',(53.0287017229543,28.6949278439711,17.4728302018829));
#50543=CARTESIAN_POINT('Ctrl Pts',(53.0298844947448,28.6873807143479,17.4733298875341));
#50544=CARTESIAN_POINT('Ctrl Pts',(53.0319219811726,28.6748507582436,17.4741564985698));
#50545=CARTESIAN_POINT('Ctrl Pts',(53.0327523225448,28.6698641272487,17.4744846842174));
#50546=CARTESIAN_POINT('Ctrl Pts',(53.0342886996821,28.6608490421964,17.475076506032));
#50547=CARTESIAN_POINT('Ctrl Pts',(53.0349881813016,28.6568195205474,17.4753404968462));
#50548=CARTESIAN_POINT('Ctrl Pts',(53.0364490527759,28.6485547603198,17.4758808094941));
#50549=CARTESIAN_POINT('Ctrl Pts',(53.0372117462018,28.6443198765236,17.4761570409539));
#50550=CARTESIAN_POINT('Ctrl Pts',(53.0389655764266,28.6347591239462,17.4767792727686));
#50551=CARTESIAN_POINT('Ctrl Pts',(53.0399647065677,28.6294348125653,17.4771248194195));
#50552=CARTESIAN_POINT('Ctrl Pts',(53.0429832130151,28.6137031634454,17.4781431075827));
#50553=CARTESIAN_POINT('Ctrl Pts',(53.0450639162683,28.6033075869515,17.4788125093786));
#50554=CARTESIAN_POINT('Ctrl Pts',(53.0646406471603,28.5093955018075,17.4848322120176));
#50555=CARTESIAN_POINT('Ctrl Pts',(53.0873982127239,28.4270543455325,17.4899141819321));
#50556=CARTESIAN_POINT('Ctrl Pts',(53.139477273129,28.2768824443825,17.499230763486));
#50557=CARTESIAN_POINT('Ctrl Pts',(53.167420809382,28.2087366600188,17.5034786898085));
#50558=CARTESIAN_POINT('Ctrl Pts',(53.2339999848588,28.0689403702465,17.5124944829673));
#50559=CARTESIAN_POINT('Ctrl Pts',(53.2733797898052,27.9977978038413,17.5172631271533));
#50560=CARTESIAN_POINT('Ctrl Pts',(53.3428000653782,27.888681474978,17.5250670699337));
#50561=CARTESIAN_POINT('Ctrl Pts',(53.3700725708284,27.8490540857701,17.5280122363345));
#50562=CARTESIAN_POINT('Ctrl Pts',(53.4069314295075,27.799438308925,17.5318670402617));
#50563=CARTESIAN_POINT('Ctrl Pts',(53.4152274124654,27.7885084914231,17.5327270479576));
#50564=CARTESIAN_POINT('Ctrl Pts',(53.4288231608752,27.7709749483434,17.5341247754483));
#50565=CARTESIAN_POINT('Ctrl Pts',(53.4340534592386,27.7643177328621,17.5346597676375));
#50566=CARTESIAN_POINT('Ctrl Pts',(53.44414903138,27.7516349485523,17.5356873674046));
#50567=CARTESIAN_POINT('Ctrl Pts',(53.449007337628,27.7456040111901,17.5361796924097));
#50568=CARTESIAN_POINT('Ctrl Pts',(53.4601612331968,27.7319218046539,17.5373051281369));
#50569=CARTESIAN_POINT('Ctrl Pts',(53.4664789200553,27.7242888928893,17.5379391194459));
#50570=CARTESIAN_POINT('Ctrl Pts',(53.4833393142276,27.7042247082529,17.5396221845758));
#50571=CARTESIAN_POINT('Ctrl Pts',(53.4939778010449,27.6918752533793,17.5406751301765));
#50572=CARTESIAN_POINT('Ctrl Pts',(53.5115614693153,27.6719624636846,17.5424013538007));
#50573=CARTESIAN_POINT('Ctrl Pts',(53.5184159593737,27.664319768209,17.5430708809837));
#50574=CARTESIAN_POINT('Ctrl Pts',(53.6156408608556,27.5575841259913,17.5525207898834));
#50575=CARTESIAN_POINT('Ctrl Pts',(53.7157055005721,27.467815378602,17.5617198556858));
#50576=CARTESIAN_POINT('Ctrl Pts',(53.9244408597701,27.3154633923174,17.579711049901));
#50577=CARTESIAN_POINT('Ctrl Pts',(54.0315267343688,27.2516993155066,17.5884371149233));
#50578=CARTESIAN_POINT('Ctrl Pts',(54.1555274857664,27.1927754428589,17.5975646930363));
#50579=CARTESIAN_POINT('Ctrl Pts',(54.1672487399049,27.1873445486173,17.5984181835781));
#50580=CARTESIAN_POINT('Ctrl Pts',(54.1880835898724,27.1779357427103,17.5999178630465));
#50581=CARTESIAN_POINT('Ctrl Pts',(54.1971756134793,27.1739114400203,17.6005664947165));
#50582=CARTESIAN_POINT('Ctrl Pts',(54.2110747522833,27.1678832924025,17.6015488339026));
#50583=CARTESIAN_POINT('Ctrl Pts',(54.2158600966855,27.1658300814104,17.6018853871387));
#50584=CARTESIAN_POINT('Ctrl Pts',(54.2206660902525,27.1637902571315,17.6022216940722));
#50585=CARTESIAN_POINT('Ctrl Pts',(54.2206786884179,27.1637849102022,17.6022225756369));
#50586=CARTESIAN_POINT('Ctrl Pts',(54.2207039232623,27.1637742003039,17.6022243414379));
#50587=CARTESIAN_POINT('Ctrl Pts',(54.2207165598943,27.1637688373559,17.6022252256708));
#50588=CARTESIAN_POINT('Ctrl Pts',(54.2207418718281,27.1637580953568,17.602226996819));
#50589=CARTESIAN_POINT('Ctrl Pts',(54.2207545468393,27.1637527164301,17.6022278837139));
#50590=CARTESIAN_POINT('Ctrl Pts',(54.2207799348258,27.1637419427759,17.6022296601363));
#50591=CARTESIAN_POINT('Ctrl Pts',(54.2207926490437,27.163736547522,17.6022305497508));
#50592=CARTESIAN_POINT('Ctrl Pts',(54.2208181166296,27.1637257407132,17.6022323316952));
#50593=CARTESIAN_POINT('Ctrl Pts',(54.2208308690471,27.1637203295625,17.6022332239586));
#50594=CARTESIAN_POINT('Ctrl Pts',(54.2208564123642,27.1637094912463,17.6022350111539));
#50595=CARTESIAN_POINT('Ctrl Pts',(54.2208692047696,27.1637040634427,17.6022359061911));
#50596=CARTESIAN_POINT('Ctrl Pts',(54.2208948296117,27.1636931911664,17.6022376990422));
#50597=CARTESIAN_POINT('Ctrl Pts',(54.220907660359,27.1636877474114,17.6022385967379));
#50598=CARTESIAN_POINT('Ctrl Pts',(54.2209333618325,27.1636768432572,17.602240394902));
#50599=CARTESIAN_POINT('Ctrl Pts',(54.2209462329074,27.1636713827111,17.6022412953948));
#50600=CARTESIAN_POINT('Ctrl Pts',(54.2209720147674,27.1636604450916,17.6022430991341));
#50601=CARTESIAN_POINT('Ctrl Pts',(54.2209849256474,27.1636549679791,17.6022440023873));
#50602=CARTESIAN_POINT('Ctrl Pts',(54.2210107873937,27.1636439971125,17.6022458116664));
#50603=CARTESIAN_POINT('Ctrl Pts',(54.2210237384327,27.1636385032863,17.6022467177044));
#50604=CARTESIAN_POINT('Ctrl Pts',(54.2210496807063,27.1636274989068,17.6022485325678));
#50605=CARTESIAN_POINT('Ctrl Pts',(54.2210626721279,27.1636219882751,17.6022494414061));
#50606=CARTESIAN_POINT('Ctrl Pts',(54.221088695651,27.1636109500823,17.6022512619037));
#50607=CARTESIAN_POINT('Ctrl Pts',(54.2211017275756,27.1636054225971,17.6022521735505));
#50608=CARTESIAN_POINT('Ctrl Pts',(54.2211278324925,27.1635943505358,17.6022539996919));
#50609=CARTESIAN_POINT('Ctrl Pts',(54.2211409052794,27.1635888060479,17.6022549141721));
#50610=CARTESIAN_POINT('Ctrl Pts',(54.22116709213,27.1635776998954,17.6022567459947));
#50611=CARTESIAN_POINT('Ctrl Pts',(54.2211802060632,27.1635721382872,17.602257663328));
#50612=CARTESIAN_POINT('Ctrl Pts',(54.2212064748903,27.1635609980314,17.6022595008343));
#50613=CARTESIAN_POINT('Ctrl Pts',(54.2212196304669,27.1635554190954,17.602260421055));
#50614=CARTESIAN_POINT('Ctrl Pts',(54.2212459832692,27.163544243895,17.6022622643843));
#50615=CARTESIAN_POINT('Ctrl Pts',(54.2212591801162,27.1635386477924,17.6022631874663));
#50616=CARTESIAN_POINT('Ctrl Pts',(54.2212854599706,27.1635275041949,17.6022650256419));
#50617=CARTESIAN_POINT('Ctrl Pts',(54.2212985437312,27.1635219563777,17.6022659407885));
#50618=CARTESIAN_POINT('Ctrl Pts',(54.2213249053245,27.1635107787847,17.6022677846307));
#50619=CARTESIAN_POINT('Ctrl Pts',(54.2213381823626,27.1635051493506,17.6022687132703));
#50620=CARTESIAN_POINT('Ctrl Pts',(54.2213649339917,27.1634938070629,17.6022705843409));
#50621=CARTESIAN_POINT('Ctrl Pts',(54.2213784081539,27.163488094396,17.6022715267415));
#50622=CARTESIAN_POINT('Ctrl Pts',(54.2214055570371,27.1634765843835,17.6022734255431));
#50623=CARTESIAN_POINT('Ctrl Pts',(54.2214192315397,27.1634707871356,17.6022743819284));
#50624=CARTESIAN_POINT('Ctrl Pts',(54.2214467836432,27.1634591069002,17.6022763088758));
#50625=CARTESIAN_POINT('Ctrl Pts',(54.2214606621074,27.1634532235521,17.6022772794979));
#50626=CARTESIAN_POINT('Ctrl Pts',(54.2214886254689,27.163441369719,17.6022792351508));
#50627=CARTESIAN_POINT('Ctrl Pts',(54.2215027107765,27.1634353990655,17.60228022021));
#50628=CARTESIAN_POINT('Ctrl Pts',(54.2215310924091,27.1634233686951,17.6022822050563));
#50629=CARTESIAN_POINT('Ctrl Pts',(54.2215453876823,27.1634173094297,17.6022832047696));
#50630=CARTESIAN_POINT('Ctrl Pts',(54.2215741922858,27.1634051005644,17.6022852191354));
#50631=CARTESIAN_POINT('Ctrl Pts',(54.2215887020234,27.1633989507978,17.602286233816));
#50632=CARTESIAN_POINT('Ctrl Pts',(54.221617938954,27.1633865595075,17.6022882783528));
#50633=CARTESIAN_POINT('Ctrl Pts',(54.221632666116,27.1633803180032,17.6022893082064));
#50634=CARTESIAN_POINT('Ctrl Pts',(54.2216623412379,27.1633677418393,17.6022913833216));
#50635=CARTESIAN_POINT('Ctrl Pts',(54.221677289864,27.1633614069039,17.6022924286292));
#50636=CARTESIAN_POINT('Ctrl Pts',(54.2217074120727,27.1633486421346,17.6022945349418));
#50637=CARTESIAN_POINT('Ctrl Pts',(54.2217225853326,27.163342212444,17.6022955959236));
#50638=CARTESIAN_POINT('Ctrl Pts',(54.2217531610186,27.1633292564002,17.6022977338775));
#50639=CARTESIAN_POINT('Ctrl Pts',(54.2217685630084,27.1633227302387,17.6022988108185));
#50640=CARTESIAN_POINT('Ctrl Pts',(54.2257451600363,27.1616378176921,17.6025768587078));
#50641=CARTESIAN_POINT('Ctrl Pts',(54.2297117234843,27.1599722713291,17.6028530415225));
#50642=CARTESIAN_POINT('Ctrl Pts',(54.2386682606902,27.1562454903112,17.6034740649115));
#50643=CARTESIAN_POINT('Ctrl Pts',(54.2436612244966,27.1541916763677,17.6038184597301));
#50644=CARTESIAN_POINT('Ctrl Pts',(54.2584034658854,27.1481974414447,17.6048301849808));
#50645=CARTESIAN_POINT('Ctrl Pts',(54.268175811701,27.1443137377219,17.6054942394079));
#50646=CARTESIAN_POINT('Ctrl Pts',(54.3757655968861,27.1025377604369,17.6127378250549));
#50647=CARTESIAN_POINT('Ctrl Pts',(54.4764100865542,27.0723352431683,17.6189090372922));
#50648=CARTESIAN_POINT('Ctrl Pts',(54.6227855737681,27.0407282956951,17.6276321890022));
#50649=CARTESIAN_POINT('Ctrl Pts',(54.6669017465558,27.0327476206307,17.6302289151256));
#50650=CARTESIAN_POINT('Ctrl Pts',(54.8399505521809,27.0074312478132,17.640396164686));
#50651=CARTESIAN_POINT('Ctrl Pts',(54.9701665452203,27.0012379497982,17.6480321739293));
#50652=CARTESIAN_POINT('Ctrl Pts',(55.1186595281676,27.0086952332072,17.6572467609195));
#50653=CARTESIAN_POINT('Ctrl Pts',(55.137254736408,27.0098904907673,17.6584092137807));
#50654=CARTESIAN_POINT('Ctrl Pts',(55.1653170078396,27.0120894372619,17.6601775425317));
#50655=CARTESIAN_POINT('Ctrl Pts',(55.1747984436282,27.0129007026306,17.6607774370694));
#50656=CARTESIAN_POINT('Ctrl Pts',(55.191925084206,27.0144896439544,17.6618655886749));
#50657=CARTESIAN_POINT('Ctrl Pts',(55.1995723321909,27.0152437193823,17.6623531006616));
#50658=CARTESIAN_POINT('Ctrl Pts',(55.2159634796086,27.0169556964765,17.6634016380672));
#50659=CARTESIAN_POINT('Ctrl Pts',(55.224705756195,27.0179272835409,17.6639630813612));
#50660=CARTESIAN_POINT('Ctrl Pts',(55.2481767107033,27.0206930422779,17.6654764831163));
#50661=CARTESIAN_POINT('Ctrl Pts',(55.2628920422605,27.0225937526338,17.6664317492673));
#50662=CARTESIAN_POINT('Ctrl Pts',(55.3336380107139,27.0325353155998,17.6710562351777));
#50663=CARTESIAN_POINT('Ctrl Pts',(55.3893257329002,27.0427938204031,17.6747940950256));
#50664=CARTESIAN_POINT('Ctrl Pts',(55.6027961515303,27.0915891328643,17.6895109322272));
#50665=CARTESIAN_POINT('Ctrl Pts',(55.7560734251355,27.1469658488327,17.700975167431));
#50666=CARTESIAN_POINT('Ctrl Pts',(55.9422782234711,27.2412252414257,17.7153763809503));
#50667=CARTESIAN_POINT('Ctrl Pts',(55.9829017179762,27.2636009445861,17.7185447431241));
#50668=CARTESIAN_POINT('Ctrl Pts',(56.0377220973037,27.2963374453801,17.7228239905435));
#50669=CARTESIAN_POINT('Ctrl Pts',(56.0526153068573,27.3054988013607,17.7239868879664));
#50670=CARTESIAN_POINT('Ctrl Pts',(56.0781697105675,27.3216852018592,17.7259803515297));
#50671=CARTESIAN_POINT('Ctrl Pts',(56.0888872823697,27.3286188367388,17.7268158274645));
#50672=CARTESIAN_POINT('Ctrl Pts',(56.1043471453395,27.3388322876095,17.7280192898394));
#50673=CARTESIAN_POINT('Ctrl Pts',(56.1091426842319,27.3420303699639,17.7283923557106));
#50674=CARTESIAN_POINT('Ctrl Pts',(56.1175216589074,27.3476708230647,17.7290436772925));
#50675=CARTESIAN_POINT('Ctrl Pts',(56.1211110815544,27.3501041513765,17.7293225232524));
#50676=CARTESIAN_POINT('Ctrl Pts',(56.1287236711925,27.3553011646732,17.7299135220624));
#50677=CARTESIAN_POINT('Ctrl Pts',(56.1327446403439,27.3580679168016,17.7302254653136));
#50678=CARTESIAN_POINT('Ctrl Pts',(56.1436682042649,27.3656434386958,17.7310724180463));
#50679=CARTESIAN_POINT('Ctrl Pts',(56.1505506923276,27.3704812240284,17.7316055147836));
#50680=CARTESIAN_POINT('Ctrl Pts',(56.1827410347344,27.3934138371999,17.7340974171284));
#50681=CARTESIAN_POINT('Ctrl Pts',(56.2076554328252,27.4120566577362,17.7360218090352));
#50682=CARTESIAN_POINT('Ctrl Pts',(56.3937699748815,27.558236846224,17.7504499235633));
#50683=CARTESIAN_POINT('Ctrl Pts',(56.534834431795,27.7094265997486,17.7618160924564));
#50684=CARTESIAN_POINT('Ctrl Pts',(56.681139783878,27.9249152915941,17.777458158453));
#50685=CARTESIAN_POINT('Ctrl Pts',(56.7100716870995,27.971558406825,17.7808067421583));
#50686=CARTESIAN_POINT('Ctrl Pts',(56.7440476597548,28.0317395254409,17.7851136824006));
#50687=CARTESIAN_POINT('Ctrl Pts',(56.7509193465716,28.0442217771177,17.7860062213409));
#50688=CARTESIAN_POINT('Ctrl Pts',(56.7617146365337,28.0643383337482,17.787443929173));
#50689=CARTESIAN_POINT('Ctrl Pts',(56.7657237948351,28.0719263547986,17.7879860735772));
#50690=CARTESIAN_POINT('Ctrl Pts',(56.7732444982222,28.0863857184188,17.7890189621643));
#50691=CARTESIAN_POINT('Ctrl Pts',(56.776765389003,28.0932520440062,17.7895093675116));
#50692=CARTESIAN_POINT('Ctrl Pts',(56.7846910262917,28.1089317761663,17.790629141014));
#50693=CARTESIAN_POINT('Ctrl Pts',(56.7890704640952,28.1177576820218,17.7912593742738));
#50694=CARTESIAN_POINT('Ctrl Pts',(56.8002819012679,28.1407789470757,17.792903250329));
#50695=CARTESIAN_POINT('Ctrl Pts',(56.8070113335533,28.1550232199925,17.7939203852734));
#50696=CARTESIAN_POINT('Ctrl Pts',(56.8682703718384,28.2887702956405,17.8034727589273));
#50697=CARTESIAN_POINT('Ctrl Pts',(56.9110295851718,28.4132836362014,17.8124127544674));
#50698=CARTESIAN_POINT('Ctrl Pts',(56.9632725850951,28.6342687605549,17.8281845211868));
#50699=CARTESIAN_POINT('Ctrl Pts',(56.978565411335,28.7289316432631,17.8349027535602));
#50700=CARTESIAN_POINT('Ctrl Pts',(56.9919646082382,28.8804878471083,17.8453402503885));
#50701=CARTESIAN_POINT('Ctrl Pts',(56.9945470938814,28.936838950889,17.8491501643012));
#50702=CARTESIAN_POINT('Ctrl Pts',(56.9947709041649,29.0027727513714,17.8534711939293));
#50703=CARTESIAN_POINT('Ctrl Pts',(56.9947348070347,29.0123169206123,17.8540933146974));
#50704=CARTESIAN_POINT('Ctrl Pts',(56.9945740280993,29.0269868398502,17.8550440039881));
#50705=CARTESIAN_POINT('Ctrl Pts',(56.9944980849615,29.0321128261133,17.8553751545043));
#50706=CARTESIAN_POINT('Ctrl Pts',(56.994322068357,29.0415398341059,17.8559821766046));
#50707=CARTESIAN_POINT('Ctrl Pts',(56.9942278432773,29.0458408106386,17.8562583571489));
#50708=CARTESIAN_POINT('Ctrl Pts',(56.9939840170005,29.0555377282512,17.8568793199967));
#50709=CARTESIAN_POINT('Ctrl Pts',(56.9938264278445,29.0609333782337,17.8572236569441));
#50710=CARTESIAN_POINT('Ctrl Pts',(56.9932974282019,29.0768336343943,17.8582350529822));
#50711=CARTESIAN_POINT('Ctrl Pts',(56.9928648829864,29.0873362129997,17.858898839248));
#50712=CARTESIAN_POINT('Ctrl Pts',(56.9885803678744,29.1745875837308,17.8643814497677));
#50713=CARTESIAN_POINT('Ctrl Pts',(56.9803788827988,29.2510677792958,17.8689832328801));
#50714=CARTESIAN_POINT('Ctrl Pts',(56.9502425906742,29.4324783423043,17.8798039582074));
#50715=CARTESIAN_POINT('Ctrl Pts',(56.9242325719471,29.5364826414008,17.8859374371959));
#50716=CARTESIAN_POINT('Ctrl Pts',(56.8611302393796,29.7234456167472,17.897508191926));
#50717=CARTESIAN_POINT('Ctrl Pts',(56.8264860433627,29.8069233305392,17.9028893613067));
#50718=CARTESIAN_POINT('Ctrl Pts',(56.7764231232287,29.9076574456042,17.9098332291545));
#50719=CARTESIAN_POINT('Ctrl Pts',(56.7662041573711,29.9273855534195,17.9112153556383));
#50720=CARTESIAN_POINT('Ctrl Pts',(56.7508115781797,29.9559239570786,17.9132493580063));
#50721=CARTESIAN_POINT('Ctrl Pts',(56.7458961884439,29.9648721609598,17.9138921711154));
#50722=CARTESIAN_POINT('Ctrl Pts',(56.7371226612382,29.9805573354622,17.915028067297));
#50723=CARTESIAN_POINT('Ctrl Pts',(56.7332934513718,29.9873103043041,17.9155201145636));
#50724=CARTESIAN_POINT('Ctrl Pts',(56.725236657887,30.0013274568865,17.9165478282894));
#50725=CARTESIAN_POINT('Ctrl Pts',(56.7210023943069,30.0085876049615,17.9170837273449));
#50726=CARTESIAN_POINT('Ctrl Pts',(56.7098770974915,30.0273891974074,17.9184810481919));
#50727=CARTESIAN_POINT('Ctrl Pts',(56.7029151491255,30.0388879784544,17.9193450194241));
#50728=CARTESIAN_POINT('Ctrl Pts',(56.6740249701946,30.0855340224608,17.9228889918404));
#50729=CARTESIAN_POINT('Ctrl Pts',(56.6511219204021,30.1200623639201,17.9256043483224));
#50730=CARTESIAN_POINT('Ctrl Pts',(56.5261041751656,30.2963625699396,17.9399680452105));
#50731=CARTESIAN_POINT('Ctrl Pts',(56.4067711209741,30.4249650348056,17.9522781110881));
#50732=CARTESIAN_POINT('Ctrl Pts',(56.2202658086442,30.5794098049016,17.9690251889766));
#50733=CARTESIAN_POINT('Ctrl Pts',(56.1661190447471,30.6198000411304,17.9736363659764));
#50734=CARTESIAN_POINT('Ctrl Pts',(56.0981210486691,30.6653416873858,17.9790425256776));
#50735=CARTESIAN_POINT('Ctrl Pts',(56.0861328038122,30.6731850865667,17.9799818016131));
#50736=CARTESIAN_POINT('Ctrl Pts',(56.0689718464324,30.6841505941709,17.9813056588599));
#50737=CARTESIAN_POINT('Ctrl Pts',(56.0638681732421,30.687379194065,17.9816968045988));
#50738=CARTESIAN_POINT('Ctrl Pts',(56.055039858614,30.6929080369164,17.9823688803188));
#50739=CARTESIAN_POINT('Ctrl Pts',(56.0513221874479,30.6952192732507,17.9826505199787));
#50740=CARTESIAN_POINT('Ctrl Pts',(56.0435539934532,30.7000132925545,17.9832361121092));
#50741=CARTESIAN_POINT('Ctrl Pts',(56.03950218824,30.7024938572271,17.9835399225304));
#50742=CARTESIAN_POINT('Ctrl Pts',(56.0287526042198,30.7090222014675,17.9843417486125));
#50743=CARTESIAN_POINT('Ctrl Pts',(56.0220397206993,30.7130451307316,17.9848381824922));
#50744=CARTESIAN_POINT('Ctrl Pts',(55.9933191109478,30.7300280326622,17.9869446860678));
#50745=CARTESIAN_POINT('Ctrl Pts',(55.9710861694229,30.7426048446625,17.988531910429));
#50746=CARTESIAN_POINT('Ctrl Pts',(55.7793729537247,30.8462447649454,18.0019050651092));
#50747=CARTESIAN_POINT('Ctrl Pts',(55.5977660275354,30.9127827008792,18.0125997318855));
#50748=CARTESIAN_POINT('Ctrl Pts',(55.3385656942483,30.9671405592272,18.0283297222333));
#50749=CARTESIAN_POINT('Ctrl Pts',(55.2669619051846,30.9781300055519,18.0327093964411));
#50750=CARTESIAN_POINT('Ctrl Pts',(55.1795452669117,30.9867133314852,18.0381745538085));
#50751=CARTESIAN_POINT('Ctrl Pts',(55.1641493319842,30.9880446021534,18.0391413746449));
#50752=CARTESIAN_POINT('Ctrl Pts',(55.1399185658695,30.9898564287235,18.0406703818557));
#50753=CARTESIAN_POINT('Ctrl Pts',(55.1310931432675,30.9904573333141,18.0412288188772));
#50754=CARTESIAN_POINT('Ctrl Pts',(55.1145987996252,30.9914702248503,18.042275505755));
#50755=CARTESIAN_POINT('Ctrl Pts',(55.1069309050358,30.9918966640376,18.0427632962151));
#50756=CARTESIAN_POINT('Ctrl Pts',(55.089823695559,30.9927489923994,18.0438543403244));
#50757=CARTESIAN_POINT('Ctrl Pts',(55.0803834802504,30.9931521101139,18.044458290809));
#50758=CARTESIAN_POINT('Ctrl Pts',(55.0565244411337,30.994001165299,18.0459896168197));
#50759=CARTESIAN_POINT('Ctrl Pts',(55.0421031751652,30.9943577824104,18.046919738523));
#50760=CARTESIAN_POINT('Ctrl Pts',(54.9571838766018,30.9955362558557,18.0524244202368));
#50761=CARTESIAN_POINT('Ctrl Pts',(54.8866938513219,30.9927764287255,18.0571087171278));
#50762=CARTESIAN_POINT('Ctrl Pts',(54.6533071164275,30.9712159262342,18.0729996511112));
#50763=CARTESIAN_POINT('Ctrl Pts',(54.4926125923868,30.9360880585725,18.084622513298));
#50764=CARTESIAN_POINT('Ctrl Pts',(54.3050904240727,30.8701197511106,18.0982249773966));
#50765=CARTESIAN_POINT('Ctrl Pts',(54.2724542042124,30.8576664399839,18.100590829316));
#50766=CARTESIAN_POINT('Ctrl Pts',(54.226820196614,30.838866147518,18.1038814662716));
#50767=CARTESIAN_POINT('Ctrl Pts',(54.2135399501208,30.833225663482,18.1048369532052));
#50768=CARTESIAN_POINT('Ctrl Pts',(54.1902555979994,30.8230365586655,18.1065069898863));
#50769=CARTESIAN_POINT('Ctrl Pts',(54.1802258294138,30.818548490721,18.1072246316383));
#50770=CARTESIAN_POINT('Ctrl Pts',(54.1653006673944,30.8117212836476,18.1082894017579));
#50771=CARTESIAN_POINT('Ctrl Pts',(54.1603770977963,30.8094447682218,18.1086401374315));
#50772=CARTESIAN_POINT('Ctrl Pts',(54.1519381695338,30.8055009915392,18.109240330525));
#50773=CARTESIAN_POINT('Ctrl Pts',(54.1484183470432,30.8038435043014,18.1094903749864));
#50774=CARTESIAN_POINT('Ctrl Pts',(54.1404408438513,30.8000583369093,18.1100564124022));
#50775=CARTESIAN_POINT('Ctrl Pts',(54.1359862072817,30.7979243939776,18.1103720161398));
#50776=CARTESIAN_POINT('Ctrl Pts',(54.1239270093877,30.79209240298,18.1112252326808));
#50777=CARTESIAN_POINT('Ctrl Pts',(54.1163378599069,30.7883624615497,18.1117609292112));
#50778=CARTESIAN_POINT('Ctrl Pts',(54.0795671283573,30.7699990324613,18.1143514642539));
#50779=CARTESIAN_POINT('Ctrl Pts',(54.0507222224008,30.754698045739,18.1163682341222));
#50780=CARTESIAN_POINT('Ctrl Pts',(53.8445446736308,30.6387563692747,18.1307649890349));
#50781=CARTESIAN_POINT('Ctrl Pts',(53.6831845308571,30.5121560703674,18.1420502566199));
#50782=CARTESIAN_POINT('Ctrl Pts',(53.5063966227145,30.3233187905913,18.1575864865704));
#50783=CARTESIAN_POINT('Ctrl Pts',(53.4706512095115,30.2818405263651,18.1609272596754));
#50784=CARTESIAN_POINT('Ctrl Pts',(53.4278154519344,30.2277890798096,18.1652253853925));
#50785=CARTESIAN_POINT('Ctrl Pts',(53.4190921975894,30.2165363872221,18.1661172562577));
#50786=CARTESIAN_POINT('Ctrl Pts',(53.4053066393238,30.1983548134038,18.1675541428123));
#50787=CARTESIAN_POINT('Ctrl Pts',(53.4001671826546,30.1914848409589,18.1680961402357));
#50788=CARTESIAN_POINT('Ctrl Pts',(53.3904895710177,30.1783731550427,18.1691289145803));
#50789=CARTESIAN_POINT('Ctrl Pts',(53.3859429940054,30.1721378298651,18.169619353797));
#50790=CARTESIAN_POINT('Ctrl Pts',(53.3756716267862,30.1578782572735,18.1707394361714));
#50791=CARTESIAN_POINT('Ctrl Pts',(53.369969939187,30.1498376919417,18.1713699462091));
#50792=CARTESIAN_POINT('Ctrl Pts',(53.3553029427684,30.1288258405662,18.1730150195902));
#50793=CARTESIAN_POINT('Ctrl Pts',(53.3464315674151,30.1157901252531,18.1740330834592));
#50794=CARTESIAN_POINT('Ctrl Pts',(53.2654322607865,29.9936808876836,18.1835481770535));
#50795=CARTESIAN_POINT('Ctrl Pts',(53.2040521936149,29.8778877297199,18.1924460535315));
#50796=CARTESIAN_POINT('Ctrl Pts',(53.1185826541295,29.6694993110158,18.2080880314943));
#50797=CARTESIAN_POINT('Ctrl Pts',(53.0889773901164,29.5796150587301,18.2147178292819));
#50798=CARTESIAN_POINT('Ctrl Pts',(53.0588688089847,29.4602750038332,18.2231691213204));
#50799=CARTESIAN_POINT('Ctrl Pts',(53.0524777514281,29.4324352549098,18.2251158808612));
#50800=CARTESIAN_POINT('Ctrl Pts',(53.0466869962288,29.4044698651299,18.2270410618393));
#50801=CARTESIAN_POINT('Origin',(55.,29.,3.45145488139523));
#50802=CARTESIAN_POINT('',(53.0466869987623,29.4044698773653,19.1852189598335));
#50803=CARTESIAN_POINT('',(53.0466869973344,29.4044698704695,19.02544331564));
#50804=CARTESIAN_POINT('',(53.0466869980082,29.4044698737233,3.45145488139523));
#50805=CARTESIAN_POINT('',(53.0052500748225,29.0005463555814,18.4113483399464));
#50806=CARTESIAN_POINT('Ctrl Pts',(53.0466869987623,29.4044698773653,19.1852189598335));
#50807=CARTESIAN_POINT('Ctrl Pts',(53.0473612262886,29.4077259353972,19.1850147090984));
#50808=CARTESIAN_POINT('Ctrl Pts',(53.0480436373529,29.4109805106691,19.1848102091115));
#50809=CARTESIAN_POINT('Ctrl Pts',(53.0537663371002,29.4379375437896,19.1831134921491));
#50810=CARTESIAN_POINT('Ctrl Pts',(53.059229781962,29.461547012844,19.1816089637445));
#50811=CARTESIAN_POINT('Ctrl Pts',(53.0674968539547,29.4945245749462,19.179478881008));
#50812=CARTESIAN_POINT('Ctrl Pts',(53.0699414503623,29.5039811050769,19.1788647478418));
#50813=CARTESIAN_POINT('Ctrl Pts',(53.0743130575776,29.5203935582042,19.1777929312071));
#50814=CARTESIAN_POINT('Ctrl Pts',(53.0762085693706,29.5273577389787,19.1773362640326));
#50815=CARTESIAN_POINT('Ctrl Pts',(53.0802472017588,29.5418842465995,19.1763797217002));
#50816=CARTESIAN_POINT('Ctrl Pts',(53.0823973049675,29.5494444869004,19.1758796284688));
#50817=CARTESIAN_POINT('Ctrl Pts',(53.0876088770486,29.5673662731329,19.1746886584122));
#50818=CARTESIAN_POINT('Ctrl Pts',(53.090709932972,29.5777159573914,19.1739965114367));
#50819=CARTESIAN_POINT('Ctrl Pts',(53.1014437818026,29.6125092575854,19.1716546102347));
#50820=CARTESIAN_POINT('Ctrl Pts',(53.1094628792296,29.6368301176442,19.1699923927686));
#50821=CARTESIAN_POINT('Ctrl Pts',(53.1297722393553,29.6946575262177,19.1659776903143));
#50822=CARTESIAN_POINT('Ctrl Pts',(53.1424975298548,29.7280008717266,19.1636116926628));
#50823=CARTESIAN_POINT('Ctrl Pts',(53.1960533824514,29.8577686524445,19.1542000129544));
#50824=CARTESIAN_POINT('Ctrl Pts',(53.243551227458,29.9512484788758,19.14695833577));
#50825=CARTESIAN_POINT('Ctrl Pts',(53.361190148608,30.143647678873,19.1312465846423));
#50826=CARTESIAN_POINT('Ctrl Pts',(53.4334635779966,30.240804813961,19.1227893245507));
#50827=CARTESIAN_POINT('Ctrl Pts',(53.5246380934012,30.3426036864123,19.1137388689292));
#50828=CARTESIAN_POINT('Ctrl Pts',(53.53532376407,30.3542529214894,19.1127003753375));
#50829=CARTESIAN_POINT('Ctrl Pts',(53.5505732211759,30.3704858128896,19.1112507844475));
#50830=CARTESIAN_POINT('Ctrl Pts',(53.5550222216541,30.3751758336233,19.1108316703867));
#50831=CARTESIAN_POINT('Ctrl Pts',(53.5625455883242,30.3830299482655,19.1101294290633));
#50832=CARTESIAN_POINT('Ctrl Pts',(53.5656077672521,30.3862055934623,19.1098453887443));
#50833=CARTESIAN_POINT('Ctrl Pts',(53.5718806856916,30.3926679060776,19.1092672132134));
#50834=CARTESIAN_POINT('Ctrl Pts',(53.5750922835094,30.3959536786868,19.1089731476298));
#50835=CARTESIAN_POINT('Ctrl Pts',(53.5833095553217,30.4043028305138,19.1082255998842));
#50836=CARTESIAN_POINT('Ctrl Pts',(53.5883310888946,30.4093506110649,19.1077733341543));
#50837=CARTESIAN_POINT('Ctrl Pts',(53.6088891496666,30.4297960083727,19.1059396715377));
#50838=CARTESIAN_POINT('Ctrl Pts',(53.6246520842106,30.4449651299586,19.1045749792881));
#50839=CARTESIAN_POINT('Ctrl Pts',(53.6669604389453,30.4843599027799,19.101009056972));
#50840=CARTESIAN_POINT('Ctrl Pts',(53.6939172269262,30.5081335766629,19.0988344658239));
#50841=CARTESIAN_POINT('Ctrl Pts',(53.858719750057,30.6457406920399,19.0860061480243));
#50842=CARTESIAN_POINT('Ctrl Pts',(54.0107158702992,30.7413522000486,19.0759860422558));
#50843=CARTESIAN_POINT('Ctrl Pts',(54.2244025386128,30.8386444394249,19.0619063498638));
#50844=CARTESIAN_POINT('Ctrl Pts',(54.2763294469729,30.8596948317025,19.0584927976127));
#50845=CARTESIAN_POINT('Ctrl Pts',(54.3431604195879,30.8835639614664,19.0540744951304));
#50846=CARTESIAN_POINT('Ctrl Pts',(54.3573067972331,30.8884376768456,19.0531379388316));
#50847=CARTESIAN_POINT('Ctrl Pts',(54.3798000143404,30.8959050360664,19.0516461190086));
#50848=CARTESIAN_POINT('Ctrl Pts',(54.3881115561153,30.8986038176318,19.0510943015346));
#50849=CARTESIAN_POINT('Ctrl Pts',(54.4037010485234,30.9035527709367,19.0500581048983));
#50850=CARTESIAN_POINT('Ctrl Pts',(54.4109746994205,30.9058160414711,19.0495741631407));
#50851=CARTESIAN_POINT('Ctrl Pts',(54.4274078397576,30.9108263189888,19.0484796451272));
#50852=CARTESIAN_POINT('Ctrl Pts',(54.4365744262375,30.9135492209276,19.0478682994079));
#50853=CARTESIAN_POINT('Ctrl Pts',(54.4638797157178,30.9214469522576,19.0460446365198));
#50854=CARTESIAN_POINT('Ctrl Pts',(54.4820722140643,30.926430408249,19.0448261968074));
#50855=CARTESIAN_POINT('Ctrl Pts',(54.6334056875171,30.9655864948283,19.0346596194944));
#50856=CARTESIAN_POINT('Ctrl Pts',(54.7696566592804,30.9861647593858,19.0252692209402));
#50857=CARTESIAN_POINT('Ctrl Pts',(55.04164550012,30.9988709716941,19.0063281108385));
#50858=CARTESIAN_POINT('Ctrl Pts',(55.1766764946827,30.9914844926473,18.9968392517258));
#50859=CARTESIAN_POINT('Ctrl Pts',(55.3249319060831,30.9681659606946,18.986908721277));
#50860=CARTESIAN_POINT('Ctrl Pts',(55.3399006051719,30.9656361830665,18.9859120255489));
#50861=CARTESIAN_POINT('Ctrl Pts',(55.3604823329134,30.961915628234,18.9845511214463));
#50862=CARTESIAN_POINT('Ctrl Pts',(55.366120831676,30.9608712306551,18.9841792827924));
#50863=CARTESIAN_POINT('Ctrl Pts',(55.3757729757383,30.9590403159818,18.9835445467261));
#50864=CARTESIAN_POINT('Ctrl Pts',(55.3797888108251,30.9582657503111,18.9832809921011));
#50865=CARTESIAN_POINT('Ctrl Pts',(55.3881434546208,30.9566276578429,18.9827338333955));
#50866=CARTESIAN_POINT('Ctrl Pts',(55.3924818011706,30.955762043033,18.98245035858));
#50867=CARTESIAN_POINT('Ctrl Pts',(55.40299079337,30.9536288454599,18.9817651873235));
#50868=CARTESIAN_POINT('Ctrl Pts',(55.409158451742,30.9523464368005,18.9813643222031));
#50869=CARTESIAN_POINT('Ctrl Pts',(55.4308916211277,30.9477200608235,18.9799558891768));
#50870=CARTESIAN_POINT('Ctrl Pts',(55.4464235466126,30.9442188865876,18.9789567771364));
#50871=CARTESIAN_POINT('Ctrl Pts',(55.4846132961889,30.9351284304626,18.9765148384214));
#50872=CARTESIAN_POINT('Ctrl Pts',(55.5072185917325,30.9293266924921,18.9750822146106));
#50873=CARTESIAN_POINT('Ctrl Pts',(55.5999926576407,30.9037724682284,18.9692361598874));
#50874=CARTESIAN_POINT('Ctrl Pts',(55.6691592728681,30.8805765868043,18.9649562028322));
#50875=CARTESIAN_POINT('Ctrl Pts',(55.8944470716964,30.7910147613643,18.9508308234911));
#50876=CARTESIAN_POINT('Ctrl Pts',(56.0433440672059,30.7085657596047,18.9411217514176));
#50877=CARTESIAN_POINT('Ctrl Pts',(56.1983520944798,30.5948344255417,18.929260414512));
#50878=CARTESIAN_POINT('Ctrl Pts',(56.2164530149839,30.5810713406381,18.9278464005509));
#50879=CARTESIAN_POINT('Ctrl Pts',(56.2423216217464,30.5606948623709,18.9257810993182));
#50880=CARTESIAN_POINT('Ctrl Pts',(56.2502804955817,30.5543262661049,18.9251394256589));
#50881=CARTESIAN_POINT('Ctrl Pts',(56.2642331237616,30.5429850347085,18.9240032308046));
#50882=CARTESIAN_POINT('Ctrl Pts',(56.2702472678371,30.538037738261,18.9235097286749));
#50883=CARTESIAN_POINT('Ctrl Pts',(56.282639499884,30.5277214993771,18.9224849589668));
#50884=CARTESIAN_POINT('Ctrl Pts',(56.2890131970818,30.5223475426513,18.9219534941338));
#50885=CARTESIAN_POINT('Ctrl Pts',(56.3053395063284,30.5084060430735,18.9205806470208));
#50886=CARTESIAN_POINT('Ctrl Pts',(56.3152414125828,30.4997799940655,18.9197368799892));
#50887=CARTESIAN_POINT('Ctrl Pts',(56.3571811661686,30.4625094035105,18.9161144933386));
#50888=CARTESIAN_POINT('Ctrl Pts',(56.3883719288727,30.4329331428643,18.9132972883745));
#50889=CARTESIAN_POINT('Ctrl Pts',(56.469744892638,30.3506197720861,18.9056003616769));
#50890=CARTESIAN_POINT('Ctrl Pts',(56.5180328091014,30.2961089267274,18.9006491681735));
#50891=CARTESIAN_POINT('Ctrl Pts',(56.623998726839,30.1624224047797,18.888878393426));
#50892=CARTESIAN_POINT('Ctrl Pts',(56.6790438284208,30.0813920099518,18.8820144071344));
#50893=CARTESIAN_POINT('Ctrl Pts',(56.737621777617,29.9798342572689,18.8738978226494));
#50894=CARTESIAN_POINT('Ctrl Pts',(56.7470777350109,29.962872800663,18.8725578712145));
#50895=CARTESIAN_POINT('Ctrl Pts',(56.7619840039176,29.9351921859877,18.8703988597298));
#50896=CARTESIAN_POINT('Ctrl Pts',(56.7675876196233,29.9245572296108,18.8695758812791));
#50897=CARTESIAN_POINT('Ctrl Pts',(56.7943458862737,29.8726408353116,18.8655919107553));
#50898=CARTESIAN_POINT('Ctrl Pts',(56.8141542209255,29.8306770768205,18.862473742147));
#50899=CARTESIAN_POINT('Ctrl Pts',(56.8358816224618,29.780153988264,18.8588694745216));
#50900=CARTESIAN_POINT('Ctrl Pts',(56.8392293493898,29.7722285825898,18.8583083741708));
#50901=CARTESIAN_POINT('Ctrl Pts',(56.8446066222524,29.7592650835009,18.8573978576784));
#50902=CARTESIAN_POINT('Ctrl Pts',(56.8466670117456,29.7542400196845,18.8570466834973));
#50903=CARTESIAN_POINT('Ctrl Pts',(56.8503233490524,29.7452178133263,18.8564194208956));
#50904=CARTESIAN_POINT('Ctrl Pts',(56.8519269019202,29.7412238773746,18.8561428873038));
#50905=CARTESIAN_POINT('Ctrl Pts',(56.8554022931461,29.732486108511,18.8555403964567));
#50906=CARTESIAN_POINT('Ctrl Pts',(56.8572688685523,29.7277402832559,18.8552147526069));
#50907=CARTESIAN_POINT('Ctrl Pts',(56.8625307691064,29.7142096303184,18.8542907060947));
#50908=CARTESIAN_POINT('Ctrl Pts',(56.8658821618947,29.7054077034331,18.8536948431532));
#50909=CARTESIAN_POINT('Ctrl Pts',(56.8877957655498,29.646605916609,18.8497469092549));
#50910=CARTESIAN_POINT('Ctrl Pts',(56.904410385682,29.5958978490112,18.8464994719718));
#50911=CARTESIAN_POINT('Ctrl Pts',(56.9672952608692,29.3743061664164,18.8327347989551));
#50912=CARTESIAN_POINT('Ctrl Pts',(56.9927413634309,29.1983558426419,18.8228086119594));
#50913=CARTESIAN_POINT('Ctrl Pts',(56.9952531786524,28.9636582121487,18.8087497009117));
#50914=CARTESIAN_POINT('Ctrl Pts',(56.993367548543,28.9059741762281,18.8052366659452));
#50915=CARTESIAN_POINT('Ctrl Pts',(56.9878519494673,28.8335827366265,18.8007173255587));
#50916=CARTESIAN_POINT('Ctrl Pts',(56.9865519084127,28.8187223819696,18.7997837850739));
#50917=CARTESIAN_POINT('Ctrl Pts',(56.9842187287267,28.7951066312985,18.7982903704643));
#50918=CARTESIAN_POINT('Ctrl Pts',(56.9832939879066,28.7863409035592,18.7977338790707));
#50919=CARTESIAN_POINT('Ctrl Pts',(56.9814545716334,28.769947038771,18.7966889421048));
#50920=CARTESIAN_POINT('Ctrl Pts',(56.9805538615927,28.7623174742247,18.7962009419377));
#50921=CARTESIAN_POINT('Ctrl Pts',(56.9784419442129,28.7452744321718,18.7951069617425));
#50922=CARTESIAN_POINT('Ctrl Pts',(56.9772075871186,28.7358640617875,18.7945002672956));
#50923=CARTESIAN_POINT('Ctrl Pts',(56.9733679259799,28.7081281074441,18.7927040994539));
#50924=CARTESIAN_POINT('Ctrl Pts',(56.9705747103368,28.6898299726633,18.7915087767498));
#50925=CARTESIAN_POINT('Ctrl Pts',(56.9467229832438,28.5469396286167,18.7820906987389));
#50926=CARTESIAN_POINT('Ctrl Pts',(56.9141272656479,28.4245867032357,18.7734984083875));
#50927=CARTESIAN_POINT('Ctrl Pts',(56.8209758445084,28.1735056303051,18.7549115242551));
#50928=CARTESIAN_POINT('Ctrl Pts',(56.7577866594209,28.0464611547449,18.7449225827293));
#50929=CARTESIAN_POINT('Ctrl Pts',(56.6715104724981,27.9112217606078,18.7342548979639));
#50930=CARTESIAN_POINT('Ctrl Pts',(56.6611110832296,27.8954207381316,18.7330085065773));
#50931=CARTESIAN_POINT('Ctrl Pts',(56.646580868345,27.8740126946052,18.7313223563014));
#50932=CARTESIAN_POINT('Ctrl Pts',(56.6426435047852,27.8682764085016,18.7308708051146));
#50933=CARTESIAN_POINT('Ctrl Pts',(56.6363350020599,27.859187929455,18.7301559283263));
#50934=CARTESIAN_POINT('Ctrl Pts',(56.6339834313859,27.8558223188838,18.7298913196013));
#50935=CARTESIAN_POINT('Ctrl Pts',(56.6290834977863,27.8488553596692,18.7293438617016));
#50936=CARTESIAN_POINT('Ctrl Pts',(56.6265335648938,27.8452551847384,18.7290611324734));
#50937=CARTESIAN_POINT('Ctrl Pts',(56.6203515034614,27.836588020651,18.7283808212036));
#50938=CARTESIAN_POINT('Ctrl Pts',(56.6167074847994,27.8315294870879,18.7279840414686));
#50939=CARTESIAN_POINT('Ctrl Pts',(56.6039153994644,27.8139462473242,18.7266055126552));
#50940=CARTESIAN_POINT('Ctrl Pts',(56.5946447533087,27.8015108434554,18.7256317498743));
#50941=CARTESIAN_POINT('Ctrl Pts',(56.5371114815866,27.7261868642991,18.7197321273701));
#50942=CARTESIAN_POINT('Ctrl Pts',(56.4852750517037,27.6661062789453,18.7150193421612));
#50943=CARTESIAN_POINT('Ctrl Pts',(56.3814830028217,27.5593842549929,18.7062968685041));
#50944=CARTESIAN_POINT('Ctrl Pts',(56.3303943081412,27.512075170663,18.7022776433283));
#50945=CARTESIAN_POINT('Ctrl Pts',(56.1804514084427,27.3871344377957,18.690919920441));
#50946=CARTESIAN_POINT('Ctrl Pts',(56.0766023828346,27.3160397653366,18.6835217314814));
#50947=CARTESIAN_POINT('Ctrl Pts',(55.9529868977687,27.2475469319726,18.6747513305454));
#50948=CARTESIAN_POINT('Ctrl Pts',(55.9391162504912,27.2400748797364,18.6737680872499));
#50949=CARTESIAN_POINT('Ctrl Pts',(55.9164295509905,27.2281982264427,18.6721605653593));
#50950=CARTESIAN_POINT('Ctrl Pts',(55.9076666404438,27.2236931821994,18.671539807591));
#50951=CARTESIAN_POINT('Ctrl Pts',(55.8919821943532,27.2157761150218,18.6704288485784));
#50952=CARTESIAN_POINT('Ctrl Pts',(55.8850735128279,27.2123389636329,18.6699395332227));
#50953=CARTESIAN_POINT('Ctrl Pts',(55.8704396192563,27.2051640521082,18.6689030694874));
#50954=CARTESIAN_POINT('Ctrl Pts',(55.8627098989433,27.2014358957463,18.6683556015406));
#50955=CARTESIAN_POINT('Ctrl Pts',(55.8420838077113,27.1916511899194,18.6668945996668));
#50956=CARTESIAN_POINT('Ctrl Pts',(55.8291463843147,27.1856828242711,18.6659780687529));
#50957=CARTESIAN_POINT('Ctrl Pts',(55.7660912846575,27.1574091670254,18.6615095067478));
#50958=CARTESIAN_POINT('Ctrl Pts',(55.7151360724482,27.1370409904381,18.6578928442873));
#50959=CARTESIAN_POINT('Ctrl Pts',(55.4696618441733,27.0504738630547,18.640432294877));
#50960=CARTESIAN_POINT('Ctrl Pts',(55.2665651941625,27.0125004235771,18.6257111432123));
#50961=CARTESIAN_POINT('Ctrl Pts',(55.0300348456545,27.0052312618966,18.6097631508404));
#50962=CARTESIAN_POINT('Ctrl Pts',(54.9987746604324,27.005005472049,18.6076830294092));
#50963=CARTESIAN_POINT('Ctrl Pts',(54.9590951201889,27.005651647101,18.6050880841231));
#50964=CARTESIAN_POINT('Ctrl Pts',(54.9506708965019,27.0058422310436,18.6045397636911));
#50965=CARTESIAN_POINT('Ctrl Pts',(54.9373661608289,27.0062275915717,18.6036781548011));
#50966=CARTESIAN_POINT('Ctrl Pts',(54.9324848376813,27.0063869185538,18.6033629734354));
#50967=CARTESIAN_POINT('Ctrl Pts',(54.9232711550293,27.0067215332768,18.6027698765049));
#50968=CARTESIAN_POINT('Ctrl Pts',(54.9189388285235,27.0068930163214,18.6024917666173));
#50969=CARTESIAN_POINT('Ctrl Pts',(54.908853817549,27.0073251405435,18.6018461095837));
#50970=CARTESIAN_POINT('Ctrl Pts',(54.9031016690316,27.00759656758,18.6014791626053));
#50971=CARTESIAN_POINT('Ctrl Pts',(54.8846337437901,27.0085481829668,18.6003050273902));
#50972=CARTESIAN_POINT('Ctrl Pts',(54.8719229760259,27.0093252379516,18.5995029910424));
#50973=CARTESIAN_POINT('Ctrl Pts',(54.8418332689627,27.0114541332443,18.5976169243552));
#50974=CARTESIAN_POINT('Ctrl Pts',(54.8244626414741,27.0129121664063,18.5965380492067));
#50975=CARTESIAN_POINT('Ctrl Pts',(54.7611814264441,27.0190601094541,18.5926367822408));
#50976=CARTESIAN_POINT('Ctrl Pts',(54.7154156334403,27.0251153281871,18.589871127379));
#50977=CARTESIAN_POINT('Ctrl Pts',(54.5139592444471,27.0589194749927,18.5777870087624));
#50978=CARTESIAN_POINT('Ctrl Pts',(54.3616858640178,27.1035330096151,18.5688464610483));
#50979=CARTESIAN_POINT('Ctrl Pts',(54.1605800381065,27.1894559554453,18.5557719600474));
#50980=CARTESIAN_POINT('Ctrl Pts',(54.1060032905532,27.2157734372108,18.5520894513809));
#50981=CARTESIAN_POINT('Ctrl Pts',(54.0393784563446,27.2517256071935,18.5473783122144));
#50982=CARTESIAN_POINT('Ctrl Pts',(54.0261279657469,27.2590719877724,18.5464303739847));
#50983=CARTESIAN_POINT('Ctrl Pts',(54.0052565046965,27.2709564546964,18.5449191106362));
#50984=CARTESIAN_POINT('Ctrl Pts',(53.9975797343163,27.2753957526812,18.5443593094529));
#50985=CARTESIAN_POINT('Ctrl Pts',(53.9834439693576,27.2836964066747,18.5433210740231));
#50986=CARTESIAN_POINT('Ctrl Pts',(53.9769767070138,27.2875434232136,18.5428431628758));
#50987=CARTESIAN_POINT('Ctrl Pts',(53.9632465964651,27.2958162428832,18.5418222584892));
#50988=CARTESIAN_POINT('Ctrl Pts',(53.955989995881,27.3002520759287,18.5412789074299));
#50989=CARTESIAN_POINT('Ctrl Pts',(53.9406051945293,27.3097922235056,18.5401187577825));
#50990=CARTESIAN_POINT('Ctrl Pts',(53.9324850456039,27.3149090533706,18.539501510039));
#50991=CARTESIAN_POINT('Ctrl Pts',(53.9118109695318,27.3281460202252,18.5379172119835));
#50992=CARTESIAN_POINT('Ctrl Pts',(53.8993110106587,27.3363489475164,18.5369471371417));
#50993=CARTESIAN_POINT('Ctrl Pts',(53.8164262929565,27.3920839265698,18.530431822737));
#50994=CARTESIAN_POINT('Ctrl Pts',(53.7490557220949,27.4439229079121,18.524726697754));
#50995=CARTESIAN_POINT('Ctrl Pts',(53.596083468286,27.5779984125844,18.5107798769979));
#50996=CARTESIAN_POINT('Ctrl Pts',(53.5141063917076,27.6638907836862,18.5024455661607));
#50997=CARTESIAN_POINT('Ctrl Pts',(53.3954368462925,27.8127463847093,18.489285725354));
#50998=CARTESIAN_POINT('Ctrl Pts',(53.3536957451996,27.871337667361,18.4843836923746));
#50999=CARTESIAN_POINT('Ctrl Pts',(53.3096080021216,27.9408910531322,18.4789765428029));
#51000=CARTESIAN_POINT('Ctrl Pts',(53.30408006343,27.9497655271991,18.4782940068487));
#51001=CARTESIAN_POINT('Ctrl Pts',(53.2958104616855,27.9632769959848,18.4772664404504));
#51002=CARTESIAN_POINT('Ctrl Pts',(53.2930174853924,27.9678821452855,18.4769182342516));
#51003=CARTESIAN_POINT('Ctrl Pts',(53.2880274643022,27.9761855138605,18.476294104139));
#51004=CARTESIAN_POINT('Ctrl Pts',(53.2858237099634,27.9798795596938,18.4760177549317));
#51005=CARTESIAN_POINT('Ctrl Pts',(53.2810145613209,27.9880004902066,18.4754131201546));
#51006=CARTESIAN_POINT('Ctrl Pts',(53.2784143139336,27.9924303134935,18.4750851647352));
#51007=CARTESIAN_POINT('Ctrl Pts',(53.2710079325121,28.0051603229719,18.4741478983053));
#51008=CARTESIAN_POINT('Ctrl Pts',(53.2662444330619,28.0134853294479,18.473541242628));
#51009=CARTESIAN_POINT('Ctrl Pts',(53.2332995242657,28.0720377531291,18.4693159642909));
#51010=CARTESIAN_POINT('Ctrl Pts',(53.2072420711482,28.1234357631103,18.4658195759727));
#51011=CARTESIAN_POINT('Ctrl Pts',(53.0998465438268,28.3601652129511,18.4503351346781));
#51012=CARTESIAN_POINT('Ctrl Pts',(53.0447729023594,28.5560779080205,18.4390497704395));
#51013=CARTESIAN_POINT('Ctrl Pts',(53.0160515391722,28.7900292905039,18.4246625795518));
#51014=CARTESIAN_POINT('Ctrl Pts',(53.0128193889092,28.8232170409666,18.4226048395948));
#51015=CARTESIAN_POINT('Ctrl Pts',(53.0095320465334,28.868785031421,18.4197496550198));
#51016=CARTESIAN_POINT('Ctrl Pts',(53.0087579331777,28.8811090322041,18.4189744966872));
#51017=CARTESIAN_POINT('Ctrl Pts',(53.0077056049858,28.900779816542,18.4177321949085));
#51018=CARTESIAN_POINT('Ctrl Pts',(53.0073534894768,28.9081224566283,18.4172673536105));
#51019=CARTESIAN_POINT('Ctrl Pts',(53.0067283586573,28.9228605647168,18.4163320075453));
#51020=CARTESIAN_POINT('Ctrl Pts',(53.0064558966353,28.9302559379579,18.4158614931825));
#51021=CARTESIAN_POINT('Ctrl Pts',(53.0059888017183,28.9451929200034,18.4149087288716));
#51022=CARTESIAN_POINT('Ctrl Pts',(53.0057957876512,28.9527344546963,18.4144264364003));
#51023=CARTESIAN_POINT('Ctrl Pts',(53.0053782267271,28.973698648778,18.4130821811506));
#51024=CARTESIAN_POINT('Ctrl Pts',(53.0052463980734,28.9871225062247,18.4122173614862));
#51025=CARTESIAN_POINT('Ctrl Pts',(53.0052500748225,29.0005463555814,18.4113483399464));
#51026=CARTESIAN_POINT('Ctrl Pts',(53.0052500745292,29.0005452837287,18.4113484093351));
#51027=CARTESIAN_POINT('Ctrl Pts',(53.0052590846391,29.0335059519054,18.4092146306787));
#51028=CARTESIAN_POINT('Ctrl Pts',(53.0060850378228,29.0664600029808,18.4070558337636));
#51029=CARTESIAN_POINT('Ctrl Pts',(53.012837243978,29.201825273718,18.398079494748));
#51030=CARTESIAN_POINT('Ctrl Pts',(53.0258412931628,29.3037130880922,18.3910559369579));
#51031=CARTESIAN_POINT('Ctrl Pts',(53.046641082446,29.4042480853829,18.3839253224822));
#51032=CARTESIAN_POINT('Ctrl Pts',(53.0466640355231,29.404358980617,18.3839174568178));
#51033=CARTESIAN_POINT('Ctrl Pts',(53.0466869980087,29.4044698737256,18.3839095910714));
#51034=CARTESIAN_POINT('Ctrl Pts',(53.0466869962288,29.4044698651299,18.2270410618393));
#51035=CARTESIAN_POINT('Ctrl Pts',(53.0407025852386,29.3755692502392,18.2290306251703));
#51036=CARTESIAN_POINT('Ctrl Pts',(53.0353592981748,29.3465344503275,18.2309971371075));
#51037=CARTESIAN_POINT('Ctrl Pts',(53.0291327451794,29.3078996130939,18.2335620838893));
#51038=CARTESIAN_POINT('Ctrl Pts',(53.0276722830995,29.2984012296626,18.2341885508835));
#51039=CARTESIAN_POINT('Ctrl Pts',(53.0255360147488,29.2838061971304,18.2351444623848));
#51040=CARTESIAN_POINT('Ctrl Pts',(53.0248111973253,29.2787170281959,18.2354765322629));
#51041=CARTESIAN_POINT('Ctrl Pts',(53.023516034948,29.2693644358614,18.2360844291963));
#51042=CARTESIAN_POINT('Ctrl Pts',(53.0229398077778,29.2651019811977,18.2363605716051));
#51043=CARTESIAN_POINT('Ctrl Pts',(53.0216737041719,29.2555026155207,18.2369804420519));
#51044=CARTESIAN_POINT('Ctrl Pts',(53.0209916345264,29.2501647663337,18.2373237319712));
#51045=CARTESIAN_POINT('Ctrl Pts',(53.0190506529953,29.2344698249427,18.2383291803807));
#51046=CARTESIAN_POINT('Ctrl Pts',(53.0178513637173,29.2241053523241,18.2389881232356));
#51047=CARTESIAN_POINT('Ctrl Pts',(53.0091370429692,29.1432431205428,18.2440932978436));
#51048=CARTESIAN_POINT('Ctrl Pts',(53.0053031011992,29.0723912545005,18.2483552517889));
#51049=CARTESIAN_POINT('Ctrl Pts',(53.0051301413002,28.83900784537,18.2621308574038));
#51050=CARTESIAN_POINT('Ctrl Pts',(53.0248583520516,28.6771351772837,18.2713171826088));
#51051=CARTESIAN_POINT('Ctrl Pts',(53.0768676504811,28.4676071608181,18.2842867231159));
#51052=CARTESIAN_POINT('Ctrl Pts',(53.0918103494087,28.4163120081138,18.2875461999437));
#51053=CARTESIAN_POINT('Ctrl Pts',(53.1134714360907,28.3517299360444,18.2917886189302));
#51054=CARTESIAN_POINT('Ctrl Pts',(53.1183049004166,28.3378311149963,18.2927099377624));
#51055=CARTESIAN_POINT('Ctrl Pts',(53.1262347653306,28.3158166694844,18.2941830269197));
#51056=CARTESIAN_POINT('Ctrl Pts',(53.1292312233625,28.3076654241398,18.2947314997355));
#51057=CARTESIAN_POINT('Ctrl Pts',(53.1347137293017,28.2930468940223,18.2957207170945));
#51058=CARTESIAN_POINT('Ctrl Pts',(53.1371804383847,28.2865724671707,18.2961608137056));
#51059=CARTESIAN_POINT('Ctrl Pts',(53.1430422249385,28.2714245827083,18.2971952024989));
#51060=CARTESIAN_POINT('Ctrl Pts',(53.1464643992282,28.2627618506311,18.2977903904541));
#51061=CARTESIAN_POINT('Ctrl Pts',(53.1565471249258,28.2377529158072,18.2995194233414));
#51062=CARTESIAN_POINT('Ctrl Pts',(53.1633639949704,28.2214710846806,18.3006584761158));
#51063=CARTESIAN_POINT('Ctrl Pts',(53.2287448309737,28.0709509119039,18.3113165564617));
#51064=CARTESIAN_POINT('Ctrl Pts',(53.3016987081573,27.9434802639279,18.321345427733));
#51065=CARTESIAN_POINT('Ctrl Pts',(53.4125863212769,27.7913235569712,18.3344551193548));
#51066=CARTESIAN_POINT('Ctrl Pts',(53.4383076235699,27.7582681983959,18.3373773661658));
#51067=CARTESIAN_POINT('Ctrl Pts',(53.524402085484,27.6545354410124,18.3467513998617));
#51068=CARTESIAN_POINT('Ctrl Pts',(53.5886862966132,27.5872502709677,18.3531554281931));
#51069=CARTESIAN_POINT('Ctrl Pts',(53.6652994241423,27.5175307795837,18.3599592780833));
#51070=CARTESIAN_POINT('Ctrl Pts',(53.6732206427343,27.5104372568889,18.3606535856835));
#51071=CARTESIAN_POINT('Ctrl Pts',(53.6852677261663,27.4998213344304,18.361695294382));
#51072=CARTESIAN_POINT('Ctrl Pts',(53.6893517111335,27.4962520008137,18.362045999851));
#51073=CARTESIAN_POINT('Ctrl Pts',(53.6967020578062,27.4898806154345,18.3626727650686));
#51074=CARTESIAN_POINT('Ctrl Pts',(53.6999629625552,27.4870724458424,18.3629492668558));
#51075=CARTESIAN_POINT('Ctrl Pts',(53.7071123254989,27.4809558638196,18.3635520843739));
#51076=CARTESIAN_POINT('Ctrl Pts',(53.7110044002916,27.4776518230473,18.3638780841089));
#51077=CARTESIAN_POINT('Ctrl Pts',(53.7221326653525,27.4682781458621,18.3648041619869));
#51078=CARTESIAN_POINT('Ctrl Pts',(53.7293994518223,27.4622448118531,18.3654016827985));
#51079=CARTESIAN_POINT('Ctrl Pts',(53.7784653997161,27.4220925201614,18.3693902016324));
#51080=CARTESIAN_POINT('Ctrl Pts',(53.8215952317846,27.3896267105692,18.3726740802071));
#51081=CARTESIAN_POINT('Ctrl Pts',(54.0175782992013,27.2541976547176,18.3869028898807));
#51082=CARTESIAN_POINT('Ctrl Pts',(54.1829466849133,27.1709538031784,18.3972156162004));
#51083=CARTESIAN_POINT('Ctrl Pts',(54.4056218745212,27.0951806710256,18.4113712560602));
#51084=CARTESIAN_POINT('Ctrl Pts',(54.4544497524321,27.0806260660786,18.4144837913227));
#51085=CARTESIAN_POINT('Ctrl Pts',(54.5178054311023,27.0643539312551,18.4185589773504));
#51086=CARTESIAN_POINT('Ctrl Pts',(54.5318711944087,27.0609041514846,18.4194659462707));
#51087=CARTESIAN_POINT('Ctrl Pts',(54.5543798700972,27.0556428312966,18.4209213939677));
#51088=CARTESIAN_POINT('Ctrl Pts',(54.5627993107701,27.0537323788265,18.4214667125926));
#51089=CARTESIAN_POINT('Ctrl Pts',(54.5780045787958,27.0503857986823,18.4224532793849));
#51090=CARTESIAN_POINT('Ctrl Pts',(54.5847860335262,27.0489302858269,18.4228939026819));
#51091=CARTESIAN_POINT('Ctrl Pts',(54.6007633124383,27.045588131553,18.4239335472873));
#51092=CARTESIAN_POINT('Ctrl Pts',(54.6099650741759,27.0437309909132,18.4245334937821));
#51093=CARTESIAN_POINT('Ctrl Pts',(54.6368522229993,27.0385017474922,18.4262901436668));
#51094=CARTESIAN_POINT('Ctrl Pts',(54.6545701980414,27.0353041152861,18.42745231439));
#51095=CARTESIAN_POINT('Ctrl Pts',(54.6947645313817,27.028610590612,18.4300998358604));
#51096=CARTESIAN_POINT('Ctrl Pts',(54.7172619698113,27.0252584899838,18.4315894942432));
#51097=CARTESIAN_POINT('Ctrl Pts',(54.7912622744407,27.0155229480971,18.4365159578859));
#51098=CARTESIAN_POINT('Ctrl Pts',(54.8429540935004,27.0107648601882,18.4399999703326));
#51099=CARTESIAN_POINT('Ctrl Pts',(55.0223818338865,27.0012861503549,18.4522293164712));
#51100=CARTESIAN_POINT('Ctrl Pts',(55.1503411432454,27.0068239266349,18.4612110385858));
#51101=CARTESIAN_POINT('Ctrl Pts',(55.3544815594113,27.0354361229378,18.4754925726203));
#51102=CARTESIAN_POINT('Ctrl Pts',(55.4313875573193,27.0508781475049,18.4808543452591));
#51103=CARTESIAN_POINT('Ctrl Pts',(55.5173624180912,27.073481311968,18.486692022039));
#51104=CARTESIAN_POINT('Ctrl Pts',(55.5275107746108,27.0762353259464,18.4873785336689));
#51105=CARTESIAN_POINT('Ctrl Pts',(55.5428360415741,27.0805246184597,18.4884108788083));
#51106=CARTESIAN_POINT('Ctrl Pts',(55.5480290896857,27.0820008271946,18.4887599312577));
#51107=CARTESIAN_POINT('Ctrl Pts',(55.5573494601583,27.0846912391177,18.4893849504414));
#51108=CARTESIAN_POINT('Ctrl Pts',(55.5614788867583,27.0858977218983,18.489661348146));
#51109=CARTESIAN_POINT('Ctrl Pts',(55.5705199015236,27.0885709853777,18.490265353466));
#51110=CARTESIAN_POINT('Ctrl Pts',(55.5754297438452,27.0900433388983,18.4905926357886));
#51111=CARTESIAN_POINT('Ctrl Pts',(55.5894618585345,27.0943102814614,18.4915260460102));
#51112=CARTESIAN_POINT('Ctrl Pts',(55.598569978415,27.0971514575518,18.4921295525466));
#51113=CARTESIAN_POINT('Ctrl Pts',(55.6612785113328,27.1172074981358,18.4962705577758));
#51114=CARTESIAN_POINT('Ctrl Pts',(55.7141549468452,27.1366211181431,18.4996913224679));
#51115=CARTESIAN_POINT('Ctrl Pts',(55.8546172828006,27.1950515555501,18.5087618731247));
#51116=CARTESIAN_POINT('Ctrl Pts',(55.9403281595792,27.238184321841,18.5142833395687));
#51117=CARTESIAN_POINT('Ctrl Pts',(56.135410191401,27.3546637981494,18.5274931990627));
#51118=CARTESIAN_POINT('Ctrl Pts',(56.2412648990047,27.432982955264,18.5352098262511));
#51119=CARTESIAN_POINT('Ctrl Pts',(56.3503251252596,27.5317024327801,18.5443390757931));
#51120=CARTESIAN_POINT('Ctrl Pts',(56.361877498168,27.5424111184145,18.5453221375177));
#51121=CARTESIAN_POINT('Ctrl Pts',(56.3804471781398,27.5600381194265,18.5469294208817));
#51122=CARTESIAN_POINT('Ctrl Pts',(56.3875423191769,27.5668737194291,18.5475501234432));
#51123=CARTESIAN_POINT('Ctrl Pts',(56.4001036166386,27.5791562479326,18.5486610206546));
#51124=CARTESIAN_POINT('Ctrl Pts',(56.4055893890705,27.5845828983192,18.5491503297871));
#51125=CARTESIAN_POINT('Ctrl Pts',(56.4171097702815,27.5961121419487,18.5501868189951));
#51126=CARTESIAN_POINT('Ctrl Pts',(56.4231367428032,27.6022221111624,18.5507343188723));
#51127=CARTESIAN_POINT('Ctrl Pts',(56.4390654047547,27.6185799397475,18.5521954977465));
#51128=CARTESIAN_POINT('Ctrl Pts',(56.4488968846266,27.6288951818412,18.5531121750174));
#51129=CARTESIAN_POINT('Ctrl Pts',(56.4960551539321,27.6794475333306,18.5575826675015));
#51130=CARTESIAN_POINT('Ctrl Pts',(56.5318179060098,27.7211048590726,18.5612011819019));
#51131=CARTESIAN_POINT('Ctrl Pts',(56.6933115344229,27.9257214335051,18.578687386208));
#51132=CARTESIAN_POINT('Ctrl Pts',(56.7950169483812,28.1059811870624,18.5934357600824));
#51133=CARTESIAN_POINT('Ctrl Pts',(56.8782376999688,28.3275362617536,18.6093807727886));
#51134=CARTESIAN_POINT('Ctrl Pts',(56.8884400696301,28.3567436821395,18.611438929806));
#51135=CARTESIAN_POINT('Ctrl Pts',(56.9005429526428,28.3941662546026,18.6140105737047));
#51136=CARTESIAN_POINT('Ctrl Pts',(56.9030759141265,28.4021704984295,18.61455685502));
#51137=CARTESIAN_POINT('Ctrl Pts',(56.9070003598381,28.4148496130285,18.6154159929562));
#51138=CARTESIAN_POINT('Ctrl Pts',(56.9084253280006,28.4195138963993,18.6157307247132));
#51139=CARTESIAN_POINT('Ctrl Pts',(56.9110852607463,28.428336198533,18.6163234729626));
#51140=CARTESIAN_POINT('Ctrl Pts',(56.9123237569694,28.4324929739375,18.6166016804251));
#51141=CARTESIAN_POINT('Ctrl Pts',(56.9151785373924,28.4421899633094,18.6172482292355));
#51142=CARTESIAN_POINT('Ctrl Pts',(56.9167843472728,28.4477331848085,18.617615965024));
#51143=CARTESIAN_POINT('Ctrl Pts',(56.9218750043153,28.4655957182406,18.6187952154351));
#51144=CARTESIAN_POINT('Ctrl Pts',(56.9252653994951,28.4779419284413,18.6196015150863));
#51145=CARTESIAN_POINT('Ctrl Pts',(56.9532999380579,28.5840196062147,18.6264609482622));
#51146=CARTESIAN_POINT('Ctrl Pts',(56.9712048742252,28.6794120716764,18.6321776140071));
#51147=CARTESIAN_POINT('Ctrl Pts',(57.0016805624183,28.9487680762258,18.6479868402708));
#51148=CARTESIAN_POINT('Ctrl Pts',(56.9985166138154,29.1235952915863,18.6579373984282));
#51149=CARTESIAN_POINT('Ctrl Pts',(56.9694073378136,29.3177337735308,18.6700557836486));
#51150=CARTESIAN_POINT('Ctrl Pts',(56.9657508729171,29.3396225225335,18.6714363419178));
#51151=CARTESIAN_POINT('Ctrl Pts',(56.9599009750213,29.3713726336984,18.673461560028));
#51152=CARTESIAN_POINT('Ctrl Pts',(56.9579965327777,29.3812860299045,18.6740971303477));
#51153=CARTESIAN_POINT('Ctrl Pts',(56.9544928249464,29.3988054195163,18.6752262498478));
#51154=CARTESIAN_POINT('Ctrl Pts',(56.9529241865256,29.4064173769836,18.6757188209486));
#51155=CARTESIAN_POINT('Ctrl Pts',(56.9495720550315,29.4222162593013,18.6767453804029));
#51156=CARTESIAN_POINT('Ctrl Pts',(56.9477813846095,29.4304014888916,18.6772795880303));
#51157=CARTESIAN_POINT('Ctrl Pts',(56.9430097399748,29.4515730752197,18.6786675826109));
#51158=CARTESIAN_POINT('Ctrl Pts',(56.9399501624801,29.4645411120642,18.6795238557807));
#51159=CARTESIAN_POINT('Ctrl Pts',(56.926036172655,29.5209795520965,18.6832777698458));
#51160=CARTESIAN_POINT('Ctrl Pts',(56.9138495374494,29.5641049994275,18.6862175711223));
#51161=CARTESIAN_POINT('Ctrl Pts',(56.8521044768945,29.7574685807091,18.699734710844));
#51162=CARTESIAN_POINT('Ctrl Pts',(56.7862381142656,29.901880486207,18.7108250111487));
#51163=CARTESIAN_POINT('Ctrl Pts',(56.6592135092919,30.110617152795,18.7277915162128));
#51164=CARTESIAN_POINT('Ctrl Pts',(56.6096637734936,30.181289951954,18.7337132684562));
#51165=CARTESIAN_POINT('Ctrl Pts',(56.5490498850133,30.2568152501587,18.7400737030489));
#51166=CARTESIAN_POINT('Ctrl Pts',(56.5423433138017,30.2650364553803,18.7407664599797));
#51167=CARTESIAN_POINT('Ctrl Pts',(56.5321125695426,30.2773754344863,18.7418063069928));
#51168=CARTESIAN_POINT('Ctrl Pts',(56.5286368099669,30.2815328443955,18.7421566843741));
#51169=CARTESIAN_POINT('Ctrl Pts',(56.5223706122116,30.2889661742766,18.7427831021179));
#51170=CARTESIAN_POINT('Ctrl Pts',(56.5195864870218,30.2922472630651,18.7430595823234));
#51171=CARTESIAN_POINT('Ctrl Pts',(56.5134733665641,30.2994044929193,18.7436626314289));
#51172=CARTESIAN_POINT('Ctrl Pts',(56.510140093808,30.3032768570002,18.7439888825069));
#51173=CARTESIAN_POINT('Ctrl Pts',(56.5005906737215,30.31428488104,18.7449163955366));
#51174=CARTESIAN_POINT('Ctrl Pts',(56.4943384765876,30.3213892856868,18.7455150876824));
#51175=CARTESIAN_POINT('Ctrl Pts',(56.4518056362731,30.3690316003099,18.7495326948037));
#51176=CARTESIAN_POINT('Ctrl Pts',(56.4139267852265,30.40811907661,18.752842689817));
#51177=CARTESIAN_POINT('Ctrl Pts',(56.2367997439828,30.5765321205081,18.7674361109887));
#51178=CARTESIAN_POINT('Ctrl Pts',(56.0811087522357,30.6871097348985,18.7780543677325));
#51179=CARTESIAN_POINT('Ctrl Pts',(55.871404146068,30.7949312248483,18.7922999934147));
#51180=CARTESIAN_POINT('Ctrl Pts',(55.8299853814423,30.8144550322667,18.7951051890248));
#51181=CARTESIAN_POINT('Ctrl Pts',(55.7751261097204,30.8380428301046,18.7988282792918));
#51182=CARTESIAN_POINT('Ctrl Pts',(55.7622611121909,30.8434152848954,18.7997018705093));
#51183=CARTESIAN_POINT('Ctrl Pts',(55.7414502152256,30.8518508680827,18.8011162884634));
#51184=CARTESIAN_POINT('Ctrl Pts',(55.7335390250437,30.8549988017231,18.8016542651308));
#51185=CARTESIAN_POINT('Ctrl Pts',(55.7184060421686,30.8609084070653,18.8026840016023));
#51186=CARTESIAN_POINT('Ctrl Pts',(55.7111878566276,30.8636789344608,18.8031754550314));
#51187=CARTESIAN_POINT('Ctrl Pts',(55.6946172608157,30.8699288745247,18.8043044129638));
#51188=CARTESIAN_POINT('Ctrl Pts',(55.6852545432267,30.8733801909505,18.8049428351693));
#51189=CARTESIAN_POINT('Ctrl Pts',(55.6561235808694,30.8838709459333,18.8069310939632));
#51190=CARTESIAN_POINT('Ctrl Pts',(55.6362703897061,30.8906686198404,18.8082888191228));
#51191=CARTESIAN_POINT('Ctrl Pts',(55.5394806260597,30.9221120274313,18.8149233646866));
#51192=CARTESIAN_POINT('Ctrl Pts',(55.4612112935793,30.9423787615012,18.8203392730816));
#51193=CARTESIAN_POINT('Ctrl Pts',(55.2493265995765,30.9837133401762,18.8351085284237));
#51194=CARTESIAN_POINT('Ctrl Pts',(55.11444184238,30.9960415261751,18.8446422269414));
#51195=CARTESIAN_POINT('Ctrl Pts',(54.9668253165249,30.9945134605601,18.8547978023335));
#51196=CARTESIAN_POINT('Ctrl Pts',(54.9542996614176,30.9942657778632,18.8556570728379));
#51197=CARTESIAN_POINT('Ctrl Pts',(54.8926274306618,30.992464913638,18.8598734482139));
#51198=CARTESIAN_POINT('Ctrl Pts',(54.8435430683146,30.9892127617237,18.8631845260159));
#51199=CARTESIAN_POINT('Ctrl Pts',(54.7859086741132,30.9832471490268,18.8669830978606));
#51200=CARTESIAN_POINT('Ctrl Pts',(54.777198246606,30.9822875006682,18.8675547615788));
#51201=CARTESIAN_POINT('Ctrl Pts',(54.7630520033242,30.980634552783,18.8684789300756));
#51202=CARTESIAN_POINT('Ctrl Pts',(54.7576123326757,30.9799762133069,18.8688332792628));
#51203=CARTESIAN_POINT('Ctrl Pts',(54.7479017542589,30.9787603662588,18.8694639328039));
#51204=CARTESIAN_POINT('Ctrl Pts',(54.7436298833345,30.9782114338513,18.8697407035152));
#51205=CARTESIAN_POINT('Ctrl Pts',(54.7343407248548,30.9769871875198,18.8703410810926));
#51206=CARTESIAN_POINT('Ctrl Pts',(54.7293242250918,30.976306609899,18.870664391633));
#51207=CARTESIAN_POINT('Ctrl Pts',(54.715154561992,30.9743292782511,18.8715751654403));
#51208=CARTESIAN_POINT('Ctrl Pts',(54.7060076033033,30.9729879627099,18.8721602026378));
#51209=CARTESIAN_POINT('Ctrl Pts',(54.6479214046531,30.9640572388422,18.8758588437141));
#51210=CARTESIAN_POINT('Ctrl Pts',(54.5992653542875,30.9547104182692,18.8788824095813));
#51211=CARTESIAN_POINT('Ctrl Pts',(54.4112975053044,30.9112865687573,18.8904459816157));
#51212=CARTESIAN_POINT('Ctrl Pts',(54.2754714375952,30.8640415369295,18.8985754914798));
#51213=CARTESIAN_POINT('Ctrl Pts',(54.0628381808221,30.7632920782961,18.9124078370509));
#51214=CARTESIAN_POINT('Ctrl Pts',(53.9826262499427,30.7182603839796,18.9179098226958));
#51215=CARTESIAN_POINT('Ctrl Pts',(53.8929839932673,30.6594512359068,18.9245670447293));
#51216=CARTESIAN_POINT('Ctrl Pts',(53.8802565059526,30.6508898602387,18.925524723185));
#51217=CARTESIAN_POINT('Ctrl Pts',(53.8596209789639,30.6366605873085,18.9270986694933));
#51218=CARTESIAN_POINT('Ctrl Pts',(53.8516532853187,30.6310800125027,18.9277116591918));
#51219=CARTESIAN_POINT('Ctrl Pts',(53.8375988335926,30.6210822453082,18.9288024728939));
#51220=CARTESIAN_POINT('Ctrl Pts',(53.8314955973177,30.6166884598205,18.9292793991139));
#51221=CARTESIAN_POINT('Ctrl Pts',(53.8251649307816,30.6120763692274,18.9297775171614));
#51222=CARTESIAN_POINT('Ctrl Pts',(53.8249124851021,30.6118923637817,18.9297973861214));
#51223=CARTESIAN_POINT('Ctrl Pts',(53.8244569553259,30.6115601682289,18.9298332492671));
#51224=CARTESIAN_POINT('Ctrl Pts',(53.8242538559287,30.6114119989639,18.9298492426515));
#51225=CARTESIAN_POINT('Ctrl Pts',(53.8238852785896,30.6111430000358,18.9298782735545));
#51226=CARTESIAN_POINT('Ctrl Pts',(53.823719791243,30.6110221832642,18.9298913105751));
#51227=CARTESIAN_POINT('Ctrl Pts',(53.8234181170251,30.6108018697536,18.9299150808074));
#51228=CARTESIAN_POINT('Ctrl Pts',(53.8232819241786,30.6107023812554,18.9299258136994));
#51229=CARTESIAN_POINT('Ctrl Pts',(53.8230327537094,30.6105203144457,18.9299454530118));
#51230=CARTESIAN_POINT('Ctrl Pts',(53.8229197721184,30.6104377414894,18.9299543592271));
#51231=CARTESIAN_POINT('Ctrl Pts',(53.822712459295,30.6102861927797,18.9299707035706));
#51232=CARTESIAN_POINT('Ctrl Pts',(53.8226181254073,30.6102172206062,18.9299781415617));
#51233=CARTESIAN_POINT('Ctrl Pts',(53.8224446113756,30.610090332511,18.9299918241777));
#51234=CARTESIAN_POINT('Ctrl Pts',(53.8223654294075,30.6100324190119,18.9299980687106));
#51235=CARTESIAN_POINT('Ctrl Pts',(53.8221455068049,30.609871543251,18.9300154140449));
#51236=CARTESIAN_POINT('Ctrl Pts',(53.8220047753914,30.6097685683689,18.9300265153345));
#51237=CARTESIAN_POINT('Ctrl Pts',(53.821728154465,30.6095661057823,18.9300483394678));
#51238=CARTESIAN_POINT('Ctrl Pts',(53.8215922640638,30.6094666193337,18.9300590622619));
#51239=CARTESIAN_POINT('Ctrl Pts',(53.8213249348264,30.6092708534563,18.9300801598534));
#51240=CARTESIAN_POINT('Ctrl Pts',(53.8211934951526,30.6091745751084,18.9300905346105));
#51241=CARTESIAN_POINT('Ctrl Pts',(53.8209347144008,30.6089849718751,18.9301109636756));
#51242=CARTESIAN_POINT('Ctrl Pts',(53.8208073726633,30.6088916480173,18.9301210179408));
#51243=CARTESIAN_POINT('Ctrl Pts',(53.8205564681672,30.6087077239803,18.9301408309787));
#51244=CARTESIAN_POINT('Ctrl Pts',(53.8204329046768,30.6086171246157,18.9301505897242));
#51245=CARTESIAN_POINT('Ctrl Pts',(53.8201892656727,30.6084384401783,18.9301698344558));
#51246=CARTESIAN_POINT('Ctrl Pts',(53.820069189592,30.608350355901,18.9301793204105));
#51247=CARTESIAN_POINT('Ctrl Pts',(53.8198322599161,30.6081765104537,18.93019804031));
#51248=CARTESIAN_POINT('Ctrl Pts',(53.8197154058806,30.6080907500493,18.9302072742212));
#51249=CARTESIAN_POINT('Ctrl Pts',(53.819484677583,30.6079213774302,18.9302255090119));
#51250=CARTESIAN_POINT('Ctrl Pts',(53.8193708028546,30.6078377658539,18.9302345098665));
#51251=CARTESIAN_POINT('Ctrl Pts',(53.8191458103451,30.6076725301765,18.930252295975));
#51252=CARTESIAN_POINT('Ctrl Pts',(53.8190346921326,30.6075909066437,18.9302610812073));
#51253=CARTESIAN_POINT('Ctrl Pts',(53.8114118517275,30.601990219173,18.9308638350272));
#51254=CARTESIAN_POINT('Ctrl Pts',(53.8039390051373,30.5964186607103,18.9314598277423));
#51255=CARTESIAN_POINT('Ctrl Pts',(53.7883177230642,30.5846005913636,18.9327165883387));
#51256=CARTESIAN_POINT('Ctrl Pts',(53.780177935919,30.5783431502277,18.9333777721958));
#51257=CARTESIAN_POINT('Ctrl Pts',(53.7590295969497,30.5618241059551,18.935112414138));
#51258=CARTESIAN_POINT('Ctrl Pts',(53.7461001669936,30.5514629421171,18.9361897563826));
#51259=CARTESIAN_POINT('Ctrl Pts',(53.7078061444124,30.5199841641661,18.9394320252084));
#51260=CARTESIAN_POINT('Ctrl Pts',(53.6828360300003,30.4983977071286,18.9416151922173));
#51261=CARTESIAN_POINT('Ctrl Pts',(53.5441652558794,30.3723724950155,18.9541408431235));
#51262=CARTESIAN_POINT('Ctrl Pts',(53.4423683443152,30.2556400389244,18.9649756077121));
#51263=CARTESIAN_POINT('Ctrl Pts',(53.307567361331,30.0591266894262,18.9815128558532));
#51264=CARTESIAN_POINT('Ctrl Pts',(53.2644846681067,29.9869485312645,18.9872739244996));
#51265=CARTESIAN_POINT('Ctrl Pts',(53.2212344196793,29.9028469725585,18.9934850344956));
#51266=CARTESIAN_POINT('Ctrl Pts',(53.2164675859309,29.8933934101298,18.9941763114672));
#51267=CARTESIAN_POINT('Ctrl Pts',(53.209377067077,29.8790485690898,18.9952143813226));
#51268=CARTESIAN_POINT('Ctrl Pts',(53.2069977482108,29.8741852214916,18.9955644452487));
#51269=CARTESIAN_POINT('Ctrl Pts',(53.2027630392138,29.8654394166503,18.9961905314394));
#51270=CARTESIAN_POINT('Ctrl Pts',(53.2009003909755,29.861560604365,18.9964669914489));
#51271=CARTESIAN_POINT('Ctrl Pts',(53.1968517623983,29.8530592829174,18.9970702637217));
#51272=CARTESIAN_POINT('Ctrl Pts',(53.1946710020045,29.8484343918882,18.9973967564096));
#51273=CARTESIAN_POINT('Ctrl Pts',(53.1884972506746,29.8352097042761,18.9983256498074));
#51274=CARTESIAN_POINT('Ctrl Pts',(53.1845476939467,29.8265896162969,18.9989254686864));
#51275=CARTESIAN_POINT('Ctrl Pts',(53.1581741776796,29.7679272273677,19.0029713927468));
#51276=CARTESIAN_POINT('Ctrl Pts',(53.137758349,29.7170019555476,19.0063068100104));
#51277=CARTESIAN_POINT('Ctrl Pts',(53.0893253284311,29.5801003891777,19.0149745841698));
#51278=CARTESIAN_POINT('Ctrl Pts',(53.0650100751346,29.4929578116711,19.0201936490204));
#51279=CARTESIAN_POINT('Ctrl Pts',(53.0466869973344,29.4044698704695,19.02544331564));
#51280=CARTESIAN_POINT('Origin',(55.,29.,3.45145488139523));
#51281=CARTESIAN_POINT('',(53.0466870003186,29.404469884881,19.982208722643));
#51282=CARTESIAN_POINT('',(53.0466869979816,29.4044698735951,19.8236610414577));
#51283=CARTESIAN_POINT('',(53.0466869980082,29.4044698737233,3.45145488139523));
#51284=CARTESIAN_POINT('Ctrl Pts',(53.0466870003186,29.404469884881,19.982208722643));
#51285=CARTESIAN_POINT('Ctrl Pts',(53.0809855152632,29.5701082614707,19.9721559016089));
#51286=CARTESIAN_POINT('Ctrl Pts',(53.1362186434219,29.7307426871855,19.9626316675732));
#51287=CARTESIAN_POINT('Ctrl Pts',(53.2369797591282,29.9349931684407,19.9489879473138));
#51288=CARTESIAN_POINT('Ctrl Pts',(53.2651666453031,29.9863086988721,19.9454229282393));
#51289=CARTESIAN_POINT('Ctrl Pts',(53.3031188551555,30.0487293633254,19.9408720584243));
#51290=CARTESIAN_POINT('Ctrl Pts',(53.3108066690786,30.0610677501633,19.9399617063667));
#51291=CARTESIAN_POINT('Ctrl Pts',(53.3232804335094,30.080608071092,19.9385020991789));
#51292=CARTESIAN_POINT('Ctrl Pts',(53.3279796338778,30.0878649729846,19.9379560363604));
#51293=CARTESIAN_POINT('Ctrl Pts',(53.3369555199429,30.1015307442765,19.9369200256813));
#51294=CARTESIAN_POINT('Ctrl Pts',(53.3412224624332,30.1079458476772,19.9364304464665));
#51295=CARTESIAN_POINT('Ctrl Pts',(53.3509696889223,30.1224177204253,19.9353185355355));
#51296=CARTESIAN_POINT('Ctrl Pts',(53.3564720254768,30.1304593302738,19.9346953840858));
#51297=CARTESIAN_POINT('Ctrl Pts',(53.3708179444487,30.1510996147478,19.933082054274));
#51298=CARTESIAN_POINT('Ctrl Pts',(53.3797487038272,30.1636366308049,19.9320885943011));
#51299=CARTESIAN_POINT('Ctrl Pts',(53.4442043791538,30.2519388426516,19.924993147104));
#51300=CARTESIAN_POINT('Ctrl Pts',(53.5048668912053,30.3237912707411,19.9186918095494));
#51301=CARTESIAN_POINT('Ctrl Pts',(53.6902095118712,30.5142698031121,19.9004549542756));
#51302=CARTESIAN_POINT('Ctrl Pts',(53.8254705912628,30.6214323545154,19.8882053821055));
#51303=CARTESIAN_POINT('Ctrl Pts',(53.9859156762507,30.7178169434364,19.875706599145));
#51304=CARTESIAN_POINT('Ctrl Pts',(53.9991334958088,30.7255516042332,19.8746911161022));
#51305=CARTESIAN_POINT('Ctrl Pts',(54.0194651702628,30.7371368387581,19.8731521253314));
#51306=CARTESIAN_POINT('Ctrl Pts',(54.0265152481549,30.741097467672,19.8726226491175));
#51307=CARTESIAN_POINT('Ctrl Pts',(54.0395852710823,30.7483358054153,19.8716490184927));
#51308=CARTESIAN_POINT('Ctrl Pts',(54.0455983711186,30.7516255519124,19.8712041654684));
#51309=CARTESIAN_POINT('Ctrl Pts',(54.0555870247051,30.7570236030948,19.8704704413292));
#51310=CARTESIAN_POINT('Ctrl Pts',(54.059552911579,30.7591495344609,19.8701804843349));
#51311=CARTESIAN_POINT('Ctrl Pts',(54.0674227929945,30.7633339993845,19.8696078360786));
#51312=CARTESIAN_POINT('Ctrl Pts',(54.0713264726637,30.7653930215741,19.869325118415));
#51313=CARTESIAN_POINT('Ctrl Pts',(54.080973213246,30.7704404084755,19.8686296704532));
#51314=CARTESIAN_POINT('Ctrl Pts',(54.086724113237,30.7734138355636,19.868217866661));
#51315=CARTESIAN_POINT('Ctrl Pts',(54.106616961713,30.7835767398903,19.866802643581));
#51316=CARTESIAN_POINT('Ctrl Pts',(54.1208305594225,30.7906256928368,19.8658074961266));
#51317=CARTESIAN_POINT('Ctrl Pts',(54.2425621597303,30.8491970836889,19.8574076158891));
#51318=CARTESIAN_POINT('Ctrl Pts',(54.3544304914475,30.8911609295634,19.8504904324379));
#51319=CARTESIAN_POINT('Ctrl Pts',(54.5714065844679,30.9510343487714,19.8374189133662));
#51320=CARTESIAN_POINT('Ctrl Pts',(54.6754970631497,30.9710208435891,19.831285456852));
#51321=CARTESIAN_POINT('Ctrl Pts',(54.8347017216589,30.9886323575099,19.821662676116));
#51322=CARTESIAN_POINT('Ctrl Pts',(54.8889460492788,30.9923976504616,19.8183444698508));
#51323=CARTESIAN_POINT('Ctrl Pts',(54.9574737023675,30.9943472359192,19.8140718161429));
#51324=CARTESIAN_POINT('Ctrl Pts',(54.9716779375989,30.9945995156371,19.8131818853279));
#51325=CARTESIAN_POINT('Ctrl Pts',(54.9944559243433,30.9947607169895,19.8117473834205));
#51326=CARTESIAN_POINT('Ctrl Pts',(55.0030286679562,30.9947661212021,19.8112058125552));
#51327=CARTESIAN_POINT('Ctrl Pts',(55.0193193191825,30.9946713763764,19.810173368059));
#51328=CARTESIAN_POINT('Ctrl Pts',(55.0270371491961,30.9945816919003,19.8096828288425));
#51329=CARTESIAN_POINT('Ctrl Pts',(55.0446221043676,30.9942752658199,19.8085618423534));
#51330=CARTESIAN_POINT('Ctrl Pts',(55.0544884707148,30.9940300822371,19.8079305230116));
#51331=CARTESIAN_POINT('Ctrl Pts',(55.0801535500153,30.9932016719954,19.8062819479021));
#51332=CARTESIAN_POINT('Ctrl Pts',(55.0959476220709,30.9925038336013,19.8052611670606));
#51333=CARTESIAN_POINT('Ctrl Pts',(55.2277109001588,30.9851118095156,19.7966911438192));
#51334=CARTESIAN_POINT('Ctrl Pts',(55.3428802889527,30.9684882466191,19.7888304477018));
#51335=CARTESIAN_POINT('Ctrl Pts',(55.5359760102981,30.9231529866264,19.775107132445));
#51336=CARTESIAN_POINT('Ctrl Pts',(55.6147805215814,30.8994294389724,19.7693494140294));
#51337=CARTESIAN_POINT('Ctrl Pts',(55.7635030793175,30.844429399546,19.7583482866169));
#51338=CARTESIAN_POINT('Ctrl Pts',(55.833540638356,30.8138547793134,19.7531072022106));
#51339=CARTESIAN_POINT('Ctrl Pts',(55.9152415893866,30.7724537400094,19.7470489452602));
#51340=CARTESIAN_POINT('Ctrl Pts',(55.9287455633322,30.7654152881345,19.7460495878322));
#51341=CARTESIAN_POINT('Ctrl Pts',(55.947622953794,30.7552995755015,19.7446567488043));
#51342=CARTESIAN_POINT('Ctrl Pts',(55.9530642704512,30.7523510952891,19.7442557634354));
#51343=CARTESIAN_POINT('Ctrl Pts',(55.9623535798591,30.7472614399443,19.743572170244));
#51344=CARTESIAN_POINT('Ctrl Pts',(55.9662083420439,30.745132772437,19.7432887873472));
#51345=CARTESIAN_POINT('Ctrl Pts',(55.9741570665803,30.7407089358132,19.7427050717838));
#51346=CARTESIAN_POINT('Ctrl Pts',(55.9782500076183,30.7384120665946,19.7424048490615));
#51347=CARTESIAN_POINT('Ctrl Pts',(55.9889208990069,30.7323741747402,19.7416229208344));
#51348=CARTESIAN_POINT('Ctrl Pts',(55.9954858097408,30.7286100869687,19.7411426591838));
#51349=CARTESIAN_POINT('Ctrl Pts',(56.0222535387391,30.7130593488149,19.7391870334872));
#51350=CARTESIAN_POINT('Ctrl Pts',(56.0422706359667,30.7009546328631,19.7377306685757));
#51351=CARTESIAN_POINT('Ctrl Pts',(56.2269903972806,30.5847653917481,19.7243036199759));
#51352=CARTESIAN_POINT('Ctrl Pts',(56.3758416579623,30.4574183040491,19.7134855734595));
#51353=CARTESIAN_POINT('Ctrl Pts',(56.535378260469,30.274339204396,19.6990640616802));
#51354=CARTESIAN_POINT('Ctrl Pts',(56.5655646831117,30.2370665127549,19.696181706194));
#51355=CARTESIAN_POINT('Ctrl Pts',(56.6136016011858,30.1731755042671,19.6912939990029));
#51356=CARTESIAN_POINT('Ctrl Pts',(56.6322069473577,30.147149160133,19.6893168825357));
#51357=CARTESIAN_POINT('Ctrl Pts',(56.6567977492473,30.1109399738721,19.6865789739702));
#51358=CARTESIAN_POINT('Ctrl Pts',(56.6633311804523,30.1011338620458,19.6858387557726));
#51359=CARTESIAN_POINT('Ctrl Pts',(56.6741808027612,30.0845326154817,19.6845874213316));
#51360=CARTESIAN_POINT('Ctrl Pts',(56.6785434884909,30.0777681144629,19.6840780422092));
#51361=CARTESIAN_POINT('Ctrl Pts',(56.6870876914727,30.0643423038906,19.683067948061));
#51362=CARTESIAN_POINT('Ctrl Pts',(56.6912709926829,30.057682298701,19.6825673108078));
#51363=CARTESIAN_POINT('Ctrl Pts',(56.7004143226992,30.0429327564139,19.6814594359579));
#51364=CARTESIAN_POINT('Ctrl Pts',(56.7053562110417,30.034832252872,19.6808515510307));
#51365=CARTESIAN_POINT('Ctrl Pts',(56.7221331416946,30.0068857592873,19.6787560933355));
#51366=CARTESIAN_POINT('Ctrl Pts',(56.7336806731489,29.9868701736201,19.6772582454576));
#51367=CARTESIAN_POINT('Ctrl Pts',(56.8238865692704,29.8240431471759,19.6650920276266));
#51368=CARTESIAN_POINT('Ctrl Pts',(56.8850985591302,29.67230386812,19.6537935042898));
#51369=CARTESIAN_POINT('Ctrl Pts',(56.9545767036112,29.4122358606628,19.6350365087271));
#51370=CARTESIAN_POINT('Ctrl Pts',(56.9737539259589,29.3075855530193,19.6276613640761));
#51371=CARTESIAN_POINT('Ctrl Pts',(56.9858006598142,29.1891740677725,19.619817369963));
#51372=CARTESIAN_POINT('Ctrl Pts',(56.9869726282983,29.1764394601699,19.6189803292083));
#51373=CARTESIAN_POINT('Ctrl Pts',(56.9884954466862,29.1579452257679,19.6177750396574));
#51374=CARTESIAN_POINT('Ctrl Pts',(56.9889438765151,29.1521942637276,19.6174016903485));
#51375=CARTESIAN_POINT('Ctrl Pts',(56.9896857531418,29.1421160642841,19.6167500482779));
#51376=CARTESIAN_POINT('Ctrl Pts',(56.9899900426221,29.1377897081094,19.6164711633991));
#51377=CARTESIAN_POINT('Ctrl Pts',(56.9906066311998,29.1285947197375,19.6158802724591));
#51378=CARTESIAN_POINT('Ctrl Pts',(56.9909151814092,29.1237259220304,19.6155684748353));
#51379=CARTESIAN_POINT('Ctrl Pts',(56.9917064892622,29.110469063948,19.6147223332519));
#51380=CARTESIAN_POINT('Ctrl Pts',(56.992154125241,29.102078894279,19.6141898958572));
#51381=CARTESIAN_POINT('Ctrl Pts',(56.9940047379995,29.0627193609686,19.61170554401));
#51382=CARTESIAN_POINT('Ctrl Pts',(56.9947387391731,29.0317210075871,19.6097877921708));
#51383=CARTESIAN_POINT('Ctrl Pts',(56.9948237145519,28.7950532744245,19.5953573526225));
#51384=CARTESIAN_POINT('Ctrl Pts',(56.9630938523464,28.5906002848818,19.5839853449259));
#51385=CARTESIAN_POINT('Ctrl Pts',(56.8840039905391,28.3423009104254,19.5683356404376));
#51386=CARTESIAN_POINT('Ctrl Pts',(56.8651991233053,28.2907253414678,19.5649865024792));
#51387=CARTESIAN_POINT('Ctrl Pts',(56.8388642931578,28.2268190900567,19.5606789363534));
#51388=CARTESIAN_POINT('Ctrl Pts',(56.8332943235612,28.2137032908676,19.5597863496411));
#51389=CARTESIAN_POINT('Ctrl Pts',(56.8241452856285,28.1927855339599,19.558348582819));
#51390=CARTESIAN_POINT('Ctrl Pts',(56.8206554817723,28.1849448912794,19.5578064276401));
#51391=CARTESIAN_POINT('Ctrl Pts',(56.8139320632165,28.1700978518033,19.5567735301981));
#51392=CARTESIAN_POINT('Ctrl Pts',(56.8107081697433,28.1630872047548,19.5562831268507));
#51393=CARTESIAN_POINT('Ctrl Pts',(56.8032755155427,28.1471682181404,19.5551633742045));
#51394=CARTESIAN_POINT('Ctrl Pts',(56.7990412938667,28.1382720554921,19.5545331599245));
#51395=CARTESIAN_POINT('Ctrl Pts',(56.7878662564414,28.1152345170071,19.5528893667873));
#51396=CARTESIAN_POINT('Ctrl Pts',(56.7808236282824,28.1011435641362,19.5518722963646));
#51397=CARTESIAN_POINT('Ctrl Pts',(56.7134837752296,27.9703078501442,19.5423173556185));
#51398=CARTESIAN_POINT('Ctrl Pts',(56.6419676893934,27.8597268044612,19.5333744583581));
#51399=CARTESIAN_POINT('Ctrl Pts',(56.5003870086894,27.6820264044872,19.517593577708));
#51400=CARTESIAN_POINT('Ctrl Pts',(56.4353301739288,27.6114599644888,19.510869076918));
#51401=CARTESIAN_POINT('Ctrl Pts',(56.3244383129585,27.5073326322989,19.5004343766566));
#51402=CARTESIAN_POINT('Ctrl Pts',(56.2818102664538,27.4705699028715,19.4966327867027));
#51403=CARTESIAN_POINT('Ctrl Pts',(56.230199956324,27.4297367655303,19.4923199277571));
#51404=CARTESIAN_POINT('Ctrl Pts',(56.2226765135045,27.42387160737,19.4916981193046));
#51405=CARTESIAN_POINT('Ctrl Pts',(56.2110463573182,27.4149383124835,19.4907478052342));
#51406=CARTESIAN_POINT('Ctrl Pts',(56.2069695324575,27.411831752632,19.4904167207292));
#51407=CARTESIAN_POINT('Ctrl Pts',(56.1994488248153,27.4061466230073,19.489809760966));
#51408=CARTESIAN_POINT('Ctrl Pts',(56.1960085859419,27.4035634889783,19.4895335772083));
#51409=CARTESIAN_POINT('Ctrl Pts',(56.1882319667504,27.3977635924435,19.4889125339968));
#51410=CARTESIAN_POINT('Ctrl Pts',(56.1838908745714,27.3945532985316,19.4885681204272));
#51411=CARTESIAN_POINT('Ctrl Pts',(56.1710556528962,27.3851418569298,19.4875562892174));
#51412=CARTESIAN_POINT('Ctrl Pts',(56.1625253008029,27.3789900985121,19.4868921486032));
#51413=CARTESIAN_POINT('Ctrl Pts',(56.0899237891398,27.3275005991908,19.4813060466464));
#51414=CARTESIAN_POINT('Ctrl Pts',(56.0232687995311,27.2859077966735,19.476610700372));
#51415=CARTESIAN_POINT('Ctrl Pts',(55.8421042918325,27.1872064651714,19.4644809402379));
#51416=CARTESIAN_POINT('Ctrl Pts',(55.7242655217244,27.1369915904744,19.4571901841058));
#51417=CARTESIAN_POINT('Ctrl Pts',(55.5530467115627,27.0827492319694,19.4465574078655));
#51418=CARTESIAN_POINT('Ctrl Pts',(55.5030744296854,27.0690347720489,19.4434526049287));
#51419=CARTESIAN_POINT('Ctrl Pts',(55.4305024857964,27.0521264765659,19.4389038030478));
#51420=CARTESIAN_POINT('Ctrl Pts',(55.4082916699949,27.0473501327574,19.4375064648245));
#51421=CARTESIAN_POINT('Ctrl Pts',(55.3683579969855,27.0394736747881,19.4349819348445));
#51422=CARTESIAN_POINT('Ctrl Pts',(55.350665422506,27.0362319856017,19.4338591958836));
#51423=CARTESIAN_POINT('Ctrl Pts',(55.3236797041584,27.0316638836034,19.4321392608121));
#51424=CARTESIAN_POINT('Ctrl Pts',(55.3144167333096,27.0301630191847,19.4315475544084));
#51425=CARTESIAN_POINT('Ctrl Pts',(55.298289723885,27.0276666344277,19.430514930585));
#51426=CARTESIAN_POINT('Ctrl Pts',(55.2914303899745,27.0266414440981,19.4300749535121));
#51427=CARTESIAN_POINT('Ctrl Pts',(55.2760183492369,27.0244200820794,19.4290845915252));
#51428=CARTESIAN_POINT('Ctrl Pts',(55.2674629817585,27.0232436440592,19.4285335968298));
#51429=CARTESIAN_POINT('Ctrl Pts',(55.2445295003389,27.0202416950568,19.4270531654654));
#51430=CARTESIAN_POINT('Ctrl Pts',(55.2301388951744,27.0185172992992,19.4261205896033));
#51431=CARTESIAN_POINT('Ctrl Pts',(55.1649688744876,27.0114276149592,19.4218801157838));
#51432=CARTESIAN_POINT('Ctrl Pts',(55.1140175347032,27.0078569115449,19.4185170710026));
#51433=CARTESIAN_POINT('Ctrl Pts',(54.8789311883801,27.0004298061275,19.4027710055126));
#51434=CARTESIAN_POINT('Ctrl Pts',(54.694963403131,27.0201332395865,19.3896932137029));
#51435=CARTESIAN_POINT('Ctrl Pts',(54.4640230463797,27.0778485192307,19.3733859283527));
#51436=CARTESIAN_POINT('Ctrl Pts',(54.4122345519854,27.0930467956845,19.3697456423188));
#51437=CARTESIAN_POINT('Ctrl Pts',(54.3521747163503,27.1133524026632,19.3655915170578));
#51438=CARTESIAN_POINT('Ctrl Pts',(54.3432494279742,27.1164407497424,19.3649759860419));
#51439=CARTESIAN_POINT('Ctrl Pts',(54.3295336419076,27.1212960615824,19.3640332199847));
#51440=CARTESIAN_POINT('Ctrl Pts',(54.3247275740477,27.1230181733128,19.363703468125));
#51441=CARTESIAN_POINT('Ctrl Pts',(54.3158824854726,27.1262259185069,19.3630977641005));
#51442=CARTESIAN_POINT('Ctrl Pts',(54.3118416777655,27.1277061645309,19.3628215127369));
#51443=CARTESIAN_POINT('Ctrl Pts',(54.3027186368942,27.131081681143,19.362198830599));
#51444=CARTESIAN_POINT('Ctrl Pts',(54.2976393317177,27.132984607667,19.3618528564744));
#51445=CARTESIAN_POINT('Ctrl Pts',(54.282625649235,27.138679320949,19.3608321282679));
#51446=CARTESIAN_POINT('Ctrl Pts',(54.2727135738986,27.1425299207035,19.3601607377418));
#51447=CARTESIAN_POINT('Ctrl Pts',(54.1784857909409,27.180005047721,19.3537978312573));
#51448=CARTESIAN_POINT('Ctrl Pts',(54.0965154595727,27.2192733896552,19.3484104391332));
#51449=CARTESIAN_POINT('Ctrl Pts',(53.9148739286312,27.3220746107217,19.336202371856));
#51450=CARTESIAN_POINT('Ctrl Pts',(53.8176058788225,27.3891380697575,19.329448738821));
#51451=CARTESIAN_POINT('Ctrl Pts',(53.6881860802265,27.4964402887968,19.3194833405899));
#51452=CARTESIAN_POINT('Ctrl Pts',(53.6507669388669,27.529926132263,19.3164710132448));
#51453=CARTESIAN_POINT('Ctrl Pts',(53.5986578340375,27.5802247087775,19.3120468714056));
#51454=CARTESIAN_POINT('Ctrl Pts',(53.5829230052124,27.5959293192739,19.3106787747584));
#51455=CARTESIAN_POINT('Ctrl Pts',(53.5551516093398,27.6245897875243,19.3082026259016));
#51456=CARTESIAN_POINT('Ctrl Pts',(53.5430185078242,27.6374490744267,19.3070987776576));
#51457=CARTESIAN_POINT('Ctrl Pts',(53.5247527680116,27.6573310043498,19.3054018993267));
#51458=CARTESIAN_POINT('Ctrl Pts',(53.5184955729439,27.664238398794,19.3048141320337));
#51459=CARTESIAN_POINT('Ctrl Pts',(53.507671304719,27.6763570575715,19.3037858427187));
#51460=CARTESIAN_POINT('Ctrl Pts',(53.5030825168778,27.6815487796074,19.3033462353837));
#51461=CARTESIAN_POINT('Ctrl Pts',(53.4928062546393,27.6932980735253,19.30235336441));
#51462=CARTESIAN_POINT('Ctrl Pts',(53.4871343759873,27.6998690410253,19.3017994709368));
#51463=CARTESIAN_POINT('Ctrl Pts',(53.4719759445861,27.7176638447469,19.3003030478218));
#51464=CARTESIAN_POINT('Ctrl Pts',(53.4625703858617,27.7289556689449,19.299357259908));
#51465=CARTESIAN_POINT('Ctrl Pts',(53.4196913534228,27.7816063319796,19.2949637216228));
#51466=CARTESIAN_POINT('Ctrl Pts',(53.3877590479423,27.8241867561021,19.2914558178671));
#51467=CARTESIAN_POINT('Ctrl Pts',(53.254387391879,28.0176953151499,19.2756981544922));
#51468=CARTESIAN_POINT('Ctrl Pts',(53.1721650204346,28.1808006519824,19.2627870578473));
#51469=CARTESIAN_POINT('Ctrl Pts',(53.101464500245,28.3868973773681,19.2478623208375));
#51470=CARTESIAN_POINT('Ctrl Pts',(53.0906748889082,28.4213724860796,19.2454132675873));
#51471=CARTESIAN_POINT('Ctrl Pts',(53.0748413187565,28.47724429338,19.2415390980684));
#51472=CARTESIAN_POINT('Ctrl Pts',(53.069204631899,28.4984635416484,19.2400894000607));
#51473=CARTESIAN_POINT('Ctrl Pts',(53.0622027444243,28.5266922907014,19.2381931939999));
#51474=CARTESIAN_POINT('Ctrl Pts',(53.0605234414366,28.5336213192122,19.237730319033));
#51475=CARTESIAN_POINT('Ctrl Pts',(53.057822571403,28.5450323884993,19.2369724185095));
#51476=CARTESIAN_POINT('Ctrl Pts',(53.0567793003946,28.5495091506689,19.2366761876684));
#51477=CARTESIAN_POINT('Ctrl Pts',(53.054765453687,28.558287909771,19.2360975111195));
#51478=CARTESIAN_POINT('Ctrl Pts',(53.0537936571418,28.5625895721285,19.2358150007262));
#51479=CARTESIAN_POINT('Ctrl Pts',(53.0514341970133,28.5731972763926,19.2351208403134));
#51480=CARTESIAN_POINT('Ctrl Pts',(53.0500628552959,28.5795069704419,19.2347101089625));
#51481=CARTESIAN_POINT('Ctrl Pts',(53.0454495209873,28.6012414074214,19.2333024118755));
#51482=CARTESIAN_POINT('Ctrl Pts',(53.0423596243331,28.6166983094784,19.2323136008385));
#51483=CARTESIAN_POINT('Ctrl Pts',(53.0168140555292,28.7528647790546,19.2236976874981));
#51484=CARTESIAN_POINT('Ctrl Pts',(53.0053615296379,28.8753886883317,19.2165886790864));
#51485=CARTESIAN_POINT('Ctrl Pts',(53.0051277480755,29.1347064779513,19.2015306109203));
#51486=CARTESIAN_POINT('Ctrl Pts',(53.0190159974418,29.2708378576247,19.193601623165));
#51487=CARTESIAN_POINT('Ctrl Pts',(53.0466869987623,29.4044698773653,19.1852189598335));
#51488=CARTESIAN_POINT('',(53.0052500460737,29.0004287317334,19.0496800917662));
#51489=CARTESIAN_POINT('Ctrl Pts',(53.0466869973344,29.4044698704695,19.02544331564));
#51490=CARTESIAN_POINT('Ctrl Pts',(53.0455062711038,29.3987677698503,19.0257816004602));
#51491=CARTESIAN_POINT('Ctrl Pts',(53.0443504267425,29.3930600816379,19.0261199936269));
#51492=CARTESIAN_POINT('Ctrl Pts',(53.017991194005,29.2598997968382,19.0340108203298));
#51493=CARTESIAN_POINT('Ctrl Pts',(53.0052779626167,29.1303153687274,19.0416346866029));
#51494=CARTESIAN_POINT('Ctrl Pts',(53.0052500460737,29.0004287317334,19.0496800917662));
#51495=CARTESIAN_POINT('Ctrl Pts',(53.0052500457895,29.0004274077679,19.0496801737749));
#51496=CARTESIAN_POINT('Ctrl Pts',(53.0052478063791,28.9899758804868,19.0503275598346));
#51497=CARTESIAN_POINT('Ctrl Pts',(53.0053277084281,28.9795246123797,19.0509773538252));
#51498=CARTESIAN_POINT('Ctrl Pts',(53.005646711531,28.9589507726378,19.0522615537449));
#51499=CARTESIAN_POINT('Ctrl Pts',(53.0058807590315,28.9488284732444,19.0528957849875));
#51500=CARTESIAN_POINT('Ctrl Pts',(53.0064225229065,28.9312049216504,19.0540044101039));
#51501=CARTESIAN_POINT('Ctrl Pts',(53.0066955457967,28.9237027499559,19.0544777265378));
#51502=CARTESIAN_POINT('Ctrl Pts',(53.0073233780377,28.9087707888847,19.0554226340525));
#51503=CARTESIAN_POINT('Ctrl Pts',(53.0076774093588,28.9013410872481,19.0558941935145));
#51504=CARTESIAN_POINT('Ctrl Pts',(53.0084668548631,28.8865180927034,19.0568378711042));
#51505=CARTESIAN_POINT('Ctrl Pts',(53.0089019062289,28.8791248990796,19.0573099705662));
#51506=CARTESIAN_POINT('Ctrl Pts',(53.0101904368998,28.8591275111539,19.0585908677934));
#51507=CARTESIAN_POINT('Ctrl Pts',(53.0111224870436,28.8465288891049,19.0594020958668));
#51508=CARTESIAN_POINT('Ctrl Pts',(53.0151158014306,28.7987267486747,19.0624967101783));
#51509=CARTESIAN_POINT('Ctrl Pts',(53.0189924724166,28.7635996678762,19.064805201475));
#51510=CARTESIAN_POINT('Ctrl Pts',(53.0512359465118,28.5288222854712,19.0804753273298));
#51511=CARTESIAN_POINT('Ctrl Pts',(53.1088074172142,28.3343803605279,19.0947959733641));
#51512=CARTESIAN_POINT('Ctrl Pts',(53.2182450193238,28.1013929809828,19.1124492188469));
#51513=CARTESIAN_POINT('Ctrl Pts',(53.2440984053558,28.0518669834042,19.1162213608639));
#51514=CARTESIAN_POINT('Ctrl Pts',(53.2767556003028,27.9952378513681,19.1205052967201));
#51515=CARTESIAN_POINT('Ctrl Pts',(53.2815717483618,27.9870229079583,19.1211259900399));
#51516=CARTESIAN_POINT('Ctrl Pts',(53.2890686482566,27.9744427341258,19.1220749635518));
#51517=CARTESIAN_POINT('Ctrl Pts',(53.2917076163545,27.9700529482718,19.1224058115589));
#51518=CARTESIAN_POINT('Ctrl Pts',(53.2965943633647,27.9619945522091,19.1230125472206));
#51519=CARTESIAN_POINT('Ctrl Pts',(53.2988370946657,27.9583230622015,19.1232887417282));
#51520=CARTESIAN_POINT('Ctrl Pts',(53.3039234013095,27.9500567011087,19.1239100703869));
#51521=CARTESIAN_POINT('Ctrl Pts',(53.3067737738283,27.9454661180584,19.124254756769));
#51522=CARTESIAN_POINT('Ctrl Pts',(53.3152374736723,27.9319579490454,19.1252681414036));
#51523=CARTESIAN_POINT('Ctrl Pts',(53.3209029494058,27.9230730299676,19.1259335475991));
#51524=CARTESIAN_POINT('Ctrl Pts',(53.3701650094872,27.8471513641234,19.1316133711269));
#51525=CARTESIAN_POINT('Ctrl Pts',(53.4176913566518,27.7827389007307,19.1363924645113));
#51526=CARTESIAN_POINT('Ctrl Pts',(53.5493389577999,27.6251062556018,19.1484590061293));
#51527=CARTESIAN_POINT('Ctrl Pts',(53.6386096689264,27.5366588463793,19.1556175144074));
#51528=CARTESIAN_POINT('Ctrl Pts',(53.7760896828648,27.423988437114,19.1661359464649));
#51529=CARTESIAN_POINT('Ctrl Pts',(53.8178739184378,27.3924098024809,19.1692726681336));
#51530=CARTESIAN_POINT('Ctrl Pts',(53.8796357045458,27.3494439987075,19.1738644386051));
#51531=CARTESIAN_POINT('Ctrl Pts',(53.8986445545685,27.3366998503861,19.1752717878577));
#51532=CARTESIAN_POINT('Ctrl Pts',(53.9286244627288,27.3173396137033,19.1774849767904));
#51533=CARTESIAN_POINT('Ctrl Pts',(53.939447466235,27.3104971651932,19.178282676217));
#51534=CARTESIAN_POINT('Ctrl Pts',(53.9577414396238,27.2991765203366,19.179629298302));
#51535=CARTESIAN_POINT('Ctrl Pts',(53.9651773153871,27.2946421421735,19.1801761831571));
#51536=CARTESIAN_POINT('Ctrl Pts',(53.9797793797204,27.2858685082583,19.1812493362727));
#51537=CARTESIAN_POINT('Ctrl Pts',(53.9869428935655,27.2816251338136,19.1817754421767));
#51538=CARTESIAN_POINT('Ctrl Pts',(54.0006142827687,27.2736419586889,19.1827789156502));
#51539=CARTESIAN_POINT('Ctrl Pts',(54.007117125688,27.2698937911232,19.1832559713337));
#51540=CARTESIAN_POINT('Ctrl Pts',(54.0222097419011,27.2613076861743,19.1843626873562));
#51541=CARTESIAN_POINT('Ctrl Pts',(54.0308144788745,27.2564965813347,19.1849932907758));
#51542=CARTESIAN_POINT('Ctrl Pts',(54.053277963919,27.2441544129441,19.1866387681824));
#51543=CARTESIAN_POINT('Ctrl Pts',(54.0671907849444,27.2367237074331,19.1876571455239));
#51544=CARTESIAN_POINT('Ctrl Pts',(54.1976894877986,27.1690023063201,19.1972042738253));
#51545=CARTESIAN_POINT('Ctrl Pts',(54.3198496013681,27.1202025461571,19.20613706764));
#51546=CARTESIAN_POINT('Ctrl Pts',(54.5360915628439,27.0576734373542,19.2217713993886));
#51547=CARTESIAN_POINT('Ctrl Pts',(54.6280191536068,27.0379922921636,19.2283569245646));
#51548=CARTESIAN_POINT('Ctrl Pts',(54.7786178314443,27.0167187546396,19.2388011500169));
#51549=CARTESIAN_POINT('Ctrl Pts',(54.8365784782753,27.0111034844638,19.2427380750565));
#51550=CARTESIAN_POINT('Ctrl Pts',(54.9043078099967,27.0075234009131,19.2471835425869));
#51551=CARTESIAN_POINT('Ctrl Pts',(54.9139122676135,27.0070853243724,19.2478103027406));
#51552=CARTESIAN_POINT('Ctrl Pts',(54.9286573415978,27.0065195708625,19.2487665663839));
#51553=CARTESIAN_POINT('Ctrl Pts',(54.9337957516041,27.006342307418,19.2490986981816));
#51554=CARTESIAN_POINT('Ctrl Pts',(54.9432340627601,27.006053237581,19.2497066542654));
#51555=CARTESIAN_POINT('Ctrl Pts',(54.9475336287227,27.0059354715635,19.2499827943348));
#51556=CARTESIAN_POINT('Ctrl Pts',(54.9572121466435,27.0057017006123,19.2506025922383));
#51557=CARTESIAN_POINT('Ctrl Pts',(54.9625911975236,27.0055935493339,19.2509458124359));
#51558=CARTESIAN_POINT('Ctrl Pts',(54.9764053822487,27.0053717091144,19.2518242021446));
#51559=CARTESIAN_POINT('Ctrl Pts',(54.9848410181764,27.0052897614051,19.2523576717401));
#51560=CARTESIAN_POINT('Ctrl Pts',(55.0365749669107,27.0051154014859,19.2556128088198));
#51561=CARTESIAN_POINT('Ctrl Pts',(55.0798697677149,27.0063792411834,19.2582660652183));
#51562=CARTESIAN_POINT('Ctrl Pts',(55.1294713727338,27.0094459134535,19.2612590704408));
#51563=CARTESIAN_POINT('Ctrl Pts',(55.1358483534701,27.0098709503743,19.2616429725774));
#51564=CARTESIAN_POINT('Ctrl Pts',(55.1570280403962,27.0113848891505,19.2629153711276));
#51565=CARTESIAN_POINT('Ctrl Pts',(55.171820842013,27.012608373066,19.2637997756829));
#51566=CARTESIAN_POINT('Ctrl Pts',(55.30926044153,27.0255217837657,19.2719876816518));
#51567=CARTESIAN_POINT('Ctrl Pts',(55.4305939170739,27.048385905668,19.2790167449683));
#51568=CARTESIAN_POINT('Ctrl Pts',(55.6428903483604,27.1091673467042,19.2919737450275));
#51569=CARTESIAN_POINT('Ctrl Pts',(55.7346238256166,27.1428838728818,19.297806546523));
#51570=CARTESIAN_POINT('Ctrl Pts',(55.8386134151468,27.1900193571786,19.3049001245724));
#51571=CARTESIAN_POINT('Ctrl Pts',(55.8536262954095,27.1970511628516,19.305936209793));
#51572=CARTESIAN_POINT('Ctrl Pts',(55.8767308645133,27.2082262563654,19.307550196967));
#51573=CARTESIAN_POINT('Ctrl Pts',(55.8848850365041,27.2122392148411,19.3081236134962));
#51574=CARTESIAN_POINT('Ctrl Pts',(55.8991906174989,27.2194013508477,19.3091364483572));
#51575=CARTESIAN_POINT('Ctrl Pts',(55.9053536589434,27.2225270561144,19.3095750456032));
#51576=CARTESIAN_POINT('Ctrl Pts',(55.9193854779955,27.2297354743785,19.3105788534202));
#51577=CARTESIAN_POINT('Ctrl Pts',(55.9272434869398,27.2338387220894,19.3111447752997));
#51578=CARTESIAN_POINT('Ctrl Pts',(55.9484446365664,27.2450898988362,19.3126820498467));
#51579=CARTESIAN_POINT('Ctrl Pts',(55.9617339759139,27.2523374380213,19.3136568901226));
#51580=CARTESIAN_POINT('Ctrl Pts',(56.0276775557568,27.2892806607301,19.3185516916453));
#51581=CARTESIAN_POINT('Ctrl Pts',(56.0790404227824,27.3212051021236,19.3225504592779));
#51582=CARTESIAN_POINT('Ctrl Pts',(56.2724337871031,27.4539530841267,19.3383555247969));
#51583=CARTESIAN_POINT('Ctrl Pts',(56.4024699620655,27.5708697809595,19.3507155619692));
#51584=CARTESIAN_POINT('Ctrl Pts',(56.5388225049768,27.7302271729996,19.3650757897771));
#51585=CARTESIAN_POINT('Ctrl Pts',(56.5612644131866,27.7579245328783,19.3674916203489));
#51586=CARTESIAN_POINT('Ctrl Pts',(56.5961853514039,27.8034663573516,19.3713193255936));
#51587=CARTESIAN_POINT('Ctrl Pts',(56.6091349880337,27.8209388830386,19.3727551082474));
#51588=CARTESIAN_POINT('Ctrl Pts',(56.6259332256596,27.8443966162524,19.3746360710949));
#51589=CARTESIAN_POINT('Ctrl Pts',(56.6300387172647,27.8501948779358,19.3750972970341));
#51590=CARTESIAN_POINT('Ctrl Pts',(56.6367462392396,27.8597761668842,19.3758531977741));
#51591=CARTESIAN_POINT('Ctrl Pts',(56.6393663007456,27.8635464046931,19.3761490657136));
#51592=CARTESIAN_POINT('Ctrl Pts',(56.6444796981123,27.8709590053242,19.376727623174));
#51593=CARTESIAN_POINT('Ctrl Pts',(56.6469739934054,27.874600643861,19.3770103741043));
#51594=CARTESIAN_POINT('Ctrl Pts',(56.6530983886751,27.8836061502658,19.3777060290041));
#51595=CARTESIAN_POINT('Ctrl Pts',(56.6567145316131,27.8889795348928,19.378118005205));
#51596=CARTESIAN_POINT('Ctrl Pts',(56.6691067907516,27.9075887743114,19.379534438761));
#51597=CARTESIAN_POINT('Ctrl Pts',(56.6777512406203,27.9209121553058,19.380530605369));
#51598=CARTESIAN_POINT('Ctrl Pts',(56.7496226740914,28.0346369361543,19.388895596884));
#51599=CARTESIAN_POINT('Ctrl Pts',(56.8039431155786,28.1404057897559,19.3957817210386));
#51600=CARTESIAN_POINT('Ctrl Pts',(56.9064822507263,28.3932675341782,19.4116281495014));
#51601=CARTESIAN_POINT('Ctrl Pts',(56.9476544124801,28.5423608936478,19.4205717857586));
#51602=CARTESIAN_POINT('Ctrl Pts',(56.9739988982319,28.7124605494592,19.4312478597554));
#51603=CARTESIAN_POINT('Ctrl Pts',(56.976509438149,28.7302575414514,19.4323697442541));
#51604=CARTESIAN_POINT('Ctrl Pts',(56.9799637947506,28.7573913943248,19.434088636665));
#51605=CARTESIAN_POINT('Ctrl Pts',(56.9810828221314,28.7667053127298,19.4346801652282));
#51606=CARTESIAN_POINT('Ctrl Pts',(56.9829147939246,28.7829180338033,19.4357125923112));
#51607=CARTESIAN_POINT('Ctrl Pts',(56.9836575393697,28.7898133578423,19.4361525516411));
#51608=CARTESIAN_POINT('Ctrl Pts',(56.985244598104,28.8053052119858,19.4371430218139));
#51609=CARTESIAN_POINT('Ctrl Pts',(56.9860690567932,28.8139035933078,19.4376941433216));
#51610=CARTESIAN_POINT('Ctrl Pts',(56.9881280499444,28.8369517354825,19.4391752750005));
#51611=CARTESIAN_POINT('Ctrl Pts',(56.989260874199,28.8514098401416,19.4401084295451));
#51612=CARTESIAN_POINT('Ctrl Pts',(56.9936758689586,28.9169242766799,19.4443559737099));
#51613=CARTESIAN_POINT('Ctrl Pts',(56.9951504502837,28.9680790735397,19.4477257384473));
#51614=CARTESIAN_POINT('Ctrl Pts',(56.9928830431827,29.2032638859485,19.4634723888697));
#51615=CARTESIAN_POINT('Ctrl Pts',(56.9656455395308,29.3861577437401,19.476542492339));
#51616=CARTESIAN_POINT('Ctrl Pts',(56.898531365494,29.6144227532047,19.4928417381771));
#51617=CARTESIAN_POINT('Ctrl Pts',(56.8812230855057,29.6655355009283,19.4964814148573));
#51618=CARTESIAN_POINT('Ctrl Pts',(56.858473142986,29.7247029214556,19.5006349386809));
#51619=CARTESIAN_POINT('Ctrl Pts',(56.8550212640473,29.7334936031845,19.5012504448394));
#51620=CARTESIAN_POINT('Ctrl Pts',(56.8496073561582,29.7469981611493,19.5021931808433));
#51621=CARTESIAN_POINT('Ctrl Pts',(56.8476894991173,29.751729433355,19.5025229272637));
#51622=CARTESIAN_POINT('Ctrl Pts',(56.8441215103822,29.7604353602534,19.503128625961));
#51623=CARTESIAN_POINT('Ctrl Pts',(56.8424766876577,29.7644120212646,19.5034048774));
#51624=CARTESIAN_POINT('Ctrl Pts',(56.8387295949393,29.7733889445849,19.5040275655343));
#51625=CARTESIAN_POINT('Ctrl Pts',(56.8366197949205,29.7783859669098,19.5043735455382));
#51626=CARTESIAN_POINT('Ctrl Pts',(56.8303135453714,29.7931538089394,19.5053943080593));
#51627=CARTESIAN_POINT('Ctrl Pts',(56.8260592416577,29.8028999294047,19.5060657266824));
#51628=CARTESIAN_POINT('Ctrl Pts',(56.7844338864745,29.8962163643188,19.5124771292406));
#51629=CARTESIAN_POINT('Ctrl Pts',(56.7414243466232,29.9771661884607,19.5179077140421));
#51630=CARTESIAN_POINT('Ctrl Pts',(56.6806591299543,30.0746892586491,19.5246268651176));
#51631=CARTESIAN_POINT('Ctrl Pts',(56.6679718336253,30.0942769747882,19.5259857752489));
#51632=CARTESIAN_POINT('Ctrl Pts',(56.5914688947928,30.2079656979871,19.5339527979515));
#51633=CARTESIAN_POINT('Ctrl Pts',(56.5200497700436,30.2966885727577,19.5405108062158));
#51634=CARTESIAN_POINT('Ctrl Pts',(56.4012679012639,30.4208650354141,19.5508075993651));
#51635=CARTESIAN_POINT('Ctrl Pts',(56.3592563488577,30.4611058819626,19.5543506200421));
#51636=CARTESIAN_POINT('Ctrl Pts',(56.3046436064739,30.5090205872882,19.5588767232874));
#51637=CARTESIAN_POINT('Ctrl Pts',(56.2936333847748,30.5184698617707,19.5597853243805));
#51638=CARTESIAN_POINT('Ctrl Pts',(56.2759043600714,30.5333526222113,19.5612427786714));
#51639=CARTESIAN_POINT('Ctrl Pts',(56.2692515036537,30.5388641320096,19.5617884562186));
#51640=CARTESIAN_POINT('Ctrl Pts',(56.2565974323395,30.5492094218162,19.5628241532649));
#51641=CARTESIAN_POINT('Ctrl Pts',(56.2506035860601,30.5540519963713,19.5633138070197));
#51642=CARTESIAN_POINT('Ctrl Pts',(56.2369591711558,30.5649455951951,19.5644264591327));
#51643=CARTESIAN_POINT('Ctrl Pts',(56.229292019185,30.5709754399873,19.5650502815214));
#51644=CARTESIAN_POINT('Ctrl Pts',(56.2093855131378,30.5863959862849,19.5666664987351));
#51645=CARTESIAN_POINT('Ctrl Pts',(56.1970810753765,30.5957012319404,19.5676621948154));
#51646=CARTESIAN_POINT('Ctrl Pts',(56.1081788587082,30.6613266680748,19.5748342900133));
#51647=CARTESIAN_POINT('Ctrl Pts',(56.0277600635917,30.7122415821892,19.5812151325597));
#51648=CARTESIAN_POINT('Ctrl Pts',(55.7930011073831,30.8383604519086,19.599510613008));
#51649=CARTESIAN_POINT('Ctrl Pts',(55.6321523185078,30.8996846582156,19.6117288699982));
#51650=CARTESIAN_POINT('Ctrl Pts',(55.4438911774468,30.9448597902957,19.6246481001136));
#51651=CARTESIAN_POINT('Ctrl Pts',(55.4222493014826,30.949672948775,19.6261122879272));
#51652=CARTESIAN_POINT('Ctrl Pts',(55.3935210755427,30.9555612809892,19.6280243476571));
#51653=CARTESIAN_POINT('Ctrl Pts',(55.3865037078211,30.9569603082822,19.6284889240765));
#51654=CARTESIAN_POINT('Ctrl Pts',(55.374960575581,30.9591971086414,19.6292488880222));
#51655=CARTESIAN_POINT('Ctrl Pts',(55.3704392422043,30.960057017698,19.6295454934098));
#51656=CARTESIAN_POINT('Ctrl Pts',(55.361583596545,30.9617095296753,19.6301242978393));
#51657=CARTESIAN_POINT('Ctrl Pts',(55.3572495821939,30.9625034299789,19.6304065649286));
#51658=CARTESIAN_POINT('Ctrl Pts',(55.3465778161003,30.9644217496476,19.6310992073881));
#51659=CARTESIAN_POINT('Ctrl Pts',(55.3402371140098,30.9655298781963,19.6315086733137));
#51660=CARTESIAN_POINT('Ctrl Pts',(55.3184714623735,30.9692252556808,19.6329074843549));
#51661=CARTESIAN_POINT('Ctrl Pts',(55.3030210531202,30.9716618515259,19.6338888121188));
#51662=CARTESIAN_POINT('Ctrl Pts',(55.163667429994,30.991961677723,19.6426483055549));
#51663=CARTESIAN_POINT('Ctrl Pts',(55.0383501666605,30.9983083678952,19.6498868154105));
#51664=CARTESIAN_POINT('Ctrl Pts',(54.7647391119377,30.9863980947121,19.6657897114707));
#51665=CARTESIAN_POINT('Ctrl Pts',(54.6174369152007,30.9633550387138,19.6744421469481));
#51666=CARTESIAN_POINT('Ctrl Pts',(54.4571249606752,30.9195371323278,19.6847551310954));
#51667=CARTESIAN_POINT('Ctrl Pts',(54.4402433051979,30.9146823555533,19.6858519775186));
#51668=CARTESIAN_POINT('Ctrl Pts',(54.4145287672803,30.9069183048982,19.6875403037169));
#51669=CARTESIAN_POINT('Ctrl Pts',(54.4056481769327,30.9041690816794,19.6881266036671));
#51670=CARTESIAN_POINT('Ctrl Pts',(54.3901848252909,30.8992632768257,19.6891532873395));
#51671=CARTESIAN_POINT('Ctrl Pts',(54.3835934271708,30.8971342801739,19.6895927659308));
#51672=CARTESIAN_POINT('Ctrl Pts',(54.3687508736513,30.8922546735312,19.6905866200501));
#51673=CARTESIAN_POINT('Ctrl Pts',(54.3605063923939,30.8894843558286,19.6911416331092));
#51674=CARTESIAN_POINT('Ctrl Pts',(54.3383068928586,30.8818629247589,19.6926442405079));
#51675=CARTESIAN_POINT('Ctrl Pts',(54.3243874363688,30.8769106212394,19.6935951396701));
#51676=CARTESIAN_POINT('Ctrl Pts',(54.2598228529578,30.8531283837888,19.6980475884345));
#51677=CARTESIAN_POINT('Ctrl Pts',(54.2099052973631,30.8324018280796,19.701611272545));
#51678=CARTESIAN_POINT('Ctrl Pts',(53.9967550176066,30.7335688856311,19.7173734418554));
#51679=CARTESIAN_POINT('Ctrl Pts',(53.8437413303386,30.6354847500644,19.73022054465));
#51680=CARTESIAN_POINT('Ctrl Pts',(53.6786330371633,30.4947633314687,19.7450798477257));
#51681=CARTESIAN_POINT('Ctrl Pts',(53.6518244489224,30.4706294774457,19.7475252213904));
#51682=CARTESIAN_POINT('Ctrl Pts',(53.6097890063487,30.4306718236124,19.751394249132));
#51683=CARTESIAN_POINT('Ctrl Pts',(53.5941439532769,30.4153011499753,19.7528424099391));
#51684=CARTESIAN_POINT('Ctrl Pts',(53.5737541727934,30.3945971434197,19.7547369327676));
#51685=CARTESIAN_POINT('Ctrl Pts',(53.5687806851537,30.389492579533,19.7551996260815));
#51686=CARTESIAN_POINT('Ctrl Pts',(53.560644908272,30.3810523545494,19.7559573061627));
#51687=CARTESIAN_POINT('Ctrl Pts',(53.5574666513218,30.3777322762714,19.7562534968753));
#51688=CARTESIAN_POINT('Ctrl Pts',(53.5512610207255,30.3712047201151,19.7568321596495));
#51689=CARTESIAN_POINT('Ctrl Pts',(53.5482327719927,30.3679981472172,19.757114696037));
#51690=CARTESIAN_POINT('Ctrl Pts',(53.540795985085,30.3600709261856,19.7578090190553));
#51691=CARTESIAN_POINT('Ctrl Pts',(53.5363996437534,30.3553388068496,19.7582198860257));
#51692=CARTESIAN_POINT('Ctrl Pts',(53.5213457806812,30.3389765122593,19.7596285362708));
#51693=CARTESIAN_POINT('Ctrl Pts',(53.5108029584606,30.3272409760407,19.7606181500471));
#51694=CARTESIAN_POINT('Ctrl Pts',(53.4200400313021,30.2237667285734,19.7691778105887));
#51695=CARTESIAN_POINT('Ctrl Pts',(53.3482329652704,30.1249676973428,19.7762376092627));
#51696=CARTESIAN_POINT('Ctrl Pts',(53.2327174921941,29.9308854704085,19.7893529279146));
#51697=CARTESIAN_POINT('Ctrl Pts',(53.1866143829717,29.8375355534069,19.7953840508298));
#51698=CARTESIAN_POINT('Ctrl Pts',(53.1347953712536,29.7080271062106,19.8037674016661));
#51699=CARTESIAN_POINT('Ctrl Pts',(53.1224773587453,29.6746845234481,19.8059259747632));
#51700=CARTESIAN_POINT('Ctrl Pts',(53.10285333501,29.6168579904176,19.809682730715));
#51701=CARTESIAN_POINT('Ctrl Pts',(53.0951147381528,29.5925295742279,19.8112671094947));
#51702=CARTESIAN_POINT('Ctrl Pts',(53.0847723662567,29.557715984457,19.8135427581142));
#51703=CARTESIAN_POINT('Ctrl Pts',(53.081783366705,29.5473471922249,19.8142215772134));
#51704=CARTESIAN_POINT('Ctrl Pts',(53.0767635230396,29.5293871547827,19.8153993997752));
#51705=CARTESIAN_POINT('Ctrl Pts',(53.0746931147149,29.5218071488323,19.8158971170494));
#51706=CARTESIAN_POINT('Ctrl Pts',(53.0708062509204,29.5072387760593,19.816854972627));
#51707=CARTESIAN_POINT('Ctrl Pts',(53.0689828450676,29.5002523788463,19.8173148786383));
#51708=CARTESIAN_POINT('Ctrl Pts',(53.0647792960958,29.4837809620813,19.8184005529486));
#51709=CARTESIAN_POINT('Ctrl Pts',(53.0624309089407,29.4742881021688,19.8190273272267));
#51710=CARTESIAN_POINT('Ctrl Pts',(53.0553526387268,29.4447455022966,19.8209814332942));
#51711=CARTESIAN_POINT('Ctrl Pts',(53.0508636462377,29.4246402295994,19.8223163538649));
#51712=CARTESIAN_POINT('Ctrl Pts',(53.0466869979816,29.4044698735951,19.8236610414577));
#51713=CARTESIAN_POINT('Origin',(55.,29.,3.45145488139523));
#51714=CARTESIAN_POINT('',(53.0466870286012,29.4044700214667,20.7832412988479));
#51715=CARTESIAN_POINT('',(53.0466869978243,29.4044698728352,20.6265291208673));
#51716=CARTESIAN_POINT('',(53.0466869980082,29.4044698737233,3.45145488139523));
#51717=CARTESIAN_POINT('',(53.0052502012793,29.0008961046522,20.0080399322459));
#51718=CARTESIAN_POINT('Ctrl Pts',(53.0466870286012,29.4044700214667,20.7832412988479));
#51719=CARTESIAN_POINT('Ctrl Pts',(53.0553314951071,29.4462168695904,20.7802703107498));
#51720=CARTESIAN_POINT('Ctrl Pts',(53.0653153162778,29.4876915346209,20.7773015864245));
#51721=CARTESIAN_POINT('Ctrl Pts',(53.0950104017614,29.5956936661242,20.7695663386943));
#51722=CARTESIAN_POINT('Ctrl Pts',(53.1168708710286,29.6615611137937,20.7648434349152));
#51723=CARTESIAN_POINT('Ctrl Pts',(53.1458993127313,29.7358301089969,20.7596082951248));
#51724=CARTESIAN_POINT('Ctrl Pts',(53.1497535331037,29.7454685309452,20.7589307160286));
#51725=CARTESIAN_POINT('Ctrl Pts',(53.1557155242807,29.7600468202737,20.7579091115319));
#51726=CARTESIAN_POINT('Ctrl Pts',(53.1577682242515,29.7650088119996,20.7575619638558));
#51727=CARTESIAN_POINT('Ctrl Pts',(53.1615010351062,29.7739299807685,20.7569389415378));
#51728=CARTESIAN_POINT('Ctrl Pts',(53.1631739260645,29.7778920453244,20.7566626487112));
#51729=CARTESIAN_POINT('Ctrl Pts',(53.1668783023558,29.7865868855655,20.7560572070357));
#51730=CARTESIAN_POINT('Ctrl Pts',(53.1689153040983,29.7913172087005,20.7557283945056));
#51731=CARTESIAN_POINT('Ctrl Pts',(53.1748238748398,29.8048931020259,20.754786207604));
#51732=CARTESIAN_POINT('Ctrl Pts',(53.1787414423642,29.8137186667577,20.7541755322148));
#51733=CARTESIAN_POINT('Ctrl Pts',(53.2071827159566,29.8765571935635,20.7498381965224));
#51734=CARTESIAN_POINT('Ctrl Pts',(53.2340434615237,29.9294865745365,20.7462412908334));
#51735=CARTESIAN_POINT('Ctrl Pts',(53.3090388818845,30.062239715722,20.7371702423419));
#51736=CARTESIAN_POINT('Ctrl Pts',(53.3604769902493,30.1400301279895,20.7318021602038));
#51737=CARTESIAN_POINT('Ctrl Pts',(53.496775687192,30.3177469759902,20.7187799579456));
#51738=CARTESIAN_POINT('Ctrl Pts',(53.5863923204465,30.4134522449883,20.7110942110001));
#51739=CARTESIAN_POINT('Ctrl Pts',(53.6965754071445,30.510086221292,20.7019991799708));
#51740=CARTESIAN_POINT('Ctrl Pts',(53.7085495855829,30.5203393930225,20.7010153871055));
#51741=CARTESIAN_POINT('Ctrl Pts',(53.7282055338175,30.5367704888667,20.6994071440083));
#51742=CARTESIAN_POINT('Ctrl Pts',(53.7358139323089,30.5430354112414,20.6987862199059));
#51743=CARTESIAN_POINT('Ctrl Pts',(53.7494616737045,30.5541045672664,20.6976750756369));
#51744=CARTESIAN_POINT('Ctrl Pts',(53.7554830965794,30.558930654621,20.6971857424836));
#51745=CARTESIAN_POINT('Ctrl Pts',(53.7682585937351,30.569048849743,20.6961493584569));
#51746=CARTESIAN_POINT('Ctrl Pts',(53.7750190987135,30.5743325482571,20.6956019887293));
#51747=CARTESIAN_POINT('Ctrl Pts',(53.7930901959422,30.5882692114758,20.6941415276353));
#51748=CARTESIAN_POINT('Ctrl Pts',(53.8044595544307,30.5968448230567,20.6932254432017));
#51749=CARTESIAN_POINT('Ctrl Pts',(53.8599992043105,30.6378113127696,20.6887627472052));
#51750=CARTESIAN_POINT('Ctrl Pts',(53.9053954309941,30.6684926105381,20.6851517100277));
#51751=CARTESIAN_POINT('Ctrl Pts',(54.1259058107122,30.8046507258535,20.6677680425098));
#51752=CARTESIAN_POINT('Ctrl Pts',(54.3152498351048,30.8846483702919,20.6531283277326));
#51753=CARTESIAN_POINT('Ctrl Pts',(54.5446692825354,30.9423542430837,20.6371711979269));
#51754=CARTESIAN_POINT('Ctrl Pts',(54.5761097422814,30.9494572059151,20.635024938875));
#51755=CARTESIAN_POINT('Ctrl Pts',(54.6159642829957,30.957451147703,20.632366481615));
#51756=CARTESIAN_POINT('Ctrl Pts',(54.6242286029815,30.9590544379303,20.6318185684144));
#51757=CARTESIAN_POINT('Ctrl Pts',(54.6373491715042,30.9615137648302,20.6309542625789));
#51758=CARTESIAN_POINT('Ctrl Pts',(54.6421987592813,30.9624041750971,20.6306360038038));
#51759=CARTESIAN_POINT('Ctrl Pts',(54.6508822938563,30.9639652587919,20.6300683513419));
#51760=CARTESIAN_POINT('Ctrl Pts',(54.6547148745724,30.9646426883762,20.6298185869035));
#51761=CARTESIAN_POINT('Ctrl Pts',(54.6639064328017,30.9662396190081,20.6292214166979));
#51762=CARTESIAN_POINT('Ctrl Pts',(54.6692672084739,30.9671484304837,20.6288746148961));
#51763=CARTESIAN_POINT('Ctrl Pts',(54.6855359201763,30.9698380788148,20.627826468042));
#51764=CARTESIAN_POINT('Ctrl Pts',(54.6964552180826,30.9715502257612,20.6271288450403));
#51765=CARTESIAN_POINT('Ctrl Pts',(54.7217669673691,30.9753038322458,20.6255241146606));
#51766=CARTESIAN_POINT('Ctrl Pts',(54.7361687893421,30.9772789304423,20.6246203189618));
#51767=CARTESIAN_POINT('Ctrl Pts',(54.7856186606282,30.983510675758,20.6215448180797));
#51768=CARTESIAN_POINT('Ctrl Pts',(54.8207590562504,30.9869944471541,20.6194069284775));
#51769=CARTESIAN_POINT('Ctrl Pts',(55.0246767137982,31.001756207901,20.6071822595322));
#51770=CARTESIAN_POINT('Ctrl Pts',(55.1942504915554,30.9924634424106,20.5976747691155));
#51771=CARTESIAN_POINT('Ctrl Pts',(55.4248483668661,30.9500757014966,20.5836991240699));
#51772=CARTESIAN_POINT('Ctrl Pts',(55.488446111065,30.9351254394238,20.5797381323352));
#51773=CARTESIAN_POINT('Ctrl Pts',(55.5660636393772,30.9128091818571,20.5747145329519));
#51774=CARTESIAN_POINT('Ctrl Pts',(55.5808846553037,30.9083605545498,20.5737466626839));
#51775=CARTESIAN_POINT('Ctrl Pts',(55.604185975882,30.9010699160559,20.5722106995769));
#51776=CARTESIAN_POINT('Ctrl Pts',(55.6127016920449,30.8983424747837,20.5716463302622));
#51777=CARTESIAN_POINT('Ctrl Pts',(55.6284904987294,30.8931682800392,20.5705941664712));
#51778=CARTESIAN_POINT('Ctrl Pts',(55.6357683914033,30.8907366271787,20.5701068735415));
#51779=CARTESIAN_POINT('Ctrl Pts',(55.651862591564,30.8852558836661,20.5690241029813));
#51780=CARTESIAN_POINT('Ctrl Pts',(55.6606718628811,30.8821868318323,20.5684279787952));
#51781=CARTESIAN_POINT('Ctrl Pts',(55.6861515672887,30.8731090713802,20.5666935295342));
#51782=CARTESIAN_POINT('Ctrl Pts',(55.7027635244819,30.8669399995253,20.5655499462101));
#51783=CARTESIAN_POINT('Ctrl Pts',(55.7400854344698,30.8525113130348,20.5629509862148));
#51784=CARTESIAN_POINT('Ctrl Pts',(55.7607432495935,30.8441242522601,20.5614915257487));
#51785=CARTESIAN_POINT('Ctrl Pts',(55.8276393450442,30.8156491832557,20.5566956562784));
#51786=CARTESIAN_POINT('Ctrl Pts',(55.8732546281813,30.7941556523979,20.5533147857872));
#51787=CARTESIAN_POINT('Ctrl Pts',(56.0255327576674,30.7152199304328,20.5416547324534));
#51788=CARTESIAN_POINT('Ctrl Pts',(56.1277551988651,30.6498062428275,20.5331628660581));
#51789=CARTESIAN_POINT('Ctrl Pts',(56.2923311389045,30.5220129383272,20.5186911413622));
#51790=CARTESIAN_POINT('Ctrl Pts',(56.357680462187,30.4640186122098,20.5126937591709));
#51791=CARTESIAN_POINT('Ctrl Pts',(56.4264891700111,30.3943704480612,20.5062632836647));
#51792=CARTESIAN_POINT('Ctrl Pts',(56.4338911495428,30.3867575424905,20.5055699673716));
#51793=CARTESIAN_POINT('Ctrl Pts',(56.4449797860629,30.3751692127862,20.5045294486039));
#51794=CARTESIAN_POINT('Ctrl Pts',(56.4487114662739,30.3712374101826,20.5041789526781));
#51795=CARTESIAN_POINT('Ctrl Pts',(56.4553767472369,30.3641571038,20.5035524092397));
#51796=CARTESIAN_POINT('Ctrl Pts',(56.4583162184178,30.3610142866377,20.5032759210915));
#51797=CARTESIAN_POINT('Ctrl Pts',(56.4647225991806,30.3541201424562,20.502672955222));
#51798=CARTESIAN_POINT('Ctrl Pts',(56.4681852738671,30.3503650083425,20.5023467946637));
#51799=CARTESIAN_POINT('Ctrl Pts',(56.4780174229222,30.3396199042582,20.5014197993077));
#51800=CARTESIAN_POINT('Ctrl Pts',(56.4843517692538,30.3325977726942,20.5008215298104));
#51801=CARTESIAN_POINT('Ctrl Pts',(56.5266792026148,30.2849981209674,20.4968144667943));
#51802=CARTESIAN_POINT('Ctrl Pts',(56.5610577346746,30.2430082293071,20.4935139387138));
#51803=CARTESIAN_POINT('Ctrl Pts',(56.7066642949965,30.0495784551256,20.4790562548759));
#51804=CARTESIAN_POINT('Ctrl Pts',(56.7978781162392,29.8842852165941,20.4685519342679));
#51805=CARTESIAN_POINT('Ctrl Pts',(56.8815651996263,29.6640886648209,20.454341185917));
#51806=CARTESIAN_POINT('Ctrl Pts',(56.8969008286751,29.6189249159408,20.4514222693561));
#51807=CARTESIAN_POINT('Ctrl Pts',(56.9146688118634,29.5597062413393,20.4475686562545));
#51808=CARTESIAN_POINT('Ctrl Pts',(56.9185904085718,29.5461122262323,20.4466823114557));
#51809=CARTESIAN_POINT('Ctrl Pts',(56.9246519853572,29.5242285484562,20.4452522177104));
#51810=CARTESIAN_POINT('Ctrl Pts',(56.926883830507,29.5159646652715,20.4447114357689));
#51811=CARTESIAN_POINT('Ctrl Pts',(56.9310275000814,29.5002199236002,20.4436795973319));
#51812=CARTESIAN_POINT('Ctrl Pts',(56.9329492186225,29.4927418122427,20.4431888691491));
#51813=CARTESIAN_POINT('Ctrl Pts',(56.9372339952756,29.4756573086641,20.4420661899594));
#51814=CARTESIAN_POINT('Ctrl Pts',(56.9395690882497,29.4660441758567,20.4414333571717));
#51815=CARTESIAN_POINT('Ctrl Pts',(56.9465312990696,29.4364231710655,20.4394797481006));
#51816=CARTESIAN_POINT('Ctrl Pts',(56.9509209130551,29.4163614073564,20.4381514737828));
#51817=CARTESIAN_POINT('Ctrl Pts',(56.9603362306117,29.3699069145034,20.4350629378972));
#51818=CARTESIAN_POINT('Ctrl Pts',(56.9651399245771,29.3434737626215,20.4332960253404));
#51819=CARTESIAN_POINT('Ctrl Pts',(56.9799533083057,29.2514297393085,20.4271092710799));
#51820=CARTESIAN_POINT('Ctrl Pts',(56.9872209839308,29.1854273920682,20.4226113117506));
#51821=CARTESIAN_POINT('Ctrl Pts',(56.996697378033,29.0271161180425,20.4117070400412));
#51822=CARTESIAN_POINT('Ctrl Pts',(56.9958155750849,28.9347726036196,20.4052501342461));
#51823=CARTESIAN_POINT('Ctrl Pts',(56.9813754053983,28.7520763259508,20.3925110992425));
#51824=CARTESIAN_POINT('Ctrl Pts',(56.9679977404678,28.6619120677663,20.386243584732));
#51825=CARTESIAN_POINT('Ctrl Pts',(56.9462284939126,28.5625811111966,20.3795644616586));
#51826=CARTESIAN_POINT('Ctrl Pts',(56.9438690068451,28.5522121809567,20.3788700976218));
#51827=CARTESIAN_POINT('Ctrl Pts',(56.9401809102486,28.5365833214134,20.3778283210176));
#51828=CARTESIAN_POINT('Ctrl Pts',(56.9389136221333,28.5313093236825,20.3774776034586));
#51829=CARTESIAN_POINT('Ctrl Pts',(56.9366023132329,28.5218603109288,20.37685082523));
#51830=CARTESIAN_POINT('Ctrl Pts',(56.9355662838206,28.5176834608775,20.3765743224425));
#51831=CARTESIAN_POINT('Ctrl Pts',(56.9332716411066,28.508558867405,20.3759715127447));
#51832=CARTESIAN_POINT('Ctrl Pts',(56.9320075501746,28.5036125982868,20.3756455217654));
#51833=CARTESIAN_POINT('Ctrl Pts',(56.9283509724295,28.4895303359028,20.3747194945795));
#51834=CARTESIAN_POINT('Ctrl Pts',(56.9259125379672,28.4804062594372,20.3741220152618));
#51835=CARTESIAN_POINT('Ctrl Pts',(56.9091127571718,28.419288739278,20.3701345279476));
#51836=CARTESIAN_POINT('Ctrl Pts',(56.8927109788618,28.3678739271519,20.3668515758046));
#51837=CARTESIAN_POINT('Ctrl Pts',(56.8112374451797,28.1442398491353,20.3526351668634));
#51838=CARTESIAN_POINT('Ctrl Pts',(56.724599330744,27.9808476377776,20.3423328029556));
#51839=CARTESIAN_POINT('Ctrl Pts',(56.586838811969,27.7902136253842,20.3281798200685));
#51840=CARTESIAN_POINT('Ctrl Pts',(56.555319642321,27.7499517490247,20.3250565253297));
#51841=CARTESIAN_POINT('Ctrl Pts',(56.5129218618315,27.6998826187298,20.3209691768479));
#51842=CARTESIAN_POINT('Ctrl Pts',(56.503432538321,27.688920921385,20.3200612300968));
#51843=CARTESIAN_POINT('Ctrl Pts',(56.4881009669051,27.6715958174595,20.3186045799908));
#51844=CARTESIAN_POINT('Ctrl Pts',(56.4823353007905,27.6651650992916,20.318059046068));
#51845=CARTESIAN_POINT('Ctrl Pts',(56.4718649232624,27.6536384922174,20.3170723004125));
#51846=CARTESIAN_POINT('Ctrl Pts',(56.4671750285736,27.6485292842532,20.3166317151307));
#51847=CARTESIAN_POINT('Ctrl Pts',(56.4560781486309,27.6365660950298,20.315592439666));
#51848=CARTESIAN_POINT('Ctrl Pts',(56.4496493056796,27.629732699891,20.3149928263584));
#51849=CARTESIAN_POINT('Ctrl Pts',(56.4307609273641,27.6099374194775,20.3132381181289));
#51850=CARTESIAN_POINT('Ctrl Pts',(56.4181743272363,27.5970985951557,20.3120775743221));
#51851=CARTESIAN_POINT('Ctrl Pts',(56.3007411756435,27.4805076173041,20.301326039478));
#51852=CARTESIAN_POINT('Ctrl Pts',(56.1848825816581,27.388534254254,20.2912179121016));
#51853=CARTESIAN_POINT('Ctrl Pts',(55.9535101994514,27.2434009298712,20.2721968691635));
#51854=CARTESIAN_POINT('Ctrl Pts',(55.8409643670657,27.1868242477141,20.2633846613646));
#51855=CARTESIAN_POINT('Ctrl Pts',(55.7092712227914,27.1355413253915,20.2540274837502));
#51856=CARTESIAN_POINT('Ctrl Pts',(55.6946411449234,27.1300413018901,20.2530008733104));
#51857=CARTESIAN_POINT('Ctrl Pts',(55.6738980439167,27.1225202012563,20.2515649186153));
#51858=CARTESIAN_POINT('Ctrl Pts',(55.6678380019933,27.120356051234,20.2511477533775));
#51859=CARTESIAN_POINT('Ctrl Pts',(55.6576113325546,27.1167596256042,20.2504478331459));
#51860=CARTESIAN_POINT('Ctrl Pts',(55.6534502744929,27.1153117731264,20.2501641783316));
#51861=CARTESIAN_POINT('Ctrl Pts',(55.6449321778437,27.1123794780715,20.2495858663123));
#51862=CARTESIAN_POINT('Ctrl Pts',(55.6405747484556,27.1108963126644,20.2492912839591));
#51863=CARTESIAN_POINT('Ctrl Pts',(55.6294282065591,27.1071452963251,20.2485408302524));
#51864=CARTESIAN_POINT('Ctrl Pts',(55.6226318805277,27.1048988571841,20.2480861940411));
#51865=CARTESIAN_POINT('Ctrl Pts',(55.5947184433502,27.095838797817,20.2462303846405));
#51866=CARTESIAN_POINT('Ctrl Pts',(55.5734995279226,27.089340873188,20.2448464278422));
#51867=CARTESIAN_POINT('Ctrl Pts',(55.387447378154,27.035744593043,20.2329082187872));
#51868=CARTESIAN_POINT('Ctrl Pts',(55.2172685546736,27.0097172402152,20.2232760400318));
#51869=CARTESIAN_POINT('Ctrl Pts',(54.9508300797814,27.0035928778312,20.2076289897623));
#51870=CARTESIAN_POINT('Ctrl Pts',(54.8557978286487,27.0082014617678,20.20194730633));
#51871=CARTESIAN_POINT('Ctrl Pts',(54.746148165588,27.0214083892458,20.1950902735904));
#51872=CARTESIAN_POINT('Ctrl Pts',(54.7308553741873,27.0234305816337,20.1941272574393));
#51873=CARTESIAN_POINT('Ctrl Pts',(54.7059336231978,27.0270206114352,20.1925462964937));
#51874=CARTESIAN_POINT('Ctrl Pts',(54.6962898166136,27.0284821023465,20.1919316798763));
#51875=CARTESIAN_POINT('Ctrl Pts',(54.6790472840467,27.0312246716884,20.190827525957));
#51876=CARTESIAN_POINT('Ctrl Pts',(54.6714444822628,27.0324791720783,20.1903388330641));
#51877=CARTESIAN_POINT('Ctrl Pts',(54.6553333007128,27.0352335839746,20.1892992581965));
#51878=CARTESIAN_POINT('Ctrl Pts',(54.6468270361667,27.0367447804964,20.1887480296168));
#51879=CARTESIAN_POINT('Ctrl Pts',(54.6240616895708,27.0409419400025,20.187266308807));
#51880=CARTESIAN_POINT('Ctrl Pts',(54.6098218639321,27.0437282654283,20.1863326678506));
#51881=CARTESIAN_POINT('Ctrl Pts',(54.5386592520432,27.0584606240599,20.1816317134885));
#51882=CARTESIAN_POINT('Ctrl Pts',(54.4822528125834,27.0727358396722,20.1777913281591));
#51883=CARTESIAN_POINT('Ctrl Pts',(54.3176181343566,27.122150465332,20.166234823831));
#51884=CARTESIAN_POINT('Ctrl Pts',(54.2116883187531,27.1641015009474,20.1583305280501));
#51885=CARTESIAN_POINT('Ctrl Pts',(54.0144788372994,27.262429985131,20.1429720384443));
#51886=CARTESIAN_POINT('Ctrl Pts',(53.9229963553846,27.3176001886033,20.1355486561141));
#51887=CARTESIAN_POINT('Ctrl Pts',(53.8233015978568,27.3892030519188,20.127416773094));
#51888=CARTESIAN_POINT('Ctrl Pts',(53.8103592670076,27.3987377157222,20.1263604304975));
#51889=CARTESIAN_POINT('Ctrl Pts',(53.7923397859005,27.412351822388,20.1248903577272));
#51890=CARTESIAN_POINT('Ctrl Pts',(53.7871655911813,27.4163009666524,20.1244683128819));
#51891=CARTESIAN_POINT('Ctrl Pts',(53.7788267234149,27.4227303478538,20.1237883869248));
#51892=CARTESIAN_POINT('Ctrl Pts',(53.7756501084085,27.4251949102557,20.1235294351904));
#51893=CARTESIAN_POINT('Ctrl Pts',(53.7690110635026,27.4303780139795,20.1229883967133));
#51894=CARTESIAN_POINT('Ctrl Pts',(53.76555013977,27.4330984446766,20.1227064501391));
#51895=CARTESIAN_POINT('Ctrl Pts',(53.7572332431891,27.439680531862,20.1220290632497));
#51896=CARTESIAN_POINT('Ctrl Pts',(53.7523861809491,27.4435534652799,20.1216344121271));
#51897=CARTESIAN_POINT('Ctrl Pts',(53.7418679603286,27.4520385133603,20.1207780953088));
#51898=CARTESIAN_POINT('Ctrl Pts',(53.736203899764,27.4566593330837,20.1203170224554));
#51899=CARTESIAN_POINT('Ctrl Pts',(53.7203382421365,27.4697486710161,20.1190252448566));
#51900=CARTESIAN_POINT('Ctrl Pts',(53.7101952925552,27.4782880754162,20.1181991009269));
#51901=CARTESIAN_POINT('Ctrl Pts',(53.6766920046685,27.5070703533618,20.1154663102282));
#51902=CARTESIAN_POINT('Ctrl Pts',(53.6537161201567,27.5277558286336,20.1135857041806));
#51903=CARTESIAN_POINT('Ctrl Pts',(53.5423986913421,27.6327625124005,20.1043872997839));
#51904=CARTESIAN_POINT('Ctrl Pts',(53.461444578748,27.7245426484481,20.0974042762455));
#51905=CARTESIAN_POINT('Ctrl Pts',(53.3210266894231,27.9167165245161,20.0835254858019));
#51906=CARTESIAN_POINT('Ctrl Pts',(53.2609553638323,28.016042182112,20.0766677079713));
#51907=CARTESIAN_POINT('Ctrl Pts',(53.2028733896335,28.134197832196,20.0684975556814));
#51908=CARTESIAN_POINT('Ctrl Pts',(53.1960688057421,28.1484662827926,20.0675110735903));
#51909=CARTESIAN_POINT('Ctrl Pts',(53.1852927200342,28.1717715007861,20.0658993017305));
#51910=CARTESIAN_POINT('Ctrl Pts',(53.1812173636708,28.1807596963884,20.0652775640902));
#51911=CARTESIAN_POINT('Ctrl Pts',(53.1740739224297,28.196830594306,20.0641655130332));
#51912=CARTESIAN_POINT('Ctrl Pts',(53.1709799124847,28.2039016067456,20.0636760921307));
#51913=CARTESIAN_POINT('Ctrl Pts',(53.1645360519804,28.2188641892993,20.062640094573));
#51914=CARTESIAN_POINT('Ctrl Pts',(53.1611958910269,28.2267597370135,20.0620932025368));
#51915=CARTESIAN_POINT('Ctrl Pts',(53.1524557791894,28.247796723616,20.0606353713992));
#51916=CARTESIAN_POINT('Ctrl Pts',(53.1471452342085,28.2609745494767,20.0597214582628));
#51917=CARTESIAN_POINT('Ctrl Pts',(53.1221930727145,28.3248519350917,20.0552871525848));
#51918=CARTESIAN_POINT('Ctrl Pts',(53.1044907314344,28.3762793554329,20.051703325191));
#51919=CARTESIAN_POINT('Ctrl Pts',(53.0333349164898,28.614165836027,20.0350527207555));
#51920=CARTESIAN_POINT('Ctrl Pts',(53.0051631110213,28.8070311647972,20.0212202968295));
#51921=CARTESIAN_POINT('Ctrl Pts',(53.0052502012793,29.0008961046522,20.0080399322459));
#51922=CARTESIAN_POINT('Ctrl Pts',(53.0052502025236,29.0008988702651,20.0080397442193));
#51923=CARTESIAN_POINT('Ctrl Pts',(53.0052629847114,29.0292647731376,20.0061112226866));
#51924=CARTESIAN_POINT('Ctrl Pts',(53.0058808240606,29.0576289395148,20.0042010851021));
#51925=CARTESIAN_POINT('Ctrl Pts',(53.0077894752773,29.1018729660331,20.001259313683));
#51926=CARTESIAN_POINT('Ctrl Pts',(53.0086657422133,29.1177658134764,20.0002102331456));
#51927=CARTESIAN_POINT('Ctrl Pts',(53.0101217043145,29.1394479590473,19.9987909340733));
#51928=CARTESIAN_POINT('Ctrl Pts',(53.010536603078,29.1452472347752,19.9984124844107));
#51929=CARTESIAN_POINT('Ctrl Pts',(53.0113048449,29.1553637816291,19.9977544310216));
#51930=CARTESIAN_POINT('Ctrl Pts',(53.0116469033244,29.1596818347597,19.9974742323081));
#51931=CARTESIAN_POINT('Ctrl Pts',(53.0123411150536,29.1680970848409,19.9969295342592));
#51932=CARTESIAN_POINT('Ctrl Pts',(53.0126918790685,29.1721943859476,19.9966649600227));
#51933=CARTESIAN_POINT('Ctrl Pts',(53.0134715559545,29.1809820030418,19.9960989133663));
#51934=CARTESIAN_POINT('Ctrl Pts',(53.0139044116136,29.1856719131389,19.9957976625808));
#51935=CARTESIAN_POINT('Ctrl Pts',(53.0150831042282,29.1979668420696,19.995010027922));
#51936=CARTESIAN_POINT('Ctrl Pts',(53.0158560454696,29.2055692726816,19.9945251269722));
#51937=CARTESIAN_POINT('Ctrl Pts',(53.0192362760699,29.237019247725,19.9925272761347));
#51938=CARTESIAN_POINT('Ctrl Pts',(53.0222300849177,29.2608243407843,19.9910343636161));
#51939=CARTESIAN_POINT('Ctrl Pts',(53.0304342745286,29.3177448556571,19.9874986109912));
#51940=CARTESIAN_POINT('Ctrl Pts',(53.0360513951564,29.3507948940656,19.9854733189229));
#51941=CARTESIAN_POINT('Ctrl Pts',(53.0438584337799,29.3906247340389,19.9830495052251));
#51942=CARTESIAN_POINT('Ctrl Pts',(53.045254455155,29.3975516712013,19.9826285985524));
#51943=CARTESIAN_POINT('Ctrl Pts',(53.0466870003186,29.404469884881,19.982208722643));
#51944=CARTESIAN_POINT('Ctrl Pts',(53.0466869979816,29.4044698735951,19.8236610414577));
#51945=CARTESIAN_POINT('Ctrl Pts',(53.0459258685407,29.4007941386882,19.8239060899399));
#51946=CARTESIAN_POINT('Ctrl Pts',(53.0451751118795,29.3971162423574,19.8241514621327));
#51947=CARTESIAN_POINT('Ctrl Pts',(53.0182529607406,29.2633003408038,19.8330856262503));
#51948=CARTESIAN_POINT('Ctrl Pts',(53.0051309262974,29.1308984294748,19.8421861286945));
#51949=CARTESIAN_POINT('Ctrl Pts',(53.0053684879735,28.8679477486202,19.8604895091017));
#51950=CARTESIAN_POINT('Ctrl Pts',(53.0182430481131,28.7380122936548,19.8696375241136));
#51951=CARTESIAN_POINT('Ctrl Pts',(53.046701492835,28.5951678610035,19.8792777975915));
#51952=CARTESIAN_POINT('Ctrl Pts',(53.0498810867118,28.580118615176,19.8802878517556));
#51953=CARTESIAN_POINT('Ctrl Pts',(53.0544905052521,28.559484897967,19.8816636385968));
#51954=CARTESIAN_POINT('Ctrl Pts',(53.0557708349192,28.5538680633545,19.8820372211867));
#51955=CARTESIAN_POINT('Ctrl Pts',(53.0580033015897,28.544266338487,19.8826741605567));
#51956=CARTESIAN_POINT('Ctrl Pts',(53.0589434059971,28.5402787295693,19.882938184349));
#51957=CARTESIAN_POINT('Ctrl Pts',(53.0609228923809,28.5319967365322,19.883485467669));
#51958=CARTESIAN_POINT('Ctrl Pts',(53.0619642629959,28.5277028833428,19.8837686021172));
#51959=CARTESIAN_POINT('Ctrl Pts',(53.0645179141907,28.5173241564827,19.8844515699688));
#51960=CARTESIAN_POINT('Ctrl Pts',(53.0660446505626,28.5112428176311,19.8848505852162));
#51961=CARTESIAN_POINT('Ctrl Pts',(53.0715030205004,28.4899269604195,19.8862454168152));
#51962=CARTESIAN_POINT('Ctrl Pts',(53.075586315137,28.4747313912378,19.8872329926328));
#51963=CARTESIAN_POINT('Ctrl Pts',(53.1019674911502,28.3809962898027,19.8932919810013));
#51964=CARTESIAN_POINT('Ctrl Pts',(53.1288924652618,28.3038300292542,19.8981377023729));
#51965=CARTESIAN_POINT('Ctrl Pts',(53.1691801757111,28.2077671066386,19.9042347667852));
#51966=CARTESIAN_POINT('Ctrl Pts',(53.1782361297719,28.1871589276696,19.9055465772683));
#51967=CARTESIAN_POINT('Ctrl Pts',(53.2546931575205,28.0208693526359,19.9161933621505));
#51968=CARTESIAN_POINT('Ctrl Pts',(53.3390956026355,27.8836741638707,19.9254257294014));
#51969=CARTESIAN_POINT('Ctrl Pts',(53.4537358026589,27.7395821108431,19.9367752997941));
#51970=CARTESIAN_POINT('Ctrl Pts',(53.4687785380385,27.7213495456193,19.9382441909977));
#51971=CARTESIAN_POINT('Ctrl Pts',(53.4902642633129,27.6962307326188,19.9403166454428));
#51972=CARTESIAN_POINT('Ctrl Pts',(53.4964378593553,27.6891158779021,19.9409092840253));
#51973=CARTESIAN_POINT('Ctrl Pts',(53.5078462153795,27.6761547587684,19.9419994121569));
#51974=CARTESIAN_POINT('Ctrl Pts',(53.5130655476693,27.6702951187148,19.942496259432));
#51975=CARTESIAN_POINT('Ctrl Pts',(53.5237233945691,27.6584709851919,19.9435071042012));
#51976=CARTESIAN_POINT('Ctrl Pts',(53.5291638048277,27.6525084055346,19.9440211758571));
#51977=CARTESIAN_POINT('Ctrl Pts',(53.5427083815469,27.6378435824265,19.9452963961772));
#51978=CARTESIAN_POINT('Ctrl Pts',(53.5508543778261,27.6291805652089,19.9460593098843));
#51979=CARTESIAN_POINT('Ctrl Pts',(53.5817358081406,27.5969219974693,19.9489369371594));
#51980=CARTESIAN_POINT('Ctrl Pts',(53.6049729793758,27.5738160703316,19.9510731690277));
#51981=CARTESIAN_POINT('Ctrl Pts',(53.6647472130576,27.5172384302366,19.9565002863236));
#51982=CARTESIAN_POINT('Ctrl Pts',(53.7019804112189,27.4845375734769,19.9598207362227));
#51983=CARTESIAN_POINT('Ctrl Pts',(53.8216524980202,27.387080959678,19.9703048514465));
#51984=CARTESIAN_POINT('Ctrl Pts',(53.9079986269628,27.3274150563049,19.9776170202001));
#51985=CARTESIAN_POINT('Ctrl Pts',(54.0461432857822,27.2472296471289,19.9887431184047));
#51986=CARTESIAN_POINT('Ctrl Pts',(54.0947847259439,27.2216208724008,19.9925596269708));
#51987=CARTESIAN_POINT('Ctrl Pts',(54.1909277319891,27.1759715288244,19.9998434906164));
#51988=CARTESIAN_POINT('Ctrl Pts',(54.2382742689395,27.1556972309014,20.0033149411549));
#51989=CARTESIAN_POINT('Ctrl Pts',(54.294648297656,27.1340993097724,20.00727360884));
#51990=CARTESIAN_POINT('Ctrl Pts',(54.3029614886335,27.1309778678669,20.0078529987519));
#51991=CARTESIAN_POINT('Ctrl Pts',(54.316470739234,27.1260080787655,20.0087871394955));
#51992=CARTESIAN_POINT('Ctrl Pts',(54.3216539990172,27.12412562364,20.0091437990098));
#51993=CARTESIAN_POINT('Ctrl Pts',(54.3309019296265,27.120810305489,20.0097769442371));
#51994=CARTESIAN_POINT('Ctrl Pts',(54.3349634970455,27.1193690987681,20.010053911679));
#51995=CARTESIAN_POINT('Ctrl Pts',(54.3437819027651,27.1162721165611,20.0106528607775));
#51996=CARTESIAN_POINT('Ctrl Pts',(54.3485403462966,27.1146211916633,20.0109745580367));
#51997=CARTESIAN_POINT('Ctrl Pts',(54.3619372683264,27.1100299526725,20.0118761935313));
#51998=CARTESIAN_POINT('Ctrl Pts',(54.3705898746535,27.1071308204293,20.0124537825494));
#51999=CARTESIAN_POINT('Ctrl Pts',(54.4240486134709,27.0896260988569,20.0159948954767));
#52000=CARTESIAN_POINT('Ctrl Pts',(54.4693446541612,27.076551499702,20.0188770098322));
#52001=CARTESIAN_POINT('Ctrl Pts',(54.6310908631257,27.0360139632071,20.0288921244463));
#52002=CARTESIAN_POINT('Ctrl Pts',(54.7495045370738,27.0174281459756,20.0357375576361));
#52003=CARTESIAN_POINT('Ctrl Pts',(54.9859774136273,27.0018501061328,20.0495517046744));
#52004=CARTESIAN_POINT('Ctrl Pts',(55.1035142356001,27.0044852616821,20.0564920526417));
#52005=CARTESIAN_POINT('Ctrl Pts',(55.2358494954615,27.0191787683284,20.0647544914739));
#52006=CARTESIAN_POINT('Ctrl Pts',(55.2515480954056,27.0211111022326,20.0657415345642));
#52007=CARTESIAN_POINT('Ctrl Pts',(55.2770044300003,27.0245523143743,20.0673540422416));
#52008=CARTESIAN_POINT('Ctrl Pts',(55.2867770511817,27.0259473334792,20.0679759492637));
#52009=CARTESIAN_POINT('Ctrl Pts',(55.3041716460096,27.0285622633218,20.0690881889367));
#52010=CARTESIAN_POINT('Ctrl Pts',(55.3117977024553,27.0297539925529,20.0695776279258));
#52011=CARTESIAN_POINT('Ctrl Pts',(55.3278774565582,27.0323624809046,20.070613544683));
#52012=CARTESIAN_POINT('Ctrl Pts',(55.3363293039312,27.0337895258566,20.0711603371094));
#52013=CARTESIAN_POINT('Ctrl Pts',(55.3587584929024,27.0377254106278,20.0726176210716));
#52014=CARTESIAN_POINT('Ctrl Pts',(55.3727184849025,27.0403290750367,20.0735310826924));
#52015=CARTESIAN_POINT('Ctrl Pts',(55.4399073690834,27.0536042974031,20.0779595184352));
#52016=CARTESIAN_POINT('Ctrl Pts',(55.4927090899632,27.066295900276,20.0815377236312));
#52017=CARTESIAN_POINT('Ctrl Pts',(55.6465079757681,27.1099718054639,20.0922583970074));
#52018=CARTESIAN_POINT('Ctrl Pts',(55.7456303249572,27.1468378458137,20.099565152123));
#52019=CARTESIAN_POINT('Ctrl Pts',(55.9497623905248,27.2417982525519,20.1152520962225));
#52020=CARTESIAN_POINT('Ctrl Pts',(56.0534226525224,27.3018751965146,20.1236163459108));
#52021=CARTESIAN_POINT('Ctrl Pts',(56.1640324977419,27.3800286282452,20.1325862624167));
#52022=CARTESIAN_POINT('Ctrl Pts',(56.1768712097706,27.3893314759745,20.1336278908278));
#52023=CARTESIAN_POINT('Ctrl Pts',(56.1947934239375,27.4026465244753,20.1350810788089));
#52024=CARTESIAN_POINT('Ctrl Pts',(56.1999700056604,27.4065316319514,20.1355007071317));
#52025=CARTESIAN_POINT('Ctrl Pts',(56.208644253358,27.4131080358804,20.1362035613062));
#52026=CARTESIAN_POINT('Ctrl Pts',(56.2121520325748,27.4157858452376,20.1364877037132));
#52027=CARTESIAN_POINT('Ctrl Pts',(56.2192920134908,27.4212740457829,20.1370658454745));
#52028=CARTESIAN_POINT('Ctrl Pts',(56.222923440658,27.4240853728696,20.1373597765682));
#52029=CARTESIAN_POINT('Ctrl Pts',(56.2321522811287,27.4312811368237,20.1381065678778));
#52030=CARTESIAN_POINT('Ctrl Pts',(56.237736077697,27.4356830496389,20.1385582165152));
#52031=CARTESIAN_POINT('Ctrl Pts',(56.2603378735922,27.4536976635929,20.1403861572467));
#52032=CARTESIAN_POINT('Ctrl Pts',(56.2771565260448,27.467559537541,20.1417458755702));
#52033=CARTESIAN_POINT('Ctrl Pts',(56.3209540927002,27.5048793766787,20.1452956277409));
#52034=CARTESIAN_POINT('Ctrl Pts',(56.3475362550277,27.528792423374,20.1474593213889));
#52035=CARTESIAN_POINT('Ctrl Pts',(56.5009307203715,27.6744324124099,20.1601003662825));
#52036=CARTESIAN_POINT('Ctrl Pts',(56.6118467369842,27.8117744695597,20.1699611155816));
#52037=CARTESIAN_POINT('Ctrl Pts',(56.7339688655553,28.012151320056,20.1840059464739));
#52038=CARTESIAN_POINT('Ctrl Pts',(56.762362635997,28.0637468323247,20.1875884597438));
#52039=CARTESIAN_POINT('Ctrl Pts',(56.7950785964096,28.1299737882219,20.1921860363399));
#52040=CARTESIAN_POINT('Ctrl Pts',(56.8015731052074,28.1435030042143,20.1931251338487));
#52041=CARTESIAN_POINT('Ctrl Pts',(56.8116475298905,28.1651114754298,20.1946254377782));
#52042=CARTESIAN_POINT('Ctrl Pts',(56.8153275635434,28.1731436315659,20.1951832072608));
#52043=CARTESIAN_POINT('Ctrl Pts',(56.8221068186365,28.1882036604399,20.1962292909067));
#52044=CARTESIAN_POINT('Ctrl Pts',(56.8252190537049,28.1952255230493,20.196717150463));
#52045=CARTESIAN_POINT('Ctrl Pts',(56.8320750937027,28.2109385546904,20.1978091884106));
#52046=CARTESIAN_POINT('Ctrl Pts',(56.8357977416376,28.2196386989535,20.1984140696041));
#52047=CARTESIAN_POINT('Ctrl Pts',(56.8465656443678,28.2453077068345,20.2001995772363));
#52048=CARTESIAN_POINT('Ctrl Pts',(56.8534383696564,28.2623474334278,20.201385948705));
#52049=CARTESIAN_POINT('Ctrl Pts',(56.9118076517027,28.4130317956587,20.2118898116477));
#52050=CARTESIAN_POINT('Ctrl Pts',(56.9489971670341,28.551741808585,20.2216916776208));
#52051=CARTESIAN_POINT('Ctrl Pts',(56.9909458957835,28.821246522897,20.2406786473538));
#52052=CARTESIAN_POINT('Ctrl Pts',(56.9983533526711,28.9509313242624,20.249777392004));
#52053=CARTESIAN_POINT('Ctrl Pts',(56.9925059845408,29.0958407620512,20.2593769543132));
#52054=CARTESIAN_POINT('Ctrl Pts',(56.9917051713398,29.1112479001567,20.2603901055058));
#52055=CARTESIAN_POINT('Ctrl Pts',(56.9903595130661,29.1324002694528,20.2617693568444));
#52056=CARTESIAN_POINT('Ctrl Pts',(56.9899683978047,29.1381542627691,20.2621433580583));
#52057=CARTESIAN_POINT('Ctrl Pts',(56.989256645171,29.1479944609557,20.2627808265858));
#52058=CARTESIAN_POINT('Ctrl Pts',(56.9889483614221,29.1520814819885,20.2630449632698));
#52059=CARTESIAN_POINT('Ctrl Pts',(56.9882816754148,29.160571017478,20.2635922786538));
#52060=CARTESIAN_POINT('Ctrl Pts',(56.9879212452285,29.1649733178663,20.2638753332722));
#52061=CARTESIAN_POINT('Ctrl Pts',(56.9870144060123,29.1756147409497,20.2645577807351));
#52062=CARTESIAN_POINT('Ctrl Pts',(56.9864532241826,29.1818526260368,20.2649563585303));
#52063=CARTESIAN_POINT('Ctrl Pts',(56.9843832755523,29.2037074847165,20.2663479884683));
#52064=CARTESIAN_POINT('Ctrl Pts',(56.9827196030883,29.2193096784319,20.2673328503376));
#52065=CARTESIAN_POINT('Ctrl Pts',(56.9713135097276,29.315498945145,20.2733602891634));
#52066=CARTESIAN_POINT('Ctrl Pts',(56.9568425362784,29.3954577358452,20.2781797016291));
#52067=CARTESIAN_POINT('Ctrl Pts',(56.9288616780554,29.5097559755924,20.2850685553799));
#52068=CARTESIAN_POINT('Ctrl Pts',(56.9192161058482,29.5449478334186,20.2871892957999));
#52069=CARTESIAN_POINT('Ctrl Pts',(56.8662496329642,29.7192883846498,20.2977720079935));
#52070=CARTESIAN_POINT('Ctrl Pts',(56.8087433972027,29.8536420547964,20.3062141603725));
#52071=CARTESIAN_POINT('Ctrl Pts',(56.7253128843831,30.0014490120412,20.3166662730501));
#52072=CARTESIAN_POINT('Ctrl Pts',(56.7131276657345,30.0221537051854,20.3181580151639));
#52073=CARTESIAN_POINT('Ctrl Pts',(56.695480112871,30.0509375084443,20.3202734883446));
#52074=CARTESIAN_POINT('Ctrl Pts',(56.6903276368519,30.0592048595698,20.3208860207876));
#52075=CARTESIAN_POINT('Ctrl Pts',(56.6812560536497,30.073525800752,20.3219558343948));
#52076=CARTESIAN_POINT('Ctrl Pts',(56.6773642613603,30.0795965428431,20.3224121088525));
#52077=CARTESIAN_POINT('Ctrl Pts',(56.6691589362793,30.0922444195437,20.3233686077197));
#52078=CARTESIAN_POINT('Ctrl Pts',(56.6648392558706,30.0988173987543,20.3238690543218));
#52079=CARTESIAN_POINT('Ctrl Pts',(56.6544773036228,30.1143831439354,20.3250623034697));
#52080=CARTESIAN_POINT('Ctrl Pts',(56.6484004684786,30.1233524948079,20.3257563892084));
#52081=CARTESIAN_POINT('Ctrl Pts',(56.6276141130209,30.1535010984437,20.3281118236163));
#52082=CARTESIAN_POINT('Ctrl Pts',(56.6125675880513,30.1744437646563,20.3297858323143));
#52083=CARTESIAN_POINT('Ctrl Pts',(56.575545901197,30.2239196757102,20.333834235261));
#52084=CARTESIAN_POINT('Ctrl Pts',(56.553196342446,30.2521601793398,20.3362224441773));
#52085=CARTESIAN_POINT('Ctrl Pts',(56.4009255932269,30.4342141485875,20.3521396694851));
#52086=CARTESIAN_POINT('Ctrl Pts',(56.2491503754633,30.5681722070565,20.3665418677768));
#52087=CARTESIAN_POINT('Ctrl Pts',(56.0504041094137,30.6961459657168,20.3825274499051));
#52088=CARTESIAN_POINT('Ctrl Pts',(56.0203897840854,30.7143701390975,20.3848701817045));
#52089=CARTESIAN_POINT('Ctrl Pts',(55.9823828814955,30.7360952065576,20.3877348110478));
#52090=CARTESIAN_POINT('Ctrl Pts',(55.9748296440348,30.74034762727,20.3882991967866));
#52091=CARTESIAN_POINT('Ctrl Pts',(55.9628863538466,30.7469694653301,20.3891836154373));
#52092=CARTESIAN_POINT('Ctrl Pts',(55.9585148278326,30.7493718213574,20.3895056588589));
#52093=CARTESIAN_POINT('Ctrl Pts',(55.9503800886817,30.7538025900046,20.3901017635972));
#52094=CARTESIAN_POINT('Ctrl Pts',(55.9466193974751,30.755835286825,20.3903760846715));
#52095=CARTESIAN_POINT('Ctrl Pts',(55.9379505793471,30.760484935931,20.3910055683735));
#52096=CARTESIAN_POINT('Ctrl Pts',(55.9330380233506,30.7630934597205,20.3913602009648));
#52097=CARTESIAN_POINT('Ctrl Pts',(55.9177672883943,30.7711203840502,20.3924563089915));
#52098=CARTESIAN_POINT('Ctrl Pts',(55.9073721250756,30.7764684214648,20.3931935458831));
#52099=CARTESIAN_POINT('Ctrl Pts',(55.8036874426749,30.8286638687452,20.4004648611885));
#52100=CARTESIAN_POINT('Ctrl Pts',(55.7068900351237,30.8682177601293,20.4066010757966));
#52101=CARTESIAN_POINT('Ctrl Pts',(55.4482520227733,30.9509035461319,20.4224142989559));
#52102=CARTESIAN_POINT('Ctrl Pts',(55.2833305211374,30.9815833485493,20.4319958236938));
#52103=CARTESIAN_POINT('Ctrl Pts',(55.0958396954895,30.9925539976236,20.4435797620111));
#52104=CARTESIAN_POINT('Ctrl Pts',(55.0751429273717,30.9934417904447,20.444866705357));
#52105=CARTESIAN_POINT('Ctrl Pts',(55.0431754482489,30.9943145069531,20.4468688402119));
#52106=CARTESIAN_POINT('Ctrl Pts',(55.0319120194958,30.9945265319651,20.4475770202546));
#52107=CARTESIAN_POINT('Ctrl Pts',(55.0127813362699,30.9947245635323,20.4487847628381));
#52108=CARTESIAN_POINT('Ctrl Pts',(55.0049147728055,30.9947594564398,20.4492827988564));
#52109=CARTESIAN_POINT('Ctrl Pts',(54.9890011602543,30.9947359084866,20.4502932396808));
#52110=CARTESIAN_POINT('Ctrl Pts',(54.9809542655453,30.9946753059029,20.4508057022784));
#52111=CARTESIAN_POINT('Ctrl Pts',(54.9611365648998,30.9944061244919,20.4520716336622));
#52112=CARTESIAN_POINT('Ctrl Pts',(54.949366936242,30.9941420308167,20.4528268113612));
#52113=CARTESIAN_POINT('Ctrl Pts',(54.9057023614303,30.9927754535424,20.45564129832));
#52114=CARTESIAN_POINT('Ctrl Pts',(54.8738343612364,30.9910118258572,20.4577209216516));
#52115=CARTESIAN_POINT('Ctrl Pts',(54.7943769146838,30.9846992887201,20.4629728670991));
#52116=CARTESIAN_POINT('Ctrl Pts',(54.7468848436522,30.9792029308532,20.466172371802));
#52117=CARTESIAN_POINT('Ctrl Pts',(54.6034165452111,30.9573509307911,20.4760160636148));
#52118=CARTESIAN_POINT('Ctrl Pts',(54.5084030589648,30.9356731844385,20.4827872068433));
#52119=CARTESIAN_POINT('Ctrl Pts',(54.3129537807286,30.8757578373116,20.4970350918243));
#52120=CARTESIAN_POINT('Ctrl Pts',(54.213232674389,30.8361649258113,20.5044918611154));
#52121=CARTESIAN_POINT('Ctrl Pts',(54.1027676650897,30.7816451675347,20.5126528816709));
#52122=CARTESIAN_POINT('Ctrl Pts',(54.0884553190085,30.7743651538878,20.513708035996));
#52123=CARTESIAN_POINT('Ctrl Pts',(54.0684690556011,30.7638934178564,20.5151767450756));
#52124=CARTESIAN_POINT('Ctrl Pts',(54.0627209109932,30.7608457632865,20.5155985945279));
#52125=CARTESIAN_POINT('Ctrl Pts',(54.0534452933166,30.7558695594842,20.516278290354));
#52126=CARTESIAN_POINT('Ctrl Pts',(54.0499086168348,30.7539584051512,20.516537205984));
#52127=CARTESIAN_POINT('Ctrl Pts',(54.0425111560367,30.7499320145241,20.5170782145469));
#52128=CARTESIAN_POINT('Ctrl Pts',(54.0386515500382,30.7478146641589,20.5173601671325));
#52129=CARTESIAN_POINT('Ctrl Pts',(54.0291831062738,30.7425794961207,20.5180511547974));
#52130=CARTESIAN_POINT('Ctrl Pts',(54.0235821879486,30.7394473261514,20.5184592898812));
#52131=CARTESIAN_POINT('Ctrl Pts',(54.0115154156832,30.7326226444023,20.5193374840467));
#52132=CARTESIAN_POINT('Ctrl Pts',(54.0050548985863,30.7289208340657,20.5198069774494));
#52133=CARTESIAN_POINT('Ctrl Pts',(53.9868414760145,30.7183488269894,20.5211290514063));
#52134=CARTESIAN_POINT('Ctrl Pts',(53.9751377245541,30.7113942340231,20.5219768037957));
#52135=CARTESIAN_POINT('Ctrl Pts',(53.9360720882025,30.6876361934612,20.5248035944069));
#52136=CARTESIAN_POINT('Ctrl Pts',(53.9090437268382,30.6702913396737,20.5267545614378));
#52137=CARTESIAN_POINT('Ctrl Pts',(53.8253695243302,30.6136971780551,20.532817428938));
#52138=CARTESIAN_POINT('Ctrl Pts',(53.7703296525654,30.5721600672652,20.5368409028858));
#52139=CARTESIAN_POINT('Ctrl Pts',(53.5969867763769,30.42665936361,20.5500000806916));
#52140=CARTESIAN_POINT('Ctrl Pts',(53.488841491452,30.3115627843558,20.5590669790425));
#52141=CARTESIAN_POINT('Ctrl Pts',(53.3811609625366,30.1657436493565,20.5702371379898));
#52142=CARTESIAN_POINT('Ctrl Pts',(53.3673187463974,30.1462765520836,20.5717212770388));
#52143=CARTESIAN_POINT('Ctrl Pts',(53.3484874648867,30.1187597556868,20.5738116861549));
#52144=CARTESIAN_POINT('Ctrl Pts',(53.3432007384361,30.1109154992853,20.5744067736246));
#52145=CARTESIAN_POINT('Ctrl Pts',(53.3336252649365,30.0964873648291,20.5754999805151));
#52146=CARTESIAN_POINT('Ctrl Pts',(53.3293192221399,30.0899151501465,20.5759974439459));
#52147=CARTESIAN_POINT('Ctrl Pts',(53.3206756167565,30.0765510303496,20.577008064401));
#52148=CARTESIAN_POINT('Ctrl Pts',(53.3163401628376,30.0697579421131,20.5775212870127));
#52149=CARTESIAN_POINT('Ctrl Pts',(53.3057428417171,30.0529293257487,20.5787916144061));
#52150=CARTESIAN_POINT('Ctrl Pts',(53.2995289149833,30.0428641150754,20.5795504546087));
#52151=CARTESIAN_POINT('Ctrl Pts',(53.2766744528706,30.0050974510196,20.5823946803126));
#52152=CARTESIAN_POINT('Ctrl Pts',(53.260619076799,29.9770494513216,20.5845009424396));
#52153=CARTESIAN_POINT('Ctrl Pts',(53.2221335836362,29.9058597807356,20.5898350888148));
#52154=CARTESIAN_POINT('Ctrl Pts',(53.2005871599024,29.862266630887,20.5930912590761));
#52155=CARTESIAN_POINT('Ctrl Pts',(53.1210421906139,29.6853331690329,20.6062589913965));
#52156=CARTESIAN_POINT('Ctrl Pts',(53.0761357395278,29.5466871649761,20.6165112064369));
#52157=CARTESIAN_POINT('Ctrl Pts',(53.0466869978243,29.4044698728352,20.6265291208673));
#52158=CARTESIAN_POINT('Origin',(55.,29.,3.45145488139523));
#52159=CARTESIAN_POINT('',(53.0466869980088,29.4044698737264,21.5853976382171));
#52160=CARTESIAN_POINT('',(53.0466869889941,29.4044698301913,21.4261018347979));
#52161=CARTESIAN_POINT('',(53.0466869980082,29.4044698737233,3.45145488139523));
#52162=CARTESIAN_POINT('Ctrl Pts',(53.0466869980088,29.4044698737264,21.5853976382171));
#52163=CARTESIAN_POINT('Ctrl Pts',(53.0475866729437,29.4088146886609,21.5851174197649));
#52164=CARTESIAN_POINT('Ctrl Pts',(53.0485008375208,29.4131564689104,21.5848367448388));
#52165=CARTESIAN_POINT('Ctrl Pts',(53.0510413850145,29.4250261089356,21.5840676230934));
#52166=CARTESIAN_POINT('Ctrl Pts',(53.0526968760825,29.4325475893758,21.583578258594));
#52167=CARTESIAN_POINT('Ctrl Pts',(53.0565387818416,29.4495335484862,21.5824685170729));
#52168=CARTESIAN_POINT('Ctrl Pts',(53.0587508439812,29.458991967766,21.5818473329122));
#52169=CARTESIAN_POINT('Ctrl Pts',(53.0646230954277,29.4832987330159,21.5802424594353));
#52170=CARTESIAN_POINT('Ctrl Pts',(53.0683850609454,29.498121605463,21.5792555457274));
#52171=CARTESIAN_POINT('Ctrl Pts',(53.0956441761513,29.6005723596881,21.5723758036104));
#52172=CARTESIAN_POINT('Ctrl Pts',(53.1249218596305,29.6865392346039,21.5662975730865));
#52173=CARTESIAN_POINT('Ctrl Pts',(53.1882623848679,29.8378626369893,21.5550572670715));
#52174=CARTESIAN_POINT('Ctrl Pts',(53.2202905530021,29.9039028044674,21.5499526866739));
#52175=CARTESIAN_POINT('Ctrl Pts',(53.2883615924447,30.0265482942105,21.5401760873784));
#52176=CARTESIAN_POINT('Ctrl Pts',(53.3237688596617,30.0834007853545,21.5355117692802));
#52177=CARTESIAN_POINT('Ctrl Pts',(53.3924546143605,30.1822348132552,21.527268869493));
#52178=CARTESIAN_POINT('Ctrl Pts',(53.4246937558834,30.2248643451385,21.5236648751646));
#52179=CARTESIAN_POINT('Ctrl Pts',(53.4646133103848,30.2734617263761,21.5195439456683));
#52180=CARTESIAN_POINT('Ctrl Pts',(53.4706700751721,30.2807291066709,21.5189273642788));
#52181=CARTESIAN_POINT('Ctrl Pts',(53.4800769303661,30.2918542962245,21.5179833345641));
#52182=CARTESIAN_POINT('Ctrl Pts',(53.4833904253468,30.2957426672599,21.5176533590854));
#52183=CARTESIAN_POINT('Ctrl Pts',(53.4895224920075,30.3028828719338,21.5170474451264));
#52184=CARTESIAN_POINT('Ctrl Pts',(53.4923366364015,30.3061383015728,21.5167712058849));
#52185=CARTESIAN_POINT('Ctrl Pts',(53.4987189830961,30.3134733512336,21.5161488023784));
#52186=CARTESIAN_POINT('Ctrl Pts',(53.5022932850605,30.3175475451772,21.5158030929373));
#52187=CARTESIAN_POINT('Ctrl Pts',(53.5129160831282,30.3295569309571,21.5147838764607));
#52188=CARTESIAN_POINT('Ctrl Pts',(53.5200114849164,30.3374506403257,21.5141137181987));
#52189=CARTESIAN_POINT('Ctrl Pts',(53.5856367652806,30.4092976588884,21.5080077977972));
#52190=CARTESIAN_POINT('Ctrl Pts',(53.6482224551423,30.4694368291067,21.5028491131765));
#52191=CARTESIAN_POINT('Ctrl Pts',(53.8361286121852,30.6277956045964,21.4884533435434));
#52192=CARTESIAN_POINT('Ctrl Pts',(53.9695358952056,30.7153593442868,21.4794101365334));
#52193=CARTESIAN_POINT('Ctrl Pts',(54.1378952152832,30.7990675759546,21.4680253646136));
#52194=CARTESIAN_POINT('Ctrl Pts',(54.1641438568256,30.8114119320441,21.4662529701945));
#52195=CARTESIAN_POINT('Ctrl Pts',(54.210432358446,30.8319603976711,21.4631253405386));
#52196=CARTESIAN_POINT('Ctrl Pts',(54.2303543107103,30.8404188152807,21.4617786124758));
#52197=CARTESIAN_POINT('Ctrl Pts',(54.2597368819936,30.8523334978606,21.4597896198253));
#52198=CARTESIAN_POINT('Ctrl Pts',(54.2690927592634,30.8560451154775,21.4591558974024));
#52199=CARTESIAN_POINT('Ctrl Pts',(54.2857219773621,30.8624969458554,21.4580286338037));
#52200=CARTESIAN_POINT('Ctrl Pts',(54.2929840471148,30.8652657737004,21.4575360567882));
#52201=CARTESIAN_POINT('Ctrl Pts',(54.308108179015,30.8709311775209,21.456509508502));
#52202=CARTESIAN_POINT('Ctrl Pts',(54.3159726680144,30.8738207941411,21.4559753180964));
#52203=CARTESIAN_POINT('Ctrl Pts',(54.3363891202137,30.8811766689238,21.4545874194387));
#52204=CARTESIAN_POINT('Ctrl Pts',(54.3489678786778,30.8855668172432,21.4537312256197));
#52205=CARTESIAN_POINT('Ctrl Pts',(54.3999095468147,30.9027756086774,21.4502587846134));
#52206=CARTESIAN_POINT('Ctrl Pts',(54.4386120410212,30.9145513149261,21.4476089489539));
#52207=CARTESIAN_POINT('Ctrl Pts',(54.6669542790494,30.9765083331097,21.4318971128434));
#52208=CARTESIAN_POINT('Ctrl Pts',(54.8627945184981,30.999663148227,21.4179627900108));
#52209=CARTESIAN_POINT('Ctrl Pts',(55.1136080505873,30.992266951694,21.4007642780754));
#52210=CARTESIAN_POINT('Ctrl Pts',(55.1683345292068,30.9883910749464,21.3970620342585));
#52211=CARTESIAN_POINT('Ctrl Pts',(55.2322586958507,30.9812050266889,21.3928468493298));
#52212=CARTESIAN_POINT('Ctrl Pts',(55.2416733086971,30.9800786549909,21.3922288572349));
#52213=CARTESIAN_POINT('Ctrl Pts',(55.2561522353545,30.9782415775427,21.3912831313436));
#52214=CARTESIAN_POINT('Ctrl Pts',(55.261222293697,30.9775784741657,21.3909528564705));
#52215=CARTESIAN_POINT('Ctrl Pts',(55.2705541975896,30.9763214575533,21.3903466613938));
#52216=CARTESIAN_POINT('Ctrl Pts',(55.2748166546953,30.9757332523321,21.3900704383363));
#52217=CARTESIAN_POINT('Ctrl Pts',(55.2844381566664,30.9743737766701,21.3894484073221));
#52218=CARTESIAN_POINT('Ctrl Pts',(55.2897959767613,30.973594479238,21.3891030517513));
#52219=CARTESIAN_POINT('Ctrl Pts',(55.305621128299,30.9712268701544,21.3880858542176));
#52220=CARTESIAN_POINT('Ctrl Pts',(55.3160792560108,30.9695770010663,21.3874173413406));
#52221=CARTESIAN_POINT('Ctrl Pts',(55.4093491075843,30.9541007497376,21.3814844312317));
#52222=CARTESIAN_POINT('Ctrl Pts',(55.4912349431084,30.9351403653771,21.3764797168246));
#52223=CARTESIAN_POINT('Ctrl Pts',(55.7195727714648,30.8668338603714,21.3625016573911));
#52224=CARTESIAN_POINT('Ctrl Pts',(55.8618131388206,30.8055833633758,21.3537264356013));
#52225=CARTESIAN_POINT('Ctrl Pts',(56.024175401637,30.7120695261921,21.3424343371581));
#52226=CARTESIAN_POINT('Ctrl Pts',(56.0523667046824,30.694886857151,21.3404247528584));
#52227=CARTESIAN_POINT('Ctrl Pts',(56.1003930862474,30.6639544007427,21.3369053769586));
#52228=CARTESIAN_POINT('Ctrl Pts',(56.1204293606411,30.6505293581636,21.3354071073224));
#52229=CARTESIAN_POINT('Ctrl Pts',(56.1488730299327,30.6307144511484,21.3332340089243));
#52230=CARTESIAN_POINT('Ctrl Pts',(56.1574812796662,30.6246156285403,21.3325701232361));
#52231=CARTESIAN_POINT('Ctrl Pts',(56.1723823672207,30.6138798720346,21.3314098356442));
#52232=CARTESIAN_POINT('Ctrl Pts',(56.1786971340212,30.6092736621721,21.3309146150367));
#52233=CARTESIAN_POINT('Ctrl Pts',(56.1916371949081,30.5997177097605,21.3298924691774));
#52234=CARTESIAN_POINT('Ctrl Pts',(56.198259096259,30.5947636470875,21.329365383029));
#52235=CARTESIAN_POINT('Ctrl Pts',(56.2150709093343,30.5820223515973,21.3280168008159));
#52236=CARTESIAN_POINT('Ctrl Pts',(56.2252167556231,30.574177856771,21.3271930794357));
#52237=CARTESIAN_POINT('Ctrl Pts',(56.2640187489987,30.5435748347311,21.3240040339419));
#52238=CARTESIAN_POINT('Ctrl Pts',(56.2921207259121,30.5201284180012,21.32161163995));
#52239=CARTESIAN_POINT('Ctrl Pts',(56.4701012857083,30.3631310161828,21.305901274376));
#52240=CARTESIAN_POINT('Ctrl Pts',(56.5997206967542,30.2083822667965,21.2916410916346));
#52241=CARTESIAN_POINT('Ctrl Pts',(56.7326947913602,29.9898664933802,21.2741056128495));
#52242=CARTESIAN_POINT('Ctrl Pts',(56.7593922637672,29.9415980980176,21.2703827649737));
#52243=CARTESIAN_POINT('Ctrl Pts',(56.7883043616662,29.8837902469877,21.2661472993053));
#52244=CARTESIAN_POINT('Ctrl Pts',(56.792490413267,29.8752689972314,21.2655285026119));
#52245=CARTESIAN_POINT('Ctrl Pts',(56.798838356384,29.8621103763271,21.2645818091744));
#52246=CARTESIAN_POINT('Ctrl Pts',(56.8010434431125,29.8574941695458,21.2642513634029));
#52247=CARTESIAN_POINT('Ctrl Pts',(56.8050704371073,29.8489798543156,21.2636450072715));
#52248=CARTESIAN_POINT('Ctrl Pts',(56.8068974844995,29.845084349113,21.2633687928649));
#52249=CARTESIAN_POINT('Ctrl Pts',(56.8109937399303,29.8362765776634,21.2627469720233));
#52250=CARTESIAN_POINT('Ctrl Pts',(56.8132555705126,29.8313609794026,21.262401816593));
#52251=CARTESIAN_POINT('Ctrl Pts',(56.8198774729612,29.8168141249134,21.2613857605827));
#52252=CARTESIAN_POINT('Ctrl Pts',(56.8241810917021,29.807157164007,21.2607181779785));
#52253=CARTESIAN_POINT('Ctrl Pts',(56.8684164559205,29.7057355777539,21.2537745422634));
#52254=CARTESIAN_POINT('Ctrl Pts',(56.9014710342913,29.6111106577518,21.2478694496601));
#52255=CARTESIAN_POINT('Ctrl Pts',(56.9311218502605,29.5000173279117,21.2411634803102));
#52256=CARTESIAN_POINT('Ctrl Pts',(56.9347976548042,29.4855995968175,21.2402975415681));
#52257=CARTESIAN_POINT('Ctrl Pts',(56.9651722033418,29.3606365404419,21.2328206320292));
#52258=CARTESIAN_POINT('Ctrl Pts',(56.9825320292906,29.2480432304664,21.2262611585592));
#52259=CARTESIAN_POINT('Ctrl Pts',(56.994128524497,29.0765604276137,21.2159623428842));
#52260=CARTESIAN_POINT('Ctrl Pts',(56.9955126541715,29.0183945161383,21.2124188690831));
#52261=CARTESIAN_POINT('Ctrl Pts',(56.994064904118,28.9457482884481,21.2078922551418));
#52262=CARTESIAN_POINT('Ctrl Pts',(56.9936175388369,28.9312454989239,21.2069836173327));
#52263=CARTESIAN_POINT('Ctrl Pts',(56.9926514408767,28.9081172616422,21.2055261175926));
#52264=CARTESIAN_POINT('Ctrl Pts',(56.9922348042019,28.8994878933492,21.2049804316586));
#52265=CARTESIAN_POINT('Ctrl Pts',(56.9913405308366,28.8831675147011,21.2039447272672));
#52266=CARTESIAN_POINT('Ctrl Pts',(56.9908743591029,28.8754760146559,21.2034550746141));
#52267=CARTESIAN_POINT('Ctrl Pts',(56.9897171415978,28.8580549419975,21.2023424367542));
#52268=CARTESIAN_POINT('Ctrl Pts',(56.9889992764816,28.8483274063523,21.2017186276038));
#52269=CARTESIAN_POINT('Ctrl Pts',(56.986961998098,28.8232302583095,21.2001024683209));
#52270=CARTESIAN_POINT('Ctrl Pts',(56.9855356070042,28.807870213824,21.1991068173323));
#52271=CARTESIAN_POINT('Ctrl Pts',(56.9740451350478,28.6979933490655,21.1919362989337));
#52272=CARTESIAN_POINT('Ctrl Pts',(56.9574163504813,28.6042996718033,21.1855570936841));
#52273=CARTESIAN_POINT('Ctrl Pts',(56.8922463236282,28.3459155112234,21.1672628605141));
#52274=CARTESIAN_POINT('Ctrl Pts',(56.8290616118007,28.1857796816078,21.1550440028991));
#52275=CARTESIAN_POINT('Ctrl Pts',(56.7354585648006,28.0162809621643,21.1421231446964));
#52276=CARTESIAN_POINT('Ctrl Pts',(56.7244119724049,27.9970428605373,21.1406580555409));
#52277=CARTESIAN_POINT('Ctrl Pts',(56.7093794110298,27.9718459197623,21.1387450099526));
#52278=CARTESIAN_POINT('Ctrl Pts',(56.7056794685354,27.9657194104438,21.1382803279182));
#52279=CARTESIAN_POINT('Ctrl Pts',(56.6995459877783,27.9556857836644,21.1375202356841));
#52280=CARTESIAN_POINT('Ctrl Pts',(56.6971317957851,27.9517670030988,21.1372236068421));
#52281=CARTESIAN_POINT('Ctrl Pts',(56.6923801381624,27.9441134331864,21.1366447937774));
#52282=CARTESIAN_POINT('Ctrl Pts',(56.6900438349191,27.9403779869113,21.1363625413001));
#52283=CARTESIAN_POINT('Ctrl Pts',(56.6842645950846,27.9312054682969,21.1356699911688));
#52284=CARTESIAN_POINT('Ctrl Pts',(56.6808076483625,27.9257771976033,21.1352606023971));
#52285=CARTESIAN_POINT('Ctrl Pts',(56.6688633535334,27.9072204910524,21.1338623344909));
#52286=CARTESIAN_POINT('Ctrl Pts',(56.6602477292406,27.8941747602424,21.1328814643415));
#52287=CARTESIAN_POINT('Ctrl Pts',(56.5808963407455,27.7770395874117,21.1240809376007));
#52288=CARTESIAN_POINT('Ctrl Pts',(56.5006012768501,27.6797462186289,21.1168067781436));
#52289=CARTESIAN_POINT('Ctrl Pts',(56.3071510762284,27.4859773917615,21.1009075841975));
#52290=CARTESIAN_POINT('Ctrl Pts',(56.1913370186391,27.3932588928929,21.0922946927273));
#52291=CARTESIAN_POINT('Ctrl Pts',(56.0514643828032,27.3047831039346,21.0820248406906));
#52292=CARTESIAN_POINT('Ctrl Pts',(56.0364582368483,27.295566966588,21.0809252634917));
#52293=CARTESIAN_POINT('Ctrl Pts',(56.0133390183227,27.2817863368983,21.0792336013539));
#52294=CARTESIAN_POINT('Ctrl Pts',(56.0053125018352,27.277077794248,21.0786467285246));
#52295=CARTESIAN_POINT('Ctrl Pts',(55.9912537081761,27.2689622648976,21.0776194184293));
#52296=CARTESIAN_POINT('Ctrl Pts',(55.9852360367152,27.2655301950416,21.0771798900242));
#52297=CARTESIAN_POINT('Ctrl Pts',(55.971629084303,27.2578633766516,21.0761864224438));
#52298=CARTESIAN_POINT('Ctrl Pts',(55.9640297986444,27.2536467610235,21.0756318487557));
#52299=CARTESIAN_POINT('Ctrl Pts',(55.9434650841826,27.2424111506515,21.0741316694769));
#52300=CARTESIAN_POINT('Ctrl Pts',(55.9304491942491,27.2354861275397,21.0731827773761));
#52301=CARTESIAN_POINT('Ctrl Pts',(55.8696675157905,27.2040071265859,21.0687535379843));
#52302=CARTESIAN_POINT('Ctrl Pts',(55.8210031216531,27.1812463161389,21.0652118407498));
#52303=CARTESIAN_POINT('Ctrl Pts',(55.6043126855331,27.0903677757737,21.0494514633099));
#52304=CARTESIAN_POINT('Ctrl Pts',(55.4283711448534,27.0433779294654,21.0365791649457));
#52305=CARTESIAN_POINT('Ctrl Pts',(55.2127517289641,27.016299853377,21.0216940953161));
#52306=CARTESIAN_POINT('Ctrl Pts',(55.1768319924736,27.0127757233648,21.0192472671285));
#52307=CARTESIAN_POINT('Ctrl Pts',(55.1189504424811,27.0086789152652,21.0153762066015));
#52308=CARTESIAN_POINT('Ctrl Pts',(55.0970412904931,27.0074910404696,21.013927437896));
#52309=CARTESIAN_POINT('Ctrl Pts',(55.0679932290472,27.0063964063919,21.0120322492798));
#52310=CARTESIAN_POINT('Ctrl Pts',(55.0608689936922,27.0061661711769,21.0115694839951));
#52311=CARTESIAN_POINT('Ctrl Pts',(55.049148934728,27.0058502888386,21.0108117164979));
#52312=CARTESIAN_POINT('Ctrl Pts',(55.0445538500787,27.0057423326479,21.0105155098098));
#52313=CARTESIAN_POINT('Ctrl Pts',(55.0355489803478,27.0055619129486,21.0099368413561));
#52314=CARTESIAN_POINT('Ctrl Pts',(55.0311392735246,27.0054881902333,21.0096543151223));
#52315=CARTESIAN_POINT('Ctrl Pts',(55.0202717386222,27.0053425539706,21.008960056072));
#52316=CARTESIAN_POINT('Ctrl Pts',(55.013813665148,27.005287375134,21.0085492425247));
#52317=CARTESIAN_POINT('Ctrl Pts',(54.9915859702474,27.0052054133999,21.0071409683663));
#52318=CARTESIAN_POINT('Ctrl Pts',(54.9758158972198,27.0053342625682,21.00615167141));
#52319=CARTESIAN_POINT('Ctrl Pts',(54.8379178685051,27.0080966871332,20.9975741894971));
#52320=CARTESIAN_POINT('Ctrl Pts',(54.7162526165712,27.0217570817255,20.9904987464281));
#52321=CARTESIAN_POINT('Ctrl Pts',(54.4949827445759,27.0674500854174,20.9773788164561));
#52322=CARTESIAN_POINT('Ctrl Pts',(54.3951730042513,27.0963262137655,20.9713592013312));
#52323=CARTESIAN_POINT('Ctrl Pts',(54.2648390214939,27.14532318027,20.9629905732852));
#52324=CARTESIAN_POINT('Ctrl Pts',(54.2319510402049,27.1586992775821,20.9608344175842));
#52325=CARTESIAN_POINT('Ctrl Pts',(54.1760774994199,27.1831814054556,20.9570814995931));
#52326=CARTESIAN_POINT('Ctrl Pts',(54.1529155582769,27.1938643601365,20.955498502523));
#52327=CARTESIAN_POINT('Ctrl Pts',(54.1202585254526,27.2096930809307,20.9532244954146));
#52328=CARTESIAN_POINT('Ctrl Pts',(54.1105899355263,27.2144766435468,20.9525459111537));
#52329=CARTESIAN_POINT('Ctrl Pts',(54.0939469993248,27.2228795045259,20.9513683654091));
#52330=CARTESIAN_POINT('Ctrl Pts',(54.0869542957043,27.226462057222,20.9508706884499));
#52331=CARTESIAN_POINT('Ctrl Pts',(54.0735756660803,27.2334163866106,20.9499128182821));
#52332=CARTESIAN_POINT('Ctrl Pts',(54.0671865152667,27.2367817179849,20.9494528568374));
#52333=CARTESIAN_POINT('Ctrl Pts',(54.0521855716578,27.2447874581097,20.948366909629));
#52334=CARTESIAN_POINT('Ctrl Pts',(54.043589423659,27.2494566381734,20.9477399166424));
#52335=CARTESIAN_POINT('Ctrl Pts',(54.0137138783033,27.2659699139842,20.9455441382238));
#52336=CARTESIAN_POINT('Ctrl Pts',(53.992618021504,27.2781399255592,20.9439638454979));
#52337=CARTESIAN_POINT('Ctrl Pts',(53.8593808753254,27.3582899138892,20.9337866924179));
#52338=CARTESIAN_POINT('Ctrl Pts',(53.7539694850766,27.436791456716,20.9248018826938));
#52339=CARTESIAN_POINT('Ctrl Pts',(53.5828300923145,27.5926162860125,20.9086945810757));
#52340=CARTESIAN_POINT('Ctrl Pts',(53.51382534887,27.6656889549421,20.9016609362184));
#52341=CARTESIAN_POINT('Ctrl Pts',(53.4329748277004,27.7653973162296,20.8929369266958));
#52342=CARTESIAN_POINT('Ctrl Pts',(53.4157973145792,27.7875175505144,20.8910519734023));
#52343=CARTESIAN_POINT('Ctrl Pts',(53.3882058932978,27.8246361380822,20.8879803380853));
#52344=CARTESIAN_POINT('Ctrl Pts',(53.3775223010567,27.839428320528,20.8867793823382));
#52345=CARTESIAN_POINT('Ctrl Pts',(53.3632259115094,27.8598060200889,20.8851584586557));
#52346=CARTESIAN_POINT('Ctrl Pts',(53.3594362349707,27.8652655533219,20.8847274131131));
#52347=CARTESIAN_POINT('Ctrl Pts',(53.3531304752003,27.874447462333,20.8840080044845));
#52348=CARTESIAN_POINT('Ctrl Pts',(53.3505995825922,27.8781595429862,20.8837186629159));
#52349=CARTESIAN_POINT('Ctrl Pts',(53.3458278299211,27.8852093670303,20.8831720464143));
#52350=CARTESIAN_POINT('Ctrl Pts',(53.3435844888756,27.8885453770744,20.8829146011717));
#52351=CARTESIAN_POINT('Ctrl Pts',(53.3377367195202,27.8972984607662,20.8822422261263));
#52352=CARTESIAN_POINT('Ctrl Pts',(53.3341486476719,27.9027264821275,20.8818283776927));
#52353=CARTESIAN_POINT('Ctrl Pts',(53.3217966418752,27.9216127886908,20.8803988197069));
#52354=CARTESIAN_POINT('Ctrl Pts',(53.3131684579371,27.9351596947544,20.879391607141));
#52355=CARTESIAN_POINT('Ctrl Pts',(53.2472355815369,28.0414922220892,20.8716142837777));
#52356=CARTESIAN_POINT('Ctrl Pts',(53.1974560591343,28.1387440574427,20.8652499193493));
#52357=CARTESIAN_POINT('Ctrl Pts',(53.1302656413683,28.3016923803078,20.8550055780894));
#52358=CARTESIAN_POINT('Ctrl Pts',(53.1078116434887,28.3650487307882,20.8511184608071));
#52359=CARTESIAN_POINT('Ctrl Pts',(53.06295064399,28.5153288405849,20.8419195531604));
#52360=CARTESIAN_POINT('Ctrl Pts',(53.043128424588,28.6028637249946,20.8365739464099));
#52361=CARTESIAN_POINT('Ctrl Pts',(53.0258366984816,28.7132999664281,20.8296731230831));
#52362=CARTESIAN_POINT('Ctrl Pts',(53.0227765874294,28.7352261972321,20.8282958260924));
#52363=CARTESIAN_POINT('Ctrl Pts',(53.0188411939818,28.767317205628,20.8262676273844));
#52364=CARTESIAN_POINT('Ctrl Pts',(53.0176778847017,28.7774454617425,20.8256257140402));
#52365=CARTESIAN_POINT('Ctrl Pts',(53.0157658242641,28.7952989213614,20.8244908480397));
#52366=CARTESIAN_POINT('Ctrl Pts',(53.0149844189756,28.8030204678559,20.8239989250313));
#52367=CARTESIAN_POINT('Ctrl Pts',(53.0134500878188,28.8191194970896,20.8229709179553));
#52368=CARTESIAN_POINT('Ctrl Pts',(53.0127050508937,28.8274975605128,20.8224345980065));
#52369=CARTESIAN_POINT('Ctrl Pts',(53.0109046605308,28.8493057019706,20.8210349589545));
#52370=CARTESIAN_POINT('Ctrl Pts',(53.0099323441504,28.8627420260075,20.8201690746088));
#52371=CARTESIAN_POINT('Ctrl Pts',(53.0065097342746,28.9177772930961,20.8166072788937));
#52372=CARTESIAN_POINT('Ctrl Pts',(53.0052272996647,28.9594357326713,20.8138755641965));
#52373=CARTESIAN_POINT('Ctrl Pts',(53.0052897809569,29.0726028522538,20.8063530938477));
#52374=CARTESIAN_POINT('Ctrl Pts',(53.0091736191226,29.1440436529404,20.801492171297));
#52375=CARTESIAN_POINT('Ctrl Pts',(53.0237803554166,29.278700715536,20.7921524527072));
#52376=CARTESIAN_POINT('Ctrl Pts',(53.0337289129306,29.3418912045436,20.7876948307582));
#52377=CARTESIAN_POINT('Ctrl Pts',(53.0466870286012,29.4044700214667,20.7832412988479));
#52378=CARTESIAN_POINT('',(53.0052497878256,29.0009911092822,20.6530359722443));
#52379=CARTESIAN_POINT('Ctrl Pts',(53.0466869978243,29.4044698728352,20.6265291208673));
#52380=CARTESIAN_POINT('Ctrl Pts',(53.0423917803693,29.3837269086108,20.6279902739909));
#52381=CARTESIAN_POINT('Ctrl Pts',(53.0384253997232,29.3629079073144,20.6294455367161));
#52382=CARTESIAN_POINT('Ctrl Pts',(53.0291254426595,29.3094714389379,20.6331463186058));
#52383=CARTESIAN_POINT('Ctrl Pts',(53.02426986673,29.2767847291785,20.6353774910218));
#52384=CARTESIAN_POINT('Ctrl Pts',(53.0179376162708,29.2254040379901,20.638819347937));
#52385=CARTESIAN_POINT('Ctrl Pts',(53.0159087212894,29.2067852307779,20.6400532000872));
#52386=CARTESIAN_POINT('Ctrl Pts',(53.0134887093812,29.1812414667323,20.6417252052073));
#52387=CARTESIAN_POINT('Ctrl Pts',(53.0128710972373,29.1743396232666,20.6421749038912));
#52388=CARTESIAN_POINT('Ctrl Pts',(53.0119452901785,29.1633488443142,20.6428875777845));
#52389=CARTESIAN_POINT('Ctrl Pts',(53.0116137230563,29.1592620123635,20.6431518224063));
#52390=CARTESIAN_POINT('Ctrl Pts',(53.0109763952033,29.1510940455679,20.6436783913493));
#52391=CARTESIAN_POINT('Ctrl Pts',(53.0106705909434,29.1470129708689,20.6439407100236));
#52392=CARTESIAN_POINT('Ctrl Pts',(53.0100651935259,29.1385857382147,20.6444808278499));
#52393=CARTESIAN_POINT('Ctrl Pts',(53.0097672726809,29.1342394607415,20.6447585350891));
#52394=CARTESIAN_POINT('Ctrl Pts',(53.0091005646849,29.1240225787607,20.6454094130717));
#52395=CARTESIAN_POINT('Ctrl Pts',(53.0087434985907,29.1181512132631,20.6457819551888));
#52396=CARTESIAN_POINT('Ctrl Pts',(53.0076145848768,29.0981265854036,20.6470476796835));
#52397=CARTESIAN_POINT('Ctrl Pts',(53.0069675999165,29.0839663452612,20.6479344661133));
#52398=CARTESIAN_POINT('Ctrl Pts',(53.0056688480167,29.0468732193099,20.6502386092127));
#52399=CARTESIAN_POINT('Ctrl Pts',(53.0052616459177,29.0239335306591,20.6516447617078));
#52400=CARTESIAN_POINT('Ctrl Pts',(53.0052502462445,29.0009911570512,20.6530367634788));
#52401=CARTESIAN_POINT('Ctrl Pts',(53.0052502449332,29.0009885144422,20.653036923816));
#52402=CARTESIAN_POINT('Ctrl Pts',(53.0051989849948,28.8975497125354,20.6593129475683));
#52403=CARTESIAN_POINT('Ctrl Pts',(53.0131936139981,28.794251182285,20.6652955731722));
#52404=CARTESIAN_POINT('Ctrl Pts',(53.0514847436693,28.5492109164505,20.6796977461016));
#52405=CARTESIAN_POINT('Ctrl Pts',(53.0892555137733,28.4092625251289,20.6881242733579));
#52406=CARTESIAN_POINT('Ctrl Pts',(53.1484359598757,28.2576590340402,20.6982154482694));
#52407=CARTESIAN_POINT('Ctrl Pts',(53.1552932332696,28.2407790736154,20.6993524755353));
#52408=CARTESIAN_POINT('Ctrl Pts',(53.1660497119535,28.2153071562461,20.7010898339193));
#52409=CARTESIAN_POINT('Ctrl Pts',(53.1697803591026,28.2066447332736,20.701684500728));
#52410=CARTESIAN_POINT('Ctrl Pts',(53.1766594771817,28.1909784533875,20.7027670936905));
#52411=CARTESIAN_POINT('Ctrl Pts',(53.1797872425967,28.1839656624003,20.7032543100944));
#52412=CARTESIAN_POINT('Ctrl Pts',(53.1866106031195,28.1689013654378,20.7043066248604));
#52413=CARTESIAN_POINT('Ctrl Pts',(53.1903194900122,28.1608560953517,20.7048721690013));
#52414=CARTESIAN_POINT('Ctrl Pts',(53.2004996920883,28.1391547363046,20.7064074270979));
#52415=CARTESIAN_POINT('Ctrl Pts',(53.2070726964551,28.1255472627527,20.7073806133059));
#52416=CARTESIAN_POINT('Ctrl Pts',(53.2405537686634,28.0581993005751,20.7122509336185));
#52417=CARTESIAN_POINT('Ctrl Pts',(53.2697238921021,28.0056243481379,20.7162259181694));
#52418=CARTESIAN_POINT('Ctrl Pts',(53.3721458578102,27.8392119879154,20.7293891472845));
#52419=CARTESIAN_POINT('Ctrl Pts',(53.4546078327571,27.7314996108954,20.7388688884355));
#52420=CARTESIAN_POINT('Ctrl Pts',(53.5902251982648,27.5873847271806,20.7526213803075));
#52421=CARTESIAN_POINT('Ctrl Pts',(53.6352544108055,27.5438346798413,20.7569421839769));
#52422=CARTESIAN_POINT('Ctrl Pts',(53.6982097756871,27.4884375186073,20.7625937797129));
#52423=CARTESIAN_POINT('Ctrl Pts',(53.7143832161155,27.4746579120183,20.7640135131849));
#52424=CARTESIAN_POINT('Ctrl Pts',(53.7386347278624,27.4546556927652,20.7660916254736));
#52425=CARTESIAN_POINT('Ctrl Pts',(53.7465448144534,27.4482327863435,20.7667616588283));
#52426=CARTESIAN_POINT('Ctrl Pts',(53.7592680630799,27.4380624140574,20.7678265685715));
#52427=CARTESIAN_POINT('Ctrl Pts',(53.7640496859873,27.4342760188215,20.7682239229845));
#52428=CARTESIAN_POINT('Ctrl Pts',(53.7731685390955,27.4271229313564,20.7689761719254));
#52429=CARTESIAN_POINT('Ctrl Pts',(53.7775024396143,27.4237521060715,20.7693313419399));
#52430=CARTESIAN_POINT('Ctrl Pts',(53.7851797162008,27.4178315771225,20.7699562882723));
#52431=CARTESIAN_POINT('Ctrl Pts',(53.7885172983543,27.415274501652,20.7702265743523));
#52432=CARTESIAN_POINT('Ctrl Pts',(53.7957885449339,27.40974006183,20.770812364423));
#52433=CARTESIAN_POINT('Ctrl Pts',(53.7997251763587,27.40676673131,20.7711275894078));
#52434=CARTESIAN_POINT('Ctrl Pts',(53.8104183069469,27.3987523555781,20.7719787755734));
#52435=CARTESIAN_POINT('Ctrl Pts',(53.8171958861225,27.3937394179745,20.7725128357389));
#52436=CARTESIAN_POINT('Ctrl Pts',(53.8501385958939,27.3696953995737,20.7750835354035));
#52437=CARTESIAN_POINT('Ctrl Pts',(53.876733956542,27.351258658223,20.777082801111));
#52438=CARTESIAN_POINT('Ctrl Pts',(54.0743707090325,27.2212540717832,20.7914853567128));
#52439=CARTESIAN_POINT('Ctrl Pts',(54.2612048450082,27.1358840933454,20.8027859059759));
#52440=CARTESIAN_POINT('Ctrl Pts',(54.5104654921247,27.0654761840217,20.81834212755));
#52441=CARTESIAN_POINT('Ctrl Pts',(54.563751897701,27.0527678081384,20.8216843951475));
#52442=CARTESIAN_POINT('Ctrl Pts',(54.63146587729,27.0395375705888,20.8259842075171));
#52443=CARTESIAN_POINT('Ctrl Pts',(54.6454700426122,27.0369567428291,20.8268762063524));
#52444=CARTESIAN_POINT('Ctrl Pts',(54.6679545680287,27.0330615128253,20.8283132502221));
#52445=CARTESIAN_POINT('Ctrl Pts',(54.6764180295075,27.0316514826152,20.8288552757992));
#52446=CARTESIAN_POINT('Ctrl Pts',(54.6925101639894,27.0290770910995,20.8298880720088));
#52447=CARTESIAN_POINT('Ctrl Pts',(54.700137029478,27.0279023076273,20.8303785047201));
#52448=CARTESIAN_POINT('Ctrl Pts',(54.7175202640017,27.0253278992801,20.8314985278464));
#52449=CARTESIAN_POINT('Ctrl Pts',(54.7272805155149,27.0239562799208,20.8321289848006));
#52450=CARTESIAN_POINT('Ctrl Pts',(54.7526779736182,27.0205788932182,20.8337738285262));
#52451=CARTESIAN_POINT('Ctrl Pts',(54.7683292622009,27.0186861055289,20.8347917142158));
#52452=CARTESIAN_POINT('Ctrl Pts',(54.9138070400975,27.0028400510913,20.8442942080277));
#52453=CARTESIAN_POINT('Ctrl Pts',(55.0446634812681,27.0014828624549,20.8531784177598));
#52454=CARTESIAN_POINT('Ctrl Pts',(55.2684251834071,27.0211545405083,20.8687773625685));
#52455=CARTESIAN_POINT('Ctrl Pts',(55.3614586451128,27.0360169228024,20.8753775001902));
#52456=CARTESIAN_POINT('Ctrl Pts',(55.510221269787,27.0707144866618,20.8858697444773));
#52457=CARTESIAN_POINT('Ctrl Pts',(55.5667367503657,27.0865530578495,20.8898388362679));
#52458=CARTESIAN_POINT('Ctrl Pts',(55.6316273930924,27.107867034147,20.8943157484908));
#52459=CARTESIAN_POINT('Ctrl Pts',(55.6407560571719,27.1109388553363,20.8949436454975));
#52460=CARTESIAN_POINT('Ctrl Pts',(55.6547266615384,27.1157529269056,20.8959012745984));
#52461=CARTESIAN_POINT('Ctrl Pts',(55.659584555704,27.1174479425236,20.8962336464041));
#52462=CARTESIAN_POINT('Ctrl Pts',(55.6684913226914,27.1205943990513,20.89684183203));
#52463=CARTESIAN_POINT('Ctrl Pts',(55.6725420494519,27.122040135198,20.8971179632994));
#52464=CARTESIAN_POINT('Ctrl Pts',(55.6816452636787,27.1253223755439,20.8977374812206));
#52465=CARTESIAN_POINT('Ctrl Pts',(55.6866950131695,27.1271662055478,20.8980804320996));
#52466=CARTESIAN_POINT('Ctrl Pts',(55.7014995162723,27.1326397458753,20.8990839580816));
#52467=CARTESIAN_POINT('Ctrl Pts',(55.711233564339,27.1363254796112,20.8997413359285));
#52468=CARTESIAN_POINT('Ctrl Pts',(55.7882970131251,27.166196780996,20.9049296114878));
#52469=CARTESIAN_POINT('Ctrl Pts',(55.85419552537,27.1959493195657,20.9092689068439));
#52470=CARTESIAN_POINT('Ctrl Pts',(56.0085333695467,27.2759899920151,20.9195238182742));
#52471=CARTESIAN_POINT('Ctrl Pts',(56.0950222611976,27.3295876336119,20.9253539733489));
#52472=CARTESIAN_POINT('Ctrl Pts',(56.235903304666,27.432554949113,20.9355516547217));
#52473=CARTESIAN_POINT('Ctrl Pts',(56.2923476820771,27.4787580170933,20.9398573874958));
#52474=CARTESIAN_POINT('Ctrl Pts',(56.3778833095861,27.5569767433172,20.9468793420569));
#52475=CARTESIAN_POINT('Ctrl Pts',(56.4086831805226,27.587028019372,20.9495215011912));
#52476=CARTESIAN_POINT('Ctrl Pts',(56.4475872885617,27.6275237004495,20.9530267201318));
#52477=CARTESIAN_POINT('Ctrl Pts',(56.4565947282819,27.637086967064,20.9538506423045));
#52478=CARTESIAN_POINT('Ctrl Pts',(56.4711634773622,27.6528641094489,20.9552040773903));
#52479=CARTESIAN_POINT('Ctrl Pts',(56.476781538925,27.6590252173804,20.9557311777323));
#52480=CARTESIAN_POINT('Ctrl Pts',(56.487571456292,27.6710081399447,20.9567537102882));
#52481=CARTESIAN_POINT('Ctrl Pts',(56.4927481803061,27.6768253822508,20.9572489256947));
#52482=CARTESIAN_POINT('Ctrl Pts',(56.5046204741856,27.6903249873051,20.9583955019549));
#52483=CARTESIAN_POINT('Ctrl Pts',(56.5112914543566,27.6980285932985,20.9590478598907));
#52484=CARTESIAN_POINT('Ctrl Pts',(56.5326460480436,27.7230740057945,20.9611627735162));
#52485=CARTESIAN_POINT('Ctrl Pts',(56.5470920213188,27.7406151857018,20.962634875113));
#52486=CARTESIAN_POINT('Ctrl Pts',(56.6668547161944,27.8912091663019,20.9752016806785));
#52487=CARTESIAN_POINT('Ctrl Pts',(56.7550772698159,28.0369305422543,20.98698673135));
#52488=CARTESIAN_POINT('Ctrl Pts',(56.8532753195288,28.2585828905094,21.0038712842703));
#52489=CARTESIAN_POINT('Ctrl Pts',(56.8791022980351,28.3267209644896,21.0089216946339));
#52490=CARTESIAN_POINT('Ctrl Pts',(56.9082063151757,28.4183471899178,21.0154188183984));
#52491=CARTESIAN_POINT('Ctrl Pts',(56.9148757924548,28.4406949567341,21.0169808305956));
#52492=CARTESIAN_POINT('Ctrl Pts',(56.9254345576521,28.4784805634041,21.0195783612159));
#52493=CARTESIAN_POINT('Ctrl Pts',(56.929533607894,28.4938568851945,21.0206234023165));
#52494=CARTESIAN_POINT('Ctrl Pts',(56.9349977397196,28.5153857450806,21.0220683676396));
#52495=CARTESIAN_POINT('Ctrl Pts',(56.9365182146849,28.5214977162313,21.0224765487398));
#52496=CARTESIAN_POINT('Ctrl Pts',(56.9390572898854,28.5319145840581,21.0231686396929));
#52497=CARTESIAN_POINT('Ctrl Pts',(56.9400905576879,28.5362158266049,21.0234533727512));
#52498=CARTESIAN_POINT('Ctrl Pts',(56.942051661859,28.5445006760501,21.0239997708041));
#52499=CARTESIAN_POINT('Ctrl Pts',(56.9429815608248,28.5484837251296,21.024261557326));
#52500=CARTESIAN_POINT('Ctrl Pts',(56.9451859851918,28.5580588942474,21.024888784609));
#52501=CARTESIAN_POINT('Ctrl Pts',(56.9464486649457,28.5636537446015,21.0252535592312));
#52502=CARTESIAN_POINT('Ctrl Pts',(56.9509670883086,28.5840845236042,21.0265796028233));
#52503=CARTESIAN_POINT('Ctrl Pts',(56.9540775835192,28.5989525048917,21.0275330598609));
#52504=CARTESIAN_POINT('Ctrl Pts',(56.9830896585188,28.7459883773731,21.0368616299607));
#52505=CARTESIAN_POINT('Ctrl Pts',(56.9957161398604,28.8804422194785,21.04460795487));
#52506=CARTESIAN_POINT('Ctrl Pts',(56.9936358400592,29.1541944385792,21.0605099228372));
#52507=CARTESIAN_POINT('Ctrl Pts',(56.9780465592986,29.2927193188917,21.068640455057));
#52508=CARTESIAN_POINT('Ctrl Pts',(56.9443190271023,29.4460661045214,21.0783787188003));
#52509=CARTESIAN_POINT('Ctrl Pts',(56.9402155630594,29.46358924134,21.0795020776734));
#52510=CARTESIAN_POINT('Ctrl Pts',(56.9336121687649,29.4901628686293,21.0812227687045));
#52511=CARTESIAN_POINT('Ctrl Pts',(56.9312844431495,29.4992554975174,21.0818146036314));
#52512=CARTESIAN_POINT('Ctrl Pts',(56.9271251929072,29.5150380162726,21.082847369183));
#52513=CARTESIAN_POINT('Ctrl Pts',(56.9253227712924,29.5217354614298,21.083287358622));
#52514=CARTESIAN_POINT('Ctrl Pts',(56.9211981428157,29.5367493015338,21.08427764088));
#52515=CARTESIAN_POINT('Ctrl Pts',(56.9188568040183,29.5450602521618,21.0848285428376));
#52516=CARTESIAN_POINT('Ctrl Pts',(56.9124428303823,29.5672740573276,21.0863084641226));
#52517=CARTESIAN_POINT('Ctrl Pts',(56.9082726347894,29.5811479748371,21.087240618879));
#52518=CARTESIAN_POINT('Ctrl Pts',(56.8887435186629,29.6436421955234,21.0914758811401));
#52519=CARTESIAN_POINT('Ctrl Pts',(56.8716761341378,29.691704438567,21.0948339672078));
#52520=CARTESIAN_POINT('Ctrl Pts',(56.784530840852,29.9101744233413,21.1105795940926));
#52521=CARTESIAN_POINT('Ctrl Pts',(56.6928979618292,30.0710020284877,21.1236630514197));
#52522=CARTESIAN_POINT('Ctrl Pts',(56.5476231286222,30.259682878865,21.13997625934));
#52523=CARTESIAN_POINT('Ctrl Pts',(56.5129850168429,30.301082540889,21.1436169928867));
#52524=CARTESIAN_POINT('Ctrl Pts',(56.4703582781784,30.3480219929654,21.1477715592361));
#52525=CARTESIAN_POINT('Ctrl Pts',(56.4639592534428,30.3549686610402,21.1483871079318));
#52526=CARTESIAN_POINT('Ctrl Pts',(56.4540254875256,30.3656000540955,21.1493298951057));
#52527=CARTESIAN_POINT('Ctrl Pts',(56.4505256375328,30.3693169838959,21.1496596505769));
#52528=CARTESIAN_POINT('Ctrl Pts',(56.4440493781061,30.3761422439869,21.150265357755));
#52529=CARTESIAN_POINT('Ctrl Pts',(56.4410771928575,30.3792543663,21.1505416086872));
#52530=CARTESIAN_POINT('Ctrl Pts',(56.4343361275596,30.3862672376662,21.1511642854768));
#52531=CARTESIAN_POINT('Ctrl Pts',(56.4305614008705,30.3901622427088,21.151510254717));
#52532=CARTESIAN_POINT('Ctrl Pts',(56.4193398945117,30.4016472044408,21.1525309557542));
#52533=CARTESIAN_POINT('Ctrl Pts',(56.4118481249087,30.4091932109312,21.1532023242584));
#52534=CARTESIAN_POINT('Ctrl Pts',(56.3384606989584,30.4819391693019,21.1596861158934));
#52535=CARTESIAN_POINT('Ctrl Pts',(56.2681468515568,30.5425397558459,21.1651811678491));
#52536=CARTESIAN_POINT('Ctrl Pts',(56.1050740192947,30.6643685420558,21.1770795042808));
#52537=CARTESIAN_POINT('Ctrl Pts',(56.0109124953292,30.7231851296029,21.1834364628123));
#52538=CARTESIAN_POINT('Ctrl Pts',(55.8648789916884,30.7982941746864,21.1931463494728));
#52539=CARTESIAN_POINT('Ctrl Pts',(55.8164463283188,30.8207944358888,21.1963422083825));
#52540=CARTESIAN_POINT('Ctrl Pts',(55.7457636213967,30.8502437852368,21.2010135106738));
#52541=CARTESIAN_POINT('Ctrl Pts',(55.7242019409201,30.8587891023694,21.2024392984853));
#52542=CARTESIAN_POINT('Ctrl Pts',(55.685383805207,30.8733955591535,21.2050108168111));
#52543=CARTESIAN_POINT('Ctrl Pts',(55.6681835368932,30.879599055123,21.206151844966));
#52544=CARTESIAN_POINT('Ctrl Pts',(55.6419728613992,30.8886470329995,21.2078940796743));
#52545=CARTESIAN_POINT('Ctrl Pts',(55.6330232181185,30.8916655017306,21.2084895725686));
#52546=CARTESIAN_POINT('Ctrl Pts',(55.6167585579605,30.8970227776174,21.2095730390657));
#52547=CARTESIAN_POINT('Ctrl Pts',(55.6094507895989,30.8993831288064,21.2100602973306));
#52548=CARTESIAN_POINT('Ctrl Pts',(55.5936936120888,30.9043722742563,21.2111119919665));
#52549=CARTESIAN_POINT('Ctrl Pts',(55.5852400019251,30.9069871525526,21.2116768696042));
#52550=CARTESIAN_POINT('Ctrl Pts',(55.5623458925904,30.9139022117629,21.2132085711775));
#52551=CARTESIAN_POINT('Ctrl Pts',(55.5478738423156,30.918095099694,21.2141788403523));
#52552=CARTESIAN_POINT('Ctrl Pts',(55.4758598560546,30.9380777339457,21.2190180343386));
#52553=CARTESIAN_POINT('Ctrl Pts',(55.4176823693218,30.9514425735709,21.2229636508999));
#52554=CARTESIAN_POINT('Ctrl Pts',(55.2027368528984,30.9907687649775,21.2376791721169));
#52555=CARTESIAN_POINT('Ctrl Pts',(55.0436290404494,31.0005868376054,21.248892807459));
#52556=CARTESIAN_POINT('Ctrl Pts',(54.8387742540884,30.9887645837924,21.2630521102782));
#52557=CARTESIAN_POINT('Ctrl Pts',(54.7925792096729,30.9844786449024,21.2662215441081));
#52558=CARTESIAN_POINT('Ctrl Pts',(54.7292267383726,30.9763641429337,21.2705020917353));
#52559=CARTESIAN_POINT('Ctrl Pts',(54.7119099900578,30.973914277789,21.2716652488485));
#52560=CARTESIAN_POINT('Ctrl Pts',(54.682011235717,30.9692825311097,21.273659112919));
#52561=CARTESIAN_POINT('Ctrl Pts',(54.6694140520212,30.967207028434,21.2744947322004));
#52562=CARTESIAN_POINT('Ctrl Pts',(54.6511588324566,30.964018999523,21.2756983619489));
#52563=CARTESIAN_POINT('Ctrl Pts',(54.645484624748,30.9630027104846,21.2760714537769));
#52564=CARTESIAN_POINT('Ctrl Pts',(54.6355496212595,30.9611788008642,21.2767228046752));
#52565=CARTESIAN_POINT('Ctrl Pts',(54.6312869485221,30.9603818644855,21.2770016541657));
#52566=CARTESIAN_POINT('Ctrl Pts',(54.6222322648156,30.9586584492949,21.2775926429705));
#52567=CARTESIAN_POINT('Ctrl Pts',(54.6174410431473,30.9577282826023,21.2779045727925));
#52568=CARTESIAN_POINT('Ctrl Pts',(54.6044019053851,30.9551471714728,21.278751450841));
#52569=CARTESIAN_POINT('Ctrl Pts',(54.5961608295053,30.9534616056857,21.2792844868916));
#52570=CARTESIAN_POINT('Ctrl Pts',(54.5575005197377,30.9452992141314,21.2817756936754));
#52571=CARTESIAN_POINT('Ctrl Pts',(54.5272229866976,30.9381632972807,21.2836994738747));
#52572=CARTESIAN_POINT('Ctrl Pts',(54.2982074118985,30.8785013771913,21.2981278033037));
#52573=CARTESIAN_POINT('Ctrl Pts',(54.1084812608212,30.7962447791321,21.3094945107392));
#52574=CARTESIAN_POINT('Ctrl Pts',(53.8882665777907,30.6571321600984,21.3251372814889));
#52575=CARTESIAN_POINT('Ctrl Pts',(53.8431104881462,30.6259286693526,21.3284859164819));
#52576=CARTESIAN_POINT('Ctrl Pts',(53.7879223535345,30.5843289958351,21.3327929145874));
#52577=CARTESIAN_POINT('Ctrl Pts',(53.7766365262738,30.575630788828,21.3336854578911));
#52578=CARTESIAN_POINT('Ctrl Pts',(53.7587041306838,30.5615011301157,21.3351231710755));
#52579=CARTESIAN_POINT('Ctrl Pts',(53.7519976172571,30.5561462860208,21.3356653164279));
#52580=CARTESIAN_POINT('Ctrl Pts',(53.7393270762424,30.5458948493462,21.3366982057311));
#52581=CARTESIAN_POINT('Ctrl Pts',(53.7333564849006,30.5410065894931,21.3371886108393));
#52582=CARTESIAN_POINT('Ctrl Pts',(53.7198272671223,30.5297981606379,21.338308382274));
#52583=CARTESIAN_POINT('Ctrl Pts',(53.7122868492832,30.5234564234145,21.3389386136935));
#52584=CARTESIAN_POINT('Ctrl Pts',(53.692812799206,30.5068302362748,21.3405824818258));
#52585=CARTESIAN_POINT('Ctrl Pts',(53.6809536552743,30.4964599746932,21.3415996106325));
#52586=CARTESIAN_POINT('Ctrl Pts',(53.5713651742345,30.3983152004726,21.3511522218678));
#52587=CARTESIAN_POINT('Ctrl Pts',(53.4824253743957,30.3012449470915,21.3600924861554));
#52588=CARTESIAN_POINT('Ctrl Pts',(53.3462509420951,30.119515165601,21.3758650957462));
#52589=CARTESIAN_POINT('Ctrl Pts',(53.2944138081073,30.0388341798271,21.3825839074236));
#52590=CARTESIAN_POINT('Ctrl Pts',(53.2215933760939,29.9052484691171,21.3930211451163));
#52591=CARTESIAN_POINT('Ctrl Pts',(53.1967212984401,29.8546298071825,21.3968302890198));
#52592=CARTESIAN_POINT('Ctrl Pts',(53.1701829852911,29.7942847931287,21.4011505628708));
#52593=CARTESIAN_POINT('Ctrl Pts',(53.1664037569904,29.7855211430696,21.4017726547652));
#52594=CARTESIAN_POINT('Ctrl Pts',(53.1606913386702,29.7720087373195,21.4027233093546));
#52595=CARTESIAN_POINT('Ctrl Pts',(53.1587133781316,29.7672792318912,21.4030544537562));
#52596=CARTESIAN_POINT('Ctrl Pts',(53.1551090783361,29.7585667784494,21.403661470089));
#52597=CARTESIAN_POINT('Ctrl Pts',(53.1534773963189,29.7545862077781,21.4039376509376));
#52598=CARTESIAN_POINT('Ctrl Pts',(53.1498273654406,29.7455990362546,21.4045586212454));
#52599=CARTESIAN_POINT('Ctrl Pts',(53.1478164566483,29.7405895110753,21.4049029652995));
#52600=CARTESIAN_POINT('Ctrl Pts',(53.1419496953011,29.7258010202053,21.4059144015996));
#52601=CARTESIAN_POINT('Ctrl Pts',(53.1381507049136,29.7159994898052,21.4065782206326));
#52602=CARTESIAN_POINT('Ctrl Pts',(53.1067720770863,29.6331027315131,21.4121411816274));
#52603=CARTESIAN_POINT('Ctrl Pts',(53.0834276957116,29.5584663008516,21.4168158330767));
#52604=CARTESIAN_POINT('Ctrl Pts',(53.0580509838884,29.4567017169179,21.4229833679291));
#52605=CARTESIAN_POINT('Ctrl Pts',(53.0521056353475,29.4306381909294,21.4245451343344));
#52606=CARTESIAN_POINT('Ctrl Pts',(53.0466869889941,29.4044698301913,21.4261018347978));
#52607=CARTESIAN_POINT('Origin',(55.,29.,3.45145488139523));
#52608=CARTESIAN_POINT('',(53.0466870263011,29.4044700103589,22.3827843708292));
#52609=CARTESIAN_POINT('',(53.0466869980082,29.4044698737232,22.2235966764224));
#52610=CARTESIAN_POINT('',(53.0466869980082,29.4044698737233,3.45145488139523));
#52611=CARTESIAN_POINT('',(53.0052507292241,28.9982943508983,21.6101045922788));
#52612=CARTESIAN_POINT('Ctrl Pts',(53.0466870263011,29.4044700103589,22.3827843708292));
#52613=CARTESIAN_POINT('Ctrl Pts',(53.0598329847647,29.467955981039,22.3790005439717));
#52614=CARTESIAN_POINT('Ctrl Pts',(53.0760731107924,29.5307966436041,22.3752521208703));
#52615=CARTESIAN_POINT('Ctrl Pts',(53.130699039501,29.7063173768748,22.364540696809));
#52616=CARTESIAN_POINT('Ctrl Pts',(53.1761169485835,29.8164652051821,22.3575129973853));
#52617=CARTESIAN_POINT('Ctrl Pts',(53.2383853048394,29.9359443700092,22.3491524672674));
#52618=CARTESIAN_POINT('Ctrl Pts',(53.2458687742928,29.9498956882499,22.3481645272101));
#52619=CARTESIAN_POINT('Ctrl Pts',(53.2582890630588,29.9724032684934,22.3465508262489));
#52620=CARTESIAN_POINT('Ctrl Pts',(53.2631248606693,29.981014703867,22.3459286313328));
#52621=CARTESIAN_POINT('Ctrl Pts',(53.2718539702567,29.9962923533435,22.3448160484956));
#52622=CARTESIAN_POINT('Ctrl Pts',(53.275722431704,30.0029725909519,22.3443265560172));
#52623=CARTESIAN_POINT('Ctrl Pts',(53.2839670109837,30.0170210333699,22.3432907044636));
#52624=CARTESIAN_POINT('Ctrl Pts',(53.2883520209901,30.0243838118137,22.3427440317953));
#52625=CARTESIAN_POINT('Ctrl Pts',(53.3001241268624,30.0438634796229,22.341287487662));
#52626=CARTESIAN_POINT('Ctrl Pts',(53.3075932079485,30.0559300077317,22.3403746518494));
#52627=CARTESIAN_POINT('Ctrl Pts',(53.344189427374,30.1136664708123,22.3359546852019));
#52628=CARTESIAN_POINT('Ctrl Pts',(53.3750375524976,30.1582131837948,22.332384621682));
#52629=CARTESIAN_POINT('Ctrl Pts',(53.4710172058588,30.2854202573017,22.3217001467797));
#52630=CARTESIAN_POINT('Ctrl Pts',(53.5409134440939,30.3642417298118,22.3144228628248));
#52631=CARTESIAN_POINT('Ctrl Pts',(53.7032292166296,30.520473820879,22.2987262026748));
#52632=CARTESIAN_POINT('Ctrl Pts',(53.7971238529569,30.5957911056109,22.2903214106043));
#52633=CARTESIAN_POINT('Ctrl Pts',(53.9104264742239,30.6709601448555,22.2813162909636));
#52634=CARTESIAN_POINT('Ctrl Pts',(53.923724942976,30.6795565822045,22.2802759860643));
#52635=CARTESIAN_POINT('Ctrl Pts',(53.9425991770478,30.6914410756005,22.2788242979449));
#52636=CARTESIAN_POINT('Ctrl Pts',(53.9480903320249,30.6948614886845,22.2784048687356));
#52637=CARTESIAN_POINT('Ctrl Pts',(53.9573548542675,30.7005699437952,22.2777022379552));
#52638=CARTESIAN_POINT('Ctrl Pts',(53.9611193167372,30.7028722679239,22.2774181213302));
#52639=CARTESIAN_POINT('Ctrl Pts',(53.9688180553954,30.7075457415525,22.2768399390771));
#52640=CARTESIAN_POINT('Ctrl Pts',(53.9727529292902,30.7099158222335,22.2765459422578));
#52641=CARTESIAN_POINT('Ctrl Pts',(53.9828031578799,30.7159221326631,22.2757987951736));
#52642=CARTESIAN_POINT('Ctrl Pts',(53.9889299056617,30.7195393130044,22.2753468587109));
#52643=CARTESIAN_POINT('Ctrl Pts',(54.0139331669215,30.7341211899004,22.273516286604));
#52644=CARTESIAN_POINT('Ctrl Pts',(54.0329705240681,30.7448089252109,22.2721542844037));
#52645=CARTESIAN_POINT('Ctrl Pts',(54.0837093534366,30.7722085016365,22.2685971189489));
#52646=CARTESIAN_POINT('Ctrl Pts',(54.1156932339018,30.7883828914282,22.2664284319025));
#52647=CARTESIAN_POINT('Ctrl Pts',(54.3082560096138,30.879332532698,22.2537025173719));
#52648=CARTESIAN_POINT('Ctrl Pts',(54.4777784629726,30.9333113102216,22.2437695716354));
#52649=CARTESIAN_POINT('Ctrl Pts',(54.7088976602232,30.9742343312022,22.2297093038134));
#52650=CARTESIAN_POINT('Ctrl Pts',(54.7659883876497,30.981812151576,22.2262035533025));
#52651=CARTESIAN_POINT('Ctrl Pts',(54.838171971324,30.9882307411456,22.2216924231182));
#52652=CARTESIAN_POINT('Ctrl Pts',(54.853034718526,30.9893845726872,22.2207594768401));
#52653=CARTESIAN_POINT('Ctrl Pts',(54.8767015203862,30.9909552234435,22.2192667992507));
#52654=CARTESIAN_POINT('Ctrl Pts',(54.8854980024805,30.9914804807956,22.2187104448917));
#52655=CARTESIAN_POINT('Ctrl Pts',(54.9019695441293,30.9923545410491,22.2176656307446));
#52656=CARTESIAN_POINT('Ctrl Pts',(54.9096437231439,30.9927173226681,22.2171776153755));
#52657=CARTESIAN_POINT('Ctrl Pts',(54.9268055593143,30.9934292744804,22.2160834257242));
#52658=CARTESIAN_POINT('Ctrl Pts',(54.9362939495634,30.9937550583067,22.2154765357684));
#52659=CARTESIAN_POINT('Ctrl Pts',(54.964301834862,30.9945165732256,22.2136792152674));
#52660=CARTESIAN_POINT('Ctrl Pts',(54.982825076913,30.9947620669439,22.2124829240611));
#52661=CARTESIAN_POINT('Ctrl Pts',(55.1281424834146,30.994663825164,22.203035420841));
#52662=CARTESIAN_POINT('Ctrl Pts',(55.2546163816618,30.9824894065802,22.1944119596635));
#52663=CARTESIAN_POINT('Ctrl Pts',(55.5191926350764,30.9312792723567,22.1757062655652));
#52664=CARTESIAN_POINT('Ctrl Pts',(55.6560162689696,30.8891923875666,22.1656282796835));
#52665=CARTESIAN_POINT('Ctrl Pts',(55.8033839513498,30.8259005291532,22.1549802122286));
#52666=CARTESIAN_POINT('Ctrl Pts',(55.8194943662817,30.8187269037097,22.1538195818));
#52667=CARTESIAN_POINT('Ctrl Pts',(55.8416510031535,30.8085068189757,22.1522302229855));
#52668=CARTESIAN_POINT('Ctrl Pts',(55.8477794842616,30.8056420671445,22.1517913435245));
#52669=CARTESIAN_POINT('Ctrl Pts',(55.8575701313108,30.8010046040626,22.1510915223317));
#52670=CARTESIAN_POINT('Ctrl Pts',(55.8612415875257,30.7992518007796,22.1508293902107));
#52671=CARTESIAN_POINT('Ctrl Pts',(55.8689102892833,30.7955618067127,22.1502825300579));
#52672=CARTESIAN_POINT('Ctrl Pts',(55.8729064588538,30.7936224817755,22.1499979443256));
#52673=CARTESIAN_POINT('Ctrl Pts',(55.8826389460832,30.7888591149401,22.1493057096109));
#52674=CARTESIAN_POINT('Ctrl Pts',(55.8883682921963,30.7860207788114,22.1488989343593));
#52675=CARTESIAN_POINT('Ctrl Pts',(55.9088601551993,30.7757460424047,22.1474463174213));
#52676=CARTESIAN_POINT('Ctrl Pts',(55.9235442290236,30.7681535248846,22.146409651711));
#52677=CARTESIAN_POINT('Ctrl Pts',(55.9597788134409,30.7488435637173,22.143857977051));
#52678=CARTESIAN_POINT('Ctrl Pts',(55.9812112508956,30.7369092587347,22.1423543996137));
#52679=CARTESIAN_POINT('Ctrl Pts',(56.0709394941548,30.6847544206982,22.1360607951342));
#52680=CARTESIAN_POINT('Ctrl Pts',(56.1370309272559,30.6408752159367,22.1314262586001));
#52681=CARTESIAN_POINT('Ctrl Pts',(56.3278848816975,30.4970809228322,22.1175273258594));
#52682=CARTESIAN_POINT('Ctrl Pts',(56.4434140708205,30.3860300646697,22.1083386247208));
#52683=CARTESIAN_POINT('Ctrl Pts',(56.5594680228495,30.2440454127757,22.0970362813726));
#52684=CARTESIAN_POINT('Ctrl Pts',(56.5741412891131,30.2254258979602,22.0955631581706));
#52685=CARTESIAN_POINT('Ctrl Pts',(56.594183169545,30.1990398348524,22.0934857231678));
#52686=CARTESIAN_POINT('Ctrl Pts',(56.5998341341592,30.1914895055922,22.0928924074817));
#52687=CARTESIAN_POINT('Ctrl Pts',(56.610090211931,30.1775817135092,22.0918014329077));
#52688=CARTESIAN_POINT('Ctrl Pts',(56.6147117661703,30.1712365652968,22.0913044201152));
#52689=CARTESIAN_POINT('Ctrl Pts',(56.6240070450825,30.1583150566358,22.0902936535355));
#52690=CARTESIAN_POINT('Ctrl Pts',(56.6286785607081,30.1517372945556,22.0897798279951));
#52691=CARTESIAN_POINT('Ctrl Pts',(56.6401262896793,30.1354093087656,22.0885060036167));
#52692=CARTESIAN_POINT('Ctrl Pts',(56.6468555246192,30.1256266767992,22.0877442481267));
#52693=CARTESIAN_POINT('Ctrl Pts',(56.6717534052805,30.0887301610368,22.0848761133982));
#52694=CARTESIAN_POINT('Ctrl Pts',(56.689342205288,30.0612330177196,22.0827483988628));
#52695=CARTESIAN_POINT('Ctrl Pts',(56.7317742321882,29.9911679014684,22.0773477467103));
#52696=CARTESIAN_POINT('Ctrl Pts',(56.7557282234358,29.9480894243627,22.0740456113054));
#52697=CARTESIAN_POINT('Ctrl Pts',(56.8247812581386,29.8122959517584,22.0636991339926));
#52698=CARTESIAN_POINT('Ctrl Pts',(56.864306594491,29.7169442821764,22.0565118771273));
#52699=CARTESIAN_POINT('Ctrl Pts',(56.9145299129415,29.5630806498938,22.0452357551412));
#52700=CARTESIAN_POINT('Ctrl Pts',(56.9302951920905,29.5064046284258,22.0411498066037));
#52701=CARTESIAN_POINT('Ctrl Pts',(56.9547852154069,29.40042415409,22.0337127819011));
#52702=CARTESIAN_POINT('Ctrl Pts',(56.9642037359643,29.3513251287401,22.0303462325659));
#52703=CARTESIAN_POINT('Ctrl Pts',(56.9730978000059,29.2932400739027,22.026493773977));
#52704=CARTESIAN_POINT('Ctrl Pts',(56.9743695761721,29.2845513182708,22.0259209056333));
#52705=CARTESIAN_POINT('Ctrl Pts',(56.9763424442228,29.270422239856,22.0249951836858));
#52706=CARTESIAN_POINT('Ctrl Pts',(56.9770785309122,29.2649870354986,22.0246404756779));
#52707=CARTESIAN_POINT('Ctrl Pts',(56.978352657116,29.2552780443603,22.0240094375561));
#52708=CARTESIAN_POINT('Ctrl Pts',(56.978899279649,29.2510054939982,22.0237326386927));
#52709=CARTESIAN_POINT('Ctrl Pts',(56.9800577335877,29.241711646977,22.0231324914836));
#52710=CARTESIAN_POINT('Ctrl Pts',(56.9806643062082,29.2366897887507,22.0228094375814));
#52711=CARTESIAN_POINT('Ctrl Pts',(56.9823231906738,29.2225026688582,22.0219001235922));
#52712=CARTESIAN_POINT('Ctrl Pts',(56.9833310495227,29.2133321956124,22.0213162771984));
#52713=CARTESIAN_POINT('Ctrl Pts',(56.9893033866144,29.1552842938777,22.0176435710284));
#52714=CARTESIAN_POINT('Ctrl Pts',(56.9925248057147,29.1062400867935,22.0146432965894));
#52715=CARTESIAN_POINT('Ctrl Pts',(56.9979573651124,28.9166105992374,22.0032684818477));
#52716=CARTESIAN_POINT('Ctrl Pts',(56.9871193359043,28.7760591004324,21.9952902217953));
#52717=CARTESIAN_POINT('Ctrl Pts',(56.9443482811274,28.5444162561162,21.9814599410495));
#52718=CARTESIAN_POINT('Ctrl Pts',(56.9204592460025,28.4523872896624,21.9757819451573));
#52719=CARTESIAN_POINT('Ctrl Pts',(56.8851797956597,28.3478017195607,21.9689290241223));
#52720=CARTESIAN_POINT('Ctrl Pts',(56.8800806145646,28.333244931807,21.9679661213253));
#52721=CARTESIAN_POINT('Ctrl Pts',(56.8714822425185,28.309582077704,21.9663853069995));
#52722=CARTESIAN_POINT('Ctrl Pts',(56.8680840988328,28.3004397911743,21.9657707225438));
#52723=CARTESIAN_POINT('Ctrl Pts',(56.8618815063645,28.2841199853164,21.9646666009084));
#52724=CARTESIAN_POINT('Ctrl Pts',(56.8591022379137,28.2769330560418,21.9641779078969));
#52725=CARTESIAN_POINT('Ctrl Pts',(56.8531185358715,28.2617223405605,21.9631383056347));
#52726=CARTESIAN_POINT('Ctrl Pts',(56.8499034810511,28.2537029295486,21.96258704961));
#52727=CARTESIAN_POINT('Ctrl Pts',(56.8411490887477,28.2322707644579,21.9611051889312));
#52728=CARTESIAN_POINT('Ctrl Pts',(56.8355153987317,28.2188973506798,21.9601714345742));
#52729=CARTESIAN_POINT('Ctrl Pts',(56.8065643980926,28.1522157981566,21.9554689429363));
#52730=CARTESIAN_POINT('Ctrl Pts',(56.7810705427922,28.0998891415957,21.9516270768162));
#52731=CARTESIAN_POINT('Ctrl Pts',(56.6990530758438,27.9487150136528,21.9400637408719));
#52732=CARTESIAN_POINT('Ctrl Pts',(56.6363204513971,27.8535133798241,21.9321538107858));
#52733=CARTESIAN_POINT('Ctrl Pts',(56.4998455899081,27.6805940728614,21.9168006916445));
#52734=CARTESIAN_POINT('Ctrl Pts',(56.4272732596328,27.6024076848864,21.9093883189934));
#52735=CARTESIAN_POINT('Ctrl Pts',(56.3369298733133,27.5194914413605,21.9012638662573));
#52736=CARTESIAN_POINT('Ctrl Pts',(56.3249293585527,27.508742372175,21.9002051567743));
#52737=CARTESIAN_POINT('Ctrl Pts',(56.3078944002621,27.4938518519565,21.8987323655551));
#52738=CARTESIAN_POINT('Ctrl Pts',(56.3029682492781,27.4895882182928,21.8983099294069));
#52739=CARTESIAN_POINT('Ctrl Pts',(56.2949675216596,27.482731779217,21.8976295410589));
#52740=CARTESIAN_POINT('Ctrl Pts',(56.2919058874237,27.4801240462822,21.8973705155157));
#52741=CARTESIAN_POINT('Ctrl Pts',(56.2854087202918,27.4746239308153,21.896823695741));
#52742=CARTESIAN_POINT('Ctrl Pts',(56.2819712651923,27.4717338560896,21.8965360750329));
#52743=CARTESIAN_POINT('Ctrl Pts',(56.2734295870199,27.4646014527571,21.8958254507801));
#52744=CARTESIAN_POINT('Ctrl Pts',(56.2683138424793,27.4603728984157,21.8954034326054));
#52745=CARTESIAN_POINT('Ctrl Pts',(56.249104242892,27.4446554148857,21.8938316995477));
#52746=CARTESIAN_POINT('Ctrl Pts',(56.2348741166123,27.4333334244437,21.8926932577358));
#52747=CARTESIAN_POINT('Ctrl Pts',(56.1984435689165,27.4051528302748,21.8898378276753));
#52748=CARTESIAN_POINT('Ctrl Pts',(56.1760403984157,27.3885616301051,21.8881360860405));
#52749=CARTESIAN_POINT('Ctrl Pts',(56.0721190181157,27.3149222997963,21.8804494352355));
#52750=CARTESIAN_POINT('Ctrl Pts',(55.9867461779164,27.2635492924463,21.8746983888214));
#52751=CARTESIAN_POINT('Ctrl Pts',(55.7798689253882,27.1592663222408,21.8612439595537));
#52752=CARTESIAN_POINT('Ctrl Pts',(55.6562419831442,27.1116576282914,21.8535363897701));
#52753=CARTESIAN_POINT('Ctrl Pts',(55.5053468750363,27.0701697235569,21.8439024252603));
#52754=CARTESIAN_POINT('Ctrl Pts',(55.4817552474219,27.0641456248202,21.8423908980651));
#52755=CARTESIAN_POINT('Ctrl Pts',(55.4485251495608,27.0563053923958,21.8402518899577));
#52756=CARTESIAN_POINT('Ctrl Pts',(55.438973958947,27.0541260587233,21.8396359462226));
#52757=CARTESIAN_POINT('Ctrl Pts',(55.422351766823,27.0504619146785,21.8385618624199));
#52758=CARTESIAN_POINT('Ctrl Pts',(55.415287976312,27.0489449890971,21.838104749518));
#52759=CARTESIAN_POINT('Ctrl Pts',(55.4005282244063,27.0458591678138,21.837148148686));
#52760=CARTESIAN_POINT('Ctrl Pts',(55.3928309390589,27.0442972871621,21.8366484473059));
#52761=CARTESIAN_POINT('Ctrl Pts',(55.3745563030294,27.0407013616197,21.8354600157491));
#52762=CARTESIAN_POINT('Ctrl Pts',(55.3639713914206,27.0387074677042,21.834770029925));
#52763=CARTESIAN_POINT('Ctrl Pts',(55.3283634708023,27.032298134205,21.8324431422806));
#52764=CARTESIAN_POINT('Ctrl Pts',(55.3032732046244,27.0282752558391,21.8307939936068));
#52765=CARTESIAN_POINT('Ctrl Pts',(55.2431334100836,27.0198076868543,21.8268165612725));
#52766=CARTESIAN_POINT('Ctrl Pts',(55.2080301959714,27.0158128521791,21.8244750945022));
#52767=CARTESIAN_POINT('Ctrl Pts',(55.0703578944151,27.0038387858167,21.8152139911706));
#52768=CARTESIAN_POINT('Ctrl Pts',(54.9673496283287,27.0028671916453,21.8081052102771));
#52769=CARTESIAN_POINT('Ctrl Pts',(54.7416239791641,27.0182088185041,21.7923455960044));
#52770=CARTESIAN_POINT('Ctrl Pts',(54.61954221925,27.0379827645893,21.7837003415978));
#52771=CARTESIAN_POINT('Ctrl Pts',(54.4848223885558,27.0728603010286,21.7744850170074));
#52772=CARTESIAN_POINT('Ctrl Pts',(54.4696289384813,27.0769862287012,21.7734508041158));
#52773=CARTESIAN_POINT('Ctrl Pts',(54.4482777182078,27.0830566684888,21.772006126021));
#52774=CARTESIAN_POINT('Ctrl Pts',(54.4420785588406,27.0848517340103,21.7715877147889));
#52775=CARTESIAN_POINT('Ctrl Pts',(54.4316587535354,27.0879238423909,21.7708863113902));
#52776=CARTESIAN_POINT('Ctrl Pts',(54.4274334686279,27.0891848406086,21.7706024109387));
#52777=CARTESIAN_POINT('Ctrl Pts',(54.4188112020043,27.0917892462421,21.7700241894135));
#52778=CARTESIAN_POINT('Ctrl Pts',(54.4144146315422,27.0931338597171,21.7697299398412));
#52779=CARTESIAN_POINT('Ctrl Pts',(54.4032083999987,27.0966035004131,21.7689813552683));
#52780=CARTESIAN_POINT('Ctrl Pts',(54.3964053478848,27.0987498985961,21.7685282433718));
#52781=CARTESIAN_POINT('Ctrl Pts',(54.369571621524,27.1073746251021,21.7667457564929));
#52782=CARTESIAN_POINT('Ctrl Pts',(54.3496316992131,27.1141336456549,21.7654316957567));
#52783=CARTESIAN_POINT('Ctrl Pts',(54.2973124034251,27.1327968594876,21.7620023921236));
#52784=CARTESIAN_POINT('Ctrl Pts',(54.2651273887918,27.1452277918205,21.759911788675));
#52785=CARTESIAN_POINT('Ctrl Pts',(54.0871224263905,27.2193408557184,21.7483720451434));
#52786=CARTESIAN_POINT('Ctrl Pts',(53.9487243055471,27.2973790158574,21.7394425326835));
#52787=CARTESIAN_POINT('Ctrl Pts',(53.7596366433212,27.4359303293865,21.7255568693647));
#52788=CARTESIAN_POINT('Ctrl Pts',(53.7008995385378,27.484364414519,21.7209668128009));
#52789=CARTESIAN_POINT('Ctrl Pts',(53.6342533272438,27.5460464131429,21.7153234193134));
#52790=CARTESIAN_POINT('Ctrl Pts',(53.6235427051677,27.5561820391053,21.7144021865132));
#52791=CARTESIAN_POINT('Ctrl Pts',(53.6060844113694,27.5730739183128,21.7128761905145));
#52792=CARTESIAN_POINT('Ctrl Pts',(53.5992710086468,27.5797616402398,21.7122743729387));
#52793=CARTESIAN_POINT('Ctrl Pts',(53.5870590847981,27.5919216576817,21.7111841593285));
#52794=CARTESIAN_POINT('Ctrl Pts',(53.5816436576878,27.5973767678048,21.7106965213601));
#52795=CARTESIAN_POINT('Ctrl Pts',(53.571197290975,27.6080220448201,21.709747636686));
#52796=CARTESIAN_POINT('Ctrl Pts',(53.566162760002,27.6132085319105,21.7092865574761));
#52797=CARTESIAN_POINT('Ctrl Pts',(53.5524946308395,27.6274431974088,21.7080243475205));
#52798=CARTESIAN_POINT('Ctrl Pts',(53.5439178745069,27.6365452694837,21.7072207993786));
#52799=CARTESIAN_POINT('Ctrl Pts',(53.5076950252474,27.6757183165869,21.7037769947041));
#52800=CARTESIAN_POINT('Ctrl Pts',(53.4808922020602,27.7065522005325,21.7011018837599));
#52801=CARTESIAN_POINT('Ctrl Pts',(53.4121394175042,27.7907319018335,21.6938856302979));
#52802=CARTESIAN_POINT('Ctrl Pts',(53.3719353200296,27.8454289052491,21.6892832737757));
#52803=CARTESIAN_POINT('Ctrl Pts',(53.3004259960457,27.9538975417717,21.6803428151126));
#52804=CARTESIAN_POINT('Ctrl Pts',(53.2686931772748,28.0072974703124,21.6760205067402));
#52805=CARTESIAN_POINT('Ctrl Pts',(53.2065816110673,28.1238832709777,21.6668134307857));
#52806=CARTESIAN_POINT('Ctrl Pts',(53.1769351165128,28.1873714011938,21.6619332178443));
#52807=CARTESIAN_POINT('Ctrl Pts',(53.1317504450598,28.2991265983257,21.6536885513824));
#52808=CARTESIAN_POINT('Ctrl Pts',(53.1145976000471,28.3466710915223,21.6502838892133));
#52809=CARTESIAN_POINT('Ctrl Pts',(53.096595283424,28.4032122476348,21.646393462868));
#52810=CARTESIAN_POINT('Ctrl Pts',(53.0939787288689,28.4116225214854,21.6458188371866));
#52811=CARTESIAN_POINT('Ctrl Pts',(53.089820956718,28.4253055112258,21.6448908444411));
#52812=CARTESIAN_POINT('Ctrl Pts',(53.0882456951202,28.4305676402481,21.6445356084347));
#52813=CARTESIAN_POINT('Ctrl Pts',(53.0854737665576,28.4399683735514,21.6439040006906));
#52814=CARTESIAN_POINT('Ctrl Pts',(53.0842687534931,28.4441044041449,21.6436271566926));
#52815=CARTESIAN_POINT('Ctrl Pts',(53.0816796105856,28.4530996686802,21.6430273374766));
#52816=CARTESIAN_POINT('Ctrl Pts',(53.0803005409883,28.4579602622801,21.6427046539598));
#52817=CARTESIAN_POINT('Ctrl Pts',(53.0764629770322,28.4716842927374,21.6417974368092));
#52818=CARTESIAN_POINT('Ctrl Pts',(53.0740472608403,28.4805597055689,21.6412152991928));
#52819=CARTESIAN_POINT('Ctrl Pts',(53.0687452361623,28.5005851011892,21.6399114381129));
#52820=CARTESIAN_POINT('Ctrl Pts',(53.0658939032587,28.5117440996214,21.6391915435963));
#52821=CARTESIAN_POINT('Ctrl Pts',(53.0248278849474,28.6784674989925,21.6285265107986));
#52822=CARTESIAN_POINT('Ctrl Pts',(53.0053877304754,28.8380719780943,21.6194559710624));
#52823=CARTESIAN_POINT('Ctrl Pts',(53.0052507292241,28.9982943508983,21.6101045922788));
#52824=CARTESIAN_POINT('Ctrl Pts',(53.0052507279944,28.9982957896247,21.6101045083075));
#52825=CARTESIAN_POINT('Ctrl Pts',(53.0051543369249,29.111119897792,21.6035195283877));
#52826=CARTESIAN_POINT('Ctrl Pts',(53.0146297098485,29.2237376212089,21.5968303826914));
#52827=CARTESIAN_POINT('Ctrl Pts',(53.0356382363993,29.3470761145801,21.5890638196957));
#52828=CARTESIAN_POINT('Ctrl Pts',(53.0378165173038,29.3591864938383,21.5882966432258));
#52829=CARTESIAN_POINT('Ctrl Pts',(53.0416896620939,29.3796320814841,21.5869932937447));
#52830=CARTESIAN_POINT('Ctrl Pts',(53.043326067099,29.387978109682,21.5864589521394));
#52831=CARTESIAN_POINT('Ctrl Pts',(53.0455671781555,29.3990333444643,21.5857480115283));
#52832=CARTESIAN_POINT('Ctrl Pts',(53.0461242535664,29.401752202751,21.5855729141647));
#52833=CARTESIAN_POINT('Ctrl Pts',(53.0466869980088,29.4044698737264,21.5853976382171));
#52834=CARTESIAN_POINT('Ctrl Pts',(53.0466869889941,29.4044698301913,21.4261018347978));
#52835=CARTESIAN_POINT('Ctrl Pts',(53.0326898260591,29.3368730938287,21.4301230217525));
#52836=CARTESIAN_POINT('Ctrl Pts',(53.0222071592501,29.2685769241553,21.4341119456716));
#52837=CARTESIAN_POINT('Ctrl Pts',(53.0053974029733,29.101643606587,21.4439176190189));
#52838=CARTESIAN_POINT('Ctrl Pts',(53.0028121123142,29.0028444611566,21.4497733469691));
#52839=CARTESIAN_POINT('Ctrl Pts',(53.0086640626487,28.881050474017,21.4572921980709));
#52840=CARTESIAN_POINT('Ctrl Pts',(53.0101852158744,28.8578561986267,21.4587370814236));
#52841=CARTESIAN_POINT('Ctrl Pts',(53.0129727323458,28.8243347891428,21.4608463566309));
#52842=CARTESIAN_POINT('Ctrl Pts',(53.0139151663532,28.8139821090879,21.4615006914772));
#52843=CARTESIAN_POINT('Ctrl Pts',(53.0157054367892,28.7958839713239,21.4626498665838));
#52844=CARTESIAN_POINT('Ctrl Pts',(53.0165178200337,28.788135171123,21.4631435918216));
#52845=CARTESIAN_POINT('Ctrl Pts',(53.0182923695322,28.7721145532399,21.46416797403));
#52846=CARTESIAN_POINT('Ctrl Pts',(53.0192609792212,28.7638436161743,21.4646988232406));
#52847=CARTESIAN_POINT('Ctrl Pts',(53.0218851739499,28.7425886129283,21.4660682668944));
#52848=CARTESIAN_POINT('Ctrl Pts',(53.0236167993391,28.7296145012734,21.4669092235009));
#52849=CARTESIAN_POINT('Ctrl Pts',(53.030957964626,28.6784560454844,21.4702457186156));
#52850=CARTESIAN_POINT('Ctrl Pts',(53.037547178178,28.6404229796717,21.4727716231307));
#52851=CARTESIAN_POINT('Ctrl Pts',(53.0806777163801,28.4282650601508,21.487126918388));
#52852=CARTESIAN_POINT('Ctrl Pts',(53.1392826006906,28.2594675373326,21.4996600711593));
#52853=CARTESIAN_POINT('Ctrl Pts',(53.2500330016433,28.0401866019628,21.5166520829093));
#52854=CARTESIAN_POINT('Ctrl Pts',(53.2836751641037,27.9812472549074,21.5212854254095));
#52855=CARTESIAN_POINT('Ctrl Pts',(53.3280019545623,27.9120403227734,21.5267146822501));
#52856=CARTESIAN_POINT('Ctrl Pts',(53.3358766949517,27.9000330108804,21.527656162949));
#52857=CARTESIAN_POINT('Ctrl Pts',(53.3472499933094,27.8830928796436,21.5289825604316));
#52858=CARTESIAN_POINT('Ctrl Pts',(53.3506421653916,27.8780896489335,21.5293740750825));
#52859=CARTESIAN_POINT('Ctrl Pts',(53.356530579013,27.8694890557082,21.5300465801928));
#52860=CARTESIAN_POINT('Ctrl Pts',(53.3590160020726,27.8658843740917,21.5303282827753));
#52861=CARTESIAN_POINT('Ctrl Pts',(53.3638848491774,27.8588724591405,21.5308759132449));
#52862=CARTESIAN_POINT('Ctrl Pts',(53.3662670632256,27.8554644857747,21.5311419225735));
#52863=CARTESIAN_POINT('Ctrl Pts',(53.3728165779378,27.846156924004,21.5318680775835));
#52864=CARTESIAN_POINT('Ctrl Pts',(53.377005342635,27.8402724117119,21.5323267910038));
#52865=CARTESIAN_POINT('Ctrl Pts',(53.3933614059699,27.817557061976,21.5340965727038));
#52866=CARTESIAN_POINT('Ctrl Pts',(53.4057597841301,27.8008932127253,21.5353928621875));
#52867=CARTESIAN_POINT('Ctrl Pts',(53.5035691672887,27.6736335033382,21.5453027078332));
#52868=CARTESIAN_POINT('Ctrl Pts',(53.6001387647533,27.5720812053738,21.5532912755637));
#52869=CARTESIAN_POINT('Ctrl Pts',(53.8037562360298,27.3986458058006,21.5688512959098));
#52870=CARTESIAN_POINT('Ctrl Pts',(53.9086817374746,27.3253798759876,21.5763673221513));
#52871=CARTESIAN_POINT('Ctrl Pts',(54.0349432554034,27.2541500260347,21.5853661824784));
#52872=CARTESIAN_POINT('Ctrl Pts',(54.050115343245,27.2458489912622,21.5864463430546));
#52873=CARTESIAN_POINT('Ctrl Pts',(54.0735558311548,27.2334173848938,21.5881142769111));
#52874=CARTESIAN_POINT('Ctrl Pts',(54.0817484454076,27.2291451183499,21.588697065626));
#52875=CARTESIAN_POINT('Ctrl Pts',(54.0967313600687,27.2214637893646,21.5897627265298));
#52876=CARTESIAN_POINT('Ctrl Pts',(54.1035120547547,27.2180362938999,21.5902449439673));
#52877=CARTESIAN_POINT('Ctrl Pts',(54.1183588435381,27.2106377495471,21.5913007431632));
#52878=CARTESIAN_POINT('Ctrl Pts',(54.1264325046708,27.2066823430086,21.5918748543908));
#52879=CARTESIAN_POINT('Ctrl Pts',(54.1486670559882,27.1959750844159,21.5934559993439));
#52880=CARTESIAN_POINT('Ctrl Pts',(54.1628810508908,27.1893356137982,21.5944668621273));
#52881=CARTESIAN_POINT('Ctrl Pts',(54.2394653392656,27.1546570023187,21.5999149482736));
#52882=CARTESIAN_POINT('Ctrl Pts',(54.3031615134258,27.1296743463669,21.6044541979121));
#52883=CARTESIAN_POINT('Ctrl Pts',(54.5254893990466,27.0554088775765,21.6203265488493));
#52884=CARTESIAN_POINT('Ctrl Pts',(54.6888980684427,27.0226784634631,21.6321034574298));
#52885=CARTESIAN_POINT('Ctrl Pts',(54.8894471260371,27.0080069514659,21.6458650583217));
#52886=CARTESIAN_POINT('Ctrl Pts',(54.9244982428272,27.006370642205,21.6482419143026));
#52887=CARTESIAN_POINT('Ctrl Pts',(54.9740456268257,27.0053663536532,21.6515463258986));
#52888=CARTESIAN_POINT('Ctrl Pts',(54.9885182770832,27.005230537293,21.6525048464667));
#52889=CARTESIAN_POINT('Ctrl Pts',(55.0140059888009,27.0052687618697,21.6541796672458));
#52890=CARTESIAN_POINT('Ctrl Pts',(55.0250203785965,27.0053765082341,21.6548990831112));
#52891=CARTESIAN_POINT('Ctrl Pts',(55.0414623546451,27.0056735681967,21.6559659579855));
#52892=CARTESIAN_POINT('Ctrl Pts',(55.046890758797,27.0057938166122,21.6563170447705));
#52893=CARTESIAN_POINT('Ctrl Pts',(55.0562084738759,27.0060382875121,21.6569176286165));
#52894=CARTESIAN_POINT('Ctrl Pts',(55.0600979741194,27.006151726476,21.6571677149568));
#52895=CARTESIAN_POINT('Ctrl Pts',(55.0689203370409,27.006434874318,21.6577335643256));
#52896=CARTESIAN_POINT('Ctrl Pts',(55.0738529119217,27.0066115100507,21.6580489398408));
#52897=CARTESIAN_POINT('Ctrl Pts',(55.087218429008,27.0071398080612,21.6589009331939));
#52898=CARTESIAN_POINT('Ctrl Pts',(55.095649990006,27.0075266916801,21.6594356439555));
#52899=CARTESIAN_POINT('Ctrl Pts',(55.136504050019,27.0096612198826,21.6620142101926));
#52900=CARTESIAN_POINT('Ctrl Pts',(55.168885068367,27.0121469044711,21.6640204171014));
#52901=CARTESIAN_POINT('Ctrl Pts',(55.404232352239,27.0360060032627,21.6784206717914));
#52902=CARTESIAN_POINT('Ctrl Pts',(55.6029251026515,27.0876252512724,21.6897151636601));
#52903=CARTESIAN_POINT('Ctrl Pts',(55.8406180259541,27.1901970622447,21.7052634624077));
#52904=CARTESIAN_POINT('Ctrl Pts',(55.8899706301136,27.2139493837507,21.7086051396365));
#52905=CARTESIAN_POINT('Ctrl Pts',(55.9508463435213,27.246397552357,21.7129042856659));
#52906=CARTESIAN_POINT('Ctrl Pts',(55.9633394991137,27.2532294637553,21.7137962338686));
#52907=CARTESIAN_POINT('Ctrl Pts',(55.9832415624452,27.2643914012693,21.7152332154343));
#52908=CARTESIAN_POINT('Ctrl Pts',(55.9906976796374,27.2686365829308,21.7157752298101));
#52909=CARTESIAN_POINT('Ctrl Pts',(56.004807414227,27.2767910245874,21.716808017208));
#52910=CARTESIAN_POINT('Ctrl Pts',(56.0114662027884,27.2806910601878,21.7172984523943));
#52911=CARTESIAN_POINT('Ctrl Pts',(56.0265781343705,27.2896602539413,21.7184184986742));
#52912=CARTESIAN_POINT('Ctrl Pts',(56.035016619846,27.2947535943949,21.7190489764413));
#52913=CARTESIAN_POINT('Ctrl Pts',(56.0568541695821,27.3081562126981,21.7206939104042));
#52914=CARTESIAN_POINT('Ctrl Pts',(56.0701928740682,27.316562051885,21.7217118661511));
#52915=CARTESIAN_POINT('Ctrl Pts',(56.193079677447,27.396054116401,21.7312155434476));
#52916=CARTESIAN_POINT('Ctrl Pts',(56.2954785588323,27.4775659943593,21.7401009757547));
#52917=CARTESIAN_POINT('Ctrl Pts',(56.4555243147278,27.6328763654893,21.7555882373448));
#52918=CARTESIAN_POINT('Ctrl Pts',(56.5173263503175,27.7018092581273,21.76207309058));
#52919=CARTESIAN_POINT('Ctrl Pts',(56.611082256705,27.8222640172783,21.7725658297789));
#52920=CARTESIAN_POINT('Ctrl Pts',(56.6458770911098,27.8713998997048,21.7766407568717));
#52921=CARTESIAN_POINT('Ctrl Pts',(56.6836345385913,27.9301887422015,21.7812209328473));
#52922=CARTESIAN_POINT('Ctrl Pts',(56.6888096997353,27.9383770942622,21.7818524659045));
#52923=CARTESIAN_POINT('Ctrl Pts',(56.6966482951519,27.9509820228463,21.7828144609058));
#52924=CARTESIAN_POINT('Ctrl Pts',(56.6993545047949,27.9553716343531,21.7831475991763));
#52925=CARTESIAN_POINT('Ctrl Pts',(56.7042863298049,27.9634411918571,21.7837565209236));
#52926=CARTESIAN_POINT('Ctrl Pts',(56.7065170632049,27.9671178332437,21.7840326271597));
#52927=CARTESIAN_POINT('Ctrl Pts',(56.7115025998036,27.9753951169,21.7846512645056));
#52928=CARTESIAN_POINT('Ctrl Pts',(56.7142507477354,27.9799996612229,21.7849933657298));
#52929=CARTESIAN_POINT('Ctrl Pts',(56.7212446230271,27.9918260618727,21.7858669626214));
#52930=CARTESIAN_POINT('Ctrl Pts',(56.7254635340341,27.9990637681063,21.7863967895636));
#52931=CARTESIAN_POINT('Ctrl Pts',(56.7506730196657,28.042944700352,21.7895814181753));
#52932=CARTESIAN_POINT('Ctrl Pts',(56.7705428915108,28.0802232244211,21.7921711936333));
#52933=CARTESIAN_POINT('Ctrl Pts',(56.8014196790028,28.1428671715307,21.7963814635769));
#52934=CARTESIAN_POINT('Ctrl Pts',(56.8131087773977,28.1678784872796,21.7980264448393));
#52935=CARTESIAN_POINT('Ctrl Pts',(56.8437140475889,28.2370744009187,21.8025003474452));
#52936=CARTESIAN_POINT('Ctrl Pts',(56.8615587982408,28.2817130944537,21.805302308808));
#52937=CARTESIAN_POINT('Ctrl Pts',(56.9159862333013,28.433563677902,21.8146800581273));
#52938=CARTESIAN_POINT('Ctrl Pts',(56.9450476328063,28.5432273704115,21.8212138781943));
#52939=CARTESIAN_POINT('Ctrl Pts',(56.9746896007058,28.7119107011216,21.8314772757107));
#52940=CARTESIAN_POINT('Ctrl Pts',(56.9822330190645,28.7694663422195,21.8350128058286));
#52941=CARTESIAN_POINT('Ctrl Pts',(56.9885125258223,28.8417099940911,21.8395304752656));
#52942=CARTESIAN_POINT('Ctrl Pts',(56.9896105291314,28.8561677495695,21.8404384778559));
#52943=CARTESIAN_POINT('Ctrl Pts',(56.9911109417793,28.8792548929383,21.8418951966982));
#52944=CARTESIAN_POINT('Ctrl Pts',(56.9916150896518,28.8878773250058,21.8424407429929));
#52945=CARTESIAN_POINT('Ctrl Pts',(56.9924630437307,28.9041983047796,21.8434763342679));
#52946=CARTESIAN_POINT('Ctrl Pts',(56.9928182679779,28.9118961207521,21.8439660144987));
#52947=CARTESIAN_POINT('Ctrl Pts',(56.9935221909096,28.9293455529221,21.8450789234196));
#52948=CARTESIAN_POINT('Ctrl Pts',(56.9938439551319,28.9390980003042,21.845702977621));
#52949=CARTESIAN_POINT('Ctrl Pts',(56.9944900081758,28.9642856427506,21.8473201914177));
#52950=CARTESIAN_POINT('Ctrl Pts',(56.9947066745876,28.9797227150708,21.8483166590519));
#52951=CARTESIAN_POINT('Ctrl Pts',(56.9949757611202,29.0906323886909,21.8555154645358));
#52952=CARTESIAN_POINT('Ctrl Pts',(56.9883530580062,29.1859835505098,21.8619240371279));
#52953=CARTESIAN_POINT('Ctrl Pts',(56.9552288061438,29.41921775728,21.8780997667597));
#52954=CARTESIAN_POINT('Ctrl Pts',(56.9209633799058,29.5554822622232,21.888008849744));
#52955=CARTESIAN_POINT('Ctrl Pts',(56.8558056995437,29.7330893207081,21.9009298231738));
#52956=CARTESIAN_POINT('Ctrl Pts',(56.837212222332,29.7785158201695,21.9042311120878));
#52957=CARTESIAN_POINT('Ctrl Pts',(56.813154748049,29.8316143759536,21.9080490748728));
#52958=CARTESIAN_POINT('Ctrl Pts',(56.8092905560906,29.8399882750129,21.9086499398049));
#52959=CARTESIAN_POINT('Ctrl Pts',(56.8032174362263,29.8529126679774,21.9095750484779));
#52960=CARTESIAN_POINT('Ctrl Pts',(56.8010491032363,29.8574819360236,21.9099016665574));
#52961=CARTESIAN_POINT('Ctrl Pts',(56.7970018776368,29.8659274616107,21.9105044754199));
#52962=CARTESIAN_POINT('Ctrl Pts',(56.7951278198106,29.8698058565635,21.9107809433718));
#52963=CARTESIAN_POINT('Ctrl Pts',(56.7908384823345,29.8786098027946,21.9114077393708));
#52964=CARTESIAN_POINT('Ctrl Pts',(56.7884154408008,29.8835314755013,21.9117575841526));
#52965=CARTESIAN_POINT('Ctrl Pts',(56.7820596900496,29.8963079748639,21.9126644892759));
#52966=CARTESIAN_POINT('Ctrl Pts',(56.7780952955702,29.9041470296405,21.9132196587441));
#52967=CARTESIAN_POINT('Ctrl Pts',(56.7512034424082,29.9564610416247,21.9169177992159));
#52968=CARTESIAN_POINT('Ctrl Pts',(56.7266592536226,30.0000899763826,21.9199691089865));
#52969=CARTESIAN_POINT('Ctrl Pts',(56.6698072448161,30.092802913023,21.9264812092313));
#52970=CARTESIAN_POINT('Ctrl Pts',(56.6369203194908,30.1414758019681,21.9299184786696));
#52971=CARTESIAN_POINT('Ctrl Pts',(56.5405308079826,30.2713813356631,21.9393362646317));
#52972=CARTESIAN_POINT('Ctrl Pts',(56.472811461787,30.3492484060225,21.9452702183037));
#52973=CARTESIAN_POINT('Ctrl Pts',(56.3642486454867,30.4561193619647,21.9543070540327));
#52974=CARTESIAN_POINT('Ctrl Pts',(56.3278483059836,30.4893879037489,21.9572673837152));
#52975=CARTESIAN_POINT('Ctrl Pts',(56.2735121908096,30.5354726392185,21.9616213179429));
#52976=CARTESIAN_POINT('Ctrl Pts',(56.256536716552,30.5493950270616,21.9629728157528));
#52977=CARTESIAN_POINT('Ctrl Pts',(56.2256194625723,30.5739094309909,21.9654214623042));
#52978=CARTESIAN_POINT('Ctrl Pts',(56.2117613254909,30.5846035541081,21.9665145448715));
#52979=CARTESIAN_POINT('Ctrl Pts',(56.1903408615432,30.6006880963543,21.9681982721597));
#52980=CARTESIAN_POINT('Ctrl Pts',(56.182878421693,30.6062105662989,21.9687837813924));
#52981=CARTESIAN_POINT('Ctrl Pts',(56.1692377802098,30.6161585091717,21.9698522503255));
#52982=CARTESIAN_POINT('Ctrl Pts',(56.163072288097,30.6206011734851,21.9703345368431));
#52983=CARTESIAN_POINT('Ctrl Pts',(56.1495888541343,30.6302003463717,21.97138791928));
#52984=CARTESIAN_POINT('Ctrl Pts',(56.1422613110252,30.6353430208707,21.9719595280313));
#52985=CARTESIAN_POINT('Ctrl Pts',(56.1221368617105,30.6492656765441,21.9735272362233));
#52986=CARTESIAN_POINT('Ctrl Pts',(56.1092719287055,30.6579457693105,21.9745270586532));
#52987=CARTESIAN_POINT('Ctrl Pts',(56.0412036294163,30.702725192572,21.9798059464523));
#52988=CARTESIAN_POINT('Ctrl Pts',(55.9843417605355,30.7362165005147,21.9841796263484));
#52989=CARTESIAN_POINT('Ctrl Pts',(55.7766837935421,30.8450425765089,22.000031335567));
#52990=CARTESIAN_POINT('Ctrl Pts',(55.6181520175082,30.9040212223296,22.0119854499516));
#52991=CARTESIAN_POINT('Ctrl Pts',(55.4197768690426,30.950399451454,22.0259298360871));
#52992=CARTESIAN_POINT('Ctrl Pts',(55.3852364749688,30.9575146973316,22.0283189908872));
#52993=CARTESIAN_POINT('Ctrl Pts',(55.329281000868,30.9675027867316,22.0321093197401));
#52994=CARTESIAN_POINT('Ctrl Pts',(55.3079770997849,30.9709498701211,22.0335338666503));
#52995=CARTESIAN_POINT('Ctrl Pts',(55.2796099601323,30.9750686103723,22.0354025085003));
#52996=CARTESIAN_POINT('Ctrl Pts',(55.2725939745955,30.9760491578249,22.0358623920578));
#52997=CARTESIAN_POINT('Ctrl Pts',(55.2610269212721,30.9776029800429,22.0366166649311));
#52998=CARTESIAN_POINT('Ctrl Pts',(55.2564789058193,30.9781979608235,22.0369122375321));
#52999=CARTESIAN_POINT('Ctrl Pts',(55.2475470559683,30.9793351228833,22.0374907014316));
#53000=CARTESIAN_POINT('Ctrl Pts',(55.2431634162335,30.9798784374832,22.0377736514599));
#53001=CARTESIAN_POINT('Ctrl Pts',(55.2323315595517,30.9811844359558,22.0384705395914));
#53002=CARTESIAN_POINT('Ctrl Pts',(55.2258812838997,30.9819302135095,22.0388835424001));
#53003=CARTESIAN_POINT('Ctrl Pts',(55.2035451186552,30.984402248269,22.0403071781012));
#53004=CARTESIAN_POINT('Ctrl Pts',(55.1876417267717,30.9859691634881,22.0413094073121));
#53005=CARTESIAN_POINT('Ctrl Pts',(55.0575696636511,30.9972083091225,22.0494260045621));
#53006=CARTESIAN_POINT('Ctrl Pts',(54.9427650930077,30.9972196809258,22.0560912670462));
#53007=CARTESIAN_POINT('Ctrl Pts',(54.7210883157731,30.9780992741398,22.0690161452696));
#53008=CARTESIAN_POINT('Ctrl Pts',(54.6145308213104,30.9601224604578,22.0752581106597));
#53009=CARTESIAN_POINT('Ctrl Pts',(54.4738224377186,30.9244620008916,22.0839660105202));
#53010=CARTESIAN_POINT('Ctrl Pts',(54.4379574464821,30.9142948421327,22.0862263253102));
#53011=CARTESIAN_POINT('Ctrl Pts',(54.3771407039134,30.8951978241047,22.0901442301412));
#53012=CARTESIAN_POINT('Ctrl Pts',(54.3520429829838,30.8867644520071,22.0917863258965));
#53013=CARTESIAN_POINT('Ctrl Pts',(54.3168154391487,30.87414147518,22.0941304510988));
#53014=CARTESIAN_POINT('Ctrl Pts',(54.3065402083608,30.870363847745,22.0948189646843));
#53015=CARTESIAN_POINT('Ctrl Pts',(54.2889178145575,30.8637199028417,22.0960082596749));
#53016=CARTESIAN_POINT('Ctrl Pts',(54.2815555243378,30.8608942160159,22.096507685885));
#53017=CARTESIAN_POINT('Ctrl Pts',(54.2675152332534,30.8554097369493,22.0974651112245));
#53018=CARTESIAN_POINT('Ctrl Pts',(54.2608344558986,30.8527583549089,22.0979228566811));
#53019=CARTESIAN_POINT('Ctrl Pts',(54.2435299184012,30.8457822581777,22.0991142418413));
#53020=CARTESIAN_POINT('Ctrl Pts',(54.2329289887807,30.8414019614572,22.0998497347644));
#53021=CARTESIAN_POINT('Ctrl Pts',(54.2025837339469,30.8285558125094,22.1019716358125));
#53022=CARTESIAN_POINT('Ctrl Pts',(54.1829381086179,30.8198623209147,22.1033656560979));
#53023=CARTESIAN_POINT('Ctrl Pts',(54.0201399059574,30.7446541950829,22.1150918315081));
#53024=CARTESIAN_POINT('Ctrl Pts',(53.8852323302802,30.6616915009662,22.1260115949719));
#53025=CARTESIAN_POINT('Ctrl Pts',(53.6727900266267,30.4934381365881,22.1448987434276));
#53026=CARTESIAN_POINT('Ctrl Pts',(53.5901777376367,30.415715615389,22.1527751135213));
#53027=CARTESIAN_POINT('Ctrl Pts',(53.5071420683006,30.3230750550441,22.1609522652364));
#53028=CARTESIAN_POINT('Ctrl Pts',(53.4997542731274,30.3146920469187,22.1616822072969));
#53029=CARTESIAN_POINT('Ctrl Pts',(53.4888608886134,30.3021197998366,22.1627615601897));
#53030=CARTESIAN_POINT('Ctrl Pts',(53.4853015829056,30.2979776939723,22.1631147213075));
#53031=CARTESIAN_POINT('Ctrl Pts',(53.4789665206678,30.2905437833259,22.1637441026496));
#53032=CARTESIAN_POINT('Ctrl Pts',(53.4761843765348,30.2872575689229,22.1640207812985));
#53033=CARTESIAN_POINT('Ctrl Pts',(53.4701454677765,30.2800775131251,22.1646219337992));
#53034=CARTESIAN_POINT('Ctrl Pts',(53.4668929222065,30.2761802454073,22.1649461050142));
#53035=CARTESIAN_POINT('Ctrl Pts',(53.4578809613239,30.2652977496979,22.1658455313301));
#53036=CARTESIAN_POINT('Ctrl Pts',(53.4521540844598,30.258285561355,22.1664185085655));
#53037=CARTESIAN_POINT('Ctrl Pts',(53.4212013058256,30.2198547828103,22.1695246459531));
#53038=CARTESIAN_POINT('Ctrl Pts',(53.3968821353645,30.1877140351431,22.171999200276));
#53039=CARTESIAN_POINT('Ctrl Pts',(53.3017090756875,30.0536765006612,22.1819273843312));
#53040=CARTESIAN_POINT('Ctrl Pts',(53.2394590326199,29.9460057261593,22.1890262323963));
#53041=CARTESIAN_POINT('Ctrl Pts',(53.1441913718116,29.7387886607047,22.2023135761678));
#53042=CARTESIAN_POINT('Ctrl Pts',(53.1082217751973,29.6410974848849,22.2084411469301));
#53043=CARTESIAN_POINT('Ctrl Pts',(53.0724242703148,29.5140676355583,22.2165405869007));
#53044=CARTESIAN_POINT('Ctrl Pts',(53.0653892506668,29.4869238705244,22.2182778564859));
#53045=CARTESIAN_POINT('Ctrl Pts',(53.0563487391451,29.4487457204341,22.2207344690498));
#53046=CARTESIAN_POINT('Ctrl Pts',(53.0538603934951,29.437828241775,22.2214384438084));
#53047=CARTESIAN_POINT('Ctrl Pts',(53.0498288077357,29.4194261264137,22.2226277635318));
#53048=CARTESIAN_POINT('Ctrl Pts',(53.0482364028276,29.4119524398565,22.2231115367065));
#53049=CARTESIAN_POINT('Ctrl Pts',(53.0466869980082,29.4044698737232,22.2235966764224));
#53050=CARTESIAN_POINT('Origin',(55.,29.,3.45145488139523));
#53051=CARTESIAN_POINT('',(53.0466869980276,29.4044698738173,23.182578193545));
#53052=CARTESIAN_POINT('',(53.0466869607994,29.4044696940301,23.0258937941419));
#53053=CARTESIAN_POINT('',(53.0466869980082,29.4044698737233,3.45145488139523));
#53054=CARTESIAN_POINT('Ctrl Pts',(53.0466869980277,29.4044698738173,23.182578193545));
#53055=CARTESIAN_POINT('Ctrl Pts',(53.0538997031978,29.4393023093092,23.1801157224449));
#53056=CARTESIAN_POINT('Ctrl Pts',(53.0620477325019,29.4739592596979,23.1776673773361));
#53057=CARTESIAN_POINT('Ctrl Pts',(53.0781797018133,29.5351636908076,23.1733655989426));
#53058=CARTESIAN_POINT('Ctrl Pts',(53.0857896001927,29.5617758786925,23.1715027165459));
#53059=CARTESIAN_POINT('Ctrl Pts',(53.0992777680491,29.6054823173301,23.1684649597213));
#53060=CARTESIAN_POINT('Ctrl Pts',(53.104838748457,29.6226698367687,23.1672760126887));
#53061=CARTESIAN_POINT('Ctrl Pts',(53.1127462437541,29.6460218635402,23.1656705992356));
#53062=CARTESIAN_POINT('Ctrl Pts',(53.1148907733692,29.6522531680889,23.165243183718));
#53063=CARTESIAN_POINT('Ctrl Pts',(53.1185386463897,29.6626844154669,23.1645294627576));
#53064=CARTESIAN_POINT('Ctrl Pts',(53.1200252559022,29.6668901129382,23.1642421899611));
#53065=CARTESIAN_POINT('Ctrl Pts',(53.1228785943496,29.6748769925741,23.163697609728));
#53066=CARTESIAN_POINT('Ctrl Pts',(53.124242652323,29.6786590454626,23.1634401420789));
#53067=CARTESIAN_POINT('Ctrl Pts',(53.1278446089525,29.6885521817349,23.1627676640657));
#53068=CARTESIAN_POINT('Ctrl Pts',(53.1301010176534,29.6946565437952,23.1623537353227));
#53069=CARTESIAN_POINT('Ctrl Pts',(53.138030009091,29.7157885997186,23.1609239495184));
#53070=CARTESIAN_POINT('Ctrl Pts',(53.1438543705644,29.7307591991237,23.1599165893653));
#53071=CARTESIAN_POINT('Ctrl Pts',(53.1887640577894,29.8421899182108,23.1524485231488));
#53072=CARTESIAN_POINT('Ctrl Pts',(53.2351694282081,29.9355415919484,23.1463566052155));
#53073=CARTESIAN_POINT('Ctrl Pts',(53.3343985266328,30.1012385421766,23.1351231307564));
#53074=CARTESIAN_POINT('Ctrl Pts',(53.3852041377663,30.1744736506369,23.1299839114327));
#53075=CARTESIAN_POINT('Ctrl Pts',(53.4749864673935,30.2870036031922,23.1214813156407));
#53076=CARTESIAN_POINT('Ctrl Pts',(53.5109994945791,30.3285034342905,23.1181967461995));
#53077=CARTESIAN_POINT('Ctrl Pts',(53.5649115754111,30.3856798973613,23.1134054420972));
#53078=CARTESIAN_POINT('Ctrl Pts',(53.5814506510131,30.4026065875893,23.111951307643));
#53079=CARTESIAN_POINT('Ctrl Pts',(53.6113725186843,30.4321590586585,23.1093446147938));
#53080=CARTESIAN_POINT('Ctrl Pts',(53.6246363705457,30.4449016239568,23.1081971590598));
#53081=CARTESIAN_POINT('Ctrl Pts',(53.6449817403593,30.4639134048103,23.1064480068358));
#53082=CARTESIAN_POINT('Ctrl Pts',(53.6519349881482,30.4703188972623,23.1058520998634));
#53083=CARTESIAN_POINT('Ctrl Pts',(53.6590269554757,30.4767595851479,23.1052461177814));
#53084=CARTESIAN_POINT('Ctrl Pts',(53.6591205060713,30.4768445284554,23.1052381245507));
#53085=CARTESIAN_POINT('Ctrl Pts',(53.659311035933,30.4770174952526,23.1052218457807));
#53086=CARTESIAN_POINT('Ctrl Pts',(53.6594080157387,30.4771055180275,23.1052135602188));
#53087=CARTESIAN_POINT('Ctrl Pts',(53.6596056274981,30.4772848429224,23.105196677765));
#53088=CARTESIAN_POINT('Ctrl Pts',(53.6597062602118,30.4773761444017,23.1051880808341));
#53089=CARTESIAN_POINT('Ctrl Pts',(53.6599114211406,30.4775622434345,23.1051705549317));
#53090=CARTESIAN_POINT('Ctrl Pts',(53.6600159500464,30.4776570401425,23.1051616259301));
#53091=CARTESIAN_POINT('Ctrl Pts',(53.6602291679991,30.4778503651388,23.1051434133678));
#53092=CARTESIAN_POINT('Ctrl Pts',(53.6603378578581,30.4779488925307,23.1051341297696));
#53093=CARTESIAN_POINT('Ctrl Pts',(53.6605596862744,30.4781499354858,23.1051151834644));
#53094=CARTESIAN_POINT('Ctrl Pts',(53.6606728257552,30.4782524500704,23.105105520714));
#53095=CARTESIAN_POINT('Ctrl Pts',(53.6609038687936,30.4784617476255,23.1050857892767));
#53096=CARTESIAN_POINT('Ctrl Pts',(53.6610217732926,30.4785685294255,23.105075720549));
#53097=CARTESIAN_POINT('Ctrl Pts',(53.6612626912722,30.4787866675936,23.1050551478234));
#53098=CARTESIAN_POINT('Ctrl Pts',(53.6613857058697,30.4788980227123,23.1050446437742));
#53099=CARTESIAN_POINT('Ctrl Pts',(53.6616372219687,30.479125642706,23.1050231682693));
#53100=CARTESIAN_POINT('Ctrl Pts',(53.6617657248338,30.479241906282,23.1050121967465));
#53101=CARTESIAN_POINT('Ctrl Pts',(53.6619655359365,30.4794226389776,23.1049951378772));
#53102=CARTESIAN_POINT('Ctrl Pts',(53.6620368336565,30.4794871196632,23.1049890510182));
#53103=CARTESIAN_POINT('Ctrl Pts',(53.6621962401624,30.4796312637863,23.1049754425064));
#53104=CARTESIAN_POINT('Ctrl Pts',(53.6622843514159,30.4797109245196,23.1049679207391));
#53105=CARTESIAN_POINT('Ctrl Pts',(53.6624817405421,30.4798893505303,23.1049510709034));
#53106=CARTESIAN_POINT('Ctrl Pts',(53.6625910222643,30.4799881115969,23.1049417426559));
#53107=CARTESIAN_POINT('Ctrl Pts',(53.6628364429752,30.4802098560419,23.1049207945949));
#53108=CARTESIAN_POINT('Ctrl Pts',(53.6629725879568,30.4803328327115,23.1049091745054));
#53109=CARTESIAN_POINT('Ctrl Pts',(53.6632792815313,30.4806097852277,23.1048829994416));
#53110=CARTESIAN_POINT('Ctrl Pts',(53.6634498397601,30.4807637503863,23.1048684440216));
#53111=CARTESIAN_POINT('Ctrl Pts',(53.6638355491008,30.4811118143535,23.1048355299769));
#53112=CARTESIAN_POINT('Ctrl Pts',(53.6640507157838,30.4813058956429,23.1048171706361));
#53113=CARTESIAN_POINT('Ctrl Pts',(53.6700012291259,30.4866709336535,23.1043094819185));
#53114=CARTESIAN_POINT('Ctrl Pts',(53.675766446143,30.4918085291384,23.103818772236));
#53115=CARTESIAN_POINT('Ctrl Pts',(53.688893197399,30.5033702052665,23.1027040309015));
#53116=CARTESIAN_POINT('Ctrl Pts',(53.6962723473708,30.5097738983413,23.1020791757001));
#53117=CARTESIAN_POINT('Ctrl Pts',(53.7154361783318,30.5261591845363,23.1004608349454));
#53118=CARTESIAN_POINT('Ctrl Pts',(53.7272900939902,30.536058443408,23.0994640513898));
#53119=CARTESIAN_POINT('Ctrl Pts',(53.8114114508847,30.6046663344822,23.0924185568241));
#53120=CARTESIAN_POINT('Ctrl Pts',(53.8875864830662,30.6583813032988,23.0861747656923));
#53121=CARTESIAN_POINT('Ctrl Pts',(54.1147510317692,30.7958554966519,23.0679656339418));
#53122=CARTESIAN_POINT('Ctrl Pts',(54.2732232102207,30.8656248933099,23.055680124614));
#53123=CARTESIAN_POINT('Ctrl Pts',(54.4599100713233,30.92036962702,23.0427010891681));
#53124=CARTESIAN_POINT('Ctrl Pts',(54.4812345446595,30.9262396359463,23.0412406487318));
#53125=CARTESIAN_POINT('Ctrl Pts',(54.5095921058613,30.9335405345991,23.0393315634974));
#53126=CARTESIAN_POINT('Ctrl Pts',(54.5165406562702,30.9352896342105,23.0388663814523));
#53127=CARTESIAN_POINT('Ctrl Pts',(54.5279807889037,30.9381039013883,23.0381049542647));
#53128=CARTESIAN_POINT('Ctrl Pts',(54.5324668404817,30.9391909689403,23.037807495589));
#53129=CARTESIAN_POINT('Ctrl Pts',(54.5412519120285,30.9412875248254,23.0372272276282));
#53130=CARTESIAN_POINT('Ctrl Pts',(54.5455505535809,30.9422983198658,23.0369443508637));
#53131=CARTESIAN_POINT('Ctrl Pts',(54.5561471963361,30.9447529405661,23.0362495496678));
#53132=CARTESIAN_POINT('Ctrl Pts',(54.5624489963716,30.9461804729115,23.0358385423359));
#53133=CARTESIAN_POINT('Ctrl Pts',(54.5841456636752,30.9509846569421,23.0344306452576));
#53134=CARTESIAN_POINT('Ctrl Pts',(54.5995740052117,30.9542095638736,23.0334418948166));
#53135=CARTESIAN_POINT('Ctrl Pts',(54.7355571940909,30.9809553136539,23.0248229898514));
#53136=CARTESIAN_POINT('Ctrl Pts',(54.8580240203191,30.9934806403364,23.0177105924691));
#53137=CARTESIAN_POINT('Ctrl Pts',(55.0840258055236,30.995647141275,23.0045846162774));
#53138=CARTESIAN_POINT('Ctrl Pts',(55.1870894825611,30.9886335408157,22.9985971347068));
#53139=CARTESIAN_POINT('Ctrl Pts',(55.3241485259237,30.9685545562316,22.9902700116087));
#53140=CARTESIAN_POINT('Ctrl Pts',(55.3590106242435,30.9624959787507,22.9881207634184));
#53141=CARTESIAN_POINT('Ctrl Pts',(55.4186318350391,30.9504928009747,22.9843787845915));
#53142=CARTESIAN_POINT('Ctrl Pts',(55.4434726324289,30.9449952991038,22.9827996954215));
#53143=CARTESIAN_POINT('Ctrl Pts',(55.4786787819389,30.9364943528188,22.9805301464296));
#53144=CARTESIAN_POINT('Ctrl Pts',(55.4891360556734,30.9338794343386,22.9798520324048));
#53145=CARTESIAN_POINT('Ctrl Pts',(55.5071794290482,30.9292118452308,22.9786748555919));
#53146=CARTESIAN_POINT('Ctrl Pts',(55.5147756107562,30.9271988441098,22.9781770722162));
#53147=CARTESIAN_POINT('Ctrl Pts',(55.5293349519768,30.9232483741408,22.9772186804588));
#53148=CARTESIAN_POINT('Ctrl Pts',(55.5362998772211,30.9213178392616,22.9767583021505));
#53149=CARTESIAN_POINT('Ctrl Pts',(55.5526822332216,30.9166809653052,22.9756708806159));
#53150=CARTESIAN_POINT('Ctrl Pts',(55.5620904516329,30.9139430222001,22.9750428253226));
#53151=CARTESIAN_POINT('Ctrl Pts',(55.5948004045686,30.904161918882,22.97284658496));
#53152=CARTESIAN_POINT('Ctrl Pts',(55.6179923185565,30.8967618570668,22.9712669157421));
#53153=CARTESIAN_POINT('Ctrl Pts',(55.766219297105,30.8464586331983,22.9610211012216));
#53154=CARTESIAN_POINT('Ctrl Pts',(55.8868422687238,30.7916475759597,22.9519602324581));
#53155=CARTESIAN_POINT('Ctrl Pts',(56.087363590916,30.6752927204214,22.9358227548717));
#53156=CARTESIAN_POINT('Ctrl Pts',(56.1697184137742,30.6188655666442,22.9288370616602));
#53157=CARTESIAN_POINT('Ctrl Pts',(56.2692875145394,30.5390632008799,22.920165677334));
#53158=CARTESIAN_POINT('Ctrl Pts',(56.2906955797649,30.5211546309681,22.9182872735512));
#53159=CARTESIAN_POINT('Ctrl Pts',(56.32543303876,30.4908340109624,22.9152251094162));
#53160=CARTESIAN_POINT('Ctrl Pts',(56.3389803978116,30.4786785786073,22.9140271755895));
#53161=CARTESIAN_POINT('Ctrl Pts',(56.3572404087538,30.4618379227196,22.9124096502127));
#53162=CARTESIAN_POINT('Ctrl Pts',(56.3620983495171,30.4573125020788,22.9119790366044));
#53163=CARTESIAN_POINT('Ctrl Pts',(56.3702044316858,30.449685326789,22.9112601648336));
#53164=CARTESIAN_POINT('Ctrl Pts',(56.3734648183057,30.4465967390132,22.9109709310116));
#53165=CARTESIAN_POINT('Ctrl Pts',(56.3796225754742,30.4407238659447,22.9104245387317));
#53166=CARTESIAN_POINT('Ctrl Pts',(56.3825220040547,30.4379417991214,22.9101672100938));
#53167=CARTESIAN_POINT('Ctrl Pts',(56.3900946069374,30.4306316393876,22.9094949203922));
#53168=CARTESIAN_POINT('Ctrl Pts',(56.3947541128942,30.426089362992,22.9090810424584));
#53169=CARTESIAN_POINT('Ctrl Pts',(56.4108500515556,30.4102440355237,22.907650235004));
#53170=CARTESIAN_POINT('Ctrl Pts',(56.4221723330464,30.3988252218292,22.9066418338055));
#53171=CARTESIAN_POINT('Ctrl Pts',(56.5047858959526,30.3134672204676,22.899257962477));
#53172=CARTESIAN_POINT('Ctrl Pts',(56.570418759547,30.2342475435585,22.8932417548336));
#53173=CARTESIAN_POINT('Ctrl Pts',(56.6796015345761,30.0795672201732,22.882227719001));
#53174=CARTESIAN_POINT('Ctrl Pts',(56.724879290495,30.0056429173181,22.8772298975857));
#53175=CARTESIAN_POINT('Ctrl Pts',(56.8018831294644,29.8593285826721,22.8674810397443));
#53176=CARTESIAN_POINT('Ctrl Pts',(56.8343951249771,29.7875410575784,22.8627577505855));
#53177=CARTESIAN_POINT('Ctrl Pts',(56.869987797857,29.6946954369629,22.8566098673597));
#53178=CARTESIAN_POINT('Ctrl Pts',(56.8770963627109,29.6752520341767,22.8553205676457));
#53179=CARTESIAN_POINT('Ctrl Pts',(56.8871615723847,29.6463336307355,22.853398716248));
#53180=CARTESIAN_POINT('Ctrl Pts',(56.890352332517,29.6369411399545,22.8527738583601));
#53181=CARTESIAN_POINT('Ctrl Pts',(56.895901132691,29.6201983866708,22.8516586739924));
#53182=CARTESIAN_POINT('Ctrl Pts',(56.8982868292375,29.6128574507927,22.8511692638996));
#53183=CARTESIAN_POINT('Ctrl Pts',(56.903220233472,29.5973718524534,22.850135824718));
#53184=CARTESIAN_POINT('Ctrl Pts',(56.9057583966007,29.5892243352719,22.8495914958556));
#53185=CARTESIAN_POINT('Ctrl Pts',(56.9123367436444,29.5676205881953,22.848146456147));
#53186=CARTESIAN_POINT('Ctrl Pts',(56.9162871188425,29.5541377218099,22.8472428568503));
#53187=CARTESIAN_POINT('Ctrl Pts',(56.9327872710219,29.4955343134574,22.8433070453543));
#53188=CARTESIAN_POINT('Ctrl Pts',(56.9438874042038,29.4500244964851,22.8402288658391));
#53189=CARTESIAN_POINT('Ctrl Pts',(56.9916628136589,29.2191229417368,22.824492232927));
#53190=CARTESIAN_POINT('Ctrl Pts',(57.0034566568534,29.0295845494409,22.8110686740147));
#53191=CARTESIAN_POINT('Ctrl Pts',(56.9841024379244,28.7871241464056,22.7944012858426));
#53192=CARTESIAN_POINT('Ctrl Pts',(56.9775691187795,28.7331664349957,22.7907344992934));
#53193=CARTESIAN_POINT('Ctrl Pts',(56.9673213353977,28.6702065685746,22.7865547430236));
#53194=CARTESIAN_POINT('Ctrl Pts',(56.9657361380247,28.6608858772697,22.7859385424139));
#53195=CARTESIAN_POINT('Ctrl Pts',(56.9631930925143,28.6465505695968,22.7849951581774));
#53196=CARTESIAN_POINT('Ctrl Pts',(56.9622821887394,28.641527920877,22.7846654476872));
#53197=CARTESIAN_POINT('Ctrl Pts',(56.9605681296859,28.6322790786566,22.7840598951356));
#53198=CARTESIAN_POINT('Ctrl Pts',(56.959770588306,28.6280520077412,22.7837837535927));
#53199=CARTESIAN_POINT('Ctrl Pts',(56.9579374055326,28.618505510358,22.7831614852482));
#53200=CARTESIAN_POINT('Ctrl Pts',(56.9568937591502,28.6131877113254,22.7828158136982));
#53201=CARTESIAN_POINT('Ctrl Pts',(56.9537428811031,28.5974718971388,22.781796901337));
#53202=CARTESIAN_POINT('Ctrl Pts',(56.951574313855,28.587086173454,22.7811270056566));
#53203=CARTESIAN_POINT('Ctrl Pts',(56.9310516115129,28.4925738331424,22.7750581991181));
#53204=CARTESIAN_POINT('Ctrl Pts',(56.9073487212173,28.4096896541196,22.7699325448912));
#53205=CARTESIAN_POINT('Ctrl Pts',(56.8251953968689,28.1798554681987,22.755630579849));
#53206=CARTESIAN_POINT('Ctrl Pts',(56.7545587792672,28.0379720580763,22.7466489723096));
#53207=CARTESIAN_POINT('Ctrl Pts',(56.6431918198514,27.8681952105304,22.7343677748723));
#53208=CARTESIAN_POINT('Ctrl Pts',(56.6171857394711,27.8313378373637,22.7316012495629));
#53209=CARTESIAN_POINT('Ctrl Pts',(56.5818883782659,27.7847489439689,22.7279539382438));
#53210=CARTESIAN_POINT('Ctrl Pts',(56.5737157154849,27.7741840253791,22.7271164414022));
#53211=CARTESIAN_POINT('Ctrl Pts',(56.5602390914297,27.7571195160947,22.725746236237));
#53212=CARTESIAN_POINT('Ctrl Pts',(56.5549990583862,27.7505697920041,22.7252160557743));
#53213=CARTESIAN_POINT('Ctrl Pts',(56.5448241973342,27.7380149870812,22.7241914157125));
#53214=CARTESIAN_POINT('Ctrl Pts',(56.5398952660091,27.73200530741,22.7236971976861));
#53215=CARTESIAN_POINT('Ctrl Pts',(56.5284909807001,27.7182650135866,22.7225584974618));
#53216=CARTESIAN_POINT('Ctrl Pts',(56.5219919173525,27.7105544405231,22.721913063356));
#53217=CARTESIAN_POINT('Ctrl Pts',(56.5010493940144,27.6860868812332,22.7198440281444));
#53218=CARTESIAN_POINT('Ctrl Pts',(56.4863859309555,27.6695212266667,22.718411456505));
#53219=CARTESIAN_POINT('Ctrl Pts',(56.3535810177888,27.5244244454763,22.7055727411746));
#53220=CARTESIAN_POINT('Ctrl Pts',(56.2193363922665,27.4116993904971,22.6934296479604));
#53221=CARTESIAN_POINT('Ctrl Pts',(56.0634871035524,27.3123599166396,22.6805649733658));
#53222=CARTESIAN_POINT('Ctrl Pts',(56.0547497063202,27.306885435272,22.6798477890294));
#53223=CARTESIAN_POINT('Ctrl Pts',(55.9762115955583,27.2585206984383,22.6734391786604));
#53224=CARTESIAN_POINT('Ctrl Pts',(55.9038651631222,27.2198961354828,22.6677991412972));
#53225=CARTESIAN_POINT('Ctrl Pts',(55.8150059943801,27.1792745287799,22.6613318743826));
#53226=CARTESIAN_POINT('Ctrl Pts',(55.8005928923439,27.1728910623025,22.6602968448215));
#53227=CARTESIAN_POINT('Ctrl Pts',(55.780336580407,27.1642054096953,22.6588631462726));
#53228=CARTESIAN_POINT('Ctrl Pts',(55.7745563139171,27.1617591355744,22.6584563940354));
#53229=CARTESIAN_POINT('Ctrl Pts',(55.7646850208706,27.1576363207665,22.6577658972735));
#53230=CARTESIAN_POINT('Ctrl Pts',(55.7605998172617,27.1559460346482,22.6574813400384));
#53231=CARTESIAN_POINT('Ctrl Pts',(55.7527182105534,27.1527156034691,22.656934698963));
#53232=CARTESIAN_POINT('Ctrl Pts',(55.7489226580933,27.1511735616632,22.6566724968923));
#53233=CARTESIAN_POINT('Ctrl Pts',(55.7397800984469,27.1474919336289,22.6560433633041));
#53234=CARTESIAN_POINT('Ctrl Pts',(55.7344284863538,27.1453637741024,22.6556771065823));
#53235=CARTESIAN_POINT('Ctrl Pts',(55.7147671599753,27.1376435613859,22.6543386006907));
#53236=CARTESIAN_POINT('Ctrl Pts',(55.7004017598008,27.1321935309153,22.6533743586092));
#53237=CARTESIAN_POINT('Ctrl Pts',(55.5634354234915,27.0820328976609,22.6442976507526));
#53238=CARTESIAN_POINT('Ctrl Pts',(55.4367702701057,27.0492825186422,22.6367740082767));
#53239=CARTESIAN_POINT('Ctrl Pts',(55.1670533116677,27.0071595280791,22.6209203324711));
#53240=CARTESIAN_POINT('Ctrl Pts',(55.024378691819,27.0003203985089,22.6126076976001));
#53241=CARTESIAN_POINT('Ctrl Pts',(54.8639226821456,27.0098126247242,22.6026420906276));
#53242=CARTESIAN_POINT('Ctrl Pts',(54.8456607065585,27.0111455123618,22.6014994741977));
#53243=CARTESIAN_POINT('Ctrl Pts',(54.8180051514018,27.0135471946582,22.5997552934014));
#53244=CARTESIAN_POINT('Ctrl Pts',(54.8085962379358,27.0144317015751,22.5991594619777));
#53245=CARTESIAN_POINT('Ctrl Pts',(54.7915530404021,27.0161561525795,22.5980756230096));
#53246=CARTESIAN_POINT('Ctrl Pts',(54.7839166050162,27.0169733966369,22.5975883329859));
#53247=CARTESIAN_POINT('Ctrl Pts',(54.767495841239,27.0188267074952,22.5965368437857));
#53248=CARTESIAN_POINT('Ctrl Pts',(54.7587133308977,27.0198771406912,22.5959722050662));
#53249=CARTESIAN_POINT('Ctrl Pts',(54.7350066153004,27.0228726442627,22.5944418240503));
#53250=CARTESIAN_POINT('Ctrl Pts',(54.7200971987941,27.0249282351914,22.5934726467313));
#53251=CARTESIAN_POINT('Ctrl Pts',(54.6464264048459,27.0359362856412,22.5886494973666));
#53252=CARTESIAN_POINT('Ctrl Pts',(54.5880676461809,27.0473425582163,22.5847194519114));
#53253=CARTESIAN_POINT('Ctrl Pts',(54.3600011951108,27.1025974036752,22.5689185555687));
#53254=CARTESIAN_POINT('Ctrl Pts',(54.1958782146237,27.1661218475954,22.5564789473656));
#53255=CARTESIAN_POINT('Ctrl Pts',(54.0108737930314,27.2673914721722,22.5420370302211));
#53256=CARTESIAN_POINT('Ctrl Pts',(53.9800114809717,27.2853785588183,22.5396160631595));
#53257=CARTESIAN_POINT('Ctrl Pts',(53.9311331567388,27.3156527985473,22.5357811743812));
#53258=CARTESIAN_POINT('Ctrl Pts',(53.912807324986,27.3274229450696,22.5343432382754));
#53259=CARTESIAN_POINT('Ctrl Pts',(53.8887600434674,27.3434300963437,22.5324599310119));
#53260=CARTESIAN_POINT('Ctrl Pts',(53.8828640192392,27.3474004444923,22.531998463147));
#53261=CARTESIAN_POINT('Ctrl Pts',(53.8731942655931,27.3539873985975,22.5312422793703));
#53262=CARTESIAN_POINT('Ctrl Pts',(53.8694081842772,27.3565856291473,22.5309463683965));
#53263=CARTESIAN_POINT('Ctrl Pts',(53.8620012466177,27.3617064143402,22.5303678363168));
#53264=CARTESIAN_POINT('Ctrl Pts',(53.8583797433621,27.3642279420008,22.5300851532358));
#53265=CARTESIAN_POINT('Ctrl Pts',(53.8494669585984,27.3704776224028,22.5293898187092));
#53266=CARTESIAN_POINT('Ctrl Pts',(53.8441853403444,27.3742195923964,22.5289780934057));
#53267=CARTESIAN_POINT('Ctrl Pts',(53.8260262482276,27.387218333381,22.527563276225));
#53268=CARTESIAN_POINT('Ctrl Pts',(53.813240624408,27.3966032009004,22.5265684514128));
#53269=CARTESIAN_POINT('Ctrl Pts',(53.705188553773,27.4779159396128,22.5181598109004));
#53270=CARTESIAN_POINT('Ctrl Pts',(53.6164310181734,27.5581188741702,22.5112348402623));
#53271=CARTESIAN_POINT('Ctrl Pts',(53.4635918929388,27.7234199871026,22.4981608545747));
#53272=CARTESIAN_POINT('Ctrl Pts',(53.3981018789543,27.8066321664326,22.4920328761045));
#53273=CARTESIAN_POINT('Ctrl Pts',(53.3196341083094,27.9245067909746,22.4835257171264));
#53274=CARTESIAN_POINT('Ctrl Pts',(53.3005604218475,27.9549066685323,22.4813470044653));
#53275=CARTESIAN_POINT('Ctrl Pts',(53.269242735418,28.007947490989,22.4775583167706));
#53276=CARTESIAN_POINT('Ctrl Pts',(53.2565976683357,28.0303417582436,22.4759624738757));
#53277=CARTESIAN_POINT('Ctrl Pts',(53.2392517338491,28.0624978842584,22.4736732484704));
#53278=CARTESIAN_POINT('Ctrl Pts',(53.2341916578246,28.0720638140863,22.4729925263917));
#53279=CARTESIAN_POINT('Ctrl Pts',(53.2255900336217,28.0886500926603,22.47181249678));
#53280=CARTESIAN_POINT('Ctrl Pts',(53.2220116614762,28.0956511471796,22.4713144892854));
#53281=CARTESIAN_POINT('Ctrl Pts',(53.2152301948318,28.1091148620658,22.4703568454649));
#53282=CARTESIAN_POINT('Ctrl Pts',(53.212020573306,28.1155741105571,22.4698974458219));
#53283=CARTESIAN_POINT('Ctrl Pts',(53.2037352365732,28.1324774908103,22.4686952366882));
#53284=CARTESIAN_POINT('Ctrl Pts',(53.198715621955,28.1429486688055,22.4679505060558));
#53285=CARTESIAN_POINT('Ctrl Pts',(53.1816520502392,28.1793563244686,22.465360776941));
#53286=CARTESIAN_POINT('Ctrl Pts',(53.1700750521043,28.2055065425248,22.4635000086074));
#53287=CARTESIAN_POINT('Ctrl Pts',(53.0946356819842,28.3863139775897,22.4506234384185));
#53288=CARTESIAN_POINT('Ctrl Pts',(53.0499022741434,28.5482012936273,22.4389579101157));
#53289=CARTESIAN_POINT('Ctrl Pts',(53.0121406845093,28.8086022671649,22.420648066318));
#53290=CARTESIAN_POINT('Ctrl Pts',(53.0052383308774,28.9043553628939,22.4140288393459));
#53291=CARTESIAN_POINT('Ctrl Pts',(53.0052514115234,29.0117056221172,22.4069693451081));
#53292=CARTESIAN_POINT('Ctrl Pts',(53.00535161038,29.0231682838032,22.4062202334303));
#53293=CARTESIAN_POINT('Ctrl Pts',(53.0056464057258,29.0401465810844,22.405118227178));
#53294=CARTESIAN_POINT('Ctrl Pts',(53.00576508561,29.0456630589919,22.4047613539211));
#53295=CARTESIAN_POINT('Ctrl Pts',(53.0060172294825,29.0554873599829,22.4041279903023));
#53296=CARTESIAN_POINT('Ctrl Pts',(53.0061417656245,29.0597953062303,22.4038510167415));
#53297=CARTESIAN_POINT('Ctrl Pts',(53.0064420368293,29.0691342941143,22.4032522296248));
#53298=CARTESIAN_POINT('Ctrl Pts',(53.006622854182,29.074165079496,22.4029306993279));
#53299=CARTESIAN_POINT('Ctrl Pts',(53.0071844967961,29.088300448807,22.4020300268339));
#53300=CARTESIAN_POINT('Ctrl Pts',(53.0076086732183,29.0974033239466,22.4014532257062));
#53301=CARTESIAN_POINT('Ctrl Pts',(53.0105982048108,29.1533158558037,22.3979283418912));
#53302=CARTESIAN_POINT('Ctrl Pts',(53.0147508877728,29.2000299805981,22.3950608033523));
#53303=CARTESIAN_POINT('Ctrl Pts',(53.0271467672353,29.2995483206916,22.3890361504842));
#53304=CARTESIAN_POINT('Ctrl Pts',(53.0358692663766,29.3522276431481,22.3858980677615));
#53305=CARTESIAN_POINT('Ctrl Pts',(53.0466870263011,29.4044700103589,22.3827843708292));
#53306=CARTESIAN_POINT('Ctrl Pts',(53.0466869980082,29.4044698737232,22.2235966764224));
#53307=CARTESIAN_POINT('Ctrl Pts',(53.0466279142296,29.4041845394613,22.2236151763568));
#53308=CARTESIAN_POINT('Ctrl Pts',(53.0465688929793,29.4038991922872,22.2236336782779));
#53309=CARTESIAN_POINT('Ctrl Pts',(53.0448752433889,29.3957019319717,22.2241652220084));
#53310=CARTESIAN_POINT('Ctrl Pts',(53.0432886540183,29.3877802705747,22.2246797803914));
#53311=CARTESIAN_POINT('Ctrl Pts',(53.0394790740625,29.3681406152766,22.2259577851166));
#53312=CARTESIAN_POINT('Ctrl Pts',(53.037312997492,29.3564120279491,22.226723013369));
#53313=CARTESIAN_POINT('Ctrl Pts',(53.0295460413525,29.3121368254177,22.2296197496557));
#53314=CARTESIAN_POINT('Ctrl Pts',(53.0246487884617,29.2794737509575,22.2317731475286));
#53315=CARTESIAN_POINT('Ctrl Pts',(53.0143716279036,29.1970152869603,22.2372537451535));
#53316=CARTESIAN_POINT('Ctrl Pts',(53.0100522244178,29.1471129740373,22.2406112592087));
#53317=CARTESIAN_POINT('Ctrl Pts',(53.0019573640592,28.9810226014101,22.2519123805226));
#53318=CARTESIAN_POINT('Ctrl Pts',(53.0064559700848,28.8646758132676,22.2600486505167));
#53319=CARTESIAN_POINT('Ctrl Pts',(53.0326987454006,28.65744554289,22.2745732287844));
#53320=CARTESIAN_POINT('Ctrl Pts',(53.0507385803354,28.5664083035089,22.2809593160895));
#53321=CARTESIAN_POINT('Ctrl Pts',(53.077835422851,28.4666858705796,22.2877467968102));
#53322=CARTESIAN_POINT('Ctrl Pts',(53.0807056153905,28.456447151284,22.2884411217788));
#53323=CARTESIAN_POINT('Ctrl Pts',(53.0851633623117,28.4410209018282,22.2894828520759));
#53324=CARTESIAN_POINT('Ctrl Pts',(53.0866903758059,28.4358162844709,22.2898335619525));
#53325=CARTESIAN_POINT('Ctrl Pts',(53.089466982211,28.4264935313206,22.2904603308994));
#53326=CARTESIAN_POINT('Ctrl Pts',(53.0907086852651,28.4223731669599,22.2907368320506));
#53327=CARTESIAN_POINT('Ctrl Pts',(53.0934526153654,28.4133734615281,22.2913396423756));
#53328=CARTESIAN_POINT('Ctrl Pts',(53.0949602406917,28.4084958644702,22.2916656355923));
#53329=CARTESIAN_POINT('Ctrl Pts',(53.0993101894195,28.3946116935405,22.2925916876043));
#53330=CARTESIAN_POINT('Ctrl Pts',(53.1021978181974,28.3856192998748,22.2931891892226));
#53331=CARTESIAN_POINT('Ctrl Pts',(53.1220086131748,28.3253989557272,22.2971773536682));
#53332=CARTESIAN_POINT('Ctrl Pts',(53.1409418338569,28.274850300297,22.3004609169913));
#53333=CARTESIAN_POINT('Ctrl Pts',(53.2334537947233,28.0554002353968,22.3146855580666));
#53334=CARTESIAN_POINT('Ctrl Pts',(53.3281663945419,27.8963993089427,22.3249947921508));
#53335=CARTESIAN_POINT('Ctrl Pts',(53.4752481410213,27.7128480765358,22.3391495801228));
#53336=CARTESIAN_POINT('Ctrl Pts',(53.5086499464523,27.6742916384692,22.3422657754461));
#53337=CARTESIAN_POINT('Ctrl Pts',(53.5533891754133,27.6264809506489,22.3463450880223));
#53338=CARTESIAN_POINT('Ctrl Pts',(53.5634028561744,27.6160108072289,22.3472523780619));
#53339=CARTESIAN_POINT('Ctrl Pts',(53.5795651396772,27.5994761959036,22.3487082161511));
#53340=CARTESIAN_POINT('Ctrl Pts',(53.5856407347501,27.5933408432425,22.3492536009295));
#53341=CARTESIAN_POINT('Ctrl Pts',(53.5966679733433,27.582348812778,22.3502402155453));
#53342=CARTESIAN_POINT('Ctrl Pts',(53.601605502494,27.5774781221229,22.3506808199816));
#53343=CARTESIAN_POINT('Ctrl Pts',(53.6132841481262,27.5660771306427,22.3517203246385));
#53344=CARTESIAN_POINT('Ctrl Pts',(53.6200461051383,27.559568504851,22.3523201493295));
#53345=CARTESIAN_POINT('Ctrl Pts',(53.6399064426672,27.5407204161777,22.3540761120386));
#53346=CARTESIAN_POINT('Ctrl Pts',(53.6531258984516,27.5285104458243,22.3552377110104));
#53347=CARTESIAN_POINT('Ctrl Pts',(53.6834137892194,27.5012855454956,22.3578837408916));
#53348=CARTESIAN_POINT('Ctrl Pts',(53.7005771017622,27.4863803884188,22.359372472571));
#53349=CARTESIAN_POINT('Ctrl Pts',(53.757713618036,27.4384493522052,22.3642949249135));
#53350=CARTESIAN_POINT('Ctrl Pts',(53.798717505439,27.4066903938278,22.3677757680215));
#53351=CARTESIAN_POINT('Ctrl Pts',(53.9450015653188,27.3022472252632,22.3800090735154));
#53352=CARTESIAN_POINT('Ctrl Pts',(54.0559960423527,27.2381152103718,22.3889986724976));
#53353=CARTESIAN_POINT('Ctrl Pts',(54.2436196051254,27.1525553690392,22.4032852939445));
#53354=CARTESIAN_POINT('Ctrl Pts',(54.3167490057629,27.1242777764996,22.4086446039783));
#53355=CARTESIAN_POINT('Ctrl Pts',(54.4013726971017,27.0971643615563,22.4144799606055));
#53356=CARTESIAN_POINT('Ctrl Pts',(54.4114111556857,27.0940353364946,22.4151664339282));
#53357=CARTESIAN_POINT('Ctrl Pts',(54.4266406341925,27.0894200503009,22.416198730247));
#53358=CARTESIAN_POINT('Ctrl Pts',(54.4318135332571,27.0878753055267,22.4165477718197));
#53359=CARTESIAN_POINT('Ctrl Pts',(54.4411198032717,27.0851373429404,22.417172776062));
#53360=CARTESIAN_POINT('Ctrl Pts',(54.4452508016077,27.083936483924,22.417449169654));
#53361=CARTESIAN_POINT('Ctrl Pts',(54.4543124010385,27.0813340884088,22.418053170844));
#53362=CARTESIAN_POINT('Ctrl Pts',(54.4592445236492,27.0799381905332,22.4183804531221));
#53363=CARTESIAN_POINT('Ctrl Pts',(54.4733722042709,27.0759985045899,22.4193138752085));
#53364=CARTESIAN_POINT('Ctrl Pts',(54.4825808544397,27.0735016153837,22.4199173934789));
#53365=CARTESIAN_POINT('Ctrl Pts',(54.5462527776601,27.0567267081257,22.4240588303713));
#53366=CARTESIAN_POINT('Ctrl Pts',(54.601286804014,27.0446926872494,22.4274799850179));
#53367=CARTESIAN_POINT('Ctrl Pts',(54.751152958943,27.0185146183934,22.4365507507374));
#53368=CARTESIAN_POINT('Ctrl Pts',(54.8466146534227,27.0088485625662,22.4420720743799));
#53369=CARTESIAN_POINT('Ctrl Pts',(55.0737294666312,27.0022883360107,22.4552818637473));
#53370=CARTESIAN_POINT('Ctrl Pts',(55.2050880312969,27.0114778669021,22.4629985723785));
#53371=CARTESIAN_POINT('Ctrl Pts',(55.3501099195795,27.0361520582397,22.4721279260015));
#53372=CARTESIAN_POINT('Ctrl Pts',(55.3656067510442,27.0389779767527,22.4731109963521));
#53373=CARTESIAN_POINT('Ctrl Pts',(55.3907389808102,27.0438692071489,22.4747182908607));
#53374=CARTESIAN_POINT('Ctrl Pts',(55.4003955910327,27.0458229366361,22.4753389958397));
#53375=CARTESIAN_POINT('Ctrl Pts',(55.4175887938356,27.0494342604448,22.4764498953761));
#53376=CARTESIAN_POINT('Ctrl Pts',(55.4251310375242,27.0510642126325,22.4769392043954));
#53377=CARTESIAN_POINT('Ctrl Pts',(55.4410415352649,27.0545993773658,22.4779756912345));
#53378=CARTESIAN_POINT('Ctrl Pts',(55.4494073112564,27.0565149130512,22.4785231888429));
#53379=CARTESIAN_POINT('Ctrl Pts',(55.4716298279579,27.0617544212893,22.479984356558));
#53380=CARTESIAN_POINT('Ctrl Pts',(55.4854635515009,27.065172942921,22.4809010248597));
#53381=CARTESIAN_POINT('Ctrl Pts',(55.5523950236962,27.0824757087335,22.4853714076687));
#53382=CARTESIAN_POINT('Ctrl Pts',(55.6049366126394,27.0983979379471,22.4889898173175));
#53383=CARTESIAN_POINT('Ctrl Pts',(55.8510569401975,27.1842151705142,22.5064749305106));
#53384=CARTESIAN_POINT('Ctrl Pts',(56.0336676877004,27.2816052054567,22.5212221655983));
#53385=CARTESIAN_POINT('Ctrl Pts',(56.2228850928981,27.4237585604516,22.5371671109658));
#53386=CARTESIAN_POINT('Ctrl Pts',(56.247190184982,27.4429187821038,22.5392260244135));
#53387=CARTESIAN_POINT('Ctrl Pts',(56.2775122347541,27.4679880707784,22.5417984767466));
#53388=CARTESIAN_POINT('Ctrl Pts',(56.2839496314808,27.4733790873239,22.5423448336399));
#53389=CARTESIAN_POINT('Ctrl Pts',(56.2940723561193,27.4819657158504,22.5432040661044));
#53390=CARTESIAN_POINT('Ctrl Pts',(56.2977802456266,27.4851344000146,22.5435188174282));
#53391=CARTESIAN_POINT('Ctrl Pts',(56.3047637130131,27.491146782908,22.5441115984268));
#53392=CARTESIAN_POINT('Ctrl Pts',(56.3080416021934,27.4939875349767,22.5443898191192));
#53393=CARTESIAN_POINT('Ctrl Pts',(56.3156591333626,27.5006328292874,22.5450363851539));
#53394=CARTESIAN_POINT('Ctrl Pts',(56.3199915572768,27.5044455347532,22.545404125019));
#53395=CARTESIAN_POINT('Ctrl Pts',(56.3338807290319,27.5167759298904,22.5465833130639));
#53396=CARTESIAN_POINT('Ctrl Pts',(56.3433722770605,27.5253670332411,22.5473895477711));
#53397=CARTESIAN_POINT('Ctrl Pts',(56.4212574875305,27.5972395759938,22.5540152090296));
#53398=CARTESIAN_POINT('Ctrl Pts',(56.4852317859414,27.6651589344583,22.5595240989389));
#53399=CARTESIAN_POINT('Ctrl Pts',(56.6488314091771,27.8652361081725,22.5746135335527));
#53400=CARTESIAN_POINT('Ctrl Pts',(56.7371240184743,28.0056506229502,22.5840433937638));
#53401=CARTESIAN_POINT('Ctrl Pts',(56.8200288006433,28.1830200895703,22.5960242153697));
#53402=CARTESIAN_POINT('Ctrl Pts',(56.8323277368797,28.2109905452035,22.5979131173461));
#53403=CARTESIAN_POINT('Ctrl Pts',(56.8485283290613,28.250258133462,22.6005695971389));
#53404=CARTESIAN_POINT('Ctrl Pts',(56.8529785754591,28.2613253497816,22.6013187958591));
#53405=CARTESIAN_POINT('Ctrl Pts',(56.8599815679416,28.279202518492,22.602530073859));
#53406=CARTESIAN_POINT('Ctrl Pts',(56.8625968440385,28.2859877894969,22.6029900612316));
#53407=CARTESIAN_POINT('Ctrl Pts',(56.8679476696764,28.3000998431279,22.6039473317306));
#53408=CARTESIAN_POINT('Ctrl Pts',(56.8706773441114,28.3074287057457,22.6044448001278));
#53409=CARTESIAN_POINT('Ctrl Pts',(56.8769964100254,28.3247046091197,22.6056183099861));
#53410=CARTESIAN_POINT('Ctrl Pts',(56.880549912397,28.3346644394788,22.6062955218131));
#53411=CARTESIAN_POINT('Ctrl Pts',(56.8919939276747,28.3675642058324,22.608534973175));
#53412=CARTESIAN_POINT('Ctrl Pts',(56.8995449214612,28.3906191158875,22.6101082377976));
#53413=CARTESIAN_POINT('Ctrl Pts',(56.916448161428,28.4455990578515,22.6138709086531));
#53414=CARTESIAN_POINT('Ctrl Pts',(56.9254257155978,28.4776308183483,22.6160716873626));
#53415=CARTESIAN_POINT('Ctrl Pts',(56.971463482644,28.6592533101598,22.6285999238263));
#53416=CARTESIAN_POINT('Ctrl Pts',(56.9918860331995,28.8125061357827,22.6394163157833));
#53417=CARTESIAN_POINT('Ctrl Pts',(56.9958743096145,29.0503126074673,22.655920493156));
#53418=CARTESIAN_POINT('Ctrl Pts',(56.992001173939,29.1340903230906,22.6616679390425));
#53419=CARTESIAN_POINT('Ctrl Pts',(56.9817159759096,29.2279065481281,22.6678663740218));
#53420=CARTESIAN_POINT('Ctrl Pts',(56.9804786816828,29.2384193929931,22.6685575199026));
#53421=CARTESIAN_POINT('Ctrl Pts',(56.9784821590729,29.2542935648063,22.6695954364631));
#53422=CARTESIAN_POINT('Ctrl Pts',(56.9777847144697,29.2596622724775,22.6699454766677));
#53423=CARTESIAN_POINT('Ctrl Pts',(56.9764937448485,29.2692926886636,22.6705715274912));
#53424=CARTESIAN_POINT('Ctrl Pts',(56.9759082826968,29.2735553601114,22.6708479758256));
#53425=CARTESIAN_POINT('Ctrl Pts',(56.9745969132792,29.2828793646414,22.6714512228779));
#53426=CARTESIAN_POINT('Ctrl Pts',(56.9738653384883,29.2879398058453,22.6717777020297));
#53427=CARTESIAN_POINT('Ctrl Pts',(56.9717215338075,29.3023766951074,22.6727066197861));
#53428=CARTESIAN_POINT('Ctrl Pts',(56.9702618714004,29.3117461132499,22.6733064757201));
#53429=CARTESIAN_POINT('Ctrl Pts',(56.9599029988237,29.375257675986,22.6773544293194));
#53430=CARTESIAN_POINT('Ctrl Pts',(56.9488391216017,29.4290283824883,22.6806916942969));
#53431=CARTESIAN_POINT('Ctrl Pts',(56.8880316166375,29.6730720773779,22.6957032092314));
#53432=CARTESIAN_POINT('Ctrl Pts',(56.8125469833334,29.8557871002795,22.7066737363523));
#53433=CARTESIAN_POINT('Ctrl Pts',(56.6909887663972,30.0588610640438,22.7210374346837));
#53434=CARTESIAN_POINT('Ctrl Pts',(56.6694024867358,30.0925771200705,22.7234980399389));
#53435=CARTESIAN_POINT('Ctrl Pts',(56.6393295851477,30.1365747515199,22.7268239351601));
#53436=CARTESIAN_POINT('Ctrl Pts',(56.631732476269,30.1474549084826,22.7276560499901));
#53437=CARTESIAN_POINT('Ctrl Pts',(56.6191695210474,30.1650697926875,22.729019496458));
#53438=CARTESIAN_POINT('Ctrl Pts',(56.6142687782571,30.171850616686,22.7295483447846));
#53439=CARTESIAN_POINT('Ctrl Pts',(56.6047315743875,30.1848732383603,22.7305718425194));
#53440=CARTESIAN_POINT('Ctrl Pts',(56.6001009833363,30.1911191616094,22.7310662596901));
#53441=CARTESIAN_POINT('Ctrl Pts',(56.5892541401297,30.2055724121651,22.7322186757651));
#53442=CARTESIAN_POINT('Ctrl Pts',(56.5830106701347,30.2137589441886,22.73287772627));
#53443=CARTESIAN_POINT('Ctrl Pts',(56.5628038377754,30.2398333240396,22.7349973895402));
#53444=CARTESIAN_POINT('Ctrl Pts',(56.5485989129713,30.2575308518829,22.7364674663212));
#53445=CARTESIAN_POINT('Ctrl Pts',(56.4739250625041,30.3473806400944,22.7440976738615));
#53446=CARTESIAN_POINT('Ctrl Pts',(56.4087134840878,30.4154192244916,22.7504489683036));
#53447=CARTESIAN_POINT('Ctrl Pts',(56.2456792579482,30.5630561175936,22.7655957844854));
#53448=CARTESIAN_POINT('Ctrl Pts',(56.1446287702448,30.6385008105236,22.774469699348));
#53449=CARTESIAN_POINT('Ctrl Pts',(55.9905072924911,30.7323117683897,22.7868405394336));
#53450=CARTESIAN_POINT('Ctrl Pts',(55.9427167919945,30.7587765546672,22.7905290403572));
#53451=CARTESIAN_POINT('Ctrl Pts',(55.8858514754668,30.787281652349,22.7947012156162));
#53452=CARTESIAN_POINT('Ctrl Pts',(55.8777794056537,30.7912598537439,22.7952884994628));
#53453=CARTESIAN_POINT('Ctrl Pts',(55.8646859020451,30.7976030301898,22.7962327987375));
#53454=CARTESIAN_POINT('Ctrl Pts',(55.8596811421078,30.8000018608431,22.7965917897665));
#53455=CARTESIAN_POINT('Ctrl Pts',(55.8507698817116,30.8042274710534,22.7972274486804));
#53456=CARTESIAN_POINT('Ctrl Pts',(55.8468674062139,30.8060625007061,22.7975046139053));
#53457=CARTESIAN_POINT('Ctrl Pts',(55.8384173360632,30.8100024980625,22.7981021438577));
#53458=CARTESIAN_POINT('Ctrl Pts',(55.8338677553347,30.8121029883375,22.7984222359931));
#53459=CARTESIAN_POINT('Ctrl Pts',(55.821118096166,30.817931178514,22.799314857448));
#53460=CARTESIAN_POINT('Ctrl Pts',(55.8129004904925,30.8216205690145,22.7998851119913));
#53461=CARTESIAN_POINT('Ctrl Pts',(55.7635508701782,30.843376204672,22.8032810638749));
#53462=CARTESIAN_POINT('Ctrl Pts',(55.7218396850365,30.8601058905158,22.8060328915489));
#53463=CARTESIAN_POINT('Ctrl Pts',(55.5776517173704,30.912355432801,22.8152617051967));
#53464=CARTESIAN_POINT('Ctrl Pts',(55.4728580581662,30.940925938301,22.8214987688217));
#53465=CARTESIAN_POINT('Ctrl Pts',(55.2373693298085,30.9849116985918,22.8354270744988));
#53466=CARTESIAN_POINT('Ctrl Pts',(55.1064426962563,30.9962169393929,22.843129300215));
#53467=CARTESIAN_POINT('Ctrl Pts',(54.9596091462491,30.9944032585414,22.852242432457));
#53468=CARTESIAN_POINT('Ctrl Pts',(54.9438586895901,30.9940220434908,22.8532256701733));
#53469=CARTESIAN_POINT('Ctrl Pts',(54.918267910712,30.993099223391,22.8548331944138));
#53470=CARTESIAN_POINT('Ctrl Pts',(54.9084239884708,30.9926711914521,22.8554539602591));
#53471=CARTESIAN_POINT('Ctrl Pts',(54.8908770814694,30.9917779239375,22.856564940424));
#53472=CARTESIAN_POINT('Ctrl Pts',(54.8831728132156,30.9913408837629,22.8570542688876));
#53473=CARTESIAN_POINT('Ctrl Pts',(54.8669059379484,30.990323387462,22.8580907673206));
#53474=CARTESIAN_POINT('Ctrl Pts',(54.8583441728841,30.9897323535854,22.8586382569076));
#53475=CARTESIAN_POINT('Ctrl Pts',(54.83557861582,30.9880131259394,22.8600993331932));
#53476=CARTESIAN_POINT('Ctrl Pts',(54.8213828528857,30.9867879801013,22.8610159171576));
#53477=CARTESIAN_POINT('Ctrl Pts',(54.7525948384834,30.9801081486227,22.865484990311));
#53478=CARTESIAN_POINT('Ctrl Pts',(54.6982348175648,30.9725552990531,22.8691021241113));
#53479=CARTESIAN_POINT('Ctrl Pts',(54.4419864452696,30.9261118108534,22.886571589375));
#53480=CARTESIAN_POINT('Ctrl Pts',(54.2466400690703,30.8584164759875,22.9013022891682));
#53481=CARTESIAN_POINT('Ctrl Pts',(54.0376039193733,30.7475096544542,22.9172477620295));
#53482=CARTESIAN_POINT('Ctrl Pts',(54.0104541132185,30.732280404806,22.9193189215391));
#53483=CARTESIAN_POINT('Ctrl Pts',(53.976429916474,30.712133945314,22.9219044130911));
#53484=CARTESIAN_POINT('Ctrl Pts',(53.9692167319578,30.7078009904327,22.9224519498709));
#53485=CARTESIAN_POINT('Ctrl Pts',(53.9578623286614,30.7008822613596,22.9233126360267));
#53486=CARTESIAN_POINT('Ctrl Pts',(53.9537029121571,30.6983267642705,22.9236276710994));
#53487=CARTESIAN_POINT('Ctrl Pts',(53.9458647766519,30.6934713799886,22.9242207848029));
#53488=CARTESIAN_POINT('Ctrl Pts',(53.9421842188321,30.6911747861774,22.9244990559264));
#53489=CARTESIAN_POINT('Ctrl Pts',(53.9336282908388,30.6857972002675,22.925145425672));
#53490=CARTESIAN_POINT('Ctrl Pts',(53.9287587599139,30.6827070541403,22.9255129211782));
#53491=CARTESIAN_POINT('Ctrl Pts',(53.9131488998003,30.6727059993634,22.9266899783752));
#53492=CARTESIAN_POINT('Ctrl Pts',(53.9024612615716,30.6657128839652,22.9274943573537));
#53493=CARTESIAN_POINT('Ctrl Pts',(53.8772942793409,30.6488982690352,22.9293867216191));
#53494=CARTESIAN_POINT('Ctrl Pts',(53.8628753195279,30.638987840701,22.9304695100193));
#53495=CARTESIAN_POINT('Ctrl Pts',(53.8106999113317,30.6021066296465,22.934389737978));
#53496=CARTESIAN_POINT('Ctrl Pts',(53.7737550762776,30.5740089947114,22.9371698941071));
#53497=CARTESIAN_POINT('Ctrl Pts',(53.6148456686757,30.4441592129391,22.9493078032797));
#53498=CARTESIAN_POINT('Ctrl Pts',(53.5043107729896,30.3293475010938,22.9582876740802));
#53499=CARTESIAN_POINT('Ctrl Pts',(53.3726615447035,30.1551372828438,22.9713516382022));
#53500=CARTESIAN_POINT('Ctrl Pts',(53.338912400064,30.106055856973,22.9749738815175));
#53501=CARTESIAN_POINT('Ctrl Pts',(53.2994412992652,30.0427629085061,22.9796163039157));
#53502=CARTESIAN_POINT('Ctrl Pts',(53.2916170958747,30.0298942719655,22.9805586935427));
#53503=CARTESIAN_POINT('Ctrl Pts',(53.2794281756914,30.0093257486017,22.9820631939168));
#53504=CARTESIAN_POINT('Ctrl Pts',(53.274967596055,30.0016831188956,22.9826218376749));
#53505=CARTESIAN_POINT('Ctrl Pts',(53.2667298270567,29.9873505402908,22.9836689005801));
#53506=CARTESIAN_POINT('Ctrl Pts',(53.2629401348411,29.9806679376805,22.9841568600963));
#53507=CARTESIAN_POINT('Ctrl Pts',(53.2545741703182,29.9657150582695,22.9852482701948));
#53508=CARTESIAN_POINT('Ctrl Pts',(53.2500179106197,29.9574338528013,22.9858524177522));
#53509=CARTESIAN_POINT('Ctrl Pts',(53.2368092785104,29.9330172836346,22.9876330169227));
#53510=CARTESIAN_POINT('Ctrl Pts',(53.2283201846487,29.9167951608448,22.9888151619028));
#53511=CARTESIAN_POINT('Ctrl Pts',(53.1557643431617,29.773373461889,22.9992620178185));
#53512=CARTESIAN_POINT('Ctrl Pts',(53.1052803448653,29.639792556273,23.0090052571375));
#53513=CARTESIAN_POINT('Ctrl Pts',(53.0610441144254,29.4696738527281,23.0212400442453));
#53514=CARTESIAN_POINT('Ctrl Pts',(53.0534544604073,29.4371521061416,23.023569125178));
#53515=CARTESIAN_POINT('Ctrl Pts',(53.0466869607994,29.4044696940301,23.0258937941419));
#53516=CARTESIAN_POINT('Origin',(55.,29.,14.365));
#53517=CARTESIAN_POINT('',(52.5495005484666,29.0016395226469,5.18832749621205));
#53518=CARTESIAN_POINT('',(56.0772398577513,31.2053700969644,4.93052640483872));
#53519=CARTESIAN_POINT('Ctrl Pts',(52.5467359272522,29.0016413723348,5.18832749621205));
#53520=CARTESIAN_POINT('Ctrl Pts',(52.5460824238429,29.0920814519017,5.18361297623425));
#53521=CARTESIAN_POINT('Ctrl Pts',(52.5915758653443,29.9920162182401,5.13666417946793));
#53522=CARTESIAN_POINT('Ctrl Pts',(53.6625878394777,31.5282585313447,5.05073048234352));
#53523=CARTESIAN_POINT('Ctrl Pts',(55.4037421823906,31.5296428126932,4.96951130519688));
#53524=CARTESIAN_POINT('Ctrl Pts',(56.0772398577513,31.2053700969644,4.93052640483872));
#53525=CARTESIAN_POINT('',(53.9249115396487,31.2020751695661,4.9305));
#53526=CARTESIAN_POINT('Origin',(55.,29.,4.9305));
#53527=CARTESIAN_POINT('',(52.5493359835256,29.0024358842253,5.07267250378794));
#53528=CARTESIAN_POINT('Ctrl Pts',(53.9249115396487,31.2020751695661,4.9305));
#53529=CARTESIAN_POINT('Ctrl Pts',(53.1944672756053,30.8454605498401,4.97273427678848));
#53530=CARTESIAN_POINT('Ctrl Pts',(52.5965917064306,30.0088392096125,5.02012511138446));
#53531=CARTESIAN_POINT('Ctrl Pts',(52.5465875494899,29.1013071020944,5.06751594598044));
#53532=CARTESIAN_POINT('Ctrl Pts',(52.5473557780223,29.0024378524883,5.07267250378794));
#53533=CARTESIAN_POINT('',(52.5495001447487,29.0008422667624,5.87267250374925));
#53534=CARTESIAN_POINT('Ctrl Pts',(52.5495012105149,29.0024357199948,5.07267250378794));
#53535=CARTESIAN_POINT('Ctrl Pts',(52.5494224648678,28.9232122816583,5.0768080814921));
#53536=CARTESIAN_POINT('Ctrl Pts',(52.5531897391159,28.8438158281259,5.08094365919625));
#53537=CARTESIAN_POINT('Ctrl Pts',(52.5608267508401,28.764661710334,5.0850792369004));
#53538=CARTESIAN_POINT('Ctrl Pts',(52.5684526154381,28.6856231273839,5.08920877823741));
#53539=CARTESIAN_POINT('Ctrl Pts',(52.5799369575232,28.606826657945,5.09333831957442));
#53540=CARTESIAN_POINT('Ctrl Pts',(52.5952514853866,28.5286881802196,5.09746786091143));
#53541=CARTESIAN_POINT('Ctrl Pts',(52.6105535814955,28.4506131323553,5.10159405004295));
#53542=CARTESIAN_POINT('Ctrl Pts',(52.6296796078446,28.3731954926565,5.10572023917448));
#53543=CARTESIAN_POINT('Ctrl Pts',(52.652549558233,28.296845199513,5.10984642830601));
#53544=CARTESIAN_POINT('Ctrl Pts',(52.6754086101304,28.2205312904879,5.11397065113528));
#53545=CARTESIAN_POINT('Ctrl Pts',(52.702007908902,28.1452841847404,5.11809487396455));
#53546=CARTESIAN_POINT('Ctrl Pts',(52.7322169248663,28.0715011178591,5.12221909679382));
#53547=CARTESIAN_POINT('Ctrl Pts',(52.7624216675123,27.9977284882103,5.12634273621725));
#53548=CARTESIAN_POINT('Ctrl Pts',(52.7962349286359,27.9254199362223,5.13046637564066));
#53549=CARTESIAN_POINT('Ctrl Pts',(52.8334777514998,27.8549534521455,5.13459001506409));
#53550=CARTESIAN_POINT('Ctrl Pts',(52.8707535168953,27.7844246380892,5.13871730198553));
#53551=CARTESIAN_POINT('Ctrl Pts',(52.9114646769339,27.7157415784887,5.14284458890697));
#53552=CARTESIAN_POINT('Ctrl Pts',(52.9553863302534,27.6492575406521,5.14697187582841));
#53553=CARTESIAN_POINT('Ctrl Pts',(52.9993258736485,27.5827464226767,5.15110084386769));
#53554=CARTESIAN_POINT('Ctrl Pts',(53.0464782241391,27.5184365014121,5.15522981190697));
#53555=CARTESIAN_POINT('Ctrl Pts',(53.0965767764186,27.4566496567756,5.15935877994625));
#53556=CARTESIAN_POINT('Ctrl Pts',(53.1467657495005,27.3947512956217,5.16349520018898));
#53557=CARTESIAN_POINT('Ctrl Pts',(53.1999112198573,27.3353854695021,5.1676316204317));
#53558=CARTESIAN_POINT('Ctrl Pts',(53.2557084502778,27.2788384039935,5.17176804067443));
#53559=CARTESIAN_POINT('Ctrl Pts',(53.3102842705368,27.2235291626545,5.17581391402659));
#53560=CARTESIAN_POINT('Ctrl Pts',(53.3673965452187,27.1709167338838,5.17985978737875));
#53561=CARTESIAN_POINT('Ctrl Pts',(53.4267314148439,27.1212301341141,5.18390566073091));
#53562=CARTESIAN_POINT('Ctrl Pts',(53.4888727187617,27.0691934461356,5.18814289673021));
#53563=CARTESIAN_POINT('Ctrl Pts',(53.5537128604257,27.0201473329936,5.19238013272951));
#53564=CARTESIAN_POINT('Ctrl Pts',(53.6209324746831,26.9743833011607,5.19661736872881));
#53565=CARTESIAN_POINT('Ctrl Pts',(53.6880561113035,26.9286846122147,5.20084855470976));
#53566=CARTESIAN_POINT('Ctrl Pts',(53.757552092408,26.886258955162,5.20507974069071));
#53567=CARTESIAN_POINT('Ctrl Pts',(53.8290676315859,26.8473579864269,5.20931092667167));
#53568=CARTESIAN_POINT('Ctrl Pts',(53.9005001602593,26.8085021713615,5.21353720137199));
#53569=CARTESIAN_POINT('Ctrl Pts',(53.9739471826816,26.7731631330336,5.21776347607231));
#53570=CARTESIAN_POINT('Ctrl Pts',(54.049027780934,26.7415487411581,5.22198975077262));
#53571=CARTESIAN_POINT('Ctrl Pts',(54.1240604562315,26.7099545283316,5.22621332789758));
#53572=CARTESIAN_POINT('Ctrl Pts',(54.2007242114499,26.682080421538,5.23043690502253));
#53573=CARTESIAN_POINT('Ctrl Pts',(54.2786154424704,26.6580874119306,5.23466048214749));
#53574=CARTESIAN_POINT('Ctrl Pts',(54.3564806232596,26.6341024266341,5.23888264672369));
#53575=CARTESIAN_POINT('Ctrl Pts',(54.4355720220388,26.6139960968527,5.24310481129989));
#53576=CARTESIAN_POINT('Ctrl Pts',(54.5154693972406,26.5978800310997,5.24732697587609));
#53577=CARTESIAN_POINT('Ctrl Pts',(54.5953643267749,26.5817644586612,5.25154901121137));
#53578=CARTESIAN_POINT('Ctrl Pts',(54.6760647292506,26.5696389979145,5.25577104654666));
#53579=CARTESIAN_POINT('Ctrl Pts',(54.7571400476834,26.5615641707109,5.25999308188194));
#53580=CARTESIAN_POINT('Ctrl Pts',(54.8382930369531,26.5534816077549,5.26421916196258));
#53581=CARTESIAN_POINT('Ctrl Pts',(54.9198211976031,26.5494574773029,5.26844524204323));
#53582=CARTESIAN_POINT('Ctrl Pts',(55.0012892530824,26.5495003391499,5.27267132212388));
#53583=CARTESIAN_POINT('Ctrl Pts',(55.0827941835916,26.5495432203976,5.27689931506261));
#53584=CARTESIAN_POINT('Ctrl Pts',(55.164238491225,26.5536567390748,5.28112730800134));
#53585=CARTESIAN_POINT('Ctrl Pts',(55.2451897908321,26.5617973389253,5.28535530094008));
#53586=CARTESIAN_POINT('Ctrl Pts',(55.3262852922789,26.5699524399572,5.28959082537444));
#53587=CARTESIAN_POINT('Ctrl Pts',(55.4068855710543,26.5821488893415,5.29382634980881));
#53588=CARTESIAN_POINT('Ctrl Pts',(55.4865663435973,26.5982915573954,5.29806187424317));
#53589=CARTESIAN_POINT('Ctrl Pts',(55.565244056291,26.6142310137877,5.3022440798609));
#53590=CARTESIAN_POINT('Ctrl Pts',(55.6430248886805,26.6340176960711,5.30642628547863));
#53591=CARTESIAN_POINT('Ctrl Pts',(55.7195166982866,26.6575128664416,5.31060849109635));
#53592=CARTESIAN_POINT('Ctrl Pts',(55.797057875483,26.6813303598222,5.31484807110559));
#53593=CARTESIAN_POINT('Ctrl Pts',(55.8735539493563,26.7090447615575,5.31908765111483));
#53594=CARTESIAN_POINT('Ctrl Pts',(55.9485863104976,26.7405455832134,5.32332723112406));
#53595=CARTESIAN_POINT('Ctrl Pts',(56.0235143306667,26.7720025994192,5.32756091551849));
#53596=CARTESIAN_POINT('Ctrl Pts',(56.0969822579391,26.8072353987265,5.33179459991293));
#53597=CARTESIAN_POINT('Ctrl Pts',(56.1685868793458,26.8460838095644,5.33602828430736));
#53598=CARTESIAN_POINT('Ctrl Pts',(56.2401122064234,26.8848892000131,5.34025728035685));
#53599=CARTESIAN_POINT('Ctrl Pts',(56.3097779240461,26.9273020243104,5.34448627640635));
#53600=CARTESIAN_POINT('Ctrl Pts',(56.377202362273,26.9731147286169,5.34871527245585));
#53601=CARTESIAN_POINT('Ctrl Pts',(56.4445859316388,27.0188996638667,5.35294170512838));
#53602=CARTESIAN_POINT('Ctrl Pts',(56.5097305369672,27.0680801282834,5.35716813780091));
#53603=CARTESIAN_POINT('Ctrl Pts',(56.5722816165271,27.1204040944046,5.36139457047344));
#53604=CARTESIAN_POINT('Ctrl Pts',(56.6348137209451,27.1727121878233,5.36561972103925));
#53605=CARTESIAN_POINT('Ctrl Pts',(56.6947535075508,27.2281615922263,5.36984487160506));
#53606=CARTESIAN_POINT('Ctrl Pts',(56.7517788976561,27.2864595295918,5.37407002217087));
#53607=CARTESIAN_POINT('Ctrl Pts',(56.808804254942,27.3447574334055,5.37829517030501));
#53608=CARTESIAN_POINT('Ctrl Pts',(56.862914896437,27.4059035351946,5.38252031843916));
#53609=CARTESIAN_POINT('Ctrl Pts',(56.9138260782558,27.4695686907973,5.38674546657331));
#53610=CARTESIAN_POINT('Ctrl Pts',(56.9647881705314,27.5332975106489,5.39097483979543));
#53611=CARTESIAN_POINT('Ctrl Pts',(57.0125441218747,27.5995500543816,5.39520421301754));
#53612=CARTESIAN_POINT('Ctrl Pts',(57.0568502762523,27.6679650188224,5.39943358623965));
#53613=CARTESIAN_POINT('Ctrl Pts',(57.101177550683,27.7364125956102,5.40366497553804));
#53614=CARTESIAN_POINT('Ctrl Pts',(57.1420515193405,27.8070242459414,5.40789636483643));
#53615=CARTESIAN_POINT('Ctrl Pts',(57.179273880197,27.8794128302131,5.41212775413482));
#53616=CARTESIAN_POINT('Ctrl Pts',(57.2165637116688,27.9519326286852,5.4163668134045));
#53617=CARTESIAN_POINT('Ctrl Pts',(57.2501885161182,28.0262353752396,5.42060587267418));
#53618=CARTESIAN_POINT('Ctrl Pts',(57.2799977056027,28.1019127478654,5.42484493194386));
#53619=CARTESIAN_POINT('Ctrl Pts',(57.3092190448736,28.1760977297077,5.42900039511651));
#53620=CARTESIAN_POINT('Ctrl Pts',(57.3347738512411,28.2516031919899,5.43315585828916));
#53621=CARTESIAN_POINT('Ctrl Pts',(57.356567525692,28.3280329272548,5.4373113214618));
#53622=CARTESIAN_POINT('Ctrl Pts',(57.3787400345672,28.4057912230072,5.44153901809384));
#53623=CARTESIAN_POINT('Ctrl Pts',(57.3971019507572,28.4847960014073,5.44576671472587));
#53624=CARTESIAN_POINT('Ctrl Pts',(57.4115163311385,28.5646389605716,5.4499944113579));
#53625=CARTESIAN_POINT('Ctrl Pts',(57.4259098908971,28.6443665918421,5.45421600136069));
#53626=CARTESIAN_POINT('Ctrl Pts',(57.4363671567194,28.7249295450193,5.45843759136349));
#53627=CARTESIAN_POINT('Ctrl Pts',(57.4428011376394,28.8059050439926,5.46265918136628));
#53628=CARTESIAN_POINT('Ctrl Pts',(57.4492374561203,28.8869099625686,5.46688230513549));
#53629=CARTESIAN_POINT('Ctrl Pts',(57.4516474613226,28.9683272704142,5.47110542890469));
#53630=CARTESIAN_POINT('Ctrl Pts',(57.449995460337,29.0497241825289,5.4753285526739));
#53631=CARTESIAN_POINT('Ctrl Pts',(57.4483470598133,29.1309436937316,5.47954247233464));
#53632=CARTESIAN_POINT('Ctrl Pts',(57.4426543248039,29.2121424316842,5.48375639199537));
#53633=CARTESIAN_POINT('Ctrl Pts',(57.4329338161821,29.2928878558045,5.48797031165611));
#53634=CARTESIAN_POINT('Ctrl Pts',(57.4232165743765,29.3736061434363,5.49218281512536));
#53635=CARTESIAN_POINT('Ctrl Pts',(57.4094743025865,29.4538709576714,5.49639531859461));
#53636=CARTESIAN_POINT('Ctrl Pts',(57.3917754470409,29.5332545929782,5.50060782206385));
#53637=CARTESIAN_POINT('Ctrl Pts',(57.3740770926785,29.6126359803575,5.50482020624652));
#53638=CARTESIAN_POINT('Ctrl Pts',(57.35242247976,29.6911357840195,5.50903259042918));
#53639=CARTESIAN_POINT('Ctrl Pts',(57.3269309246493,29.7683376353602,5.51324497461185));
#53640=CARTESIAN_POINT('Ctrl Pts',(57.3013281380643,29.8458763541735,5.5174757393798));
#53641=CARTESIAN_POINT('Ctrl Pts',(57.2718549837999,29.9221053139697,5.52170650414775));
#53642=CARTESIAN_POINT('Ctrl Pts',(57.2386819677278,29.9966209396608,5.5259372689157));
#53643=CARTESIAN_POINT('Ctrl Pts',(57.2056054035238,30.0709199081966,5.53015573256625));
#53644=CARTESIAN_POINT('Ctrl Pts',(57.168850712839,30.1435150931823,5.53437419621681));
#53645=CARTESIAN_POINT('Ctrl Pts',(57.1286331694868,30.2140309220775,5.53859265986736));
#53646=CARTESIAN_POINT('Ctrl Pts',(57.0882397134933,30.2848551891488,5.54282957519401));
#53647=CARTESIAN_POINT('Ctrl Pts',(57.0443533024324,30.3535814727305,5.54706649052066));
#53648=CARTESIAN_POINT('Ctrl Pts',(56.9972350276436,30.4198600263243,5.55130340584731));
#53649=CARTESIAN_POINT('Ctrl Pts',(56.9501167528548,30.486138579918,5.55554032117396));
#53650=CARTESIAN_POINT('Ctrl Pts',(56.8997669543256,30.5499690741391,5.55977723650061));
#53651=CARTESIAN_POINT('Ctrl Pts',(56.8464850698016,30.6110379067544,5.56401415182726));
#53652=CARTESIAN_POINT('Ctrl Pts',(56.793245634285,30.6720580865987,5.56824769165674));
#53653=CARTESIAN_POINT('Ctrl Pts',(56.7368794524142,30.7305495121183,5.57248123148623));
#53654=CARTESIAN_POINT('Ctrl Pts',(56.6776559975179,30.7861748525809,5.57671477131572));
#53655=CARTESIAN_POINT('Ctrl Pts',(56.6185169604046,30.8417209040535,5.58094227660962));
#53656=CARTESIAN_POINT('Ctrl Pts',(56.5565290750968,30.8944086693625,5.58516978190351));
#53657=CARTESIAN_POINT('Ctrl Pts',(56.4920010549055,30.9439349531712,5.5893972871974));
#53658=CARTESIAN_POINT('Ctrl Pts',(56.4275473552574,30.9934041947786,5.59361992343613));
#53659=CARTESIAN_POINT('Ctrl Pts',(56.3605597018324,31.0397189106184,5.59784255967486));
#53660=CARTESIAN_POINT('Ctrl Pts',(56.2913814346201,31.0826147604198,5.60206519591359));
#53661=CARTESIAN_POINT('Ctrl Pts',(56.2222469102552,31.1254834862893,5.6062851620922));
#53662=CARTESIAN_POINT('Ctrl Pts',(56.1509249154057,31.1649373935957,5.6105051282708));
#53663=CARTESIAN_POINT('Ctrl Pts',(56.0777885058566,31.2007549128977,5.61472509444941));
#53664=CARTESIAN_POINT('Ctrl Pts',(56.0046760072943,31.236560722133,5.6189436809656));
#53665=CARTESIAN_POINT('Ctrl Pts',(55.9297506887809,31.2687323003632,5.62316226748179));
#53666=CARTESIAN_POINT('Ctrl Pts',(55.8534097258461,31.2970942709935,5.62738085399797));
#53667=CARTESIAN_POINT('Ctrl Pts',(55.7770704088625,31.3254556301249,5.63159934955922));
#53668=CARTESIAN_POINT('Ctrl Pts',(55.6993159437972,31.3500073843642,5.63581784512047));
#53669=CARTESIAN_POINT('Ctrl Pts',(55.6205616338611,31.3706230211866,5.64003634068171));
#53670=CARTESIAN_POINT('Ctrl Pts',(55.5417160104358,31.3912625612814,5.64425972747429));
#53671=CARTESIAN_POINT('Ctrl Pts',(55.4618686754863,31.4079567437039,5.64848311426688));
#53672=CARTESIAN_POINT('Ctrl Pts',(55.3814478996298,31.4206296184811,5.65270650105946));
#53673=CARTESIAN_POINT('Ctrl Pts',(55.3010043621856,31.4333060800771,5.65693108320223));
#53674=CARTESIAN_POINT('Ctrl Pts',(55.2199875239284,31.4419589243,5.661155665345));
#53675=CARTESIAN_POINT('Ctrl Pts',(55.1388306373433,31.4465641835306,5.66538024748776));
#53676=CARTESIAN_POINT('Ctrl Pts',(55.0575268890906,31.4511777764477,5.669612474443));
#53677=CARTESIAN_POINT('Ctrl Pts',(54.9760830516879,31.4517291433342,5.67384470139824));
#53678=CARTESIAN_POINT('Ctrl Pts',(54.8949323643657,31.4482465239314,5.67807692835348));
#53679=CARTESIAN_POINT('Ctrl Pts',(54.8141436080213,31.4447794369645,5.68229027963322));
#53680=CARTESIAN_POINT('Ctrl Pts',(54.7336458330819,31.4373144061993,5.68650363091296));
#53681=CARTESIAN_POINT('Ctrl Pts',(54.6538573734615,31.425929828353,5.69071698219271));
#53682=CARTESIAN_POINT('Ctrl Pts',(54.5736895690821,31.414491123883,5.69495036535091));
#53683=CARTESIAN_POINT('Ctrl Pts',(54.4939409450085,31.3990531095036,5.69918374850912));
#53684=CARTESIAN_POINT('Ctrl Pts',(54.4150411429032,31.3796582497292,5.70341713166733));
#53685=CARTESIAN_POINT('Ctrl Pts',(54.336253552147,31.3602909733367,5.70764449410529));
#53686=CARTESIAN_POINT('Ctrl Pts',(54.2583128328872,31.3369781384252,5.71187185654326));
#53687=CARTESIAN_POINT('Ctrl Pts',(54.1816413452542,31.3098137072506,5.71609921898122));
#53688=CARTESIAN_POINT('Ctrl Pts',(54.1050577729587,31.2826804241626,5.72032173411536));
#53689=CARTESIAN_POINT('Ctrl Pts',(54.0297409752458,31.2517044766712,5.7245442492495));
#53690=CARTESIAN_POINT('Ctrl Pts',(53.9560995623481,31.2170300237638,5.72876676438364));
#53691=CARTESIAN_POINT('Ctrl Pts',(53.882504484241,31.1823773878403,5.73298662273342));
#53692=CARTESIAN_POINT('Ctrl Pts',(53.8105831173282,31.144031063345,5.73720648108319));
#53693=CARTESIAN_POINT('Ctrl Pts',(53.7407243612159,31.102183416252,5.74142633943296));
#53694=CARTESIAN_POINT('Ctrl Pts',(53.6708882222943,31.0603493175854,5.74564483157833));
#53695=CARTESIAN_POINT('Ctrl Pts',(53.603113766025,31.0150163860036,5.74986332372369));
#53696=CARTESIAN_POINT('Ctrl Pts',(53.5377642646719,30.9664223616328,5.75408181586905));
#53697=CARTESIAN_POINT('Ctrl Pts',(53.4724159608207,30.9178292277269,5.75830023071233));
#53698=CARTESIAN_POINT('Ctrl Pts',(53.4094928954424,30.8659753978873,5.76251864555561));
#53699=CARTESIAN_POINT('Ctrl Pts',(53.3493272111909,30.8111404126365,5.76673706039889));
#53700=CARTESIAN_POINT('Ctrl Pts',(53.2890881052569,30.756238510888,5.77096062307883));
#53701=CARTESIAN_POINT('Ctrl Pts',(53.2316134514668,30.6983484949871,5.77518418575877));
#53702=CARTESIAN_POINT('Ctrl Pts',(53.1772000794838,30.6377883562189,5.77940774843871));
#53703=CARTESIAN_POINT('Ctrl Pts',(53.122774167702,30.5772142611027,5.78363228445708));
#53704=CARTESIAN_POINT('Ctrl Pts',(53.0714112291474,30.5139691845898,5.78785682047545));
#53705=CARTESIAN_POINT('Ctrl Pts',(53.0233671420721,30.4484035331909,5.79208135649382));
#53706=CARTESIAN_POINT('Ctrl Pts',(52.9752358696952,30.3827189002181,5.79631355875104));
#53707=CARTESIAN_POINT('Ctrl Pts',(52.9304357411302,30.3147056654596,5.80054576100826));
#53708=CARTESIAN_POINT('Ctrl Pts',(52.8891788279744,30.2447426359406,5.80477796326547));
#53709=CARTESIAN_POINT('Ctrl Pts',(52.848099846182,30.1750813405138,5.8089919130297));
#53710=CARTESIAN_POINT('Ctrl Pts',(52.8105337072027,30.103487477362,5.81320586279394));
#53711=CARTESIAN_POINT('Ctrl Pts',(52.7766423574683,30.0303548143216,5.81741981255817));
#53712=CARTESIAN_POINT('Ctrl Pts',(52.7396108236006,29.9504460851199,5.82202420349075));
#53713=CARTESIAN_POINT('Ctrl Pts',(52.7068454862175,29.8684405297593,5.82662859442335));
#53714=CARTESIAN_POINT('Ctrl Pts',(52.6785676497307,29.7847942998794,5.83123298535594));
#53715=CARTESIAN_POINT('Ctrl Pts',(52.6504458222707,29.70160954685,5.83581197383071));
#53716=CARTESIAN_POINT('Ctrl Pts',(52.626762269592,29.6168024762131,5.84039096230549));
#53717=CARTESIAN_POINT('Ctrl Pts',(52.6076887509001,29.5308456813709,5.84496995078027));
#53718=CARTESIAN_POINT('Ctrl Pts',(52.5884565134465,29.4441736039286,5.84958704294176));
#53719=CARTESIAN_POINT('Ctrl Pts',(52.573911597095,29.356332870434,5.85420413510326));
#53720=CARTESIAN_POINT('Ctrl Pts',(52.5641801417191,29.2678280567907,5.85882122726475));
#53721=CARTESIAN_POINT('Ctrl Pts',(52.5544486863431,29.1793232431473,5.86343831942625));
#53722=CARTESIAN_POINT('Ctrl Pts',(52.5495308425188,29.0901546848532,5.86805541158775));
#53723=CARTESIAN_POINT('Ctrl Pts',(52.5495001447487,29.0008422667624,5.87267250374924));
#53724=CARTESIAN_POINT('',(52.5495009959581,28.9977906585885,6.67267250383498));
#53725=CARTESIAN_POINT('Ctrl Pts',(52.5495001447484,29.0008422660139,5.87267250378794));
#53726=CARTESIAN_POINT('Ctrl Pts',(52.5494714453592,28.9173438843335,5.87698903369265));
#53727=CARTESIAN_POINT('Ctrl Pts',(52.5537147778818,28.8338772411954,5.88130556359736));
#53728=CARTESIAN_POINT('Ctrl Pts',(52.5621942075986,28.7508952659337,5.88562209350207));
#53729=CARTESIAN_POINT('Ctrl Pts',(52.5706794363711,28.6678565395561,5.88994157546822));
#53730=CARTESIAN_POINT('Ctrl Pts',(52.5834064823908,28.5853035711796,5.89426105743437));
#53731=CARTESIAN_POINT('Ctrl Pts',(52.6002878479079,28.5036817179453,5.89858053940052));
#53732=CARTESIAN_POINT('Ctrl Pts',(52.6171986312631,28.4219176286784,5.90290754859073));
#53733=CARTESIAN_POINT('Ctrl Pts',(52.6382781014815,28.34108831937,5.90723455778094));
#53734=CARTESIAN_POINT('Ctrl Pts',(52.6633881422363,28.2616266011304,5.91156156697115));
#53735=CARTESIAN_POINT('Ctrl Pts',(52.6885222735803,28.1820886472676,5.91589272749675));
#53736=CARTESIAN_POINT('Ctrl Pts',(52.7176945279371,28.1039213037629,5.92022388802234));
#53737=CARTESIAN_POINT('Ctrl Pts',(52.7507185128329,28.0275376400666,5.92455504854794));
#53738=CARTESIAN_POINT('Ctrl Pts',(52.7838107128232,27.9509961965367,5.92889515561726));
#53739=CARTESIAN_POINT('Ctrl Pts',(52.8207703437845,27.8762461804629,5.93323526268658));
#53740=CARTESIAN_POINT('Ctrl Pts',(52.8613649006829,27.8036763974706,5.9375753697559));
#53741=CARTESIAN_POINT('Ctrl Pts',(52.8817778881116,27.7671846561854,5.93975779414514));
#53742=CARTESIAN_POINT('Ctrl Pts',(52.9031093113642,27.7312437481034,5.94194021853437));
#53743=CARTESIAN_POINT('Ctrl Pts',(52.9253256277235,27.695900119232,5.9441226429236));
#53744=CARTESIAN_POINT('Ctrl Pts',(52.9684138980889,27.6273515888692,5.94835542799088));
#53745=CARTESIAN_POINT('Ctrl Pts',(53.014983225727,27.5608134483899,5.95258821305815));
#53746=CARTESIAN_POINT('Ctrl Pts',(53.0648200520184,27.4966607771598,5.95682099812542));
#53747=CARTESIAN_POINT('Ctrl Pts',(53.1145858079948,27.4325995915015,5.96104774698633));
#53748=CARTESIAN_POINT('Ctrl Pts',(53.1676095253359,27.3709174823951,5.96527449584723));
#53749=CARTESIAN_POINT('Ctrl Pts',(53.2236335657583,27.3119619254,5.96950124470814));
#53750=CARTESIAN_POINT('Ctrl Pts',(53.2795930839848,27.2530742667923,5.97372312567455));
#53751=CARTESIAN_POINT('Ctrl Pts',(53.3385457393656,27.1969072543506,5.97794500664097));
#53752=CARTESIAN_POINT('Ctrl Pts',(53.4001936366458,27.1437753773394,5.98216688760738));
#53753=CARTESIAN_POINT('Ctrl Pts',(53.4618025611284,27.0906770894364,5.98638609956934));
#53754=CARTESIAN_POINT('Ctrl Pts',(53.5261029941909,27.0406104304442,5.99060531153131));
#53755=CARTESIAN_POINT('Ctrl Pts',(53.5927610265866,26.9938522682249,5.99482452349327));
#53756=CARTESIAN_POINT('Ctrl Pts',(53.6593972956249,26.9471093722017,5.99904235791355));
#53757=CARTESIAN_POINT('Ctrl Pts',(53.7283892553533,26.9036730942794,6.00326019233383));
#53758=CARTESIAN_POINT('Ctrl Pts',(53.7993719794597,26.8637784276219,6.00747802675412));
#53759=CARTESIAN_POINT('Ctrl Pts',(53.8703532265075,26.8238845911209,6.01169577340672));
#53760=CARTESIAN_POINT('Ctrl Pts',(53.9433247500623,26.787532445918,6.01591352005932));
#53761=CARTESIAN_POINT('Ctrl Pts',(54.0178961121557,26.7549115377159,6.02013126671192));
#53762=CARTESIAN_POINT('Ctrl Pts',(54.0925871803587,26.7222382646126,6.02435578392668));
#53763=CARTESIAN_POINT('Ctrl Pts',(54.1688827970325,26.6933083977567,6.02858030114144));
#53764=CARTESIAN_POINT('Ctrl Pts',(54.2463712968226,26.6682637310907,6.03280481835621));
#53765=CARTESIAN_POINT('Ctrl Pts',(54.3238475441992,26.6432230244653,6.03702866759402));
#53766=CARTESIAN_POINT('Ctrl Pts',(54.4025158421119,26.6220663907872,6.04125251683184));
#53767=CARTESIAN_POINT('Ctrl Pts',(54.4819520641742,26.6048848490758,6.04547636606966));
#53768=CARTESIAN_POINT('Ctrl Pts',(54.5615323588867,26.5876721453808,6.04970787605894));
#53769=CARTESIAN_POINT('Ctrl Pts',(54.641882901495,26.5744490174182,6.05393938604822));
#53770=CARTESIAN_POINT('Ctrl Pts',(54.7225714615492,26.5652549094303,6.0581708960375));
#53771=CARTESIAN_POINT('Ctrl Pts',(54.8030060754429,26.5560897374952,6.06238908845469));
#53772=CARTESIAN_POINT('Ctrl Pts',(54.8837761231954,26.5509282062687,6.06660728087188));
#53773=CARTESIAN_POINT('Ctrl Pts',(54.9644546244757,26.5497578127298,6.07082547328907));
#53774=CARTESIAN_POINT('Ctrl Pts',(55.0454104707045,26.5485833957803,6.07505816640148));
#53775=CARTESIAN_POINT('Ctrl Pts',(55.1265750617058,26.5514232685202,6.0792908595139));
#53776=CARTESIAN_POINT('Ctrl Pts',(55.2075175257847,26.558302490788,6.08352355262632));
#53777=CARTESIAN_POINT('Ctrl Pts',(55.2883445720611,26.5651719038076,6.08775021024003));
#53778=CARTESIAN_POINT('Ctrl Pts',(55.3689496614782,26.5760691876122,6.09197686785374));
#53779=CARTESIAN_POINT('Ctrl Pts',(55.4489010794414,26.5909673993745,6.09620352546745));
#53780=CARTESIAN_POINT('Ctrl Pts',(55.5287618547007,26.6058487207023,6.10042539122524));
#53781=CARTESIAN_POINT('Ctrl Pts',(55.6079699768964,26.62472187115,6.10464725698304));
#53782=CARTESIAN_POINT('Ctrl Pts',(55.6860994621945,26.6475081768524,6.10886912274083));
#53783=CARTESIAN_POINT('Ctrl Pts',(55.7641781934191,26.6702796802323,6.11308824591196));
#53784=CARTESIAN_POINT('Ctrl Pts',(55.8411792342355,26.6969591618318,6.11730736908308));
#53785=CARTESIAN_POINT('Ctrl Pts',(55.9166885752473,26.7274172609097,6.12152649225421));
#53786=CARTESIAN_POINT('Ctrl Pts',(55.9921732824894,26.7578654234978,6.12574423900082));
#53787=CARTESIAN_POINT('Ctrl Pts',(56.0661668259025,26.7920895818231,6.12996198574742));
#53788=CARTESIAN_POINT('Ctrl Pts',(56.1382734362833,26.8299115607304,6.13417973249403));
#53789=CARTESIAN_POINT('Ctrl Pts',(56.2103785674707,26.8677327637584,6.13839739271786));
#53790=CARTESIAN_POINT('Ctrl Pts',(56.2805964317636,26.9091514238056,6.1426150529417));
#53791=CARTESIAN_POINT('Ctrl Pts',(56.3485554944774,26.9539432245622,6.14683271316554));
#53792=CARTESIAN_POINT('Ctrl Pts',(56.4166269019741,26.9988090717364,6.15105734570629));
#53793=CARTESIAN_POINT('Ctrl Pts',(56.4824316475184,27.0470589586799,6.15528197824704));
#53794=CARTESIAN_POINT('Ctrl Pts',(56.5456266484317,27.0984247283745,6.15950661078779));
#53795=CARTESIAN_POINT('Ctrl Pts',(56.6088086988259,27.1497799717082,6.16373037757675));
#53796=CARTESIAN_POINT('Ctrl Pts',(56.6693817414734,27.2042494936698,6.16795414436571));
#53797=CARTESIAN_POINT('Ctrl Pts',(56.7270385517084,27.2615270807652,6.17217791115468));
#53798=CARTESIAN_POINT('Ctrl Pts',(56.7847999776588,27.3189085954924,6.17640934178044));
#53799=CARTESIAN_POINT('Ctrl Pts',(56.8396342828474,27.3791080133401,6.18064077240621));
#53800=CARTESIAN_POINT('Ctrl Pts',(56.8912730940144,27.441784246692,6.18487220303197));
#53801=CARTESIAN_POINT('Ctrl Pts',(56.942756547875,27.5042719162376,6.18909090323949));
#53802=CARTESIAN_POINT('Ctrl Pts',(56.9910635043335,27.5692211037456,6.193309603447));
#53803=CARTESIAN_POINT('Ctrl Pts',(57.0359719347866,27.6362666936819,6.19752830365451));
#53804=CARTESIAN_POINT('Ctrl Pts',(57.0810275402198,27.7035320070256,6.20176082948703));
#53805=CARTESIAN_POINT('Ctrl Pts',(57.1228298786424,27.7731577113981,6.20599335531954));
#53806=CARTESIAN_POINT('Ctrl Pts',(57.1611233504387,27.8447960724666,6.21022588115206));
#53807=CARTESIAN_POINT('Ctrl Pts',(57.1993621864955,27.9163322225145,6.21445236816991));
#53808=CARTESIAN_POINT('Ctrl Pts',(57.2341018819306,27.9898749196236,6.21867885518777));
#53809=CARTESIAN_POINT('Ctrl Pts',(57.2651299963173,28.0650474077348,6.22290534220562));
#53810=CARTESIAN_POINT('Ctrl Pts',(57.2961244944811,28.1401384530909,6.22712725019789));
#53811=CARTESIAN_POINT('Ctrl Pts',(57.3234152239855,28.2168553542244,6.23134915819015));
#53812=CARTESIAN_POINT('Ctrl Pts',(57.3468362310893,28.2947979336057,6.23557106618242));
#53813=CARTESIAN_POINT('Ctrl Pts',(57.3702408052715,28.3726858260007,6.23979001195009));
#53814=CARTESIAN_POINT('Ctrl Pts',(57.3897809176813,28.451797244378,6.24400895771777));
#53815=CARTESIAN_POINT('Ctrl Pts',(57.4053396763186,28.5317145192005,6.24822790348545));
#53816=CARTESIAN_POINT('Ctrl Pts',(57.4208933509156,28.6116056799446,6.25244547065406));
#53817=CARTESIAN_POINT('Ctrl Pts',(57.4324681666575,28.6923017185284,6.25666303782267));
#53818=CARTESIAN_POINT('Ctrl Pts',(57.4399981075099,28.7733736878736,6.26088060499129));
#53819=CARTESIAN_POINT('Ctrl Pts',(57.4475278904343,28.8544439568688,6.26509808370343));
#53820=CARTESIAN_POINT('Ctrl Pts',(57.4510129253457,28.9358896782611,6.26931556241557));
#53821=CARTESIAN_POINT('Ctrl Pts',(57.4504390935952,29.0172771114578,6.27353304112771));
#53822=CARTESIAN_POINT('Ctrl Pts',(57.4498642601189,29.0988066209528,6.27775788220206));
#53823=CARTESIAN_POINT('Ctrl Pts',(57.4452163859456,29.1802771715604,6.28198272327642));
#53824=CARTESIAN_POINT('Ctrl Pts',(57.4365336294594,29.2612548995014,6.28620756435077));
#53825=CARTESIAN_POINT('Ctrl Pts',(57.4278534598131,29.3422085018761,6.29043114672491));
#53826=CARTESIAN_POINT('Ctrl Pts',(57.4151409058698,29.4226691180841,6.29465472909906));
#53827=CARTESIAN_POINT('Ctrl Pts',(57.3984855618914,29.5022123648403,6.2988783114732));
#53828=CARTESIAN_POINT('Ctrl Pts',(57.3817999973935,29.5818999399418,6.30310955738485));
#53829=CARTESIAN_POINT('Ctrl Pts',(57.3611574638559,29.6606663683786,6.3073408032965));
#53830=CARTESIAN_POINT('Ctrl Pts',(57.3366979597814,29.7381008703108,6.31157204920816));
#53831=CARTESIAN_POINT('Ctrl Pts',(57.3123052282629,29.8153239820362,6.31579174414543));
#53832=CARTESIAN_POINT('Ctrl Pts',(57.284116575546,29.8912220316634,6.3200114390827));
#53833=CARTESIAN_POINT('Ctrl Pts',(57.252317547349,29.9654097140095,6.32423113401997));
#53834=CARTESIAN_POINT('Ctrl Pts',(57.2204209466352,30.0398250347235,6.32846377671943));
#53835=CARTESIAN_POINT('Ctrl Pts',(57.1847731140317,30.1127962601899,6.3326964194189));
#53836=CARTESIAN_POINT('Ctrl Pts',(57.1455266185094,30.1839196675737,6.33692906211837));
#53837=CARTESIAN_POINT('Ctrl Pts',(57.1063361015515,30.2549416293075,6.34115566766065));
#53838=CARTESIAN_POINT('Ctrl Pts',(57.063557338833,30.3241206042606,6.34538227320293));
#53839=CARTESIAN_POINT('Ctrl Pts',(57.0173907381963,30.3910732760857,6.34960887874521));
#53840=CARTESIAN_POINT('Ctrl Pts',(56.9712757696119,30.45795106902,6.35383075731355));
#53841=CARTESIAN_POINT('Ctrl Pts',(56.9217807544136,30.5226071259286,6.3580526358819));
#53842=CARTESIAN_POINT('Ctrl Pts',(56.8691510261793,30.5846844137975,6.36227451445024));
#53843=CARTESIAN_POINT('Ctrl Pts',(56.8165563413487,30.6467203676233,6.36649358188883));
#53844=CARTESIAN_POINT('Ctrl Pts',(56.7608313881616,30.7061806089203,6.37071264932742));
#53845=CARTESIAN_POINT('Ctrl Pts',(56.7022629062671,30.7627396994302,6.374931716766));
#53846=CARTESIAN_POINT('Ctrl Pts',(56.6437135491964,30.8192803212584,6.37914940651954));
#53847=CARTESIAN_POINT('Ctrl Pts',(56.5823228413088,30.8729213512001,6.38336709627308));
#53848=CARTESIAN_POINT('Ctrl Pts',(56.5184146778387,30.9233738888017,6.38758478602662));
#53849=CARTESIAN_POINT('Ctrl Pts',(56.4545078433777,30.973825377212,6.39180238807073));
#53850=CARTESIAN_POINT('Ctrl Pts',(56.388084022765,31.0210882181935,6.39601999011485));
#53851=CARTESIAN_POINT('Ctrl Pts',(56.3194993840789,31.0649144353739,6.40023759215896));
#53852=CARTESIAN_POINT('Ctrl Pts',(56.2507993594464,31.1088143852391,6.4044622898445));
#53853=CARTESIAN_POINT('Ctrl Pts',(56.1799316369248,31.1492658922123,6.40868698753004));
#53854=CARTESIAN_POINT('Ctrl Pts',(56.1072808730711,31.1860648019057,6.41291168521558));
#53855=CARTESIAN_POINT('Ctrl Pts',(56.0346471581031,31.2228550760339,6.41713539149533));
#53856=CARTESIAN_POINT('Ctrl Pts',(55.9602316729672,31.2559942966441,6.42135909777508));
#53857=CARTESIAN_POINT('Ctrl Pts',(55.884439195495,31.2853265761095,6.42558280405483));
#53858=CARTESIAN_POINT('Ctrl Pts',(55.8085092107296,31.314712071969,6.42981417323778));
#53859=CARTESIAN_POINT('Ctrl Pts',(55.7311976833491,31.340276677446,6.43404554242073));
#53860=CARTESIAN_POINT('Ctrl Pts',(55.6529254204302,31.3619141909384,6.43827691160367));
#53861=CARTESIAN_POINT('Ctrl Pts',(55.5748816383604,31.3834885433917,6.44249592919759));
#53862=CARTESIAN_POINT('Ctrl Pts',(55.4958831844018,31.4011586816502,6.44671494679151));
#53863=CARTESIAN_POINT('Ctrl Pts',(55.4163540516912,31.4148705045282,6.45093396438542));
#53864=CARTESIAN_POINT('Ctrl Pts',(55.3365684865941,31.4286265395754,6.45516658570811));
#53865=CARTESIAN_POINT('Ctrl Pts',(55.2559520888206,31.4384498229009,6.45939920703079));
#53866=CARTESIAN_POINT('Ctrl Pts',(55.1749265656419,31.4442485443655,6.46363182835347));
#53867=CARTESIAN_POINT('Ctrl Pts',(55.0940166135156,31.4500389948024,6.4678584124612));
#53868=CARTESIAN_POINT('Ctrl Pts',(55.0126991545164,31.4518162517646,6.47208499656892));
#53869=CARTESIAN_POINT('Ctrl Pts',(54.9314048223081,31.4495397428083,6.47631158067665));
#53870=CARTESIAN_POINT('Ctrl Pts',(54.8502008937526,31.447265765452,6.48053346459641));
#53871=CARTESIAN_POINT('Ctrl Pts',(54.7690205029077,31.4409469926296,6.48475534851617));
#53872=CARTESIAN_POINT('Ctrl Pts',(54.6882967024528,31.430594845773,6.48897723243593));
#53873=CARTESIAN_POINT('Ctrl Pts',(54.6076271634176,31.420249657486,6.49319627846385));
#53874=CARTESIAN_POINT('Ctrl Pts',(54.5274140648117,31.4058765386067,6.49741532449176));
#53875=CARTESIAN_POINT('Ctrl Pts',(54.4480864902674,31.387538843197,6.50163437051967));
#53876=CARTESIAN_POINT('Ctrl Pts',(54.3687848182123,31.3692071355156,6.50585203892077));
#53877=CARTESIAN_POINT('Ctrl Pts',(54.2903685482559,31.3469135267206,6.51006970732187));
#53878=CARTESIAN_POINT('Ctrl Pts',(54.2132563428266,31.3207724291489,6.51428737572297));
#53879=CARTESIAN_POINT('Ctrl Pts',(54.1361457393862,31.2946318746526,6.51850495650295));
#53880=CARTESIAN_POINT('Ctrl Pts',(54.060339586184,31.2646441405596,6.52272253728292));
#53881=CARTESIAN_POINT('Ctrl Pts',(53.9862397868842,31.2309729895952,6.5269401180629));
#53882=CARTESIAN_POINT('Ctrl Pts',(53.9120145030126,31.1972448180991,6.53116484112023));
#53883=CARTESIAN_POINT('Ctrl Pts',(53.8395017796366,31.1598209428222,6.53538956417756));
#53884=CARTESIAN_POINT('Ctrl Pts',(53.7690822829628,31.1189128872806,6.5396142872349));
#53885=CARTESIAN_POINT('Ctrl Pts',(53.698680081529,31.0780148788804,6.54383797268755));
#53886=CARTESIAN_POINT('Ctrl Pts',(53.6303704580546,31.0336346732078,6.54806165814021));
#53887=CARTESIAN_POINT('Ctrl Pts',(53.5645045325747,30.9860269416605,6.55228534359286));
#53888=CARTESIAN_POINT('Ctrl Pts',(53.4985191018522,30.9383328320131,6.55651669237904));
#53889=CARTESIAN_POINT('Ctrl Pts',(53.4349865933773,30.8873997850312,6.56074804116522));
#53890=CARTESIAN_POINT('Ctrl Pts',(53.3742251754706,30.8335229668391,6.56497938995139));
#53891=CARTESIAN_POINT('Ctrl Pts',(53.3136391463264,30.7798016649071,6.56919852488455));
#53892=CARTESIAN_POINT('Ctrl Pts',(53.2558084985499,30.7231539414781,6.57341765981771));
#53893=CARTESIAN_POINT('Ctrl Pts',(53.2010094579426,30.6639060308768,6.57763679475087));
#53894=CARTESIAN_POINT('Ctrl Pts',(53.1466819577936,30.6051679428309,6.58181962443494));
#53895=CARTESIAN_POINT('Ctrl Pts',(53.0951215203334,30.5436441968321,6.586002454119));
#53896=CARTESIAN_POINT('Ctrl Pts',(53.0466317199121,30.4796292144812,6.59018528380306));
#53897=CARTESIAN_POINT('Ctrl Pts',(52.9982051281647,30.4156976785894,6.5943626609772));
#53898=CARTESIAN_POINT('Ctrl Pts',(52.9528415189243,30.3492817231138,6.59854003815135));
#53899=CARTESIAN_POINT('Ctrl Pts',(52.9108068780089,30.2807116572536,6.6027174153255));
#53900=CARTESIAN_POINT('Ctrl Pts',(52.8688134471183,30.2122088162835,6.60689069707232));
#53901=CARTESIAN_POINT('Ctrl Pts',(52.8301427563659,30.1415564588635,6.61106397881914));
#53902=CARTESIAN_POINT('Ctrl Pts',(52.7950188390088,30.0691156764701,6.61523726056597));
#53903=CARTESIAN_POINT('Ctrl Pts',(52.7599180112606,29.9967225148847,6.61940779889889));
#53904=CARTESIAN_POINT('Ctrl Pts',(52.7283595353419,29.9225436897306,6.62357833723182));
#53905=CARTESIAN_POINT('Ctrl Pts',(52.7005218406598,29.8469654330122,6.62774887556475));
#53906=CARTESIAN_POINT('Ctrl Pts',(52.6726854079696,29.7713906025524,6.63191922483083));
#53907=CARTESIAN_POINT('Ctrl Pts',(52.6485696008035,29.6944169078521,6.63608957409691));
#53908=CARTESIAN_POINT('Ctrl Pts',(52.6283044779146,29.616449998394,6.64025992336299));
#53909=CARTESIAN_POINT('Ctrl Pts',(52.6080403381833,29.5384868714822,6.64443007030555));
#53910=CARTESIAN_POINT('Ctrl Pts',(52.5916266234608,29.4595310888085,6.64860021724811));
#53911=CARTESIAN_POINT('Ctrl Pts',(52.5791428075995,29.3800009263184,6.65277036419067));
#53912=CARTESIAN_POINT('Ctrl Pts',(52.5666493497683,29.300409338104,6.65694373197786));
#53913=CARTESIAN_POINT('Ctrl Pts',(52.5580919153856,29.2202429568221,6.66111709976505));
#53914=CARTESIAN_POINT('Ctrl Pts',(52.5534982586824,29.1399266941298,6.66529046755224));
#53915=CARTESIAN_POINT('Ctrl Pts',(52.5507897714393,29.0925710498201,6.66775114629748));
#53916=CARTESIAN_POINT('Ctrl Pts',(52.5494582852881,29.0451633717764,6.67021182504271));
#53917=CARTESIAN_POINT('Ctrl Pts',(52.5495009959572,28.9977906594942,6.67267250378794));
#53918=CARTESIAN_POINT('',(52.5495001736462,29.000922518181,7.4726725038354));
#53919=CARTESIAN_POINT('Ctrl Pts',(52.5495009959581,28.9977906585885,6.67267250383499));
#53920=CARTESIAN_POINT('Ctrl Pts',(52.5495959625876,28.8924580785088,6.67814378948657));
#53921=CARTESIAN_POINT('Ctrl Pts',(52.5564861340281,28.7874253985664,6.68361507513816));
#53922=CARTESIAN_POINT('Ctrl Pts',(52.5700336860443,28.6834341094806,6.68908636078975));
#53923=CARTESIAN_POINT('Ctrl Pts',(52.5826233164065,28.5867958467944,6.69417078223194));
#53924=CARTESIAN_POINT('Ctrl Pts',(52.6009615687309,28.4910563695803,6.69925520367413));
#53925=CARTESIAN_POINT('Ctrl Pts',(52.6249018375165,28.3967927648248,6.70433962511632));
#53926=CARTESIAN_POINT('Ctrl Pts',(52.6448313475172,28.318321321146,6.70857224375928));
#53927=CARTESIAN_POINT('Ctrl Pts',(52.6686910508689,28.2406926949251,6.71280486240224));
#53928=CARTESIAN_POINT('Ctrl Pts',(52.6963930578618,28.1643294272666,6.7170374810452));
#53929=CARTESIAN_POINT('Ctrl Pts',(52.7240555509065,28.0880750836366,6.72126406231066));
#53930=CARTESIAN_POINT('Ctrl Pts',(52.7555493052408,28.0130829468798,6.72549064357613));
#53931=CARTESIAN_POINT('Ctrl Pts',(52.7907359996734,27.9397628440482,6.7297172248416));
#53932=CARTESIAN_POINT('Ctrl Pts',(52.8258835939987,27.8665242158742,6.7339391094516));
#53933=CARTESIAN_POINT('Ctrl Pts',(52.8647157744081,27.7949543464672,6.73816099406161));
#53934=CARTESIAN_POINT('Ctrl Pts',(52.9070457472336,27.7254440985868,6.74238287867162));
#53935=CARTESIAN_POINT('Ctrl Pts',(52.949347227252,27.6559806388794,6.74660192148098));
#53936=CARTESIAN_POINT('Ctrl Pts',(52.9951415827039,27.588574443057,6.75082096429035));
#53937=CARTESIAN_POINT('Ctrl Pts',(53.0441962059324,27.5235915981305,6.75504000709972));
#53938=CARTESIAN_POINT('Ctrl Pts',(53.0932348099817,27.4586299738713,6.75925767214694));
#53939=CARTESIAN_POINT('Ctrl Pts',(53.1455312877731,27.3960904993885,6.76347533719416));
#53940=CARTESIAN_POINT('Ctrl Pts',(53.2008106434059,27.3363089502199,6.76769300224139));
#53941=CARTESIAN_POINT('Ctrl Pts',(53.2560888489012,27.2765286448609,6.77191057953624));
#53942=CARTESIAN_POINT('Ctrl Pts',(53.3143494925917,27.2195064910066,6.7761281568311));
#53943=CARTESIAN_POINT('Ctrl Pts',(53.3752793311667,27.165542860063,6.78034573412596));
#53944=CARTESIAN_POINT('Ctrl Pts',(53.4363124558048,27.11148775192,6.78457046090561));
#53945=CARTESIAN_POINT('Ctrl Pts',(53.5000234786206,27.0605018496433,6.78879518768526));
#53946=CARTESIAN_POINT('Ctrl Pts',(53.5660641828255,27.0128466787326,6.79301991446491));
#53947=CARTESIAN_POINT('Ctrl Pts',(53.6320885500798,26.9652032966146,6.79724359614437));
#53948=CARTESIAN_POINT('Ctrl Pts',(53.7004410435558,26.9208892339441,6.80146727782383));
#53949=CARTESIAN_POINT('Ctrl Pts',(53.7707460734318,26.8801214577206,6.80569095950329));
#53950=CARTESIAN_POINT('Ctrl Pts',(53.8411786604362,26.8392797149477,6.8099223043714));
#53951=CARTESIAN_POINT('Ctrl Pts',(53.9135704493358,26.8019973303931,6.81415364923951));
#53952=CARTESIAN_POINT('Ctrl Pts',(53.9875222855814,26.7684446841259,6.81838499410761));
#53953=CARTESIAN_POINT('Ctrl Pts',(54.0612610565873,26.7349887075696,6.822604147899));
#53954=CARTESIAN_POINT('Ctrl Pts',(54.1365504435938,26.7052410961928,6.82682330169039));
#53955=CARTESIAN_POINT('Ctrl Pts',(54.2129799915444,26.6793212724958,6.83104245548178));
#53956=CARTESIAN_POINT('Ctrl Pts',(54.289653381695,26.6533187537286,6.83527507013706));
#53957=CARTESIAN_POINT('Ctrl Pts',(54.3677593952038,26.6310718024977,6.83950768479234));
#53958=CARTESIAN_POINT('Ctrl Pts',(54.4468957476006,26.6127367267145,6.84374029944763));
#53959=CARTESIAN_POINT('Ctrl Pts',(54.5259192198373,26.594427804099,6.84796687669778));
#53960=CARTESIAN_POINT('Ctrl Pts',(54.6059696631954,26.5800197785084,6.85219345394793));
#53961=CARTESIAN_POINT('Ctrl Pts',(54.6866280030571,26.5696197331422,6.85642003119808));
#53962=CARTESIAN_POINT('Ctrl Pts',(54.7671968095085,26.5592312321683,6.86064191680846));
#53963=CARTESIAN_POINT('Ctrl Pts',(54.8483717132538,26.5528419303845,6.86486380241884));
#53964=CARTESIAN_POINT('Ctrl Pts',(54.9297231573378,26.5505079270621,6.86908568802922));
#53965=CARTESIAN_POINT('Ctrl Pts',(55.0110197454567,26.548175497578,6.87330472678652));
#53966=CARTESIAN_POINT('Ctrl Pts',(55.092492174327,26.5498929488533,6.87752376554382));
#53967=CARTESIAN_POINT('Ctrl Pts',(55.1737067298302,26.5556644620651,6.88174280430112));
#53968=CARTESIAN_POINT('Ctrl Pts',(55.2548947639566,26.5614340905349,6.88596046529164));
#53969=CARTESIAN_POINT('Ctrl Pts',(55.3358246289293,26.5712551188676,6.89017812628216));
#53970=CARTESIAN_POINT('Ctrl Pts',(55.4160649604304,26.5850796703199,6.89439578727268));
#53971=CARTESIAN_POINT('Ctrl Pts',(55.4963036224758,26.5989039341429,6.89861336051184));
#53972=CARTESIAN_POINT('Ctrl Pts',(55.5758523219702,26.6167314754395,6.902830933751));
#53973=CARTESIAN_POINT('Ctrl Pts',(55.6542885705336,26.6384630605326,6.90704850699016));
#53974=CARTESIAN_POINT('Ctrl Pts',(55.7328579460629,26.6602315298475,6.91127323856158));
#53975=CARTESIAN_POINT('Ctrl Pts',(55.8103106429316,26.6859171757245,6.915497970133));
#53976=CARTESIAN_POINT('Ctrl Pts',(55.8862377155446,26.7153702791161,6.91972270170442));
#53977=CARTESIAN_POINT('Ctrl Pts',(55.9621458473569,26.7448160351235,6.92394637937246));
#53978=CARTESIAN_POINT('Ctrl Pts',(56.0365286989947,26.7780271597654,6.9281700570405));
#53979=CARTESIAN_POINT('Ctrl Pts',(56.1089998023546,26.814806716014,6.93239373470853));
#53980=CARTESIAN_POINT('Ctrl Pts',(56.1816023939653,26.851653003405,6.93662507562389));
#53981=CARTESIAN_POINT('Ctrl Pts',(56.252285901021,26.8920804299587,6.94085641653923));
#53982=CARTESIAN_POINT('Ctrl Pts',(56.3206901050759,26.9358469300087,6.94508775745459));
#53983=CARTESIAN_POINT('Ctrl Pts',(56.3888976522279,26.9794876046877,6.94930693358547));
#53984=CARTESIAN_POINT('Ctrl Pts',(56.4548386619489,27.0264478475014,6.95352610971635));
#53985=CARTESIAN_POINT('Ctrl Pts',(56.5181895023843,27.0764483669914,6.95774528584723));
#53986=CARTESIAN_POINT('Ctrl Pts',(56.5817420932002,27.1266081207356,6.9619778985858));
#53987=CARTESIAN_POINT('Ctrl Pts',(56.6429243445553,27.1800141267647,6.96621051132437));
#53988=CARTESIAN_POINT('Ctrl Pts',(56.7013861374598,27.2364140334933,6.97044312406294));
#53989=CARTESIAN_POINT('Ctrl Pts',(56.7597645397355,27.2927334906931,6.97466969935003));
#53990=CARTESIAN_POINT('Ctrl Pts',(56.8154298591745,27.3520380468987,6.97889627463712));
#53991=CARTESIAN_POINT('Ctrl Pts',(56.868064127092,27.4140344685107,6.98312284992422));
#53992=CARTESIAN_POINT('Ctrl Pts',(56.9206399996994,27.4759621079319,6.98734473601957));
#53993=CARTESIAN_POINT('Ctrl Pts',(56.9701912035291,27.5405753262528,6.99156662211492));
#53994=CARTESIAN_POINT('Ctrl Pts',(57.0164368293783,27.6075443406963,6.99578850821027));
#53995=CARTESIAN_POINT('Ctrl Pts',(57.0626512435225,27.6744681569815,7.00000754490613));
#53996=CARTESIAN_POINT('Ctrl Pts',(57.1055642473226,27.7437442303109,7.00422658160198));
#53997=CARTESIAN_POINT('Ctrl Pts',(57.1449362190998,27.8150110270581,7.00844561829784));
#53998=CARTESIAN_POINT('Ctrl Pts',(57.1842953332791,27.886254550401,7.01266327719433));
#53999=CARTESIAN_POINT('Ctrl Pts',(57.2201154874759,27.9594870997823,7.01688093609082));
#54000=CARTESIAN_POINT('Ctrl Pts',(57.2522020067175,28.0343207722346,7.02109859498731));
#54001=CARTESIAN_POINT('Ctrl Pts',(57.2842878581498,28.1091528871909,7.02531616610263));
#54002=CARTESIAN_POINT('Ctrl Pts',(57.3126400471418,28.1855856315427,7.02953373721796));
#54003=CARTESIAN_POINT('Ctrl Pts',(57.3371118102645,28.2632105888913,7.03375130833328));
#54004=CARTESIAN_POINT('Ctrl Pts',(57.3616251347899,28.3409673799001,7.03797604232323));
#54005=CARTESIAN_POINT('Ctrl Pts',(57.3822447073948,28.4199199896435,7.04220077631318));
#54006=CARTESIAN_POINT('Ctrl Pts',(57.398873485459,28.4996438760623,7.04642551030313));
#54007=CARTESIAN_POINT('Ctrl Pts',(57.4154980972208,28.5793477878437,7.05064918579564));
#54008=CARTESIAN_POINT('Ctrl Pts',(57.4281338626529,28.6598221260562,7.05487286128815));
#54009=CARTESIAN_POINT('Ctrl Pts',(57.4367355838727,28.7406354991745,7.05909653678066));
#54010=CARTESIAN_POINT('Ctrl Pts',(57.4453529116408,28.8215954961812,7.06332787550637));
#54011=CARTESIAN_POINT('Ctrl Pts',(57.4499215419352,28.9028952922429,7.06755921423208));
#54012=CARTESIAN_POINT('Ctrl Pts',(57.4504484222488,28.9841009466281,7.07179055295779));
#54013=CARTESIAN_POINT('Ctrl Pts',(57.4509737895403,29.0650734058319,7.07600974070942));
#54014=CARTESIAN_POINT('Ctrl Pts',(57.4474806916846,29.1459518120799,7.08022892846104));
#54015=CARTESIAN_POINT('Ctrl Pts',(57.4400272205332,29.2263126444922,7.08444811621268));
#54016=CARTESIAN_POINT('Ctrl Pts',(57.4325500295491,29.3069292162051,7.08868073105426));
#54017=CARTESIAN_POINT('Ctrl Pts',(57.4210593812124,29.3873247478163,7.09291334589584));
#54018=CARTESIAN_POINT('Ctrl Pts',(57.4055763497897,29.4670681698986,7.09714596073742));
#54019=CARTESIAN_POINT('Ctrl Pts',(57.3901154034242,29.5466978456486,7.10137253816046));
#54020=CARTESIAN_POINT('Ctrl Pts',(57.3706734722897,29.6256768070676,7.10559911558351));
#54021=CARTESIAN_POINT('Ctrl Pts',(57.3473234261653,29.7035786970735,7.10982569300656));
#54022=CARTESIAN_POINT('Ctrl Pts',(57.3239993005622,29.7813941094085,7.11404757857204));
#54023=CARTESIAN_POINT('Ctrl Pts',(57.2967758129541,29.858134383322,7.11826946413752));
#54024=CARTESIAN_POINT('Ctrl Pts',(57.2657766664408,29.9333843516004,7.122491349703));
#54025=CARTESIAN_POINT('Ctrl Pts',(57.2347984215653,30.0085835814629,7.12671038859903));
#54026=CARTESIAN_POINT('Ctrl Pts',(57.2000497504312,30.0822940730062,7.13092942749507));
#54027=CARTESIAN_POINT('Ctrl Pts',(57.1617034667217,30.1541180060824,7.1351484663911));
#54028=CARTESIAN_POINT('Ctrl Pts',(57.1233697054719,30.2259184841526,7.13936612750708));
#54029=CARTESIAN_POINT('Ctrl Pts',(57.0814408834396,30.2958332177653,7.14358378862307));
#54030=CARTESIAN_POINT('Ctrl Pts',(57.0361364025847,30.3634877337436,7.14780144973905));
#54031=CARTESIAN_POINT('Ctrl Pts',(56.990832864466,30.4311408419062,7.15201902309015));
#54032=CARTESIAN_POINT('Ctrl Pts',(56.9421540666431,30.4965334406053,7.15623659644126));
#54033=CARTESIAN_POINT('Ctrl Pts',(56.8903627013274,30.5593200785695,7.16045416979237));
#54034=CARTESIAN_POINT('Ctrl Pts',(56.838483435925,30.6222132777509,7.16467890119119));
#54035=CARTESIAN_POINT('Ctrl Pts',(56.7834813308738,30.6824913069132,7.16890363259));
#54036=CARTESIAN_POINT('Ctrl Pts',(56.7256596719692,30.7398416440985,7.17312836398881));
#54037=CARTESIAN_POINT('Ctrl Pts',(56.667852433859,30.7971776780375,7.1773520417343));
#54038=CARTESIAN_POINT('Ctrl Pts',(56.6072274092363,30.8515871846148,7.18157571947978));
#54039=CARTESIAN_POINT('Ctrl Pts',(56.5441218547341,30.9027974006007,7.18579939722527));
#54040=CARTESIAN_POINT('Ctrl Pts',(56.480901804728,30.954100529794,7.19003073819652));
#54041=CARTESIAN_POINT('Ctrl Pts',(56.4151926066136,31.0021924928793,7.19426207916778));
#54042=CARTESIAN_POINT('Ctrl Pts',(56.3473620433452,31.0468428796937,7.19849342013903));
#54043=CARTESIAN_POINT('Ctrl Pts',(56.2797264991382,31.09136489257,7.20271259561873));
#54044=CARTESIAN_POINT('Ctrl Pts',(56.2099822061629,31.1324649329676,7.20693177109843));
#54045=CARTESIAN_POINT('Ctrl Pts',(56.1385160459505,31.1699611662685,7.21115094657812));
#54046=CARTESIAN_POINT('Ctrl Pts',(56.0668222555387,31.2075768305705,7.21538356075038));
#54047=CARTESIAN_POINT('Ctrl Pts',(55.993128950007,31.2417055725833,7.21961617492265));
#54048=CARTESIAN_POINT('Ctrl Pts',(55.9178091939508,31.2721303953558,7.22384878909491));
#54049=CARTESIAN_POINT('Ctrl Pts',(55.8425968744201,31.3025118199891,7.22807536584239));
#54050=CARTESIAN_POINT('Ctrl Pts',(55.7657631392959,31.3291996461331,7.23230194258988));
#54051=CARTESIAN_POINT('Ctrl Pts',(55.6877052978712,31.3520228896165,7.23652851933737));
#54052=CARTESIAN_POINT('Ctrl Pts',(55.6097340916694,31.3748208019255,7.24075040507096));
#54053=CARTESIAN_POINT('Ctrl Pts',(55.5305419223693,31.393762524576,7.24497229080455));
#54054=CARTESIAN_POINT('Ctrl Pts',(55.4505443868852,31.4087258053681,7.24919417653814));
#54055=CARTESIAN_POINT('Ctrl Pts',(55.3706008071098,31.4236789939191,7.25341321474855));
#54056=CARTESIAN_POINT('Ctrl Pts',(55.2898533954299,31.4346589847455,7.25763225295896));
#54057=CARTESIAN_POINT('Ctrl Pts',(55.2087299332046,31.4415941646769,7.26185129116937));
#54058=CARTESIAN_POINT('Ctrl Pts',(55.1276329629106,31.4485270798344,7.26606895159749));
#54059=CARTESIAN_POINT('Ctrl Pts',(55.0461606484581,31.4514177677565,7.2702866120256));
#54060=CARTESIAN_POINT('Ctrl Pts',(54.9647465498802,31.4502464048039,7.27450427245371));
#54061=CARTESIAN_POINT('Ctrl Pts',(54.883334145465,31.4490750662265,7.27872184511566));
#54062=CARTESIAN_POINT('Ctrl Pts',(54.8019804189986,31.4438418526952,7.28293941777761));
#54063=CARTESIAN_POINT('Ctrl Pts',(54.7211181534601,31.4345790530748,7.28715699043955));
#54064=CARTESIAN_POINT('Ctrl Pts',(54.640118620063,31.4253005293751,7.29138172264822));
#54065=CARTESIAN_POINT('Ctrl Pts',(54.5596126807539,31.4119787866303,7.29560645485689));
#54066=CARTESIAN_POINT('Ctrl Pts',(54.4800275962078,31.394698091471,7.29983118706556));
#54067=CARTESIAN_POINT('Ctrl Pts',(54.400462388443,31.3774217122534,7.30405486412579));
#54068=CARTESIAN_POINT('Ctrl Pts',(54.3218180200224,31.3561884999339,7.30827854118603));
#54069=CARTESIAN_POINT('Ctrl Pts',(54.2445068942906,31.3311328613414,7.31250221824626));
#54070=CARTESIAN_POINT('Ctrl Pts',(54.1670554990246,31.3060317630207,7.31673355854006));
#54071=CARTESIAN_POINT('Ctrl Pts',(54.0909426161636,31.2770945441863,7.32096489883387));
#54072=CARTESIAN_POINT('Ctrl Pts',(54.0165617407828,31.2445042749587,7.32519623912767));
#54073=CARTESIAN_POINT('Ctrl Pts',(53.9423946386715,31.2120076713187,7.32941541839964));
#54074=CARTESIAN_POINT('Ctrl Pts',(53.8699499719123,31.1758792648432,7.33363459767161));
#54075=CARTESIAN_POINT('Ctrl Pts',(53.7995908876004,31.1363445913213,7.33785377694359));
#54076=CARTESIAN_POINT('Ctrl Pts',(53.729007765659,31.096684031361,7.34208639094018));
#54077=CARTESIAN_POINT('Ctrl Pts',(53.6602610241045,31.0534479446395,7.34631900493677));
#54078=CARTESIAN_POINT('Ctrl Pts',(53.593735782111,31.0068311337741,7.35055161893336));
#54079=CARTESIAN_POINT('Ctrl Pts',(53.5273054321829,30.9602808174503,7.35477819550006));
#54080=CARTESIAN_POINT('Ctrl Pts',(53.4630906655255,30.9103596190429,7.35900477206677));
#54081=CARTESIAN_POINT('Ctrl Pts',(53.4014512034721,30.8573077276314,7.36323134863347));
#54082=CARTESIAN_POINT('Ctrl Pts',(53.3398801508463,30.8043147148895,7.36745323441162));
#54083=CARTESIAN_POINT('Ctrl Pts',(53.2808790739997,30.7481982145639,7.37167512018977));
#54084=CARTESIAN_POINT('Ctrl Pts',(53.2247767725121,30.6892402856277,7.37589700596792));
#54085=CARTESIAN_POINT('Ctrl Pts',(53.1687123133251,30.6303221251788,7.38011604398642));
#54086=CARTESIAN_POINT('Ctrl Pts',(53.115543065524,30.5685666783409,7.38433508200491));
#54087=CARTESIAN_POINT('Ctrl Pts',(53.0655619845638,30.5042937925935,7.38855412002341));
#54088=CARTESIAN_POINT('Ctrl Pts',(53.0155972256271,30.4400418960589,7.39277178025584));
#54089=CARTESIAN_POINT('Ctrl Pts',(52.9688188508445,30.3732745597009,7.39698944048826));
#54090=CARTESIAN_POINT('Ctrl Pts',(52.9254795192243,30.3043446725625,7.40120710072068));
#54091=CARTESIAN_POINT('Ctrl Pts',(52.8821410894974,30.235416219858,7.40542467318341));
#54092=CARTESIAN_POINT('Ctrl Pts',(52.8422418069139,30.1643256997478,7.40964224564614));
#54093=CARTESIAN_POINT('Ctrl Pts',(52.8059901941722,30.0914537195554,7.41385981810887));
#54094=CARTESIAN_POINT('Ctrl Pts',(52.7696770388051,30.0184580280952,7.41808455054222));
#54095=CARTESIAN_POINT('Ctrl Pts',(52.7370241509763,29.9436752437499,7.42230928297556));
#54096=CARTESIAN_POINT('Ctrl Pts',(52.7081934468242,29.8675096384598,7.42653401540891));
#54097=CARTESIAN_POINT('Ctrl Pts',(52.6793699462255,29.7913630636794,7.43075769226328));
#54098=CARTESIAN_POINT('Ctrl Pts',(52.654366842397,29.7138348090581,7.43498136911765));
#54099=CARTESIAN_POINT('Ctrl Pts',(52.6332959042206,29.6353439800776,7.43920504597202));
#54100=CARTESIAN_POINT('Ctrl Pts',(52.6121867359721,29.5567107412045,7.44343638605756));
#54101=CARTESIAN_POINT('Ctrl Pts',(52.5950240892831,29.4771118931882,7.4476677261431));
#54102=CARTESIAN_POINT('Ctrl Pts',(52.581868619362,29.396977173114,7.45189906622864));
#54103=CARTESIAN_POINT('Ctrl Pts',(52.5687509546984,29.317072738522,7.45611824658877));
#54104=CARTESIAN_POINT('Ctrl Pts',(52.5596174351928,29.2366359693903,7.4603374269489));
#54105=CARTESIAN_POINT('Ctrl Pts',(52.5544765733145,29.1560942648932,7.46455660730903));
#54106=CARTESIAN_POINT('Ctrl Pts',(52.5511803009539,29.1044516803041,7.46726190613533));
#54107=CARTESIAN_POINT('Ctrl Pts',(52.549519667232,29.0527035916731,7.46996720496163));
#54108=CARTESIAN_POINT('Ctrl Pts',(52.5495001736465,29.0009225190894,7.47267250378794));
#54109=CARTESIAN_POINT('',(52.5495004479559,29.0014816989085,8.27267250375952));
#54110=CARTESIAN_POINT('Ctrl Pts',(52.5495001736462,29.000922518181,7.4726725038354));
#54111=CARTESIAN_POINT('Ctrl Pts',(52.5494699637188,28.9206754040258,7.47686500918346));
#54112=CARTESIAN_POINT('Ctrl Pts',(52.553385810479,28.8402695844599,7.48105751453152));
#54113=CARTESIAN_POINT('Ctrl Pts',(52.5612682705951,28.7601296141792,7.48525001987958));
#54114=CARTESIAN_POINT('Ctrl Pts',(52.569139928792,28.6800994656379,7.48943677992691));
#54115=CARTESIAN_POINT('Ctrl Pts',(52.5809673631317,28.6003349110385,7.49362353997424));
#54116=CARTESIAN_POINT('Ctrl Pts',(52.5967191103635,28.5212608063798,7.49781030002156));
#54117=CARTESIAN_POINT('Ctrl Pts',(52.6124543520702,28.4422695598069,7.50199267295727));
#54118=CARTESIAN_POINT('Ctrl Pts',(52.6321056463101,28.3639677887937,7.50617504589298));
#54119=CARTESIAN_POINT('Ctrl Pts',(52.6555898647205,28.2867739715918,7.51035741882869));
#54120=CARTESIAN_POINT('Ctrl Pts',(52.6790611159983,28.2096227780129,7.51453748240992));
#54121=CARTESIAN_POINT('Ctrl Pts',(52.7063609543197,28.1335787769367,7.51871754599115));
#54122=CARTESIAN_POINT('Ctrl Pts',(52.737355744061,28.0590477052122,7.52289760957238));
#54123=CARTESIAN_POINT('Ctrl Pts',(52.7683433358281,27.9845339419688,7.52707670241014));
#54124=CARTESIAN_POINT('Ctrl Pts',(52.803023993077,27.9115328479399,7.5312557952479));
#54125=CARTESIAN_POINT('Ctrl Pts',(52.8412156020801,27.8404310398696,7.53543488808566));
#54126=CARTESIAN_POINT('Ctrl Pts',(52.8794105604764,27.7693229961913,7.53961434742865));
#54127=CARTESIAN_POINT('Ctrl Pts',(52.9211168554604,27.7001149856384,7.54379380677165));
#54128=CARTESIAN_POINT('Ctrl Pts',(52.9661067479375,27.6331684488517,7.54797326611464));
#54129=CARTESIAN_POINT('Ctrl Pts',(53.0111431277268,27.5661527373152,7.55215704402388));
#54130=CARTESIAN_POINT('Ctrl Pts',(53.0594696106475,27.5014035566214,7.55634082193313));
#54131=CARTESIAN_POINT('Ctrl Pts',(53.1108159391139,27.4392521555056,7.56052459984237));
#54132=CARTESIAN_POINT('Ctrl Pts',(53.162192422478,27.3770642538416,7.5647108348191));
#54133=CARTESIAN_POINT('Ctrl Pts',(53.2165919598393,27.3174775163968,7.56889706979584));
#54134=CARTESIAN_POINT('Ctrl Pts',(53.2737066682083,27.260787079564,7.57308330477257));
#54135=CARTESIAN_POINT('Ctrl Pts',(53.3309146588018,27.2040040534455,7.57727637689024));
#54136=CARTESIAN_POINT('Ctrl Pts',(53.3908463167065,27.1501270827268,7.58146944900791));
#54137=CARTESIAN_POINT('Ctrl Pts',(53.4531603921842,27.0994112812888,7.58566252112559));
#54138=CARTESIAN_POINT('Ctrl Pts',(53.4808860207514,27.0768461150342,7.58752815997522));
#54139=CARTESIAN_POINT('Ctrl Pts',(53.5090829004989,27.0549061785739,7.58939379882486));
#54140=CARTESIAN_POINT('Ctrl Pts',(53.5377192653921,27.0336111007244,7.59125943767449));
#54141=CARTESIAN_POINT('Ctrl Pts',(53.6026871897314,26.985298508966,7.59549205183763));
#54142=CARTESIAN_POINT('Ctrl Pts',(53.6701728177024,26.9401192630011,7.59972466600077));
#54143=CARTESIAN_POINT('Ctrl Pts',(53.7398413913357,26.8983457632119,7.60395728016392));
#54144=CARTESIAN_POINT('Ctrl Pts',(53.8094105892923,26.8566318493967,7.6081838569005));
#54145=CARTESIAN_POINT('Ctrl Pts',(53.8811561534627,26.8183142700959,7.61241043363708));
#54146=CARTESIAN_POINT('Ctrl Pts',(53.9547122171902,26.7836237455909,7.61663701037366));
#54147=CARTESIAN_POINT('Ctrl Pts',(54.0281866423831,26.7489717234668,7.62085889610975));
#54148=CARTESIAN_POINT('Ctrl Pts',(54.1034671563318,26.7179389544352,7.62508078184585));
#54149=CARTESIAN_POINT('Ctrl Pts',(54.1801622451278,26.6907108657238,7.62930266758195));
#54150=CARTESIAN_POINT('Ctrl Pts',(54.2568056052848,26.6635011415778,7.63352170577713));
#54151=CARTESIAN_POINT('Ctrl Pts',(54.3348612087337,26.6400911561762,7.63774074397231));
#54152=CARTESIAN_POINT('Ctrl Pts',(54.4139176264464,26.6206182102467,7.64195978216749));
#54153=CARTESIAN_POINT('Ctrl Pts',(54.4929482272182,26.6011516234706,7.64617744257876));
#54154=CARTESIAN_POINT('Ctrl Pts',(54.5729785424699,26.5856196338783,7.65039510299004));
#54155=CARTESIAN_POINT('Ctrl Pts',(54.6535833767961,26.5741092825174,7.65461276340132));
#54156=CARTESIAN_POINT('Ctrl Pts',(54.7341865337694,26.5625991706822,7.65883033604485));
#54157=CARTESIAN_POINT('Ctrl Pts',(54.8153637259979,26.5551105951925,7.66304790868838));
#54158=CARTESIAN_POINT('Ctrl Pts',(54.8966824173337,26.5516789983517,7.6672654813319));
#54159=CARTESIAN_POINT('Ctrl Pts',(54.978139152018,26.5482415761698,7.67149021355757));
#54160=CARTESIAN_POINT('Ctrl Pts',(55.0597373998212,26.5488749315336,7.67571494578324));
#54161=CARTESIAN_POINT('Ctrl Pts',(55.1410419922651,26.5535623027721,7.67993967800891));
#54162=CARTESIAN_POINT('Ctrl Pts',(55.2223262777186,26.5582485032722,7.684163355047));
#54163=CARTESIAN_POINT('Ctrl Pts',(55.3033165932996,26.5669866236706,7.68838703208508));
#54164=CARTESIAN_POINT('Ctrl Pts',(55.3835846454728,26.5797080610477,7.69261070912317));
#54165=CARTESIAN_POINT('Ctrl Pts',(55.4639983320443,26.5924525795739,7.69684204939274));
#54166=CARTESIAN_POINT('Ctrl Pts',(55.5436866803965,26.6091947624671,7.70107338966231));
#54167=CARTESIAN_POINT('Ctrl Pts',(55.6222325033254,26.6298149941818,7.70530472993188));
#54168=CARTESIAN_POINT('Ctrl Pts',(55.7005525850342,26.6503759632128,7.70952390930123));
#54169=CARTESIAN_POINT('Ctrl Pts',(55.7777362908384,26.6747925031437,7.71374308867058));
#54170=CARTESIAN_POINT('Ctrl Pts',(55.8533898045263,26.7028983279945,7.71796226803993));
#54171=CARTESIAN_POINT('Ctrl Pts',(55.9292842153978,26.7310936478828,7.7221948821908));
#54172=CARTESIAN_POINT('Ctrl Pts',(56.0039209366839,26.7631066770454,7.72642749634167));
#54173=CARTESIAN_POINT('Ctrl Pts',(56.0768892295648,26.7988049070454,7.73066011049255));
#54174=CARTESIAN_POINT('Ctrl Pts',(56.1497534400199,26.8344522168686,7.73488668721632));
#54175=CARTESIAN_POINT('Ctrl Pts',(56.2209535349518,26.8737740848049,7.73911326394009));
#54176=CARTESIAN_POINT('Ctrl Pts',(56.2900968022657,26.9165892169849,7.74333984066387));
#54177=CARTESIAN_POINT('Ctrl Pts',(56.359163328988,26.9593568295913,7.7475617264031));
#54178=CARTESIAN_POINT('Ctrl Pts',(56.4261771710985,27.0056097593228,7.75178361214233));
#54179=CARTESIAN_POINT('Ctrl Pts',(56.4907696470691,27.0551205411704,7.75600549788156));
#54180=CARTESIAN_POINT('Ctrl Pts',(56.5553185570041,27.1045979292139,7.76022453606275));
#54181=CARTESIAN_POINT('Ctrl Pts',(56.6174489766366,27.1573285233817,7.76444357424394));
#54182=CARTESIAN_POINT('Ctrl Pts',(56.6768217523575,27.2130419532567,7.76866261242513));
#54183=CARTESIAN_POINT('Ctrl Pts',(56.7361751390909,27.2687371891532,7.77288027282201));
#54184=CARTESIAN_POINT('Ctrl Pts',(56.792772331843,27.3274130086463,7.77709793321888));
#54185=CARTESIAN_POINT('Ctrl Pts',(56.846308841665,27.3887601323237,7.78131559361576));
#54186=CARTESIAN_POINT('Ctrl Pts',(56.8998442374095,27.4501059793872,7.78553316624449));
#54187=CARTESIAN_POINT('Ctrl Pts',(56.9503187722974,27.5141226693279,7.78975073887322));
#54188=CARTESIAN_POINT('Ctrl Pts',(56.9974672434017,27.5804666747353,7.79396831150194));
#54189=CARTESIAN_POINT('Ctrl Pts',(57.0446957522071,27.6469233035544,7.7981930437439));
#54190=CARTESIAN_POINT('Ctrl Pts',(57.0885866299451,27.7157147717585,7.80241777598585));
#54191=CARTESIAN_POINT('Ctrl Pts',(57.1289170306517,27.7864669239773,7.8066425082278));
#54192=CARTESIAN_POINT('Ctrl Pts',(57.1692373579566,27.857201404295,7.81086618525025));
#54193=CARTESIAN_POINT('Ctrl Pts',(57.2059987952204,27.9298951637249,7.8150898622727));
#54194=CARTESIAN_POINT('Ctrl Pts',(57.239025724956,28.0041515913629,7.81931353929515));
#54195=CARTESIAN_POINT('Ctrl Pts',(57.2721125771228,28.0785427461979,7.82354487954871));
#54196=CARTESIAN_POINT('Ctrl Pts',(57.3014512128808,28.1545018007412,7.82777621980226));
#54197=CARTESIAN_POINT('Ctrl Pts',(57.326914851716,28.2316136890446,7.83200756005582));
#54198=CARTESIAN_POINT('Ctrl Pts',(57.3523053084635,28.3085039590237,7.83622673950567));
#54199=CARTESIAN_POINT('Ctrl Pts',(57.3738429709623,28.3865399841882,7.84044591895553));
#54200=CARTESIAN_POINT('Ctrl Pts',(57.3914529302185,28.4653008953164,7.84466509840538));
#54201=CARTESIAN_POINT('Ctrl Pts',(57.4091189632073,28.5443125973866,7.84889771259049));
#54202=CARTESIAN_POINT('Ctrl Pts',(57.422897918044,28.6243476817022,7.85313032677559));
#54203=CARTESIAN_POINT('Ctrl Pts',(57.432677339609,28.7049894724712,7.8573629409607));
#54204=CARTESIAN_POINT('Ctrl Pts',(57.4424428117479,28.7855162353014,7.86158951771929));
#54205=CARTESIAN_POINT('Ctrl Pts',(57.4482200259361,28.8666475284319,7.86581609447789));
#54206=CARTESIAN_POINT('Ctrl Pts',(57.4499472632695,28.9479552385142,7.87004267123648));
#54207=CARTESIAN_POINT('Ctrl Pts',(57.4516725835626,29.0291727061224,7.87426455696708));
#54208=CARTESIAN_POINT('Ctrl Pts',(57.4493568487837,29.1105657395192,7.87848644269768));
#54209=CARTESIAN_POINT('Ctrl Pts',(57.4429901518053,29.191701247211,7.88270832842828));
#54210=CARTESIAN_POINT('Ctrl Pts',(57.4366277489401,29.2727820318571,7.88692736664547));
#54211=CARTESIAN_POINT('Ctrl Pts',(57.4262198465732,29.353605173836,7.89114640486267));
#54212=CARTESIAN_POINT('Ctrl Pts',(57.4118086027381,29.4337389926658,7.89536544307987));
#54213=CARTESIAN_POINT('Ctrl Pts',(57.3974020650894,29.5138466427139,7.89958310351311));
#54214=CARTESIAN_POINT('Ctrl Pts',(57.3789948644423,29.5932649598001,7.90380076394635));
#54215=CARTESIAN_POINT('Ctrl Pts',(57.356680668146,29.671570158946,7.90801842437959));
#54216=CARTESIAN_POINT('Ctrl Pts',(57.3343669361993,29.7498737285918,7.91223599704499));
#54217=CARTESIAN_POINT('Ctrl Pts',(57.3081464986954,29.8270637799121,7.9164535697104));
#54218=CARTESIAN_POINT('Ctrl Pts',(57.2781631384104,29.9027308373974,7.9206711423758));
#54219=CARTESIAN_POINT('Ctrl Pts',(57.2481288799168,29.9785263433832,7.92489587457538));
#54220=CARTESIAN_POINT('Ctrl Pts',(57.2143190902924,30.0527932486888,7.92912060677497));
#54221=CARTESIAN_POINT('Ctrl Pts',(57.1769263029716,30.1251409340302,7.93334533897456));
#54222=CARTESIAN_POINT('Ctrl Pts',(57.1395428546162,30.1974705503114,7.93756901603409));
#54223=CARTESIAN_POINT('Ctrl Pts',(57.0985784508561,30.2678815129337,7.94179269309362));
#54224=CARTESIAN_POINT('Ctrl Pts',(57.0542701726253,30.3360105942177,7.94601637015315));
#54225=CARTESIAN_POINT('Ctrl Pts',(57.0098815036429,30.404263285542,7.95024771044373));
#54226=CARTESIAN_POINT('Ctrl Pts',(56.9621371087501,30.4702254442061,7.95447905073432));
#54227=CARTESIAN_POINT('Ctrl Pts',(56.9113161363247,30.5335647612751,7.9587103910249));
#54228=CARTESIAN_POINT('Ctrl Pts',(56.8606412254153,30.5967220386029,7.96292957027355));
#54229=CARTESIAN_POINT('Ctrl Pts',(56.8069077621599,30.6572712452121,7.96714874952219));
#54230=CARTESIAN_POINT('Ctrl Pts',(56.7504280017128,30.7149204240488,7.97136792877084));
#54231=CARTESIAN_POINT('Ctrl Pts',(56.6937683956003,30.7727531722711,7.97560054294012));
#54232=CARTESIAN_POINT('Ctrl Pts',(56.6341342221795,30.8278824714284,7.97983315710941));
#54233=CARTESIAN_POINT('Ctrl Pts',(56.5718137789544,30.8799871526926,7.98406577127869));
#54234=CARTESIAN_POINT('Ctrl Pts',(56.5095822299898,30.9320175115214,7.98829234802129));
#54235=CARTESIAN_POINT('Ctrl Pts',(56.4446723749273,30.9810315257815,7.99251892476389));
#54236=CARTESIAN_POINT('Ctrl Pts',(56.3774097262184,31.0267443588472,7.99674550150648));
#54237=CARTESIAN_POINT('Ctrl Pts',(56.3102217312172,31.0724064559912,8.00096738724106));
#54238=CARTESIAN_POINT('Ctrl Pts',(56.2406865135504,31.1147743923521,8.00518927297563));
#54239=CARTESIAN_POINT('Ctrl Pts',(56.1691619678421,31.1536040822193,8.00941115871021));
#54240=CARTESIAN_POINT('Ctrl Pts',(56.0976856632683,31.1924075826396,8.01363019691104));
#54241=CARTESIAN_POINT('Ctrl Pts',(56.02422310268,31.2276773551747,8.01784923511188));
#54242=CARTESIAN_POINT('Ctrl Pts',(55.9491593414199,31.2592137558441,8.02206827331271));
#54243=CARTESIAN_POINT('Ctrl Pts',(55.8741200932473,31.2907398578749,8.0262859337295));
#54244=CARTESIAN_POINT('Ctrl Pts',(55.7974811107954,31.3185348294661,8.0305035941463));
#54245=CARTESIAN_POINT('Ctrl Pts',(55.7196488681722,31.3424465322689,8.03472125456309));
#54246=CARTESIAN_POINT('Ctrl Pts',(55.6418182452084,31.3663577374782,8.03893882721197));
#54247=CARTESIAN_POINT('Ctrl Pts',(55.5627948558531,31.3863856992659,8.04315639986085));
#54248=CARTESIAN_POINT('Ctrl Pts',(55.4830004539498,31.4024281074539,8.04737397250973));
#54249=CARTESIAN_POINT('Ctrl Pts',(55.4030705965005,31.4184977485442,8.05159870472861));
#54250=CARTESIAN_POINT('Ctrl Pts',(55.3223675656575,31.4305682073941,8.05582343694749));
#54251=CARTESIAN_POINT('Ctrl Pts',(55.2413238380958,31.4385883324511,8.06004816916637));
#54252=CARTESIAN_POINT('Ctrl Pts',(55.1603003521452,31.4466064543888,8.06427184620937));
#54253=CARTESIAN_POINT('Ctrl Pts',(55.0789368062758,31.4505762640251,8.06849552325237));
#54254=CARTESIAN_POINT('Ctrl Pts',(54.9976669520771,31.4504988893871,8.07271920029537));
#54255=CARTESIAN_POINT('Ctrl Pts',(54.9162496458658,31.4504213743644,8.07695054056955));
#54256=CARTESIAN_POINT('Ctrl Pts',(54.8349268363389,31.4462820239938,8.08118188084373));
#54257=CARTESIAN_POINT('Ctrl Pts',(54.7541292412137,31.438134085725,8.08541322111791));
#54258=CARTESIAN_POINT('Ctrl Pts',(54.6735638595754,31.4300095647516,8.08963240045737));
#54259=CARTESIAN_POINT('Ctrl Pts',(54.5935211151077,31.4178996169355,8.09385157979683));
#54260=CARTESIAN_POINT('Ctrl Pts',(54.5144159007389,31.4019072281303,8.09807075913629));
#54261=CARTESIAN_POINT('Ctrl Pts',(54.4350587973182,31.3858639159103,8.10230337330545));
#54262=CARTESIAN_POINT('Ctrl Pts',(54.3563500583321,31.3658537017414,8.10653598747461));
#54263=CARTESIAN_POINT('Ctrl Pts',(54.2787160376896,31.3419435722736,8.11076860164377));
#54264=CARTESIAN_POINT('Ctrl Pts',(54.2011927546892,31.3180675483609,8.11499517838617));
#54265=CARTESIAN_POINT('Ctrl Pts',(54.1247415856073,31.2903027933118,8.11922175512857));
#54266=CARTESIAN_POINT('Ctrl Pts',(54.0497786678322,31.2587672898936,8.12344833187097));
#54267=CARTESIAN_POINT('Ctrl Pts',(53.9748989501626,31.2272667872103,8.12767021760559));
#54268=CARTESIAN_POINT('Ctrl Pts',(53.9015046277485,31.1920040311541,8.13189210334021));
#54269=CARTESIAN_POINT('Ctrl Pts',(53.8299952839634,31.1531463523068,8.13611398907482));
#54270=CARTESIAN_POINT('Ctrl Pts',(53.7585341710649,31.114314881787,8.14033302727537));
#54271=CARTESIAN_POINT('Ctrl Pts',(53.6889559188865,31.0718935253044,8.14455206547593));
#54272=CARTESIAN_POINT('Ctrl Pts',(53.6216376182746,31.0260965906502,8.14877110367648));
#54273=CARTESIAN_POINT('Ctrl Pts',(53.5543413013658,30.9803146116055,8.15298876409294));
#54274=CARTESIAN_POINT('Ctrl Pts',(53.489303854164,30.9311595046703,8.15720642450941));
#54275=CARTESIAN_POINT('Ctrl Pts',(53.4268741789863,30.8788894063409,8.16142408492587));
#54276=CARTESIAN_POINT('Ctrl Pts',(53.3644458029471,30.8266203957329,8.16564165757438));
#54277=CARTESIAN_POINT('Ctrl Pts',(53.3046254464679,30.7712368217353,8.16985923022289));
#54278=CARTESIAN_POINT('Ctrl Pts',(53.2477285330397,30.7130367643681,8.1740768028714));
#54279=CARTESIAN_POINT('Ctrl Pts',(53.1907350338482,30.6547379090763,8.17830153509059));
#54280=CARTESIAN_POINT('Ctrl Pts',(53.1366752333902,30.5936133383991,8.18252626730979));
#54281=CARTESIAN_POINT('Ctrl Pts',(53.0858274795292,30.5299979777354,8.18675099952899));
#54282=CARTESIAN_POINT('Ctrl Pts',(53.0349924254941,30.4663985057579,8.19097467657151));
#54283=CARTESIAN_POINT('Ctrl Pts',(52.9873680690511,30.4003098784601,8.19519835361404));
#54284=CARTESIAN_POINT('Ctrl Pts',(52.9431895986978,30.3320965517166,8.19942203065656));
#54285=CARTESIAN_POINT('Ctrl Pts',(52.8989309731088,30.2637594620803,8.20365337093021));
#54286=CARTESIAN_POINT('Ctrl Pts',(52.8581309615497,30.1932903722078,8.20788471120387));
#54287=CARTESIAN_POINT('Ctrl Pts',(52.8209793817891,30.1210795669407,8.21211605147752));
#54288=CARTESIAN_POINT('Ctrl Pts',(52.7839345761983,30.049076296557,8.21633523081893));
#54289=CARTESIAN_POINT('Ctrl Pts',(52.750517371286,29.9753417578273,8.22055441016033));
#54290=CARTESIAN_POINT('Ctrl Pts',(52.7208672479652,29.9002800389891,8.22477358950174));
#54291=CARTESIAN_POINT('Ctrl Pts',(52.6873086607357,29.8153237232269,8.22954893888001));
#54292=CARTESIAN_POINT('Ctrl Pts',(52.6584702201738,29.7284032433861,8.23432428825828));
#54293=CARTESIAN_POINT('Ctrl Pts',(52.6345571909943,29.6400238802757,8.23909963763655));
#54294=CARTESIAN_POINT('Ctrl Pts',(52.6107313882432,29.5519668943989,8.24385756819817));
#54295=CARTESIAN_POINT('Ctrl Pts',(52.5917952654792,29.4624618606748,8.24861549875978));
#54296=CARTESIAN_POINT('Ctrl Pts',(52.5779051312006,29.3720305048458,8.2533734293214));
#54297=CARTESIAN_POINT('Ctrl Pts',(52.564101568475,29.2821627708467,8.25810170563859));
#54298=CARTESIAN_POINT('Ctrl Pts',(52.5552814037465,29.1913804539606,8.26282998195578));
#54299=CARTESIAN_POINT('Ctrl Pts',(52.5515500002522,29.1002140146641,8.26755825827297));
#54300=CARTESIAN_POINT('Ctrl Pts',(52.5502046676053,29.0673445629218,8.26926300676849));
#54301=CARTESIAN_POINT('Ctrl Pts',(52.5495203673848,29.0344253362664,8.270967755264));
#54302=CARTESIAN_POINT('Ctrl Pts',(52.5495004479559,29.0014816989085,8.27267250375952));
#54303=CARTESIAN_POINT('',(52.5495008396014,28.9979714818537,9.07267250383346));
#54304=CARTESIAN_POINT('Ctrl Pts',(52.5495004479556,29.0014816983595,8.27267250378793));
#54305=CARTESIAN_POINT('Ctrl Pts',(52.5494507665478,28.9193163462504,8.27692434941349));
#54306=CARTESIAN_POINT('Ctrl Pts',(52.5535379338215,28.837136673185,8.28117619503905));
#54307=CARTESIAN_POINT('Ctrl Pts',(52.5617397578869,28.7553834802586,8.28542804066461));
#54308=CARTESIAN_POINT('Ctrl Pts',(52.5699428094404,28.6736180521174,8.28968052262306));
#54309=CARTESIAN_POINT('Ctrl Pts',(52.582261695604,28.5922796825047,8.2939330045815));
#54310=CARTESIAN_POINT('Ctrl Pts',(52.5986224231266,28.5118033354378,8.29818548653995));
#54311=CARTESIAN_POINT('Ctrl Pts',(52.6157081009362,28.4277610497037,8.30262639765055));
#54312=CARTESIAN_POINT('Ctrl Pts',(52.6372020240865,28.3446594869578,8.30706730876115));
#54313=CARTESIAN_POINT('Ctrl Pts',(52.6629611688432,28.2629791375644,8.31150821987176));
#54314=CARTESIAN_POINT('Ctrl Pts',(52.6876730016431,28.1846197371921,8.31576857299608));
#54315=CARTESIAN_POINT('Ctrl Pts',(52.716309733793,28.1075686378834,8.32002892612039));
#54316=CARTESIAN_POINT('Ctrl Pts',(52.7486955163619,28.032230207151,8.32428927924471));
#54317=CARTESIAN_POINT('Ctrl Pts',(52.7811086573637,27.9568281330158,8.32855323137377));
#54318=CARTESIAN_POINT('Ctrl Pts',(52.8172769529868,27.8831420135458,8.33281718350283));
#54319=CARTESIAN_POINT('Ctrl Pts',(52.8569786237512,27.8115515867567,8.33708113563188));
#54320=CARTESIAN_POINT('Ctrl Pts',(52.8967483001918,27.7398385314915,8.34135239155804));
#54321=CARTESIAN_POINT('Ctrl Pts',(52.940063187104,27.6702287139669,8.3456236474842));
#54322=CARTESIAN_POINT('Ctrl Pts',(52.9866585870374,27.6030724410873,8.34989490341036));
#54323=CARTESIAN_POINT('Ctrl Pts',(52.9924095412518,27.5947837977644,8.35042207556264));
#54324=CARTESIAN_POINT('Ctrl Pts',(52.9982104195672,27.5865324869345,8.35094924771491));
#54325=CARTESIAN_POINT('Ctrl Pts',(53.0040606837377,27.5783191301145,8.35147641986719));
#54326=CARTESIAN_POINT('Ctrl Pts',(53.0510318883543,27.5123748834046,8.35570903403824));
#54327=CARTESIAN_POINT('Ctrl Pts',(53.1013620710945,27.4486383399154,8.35994164820929));
#54328=CARTESIAN_POINT('Ctrl Pts',(53.1548164171103,27.3874716140687,8.36417426238034));
#54329=CARTESIAN_POINT('Ctrl Pts',(53.2081945155205,27.3263921368131,8.3684008391247));
#54330=CARTESIAN_POINT('Ctrl Pts',(53.2646876232179,27.2678755437295,8.37262741586906));
#54331=CARTESIAN_POINT('Ctrl Pts',(53.3240185106077,27.2122538498952,8.37685399261342));
#54332=CARTESIAN_POINT('Ctrl Pts',(53.3832835475904,27.1566938896932,8.38107587834755));
#54333=CARTESIAN_POINT('Ctrl Pts',(53.4453797688037,27.1040227606304,8.38529776408169));
#54334=CARTESIAN_POINT('Ctrl Pts',(53.509991616305,27.054537261596,8.38951964981582));
#54335=CARTESIAN_POINT('Ctrl Pts',(53.5745598851104,27.0050851390024,8.39373868801841));
#54336=CARTESIAN_POINT('Ctrl Pts',(53.6416400425298,26.9588146608482,8.39795772622101));
#54337=CARTESIAN_POINT('Ctrl Pts',(53.7108827858705,26.9159829515489,8.40217676442359));
#54338=CARTESIAN_POINT('Ctrl Pts',(53.7801029170556,26.8731652295243,8.40639442484212));
#54339=CARTESIAN_POINT('Ctrl Pts',(53.8514838368787,26.8337842903864,8.41061208526065));
#54340=CARTESIAN_POINT('Ctrl Pts',(53.9246476931999,26.7980536640827,8.41482974567919));
#54341=CARTESIAN_POINT('Ctrl Pts',(53.997810027009,26.7623237813198,8.4190473183298));
#54342=CARTESIAN_POINT('Ctrl Pts',(54.0727548056031,26.7302442631621,8.42326489098041));
#54343=CARTESIAN_POINT('Ctrl Pts',(54.14908133029,26.7019817956468,8.42748246363102));
#54344=CARTESIAN_POINT('Ctrl Pts',(54.2255374235346,26.6736713510073,8.43170719584782));
#54345=CARTESIAN_POINT('Ctrl Pts',(54.3033795179171,26.6491910834525,8.43593192806462));
#54346=CARTESIAN_POINT('Ctrl Pts',(54.3821883625906,26.6286588118363,8.44015666028142));
#54347=CARTESIAN_POINT('Ctrl Pts',(54.4609775239111,26.6081316683748,8.44438033732611));
#54348=CARTESIAN_POINT('Ctrl Pts',(54.5407324919504,26.5915506230681,8.44860401437079));
#54349=CARTESIAN_POINT('Ctrl Pts',(54.6210246221457,26.5789820502565,8.45282769141548));
#54350=CARTESIAN_POINT('Ctrl Pts',(54.7014624304185,26.5663906736468,8.4570590316913));
#54351=CARTESIAN_POINT('Ctrl Pts',(54.7824388852395,26.5578263674288,8.46129037196712));
#54352=CARTESIAN_POINT('Ctrl Pts',(54.8635202295622,26.5533035492196,8.46552171224294));
#54353=CARTESIAN_POINT('Ctrl Pts',(54.9443685446839,26.548793729669,8.46974089157284));
#54354=CARTESIAN_POINT('Ctrl Pts',(55.0253206914566,26.5483021181239,8.47396007090274));
#54355=CARTESIAN_POINT('Ctrl Pts',(55.1059508059623,26.5517915373245,8.47817925023265));
#54356=CARTESIAN_POINT('Ctrl Pts',(55.1868376653727,26.5552920676417,8.48241186440388));
#54357=CARTESIAN_POINT('Ctrl Pts',(55.2677012780256,26.5628120689609,8.48664447857512));
#54358=CARTESIAN_POINT('Ctrl Pts',(55.3481100598163,26.574351708047,8.49087709274636));
#54359=CARTESIAN_POINT('Ctrl Pts',(55.4284041460295,26.5858748869214,8.49510366949089));
#54360=CARTESIAN_POINT('Ctrl Pts',(55.5082442339118,26.6014062503793,8.49933024623543));
#54361=CARTESIAN_POINT('Ctrl Pts',(55.5872008968254,26.6208940005188,8.50355682297996));
#54362=CARTESIAN_POINT('Ctrl Pts',(55.666069926992,26.6403601215137,8.50777870871405));
#54363=CARTESIAN_POINT('Ctrl Pts',(55.7440570316991,26.6637737932659,8.51200059444813));
#54364=CARTESIAN_POINT('Ctrl Pts',(55.8207414585528,26.691031895367,8.51622248018222));
#54365=CARTESIAN_POINT('Ctrl Pts',(55.8973741641327,26.7182716127214,8.52044151838499));
#54366=CARTESIAN_POINT('Ctrl Pts',(55.9727055002787,26.7493504554118,8.52466055658775));
#54367=CARTESIAN_POINT('Ctrl Pts',(56.0463296238771,26.7841153982671,8.52887959479051));
#54368=CARTESIAN_POINT('Ctrl Pts',(56.1199297045208,26.8188689881594,8.53309725520921));
#54369=CARTESIAN_POINT('Ctrl Pts',(56.1918232600546,26.857306089447,8.53731491562791));
#54370=CARTESIAN_POINT('Ctrl Pts',(56.2616254731621,26.8992259960985,8.54153257604661));
#54371=CARTESIAN_POINT('Ctrl Pts',(56.331426233712,26.9411450304126,8.54575014869739));
#54372=CARTESIAN_POINT('Ctrl Pts',(56.3991353407199,26.9865464858135,8.54996772134817));
#54373=CARTESIAN_POINT('Ctrl Pts',(56.4643948330412,27.0351849901423,8.55418529399896));
#54374=CARTESIAN_POINT('Ctrl Pts',(56.5297651070062,27.0839060610566,8.55841002621555));
#54375=CARTESIAN_POINT('Ctrl Pts',(56.5926770719442,27.1358748961834,8.56263475843215));
#54376=CARTESIAN_POINT('Ctrl Pts',(56.6528036579295,27.1908039580148,8.56685949064874));
#54377=CARTESIAN_POINT('Ctrl Pts',(56.712915226661,27.2457193007293,8.57108316769358));
#54378=CARTESIAN_POINT('Ctrl Pts',(56.7702424946668,27.3035930455017,8.57530684473841));
#54379=CARTESIAN_POINT('Ctrl Pts',(56.8244964310299,27.3641017687035,8.57953052178325));
#54380=CARTESIAN_POINT('Ctrl Pts',(56.8788488030569,27.4247202759456,8.58376186205921));
#54381=CARTESIAN_POINT('Ctrl Pts',(56.9301164064617,27.4879829538693,8.58799320233517));
#54382=CARTESIAN_POINT('Ctrl Pts',(56.9780510096974,27.5535338050839,8.59222454261113));
#54383=CARTESIAN_POINT('Ctrl Pts',(57.0258478480335,27.6188962619899,8.59644372194012));
#54384=CARTESIAN_POINT('Ctrl Pts',(57.0703306381617,27.6865333311812,8.60066290126911));
#54385=CARTESIAN_POINT('Ctrl Pts',(57.1112987246448,27.7560675479299,8.6048820805981));
#54386=CARTESIAN_POINT('Ctrl Pts',(57.15239726299,27.8258231777058,8.60911469476982));
#54387=CARTESIAN_POINT('Ctrl Pts',(57.190111512103,27.8977475107696,8.61334730894156));
#54388=CARTESIAN_POINT('Ctrl Pts',(57.224206377363,27.971478614273,8.61757992311328));
#54389=CARTESIAN_POINT('Ctrl Pts',(57.2582526094991,28.0451045472805,8.62180649985832));
#54390=CARTESIAN_POINT('Ctrl Pts',(57.2886895182319,28.1205317139537,8.62603307660336));
#54391=CARTESIAN_POINT('Ctrl Pts',(57.3153267727405,28.197371701576,8.6302596533484));
#54392=CARTESIAN_POINT('Ctrl Pts',(57.3419344629792,28.2741264057041,8.63448153908237));
#54393=CARTESIAN_POINT('Ctrl Pts',(57.364750727125,28.3522903783227,8.63870342481633));
#54394=CARTESIAN_POINT('Ctrl Pts',(57.3836330072357,28.4314545428757,8.6429253105503));
#54395=CARTESIAN_POINT('Ctrl Pts',(57.4025025518354,28.5105653136608,8.64714434875358));
#54396=CARTESIAN_POINT('Ctrl Pts',(57.417443274682,28.5906744858628,8.65136338695687));
#54397=CARTESIAN_POINT('Ctrl Pts',(57.4283625958313,28.6713583210128,8.65558242516015));
#54398=CARTESIAN_POINT('Ctrl Pts',(57.4392783511284,28.7520158077637,8.65980008557938));
#54399=CARTESIAN_POINT('Ctrl Pts',(57.4461752504949,28.8332471247745,8.66401774599861));
#54400=CARTESIAN_POINT('Ctrl Pts',(57.4490121563561,28.9146202130469,8.66823540641784));
#54401=CARTESIAN_POINT('Ctrl Pts',(57.4518490031823,28.9959916079761,8.67245297906914));
#54402=CARTESIAN_POINT('Ctrl Pts',(57.4506260094729,29.0775043039943,8.67667055172045));
#54403=CARTESIAN_POINT('Ctrl Pts',(57.4453541252492,29.158724453462,8.68088812437176));
#54404=CARTESIAN_POINT('Ctrl Pts',(57.4400732917081,29.2400824786609,8.68511285658774));
#54405=CARTESIAN_POINT('Ctrl Pts',(57.4307298461979,29.3211464976868,8.68933758880372));
#54406=CARTESIAN_POINT('Ctrl Pts',(57.4173869253028,29.401485620384,8.69356232101971));
#54407=CARTESIAN_POINT('Ctrl Pts',(57.4040473369403,29.4818046775536,8.69778599806508));
#54408=CARTESIAN_POINT('Ctrl Pts',(57.3867103907381,29.5613987494988,8.70200967511045));
#54409=CARTESIAN_POINT('Ctrl Pts',(57.3654900339305,29.6398493177111,8.70623335215583));
#54410=CARTESIAN_POINT('Ctrl Pts',(57.3442311759551,29.7184422227618,8.71046469243233));
#54411=CARTESIAN_POINT('Ctrl Pts',(57.3190749703805,29.7958870347219,8.71469603270884));
#54412=CARTESIAN_POINT('Ctrl Pts',(57.2901848993448,29.8717817254412,8.71892737298535));
#54413=CARTESIAN_POINT('Ctrl Pts',(57.261377858909,29.9474582934116,8.72314655231142));
#54414=CARTESIAN_POINT('Ctrl Pts',(57.2288586457946,30.0215932549045,8.72736573163748));
#54415=CARTESIAN_POINT('Ctrl Pts',(57.1928346499557,30.0938128029758,8.73158491096355));
#54416=CARTESIAN_POINT('Ctrl Pts',(57.1566959453605,30.1662623148349,8.73581752513496));
#54417=CARTESIAN_POINT('Ctrl Pts',(57.1168956679506,30.2370536433283,8.74005013930637));
#54418=CARTESIAN_POINT('Ctrl Pts',(57.0736094304284,30.3057925486226,8.74428275347778));
#54419=CARTESIAN_POINT('Ctrl Pts',(57.0303849366597,30.3744334043227,8.74850933022249));
#54420=CARTESIAN_POINT('Ctrl Pts',(56.9836846040812,30.4410272615588,8.7527359069672));
#54421=CARTESIAN_POINT('Ctrl Pts',(56.9337306268262,30.5052030138405,8.75696248371191));
#54422=CARTESIAN_POINT('Ctrl Pts',(56.8838320927002,30.5693075384699,8.76118436944595));
#54423=CARTESIAN_POINT('Ctrl Pts',(56.8306873731901,30.6309989261475,8.76540625518));
#54424=CARTESIAN_POINT('Ctrl Pts',(56.7745620033723,30.6899348940676,8.76962814091404));
#54425=CARTESIAN_POINT('Ctrl Pts',(56.7184744883772,30.7488311115038,8.773847179117));
#54426=CARTESIAN_POINT('Ctrl Pts',(56.6594106353566,30.8049752646763,8.77806621731995));
#54427=CARTESIAN_POINT('Ctrl Pts',(56.597675486232,30.8580590116283,8.7822852555229));
#54428=CARTESIAN_POINT('Ctrl Pts',(56.5359604975564,30.9111254233639,8.7865029159418));
#54429=CARTESIAN_POINT('Ctrl Pts',(56.471576297174,30.9611331110164,8.79072057636069));
#54430=CARTESIAN_POINT('Ctrl Pts',(56.4048629117432,31.007812354083,8.79493823677958));
#54431=CARTESIAN_POINT('Ctrl Pts',(56.3381509145928,31.0544906257723,8.79915580943055));
#54432=CARTESIAN_POINT('Ctrl Pts',(56.2691102100636,31.0978403252284,8.80337338208153));
#54433=CARTESIAN_POINT('Ctrl Pts',(56.1981106817008,31.1376344506006,8.8075909547325));
#54434=CARTESIAN_POINT('Ctrl Pts',(56.1269906276686,31.1774961287258,8.81181568694887));
#54435=CARTESIAN_POINT('Ctrl Pts',(56.0539055041992,31.2137899282438,8.81604041916525));
#54436=CARTESIAN_POINT('Ctrl Pts',(55.979251124433,31.2463342327661,8.82026515138162));
#54437=CARTESIAN_POINT('Ctrl Pts',(55.904615390384,31.2788704090057,8.82448882842666));
#54438=CARTESIAN_POINT('Ctrl Pts',(55.8284116273999,31.3076588181063,8.82871250547169));
#54439=CARTESIAN_POINT('Ctrl Pts',(55.7510529323302,31.3325672000691,8.83293618251673));
#54440=CARTESIAN_POINT('Ctrl Pts',(55.6735538814628,31.3575207745706,8.83716752279289));
#54441=CARTESIAN_POINT('Ctrl Pts',(55.594896160868,31.3785801327825,8.84139886306906));
#54442=CARTESIAN_POINT('Ctrl Pts',(55.515506001708,31.395663543197,8.84563020334522));
#54443=CARTESIAN_POINT('Ctrl Pts',(55.4363440112969,31.4126978555819,8.84984938267315));
#54444=CARTESIAN_POINT('Ctrl Pts',(55.3564542494899,31.4257790520627,8.85406856200107));
#54445=CARTESIAN_POINT('Ctrl Pts',(55.2762631782407,31.434877595763,8.858287741329));
#54446=CARTESIAN_POINT('Ctrl Pts',(55.1958167600599,31.4440051113323,8.86252035550045));
#54447=CARTESIAN_POINT('Ctrl Pts',(55.1147679047255,31.4491584908913,8.86675296967191));
#54448=CARTESIAN_POINT('Ctrl Pts',(55.0335429142519,31.4502704183219,8.87098558384337));
#54449=CARTESIAN_POINT('Ctrl Pts',(54.9524337836005,31.4513807596925,8.87521216058813));
#54450=CARTESIAN_POINT('Ctrl Pts',(54.8711494774509,31.4484610921686,8.8794387373329));
#54451=CARTESIAN_POINT('Ctrl Pts',(54.7901222519542,31.4414957671221,8.88366531407767));
#54452=CARTESIAN_POINT('Ctrl Pts',(54.7091849572946,31.4345381727798,8.8878871998117));
#54453=CARTESIAN_POINT('Ctrl Pts',(54.6285046368471,31.4235438825422,8.89210908554573));
#54454=CARTESIAN_POINT('Ctrl Pts',(54.5485129635736,31.4085492948949,8.89633097127977));
#54455=CARTESIAN_POINT('Ctrl Pts',(54.4685752422038,31.3935648206322,8.90055000948276));
#54456=CARTESIAN_POINT('Ctrl Pts',(54.389325700945,31.3745854929444,8.90476904768575));
#54457=CARTESIAN_POINT('Ctrl Pts',(54.3111890498774,31.3516993270806,8.90898808588874));
#54458=CARTESIAN_POINT('Ctrl Pts',(54.2330779153911,31.3288206350041,8.91320574630769));
#54459=CARTESIAN_POINT('Ctrl Pts',(54.1560793948241,31.3020377689536,8.91742340672663));
#54460=CARTESIAN_POINT('Ctrl Pts',(54.0806048473256,31.271489115809,8.92164106714557));
#54461=CARTESIAN_POINT('Ctrl Pts',(54.005131870424,31.2409410983705,8.92585863979659));
#54462=CARTESIAN_POINT('Ctrl Pts',(53.9311832337083,31.2066276250278,8.93007621244761));
#54463=CARTESIAN_POINT('Ctrl Pts',(53.8591507169577,31.1687353834394,8.93429378509862));
#54464=CARTESIAN_POINT('Ctrl Pts',(53.7869959209839,31.130778817653,8.93851851731494));
#54465=CARTESIAN_POINT('Ctrl Pts',(53.7167641662081,31.0892315460588,8.94274324953126));
#54466=CARTESIAN_POINT('Ctrl Pts',(53.6488232780315,31.0443267145959,8.94696798174758));
#54467=CARTESIAN_POINT('Ctrl Pts',(53.5808993588053,30.9994330985863,8.95119165879266));
#54468=CARTESIAN_POINT('Ctrl Pts',(53.5152655249853,30.9511838928963,8.95541533583774));
#54469=CARTESIAN_POINT('Ctrl Pts',(53.4522576098529,30.8998536111348,8.95963901288282));
#54470=CARTESIAN_POINT('Ctrl Pts',(53.3891353762696,30.8484301982439,8.96387035315904));
#54471=CARTESIAN_POINT('Ctrl Pts',(53.3286489288173,30.7939148494673,8.96810169343525));
#54472=CARTESIAN_POINT('Ctrl Pts',(53.2710988665349,30.7366206035583,8.97233303371146));
#54473=CARTESIAN_POINT('Ctrl Pts',(53.2137142041733,30.6794910223491,8.97655221303913));
#54474=CARTESIAN_POINT('Ctrl Pts',(53.1592493158241,30.6195988886482,8.98077139236679));
#54475=CARTESIAN_POINT('Ctrl Pts',(53.1079611439954,30.5572858496014,8.98499057169445));
#54476=CARTESIAN_POINT('Ctrl Pts',(53.0567614607749,30.4950803206081,8.98920247157944));
#54477=CARTESIAN_POINT('Ctrl Pts',(53.0085312255926,30.4302236210157,8.99341437146443));
#54478=CARTESIAN_POINT('Ctrl Pts',(52.9635585782611,30.3630321294181,8.99762627134942));
#54479=CARTESIAN_POINT('Ctrl Pts',(52.9186470371168,30.295931933666,9.00183244835266));
#54480=CARTESIAN_POINT('Ctrl Pts',(52.8769845582534,30.2265036275436,9.0060386253559));
#54481=CARTESIAN_POINT('Ctrl Pts',(52.8388195372745,30.1550970771038,9.01024480235913));
#54482=CARTESIAN_POINT('Ctrl Pts',(52.8006944219304,30.0837651898935,9.01444658135187));
#54483=CARTESIAN_POINT('Ctrl Pts',(52.7660597242993,30.0104595761678,9.0186483603446));
#54484=CARTESIAN_POINT('Ctrl Pts',(52.7351201108098,29.9355583025883,9.02285013933733));
#54485=CARTESIAN_POINT('Ctrl Pts',(52.7041994735316,29.8607029682508,9.02704934125049));
#54486=CARTESIAN_POINT('Ctrl Pts',(52.6769696037845,29.7842543477414,9.03124854316364));
#54487=CARTESIAN_POINT('Ctrl Pts',(52.6535882303907,29.7066130889241,9.0354477450768));
#54488=CARTESIAN_POINT('Ctrl Pts',(52.630216246542,29.62900300946,9.03964526066491));
#54489=CARTESIAN_POINT('Ctrl Pts',(52.6106898219177,29.5502016927393,9.04384277625303));
#54490=CARTESIAN_POINT('Ctrl Pts',(52.5951171935888,29.4706261121396,9.04804029184114));
#54491=CARTESIAN_POINT('Ctrl Pts',(52.5795387820052,29.3910209793131,9.05223936627346));
#54492=CARTESIAN_POINT('Ctrl Pts',(52.5679171975141,29.3106414678569,9.05643844070578));
#54493=CARTESIAN_POINT('Ctrl Pts',(52.5603095856078,29.2299150537103,9.0606375151381));
#54494=CARTESIAN_POINT('Ctrl Pts',(52.5530415138441,29.152791591254,9.06464917802138));
#54495=CARTESIAN_POINT('Ctrl Pts',(52.5494367842607,29.0753519218323,9.06866084090466));
#54496=CARTESIAN_POINT('Ctrl Pts',(52.5495008396007,28.9979714827317,9.07267250378794));
#54497=CARTESIAN_POINT('',(52.5495000016466,29.0000898342118,9.87267250383148));
#54498=CARTESIAN_POINT('Ctrl Pts',(52.5495008396014,28.9979714818537,9.07267250383347));
#54499=CARTESIAN_POINT('Ctrl Pts',(52.5495811640756,28.9009375672519,9.07770306915667));
#54500=CARTESIAN_POINT('Ctrl Pts',(52.5554288148724,28.8041502685366,9.08273363447987));
#54501=CARTESIAN_POINT('Ctrl Pts',(52.5669331831094,28.7082190641151,9.08776419980306));
#54502=CARTESIAN_POINT('Ctrl Pts',(52.5785831185121,28.611074022198,9.0928584179163));
#54503=CARTESIAN_POINT('Ctrl Pts',(52.5960337473273,28.5148069165952,9.09795263602954));
#54504=CARTESIAN_POINT('Ctrl Pts',(52.6191211193409,28.4200293062307,9.10304685414278));
#54505=CARTESIAN_POINT('Ctrl Pts',(52.6321833835234,28.3664064779398,9.10592903678181));
#54506=CARTESIAN_POINT('Ctrl Pts',(52.6470491004416,28.3132600501885,9.10881121942086));
#54507=CARTESIAN_POINT('Ctrl Pts',(52.6636818643731,28.2606977484539,9.1116934020599));
#54508=CARTESIAN_POINT('Ctrl Pts',(52.6881078224556,28.1835076564059,9.11592601623136));
#54509=CARTESIAN_POINT('Ctrl Pts',(52.7164087614872,28.1073858387591,9.12015863040283));
#54510=CARTESIAN_POINT('Ctrl Pts',(52.7484725483883,28.0327490580833,9.12439124457429));
#54511=CARTESIAN_POINT('Ctrl Pts',(52.7804905993079,27.9582187397671,9.12861782131907));
#54512=CARTESIAN_POINT('Ctrl Pts',(52.8162606560091,27.8851696745553,9.13284439806384));
#54513=CARTESIAN_POINT('Ctrl Pts',(52.8556209719017,27.8140030211455,9.13707097480862));
#54514=CARTESIAN_POINT('Ctrl Pts',(52.8949376024015,27.7429153544798,9.14129286054265));
#54515=CARTESIAN_POINT('Ctrl Pts',(52.9378363506593,27.6737063527297,9.14551474627668));
#54516=CARTESIAN_POINT('Ctrl Pts',(52.9841081722206,27.6067554454826,9.14973663201071));
#54517=CARTESIAN_POINT('Ctrl Pts',(53.0303487848731,27.5398496945465,9.15395567021372));
#54518=CARTESIAN_POINT('Ctrl Pts',(53.0799576889743,27.4751993944456,9.15817470841674));
#54519=CARTESIAN_POINT('Ctrl Pts',(53.1326815334158,27.4131565942559,9.16239374661975));
#54520=CARTESIAN_POINT('Ctrl Pts',(53.1853881601719,27.3511340549828,9.1666114070387));
#54521=CARTESIAN_POINT('Ctrl Pts',(53.2412074065279,27.2917176782871,9.17082906745765));
#54522=CARTESIAN_POINT('Ctrl Pts',(53.2998453534869,27.2352268055243,9.1750467278766));
#54523=CARTESIAN_POINT('Ctrl Pts',(53.3584820802124,27.1787371083153,9.17926430052763));
#54524=CARTESIAN_POINT('Ctrl Pts',(53.4199370555498,27.1251731154538,9.18348187317866));
#54525=CARTESIAN_POINT('Ctrl Pts',(53.4838802205191,27.074816615419,9.18769944582969));
#54526=CARTESIAN_POINT('Ctrl Pts',(53.5479319325845,27.0243746324112,9.19192417804599));
#54527=CARTESIAN_POINT('Ctrl Pts',(53.6144799183171,26.9771513251288,9.1961489102623));
#54528=CARTESIAN_POINT('Ctrl Pts',(53.6831614432795,26.9333876837844,9.20037364247861));
#54529=CARTESIAN_POINT('Ctrl Pts',(53.7518258143102,26.8896349728687,9.2045973195237));
#54530=CARTESIAN_POINT('Ctrl Pts',(53.8226222433147,26.8493404120462,9.2088209965688));
#54531=CARTESIAN_POINT('Ctrl Pts',(53.8951632431404,26.8126989254581,9.2130446736139));
#54532=CARTESIAN_POINT('Ctrl Pts',(53.9678358577752,26.7759909583657,9.21727601389013));
#54533=CARTESIAN_POINT('Ctrl Pts',(54.0422589430834,26.7429495003037,9.22150735416635));
#54534=CARTESIAN_POINT('Ctrl Pts',(54.1180241756887,26.7137216058996,9.22573869444258));
#54535=CARTESIAN_POINT('Ctrl Pts',(54.1935716576423,26.6845777129937,9.22995787377017));
#54536=CARTESIAN_POINT('Ctrl Pts',(54.2704531240852,26.6592255560931,9.23417705309777));
#54537=CARTESIAN_POINT('Ctrl Pts',(54.3482519025511,26.6377606667673,9.23839623242536));
#54538=CARTESIAN_POINT('Ctrl Pts',(54.4262984103412,26.6162274282639,9.24262884659684));
#54539=CARTESIAN_POINT('Ctrl Pts',(54.5055583653667,26.5985261909816,9.24686146076832));
#54540=CARTESIAN_POINT('Ctrl Pts',(54.5856211313313,26.5847897807435,9.2510940749398));
#54541=CARTESIAN_POINT('Ctrl Pts',(54.6655696952777,26.5710729642049,9.25532065168458));
#54542=CARTESIAN_POINT('Ctrl Pts',(54.7463183417245,26.5613098201536,9.25954722842937));
#54543=CARTESIAN_POINT('Ctrl Pts',(54.8274425136619,26.5555830625876,9.26377380517416));
#54544=CARTESIAN_POINT('Ctrl Pts',(54.9084766471625,26.5498626610593,9.26799569090819));
#54545=CARTESIAN_POINT('Ctrl Pts',(54.9898850169335,26.5481697769688,9.27221757664221));
#54546=CARTESIAN_POINT('Ctrl Pts',(55.0712355438955,26.5505356203272,9.27643946237624));
#54547=CARTESIAN_POINT('Ctrl Pts',(55.1525312024498,26.5528998679976,9.28065850057926));
#54548=CARTESIAN_POINT('Ctrl Pts',(55.2337686325249,26.5593173927617,9.28487753878228));
#54549=CARTESIAN_POINT('Ctrl Pts',(55.3145146019266,26.5697673331191,9.28909657698531));
#54550=CARTESIAN_POINT('Ctrl Pts',(55.3952342026387,26.580213860907,9.29331423740427));
#54551=CARTESIAN_POINT('Ctrl Pts',(55.4754622010538,26.5946901295471,9.29753189782324));
#54552=CARTESIAN_POINT('Ctrl Pts',(55.5547707158481,26.6131234420613,9.30174955824221));
#54553=CARTESIAN_POINT('Ctrl Pts',(55.6340775802621,26.6315563709852,9.30596713089325));
#54554=CARTESIAN_POINT('Ctrl Pts',(55.712464546878,26.6539460737477,9.3101847035443));
#54555=CARTESIAN_POINT('Ctrl Pts',(55.7895155600359,26.680169094425,9.31440227619534));
#54556=CARTESIAN_POINT('Ctrl Pts',(55.866697371594,26.7064366301451,9.31862700841163));
#54557=CARTESIAN_POINT('Ctrl Pts',(55.942538250152,26.7365503528518,9.32285174062792));
#54558=CARTESIAN_POINT('Ctrl Pts',(56.0166385741196,26.7703371870142,9.32707647284421));
#54559=CARTESIAN_POINT('Ctrl Pts',(56.0907203907542,26.8041155825603,9.33130014988932));
#54560=CARTESIAN_POINT('Ctrl Pts',(56.1630621179304,26.8415650218201,9.33552382693443));
#54561=CARTESIAN_POINT('Ctrl Pts',(56.2332893000427,26.8824665876543,9.33974750397954));
#54562=CARTESIAN_POINT('Ctrl Pts',(56.3036438988875,26.9234423632705,9.34397884425578));
#54563=CARTESIAN_POINT('Ctrl Pts',(56.3718758951069,26.9678825283198,9.34821018453202));
#54564=CARTESIAN_POINT('Ctrl Pts',(56.4376396439943,27.0155246275109,9.35244152480826));
#54565=CARTESIAN_POINT('Ctrl Pts',(56.5032143866743,27.0630298024444,9.35666070413577));
#54566=CARTESIAN_POINT('Ctrl Pts',(56.5663347477688,27.1137181813588,9.36087988346329));
#54567=CARTESIAN_POINT('Ctrl Pts',(56.6266937561611,27.1672922563413,9.3650990627908));
#54568=CARTESIAN_POINT('Ctrl Pts',(56.6872449616128,27.2210369235841,9.36933167696229));
#54569=CARTESIAN_POINT('Ctrl Pts',(56.745242389422,27.2778856055347,9.37356429113377));
#54570=CARTESIAN_POINT('Ctrl Pts',(56.8003510712067,27.3375661605932,9.37779690530526));
#54571=CARTESIAN_POINT('Ctrl Pts',(56.8553811456313,27.3971615869437,9.38202348205006));
#54572=CARTESIAN_POINT('Ctrl Pts',(56.9075303453909,27.4595805251693,9.38625005879485));
#54573=CARTESIAN_POINT('Ctrl Pts',(56.9564981587189,27.524511875707,9.39047663553964));
#54574=CARTESIAN_POINT('Ctrl Pts',(57.0054116234443,27.5893711599644,9.39469852127367));
#54575=CARTESIAN_POINT('Ctrl Pts',(57.0511504394666,27.6567369467867,9.39892040700769));
#54576=CARTESIAN_POINT('Ctrl Pts',(57.0934532028416,27.7262637880973,9.40314229274172));
#54577=CARTESIAN_POINT('Ctrl Pts',(57.1357274343147,27.7957437357096,9.40736133094475));
#54578=CARTESIAN_POINT('Ctrl Pts',(57.1745699750768,27.8673814471224,9.41158036914778));
#54579=CARTESIAN_POINT('Ctrl Pts',(57.2097624723251,27.9408021592243,9.41579940735081));
#54580=CARTESIAN_POINT('Ctrl Pts',(57.2449434769868,28.0141988947985,9.42001706776978));
#54581=CARTESIAN_POINT('Ctrl Pts',(57.276476604675,28.0893770561332,9.42423472818876));
#54582=CARTESIAN_POINT('Ctrl Pts',(57.304189896511,28.1659381492859,9.42845238860773));
#54583=CARTESIAN_POINT('Ctrl Pts',(57.3319026116439,28.2424976492313,9.43266996125878));
#54584=CARTESIAN_POINT('Ctrl Pts',(57.3557954919589,28.3204395865649,9.43688753390983));
#54585=CARTESIAN_POINT('Ctrl Pts',(57.3757455943626,28.3993477537987,9.44110510656089));
#54586=CARTESIAN_POINT('Ctrl Pts',(57.3957295631798,28.4783898720553,9.44532983877717));
#54587=CARTESIAN_POINT('Ctrl Pts',(57.4117572483169,28.5584010491796,9.44955457099345));
#54588=CARTESIAN_POINT('Ctrl Pts',(57.4237562755797,28.6389518500418,9.45377930320973));
#54589=CARTESIAN_POINT('Ctrl Pts',(57.4357523059595,28.719482532497,9.45800298025485));
#54590=CARTESIAN_POINT('Ctrl Pts',(57.4437216661573,28.800552103174,9.46222665729996));
#54591=CARTESIAN_POINT('Ctrl Pts',(57.4476441354587,28.8817272805974,9.46645033434508));
#54592=CARTESIAN_POINT('Ctrl Pts',(57.4515737214946,28.9630497382556,9.47068167462133));
#54593=CARTESIAN_POINT('Ctrl Pts',(57.4514417436959,29.0444777196845,9.47491301489758));
#54594=CARTESIAN_POINT('Ctrl Pts',(57.447280186925,29.1255784085121,9.47914435517382));
#54595=CARTESIAN_POINT('Ctrl Pts',(57.4431305905438,29.2064460124878,9.4833635345013));
#54596=CARTESIAN_POINT('Ctrl Pts',(57.4349746750456,29.2869877580856,9.48758271382878));
#54597=CARTESIAN_POINT('Ctrl Pts',(57.4228948822493,29.3667841866411,9.49180189315626));
#54598=CARTESIAN_POINT('Ctrl Pts',(57.4107766245956,29.4468347055032,9.49603450732774));
#54599=CARTESIAN_POINT('Ctrl Pts',(57.3946643624912,29.5264328793633,9.50026712149921));
#54600=CARTESIAN_POINT('Ctrl Pts',(57.3746040181182,29.6051495741856,9.50449973567069));
#54601=CARTESIAN_POINT('Ctrl Pts',(57.3545722879428,29.6837539870339,9.50872631241547));
#54602=CARTESIAN_POINT('Ctrl Pts',(57.3306037742864,29.7614789716775,9.51295288916026));
#54603=CARTESIAN_POINT('Ctrl Pts',(57.3027958364625,29.8379030884125,9.51717946590504));
#54604=CARTESIAN_POINT('Ctrl Pts',(57.2750187622294,29.9142423832277,9.52140135163907));
#54605=CARTESIAN_POINT('Ctrl Pts',(57.2434108890987,29.9892832446398,9.5256232373731));
#54606=CARTESIAN_POINT('Ctrl Pts',(57.2081196791139,30.0626183382145,9.52984512310713));
#54607=CARTESIAN_POINT('Ctrl Pts',(57.1728522719559,30.1359039695427,9.53406416131015));
#54608=CARTESIAN_POINT('Ctrl Pts',(57.1339066628975,30.2074857004826,9.53828319951317));
#54609=CARTESIAN_POINT('Ctrl Pts',(57.0914783412486,30.2769763498547,9.54250223771619));
#54610=CARTESIAN_POINT('Ctrl Pts',(57.0490638751426,30.3464443061142,9.54671989813515));
#54611=CARTESIAN_POINT('Ctrl Pts',(57.0031691970025,30.4138221407622,9.55093755855411));
#54612=CARTESIAN_POINT('Ctrl Pts',(56.9540349590479,30.4787486699296,9.55515521897308));
#54613=CARTESIAN_POINT('Ctrl Pts',(56.9049017435583,30.5436738480005,9.55937279162412));
#54614=CARTESIAN_POINT('Ctrl Pts',(56.8525293835573,30.6061474522904,9.56359036427516));
#54615=CARTESIAN_POINT('Ctrl Pts',(56.7972000740668,30.6658397713389,9.56780793692621));
#54616=CARTESIAN_POINT('Ctrl Pts',(56.7417768399817,30.7256334214345,9.5720326691425));
#54617=CARTESIAN_POINT('Ctrl Pts',(56.6833869308462,30.7826359974014,9.57625740135879));
#54618=CARTESIAN_POINT('Ctrl Pts',(56.6223511671111,30.8365530051086,9.58048213357508));
#54619=CARTESIAN_POINT('Ctrl Pts',(56.5613306476981,30.8904565464776,9.58470581062019));
#54620=CARTESIAN_POINT('Ctrl Pts',(56.4976659727563,30.9412757864979,9.58892948766529));
#54621=CARTESIAN_POINT('Ctrl Pts',(56.4317095815444,30.9887578847396,9.5931531647104));
#54622=CARTESIAN_POINT('Ctrl Pts',(56.3656335223123,31.0363261321564,9.59738450498664));
#54623=CARTESIAN_POINT('Ctrl Pts',(56.2972578284529,31.0805448845917,9.60161584526288));
#54624=CARTESIAN_POINT('Ctrl Pts',(56.2269629698428,31.1212053461734,9.60584718553912));
#54625=CARTESIAN_POINT('Ctrl Pts',(56.1568701399315,31.1617489488509,9.61006636486664));
#54626=CARTESIAN_POINT('Ctrl Pts',(56.0848696048905,31.1987545524203,9.61428554419417));
#54627=CARTESIAN_POINT('Ctrl Pts',(56.0113580986224,31.232062957524,9.6185047235217));
#54628=CARTESIAN_POINT('Ctrl Pts',(55.9376125146963,31.2654774243023,9.62273733769318));
#54629=CARTESIAN_POINT('Ctrl Pts',(55.8620720299263,31.2952953624052,9.62696995186467));
#54630=CARTESIAN_POINT('Ctrl Pts',(55.7851216128404,31.3213216716024,9.63120256603615));
#54631=CARTESIAN_POINT('Ctrl Pts',(55.7082809582991,31.3473108567133,9.63542914278094));
#54632=CARTESIAN_POINT('Ctrl Pts',(55.6300348022204,31.3695190071016,9.63965571952573));
#54633=CARTESIAN_POINT('Ctrl Pts',(55.5507896613485,31.3877983581014,9.64388229627053));
#54634=CARTESIAN_POINT('Ctrl Pts',(55.4716324734068,31.4060574211382,9.64810418200455));
#54635=CARTESIAN_POINT('Ctrl Pts',(55.3914789541511,31.4203962452269,9.65232606773858));
#54636=CARTESIAN_POINT('Ctrl Pts',(55.3107510644365,31.4307167720554,9.65654795347261));
#54637=CARTESIAN_POINT('Ctrl Pts',(55.23007762318,31.4410303380087,9.66076699167563));
#54638=CARTESIAN_POINT('Ctrl Pts',(55.148831040474,31.4473309306711,9.66498602987866));
#54639=CARTESIAN_POINT('Ctrl Pts',(55.0674425181974,31.4495717496614,9.66920506808168));
#54640=CARTESIAN_POINT('Ctrl Pts',(54.9860805744449,31.4518118368819,9.67342272850065));
#54641=CARTESIAN_POINT('Ctrl Pts',(54.9045772471911,31.4499947705608,9.67764038891962));
#54642=CARTESIAN_POINT('Ctrl Pts',(54.8233665178396,31.4441257870617,9.68185804933859));
#54643=CARTESIAN_POINT('Ctrl Pts',(54.7421574784526,31.4382569256938,9.68607562198964));
#54644=CARTESIAN_POINT('Ctrl Pts',(54.6612414881165,31.4283363494517,9.69029319464069));
#54645=CARTESIAN_POINT('Ctrl Pts',(54.5810487443192,31.4144212754537,9.69451076729174));
#54646=CARTESIAN_POINT('Ctrl Pts',(54.5007198688585,31.40048257984,9.69873549950803));
#54647=CARTESIAN_POINT('Ctrl Pts',(54.4211171564992,31.3825358993466,9.70296023172431));
#54648=CARTESIAN_POINT('Ctrl Pts',(54.3426622912597,31.3606900234186,9.70718496394059));
#54649=CARTESIAN_POINT('Ctrl Pts',(54.2642270209455,31.3388496037272,9.71140864098571));
#54650=CARTESIAN_POINT('Ctrl Pts',(54.1869394600097,31.3131121035319,9.71563231803082));
#54651=CARTESIAN_POINT('Ctrl Pts',(54.1112035656001,31.2836355112404,9.71985599507593));
#54652=CARTESIAN_POINT('Ctrl Pts',(54.0353302597224,31.2541054380749,9.72408733535218));
#54653=CARTESIAN_POINT('Ctrl Pts',(53.961014671789,31.2208229056018,9.72831867562842));
#54654=CARTESIAN_POINT('Ctrl Pts',(53.8886390731525,31.1839933929105,9.73255001590466));
#54655=CARTESIAN_POINT('Ctrl Pts',(53.8164714833,31.1472697289071,9.73676919523216));
#54656=CARTESIAN_POINT('Ctrl Pts',(53.7462331001432,31.1070197441476,9.74098837455966));
#54657=CARTESIAN_POINT('Ctrl Pts',(53.6782734463758,31.0634895607792,9.74520755388716));
#54658=CARTESIAN_POINT('Ctrl Pts',(53.6100973933339,31.019820767227,9.74944016805864));
#54659=CARTESIAN_POINT('Ctrl Pts',(53.5439610538095,30.9726884124556,9.75367278223012));
#54660=CARTESIAN_POINT('Ctrl Pts',(53.4802376599746,30.9223092050553,9.7579053964016));
#54661=CARTESIAN_POINT('Ctrl Pts',(53.4166051615776,30.872001858864,9.76213197314639));
#54662=CARTESIAN_POINT('Ctrl Pts',(53.3553791343214,30.8184571441745,9.76635854989118));
#54663=CARTESIAN_POINT('Ctrl Pts',(53.296904834979,30.7619356142839,9.77058512663597));
#54664=CARTESIAN_POINT('Ctrl Pts',(53.2384954353377,30.7054768167465,9.77480701237));
#54665=CARTESIAN_POINT('Ctrl Pts',(53.1828320274529,30.646048090124,9.77902889810402));
#54666=CARTESIAN_POINT('Ctrl Pts',(53.1302265809403,30.5839500028024,9.78325078383805));
#54667=CARTESIAN_POINT('Ctrl Pts',(53.07765661517,30.521893798715,9.78746982204107));
#54668=CARTESIAN_POINT('Ctrl Pts',(53.0281408139656,30.4571721632258,9.7916888602441));
#54669=CARTESIAN_POINT('Ctrl Pts',(52.9819531813185,30.3901213211836,9.79590789844712));
#54670=CARTESIAN_POINT('Ctrl Pts',(52.9357806318681,30.3230923755019,9.80012555886609));
#54671=CARTESIAN_POINT('Ctrl Pts',(52.8929343558679,30.2537361161135,9.80434321928506));
#54672=CARTESIAN_POINT('Ctrl Pts',(52.8536462207499,30.1824194282482,9.80856087970403));
#54673=CARTESIAN_POINT('Ctrl Pts',(52.8143589032031,30.1111042244562,9.81277845235508));
#54674=CARTESIAN_POINT('Ctrl Pts',(52.7786298024467,30.0378290807567,9.81699602500613));
#54675=CARTESIAN_POINT('Ctrl Pts',(52.7466451231777,29.9629860067006,9.82121359765718));
#54676=CARTESIAN_POINT('Ctrl Pts',(52.7146061481284,29.8880158823444,9.82543832987347));
#54677=CARTESIAN_POINT('Ctrl Pts',(52.6863244956853,29.8114729317168,9.82966306208975));
#54678=CARTESIAN_POINT('Ctrl Pts',(52.6619384756368,29.7337700990721,9.83388779430604));
#54679=CARTESIAN_POINT('Ctrl Pts',(52.6375585462525,29.6560866735248,9.83811147135115));
#54680=CARTESIAN_POINT('Ctrl Pts',(52.617072400219,29.5772444017894,9.84233514839625));
#54681=CARTESIAN_POINT('Ctrl Pts',(52.6005674274715,29.4976681423289,9.84655882544136));
#54682=CARTESIAN_POINT('Ctrl Pts',(52.5840325089161,29.4179475036315,9.8507901657176));
#54683=CARTESIAN_POINT('Ctrl Pts',(52.5714932707976,29.3374906761704,9.85502150599384));
#54684=CARTESIAN_POINT('Ctrl Pts',(52.5629854609046,29.2567301817819,9.85925284627008));
#54685=CARTESIAN_POINT('Ctrl Pts',(52.5545021026116,29.1762017945196,9.86347202559759));
#54686=CARTESIAN_POINT('Ctrl Pts',(52.5500269728094,29.0953719426398,9.8676912049251));
#54687=CARTESIAN_POINT('Ctrl Pts',(52.5495438984681,29.0146678036909,9.87191038425261));
#54688=CARTESIAN_POINT('Ctrl Pts',(52.5495148122119,29.0098085489954,9.87216442409772));
#54689=CARTESIAN_POINT('Ctrl Pts',(52.5495001797907,29.0049492076967,9.87241846394283));
#54690=CARTESIAN_POINT('Ctrl Pts',(52.5495000016467,29.0000898350446,9.87267250378794));
#54691=CARTESIAN_POINT('',(52.5495007823165,29.0019580941228,10.6726725037379));
#54692=CARTESIAN_POINT('Ctrl Pts',(52.5495000016466,29.0000898342118,9.87267250383148));
#54693=CARTESIAN_POINT('Ctrl Pts',(52.5494970367443,28.919213151244,9.87690060105406));
#54694=CARTESIAN_POINT('Ctrl Pts',(52.5535022747491,28.8381843604706,9.88112869827663));
#54695=CARTESIAN_POINT('Ctrl Pts',(52.5615349283419,28.7574338352052,9.88535679549921));
#54696=CARTESIAN_POINT('Ctrl Pts',(52.5695561224771,28.6767985093822,9.88957886087938));
#54697=CARTESIAN_POINT('Ctrl Pts',(52.5815932757421,28.5964411201722,9.89380092625955));
#54698=CARTESIAN_POINT('Ctrl Pts',(52.5976135911843,28.5167921847304,9.89802299163973));
#54699=CARTESIAN_POINT('Ctrl Pts',(52.6136155028604,28.4372347481349,9.9022402068093));
#54700=CARTESIAN_POINT('Ctrl Pts',(52.6335913916787,28.3583846020731,9.90645742197887));
#54701=CARTESIAN_POINT('Ctrl Pts',(52.6574568174838,28.2806658022539,9.91067463714844));
#54702=CARTESIAN_POINT('Ctrl Pts',(52.6813072384086,28.2029958664822,9.91488920083339));
#54703=CARTESIAN_POINT('Ctrl Pts',(52.7090422057637,28.1264563089838,9.91910376451835));
#54704=CARTESIAN_POINT('Ctrl Pts',(52.7405267611704,28.0514585233039,9.9233183282033));
#54705=CARTESIAN_POINT('Ctrl Pts',(52.77200120486,27.9764848242398,9.9275315383206));
#54706=CARTESIAN_POINT('Ctrl Pts',(52.8072226650356,27.9030523427262,9.9317447484379));
#54707=CARTESIAN_POINT('Ctrl Pts',(52.8460076353914,27.8315535342996,9.9359579585552));
#54708=CARTESIAN_POINT('Ctrl Pts',(52.8847920780597,27.7600556986472,9.94017111134983));
#54709=CARTESIAN_POINT('Ctrl Pts',(52.927139711311,27.6904918924786,9.94438426414447));
#54710=CARTESIAN_POINT('Ctrl Pts',(52.9728212478134,27.6232296645107,9.9485974169391));
#54711=CARTESIAN_POINT('Ctrl Pts',(53.0185477830497,27.5559011796845,9.95281471991247));
#54712=CARTESIAN_POINT('Ctrl Pts',(53.0676145196535,27.4908791881758,9.95703202288583));
#54713=CARTESIAN_POINT('Ctrl Pts',(53.1197493286007,27.4285014595289,9.9612493258592));
#54714=CARTESIAN_POINT('Ctrl Pts',(53.1719088452404,27.3660941688723,9.96546862749385));
#54715=CARTESIAN_POINT('Ctrl Pts',(53.2271390143538,27.3063339800033,9.96968792912851));
#54716=CARTESIAN_POINT('Ctrl Pts',(53.2851296666642,27.2495229250731,9.97390723076317));
#54717=CARTESIAN_POINT('Ctrl Pts',(53.3432245635654,27.1926097460083,9.97813411705768));
#54718=CARTESIAN_POINT('Ctrl Pts',(53.4040895099795,27.1386566038592,9.9823610033522));
#54719=CARTESIAN_POINT('Ctrl Pts',(53.4673801026197,27.0879261258639,9.98658788964671));
#54720=CARTESIAN_POINT('Ctrl Pts',(53.5273998501042,27.0398173888141,9.99059633130383));
#54721=CARTESIAN_POINT('Ctrl Pts',(53.5896004643821,26.9946066757912,9.99460477296094));
#54722=CARTESIAN_POINT('Ctrl Pts',(53.6536659988426,26.9524807675317,9.99861321461805));
#54723=CARTESIAN_POINT('Ctrl Pts',(53.7213144049457,26.9079989634947,10.0028458287895));
#54724=CARTESIAN_POINT('Ctrl Pts',(53.7912954463036,26.8667906133401,10.007078442961));
#54725=CARTESIAN_POINT('Ctrl Pts',(53.8632591990065,26.8291083395626,10.0113110571325));
#54726=CARTESIAN_POINT('Ctrl Pts',(53.9351203021732,26.7914798160104,10.0155376338773));
#54727=CARTESIAN_POINT('Ctrl Pts',(54.0089580914889,26.7573675930729,10.0197642106221));
#54728=CARTESIAN_POINT('Ctrl Pts',(54.0843939921836,26.7269808869148,10.0239907873669));
#54729=CARTESIAN_POINT('Ctrl Pts',(54.1597461677638,26.6966279064819,10.0282126731009));
#54730=CARTESIAN_POINT('Ctrl Pts',(54.2366925016168,26.6699923995052,10.0324345588349));
#54731=CARTESIAN_POINT('Ctrl Pts',(54.3148314290001,26.6472368841479,10.0366564445689));
#54732=CARTESIAN_POINT('Ctrl Pts',(54.3929176541002,26.6244967166801,10.040875482772));
#54733=CARTESIAN_POINT('Ctrl Pts',(54.4721944303176,26.6056314729265,10.045094520975));
#54734=CARTESIAN_POINT('Ctrl Pts',(54.5522430890643,26.5907544752124,10.049313559178));
#54735=CARTESIAN_POINT('Ctrl Pts',(54.6322656068374,26.5758823357833,10.053531219597));
#54736=CARTESIAN_POINT('Ctrl Pts',(54.7130590501692,26.5649959406935,10.057748880016));
#54737=CARTESIAN_POINT('Ctrl Pts',(54.7941939082545,26.5581576417384,10.0619665404349));
#54738=CARTESIAN_POINT('Ctrl Pts',(54.8753270779542,26.5513194850858,10.066184113086));
#54739=CARTESIAN_POINT('Ctrl Pts',(54.9568011852762,26.5485292949234,10.070401685737));
#54740=CARTESIAN_POINT('Ctrl Pts',(55.038182369416,26.5497974866012,10.0746192583881));
#54741=CARTESIAN_POINT('Ctrl Pts',(55.1197017026629,26.5510678311052,10.0788439906044));
#54742=CARTESIAN_POINT('Ctrl Pts',(55.2011273301845,26.5564103341134,10.0830687228207));
#54743=CARTESIAN_POINT('Ctrl Pts',(55.2820257766793,26.5657831420992,10.0872934550369));
#54744=CARTESIAN_POINT('Ctrl Pts',(55.3629040179388,26.5751536091279,10.0915171320821));
#54745=CARTESIAN_POINT('Ctrl Pts',(55.4432548851673,26.5885522705291,10.0957408091272));
#54746=CARTESIAN_POINT('Ctrl Pts',(55.5226547590382,26.6058859148205,10.0999644861723));
#54747=CARTESIAN_POINT('Ctrl Pts',(55.6021986921208,26.6232510084205,10.1041958264485));
#54748=CARTESIAN_POINT('Ctrl Pts',(55.6807877339682,26.6445652308838,10.1084271667248));
#54749=CARTESIAN_POINT('Ctrl Pts',(55.7580122977353,26.6696850842682,10.112658507001));
#54750=CARTESIAN_POINT('Ctrl Pts',(55.8350149167044,26.6947327427381,10.1168776863285));
#54751=CARTESIAN_POINT('Ctrl Pts',(55.9106604944123,26.7235639465777,10.121096865656));
#54752=CARTESIAN_POINT('Ctrl Pts',(55.984565470068,26.7559899543118,10.1253160449835));
#54753=CARTESIAN_POINT('Ctrl Pts',(56.0587057762799,26.7885192139631,10.129548659155));
#54754=CARTESIAN_POINT('Ctrl Pts',(56.1313701153078,26.8247872178455,10.1337812733265));
#54755=CARTESIAN_POINT('Ctrl Pts',(56.2021560821718,26.8646379688452,10.1380138874979));
#54756=CARTESIAN_POINT('Ctrl Pts',(56.2728410795005,26.9044318764905,10.1422404642427));
#54757=CARTESIAN_POINT('Ctrl Pts',(56.3416526246996,26.9477981552339,10.1464670409875));
#54758=CARTESIAN_POINT('Ctrl Pts',(56.4082091255623,26.9945331444566,10.1506936177323));
#54759=CARTESIAN_POINT('Ctrl Pts',(56.4746917564162,27.0412162632532,10.1549155034663));
#54760=CARTESIAN_POINT('Ctrl Pts',(56.5389239378018,27.0912603977723,10.1591373892003));
#54761=CARTESIAN_POINT('Ctrl Pts',(56.6005507332144,27.1444171803967,10.1633592749344));
#54762=CARTESIAN_POINT('Ctrl Pts',(56.6621359632645,27.1975381104196,10.1675783131374));
#54763=CARTESIAN_POINT('Ctrl Pts',(56.7211189465371,27.2537672163485,10.1717973513404));
#54764=CARTESIAN_POINT('Ctrl Pts',(56.7771767018898,27.312815001175,10.1760163895434));
#54765=CARTESIAN_POINT('Ctrl Pts',(56.8332161508234,27.3718435031478,10.1802340499624));
#54766=CARTESIAN_POINT('Ctrl Pts',(56.8863319493511,27.4336885193594,10.1844517103814));
#54767=CARTESIAN_POINT('Ctrl Pts',(56.936237969185,27.498023709679,10.1886693708003));
#54768=CARTESIAN_POINT('Ctrl Pts',(56.9861429504935,27.5623575612076,10.1928869434514));
#54769=CARTESIAN_POINT('Ctrl Pts',(57.0328380021068,27.6291811160359,10.1971045161025));
#54770=CARTESIAN_POINT('Ctrl Pts',(57.0760781931947,27.6981361109005,10.2013220887535));
#54771=CARTESIAN_POINT('Ctrl Pts',(57.1193917869232,27.7672081607219,10.2055468209698));
#54772=CARTESIAN_POINT('Ctrl Pts',(57.1592385378959,27.8384184941899,10.2097715531861));
#54773=CARTESIAN_POINT('Ctrl Pts',(57.1954175696032,27.9113807161924,10.2139962854024));
#54774=CARTESIAN_POINT('Ctrl Pts',(57.2315875652178,27.9843247151148,10.2182199624475));
#54775=CARTESIAN_POINT('Ctrl Pts',(57.2640915069243,28.0590192916598,10.2224436394926));
#54776=CARTESIAN_POINT('Ctrl Pts',(57.2927769641623,28.1350583588435,10.2266673165377));
#54777=CARTESIAN_POINT('Ctrl Pts',(57.321514466878,28.211235387557,10.2308986568139));
#54778=CARTESIAN_POINT('Ctrl Pts',(57.3464194971185,28.2887613383503,10.2351299970902));
#54779=CARTESIAN_POINT('Ctrl Pts',(57.3673894451691,28.3672145190494,10.2393613373664));
#54780=CARTESIAN_POINT('Ctrl Pts',(57.3882991252086,28.4454422238839,10.2435805166939));
#54781=CARTESIAN_POINT('Ctrl Pts',(57.405296297586,28.5245913734237,10.2477996960215));
#54782=CARTESIAN_POINT('Ctrl Pts',(57.4183304726086,28.6042374761897,10.252018875349));
#54783=CARTESIAN_POINT('Ctrl Pts',(57.4314061514626,28.6841371905896,10.2562514895205));
#54784=CARTESIAN_POINT('Ctrl Pts',(57.4405421596118,28.7648342018545,10.2604841036919));
#54785=CARTESIAN_POINT('Ctrl Pts',(57.445650281775,28.8459060375812,10.2647167178634));
#54786=CARTESIAN_POINT('Ctrl Pts',(57.4507511176815,28.9268622319465,10.2689432946082));
#54787=CARTESIAN_POINT('Ctrl Pts',(57.4518354497394,29.0081917291093,10.273169871353));
#54788=CARTESIAN_POINT('Ctrl Pts',(57.4488663745085,29.0894635668948,10.2773964480978));
#54789=CARTESIAN_POINT('Ctrl Pts',(57.4459005946073,29.1706452023514,10.2816183338318));
#54790=CARTESIAN_POINT('Ctrl Pts',(57.4388903634232,29.2517688436901,10.2858402195658));
#54791=CARTESIAN_POINT('Ctrl Pts',(57.4278507902601,29.3324015496857,10.2900621052999));
#54792=CARTESIAN_POINT('Ctrl Pts',(57.4168186629467,29.4129798714216,10.2942811435029));
#54793=CARTESIAN_POINT('Ctrl Pts',(57.4017626540284,29.4930674563818,10.2985001817059));
#54794=CARTESIAN_POINT('Ctrl Pts',(57.3827497697047,29.5722357774313,10.3027192199089));
#54795=CARTESIAN_POINT('Ctrl Pts',(57.3637430942958,29.6513782449936,10.3069368803279));
#54796=CARTESIAN_POINT('Ctrl Pts',(57.3407822180518,29.7296015934616,10.3111545407469));
#54797=CARTESIAN_POINT('Ctrl Pts',(57.3139851148365,29.8064881513791,10.3153722011658));
#54798=CARTESIAN_POINT('Ctrl Pts',(57.2871885692589,29.8833731093163,10.3195897738169));
#54799=CARTESIAN_POINT('Ctrl Pts',(57.2565561094307,29.9589208937306,10.3238073464679));
#54800=CARTESIAN_POINT('Ctrl Pts',(57.2222549150737,30.0327310116534,10.328024919119));
#54801=CARTESIAN_POINT('Ctrl Pts',(57.1878954925227,30.1066664263757,10.3322496513352));
#54802=CARTESIAN_POINT('Ctrl Pts',(57.1498550717141,30.1788578492762,10.3364743835515));
#54803=CARTESIAN_POINT('Ctrl Pts',(57.1083484132819,30.2489264262605,10.3406991157678));
#54804=CARTESIAN_POINT('Ctrl Pts',(57.0668521215728,30.318977502883,10.3449227928129));
#54805=CARTESIAN_POINT('Ctrl Pts',(57.0218915984879,30.3869064168714,10.349146469858));
#54806=CARTESIAN_POINT('Ctrl Pts',(56.973724496714,30.4523642315449,10.3533701469032));
#54807=CARTESIAN_POINT('Ctrl Pts',(56.9254700029283,30.5179408096461,10.3576014871794));
#54808=CARTESIAN_POINT('Ctrl Pts',(56.873997598167,30.5810369674196,10.3618328274556));
#54809=CARTESIAN_POINT('Ctrl Pts',(56.8196051476521,30.6413370636886,10.3660641677319));
#54810=CARTESIAN_POINT('Ctrl Pts',(56.765369022027,30.7014638563867,10.3702833470594));
#54811=CARTESIAN_POINT('Ctrl Pts',(56.7082299930118,30.7588103741959,10.3745025263869));
#54812=CARTESIAN_POINT('Ctrl Pts',(56.6485166481383,30.8131031715848,10.3787217057144));
#54813=CARTESIAN_POINT('Ctrl Pts',(56.5886131621475,30.8675688498126,10.3829543198859));
#54814=CARTESIAN_POINT('Ctrl Pts',(56.5258961235245,30.9191638819218,10.3871869340573));
#54815=CARTESIAN_POINT('Ctrl Pts',(56.4606718883087,30.9675842763919,10.3914195482288));
#54816=CARTESIAN_POINT('Ctrl Pts',(56.3955406893402,31.0159356037158,10.3956461249736));
#54817=CARTESIAN_POINT('Ctrl Pts',(56.3279097666342,31.0611210126294,10.3998727017184));
#54818=CARTESIAN_POINT('Ctrl Pts',(56.2581205318722,31.1028749314407,10.4040992784632));
#54819=CARTESIAN_POINT('Ctrl Pts',(56.1884087550794,31.1445825082371,10.4083211641972));
#54820=CARTESIAN_POINT('Ctrl Pts',(56.1165438226765,31.1828659252219,10.4125430499313));
#54821=CARTESIAN_POINT('Ctrl Pts',(56.0428971222023,31.2175021629081,10.4167649356653));
#54822=CARTESIAN_POINT('Ctrl Pts',(55.9693000941437,31.2521150395261,10.4209839738683));
#54823=CARTESIAN_POINT('Ctrl Pts',(55.8939241040826,31.2830854252455,10.4252030120713));
#54824=CARTESIAN_POINT('Ctrl Pts',(55.8171650896194,31.3102362360389,10.4294220502744));
#54825=CARTESIAN_POINT('Ctrl Pts',(55.7404311418517,31.3373781803675,10.4336397106933));
#54826=CARTESIAN_POINT('Ctrl Pts',(55.6623155042445,31.3607028721054,10.4378573711123));
#54827=CARTESIAN_POINT('Ctrl Pts',(55.5832327552187,31.3800818900282,10.4420750315313));
#54828=CARTESIAN_POINT('Ctrl Pts',(55.5041516518751,31.3994605046809,10.4462926041823));
#54829=CARTESIAN_POINT('Ctrl Pts',(55.4241039286052,31.414893499346,10.4505101768334));
#54830=CARTESIAN_POINT('Ctrl Pts',(55.3435165417897,31.4263030798968,10.4547277494844));
#54831=CARTESIAN_POINT('Ctrl Pts',(55.2627923533821,31.4377320288482,10.4589524817007));
#54832=CARTESIAN_POINT('Ctrl Pts',(55.1815271308917,31.4451238330451,10.463177213917));
#54833=CARTESIAN_POINT('Ctrl Pts',(55.1001555825528,31.4484523906508,10.4674019461333));
#54834=CARTESIAN_POINT('Ctrl Pts',(55.0188043576112,31.4517801169143,10.4716256231784));
#54835=CARTESIAN_POINT('Ctrl Pts',(54.9373473258697,31.4510466514572,10.4758493002235));
#54836=CARTESIAN_POINT('Ctrl Pts',(54.8562174505492,31.4462781584426,10.4800729772686));
#54837=CARTESIAN_POINT('Ctrl Pts',(54.7749403771879,31.4415010137097,10.4843043175449));
#54838=CARTESIAN_POINT('Ctrl Pts',(54.6939921096424,31.4326742612446,10.4885356578211));
#54839=CARTESIAN_POINT('Ctrl Pts',(54.6137995737617,31.4198759225988,10.4927669980974));
#54840=CARTESIAN_POINT('Ctrl Pts',(54.5338375126845,31.4071143666105,10.4969861774249));
#54841=CARTESIAN_POINT('Ctrl Pts',(54.4546272733771,31.3904041981347,10.5012053567524));
#54842=CARTESIAN_POINT('Ctrl Pts',(54.3765771121669,31.3698721807148,10.5054245360799));
#54843=CARTESIAN_POINT('Ctrl Pts',(54.2982784211698,31.3492747845969,10.5096571502514));
#54844=CARTESIAN_POINT('Ctrl Pts',(54.2208560002347,31.324754527491,10.5138897644229));
#54845=CARTESIAN_POINT('Ctrl Pts',(54.1447316255925,31.2964028953427,10.5181223785943));
#54846=CARTESIAN_POINT('Ctrl Pts',(54.0687158352229,31.2680917041356,10.5223489553391));
#54847=CARTESIAN_POINT('Ctrl Pts',(53.9939948454657,31.2359601530607,10.5265755320839));
#54848=CARTESIAN_POINT('Ctrl Pts',(53.9209772893505,31.2001500494063,10.5308021088287));
#54849=CARTESIAN_POINT('Ctrl Pts',(53.8480407742675,31.1643796908203,10.5350239945627));
#54850=CARTESIAN_POINT('Ctrl Pts',(53.7768043511669,31.1249390956278,10.5392458802968));
#54851=CARTESIAN_POINT('Ctrl Pts',(53.7076572780962,31.082018381077,10.5434677660308));
#54852=CARTESIAN_POINT('Ctrl Pts',(53.6385568425821,31.0391266152171,10.5476868042338));
#54853=CARTESIAN_POINT('Ctrl Pts',(53.571543351976,30.9927596361689,10.5519058424368));
#54854=CARTESIAN_POINT('Ctrl Pts',(53.506980897576,30.9431531616929,10.5561248806398));
#54855=CARTESIAN_POINT('Ctrl Pts',(53.4424395269197,30.8935628868827,10.5603425410588));
#54856=CARTESIAN_POINT('Ctrl Pts',(53.3803479709731,30.8407355003906,10.5645602014778));
#54857=CARTESIAN_POINT('Ctrl Pts',(53.3210396495258,30.7849488484367,10.5687778618967));
#54858=CARTESIAN_POINT('Ctrl Pts',(53.2617325622622,30.7291633573819,10.5729954345478));
#54859=CARTESIAN_POINT('Ctrl Pts',(53.2052089319147,30.6704190424451,10.5772130071988));
#54860=CARTESIAN_POINT('Ctrl Pts',(53.1517664495573,30.6090316942242,10.5814305798499));
#54861=CARTESIAN_POINT('Ctrl Pts',(53.0982332456,30.5475401375497,10.5856553120662));
#54862=CARTESIAN_POINT('Ctrl Pts',(53.0477919611186,30.4833969229783,10.5898800442825));
#54863=CARTESIAN_POINT('Ctrl Pts',(53.0007011465053,30.4169524848825,10.5941047764987));
#54864=CARTESIAN_POINT('Ctrl Pts',(52.9536220933168,30.3505246419819,10.5983284535438));
#54865=CARTESIAN_POINT('Ctrl Pts',(52.9098920688897,30.281797129621,10.602552130589));
#54866=CARTESIAN_POINT('Ctrl Pts',(52.8697248315904,30.211147372064,10.6067758076341));
#54867=CARTESIAN_POINT('Ctrl Pts',(52.8294847168386,30.1403694310744,10.6110071479103));
#54868=CARTESIAN_POINT('Ctrl Pts',(52.792820517365,30.0676626909834,10.6152384881866));
#54869=CARTESIAN_POINT('Ctrl Pts',(52.7598992055001,29.9934277429592,10.6194698284628));
#54870=CARTESIAN_POINT('Ctrl Pts',(52.727072510083,29.9194061475227,10.6236890077903));
#54871=CARTESIAN_POINT('Ctrl Pts',(52.6979673028113,29.8438655713314,10.6279081871178));
#54872=CARTESIAN_POINT('Ctrl Pts',(52.6726995063008,29.7672174802671,10.6321273664453));
#54873=CARTESIAN_POINT('Ctrl Pts',(52.6425523782678,29.6757682787574,10.6371612893411));
#54874=CARTESIAN_POINT('Ctrl Pts',(52.6177750447214,29.5824668337994,10.6421952122369));
#54875=CARTESIAN_POINT('Ctrl Pts',(52.5985610187568,29.4878945268862,10.6472291351327));
#54876=CARTESIAN_POINT('Ctrl Pts',(52.579555670576,29.3943493414858,10.6522083860989));
#54877=CARTESIAN_POINT('Ctrl Pts',(52.5659935010598,29.299560826227,10.6571876370652));
#54878=CARTESIAN_POINT('Ctrl Pts',(52.5580154729119,29.2041122717089,10.6621668880314));
#54879=CARTESIAN_POINT('Ctrl Pts',(52.5524045822788,29.1369839800369,10.6656687599336));
#54880=CARTESIAN_POINT('Ctrl Pts',(52.5495547759945,29.069529649616,10.6691706318358));
#54881=CARTESIAN_POINT('Ctrl Pts',(52.5495007823165,29.0019580941228,10.6726725037379));
#54882=CARTESIAN_POINT('',(52.5495005206114,28.9984026534493,11.4726725038167));
#54883=CARTESIAN_POINT('Ctrl Pts',(52.5495007823157,29.0019580931583,10.6726725037879));
#54884=CARTESIAN_POINT('Ctrl Pts',(52.5494359301699,28.9207974333899,10.6768786262003));
#54885=CARTESIAN_POINT('Ctrl Pts',(52.5534074481705,28.8395800658034,10.6810847486127));
#54886=CARTESIAN_POINT('Ctrl Pts',(52.5614055553208,28.7587379342298,10.6852908710251));
#54887=CARTESIAN_POINT('Ctrl Pts',(52.5694016866372,28.6779157737097,10.6894959543667));
#54888=CARTESIAN_POINT('Ctrl Pts',(52.5814223857094,28.5974691297911,10.6937010377083));
#54889=CARTESIAN_POINT('Ctrl Pts',(52.5974059177831,28.5178258342709,10.6979061210499));
#54890=CARTESIAN_POINT('Ctrl Pts',(52.6133904537395,28.4381775365697,10.7021114685015));
#54891=CARTESIAN_POINT('Ctrl Pts',(52.6333382235249,28.3593331452004,10.7063168159531));
#54892=CARTESIAN_POINT('Ctrl Pts',(52.6571364729459,28.2817098472068,10.7105221634047));
#54893=CARTESIAN_POINT('Ctrl Pts',(52.6809602811628,28.2040031835,10.7147320273069));
#54894=CARTESIAN_POINT('Ctrl Pts',(52.7086426895977,28.1275206795818,10.7189418912091));
#54895=CARTESIAN_POINT('Ctrl Pts',(52.7400213417708,28.0526633574339,10.7231517551112));
#54896=CARTESIAN_POINT('Ctrl Pts',(52.7714170884756,27.9777652543479,10.7273639124724));
#54897=CARTESIAN_POINT('Ctrl Pts',(52.8065128859592,27.9044945172938,10.7315760698336));
#54898=CARTESIAN_POINT('Ctrl Pts',(52.8450996785005,27.8332288765995,10.7357882271948));
#54899=CARTESIAN_POINT('Ctrl Pts',(52.8837567074427,27.761833516854,10.7400080516035));
#54900=CARTESIAN_POINT('Ctrl Pts',(52.9259171810606,27.6924509433078,10.7442278760122));
#54901=CARTESIAN_POINT('Ctrl Pts',(52.9713279963715,27.6254309214543,10.7484477004209));
#54902=CARTESIAN_POINT('Ctrl Pts',(53.0085710646733,27.5704653535739,10.7519085325509));
#54903=CARTESIAN_POINT('Ctrl Pts',(53.0479995146969,27.5170884186818,10.7553693646809));
#54904=CARTESIAN_POINT('Ctrl Pts',(53.089454357452,27.4654754489612,10.7588301968108));
#54905=CARTESIAN_POINT('Ctrl Pts',(53.1401538275023,27.4023525412707,10.7630628109823));
#54906=CARTESIAN_POINT('Ctrl Pts',(53.1940792366103,27.3416275503319,10.7672954251538));
#54907=CARTESIAN_POINT('Ctrl Pts',(53.2509752586573,27.2836484322345,10.7715280393253));
#54908=CARTESIAN_POINT('Ctrl Pts',(53.307790123871,27.2257520159052,10.7757546160701));
#54909=CARTESIAN_POINT('Ctrl Pts',(53.367566863529,27.1705940221001,10.7799811928148));
#54910=CARTESIAN_POINT('Ctrl Pts',(53.4300095449539,27.1184899093909,10.7842077695596));
#54911=CARTESIAN_POINT('Ctrl Pts',(53.4923829222331,27.0664436262132,10.7884296552936));
#54912=CARTESIAN_POINT('Ctrl Pts',(53.557416007092,27.0174447854202,10.7926515410277));
#54913=CARTESIAN_POINT('Ctrl Pts',(53.6247766352463,26.9717714756381,10.7968734267617));
#54914=CARTESIAN_POINT('Ctrl Pts',(53.6920918307458,26.9261289710869,10.8010924649647));
#54915=CARTESIAN_POINT('Ctrl Pts',(53.761731068165,26.8838078028496,10.8053115031677));
#54916=CARTESIAN_POINT('Ctrl Pts',(53.8333307849193,26.8450445033405,10.8095305413708));
#54917=CARTESIAN_POINT('Ctrl Pts',(53.9049071198164,26.8062938625119,10.8137482017897));
#54918=CARTESIAN_POINT('Ctrl Pts',(53.9784422544006,26.7710990040078,10.8179658622087));
#54919=CARTESIAN_POINT('Ctrl Pts',(54.0535466407057,26.7396512904685,10.8221835226276));
#54920=CARTESIAN_POINT('Ctrl Pts',(54.1286494641169,26.7082042313443,10.8264010952787));
#54921=CARTESIAN_POINT('Ctrl Pts',(54.2053210453675,26.6805043404856,10.8306186679297));
#54922=CARTESIAN_POINT('Ctrl Pts',(54.2831517320666,26.6566948959299,10.8348362405808));
#54923=CARTESIAN_POINT('Ctrl Pts',(54.3611145407053,26.6328450335118,10.839060972797));
#54924=CARTESIAN_POINT('Ctrl Pts',(54.4402399450273,26.6128989675693,10.8432857050133));
#54925=CARTESIAN_POINT('Ctrl Pts',(54.5201025922473,26.5969501195289,10.8475104372296));
#54926=CARTESIAN_POINT('Ctrl Pts',(54.5999452929337,26.5810052548805,10.8517341142747));
#54927=CARTESIAN_POINT('Ctrl Pts',(54.6805244040679,26.5690556590496,10.8559577913198));
#54928=CARTESIAN_POINT('Ctrl Pts',(54.7614081644119,26.5611428524838,10.8601814683649));
#54929=CARTESIAN_POINT('Ctrl Pts',(54.8424386762579,26.5532156893125,10.8644128086412));
#54930=CARTESIAN_POINT('Ctrl Pts',(54.9237744765769,26.5493399746473,10.8686441489174));
#54931=CARTESIAN_POINT('Ctrl Pts',(55.0049816993385,26.5495050637327,10.8728754891936));
#54932=CARTESIAN_POINT('Ctrl Pts',(55.0859555310684,26.5496696783491,10.8770946685211));
#54933=CARTESIAN_POINT('Ctrl Pts',(55.166801072977,26.5538517944617,10.8813138478487));
#54934=CARTESIAN_POINT('Ctrl Pts',(55.247095317281,26.5619897140952,10.8855330271762));
#54935=CARTESIAN_POINT('Ctrl Pts',(55.3276452370517,26.5701535467491,10.8897656413476));
#54936=CARTESIAN_POINT('Ctrl Pts',(55.4079399275819,26.5823288062798,10.8939982555191));
#54937=CARTESIAN_POINT('Ctrl Pts',(55.4875485147805,26.5984907462732,10.8982308696906));
#54938=CARTESIAN_POINT('Ctrl Pts',(55.5670435478046,26.6146296327769,10.9024574464354));
#54939=CARTESIAN_POINT('Ctrl Pts',(55.6458539697675,26.6347438137148,10.9066840231802));
#54940=CARTESIAN_POINT('Ctrl Pts',(55.7235540600729,26.6587567891926,10.910910599925));
#54941=CARTESIAN_POINT('Ctrl Pts',(55.8011679122755,26.6827431130481,10.915132485659));
#54942=CARTESIAN_POINT('Ctrl Pts',(55.8776734398775,26.7106194968103,10.919354371393));
#54943=CARTESIAN_POINT('Ctrl Pts',(55.9526565446198,26.74225870437,10.9235762571271));
#54944=CARTESIAN_POINT('Ctrl Pts',(56.0275890755831,26.7738765722654,10.9277952953301));
#54945=CARTESIAN_POINT('Ctrl Pts',(56.1010007961527,26.8092520433196,10.9320143335331));
#54946=CARTESIAN_POINT('Ctrl Pts',(56.1724953732078,26.8482089205022,10.9362333717361));
#54947=CARTESIAN_POINT('Ctrl Pts',(56.2439666027407,26.887153075789,10.9404510321551));
#54948=CARTESIAN_POINT('Ctrl Pts',(56.3135215244854,26.9296760924332,10.9446686925741));
#54949=CARTESIAN_POINT('Ctrl Pts',(56.380787548405,26.9755553857491,10.9488863529931));
#54950=CARTESIAN_POINT('Ctrl Pts',(56.4480521725441,27.0214337243342,10.9531039256441));
#54951=CARTESIAN_POINT('Ctrl Pts',(56.5130276104433,27.0706679379955,10.9573214982952));
#54952=CARTESIAN_POINT('Ctrl Pts',(56.5753706617782,27.1229924006525,10.9615390709462));
#54953=CARTESIAN_POINT('Ctrl Pts',(56.6378195439264,27.1754056870085,10.9657638031625));
#54954=CARTESIAN_POINT('Ctrl Pts',(56.6976267411355,27.2309194179019,10.9699885353788));
#54955=CARTESIAN_POINT('Ctrl Pts',(56.7544823267569,27.2892276553856,10.9742132675951));
#54956=CARTESIAN_POINT('Ctrl Pts',(56.8113237120996,27.3475213297754,10.9784369446402));
#54957=CARTESIAN_POINT('Ctrl Pts',(56.8652146676095,27.4086077513921,10.9826606216853));
#54958=CARTESIAN_POINT('Ctrl Pts',(56.9158853137214,27.4721473517821,10.9868842987304));
#54959=CARTESIAN_POINT('Ctrl Pts',(56.9666478941524,27.5358022352865,10.9911156390067));
#54960=CARTESIAN_POINT('Ctrl Pts',(57.0141782166597,27.601918814297,10.9953469792829));
#54961=CARTESIAN_POINT('Ctrl Pts',(57.058249013316,27.6701273560285,10.9995783195592));
#54962=CARTESIAN_POINT('Ctrl Pts',(57.1021931497031,27.7381398651735,11.0037974988867));
#54963=CARTESIAN_POINT('Ctrl Pts',(57.1426974634018,27.8082318926336,11.0080166782142));
#54964=CARTESIAN_POINT('Ctrl Pts',(57.1795834224522,27.8800150203813,11.0122358575417));
#54965=CARTESIAN_POINT('Ctrl Pts',(57.2165868349375,27.9520267222299,11.0164684717132));
#54966=CARTESIAN_POINT('Ctrl Pts',(57.2500864143564,28.0260081553786,11.0207010858847));
#54967=CARTESIAN_POINT('Ctrl Pts',(57.2798683504226,28.1015844198026,11.0249337000561));
#54968=CARTESIAN_POINT('Ctrl Pts',(57.3096078053533,28.1770528817816,11.0291602768009));
#54969=CARTESIAN_POINT('Ctrl Pts',(57.3356399802126,28.2541112282268,11.0333868535457));
#54970=CARTESIAN_POINT('Ctrl Pts',(57.3577972824058,28.3323607073578,11.0376134302905));
#54971=CARTESIAN_POINT('Ctrl Pts',(57.3799299925594,28.410523338628,11.0418353160245));
#54972=CARTESIAN_POINT('Ctrl Pts',(57.398196249521,28.4898740310127,11.0460572017586));
#54973=CARTESIAN_POINT('Ctrl Pts',(57.4124773467226,28.5699961610051,11.0502790874926));
#54974=CARTESIAN_POINT('Ctrl Pts',(57.426748811767,28.6500642511055,11.0544981256956));
#54975=CARTESIAN_POINT('Ctrl Pts',(57.4370403740825,28.7309022892708,11.0587171638986));
#54976=CARTESIAN_POINT('Ctrl Pts',(57.4432840681131,28.8120818994754,11.0629362021017));
#54977=CARTESIAN_POINT('Ctrl Pts',(57.4495257231808,28.8932349993791,11.0671538625206));
#54978=CARTESIAN_POINT('Ctrl Pts',(57.4517220995516,28.9747289869751,11.0713715229396));
#54979=CARTESIAN_POINT('Ctrl Pts',(57.4498570685586,29.0561301490586,11.0755891833586));
#54980=CARTESIAN_POINT('Ctrl Pts',(57.4479920763762,29.1375296172145,11.0798067560096));
#54981=CARTESIAN_POINT('Ctrl Pts',(57.4420658566851,29.2188357992994,11.0840243286607));
#54982=CARTESIAN_POINT('Ctrl Pts',(57.4321143848096,29.2996162031708,11.0882419013117));
#54983=CARTESIAN_POINT('Ctrl Pts',(57.4221460197545,29.3805337362913,11.092466633528));
#54984=CARTESIAN_POINT('Ctrl Pts',(57.4081387881945,29.4609232419479,11.0966913657443));
#54985=CARTESIAN_POINT('Ctrl Pts',(57.3901805942804,29.5403581929842,11.1009160979606));
#54986=CARTESIAN_POINT('Ctrl Pts',(57.3722268856136,29.6197733043086,11.1051397750057));
#54987=CARTESIAN_POINT('Ctrl Pts',(57.3503243337393,29.6982338944994,11.1093634520508));
#54988=CARTESIAN_POINT('Ctrl Pts',(57.32461085459,29.7753287204293,11.1135871290959));
#54989=CARTESIAN_POINT('Ctrl Pts',(57.2988507221733,29.8525634234056,11.1178184693721));
#54990=CARTESIAN_POINT('Ctrl Pts',(57.2692660136443,29.9284269759124,11.1220498096483));
#54991=CARTESIAN_POINT('Ctrl Pts',(57.2360431453476,30.0025274570525,11.1262811499246));
#54992=CARTESIAN_POINT('Ctrl Pts',(57.2029157601772,30.0764149720651,11.1305003292521));
#54993=CARTESIAN_POINT('Ctrl Pts',(57.1661713803383,30.1485491684762,11.1347195085796));
#54994=CARTESIAN_POINT('Ctrl Pts',(57.1260386277282,30.2185688340867,11.1389386879071));
#54995=CARTESIAN_POINT('Ctrl Pts',(57.0857780831406,30.2888114585264,11.1431713020786));
#54996=CARTESIAN_POINT('Ctrl Pts',(57.0419577887007,30.3571873027054,11.14740391625));
#54997=CARTESIAN_POINT('Ctrl Pts',(56.9947758215151,30.4233129212857,11.1516365304215));
#54998=CARTESIAN_POINT('Ctrl Pts',(56.9476611549754,30.4893442178802,11.1558631071663));
#54999=CARTESIAN_POINT('Ctrl Pts',(56.8971946069767,30.5531312888108,11.1600896839111));
#55000=CARTESIAN_POINT('Ctrl Pts',(56.8436194230284,30.6143164723908,11.1643162606559));
#55001=CARTESIAN_POINT('Ctrl Pts',(56.7901037013307,30.6754337475018,11.16853814639));
#55002=CARTESIAN_POINT('Ctrl Pts',(56.7334865037634,30.7339545255634,11.172760032124));
#55003=CARTESIAN_POINT('Ctrl Pts',(56.674052680683,30.7895524223387,11.176981917858));
#55004=CARTESIAN_POINT('Ctrl Pts',(56.6146589438731,30.8451128200567,11.181200956061));
#55005=CARTESIAN_POINT('Ctrl Pts',(56.5524526929481,30.8977539353105,11.1854199942641));
#55006=CARTESIAN_POINT('Ctrl Pts',(56.4877562600216,30.9471855486231,11.1896390324671));
#55007=CARTESIAN_POINT('Ctrl Pts',(56.4230809545914,30.9966010193729,11.1938566928861));
#55008=CARTESIAN_POINT('Ctrl Pts',(56.3559174509811,31.0428087878345,11.198074353305));
#55009=CARTESIAN_POINT('Ctrl Pts',(56.2866207783091,31.0855592110567,11.202292013724));
#55010=CARTESIAN_POINT('Ctrl Pts',(56.2173255476745,31.1283087446588,11.206509586375));
#55011=CARTESIAN_POINT('Ctrl Pts',(56.1458976322195,31.16760083316,11.2107271590261));
#55012=CARTESIAN_POINT('Ctrl Pts',(56.0727194022594,31.2032302044989,11.2149447316771));
#55013=CARTESIAN_POINT('Ctrl Pts',(55.999416948165,31.2389200586865,11.2191694638934));
#55014=CARTESIAN_POINT('Ctrl Pts',(55.9243586546465,31.2709345511826,11.2233941961097));
#55015=CARTESIAN_POINT('Ctrl Pts',(55.8479501585332,31.2991152164786,11.227618928326));
#55016=CARTESIAN_POINT('Ctrl Pts',(55.7715607462432,31.3272888433579,11.2318426053711));
#55017=CARTESIAN_POINT('Ctrl Pts',(55.6938222569342,31.3516304388611,11.2360662824162));
#55018=CARTESIAN_POINT('Ctrl Pts',(55.6151547332607,31.3720318092612,11.2402899594613));
#55019=CARTESIAN_POINT('Ctrl Pts',(55.5363444791156,31.3924701949007,11.2445212997376));
#55020=CARTESIAN_POINT('Ctrl Pts',(55.4566022782557,31.4089539741919,11.2487526400138));
#55021=CARTESIAN_POINT('Ctrl Pts',(55.376358369025,31.421426155815,11.2529839802901));
#55022=CARTESIAN_POINT('Ctrl Pts',(55.2963450822454,31.4338624921618,11.2572031596176));
#55023=CARTESIAN_POINT('Ctrl Pts',(55.2158334285267,31.442310294073,11.2614223389451));
#55024=CARTESIAN_POINT('Ctrl Pts',(55.135250863719,31.446764691151,11.2656415182726));
#55025=CARTESIAN_POINT('Ctrl Pts',(55.0544117053652,31.4512332720608,11.2698741324441));
#55026=CARTESIAN_POINT('Ctrl Pts',(54.9732005186985,31.4516995683122,11.2741067466156));
#55027=CARTESIAN_POINT('Ctrl Pts',(54.8920467806782,31.448120984028,11.2783393607871));
#55028=CARTESIAN_POINT('Ctrl Pts',(54.8110088008456,31.4445475042582,11.2825659375318));
#55029=CARTESIAN_POINT('Ctrl Pts',(54.7300285671472,31.4369406235007,11.2867925142766));
#55030=CARTESIAN_POINT('Ctrl Pts',(54.6495385182799,31.4253096709143,11.2910190910214));
#55031=CARTESIAN_POINT('Ctrl Pts',(54.5691378040462,31.4136916273384,11.2952409767554));
#55032=CARTESIAN_POINT('Ctrl Pts',(54.4892266510763,31.3980584524738,11.2994628624894));
#55033=CARTESIAN_POINT('Ctrl Pts',(54.4102339114659,31.3784714021437,11.3036847482234));
#55034=CARTESIAN_POINT('Ctrl Pts',(54.3312944500087,31.3588975626715,11.3079037864265));
#55035=CARTESIAN_POINT('Ctrl Pts',(54.2532726213765,31.33537525568,11.3121228246295));
#55036=CARTESIAN_POINT('Ctrl Pts',(54.1765873468506,31.3080168657602,11.3163418628325));
#55037=CARTESIAN_POINT('Ctrl Pts',(54.0999271149397,31.2806674100932,11.3205595232515));
#55038=CARTESIAN_POINT('Ctrl Pts',(54.0246030075348,31.2494845153099,11.3247771836704));
#55039=CARTESIAN_POINT('Ctrl Pts',(53.9510177095794,31.2146300829674,11.3289948440894));
#55040=CARTESIAN_POINT('Ctrl Pts',(53.8774339429061,31.1797763759323,11.3332124167404));
#55041=CARTESIAN_POINT('Ctrl Pts',(53.8055893330701,31.1412514831673,11.3374299893915));
#55042=CARTESIAN_POINT('Ctrl Pts',(53.7358642301629,31.0992643962632,11.3416475620425));
#55043=CARTESIAN_POINT('Ctrl Pts',(53.6660207649975,31.057206033933,11.3458722942588));
#55044=CARTESIAN_POINT('Ctrl Pts',(53.5983044055407,31.0116739593304,11.3500970264751));
#55045=CARTESIAN_POINT('Ctrl Pts',(53.5330689056756,30.9629221621105,11.3543217586914));
#55046=CARTESIAN_POINT('Ctrl Pts',(53.4678496990608,30.9141825411631,11.3585454357365));
#55047=CARTESIAN_POINT('Ctrl Pts',(53.4051104584196,30.8622251194076,11.3627691127816));
#55048=CARTESIAN_POINT('Ctrl Pts',(53.3451706109395,30.8073433384671,11.3669927898267));
#55049=CARTESIAN_POINT('Ctrl Pts',(53.285122011559,30.7523619827326,11.371224130103));
#55050=CARTESIAN_POINT('Ctrl Pts',(53.227883283205,30.6944459956986,11.3754554703792));
#55051=CARTESIAN_POINT('Ctrl Pts',(53.1737364537357,30.6339252460214,11.3796868106555));
#55052=CARTESIAN_POINT('Ctrl Pts',(53.1197452432368,30.573578434077,11.383905989983));
#55053=CARTESIAN_POINT('Ctrl Pts',(53.0688284046793,30.5106422180089,11.3881251693105));
#55054=CARTESIAN_POINT('Ctrl Pts',(53.0212227307852,30.4454725071196,11.392344348638));
#55055=CARTESIAN_POINT('Ctrl Pts',(52.9731764547246,30.3796996346016,11.3966025775031));
#55056=CARTESIAN_POINT('Ctrl Pts',(52.9283239109816,30.3114067320381,11.4008608063682));
#55057=CARTESIAN_POINT('Ctrl Pts',(52.8869376870544,30.2409342898031,11.4051190352333));
#55058=CARTESIAN_POINT('Ctrl Pts',(52.8456116405283,30.1705643176176,11.4093710724452));
#55059=CARTESIAN_POINT('Ctrl Pts',(52.8077421333248,30.0980214899934,11.4136231096571));
#55060=CARTESIAN_POINT('Ctrl Pts',(52.7735599568789,30.0236771875875,11.417875146869));
#55061=CARTESIAN_POINT('Ctrl Pts',(52.7394174626113,29.949419191677,11.4221222478798));
#55062=CARTESIAN_POINT('Ctrl Pts',(52.7089539847439,29.8733642885634,11.4263693488905));
#55063=CARTESIAN_POINT('Ctrl Pts',(52.6823549572621,29.7959093578243,11.4306164499013));
#55064=CARTESIAN_POINT('Ctrl Pts',(52.655780257259,29.7185252673887,11.4348596665121));
#55065=CARTESIAN_POINT('Ctrl Pts',(52.6330631283781,29.6397441259724,11.439102883123));
#55066=CARTESIAN_POINT('Ctrl Pts',(52.6143407820955,29.5599824515353,11.4433460997339));
#55067=CARTESIAN_POINT('Ctrl Pts',(52.5956282896561,29.4802627568275,11.4475870830781));
#55068=CARTESIAN_POINT('Ctrl Pts',(52.5809065043712,29.3995639991901,11.4518280664224));
#55069=CARTESIAN_POINT('Ctrl Pts',(52.5702623683183,29.3183163382389,11.4560690497666));
#55070=CARTESIAN_POINT('Ctrl Pts',(52.5596194925028,29.2370782967946,11.4603095309897));
#55071=CARTESIAN_POINT('Ctrl Pts',(52.5530533688563,29.1552919337269,11.4645500122128));
#55072=CARTESIAN_POINT('Ctrl Pts',(52.5505993707982,29.073394874928,11.4687904934359));
#55073=CARTESIAN_POINT('Ctrl Pts',(52.5498505213662,29.0484035894794,11.4700844968866));
#55074=CARTESIAN_POINT('Ctrl Pts',(52.5494842248953,29.023402023579,11.4713785003372));
#55075=CARTESIAN_POINT('Ctrl Pts',(52.549500520611,28.9984026540067,11.4726725037879));
#55076=CARTESIAN_POINT('',(52.5495001173786,28.9992415326165,12.2726725037456));
#55077=CARTESIAN_POINT('Ctrl Pts',(52.5495005206114,28.9984026534493,11.4726725038167));
#55078=CARTESIAN_POINT('Ctrl Pts',(52.5495606642625,28.906135896561,11.477448364322));
#55079=CARTESIAN_POINT('Ctrl Pts',(52.5548359378858,28.8140684437107,11.4822242248273));
#55080=CARTESIAN_POINT('Ctrl Pts',(52.5652348152121,28.7227478675557,11.4870000853325));
#55081=CARTESIAN_POINT('Ctrl Pts',(52.5756840754274,28.6309848403263,11.4917990850327));
#55082=CARTESIAN_POINT('Ctrl Pts',(52.5913065778112,28.5399761496053,11.4965980847329));
#55083=CARTESIAN_POINT('Ctrl Pts',(52.6119599482221,28.4502591873394,11.5013970844331));
#55084=CARTESIAN_POINT('Ctrl Pts',(52.6327297929416,28.360036267889,11.5062231480052));
#55085=CARTESIAN_POINT('Ctrl Pts',(52.6585872906741,28.2711198859228,11.5110492115772));
#55086=CARTESIAN_POINT('Ctrl Pts',(52.6893395576657,28.1840351905681,11.5158752751493));
#55087=CARTESIAN_POINT('Ctrl Pts',(52.6960768106901,28.164956544193,11.516932576434));
#55088=CARTESIAN_POINT('Ctrl Pts',(52.7030488182106,28.1459657252688,11.5179898777187));
#55089=CARTESIAN_POINT('Ctrl Pts',(52.7102532547224,28.1270681054685,11.5190471790034));
#55090=CARTESIAN_POINT('Ctrl Pts',(52.7390942298718,28.0514166950975,11.5232797931749));
#55091=CARTESIAN_POINT('Ctrl Pts',(52.7717420592589,27.9770554585001,11.5275124073464));
#55092=CARTESIAN_POINT('Ctrl Pts',(52.8080607394415,27.9043939905138,11.5317450215179));
#55093=CARTESIAN_POINT('Ctrl Pts',(52.844327614437,27.831836167289,11.5359715982626));
#55094=CARTESIAN_POINT('Ctrl Pts',(52.8842547346398,27.7609737092658,11.5401981750074));
#55095=CARTESIAN_POINT('Ctrl Pts',(52.9276574665477,27.6921977695216,11.5444247517522));
#55096=CARTESIAN_POINT('Ctrl Pts',(52.971012026449,27.6234981631065,11.5486466374862));
#55097=CARTESIAN_POINT('Ctrl Pts',(53.0178342864838,27.556880864373,11.5528685232203));
#55098=CARTESIAN_POINT('Ctrl Pts',(53.0678936484504,27.4927126032831,11.5570904089543));
#55099=CARTESIAN_POINT('Ctrl Pts',(53.1179192469296,27.4285876216954,11.5613094471573));
#55100=CARTESIAN_POINT('Ctrl Pts',(53.1711773260632,27.3669087624622,11.5655284853603));
#55101=CARTESIAN_POINT('Ctrl Pts',(53.2273946353952,27.3080128631179,11.5697475235634));
#55102=CARTESIAN_POINT('Ctrl Pts',(53.2835935862037,27.2491361970271,11.5739651839823));
#55103=CARTESIAN_POINT('Ctrl Pts',(53.3427495275366,27.1930410217581,11.5781828444013));
#55104=CARTESIAN_POINT('Ctrl Pts',(53.4045505967253,27.1400291799089,11.5824005048203));
#55105=CARTESIAN_POINT('Ctrl Pts',(53.4663503798572,27.087018441216,11.5866180774713));
#55106=CARTESIAN_POINT('Ctrl Pts',(53.5307948280387,27.0370912099325,11.5908356501224));
#55107=CARTESIAN_POINT('Ctrl Pts',(53.5975381665936,26.990509752241,11.5950532227734));
#55108=CARTESIAN_POINT('Ctrl Pts',(53.664394805695,26.9438492199224,11.5992779549897));
#55109=CARTESIAN_POINT('Ctrl Pts',(53.7335577602002,26.9005460920931,11.603502687206));
#55110=CARTESIAN_POINT('Ctrl Pts',(53.8046509895121,26.8608200185291,11.6077274194223));
#55111=CARTESIAN_POINT('Ctrl Pts',(53.8757264625446,26.8211038669686,11.6119510964674));
#55112=CARTESIAN_POINT('Ctrl Pts',(53.9487308190989,26.7849631708519,11.6161747735125));
#55113=CARTESIAN_POINT('Ctrl Pts',(54.0232659662694,26.7525701618622,11.6203984505577));
#55114=CARTESIAN_POINT('Ctrl Pts',(54.0979363463315,26.720118380596,11.6246297908339));
#55115=CARTESIAN_POINT('Ctrl Pts',(54.1741426315099,26.6914280394162,11.6288611311102));
#55116=CARTESIAN_POINT('Ctrl Pts',(54.2514686906535,26.6666223775548,11.6330924713864));
#55117=CARTESIAN_POINT('Ctrl Pts',(54.3285725132999,26.6418880076157,11.6373116507139));
#55118=CARTESIAN_POINT('Ctrl Pts',(54.4067892207011,26.621016054546,11.6415308300414));
#55119=CARTESIAN_POINT('Ctrl Pts',(54.4856973206717,26.6040778384856,11.6457500093689));
#55120=CARTESIAN_POINT('Ctrl Pts',(54.5648566823047,26.5870856872231,11.6499826235404));
#55121=CARTESIAN_POINT('Ctrl Pts',(54.6450062681451,26.5739891929746,11.6542152377119));
#55122=CARTESIAN_POINT('Ctrl Pts',(54.7257284593265,26.5648972563819,11.6584478518834));
#55123=CARTESIAN_POINT('Ctrl Pts',(54.8063355078815,26.555818288583,11.6626744286282));
#55124=CARTESIAN_POINT('Ctrl Pts',(54.8875130817777,26.5507325849851,11.666901005373));
#55125=CARTESIAN_POINT('Ctrl Pts',(54.9688325573186,26.5496982143996,11.6711275821177));
#55126=CARTESIAN_POINT('Ctrl Pts',(55.0500617776582,26.5486649918456,11.6753494678518));
#55127=CARTESIAN_POINT('Ctrl Pts',(55.1314321245319,26.5516741736254,11.6795713535858));
#55128=CARTESIAN_POINT('Ctrl Pts',(55.2125104377487,26.558731976237,11.6837932393198));
#55129=CARTESIAN_POINT('Ctrl Pts',(55.2935340661576,26.5657850185795,11.6880122775228));
#55130=CARTESIAN_POINT('Ctrl Pts',(55.3742655905007,26.5768812182241,11.6922313157259));
#55131=CARTESIAN_POINT('Ctrl Pts',(55.454273705188,26.5919747404201,11.6964503539289));
#55132=CARTESIAN_POINT('Ctrl Pts',(55.5342556921421,26.6070633336221,11.7006680143479));
#55133=CARTESIAN_POINT('Ctrl Pts',(55.6135142824507,26.6261465709193,11.7048856747668));
#55134=CARTESIAN_POINT('Ctrl Pts',(55.6916265046396,26.6491271773914,11.7091033351858));
#55135=CARTESIAN_POINT('Ctrl Pts',(55.7697371013428,26.6721073056457,11.7133209078369));
#55136=CARTESIAN_POINT('Ctrl Pts',(55.8467009320274,26.6989845095815,11.7175384804879));
#55137=CARTESIAN_POINT('Ctrl Pts',(55.9221097611905,26.7296115225986,11.7217560531389));
#55138=CARTESIAN_POINT('Ctrl Pts',(55.9976466010547,26.7602905266816,11.7259807853552));
#55139=CARTESIAN_POINT('Ctrl Pts',(56.0716227253,26.7947319000186,11.7302055175715));
#55140=CARTESIAN_POINT('Ctrl Pts',(56.1436491693487,26.8327397877855,11.7344302497878));
#55141=CARTESIAN_POINT('Ctrl Pts',(56.2156576240378,26.8707381826839,11.7386539268329));
#55142=CARTESIAN_POINT('Ctrl Pts',(56.2857169822456,26.9123010545674,11.742877603878));
#55143=CARTESIAN_POINT('Ctrl Pts',(56.3534660495926,26.9571882361313,11.7471012809231));
#55144=CARTESIAN_POINT('Ctrl Pts',(56.4213380375029,27.0021568587816,11.7513326211994));
#55145=CARTESIAN_POINT('Ctrl Pts',(56.486890982561,27.0504615684061,11.7555639614756));
#55146=CARTESIAN_POINT('Ctrl Pts',(56.5497949664561,27.1018203952346,11.7597953017519));
#55147=CARTESIAN_POINT('Ctrl Pts',(56.6125181631599,27.1530316158628,11.7640144810794));
#55148=CARTESIAN_POINT('Ctrl Pts',(56.6726073225128,27.2072790551564,11.7682336604069));
#55149=CARTESIAN_POINT('Ctrl Pts',(56.7297731586964,27.2642479815788,11.7724528397344));
#55150=CARTESIAN_POINT('Ctrl Pts',(56.7871210241398,27.3213983102546,11.7766854539058));
#55151=CARTESIAN_POINT('Ctrl Pts',(56.8417401930594,27.3815000627959,11.7809180680773));
#55152=CARTESIAN_POINT('Ctrl Pts',(56.893311964802,27.4442622155589,11.7851506822488));
#55153=CARTESIAN_POINT('Ctrl Pts',(56.9448101742546,27.5069348440041,11.7893772589936));
#55154=CARTESIAN_POINT('Ctrl Pts',(56.9932693274113,27.572259979749,11.7936038357384));
#55155=CARTESIAN_POINT('Ctrl Pts',(57.0384073716024,27.6399096951317,11.7978304124832));
#55156=CARTESIAN_POINT('Ctrl Pts',(57.0834953177914,27.7074843271639,11.8020522982172));
#55157=CARTESIAN_POINT('Ctrl Pts',(57.1252692226447,27.7773780278716,11.8062741839512));
#55158=CARTESIAN_POINT('Ctrl Pts',(57.1634880588499,27.8492308358259,11.8104960696852));
#55159=CARTESIAN_POINT('Ctrl Pts',(57.2016811176353,27.9210351812894,11.8147151078883));
#55160=CARTESIAN_POINT('Ctrl Pts',(57.2363236523884,27.9947956005885,11.8189341460913));
#55161=CARTESIAN_POINT('Ctrl Pts',(57.2672193073435,28.0701253512386,11.8231531842943));
#55162=CARTESIAN_POINT('Ctrl Pts',(57.298104872904,28.1454305019386,11.8273708447133));
#55163=CARTESIAN_POINT('Ctrl Pts',(57.3252458125059,28.222303536749,11.8315885051322));
#55164=CARTESIAN_POINT('Ctrl Pts',(57.3484934567948,28.3003366999819,11.8358061655512));
#55165=CARTESIAN_POINT('Ctrl Pts',(57.371740617309,28.3783682393742,11.8400237382023));
#55166=CARTESIAN_POINT('Ctrl Pts',(57.3910945120833,28.4575594136433,11.8442413108533));
#55167=CARTESIAN_POINT('Ctrl Pts',(57.4064564283203,28.5374876124947,11.8484588835043));
#55168=CARTESIAN_POINT('Ctrl Pts',(57.4218444222685,28.6175514939297,11.8526836157206));
#55169=CARTESIAN_POINT('Ctrl Pts',(57.4332267911302,28.6983544445862,11.8569083479369));
#55170=CARTESIAN_POINT('Ctrl Pts',(57.4405560702434,28.7794635676397,11.8611330801532));
#55171=CARTESIAN_POINT('Ctrl Pts',(57.4478835187922,28.860552432839,11.8653567571983));
#55172=CARTESIAN_POINT('Ctrl Pts',(57.4511599044275,28.941946850884,11.8695804342434));
#55173=CARTESIAN_POINT('Ctrl Pts',(57.4503900510317,29.0232130955424,11.8738041112885));
#55174=CARTESIAN_POINT('Ctrl Pts',(57.449618800852,29.1046267856634,11.8780354515648));
#55175=CARTESIAN_POINT('Ctrl Pts',(57.4447866679591,29.1859113725751,11.882266791841));
#55176=CARTESIAN_POINT('Ctrl Pts',(57.4359505679149,29.266636607905,11.8864981321173));
#55177=CARTESIAN_POINT('Ctrl Pts',(57.4271398629826,29.3471298374439,11.8907173114448));
#55178=CARTESIAN_POINT('Ctrl Pts',(57.4143483291803,29.4270664898922,11.8949364907723));
#55179=CARTESIAN_POINT('Ctrl Pts',(57.3976824838279,29.5060325649054,11.8991556700998));
#55180=CARTESIAN_POINT('Ctrl Pts',(57.3809635705649,29.5852500861869,11.9033882842713));
#55181=CARTESIAN_POINT('Ctrl Pts',(57.3602834239191,29.6637854655181,11.9076208984428));
#55182=CARTESIAN_POINT('Ctrl Pts',(57.3357126609721,29.7412129352451,11.9118535126142));
#55183=CARTESIAN_POINT('Ctrl Pts',(57.3111769459114,29.8185299619567,11.916080089359));
#55184=CARTESIAN_POINT('Ctrl Pts',(57.282761776114,29.8947417786923,11.9203066661038));
#55185=CARTESIAN_POINT('Ctrl Pts',(57.2505886758749,29.9694332684737,11.9245332428486));
#55186=CARTESIAN_POINT('Ctrl Pts',(57.2184512840515,30.0440418593505,11.9287551285826));
#55187=CARTESIAN_POINT('Ctrl Pts',(57.1825644321438,30.117133051607,11.9329770143167));
#55188=CARTESIAN_POINT('Ctrl Pts',(57.1430988494162,30.1883087021608,11.9371989000507));
#55189=CARTESIAN_POINT('Ctrl Pts',(57.1036598850002,30.2594363469456,11.9414179382537));
#55190=CARTESIAN_POINT('Ctrl Pts',(57.0606472083586,30.3286506107748,11.9456369764568));
#55191=CARTESIAN_POINT('Ctrl Pts',(57.0142783326064,30.395576242558,11.9498560146598));
#55192=CARTESIAN_POINT('Ctrl Pts',(56.9679245992385,30.46248001887,11.9540736750787));
#55193=CARTESIAN_POINT('Ctrl Pts',(56.918217107734,30.5270962658345,11.9582913354977));
#55194=CARTESIAN_POINT('Ctrl Pts',(56.8654169581344,30.5890782933212,11.9625089959167));
#55195=CARTESIAN_POINT('Ctrl Pts',(56.8126179072858,30.6510590309854,11.9667265685677));
#55196=CARTESIAN_POINT('Ctrl Pts',(56.7567266284403,30.7104053052919,11.9709441412188));
#55197=CARTESIAN_POINT('Ctrl Pts',(56.6980438784476,30.7668042440708,11.9751617138698));
#55198=CARTESIAN_POINT('Ctrl Pts',(56.6392615112077,30.8232989231997,11.9793864460861));
#55199=CARTESIAN_POINT('Ctrl Pts',(56.5776785285335,30.8768359328346,11.9836111783024));
#55200=CARTESIAN_POINT('Ctrl Pts',(56.5136322154018,30.9271397890391,11.9878359105187));
#55201=CARTESIAN_POINT('Ctrl Pts',(56.4496018985084,30.9774310813281,11.9920595875638));
#55202=CARTESIAN_POINT('Ctrl Pts',(56.3831098742635,31.0244905830628,11.9962832646089));
#55203=CARTESIAN_POINT('Ctrl Pts',(56.3145225892979,31.0680862197272,12.000506941654));
#55204=CARTESIAN_POINT('Ctrl Pts',(56.2458108629482,31.1117609541627,12.0047382819303));
#55205=CARTESIAN_POINT('Ctrl Pts',(56.1749966838042,31.1519590338415,12.0089696222065));
#55206=CARTESIAN_POINT('Ctrl Pts',(56.1024719399326,31.1884939734121,12.0132009624828));
#55207=CARTESIAN_POINT('Ctrl Pts',(56.030155633491,31.2249239109034,12.0174201418103));
#55208=CARTESIAN_POINT('Ctrl Pts',(55.9561390315075,31.2577116276957,12.0216393211378));
#55209=CARTESIAN_POINT('Ctrl Pts',(55.88082739603,31.2867210910828,12.0258585004653));
#55210=CARTESIAN_POINT('Ctrl Pts',(55.8052759508661,31.3158229273188,12.0300911146368));
#55211=CARTESIAN_POINT('Ctrl Pts',(55.7281402049313,31.341230622434,12.0343237288083));
#55212=CARTESIAN_POINT('Ctrl Pts',(55.6498157468709,31.3627716235639,12.0385563429798));
#55213=CARTESIAN_POINT('Ctrl Pts',(55.5716030112957,31.3842818984782,12.0427829197245));
#55214=CARTESIAN_POINT('Ctrl Pts',(55.4922053754433,31.4019363116889,12.0470094964693));
#55215=CARTESIAN_POINT('Ctrl Pts',(55.4120372078317,31.4156108108225,12.0512360732141));
#55216=CARTESIAN_POINT('Ctrl Pts',(55.3319580176029,31.4292701328455,12.0554579589482));
#55217=CARTESIAN_POINT('Ctrl Pts',(55.2511104505239,31.4389582401283,12.0596798446822));
#55218=CARTESIAN_POINT('Ctrl Pts',(55.1699214242054,31.4446015952699,12.0639017304162));
#55219=CARTESIAN_POINT('Ctrl Pts',(55.0887871573675,31.4502411441435,12.0681207686192));
#55220=CARTESIAN_POINT('Ctrl Pts',(55.0073123509276,31.4518413269117,12.0723398068223));
#55221=CARTESIAN_POINT('Ctrl Pts',(54.9259301892824,31.4493803120668,12.0765588450253));
#55222=CARTESIAN_POINT('Ctrl Pts',(54.8445746040842,31.4469201008996,12.0807765054443));
#55223=CARTESIAN_POINT('Ctrl Pts',(54.7633120675775,31.4404013399797,12.0849941658632));
#55224=CARTESIAN_POINT('Ctrl Pts',(54.6825755352627,31.4298543082223,12.0892118262822));
#55225=CARTESIAN_POINT('Ctrl Pts',(54.6018406830445,31.4193074959446,12.0934293989332));
#55226=CARTESIAN_POINT('Ctrl Pts',(54.5216322737369,31.4047326408381,12.0976469715843));
#55227=CARTESIAN_POINT('Ctrl Pts',(54.4423764846801,31.3862116974741,12.1018645442353));
#55228=CARTESIAN_POINT('Ctrl Pts',(54.3629861544929,31.3676593137739,12.1060892764516));
#55229=CARTESIAN_POINT('Ctrl Pts',(54.284552134791,31.345147545538,12.1103140086679));
#55230=CARTESIAN_POINT('Ctrl Pts',(54.2074891266635,31.3188093422365,12.1145387408842));
#55231=CARTESIAN_POINT('Ctrl Pts',(54.1304453658304,31.2924777171776,12.1187624179293));
#55232=CARTESIAN_POINT('Ctrl Pts',(54.0547723569769,31.2623217605063,12.1229860949744));
#55233=CARTESIAN_POINT('Ctrl Pts',(53.980864263903,31.2285225153473,12.1272097720195));
#55234=CARTESIAN_POINT('Ctrl Pts',(53.9068220756335,31.1946619465065,12.1314411122958));
#55235=CARTESIAN_POINT('Ctrl Pts',(53.8345516160845,31.1571450935697,12.135672452572));
#55236=CARTESIAN_POINT('Ctrl Pts',(53.764422658053,31.116199159358,12.1399037928482));
#55237=CARTESIAN_POINT('Ctrl Pts',(53.6944952519194,31.075370904504,12.1441229721757));
#55238=CARTESIAN_POINT('Ctrl Pts',(53.6266973901279,31.0311335709704,12.1483421515033));
#55239=CARTESIAN_POINT('Ctrl Pts',(53.5613638053301,30.9837530464717,12.1525613308308));
#55240=CARTESIAN_POINT('Ctrl Pts',(53.4963354145064,30.9365938514869,12.1567608010284));
#55241=CARTESIAN_POINT('Ctrl Pts',(53.4334980409898,30.8861391378274,12.1609602712261));
#55242=CARTESIAN_POINT('Ctrl Pts',(53.3732086710378,30.8326211343356,12.1651597414237));
#55243=CARTESIAN_POINT('Ctrl Pts',(53.3130055443728,30.7791796877648,12.169353204325));
#55244=CARTESIAN_POINT('Ctrl Pts',(53.2553435354469,30.7226839619698,12.1735466672263));
#55245=CARTESIAN_POINT('Ctrl Pts',(53.2005494727727,30.6634085637815,12.1777401301276));
#55246=CARTESIAN_POINT('Ctrl Pts',(53.145817827864,30.6042006881991,12.1819288161138));
#55247=CARTESIAN_POINT('Ctrl Pts',(53.0939479577934,30.5422197763119,12.1861175021));
#55248=CARTESIAN_POINT('Ctrl Pts',(53.0452313089151,30.4777786080311,12.1903061880862));
#55249=CARTESIAN_POINT('Ctrl Pts',(52.9965444562646,30.4133768534574,12.1944923121753));
#55250=CARTESIAN_POINT('Ctrl Pts',(52.9510072821594,30.3465182045079,12.1986784362644));
#55251=CARTESIAN_POINT('Ctrl Pts',(52.9088714062374,30.277549002719,12.2028645603535));
#55252=CARTESIAN_POINT('Ctrl Pts',(52.8667479021659,30.2086000515275,12.2070494553214));
#55253=CARTESIAN_POINT('Ctrl Pts',(52.8280239595776,30.1375421810614,12.2112343502892));
#55254=CARTESIAN_POINT('Ctrl Pts',(52.7929073850718,30.064749942066,12.215419245257));
#55255=CARTESIAN_POINT('Ctrl Pts',(52.7577899543323,29.9919559282056,12.2196042422635));
#55256=CARTESIAN_POINT('Ctrl Pts',(52.7262802696761,29.9174278885332,12.22378923927));
#55257=CARTESIAN_POINT('Ctrl Pts',(52.6985390761442,29.8415627522442,12.2279742362765));
#55258=CARTESIAN_POINT('Ctrl Pts',(52.6707711704879,29.7656245650623,12.2321632630361));
#55259=CARTESIAN_POINT('Ctrl Pts',(52.6467791619605,29.6883471559616,12.2363522897958));
#55260=CARTESIAN_POINT('Ctrl Pts',(52.6266744719774,29.6101443993322,12.2405413165554));
#55261=CARTESIAN_POINT('Ctrl Pts',(52.6065591563653,29.5319003113775,12.2447325572782));
#55262=CARTESIAN_POINT('Ctrl Pts',(52.5903353428762,29.4527303656458,12.248923798001));
#55263=CARTESIAN_POINT('Ctrl Pts',(52.5780631744243,29.3730579886831,12.2531150387239));
#55264=CARTESIAN_POINT('Ctrl Pts',(52.5657711586025,29.2932567602349,12.2573130578009));
#55265=CARTESIAN_POINT('Ctrl Pts',(52.5574435931298,29.2129519484643,12.261511076878));
#55266=CARTESIAN_POINT('Ctrl Pts',(52.5530886379128,29.1325708719454,12.2657090959551));
#55267=CARTESIAN_POINT('Ctrl Pts',(52.5506807300774,29.0881271947278,12.2680302318852));
#55268=CARTESIAN_POINT('Ctrl Pts',(52.5494863691203,29.0436601934439,12.2703513678154));
#55269=CARTESIAN_POINT('Ctrl Pts',(52.5495001173787,28.9992415326165,12.2726725037456));
#55270=CARTESIAN_POINT('',(52.5495009826471,29.0021945278826,13.0726725037477));
#55271=CARTESIAN_POINT('Ctrl Pts',(52.5495001173789,28.999241531807,12.2726725037879));
#55272=CARTESIAN_POINT('Ctrl Pts',(52.5495131316829,28.9571942176884,12.274869722924));
#55273=CARTESIAN_POINT('Ctrl Pts',(52.5506082944952,28.9151651062863,12.2770669420601));
#55274=CARTESIAN_POINT('Ctrl Pts',(52.5527831953695,28.8731924247765,12.2792641611962));
#55275=CARTESIAN_POINT('Ctrl Pts',(52.5569728167463,28.7923383289532,12.2834967753677));
#55276=CARTESIAN_POINT('Ctrl Pts',(52.565181565129,28.7115417280223,12.2877293895392));
#55277=CARTESIAN_POINT('Ctrl Pts',(52.5774059298484,28.631234191842,12.2919620037107));
#55278=CARTESIAN_POINT('Ctrl Pts',(52.5896128576594,28.5510412068216,12.2961885804556));
#55279=CARTESIAN_POINT('Ctrl Pts',(52.6058239561334,28.4713363564607,12.3004151572004));
#55280=CARTESIAN_POINT('Ctrl Pts',(52.6259837702042,28.3925486104503,12.3046417339452));
#55281=CARTESIAN_POINT('Ctrl Pts',(52.6461212092157,28.3138483097146,12.3088636196792));
#55282=CARTESIAN_POINT('Ctrl Pts',(52.6701985409968,28.2360635385855,12.3130855054132));
#55283=CARTESIAN_POINT('Ctrl Pts',(52.6981090637492,28.1596141555175,12.3173073911473));
#55284=CARTESIAN_POINT('Ctrl Pts',(52.7260007617196,28.0832163351875,12.3215264293503));
#55285=CARTESIAN_POINT('Ctrl Pts',(52.7577203569904,28.0081525493439,12.3257454675533));
#55286=CARTESIAN_POINT('Ctrl Pts',(52.7931113718505,27.9348273224756,12.3299645057563));
#55287=CARTESIAN_POINT('Ctrl Pts',(52.8284908292955,27.861526040953,12.3341821661753));
#55288=CARTESIAN_POINT('Ctrl Pts',(52.8675391235118,27.7899626089347,12.3383998265943));
#55289=CARTESIAN_POINT('Ctrl Pts',(52.9100522768151,27.7205201195976,12.3426174870132));
#55290=CARTESIAN_POINT('Ctrl Pts',(52.9525645454359,27.6510790753325,12.3468350596643));
#55291=CARTESIAN_POINT('Ctrl Pts',(52.9985412862296,27.5837592815786,12.3510526323153));
#55292=CARTESIAN_POINT('Ctrl Pts',(53.0477340858412,27.5189165957267,12.3552702049664));
#55293=CARTESIAN_POINT('Ctrl Pts',(53.0970103929788,27.4539638357925,12.3594949371826));
#55294=CARTESIAN_POINT('Ctrl Pts',(53.1495133997465,27.3914969690868,12.3637196693989));
#55295=CARTESIAN_POINT('Ctrl Pts',(53.2049527921878,27.3318406036215,12.3679444016152));
#55296=CARTESIAN_POINT('Ctrl Pts',(53.2603783380597,27.272199137959,12.3721680786603));
#55297=CARTESIAN_POINT('Ctrl Pts',(53.3187384542129,27.2153670798025,12.3763917557054));
#55298=CARTESIAN_POINT('Ctrl Pts',(53.3797072659948,27.1616306937588,12.3806154327505));
#55299=CARTESIAN_POINT('Ctrl Pts',(53.4407866965791,27.1077968110688,12.3848467730267));
#55300=CARTESIAN_POINT('Ctrl Pts',(53.5044839172587,27.0570701153811,12.3890781133029));
#55301=CARTESIAN_POINT('Ctrl Pts',(53.5704408284431,27.00969579586,12.3933094535792));
#55302=CARTESIAN_POINT('Ctrl Pts',(53.6362081782675,26.9624576309931,12.3975286329066));
#55303=CARTESIAN_POINT('Ctrl Pts',(53.7042218195668,26.9185527754667,12.4017478122341));
#55304=CARTESIAN_POINT('Ctrl Pts',(53.7741025915781,26.8781786611441,12.4059669915616));
#55305=CARTESIAN_POINT('Ctrl Pts',(53.8442058801495,26.8376759862922,12.4101996057331));
#55306=CARTESIAN_POINT('Ctrl Pts',(53.9164489565371,26.8005759568308,12.4144322199045));
#55307=CARTESIAN_POINT('Ctrl Pts',(53.9904678978455,26.7671105749009,12.418664834076));
#55308=CARTESIAN_POINT('Ctrl Pts',(54.064381258084,26.733692928196,12.4228914108208));
#55309=CARTESIAN_POINT('Ctrl Pts',(54.1400650323931,26.7038998217604,12.4271179875656));
#55310=CARTESIAN_POINT('Ctrl Pts',(54.2171292003915,26.677918269931,12.4313445643104));
#55311=CARTESIAN_POINT('Ctrl Pts',(54.2941078360873,26.6519655546154,12.4355664500444));
#55312=CARTESIAN_POINT('Ctrl Pts',(54.3724633832531,26.6298161358043,12.4397883357784));
#55313=CARTESIAN_POINT('Ctrl Pts',(54.4517855654801,26.6116090806185,12.4440102215125));
#55314=CARTESIAN_POINT('Ctrl Pts',(54.5310542473551,26.5934143055268,12.4482292597155));
#55315=CARTESIAN_POINT('Ctrl Pts',(54.6112878178253,26.5791567167086,12.4524482979185));
#55316=CARTESIAN_POINT('Ctrl Pts',(54.6920617649522,26.5689252801702,12.4566673361215));
#55317=CARTESIAN_POINT('Ctrl Pts',(54.772809334253,26.5586971848459,12.4608849965405));
#55318=CARTESIAN_POINT('Ctrl Pts',(54.8540964692445,26.5524926890319,12.4651026569595));
#55319=CARTESIAN_POINT('Ctrl Pts',(54.9354907760897,26.5503492473354,12.4693203173785));
#55320=CARTESIAN_POINT('Ctrl Pts',(55.0168833891502,26.548205850243,12.4735378900295));
#55321=CARTESIAN_POINT('Ctrl Pts',(55.0983827052123,26.5501233502976,12.4777554626806));
#55322=CARTESIAN_POINT('Ctrl Pts',(55.1795549856887,26.5560871011605,12.4819730353316));
#55323=CARTESIAN_POINT('Ctrl Pts',(55.2608650606469,26.5620609758237,12.4861977675479));
#55324=CARTESIAN_POINT('Ctrl Pts',(55.3418465235327,26.5720948098158,12.4904224997642));
#55325=CARTESIAN_POINT('Ctrl Pts',(55.4220690378045,26.5861217973297,12.4946472319805));
#55326=CARTESIAN_POINT('Ctrl Pts',(55.5022715156622,26.6001452814564,12.4988709090256));
#55327=CARTESIAN_POINT('Ctrl Pts',(55.5817149740569,26.6181598008781,12.5030945860707));
#55328=CARTESIAN_POINT('Ctrl Pts',(55.6599818805912,26.6400478463979,12.5073182631158));
#55329=CARTESIAN_POINT('Ctrl Pts',(55.7383907907371,26.661975604507,12.5115496033921));
#55330=CARTESIAN_POINT('Ctrl Pts',(55.8156184410779,26.6877907860973,12.5157809436683));
#55331=CARTESIAN_POINT('Ctrl Pts',(55.8912642110511,26.7173264893771,12.5200122839446));
#55332=CARTESIAN_POINT('Ctrl Pts',(55.9666925737087,26.7467773065098,12.5242314632721));
#55333=CARTESIAN_POINT('Ctrl Pts',(56.0405477552908,26.7799270258922,12.5284506425996));
#55334=CARTESIAN_POINT('Ctrl Pts',(56.1124577295447,26.8165650799769,12.5326698219271));
#55335=CARTESIAN_POINT('Ctrl Pts',(56.184596681808,26.8533197981096,12.5369024360986));
#55336=CARTESIAN_POINT('Ctrl Pts',(56.2550463114903,26.8937218271381,12.5411350502701));
#55337=CARTESIAN_POINT('Ctrl Pts',(56.3234138894252,26.937592201509,12.5453676644416));
#55338=CARTESIAN_POINT('Ctrl Pts',(56.3916839474295,26.9813999989101,12.5495942411864));
#55339=CARTESIAN_POINT('Ctrl Pts',(56.4578774644656,27.0286660669415,12.5538208179312));
#55340=CARTESIAN_POINT('Ctrl Pts',(56.5216252407799,27.0791650574239,12.558047394676));
#55341=CARTESIAN_POINT('Ctrl Pts',(56.5853022644443,27.1296079998745,12.56226928041));
#55342=CARTESIAN_POINT('Ctrl Pts',(56.6465385787679,27.1832764480855,12.566491166144));
#55343=CARTESIAN_POINT('Ctrl Pts',(56.7049941759336,27.2399019601078,12.570713051878));
#55344=CARTESIAN_POINT('Ctrl Pts',(56.7634103466118,27.2964892799782,12.5749320900811));
#55345=CARTESIAN_POINT('Ctrl Pts',(56.819049192248,27.3560293801257,12.5791511282841));
#55346=CARTESIAN_POINT('Ctrl Pts',(56.8716049812702,27.4182146023924,12.5833701664871));
#55347=CARTESIAN_POINT('Ctrl Pts',(56.9241436074878,27.4803795172328,12.5875878269061));
#55348=CARTESIAN_POINT('Ctrl Pts',(56.9736008769283,27.5451874842039,12.591805487325));
#55349=CARTESIAN_POINT('Ctrl Pts',(57.0197099761688,27.6122961907653,12.596023147744));
#55350=CARTESIAN_POINT('Ctrl Pts',(57.0658181158963,27.6794035008199,12.600240720395));
#55351=CARTESIAN_POINT('Ctrl Pts',(57.1085779618512,27.7488110717251,12.6044582930461));
#55352=CARTESIAN_POINT('Ctrl Pts',(57.1477656721151,27.8201470991332,12.6086758656971));
#55353=CARTESIAN_POINT('Ctrl Pts',(57.1870199057069,27.8916042234338,12.6129005979134));
#55354=CARTESIAN_POINT('Ctrl Pts',(57.2226896463142,27.9649959447701,12.6171253301297));
#55355=CARTESIAN_POINT('Ctrl Pts',(57.2545966567732,28.0399249168596,12.621350062346));
#55356=CARTESIAN_POINT('Ctrl Pts',(57.2864956981217,28.1148351746525,12.6255737393911));
#55357=CARTESIAN_POINT('Ctrl Pts',(57.3146337475737,28.1912814706043,12.6297974164362));
#55358=CARTESIAN_POINT('Ctrl Pts',(57.3388820698342,28.2688495959051,12.6340210934813));
#55359=CARTESIAN_POINT('Ctrl Pts',(57.3631743870536,28.3465584569833,12.6382524337576));
#55360=CARTESIAN_POINT('Ctrl Pts',(57.3835627565969,28.4253927640143,12.6424837740338));
#55361=CARTESIAN_POINT('Ctrl Pts',(57.3999690817405,28.5049256048937,12.64671511431));
#55362=CARTESIAN_POINT('Ctrl Pts',(57.4163282548078,28.5842298669453,12.6509342936375));
#55363=CARTESIAN_POINT('Ctrl Pts',(57.4287282543084,28.6642281903906,12.6551534729651));
#55364=CARTESIAN_POINT('Ctrl Pts',(57.4371431782213,28.7444938770808,12.6593726522926));
#55365=CARTESIAN_POINT('Ctrl Pts',(57.4455848972006,28.8250151483037,12.663605266464));
#55366=CARTESIAN_POINT('Ctrl Pts',(57.4500474912131,28.9061049721206,12.6678378806355));
#55367=CARTESIAN_POINT('Ctrl Pts',(57.450467279005,28.9873364884079,12.672070494807));
#55368=CARTESIAN_POINT('Ctrl Pts',(57.450886468009,29.0684521355645,12.6762970715518));
#55369=CARTESIAN_POINT('Ctrl Pts',(57.4472743017879,29.1497086130906,12.6805236482966));
#55370=CARTESIAN_POINT('Ctrl Pts',(57.4396188154356,29.2306735471884,12.6847502250414));
#55371=CARTESIAN_POINT('Ctrl Pts',(57.4319718257868,29.3115486195849,12.6889721107754));
#55372=CARTESIAN_POINT('Ctrl Pts',(57.4202904764019,29.3921323313502,12.6931939965094));
#55373=CARTESIAN_POINT('Ctrl Pts',(57.4046148426304,29.4719933353362,12.6974158822434));
#55374=CARTESIAN_POINT('Ctrl Pts',(57.3889497815877,29.5518004755516,12.7016349204465));
#55375=CARTESIAN_POINT('Ctrl Pts',(57.3692958759655,29.6308854214205,12.7058539586495));
#55376=CARTESIAN_POINT('Ctrl Pts',(57.3457447566737,29.7088242282385,12.7100729968525));
#55377=CARTESIAN_POINT('Ctrl Pts',(57.3222013283188,29.7867375830837,12.7142906572715));
#55378=CARTESIAN_POINT('Ctrl Pts',(57.2947633480454,29.8635050978406,12.7185083176904));
#55379=CARTESIAN_POINT('Ctrl Pts',(57.2635727028055,29.9387166074561,12.7227259781094));
#55380=CARTESIAN_POINT('Ctrl Pts',(57.2323827066312,30.0139265519484,12.7269435507604));
#55381=CARTESIAN_POINT('Ctrl Pts',(57.1974403797963,30.0875801270172,12.7311611234115));
#55382=CARTESIAN_POINT('Ctrl Pts',(57.1589357414466,30.1592871578277,12.7353786960625));
#55383=CARTESIAN_POINT('Ctrl Pts',(57.1203657393218,30.2311159153298,12.7396034282788));
#55384=CARTESIAN_POINT('Ctrl Pts',(57.0782215475278,30.300991105875,12.7438281604951));
#55385=CARTESIAN_POINT('Ctrl Pts',(57.0327394376947,30.3685469039973,12.7480528927114));
#55386=CARTESIAN_POINT('Ctrl Pts',(56.9872686874955,30.4360858293506,12.7522765697565));
#55387=CARTESIAN_POINT('Ctrl Pts',(56.9384619827175,30.5013061602331,12.7565002468016));
#55388=CARTESIAN_POINT('Ctrl Pts',(56.8865966885616,30.5638744146218,12.7607239238467));
#55389=CARTESIAN_POINT('Ctrl Pts',(56.8346372925762,30.6265561897625,12.764955264123));
#55390=CARTESIAN_POINT('Ctrl Pts',(56.7796085318711,30.6865759287903,12.7691866043992));
#55391=CARTESIAN_POINT('Ctrl Pts',(56.7218259951699,30.743635710909,12.7734179446755));
#55392=CARTESIAN_POINT('Ctrl Pts',(56.6642095265277,30.8005315021786,12.777637124003));
#55393=CARTESIAN_POINT('Ctrl Pts',(56.6038554843972,30.854484086363,12.7818563033305));
#55394=CARTESIAN_POINT('Ctrl Pts',(56.5411076928689,30.9052394413774,12.786075482658));
#55395=CARTESIAN_POINT('Ctrl Pts',(56.4781600978426,30.9561564131951,12.7903080968295));
#55396=CARTESIAN_POINT('Ctrl Pts',(56.4125693477172,31.0040451150984,12.794540711001));
#55397=CARTESIAN_POINT('Ctrl Pts',(56.3446588354071,31.0486197466494,12.7987733251724));
#55398=CARTESIAN_POINT('Ctrl Pts',(56.2768451910662,31.0931307966737,12.8029999019172));
#55399=CARTESIAN_POINT('Ctrl Pts',(56.2067187416237,31.1343369124013,12.807226478662));
#55400=CARTESIAN_POINT('Ctrl Pts',(56.1346356594244,31.1719926727231,12.8114530554068));
#55401=CARTESIAN_POINT('Ctrl Pts',(56.0626325810993,31.2096066395112,12.8156749411409));
#55402=CARTESIAN_POINT('Ctrl Pts',(55.9886775947289,31.2436778666138,12.8198968268749));
#55403=CARTESIAN_POINT('Ctrl Pts',(55.9131543422353,31.2740051445097,12.8241187126089));
#55404=CARTESIAN_POINT('Ctrl Pts',(55.8376820278334,31.3043119675972,12.8283377508119));
#55405=CARTESIAN_POINT('Ctrl Pts',(55.7606439780632,31.3308796840387,12.832556789015));
#55406=CARTESIAN_POINT('Ctrl Pts',(55.6824456923792,31.353554360314,12.836775827218));
#55407=CARTESIAN_POINT('Ctrl Pts',(55.6042729434042,31.3762216318668,12.840993487637));
#55408=CARTESIAN_POINT('Ctrl Pts',(55.5249411567974,31.3949982587529,12.8452111480559));
#55409=CARTESIAN_POINT('Ctrl Pts',(55.4448716327238,31.4097799651416,12.8494288084749));
#55410=CARTESIAN_POINT('Ctrl Pts',(55.3648037748668,31.4245613639285,12.853646381126));
#55411=CARTESIAN_POINT('Ctrl Pts',(55.2839986671085,31.4353479243268,12.857863953777));
#55412=CARTESIAN_POINT('Ctrl Pts',(55.2028870445195,31.4420866276949,12.8620815264281));
#55413=CARTESIAN_POINT('Ctrl Pts',(55.121637730419,31.4488367703885,12.8663062586444));
#55414=CARTESIAN_POINT('Ctrl Pts',(55.0400813258277,31.4515252691936,12.8705309908606));
#55415=CARTESIAN_POINT('Ctrl Pts',(54.9586533208412,31.4501511590354,12.8747557230769));
#55416=CARTESIAN_POINT('Ctrl Pts',(54.8772456533528,31.4487773920756,12.878979400122));
#55417=CARTESIAN_POINT('Ctrl Pts',(54.7959667850363,31.4433430975585,12.8832030771672));
#55418=CARTESIAN_POINT('Ctrl Pts',(54.7152474468644,31.4338993885292,12.8874267542123));
#55419=CARTESIAN_POINT('Ctrl Pts',(54.63438165551,31.4244385453004,12.8916580944885));
#55420=CARTESIAN_POINT('Ctrl Pts',(54.5540778825753,31.4109538269064,12.8958894347648));
#55421=CARTESIAN_POINT('Ctrl Pts',(54.4747578382954,31.3935477688085,12.900120775041));
#55422=CARTESIAN_POINT('Ctrl Pts',(54.3956657612624,31.3761917360374,12.9043399543685));
#55423=CARTESIAN_POINT('Ctrl Pts',(54.3175521833678,31.3549370732523,12.908559133696));
#55424=CARTESIAN_POINT('Ctrl Pts',(54.2408173628565,31.3299338989465,12.9127783130235));
#55425=CARTESIAN_POINT('Ctrl Pts',(54.1638382009078,31.3048511087438,12.917010927195));
#55426=CARTESIAN_POINT('Ctrl Pts',(54.0879602923918,31.2759025807811,12.9212435413664));
#55427=CARTESIAN_POINT('Ctrl Pts',(54.0135994292889,31.2432039952044,12.9254761555379));
#55428=CARTESIAN_POINT('Ctrl Pts',(53.9393446349751,31.2105520510897,12.9297027322827));
#55429=CARTESIAN_POINT('Ctrl Pts',(53.8666030099624,31.1741608588139,12.9339293090275));
#55430=CARTESIAN_POINT('Ctrl Pts',(53.7957743201799,31.1341955772754,12.9381558857723));
#55431=CARTESIAN_POINT('Ctrl Pts',(53.7250242420413,31.0942746525715,12.9423777715063));
#55432=CARTESIAN_POINT('Ctrl Pts',(53.6561832830115,31.0507877478164,12.9465996572403));
#55433=CARTESIAN_POINT('Ctrl Pts',(53.5896290776845,31.0039471329072,12.9508215429744));
#55434=CARTESIAN_POINT('Ctrl Pts',(53.523119761105,30.9571381105401,12.9550405811774));
#55435=CARTESIAN_POINT('Ctrl Pts',(53.4588945139114,30.9069801371739,12.9592596193804));
#55436=CARTESIAN_POINT('Ctrl Pts',(53.3973032136534,30.8537295544481,12.9634786575834));
#55437=CARTESIAN_POINT('Ctrl Pts',(53.3357320268686,30.8004963614212,12.9676963180024));
#55438=CARTESIAN_POINT('Ctrl Pts',(53.2767934299597,30.7441728682958,12.9719139784213));
#55439=CARTESIAN_POINT('Ctrl Pts',(53.2208042482739,30.6850557044323,12.9761316388403));
#55440=CARTESIAN_POINT('Ctrl Pts',(53.1648162317018,30.6259397707746,12.9803492114913));
#55441=CARTESIAN_POINT('Ctrl Pts',(53.1117778269088,30.5640306200612,12.9845667841424));
#55442=CARTESIAN_POINT('Ctrl Pts',(53.0619679997887,30.4996607003442,12.9887843567934));
#55443=CARTESIAN_POINT('Ctrl Pts',(53.0120736177038,30.4351815090918,12.9930090890097));
#55444=CARTESIAN_POINT('Ctrl Pts',(52.9654190646665,30.3682335603809,12.997233821226));
#55445=CARTESIAN_POINT('Ctrl Pts',(52.9222422313652,30.2991816289025,13.0014585534423));
#55446=CARTESIAN_POINT('Ctrl Pts',(52.8790761819308,30.2301469438683,13.0056822304874));
#55447=CARTESIAN_POINT('Ctrl Pts',(52.8393863238212,30.1590097443526,13.0099059075325));
#55448=CARTESIAN_POINT('Ctrl Pts',(52.8033642724133,30.0861591643446,13.0141295845776));
#55449=CARTESIAN_POINT('Ctrl Pts',(52.7672768643736,30.0131764078405,13.0183609248539));
#55450=CARTESIAN_POINT('Ctrl Pts',(52.7348707476153,29.938474485681,13.0225922651301));
#55451=CARTESIAN_POINT('Ctrl Pts',(52.7062894921986,29.8624629594375,13.0268236054064));
#55452=CARTESIAN_POINT('Ctrl Pts',(52.6777903798286,29.7866698916994,13.0310427847339));
#55453=CARTESIAN_POINT('Ctrl Pts',(52.6530942323866,29.7095751964007,13.0352619640614));
#55454=CARTESIAN_POINT('Ctrl Pts',(52.6322930276046,29.6315963448834,13.0394811433889));
#55455=CARTESIAN_POINT('Ctrl Pts',(52.6050199400275,29.5293559184811,13.0450130367821));
#55456=CARTESIAN_POINT('Ctrl Pts',(52.5843565008141,29.4252836172886,13.0505449301752));
#55457=CARTESIAN_POINT('Ctrl Pts',(52.5705005679496,29.3201292858624,13.0560768235684));
#55458=CARTESIAN_POINT('Ctrl Pts',(52.5566446350851,29.2149749544363,13.0616087169615));
#55459=CARTESIAN_POINT('Ctrl Pts',(52.5495963971629,29.1087382537186,13.0671406103546));
#55460=CARTESIAN_POINT('Ctrl Pts',(52.5495009826471,29.0021945278826,13.0726725037477));
#55461=CARTESIAN_POINT('',(52.5495001938469,28.9990252981815,13.8726725038318));
#55462=CARTESIAN_POINT('Ctrl Pts',(52.5495009826464,29.0021945271091,13.0726725037879));
#55463=CARTESIAN_POINT('Ctrl Pts',(52.5494289300536,28.9217376454537,13.0768499331819));
#55464=CARTESIAN_POINT('Ctrl Pts',(52.5533235784428,28.841186950602,13.081027362576));
#55465=CARTESIAN_POINT('Ctrl Pts',(52.5611859230216,28.7609683118659,13.08520479197));
#55466=CARTESIAN_POINT('Ctrl Pts',(52.5690438911062,28.6807943260201,13.0893798960404));
#55467=CARTESIAN_POINT('Ctrl Pts',(52.580865127151,28.6009525014319,13.0935550001108));
#55468=CARTESIAN_POINT('Ctrl Pts',(52.5965985987663,28.5218661750641,13.0977301041812));
#55469=CARTESIAN_POINT('Ctrl Pts',(52.6123283691213,28.4427984535589,13.1019042260687));
#55470=CARTESIAN_POINT('Ctrl Pts',(52.6319684549278,28.3644863432227,13.1060783479562));
#55471=CARTESIAN_POINT('Ctrl Pts',(52.6554165300878,28.28734398016,13.1102524698437));
#55472=CARTESIAN_POINT('Ctrl Pts',(52.6788666251593,28.2101949717435,13.1144269513069));
#55473=CARTESIAN_POINT('Ctrl Pts',(52.7061252202815,28.1342163645467,13.11860143277));
#55474=CARTESIAN_POINT('Ctrl Pts',(52.7370403045377,28.0598065801586,13.1227759142332));
#55475=CARTESIAN_POINT('Ctrl Pts',(52.7679875097762,27.9853194834994,13.1269547330109));
#55476=CARTESIAN_POINT('Ctrl Pts',(52.8025986026244,27.9124049018382,13.1311335517887));
#55477=CARTESIAN_POINT('Ctrl Pts',(52.8406739506139,27.8414400048152,13.1353123705664));
#55478=CARTESIAN_POINT('Ctrl Pts',(52.8787716922654,27.7704333704478,13.1394936470776));
#55479=CARTESIAN_POINT('Ctrl Pts',(52.9203374967399,27.7013791082765,13.1436749235887));
#55480=CARTESIAN_POINT('Ctrl Pts',(52.9651277559891,27.6346263513037,13.1478562000999));
#55481=CARTESIAN_POINT('Ctrl Pts',(53.0099918254053,27.5677635920176,13.1520443669645));
#55482=CARTESIAN_POINT('Ctrl Pts',(53.0580906682687,27.5032102855713,13.1562325338291));
#55483=CARTESIAN_POINT('Ctrl Pts',(53.1091401107616,27.4412828578382,13.1604207006937));
#55484=CARTESIAN_POINT('Ctrl Pts',(53.132556232595,27.4128770590317,13.162341791714));
#55485=CARTESIAN_POINT('Ctrl Pts',(53.1565926487538,27.3850232386561,13.1642628827342));
#55486=CARTESIAN_POINT('Ctrl Pts',(53.1812194676012,27.3577492198306,13.1661839737544));
#55487=CARTESIAN_POINT('Ctrl Pts',(53.2354781265375,27.2976581583562,13.1704165879259));
#55488=CARTESIAN_POINT('Ctrl Pts',(53.2928189273524,27.2401472304043,13.1746492020974));
#55489=CARTESIAN_POINT('Ctrl Pts',(53.3529668841377,27.1855490733412,13.1788818162689));
#55490=CARTESIAN_POINT('Ctrl Pts',(53.4130290455103,27.1310287954227,13.1831083930137));
#55491=CARTESIAN_POINT('Ctrl Pts',(53.475890068994,27.0794133460753,13.1873349697584));
#55492=CARTESIAN_POINT('Ctrl Pts',(53.5412363057285,27.0310005753491,13.1915615465032));
#55493=CARTESIAN_POINT('Ctrl Pts',(53.6065100157072,26.9826415371924,13.1957834322373));
#55494=CARTESIAN_POINT('Ctrl Pts',(53.6742630868148,26.9374783898175,13.2000053179713));
#55495=CARTESIAN_POINT('Ctrl Pts',(53.7441478561528,26.8957695841961,13.2042272037053));
#55496=CARTESIAN_POINT('Ctrl Pts',(53.8139854903811,26.8540889098706,13.2084462419083));
#55497=CARTESIAN_POINT('Ctrl Pts',(53.8859515694386,26.8158581874815,13.2126652801113));
#55498=CARTESIAN_POINT('Ctrl Pts',(53.9596694832852,26.7812925686355,13.2168843183144));
#55499=CARTESIAN_POINT('Ctrl Pts',(54.0333633235488,26.7467382376605,13.2211019787333));
#55500=CARTESIAN_POINT('Ctrl Pts',(54.1088074421907,26.7158468303473,13.2253196391523));
#55501=CARTESIAN_POINT('Ctrl Pts',(54.185601894513,26.6887869038578,13.2295372995712));
#55502=CARTESIAN_POINT('Ctrl Pts',(54.2623947487719,26.6617275404751,13.2337548722223));
#55503=CARTESIAN_POINT('Ctrl Pts',(54.3405374423082,26.638499652669,13.2379724448733));
#55504=CARTESIAN_POINT('Ctrl Pts',(54.4196127351737,26.6192226326623,13.2421900175244));
#55505=CARTESIAN_POINT('Ctrl Pts',(54.4988222627673,26.5999128888371,13.2464147497406));
#55506=CARTESIAN_POINT('Ctrl Pts',(54.5789671034754,26.5845675421948,13.2506394819569));
#55507=CARTESIAN_POINT('Ctrl Pts',(54.659617221074,26.5732553051855,13.2548642141732));
#55508=CARTESIAN_POINT('Ctrl Pts',(54.7402471954598,26.5619458935259,13.2590878912183));
#55509=CARTESIAN_POINT('Ctrl Pts',(54.8213817281834,26.5546675976121,13.2633115682634));
#55510=CARTESIAN_POINT('Ctrl Pts',(54.9025873812025,26.5514369455334,13.2675352453085));
#55511=CARTESIAN_POINT('Ctrl Pts',(54.9839403697499,26.548200431919,13.2717665855848));
#55512=CARTESIAN_POINT('Ctrl Pts',(55.0653642705953,26.5490262338384,13.275997925861));
#55513=CARTESIAN_POINT('Ctrl Pts',(55.1464265556148,26.5538786796623,13.2802292661372));
#55514=CARTESIAN_POINT('Ctrl Pts',(55.2272558661565,26.5587171794689,13.2844484454647));
#55515=CARTESIAN_POINT('Ctrl Pts',(55.3077251932352,26.56755907639,13.2886676247923));
#55516=CARTESIAN_POINT('Ctrl Pts',(55.3874157958816,26.5803183574897,13.2928868041198));
#55517=CARTESIAN_POINT('Ctrl Pts',(55.4673601518598,26.5931182670949,13.2971194182912));
#55518=CARTESIAN_POINT('Ctrl Pts',(55.546818147273,26.6099081818321,13.3013520324627));
#55519=CARTESIAN_POINT('Ctrl Pts',(55.6253610549565,26.630638524635,13.3055846466342));
#55520=CARTESIAN_POINT('Ctrl Pts',(55.7037919285573,26.6513392975505,13.309811223379));
#55521=CARTESIAN_POINT('Ctrl Pts',(55.7813098614613,26.675969217629,13.3140378001238));
#55522=CARTESIAN_POINT('Ctrl Pts',(55.85749425884,26.7044273381014,13.3182643768686));
#55523=CARTESIAN_POINT('Ctrl Pts',(55.9335941003594,26.7328538733553,13.3224862626026));
#55524=CARTESIAN_POINT('Ctrl Pts',(56.0083629142646,26.7651000047905,13.3267081483366));
#55525=CARTESIAN_POINT('Ctrl Pts',(56.0813946373982,26.8010148049142,13.3309300340707));
#55526=CARTESIAN_POINT('Ctrl Pts',(56.1543771028993,26.836905381619,13.3351490722737));
#55527=CARTESIAN_POINT('Ctrl Pts',(56.2256243887639,26.8764595081574,13.3393681104767));
#55528=CARTESIAN_POINT('Ctrl Pts',(56.2947509935872,26.9194784032351,13.3435871486797));
#55529=CARTESIAN_POINT('Ctrl Pts',(56.3638550241815,26.9624832499102,13.3478048090987));
#55530=CARTESIAN_POINT('Ctrl Pts',(56.4308393549625,27.0089503728386,13.3520224695177));
#55531=CARTESIAN_POINT('Ctrl Pts',(56.4953448657147,27.0586360509733,13.3562401299366));
#55532=CARTESIAN_POINT('Ctrl Pts',(56.5598490341317,27.1083206951678,13.3604577025877));
#55533=CARTESIAN_POINT('Ctrl Pts',(56.6218741177678,27.1612234769942,13.3646752752387));
#55534=CARTESIAN_POINT('Ctrl Pts',(56.6810928216502,27.2170594022805,13.3688928478898));
#55535=CARTESIAN_POINT('Ctrl Pts',(56.7404120525915,27.27299011217,13.3731175801061));
#55536=CARTESIAN_POINT('Ctrl Pts',(56.7969150323778,27.3318636073182,13.3773423123224));
#55537=CARTESIAN_POINT('Ctrl Pts',(56.8503100112058,27.3933565696049,13.3815670445387));
#55538=CARTESIAN_POINT('Ctrl Pts',(56.9036916540778,27.4548341733794,13.3857907215838));
#55539=CARTESIAN_POINT('Ctrl Pts',(56.9539665773336,27.5189295560783,13.3900143986289));
#55540=CARTESIAN_POINT('Ctrl Pts',(57.0008849527752,27.5852881368427,13.394238075674));
#55541=CARTESIAN_POINT('Ctrl Pts',(57.047888454601,27.6517671153402,13.3984694159503));
#55542=CARTESIAN_POINT('Ctrl Pts',(57.0915229883876,27.7205171047142,13.4027007562265));
#55543=CARTESIAN_POINT('Ctrl Pts',(57.1315830077382,27.7911558697988,13.4069320965027));
#55544=CARTESIAN_POINT('Ctrl Pts',(57.1715278938663,27.8615916177911,13.4111512758303));
#55545=CARTESIAN_POINT('Ctrl Pts',(57.207918654212,27.9339048551902,13.4153704551578));
#55546=CARTESIAN_POINT('Ctrl Pts',(57.2405994756744,28.0076975059955,13.4195896344853));
#55547=CARTESIAN_POINT('Ctrl Pts',(57.2733843604399,28.0817251296883,13.4238222486568));
#55548=CARTESIAN_POINT('Ctrl Pts',(57.3025575531594,28.1575169438805,13.4280548628283));
#55549=CARTESIAN_POINT('Ctrl Pts',(57.3279272409129,28.2346863316157,13.4322874769998));
#55550=CARTESIAN_POINT('Ctrl Pts',(57.3532607411888,28.3117456444653,13.4365140537445));
#55551=CARTESIAN_POINT('Ctrl Pts',(57.3748013680508,28.3901781905108,13.4407406304893));
#55552=CARTESIAN_POINT('Ctrl Pts',(57.3924048260317,28.4695762086971,13.4449672072341));
#55553=CARTESIAN_POINT('Ctrl Pts',(57.4099887462126,28.548886104277,13.4491890929682));
#55554=CARTESIAN_POINT('Ctrl Pts',(57.4236440802519,28.6291588915563,13.4534109787022));
#55555=CARTESIAN_POINT('Ctrl Pts',(57.4332763688275,28.7099717894661,13.4576328644362));
#55556=CARTESIAN_POINT('Ctrl Pts',(57.4429021607232,28.7907301815824,13.4618519026392));
#55557=CARTESIAN_POINT('Ctrl Pts',(57.4485102414036,28.8720275007288,13.4660709408423));
#55558=CARTESIAN_POINT('Ctrl Pts',(57.4500574863572,28.9534321619047,13.4702899790453));
#55559=CARTESIAN_POINT('Ctrl Pts',(57.4516042260371,29.0348102392863,13.4745076394643));
#55560=CARTESIAN_POINT('Ctrl Pts',(57.4490927547638,29.1162951249738,13.4787252998832));
#55561=CARTESIAN_POINT('Ctrl Pts',(57.4425320065654,29.1974528979361,13.4829429603022));
#55562=CARTESIAN_POINT('Ctrl Pts',(57.4359713948938,29.2786089820359,13.4871605329532));
#55563=CARTESIAN_POINT('Ctrl Pts',(57.4253617124377,29.3594375040021,13.4913781056043));
#55564=CARTESIAN_POINT('Ctrl Pts',(57.4107638398513,29.4395087694977,13.4955956782553));
#55565=CARTESIAN_POINT('Ctrl Pts',(57.3961411865605,29.5197159604404,13.4998204104716));
#55566=CARTESIAN_POINT('Ctrl Pts',(57.3775168813565,29.5991628635351,13.5040451426879));
#55567=CARTESIAN_POINT('Ctrl Pts',(57.3550033028067,29.6774287370413,13.5082698749042));
#55568=CARTESIAN_POINT('Ctrl Pts',(57.3324953472592,29.755675062825,13.5124935519493));
#55569=CARTESIAN_POINT('Ctrl Pts',(57.3061002320462,29.8327405147774,13.5167172289944));
#55570=CARTESIAN_POINT('Ctrl Pts',(57.2759793818649,29.9082224965977,13.5209409060395));
#55571=CARTESIAN_POINT('Ctrl Pts',(57.2458038818999,29.9838414291995,13.5251722463158));
#55572=CARTESIAN_POINT('Ctrl Pts',(57.2118893318033,30.0578707265719,13.529403586592));
#55573=CARTESIAN_POINT('Ctrl Pts',(57.1744444604506,30.1299298820794,13.5336349268683));
#55574=CARTESIAN_POINT('Ctrl Pts',(57.1371072063378,30.2017819382658,13.5378541061957));
#55575=CARTESIAN_POINT('Ctrl Pts',(57.096260197805,30.2716748108313,13.5420732855232));
#55576=CARTESIAN_POINT('Ctrl Pts',(57.0521525262661,30.3392610869206,13.5462924648507));
#55577=CARTESIAN_POINT('Ctrl Pts',(57.0079044056871,30.4070625733638,13.5505250790222));
#55578=CARTESIAN_POINT('Ctrl Pts',(56.9602102295495,30.4727949081355,13.5547576931936));
#55579=CARTESIAN_POINT('Ctrl Pts',(56.9092898788012,30.5360867191365,13.5589903073651));
#55580=CARTESIAN_POINT('Ctrl Pts',(56.8584421611521,30.5992882503118,13.5632168841099));
#55581=CARTESIAN_POINT('Ctrl Pts',(56.8043776975106,30.6600558128422,13.5674434608547));
#55582=CARTESIAN_POINT('Ctrl Pts',(56.7473599735678,30.7180463826024,13.5716700375995));
#55583=CARTESIAN_POINT('Ctrl Pts',(56.690405532696,30.7759725895454,13.5758919233335));
#55584=CARTESIAN_POINT('Ctrl Pts',(56.6305046685124,30.8311275983423,13.5801138090675));
#55585=CARTESIAN_POINT('Ctrl Pts',(56.5679605967124,30.8832020117761,13.5843356948016));
#55586=CARTESIAN_POINT('Ctrl Pts',(56.5054587089492,30.9352413026328,13.5885547330046));
#55587=CARTESIAN_POINT('Ctrl Pts',(56.4403175103725,30.9842038282754,13.5927737712076));
#55588=CARTESIAN_POINT('Ctrl Pts',(56.3728755483497,31.0298184595534,13.5969928094106));
#55589=CARTESIAN_POINT('Ctrl Pts',(56.3054556104129,31.0754181947558,13.6012104698296));
#55590=CARTESIAN_POINT('Ctrl Pts',(56.2357367856598,31.1176719467605,13.6054281302486));
#55591=CARTESIAN_POINT('Ctrl Pts',(56.1640879216899,31.1563509826964,13.6096457906675));
#55592=CARTESIAN_POINT('Ctrl Pts',(56.0924405487059,31.1950292137361,13.6138633633186));
#55593=CARTESIAN_POINT('Ctrl Pts',(56.0188636257034,31.2301326569648,13.6180809359696));
#55594=CARTESIAN_POINT('Ctrl Pts',(55.9437507346095,31.2614784546672,13.6222985086207));
#55595=CARTESIAN_POINT('Ctrl Pts',(55.8685103351858,31.2928774636128,13.626523240837));
#55596=CARTESIAN_POINT('Ctrl Pts',(55.791729181861,31.3205058846649,13.6307479730533));
#55597=CARTESIAN_POINT('Ctrl Pts',(55.7138213824043,31.344228931658,13.6349727052695));
#55598=CARTESIAN_POINT('Ctrl Pts',(55.6359330412375,31.3679460535713,13.6391963823147));
#55599=CARTESIAN_POINT('Ctrl Pts',(55.5569190739749,31.3877596592283,13.6434200593598));
#55600=CARTESIAN_POINT('Ctrl Pts',(55.4772050682852,31.4035859819867,13.6476437364049));
#55601=CARTESIAN_POINT('Ctrl Pts',(55.3973464334388,31.4194410192438,13.6518750766811));
#55602=CARTESIAN_POINT('Ctrl Pts',(55.3167856828188,31.4312942482234,13.6561064169574));
#55603=CARTESIAN_POINT('Ctrl Pts',(55.2359556271585,31.4391136078527,13.6603377572336));
#55604=CARTESIAN_POINT('Ctrl Pts',(55.1553578785446,31.4469104945006,13.6645569365611));
#55605=CARTESIAN_POINT('Ctrl Pts',(55.0744928294408,31.450696729456,13.6687761158887));
#55606=CARTESIAN_POINT('Ctrl Pts',(54.9937875040814,31.4504921250423,13.6729952952162));
#55607=CARTESIAN_POINT('Ctrl Pts',(54.9128251942782,31.4502868691208,13.6772279093877));
#55608=CARTESIAN_POINT('Ctrl Pts',(54.8317225056717,31.4460645270235,13.6814605235591));
#55609=CARTESIAN_POINT('Ctrl Pts',(54.750910657913,31.4378073651662,13.6856931377306));
#55610=CARTESIAN_POINT('Ctrl Pts',(54.6702140806669,31.429561981375,13.6899197144754));
#55611=CARTESIAN_POINT('Ctrl Pts',(54.5898079786112,31.4172932554024,13.6941462912202));
#55612=CARTESIAN_POINT('Ctrl Pts',(54.5101235308582,31.4010354630828,13.698372867965));
#55613=CARTESIAN_POINT('Ctrl Pts',(54.4305275236153,31.3847957150301,13.702594753699));
#55614=CARTESIAN_POINT('Ctrl Pts',(54.3516520320611,31.3645757902679,13.7068166394331));
#55615=CARTESIAN_POINT('Ctrl Pts',(54.2739216572553,31.3404615976762,13.7110385251671));
#55616=CARTESIAN_POINT('Ctrl Pts',(54.1962437091769,31.3163636693596,13.7152575633701));
#55617=CARTESIAN_POINT('Ctrl Pts',(54.1197097864442,31.2883768270864,13.7194766015731));
#55618=CARTESIAN_POINT('Ctrl Pts',(54.044731624488,31.2566374500009,13.7236956397761));
#55619=CARTESIAN_POINT('Ctrl Pts',(53.9697779476661,31.2249084378389,13.7279133001951));
#55620=CARTESIAN_POINT('Ctrl Pts',(53.8963794501245,31.1894295054698,13.7321309606141));
#55621=CARTESIAN_POINT('Ctrl Pts',(53.8249287996965,31.1503855292057,13.736348621033));
#55622=CARTESIAN_POINT('Ctrl Pts',(53.7534796361292,31.1113423654318,13.7405661936841));
#55623=CARTESIAN_POINT('Ctrl Pts',(53.6839786461747,31.0687345290583,13.7447837663351));
#55624=CARTESIAN_POINT('Ctrl Pts',(53.616793481816,31.0227926186471,13.7490013389862));
#55625=CARTESIAN_POINT('Ctrl Pts',(53.5494942668869,30.9767727192761,13.7532260712025));
#55626=CARTESIAN_POINT('Ctrl Pts',(53.4845191285391,30.9274076855743,13.7574508034188));
#55627=CARTESIAN_POINT('Ctrl Pts',(53.4222065694118,30.8749715038882,13.761675535635));
#55628=CARTESIAN_POINT('Ctrl Pts',(53.3599095734997,30.8225484186884,13.7658992126801));
#55629=CARTESIAN_POINT('Ctrl Pts',(53.3002741537448,30.7670560525255,13.7701228897253));
#55630=CARTESIAN_POINT('Ctrl Pts',(53.2436022659899,30.7088057964451,13.7743465667704));
#55631=CARTESIAN_POINT('Ctrl Pts',(53.1868275555596,30.6504498539755,13.7785779070466));
#55632=CARTESIAN_POINT('Ctrl Pts',(53.1330274304744,30.5893263714298,13.7828092473228));
#55633=CARTESIAN_POINT('Ctrl Pts',(53.0824644068832,30.5257809472956,13.7870405875991));
#55634=CARTESIAN_POINT('Ctrl Pts',(53.0320467023394,30.4624181538636,13.7912597669266));
#55635=CARTESIAN_POINT('Ctrl Pts',(52.9848477150114,30.3966477400224,13.7954789462541));
#55636=CARTESIAN_POINT('Ctrl Pts',(52.9410832981599,30.3288386903171,13.7996981255816));
#55637=CARTESIAN_POINT('Ctrl Pts',(52.8962263261542,30.2593368241167,13.8040226344542));
#55638=CARTESIAN_POINT('Ctrl Pts',(52.8548162274857,30.1874436103981,13.8083471433269));
#55639=CARTESIAN_POINT('Ctrl Pts',(52.8171099662843,30.1135265379436,13.8126716521995));
#55640=CARTESIAN_POINT('Ctrl Pts',(52.7794646483622,30.0397289350055,13.8169891715234));
#55641=CARTESIAN_POINT('Ctrl Pts',(52.7455114658633,29.9639143620006,13.8213066908472));
#55642=CARTESIAN_POINT('Ctrl Pts',(52.7154636607913,29.8864784062994,13.8256242101711));
#55643=CARTESIAN_POINT('Ctrl Pts',(52.685466354783,29.809172591327,13.8299344733682));
#55644=CARTESIAN_POINT('Ctrl Pts',(52.6593615204037,29.7302512227029,13.8342447365652));
#55645=CARTESIAN_POINT('Ctrl Pts',(52.6373154269118,29.6501321850909,13.8385549997623));
#55646=CARTESIAN_POINT('Ctrl Pts',(52.6152911752435,29.5700925241668,13.8428609926333));
#55647=CARTESIAN_POINT('Ctrl Pts',(52.5973177878601,29.488857972754,13.8471669855043));
#55648=CARTESIAN_POINT('Ctrl Pts',(52.5835123979253,29.4068635139934,13.8514729783753));
#55649=CARTESIAN_POINT('Ctrl Pts',(52.5697183850117,29.3249366268628,13.8557754226777));
#55650=CARTESIAN_POINT('Ctrl Pts',(52.5600856091676,29.2422515087223,13.8600778669802));
#55651=CARTESIAN_POINT('Ctrl Pts',(52.5546803144841,29.1592541541951,13.8643803112826));
#55652=CARTESIAN_POINT('Ctrl Pts',(52.5512077346424,29.1059332980501,13.8671443754511));
#55653=CARTESIAN_POINT('Ctrl Pts',(52.5494789304077,29.0524838000256,13.8699084396195));
#55654=CARTESIAN_POINT('Ctrl Pts',(52.5495001938466,28.9990252990303,13.8726725037879));
#55655=CARTESIAN_POINT('',(52.5495004475699,28.9985189396232,14.6726725037596));
#55656=CARTESIAN_POINT('Ctrl Pts',(52.5495001938469,28.9990252981815,13.8726725038318));
#55657=CARTESIAN_POINT('Ctrl Pts',(52.5495355260103,28.9101966350554,13.8772653771879));
#55658=CARTESIAN_POINT('Ctrl Pts',(52.5544050151296,28.8215184266261,13.881858250544));
#55659=CARTESIAN_POINT('Ctrl Pts',(52.5640346561721,28.733498417135,13.8864511239002));
#55660=CARTESIAN_POINT('Ctrl Pts',(52.5736906293279,28.6452377182093,13.8910565564016));
#55661=CARTESIAN_POINT('Ctrl Pts',(52.5881326985161,28.5576391306989,13.8956619889031));
#55662=CARTESIAN_POINT('Ctrl Pts',(52.6072358840093,28.4711993426373,13.9002674214045));
#55663=CARTESIAN_POINT('Ctrl Pts',(52.626421327776,28.3843873450441,13.9048926848879));
#55664=CARTESIAN_POINT('Ctrl Pts',(52.6503079795362,28.2987444485671,13.9095179483713));
#55665=CARTESIAN_POINT('Ctrl Pts',(52.6787204535448,28.2147538492877,13.9141432118546));
#55666=CARTESIAN_POINT('Ctrl Pts',(52.7038197685482,28.1405573358827,13.9182291265521));
#55667=CARTESIAN_POINT('Ctrl Pts',(52.7324501558775,28.0676500725619,13.9223150412496));
#55668=CARTESIAN_POINT('Ctrl Pts',(52.7644606708905,27.9963495837671,13.926400955947));
#55669=CARTESIAN_POINT('Ctrl Pts',(52.7976204819761,27.9224891432901,13.9306335701185));
#55670=CARTESIAN_POINT('Ctrl Pts',(52.8345063251939,27.850136473387,13.93486618429));
#55671=CARTESIAN_POINT('Ctrl Pts',(52.874958780294,27.7796926352142,13.9390987984615));
#55672=CARTESIAN_POINT('Ctrl Pts',(52.9153535337652,27.7093492785623,13.9433253752063));
#55673=CARTESIAN_POINT('Ctrl Pts',(52.9593045653985,27.6409097453732,13.947551951951));
#55674=CARTESIAN_POINT('Ctrl Pts',(53.0066049705101,27.5747538786564,13.9517785286958));
#55675=CARTESIAN_POINT('Ctrl Pts',(53.0538528776492,27.5086714372911,13.9560004144299));
#55676=CARTESIAN_POINT('Ctrl Pts',(53.1044425029408,27.4448680021315,13.9602223001639));
#55677=CARTESIAN_POINT('Ctrl Pts',(53.1581224634525,27.3836963805145,13.9644441858979));
#55678=CARTESIAN_POINT('Ctrl Pts',(53.2117662184956,27.3225660172593,13.9686632241009));
#55679=CARTESIAN_POINT('Ctrl Pts',(53.2684958634702,27.2640642903586,13.972882262304));
#55680=CARTESIAN_POINT('Ctrl Pts',(53.3280191598301,27.208511702493,13.977101300507));
#55681=CARTESIAN_POINT('Ctrl Pts',(53.3875230180515,27.1529772560772,13.981318960926));
#55682=CARTESIAN_POINT('Ctrl Pts',(53.4498183765196,27.1003903527954,13.9855366213449));
#55683=CARTESIAN_POINT('Ctrl Pts',(53.5145764689179,27.0510343298797,13.9897542817639));
#55684=CARTESIAN_POINT('Ctrl Pts',(53.5793332137248,27.0016793340441,13.993971854415));
#55685=CARTESIAN_POINT('Ctrl Pts',(53.646552220384,26.955555365559,13.998189427066));
#55686=CARTESIAN_POINT('Ctrl Pts',(53.7158731516393,26.9129042936848,14.0024069997171));
#55687=CARTESIAN_POINT('Ctrl Pts',(53.7853117590487,26.870180819233,14.0066317319334));
#55688=CARTESIAN_POINT('Ctrl Pts',(53.8568590323182,26.8309422815005,14.0108564641496));
#55689=CARTESIAN_POINT('Ctrl Pts',(53.9301268787407,26.7953862573215,14.0150811963659));
#55690=CARTESIAN_POINT('Ctrl Pts',(54.0033764257502,26.7598391136324,14.019304873411));
#55691=CARTESIAN_POINT('Ctrl Pts',(54.0783452492387,26.7279728070302,14.0235285504562));
#55692=CARTESIAN_POINT('Ctrl Pts',(54.1546259781385,26.6999363023686,14.0277522275013));
#55693=CARTESIAN_POINT('Ctrl Pts',(54.2310451070274,26.671848929657,14.0319835677775));
#55694=CARTESIAN_POINT('Ctrl Pts',(54.3087804534193,26.6476053841441,14.0362149080538));
#55695=CARTESIAN_POINT('Ctrl Pts',(54.3874094661352,26.6273046786789,14.04044624833));
#55696=CARTESIAN_POINT('Ctrl Pts',(54.4658124976416,26.6070623178096,14.0446654276575));
#55697=CARTESIAN_POINT('Ctrl Pts',(54.5451036028337,26.5907401739851,14.048884606985));
#55698=CARTESIAN_POINT('Ctrl Pts',(54.6248578754318,26.5783851180722,14.0531037863125));
#55699=CARTESIAN_POINT('Ctrl Pts',(54.704866104102,26.5659907208002,14.057336400484));
#55700=CARTESIAN_POINT('Ctrl Pts',(54.7856380316746,26.5575426447949,14.0615690146555));
#55701=CARTESIAN_POINT('Ctrl Pts',(54.8667504494212,26.5531255023458,14.065801628827));
#55702=CARTESIAN_POINT('Ctrl Pts',(54.94774716792,26.5487146605357,14.0700282055718));
#55703=CARTESIAN_POINT('Ctrl Pts',(55.0290829519683,26.5483233575919,14.0742547823165));
#55704=CARTESIAN_POINT('Ctrl Pts',(55.1103265405908,26.5519848234863,14.0784813590613));
#55705=CARTESIAN_POINT('Ctrl Pts',(55.1914799582377,26.5556422255776,14.0827032447954));
#55706=CARTESIAN_POINT('Ctrl Pts',(55.2725409220424,26.5633434379741,14.0869251305294));
#55707=CARTESIAN_POINT('Ctrl Pts',(55.3530766352391,26.5750696629288,14.0911470162634));
#55708=CARTESIAN_POINT('Ctrl Pts',(55.4335580295948,26.5867879789085,14.0953660544664));
#55709=CARTESIAN_POINT('Ctrl Pts',(55.5135144184293,26.6025258489624,14.0995850926695));
#55710=CARTESIAN_POINT('Ctrl Pts',(55.5925178611087,26.6222126179435,14.1038041308725));
#55711=CARTESIAN_POINT('Ctrl Pts',(55.6714955041441,26.6418929579435,14.1080217912915));
#55712=CARTESIAN_POINT('Ctrl Pts',(55.7495203686247,26.6655195236315,14.1122394517104));
#55713=CARTESIAN_POINT('Ctrl Pts',(55.8261758034848,26.6929707865447,14.1164571121294));
#55714=CARTESIAN_POINT('Ctrl Pts',(55.9028296431743,26.7204214782075,14.1206746847804));
#55715=CARTESIAN_POINT('Ctrl Pts',(55.9781136729493,26.7516965511231,14.1248922574315));
#55716=CARTESIAN_POINT('Ctrl Pts',(56.0516288388797,26.7866254191311,14.1291098300825));
#55717=CARTESIAN_POINT('Ctrl Pts',(56.1252688009121,26.8216135808443,14.1333345622988));
#55718=CARTESIAN_POINT('Ctrl Pts',(56.1971334695029,26.8602677470368,14.1375592945151));
#55719=CARTESIAN_POINT('Ctrl Pts',(56.2668458342363,26.9023699367434,14.1417840267314));
#55720=CARTESIAN_POINT('Ctrl Pts',(56.3365407875756,26.9444616109865,14.1460077037765));
#55721=CARTESIAN_POINT('Ctrl Pts',(56.4040841374098,26.9899993083908,14.1502313808216));
#55722=CARTESIAN_POINT('Ctrl Pts',(56.4691291551239,27.0387224124146,14.1544550578667));
#55723=CARTESIAN_POINT('Ctrl Pts',(56.5342921873072,27.087533917233,14.158686398143));
#55724=CARTESIAN_POINT('Ctrl Pts',(56.5969474701362,27.139542081124,14.1629177384192));
#55725=CARTESIAN_POINT('Ctrl Pts',(56.656781911933,27.1944463601733,14.1671490786954));
#55726=CARTESIAN_POINT('Ctrl Pts',(56.7164443884584,27.2491928433284,14.171368258023));
#55727=CARTESIAN_POINT('Ctrl Pts',(56.7733019560602,27.3068184344149,14.1755874373505));
#55728=CARTESIAN_POINT('Ctrl Pts',(56.8270839789517,27.3669922278636,14.179806616678));
#55729=CARTESIAN_POINT('Ctrl Pts',(56.8810372562578,27.4273576286044,14.1840392308495));
#55730=CARTESIAN_POINT('Ctrl Pts',(56.9320960180283,27.4905120197301,14.1882718450209));
#55731=CARTESIAN_POINT('Ctrl Pts',(56.979958894167,27.5561464660815,14.1925044591924));
#55732=CARTESIAN_POINT('Ctrl Pts',(57.027753498407,27.6216872910579,14.1967310359372));
#55733=CARTESIAN_POINT('Ctrl Pts',(57.0723609996019,27.6897007729706,14.200957612682));
#55734=CARTESIAN_POINT('Ctrl Pts',(57.1135187447903,27.7598432496575,14.2051841894268));
#55735=CARTESIAN_POINT('Ctrl Pts',(57.1546308096475,27.8299078763175,14.2094060751608));
#55736=CARTESIAN_POINT('Ctrl Pts',(57.1923004924596,27.9020964039528,14.2136279608948));
#55737=CARTESIAN_POINT('Ctrl Pts',(57.2263079463427,27.9760355582094,14.2178498466288));
#55738=CARTESIAN_POINT('Ctrl Pts',(57.2602924632527,28.0499248427994,14.2220688848319));
#55739=CARTESIAN_POINT('Ctrl Pts',(57.2906194633733,28.1255619879926,14.2262879230349));
#55740=CARTESIAN_POINT('Ctrl Pts',(57.3171152427982,28.2025495616703,14.2305069612379));
#55741=CARTESIAN_POINT('Ctrl Pts',(57.3436023696675,28.2795119940132,14.2347246216569));
#55742=CARTESIAN_POINT('Ctrl Pts',(57.3662606094634,28.3578235401146,14.2389422820758));
#55743=CARTESIAN_POINT('Ctrl Pts',(57.38496507815,28.4370685423562,14.2431599424948));
#55744=CARTESIAN_POINT('Ctrl Pts',(57.4036691576036,28.5163118955392,14.2473775151458));
#55745=CARTESIAN_POINT('Ctrl Pts',(57.4184195239614,28.5964882138468,14.2515950877969));
#55746=CARTESIAN_POINT('Ctrl Pts',(57.4291420239166,28.6771698935318,14.2558126604479));
#55747=CARTESIAN_POINT('Ctrl Pts',(57.4398827259147,28.7579885348765,14.2600373926642));
#55748=CARTESIAN_POINT('Ctrl Pts',(57.4465818196907,28.8393137910905,14.2642621248805));
#55749=CARTESIAN_POINT('Ctrl Pts',(57.4492169084032,28.9207107473131,14.2684868570968));
#55750=CARTESIAN_POINT('Ctrl Pts',(57.4518513389747,29.0020873737922,14.2727105341419));
#55751=CARTESIAN_POINT('Ctrl Pts',(57.4504238237014,29.0835351987591,14.276934211187));
#55752=CARTESIAN_POINT('Ctrl Pts',(57.4449642149757,29.1646214976492,14.2811578882321));
#55753=CARTESIAN_POINT('Ctrl Pts',(57.4394947006054,29.2458549155171,14.2853892285084));
#55754=CARTESIAN_POINT('Ctrl Pts',(57.4299785271914,29.3267250337392,14.2896205687846));
#55755=CARTESIAN_POINT('Ctrl Pts',(57.4164973511887,29.4068056067681,14.2938519090608));
#55756=CARTESIAN_POINT('Ctrl Pts',(57.4030549203305,29.4866560267772,14.2980710883884));
#55757=CARTESIAN_POINT('Ctrl Pts',(57.3856704264274,29.5657210070998,14.3022902677159));
#55758=CARTESIAN_POINT('Ctrl Pts',(57.3644741070784,29.6435933863519,14.3065094470434));
#55759=CARTESIAN_POINT('Ctrl Pts',(57.3432102937403,29.7217137292916,14.3107420612149));
#55760=CARTESIAN_POINT('Ctrl Pts',(57.3180312283172,29.798924408193,14.3149746753864));
#55761=CARTESIAN_POINT('Ctrl Pts',(57.2890319872906,29.874804441667,14.3192072895578));
#55762=CARTESIAN_POINT('Ctrl Pts',(57.2600741109585,29.950576239398,14.3234338663026));
#55763=CARTESIAN_POINT('Ctrl Pts',(57.2273070461421,30.0250207311223,14.3276604430474));
#55764=CARTESIAN_POINT('Ctrl Pts',(57.1908760768488,30.0977305069513,14.3318870197922));
#55765=CARTESIAN_POINT('Ctrl Pts',(57.1544855417128,30.1703595833488,14.3361089055262));
#55766=CARTESIAN_POINT('Ctrl Pts',(57.1144393892975,30.2412573562478,14.3403307912603));
#55767=CARTESIAN_POINT('Ctrl Pts',(57.0709310467267,30.3100362016767,14.3445526769943));
#55768=CARTESIAN_POINT('Ctrl Pts',(57.0274520491837,30.3787686579073,14.3487717151973));
#55769=CARTESIAN_POINT('Ctrl Pts',(56.9805157469836,30.445384633507,14.3529907534004));
#55770=CARTESIAN_POINT('Ctrl Pts',(56.9303609516672,30.5095220588909,14.3572097916034));
#55771=CARTESIAN_POINT('Ctrl Pts',(56.8802225350784,30.5736385393302,14.3614274520224));
#55772=CARTESIAN_POINT('Ctrl Pts',(56.8268679986246,30.6352777113171,14.3656451124413));
#55773=CARTESIAN_POINT('Ctrl Pts',(56.7705780194319,30.6941085346295,14.3698627728603));
#55774=CARTESIAN_POINT('Ctrl Pts',(56.7142892116124,30.7529381336947,14.3740803455114));
#55775=CARTESIAN_POINT('Ctrl Pts',(56.655065404513,30.8089591654391,14.3782979181624));
#55776=CARTESIAN_POINT('Ctrl Pts',(56.5932249138242,30.8618766403739,14.3825154908135));
#55777=CARTESIAN_POINT('Ctrl Pts',(56.531279445447,30.9148839456791,14.3867402230297));
#55778=CARTESIAN_POINT('Ctrl Pts',(56.4667087609621,30.9647768495918,14.390964955246));
#55779=CARTESIAN_POINT('Ctrl Pts',(56.399865485068,31.0112997970753,14.3951896874623));
#55780=CARTESIAN_POINT('Ctrl Pts',(56.333038903983,31.0578111249649,14.3994133645074));
#55781=CARTESIAN_POINT('Ctrl Pts',(56.2639412732173,31.1009539507217,14.4036370415525));
#55782=CARTESIAN_POINT('Ctrl Pts',(56.1929518247189,31.1405177396836,14.4078607185977));
#55783=CARTESIAN_POINT('Ctrl Pts',(56.1218335764694,31.1801533112311,14.4120920588739));
#55784=CARTESIAN_POINT('Ctrl Pts',(56.0488170686819,31.2161966624658,14.4163233991501));
#55785=CARTESIAN_POINT('Ctrl Pts',(55.9743043007145,31.2484842404627,14.4205547394264));
#55786=CARTESIAN_POINT('Ctrl Pts',(55.9000056837946,31.2806790233745,14.4247739187539));
#55787=CARTESIAN_POINT('Ctrl Pts',(55.8242198511984,31.3091395103577,14.4289930980814));
#55788=CARTESIAN_POINT('Ctrl Pts',(55.7473592416202,31.33375328901,14.4332122774089));
#55789=CARTESIAN_POINT('Ctrl Pts',(55.6702538900632,31.3584454436331,14.4374448915804));
#55790=CARTESIAN_POINT('Ctrl Pts',(55.591780121258,31.3793581641997,14.4416775057518));
#55791=CARTESIAN_POINT('Ctrl Pts',(55.5123428247275,31.3963420206536,14.4459101199233));
#55792=CARTESIAN_POINT('Ctrl Pts',(55.4330188380417,31.413301651231,14.4501366966681));
#55793=CARTESIAN_POINT('Ctrl Pts',(55.3527345038368,31.4263434519515,14.4543632734129));
#55794=CARTESIAN_POINT('Ctrl Pts',(55.2719106605359,31.4353674964339,14.4585898501577));
#55795=CARTESIAN_POINT('Ctrl Pts',(55.1911765223419,31.444381525272,14.4628117358917));
#55796=CARTESIAN_POINT('Ctrl Pts',(55.1099045242043,31.449386607094,14.4670336216257));
#55797=CARTESIAN_POINT('Ctrl Pts',(55.0285251167716,31.4503339706483,14.4712555073598));
#55798=CARTESIAN_POINT('Ctrl Pts',(54.9472005972257,31.4512806952354,14.4754745455628));
#55799=CARTESIAN_POINT('Ctrl Pts',(54.8657692755834,31.4481751316952,14.4796935837658));
#55800=CARTESIAN_POINT('Ctrl Pts',(54.784664874142,31.4410204901991,14.4839126219688));
#55801=CARTESIAN_POINT('Ctrl Pts',(54.7035869584412,31.433868185148,14.4881302823878));
#55802=CARTESIAN_POINT('Ctrl Pts',(54.6228362133186,31.422669468901,14.4923479428067));
#55803=CARTESIAN_POINT('Ctrl Pts',(54.5428431245178,31.4074795619484,14.4965656032257));
#55804=CARTESIAN_POINT('Ctrl Pts',(54.462851700343,31.392289971092,14.5007831758767));
#55805=CARTESIAN_POINT('Ctrl Pts',(54.3836183573154,31.3731094424833,14.5050007485278));
#55806=CARTESIAN_POINT('Ctrl Pts',(54.3055638313786,31.3500443948382,14.5092183211788));
#55807=CARTESIAN_POINT('Ctrl Pts',(54.2273768035225,31.3269401929859,14.5134430533951));
#55808=CARTESIAN_POINT('Ctrl Pts',(54.1503730443571,31.2999384110058,14.5176677856114));
#55809=CARTESIAN_POINT('Ctrl Pts',(54.0749588890643,31.269195715023,14.5218925178277));
#55810=CARTESIAN_POINT('Ctrl Pts',(53.9995635692477,31.238460697351,14.5261161948728));
#55811=CARTESIAN_POINT('Ctrl Pts',(53.9257574727214,31.2039868506371,14.5303398719179));
#55812=CARTESIAN_POINT('Ctrl Pts',(53.8539236554495,31.1659776689665,14.534563548963));
#55813=CARTESIAN_POINT('Ctrl Pts',(53.7819595064455,31.127899525313,14.5387948892393));
#55814=CARTESIAN_POINT('Ctrl Pts',(53.7119751884393,31.0862734660363,14.5430262295155));
#55815=CARTESIAN_POINT('Ctrl Pts',(53.6443267425252,31.0413476599951,14.5472575697917));
#55816=CARTESIAN_POINT('Ctrl Pts',(53.5768727194719,30.9965509715356,14.5514767491192));
#55817=CARTESIAN_POINT('Ctrl Pts',(53.5117414766369,30.9484738153338,14.5556959284468));
#55818=CARTESIAN_POINT('Ctrl Pts',(53.4492518403369,30.8974009579689,14.5599151077743));
#55819=CARTESIAN_POINT('Ctrl Pts',(53.3873827660839,30.8468352867359,14.5640923879531));
#55820=CARTESIAN_POINT('Ctrl Pts',(53.3278597894437,30.7931340933857,14.568269668132));
#55821=CARTESIAN_POINT('Ctrl Pts',(53.2710240049294,30.7365460715079,14.5724469483109));
#55822=CARTESIAN_POINT('Ctrl Pts',(53.2142047566346,30.6799745137638,14.5766230131212));
#55823=CARTESIAN_POINT('Ctrl Pts',(53.1600715331763,30.6205180773484,14.5807990779316));
#55824=CARTESIAN_POINT('Ctrl Pts',(53.1089340860591,30.5584671825646,14.584975142742));
#55825=CARTESIAN_POINT('Ctrl Pts',(53.0579134800667,30.4965580644386,14.5891416658928));
#55826=CARTESIAN_POINT('Ctrl Pts',(53.0098753147622,30.4320666680182,14.5933081890436));
#55827=CARTESIAN_POINT('Ctrl Pts',(52.9650908239207,30.3653186057138,14.5974747121944));
#55828=CARTESIAN_POINT('Ctrl Pts',(52.92033330881,30.298610748796,14.6016387256593));
#55829=CARTESIAN_POINT('Ctrl Pts',(52.8788258453699,30.2296493187588,14.6058027391242));
#55830=CARTESIAN_POINT('Ctrl Pts',(52.8407980088952,30.1587911855072,14.6099667525891));
#55831=CARTESIAN_POINT('Ctrl Pts',(52.8027807185668,30.0879527031299,14.6141296112606));
#55832=CARTESIAN_POINT('Ctrl Pts',(52.7682413646764,30.0152189829851,14.6182924699321));
#55833=CARTESIAN_POINT('Ctrl Pts',(52.7373641541067,29.9409725176001,14.6224553286035));
#55834=CARTESIAN_POINT('Ctrl Pts',(52.7063244605155,29.866335350147,14.6266400931999));
#55835=CARTESIAN_POINT('Ctrl Pts',(52.6789857771242,29.7901699093691,14.6308248577962));
#55836=CARTESIAN_POINT('Ctrl Pts',(52.655486019538,29.7128845947404,14.6350096223926));
#55837=CARTESIAN_POINT('Ctrl Pts',(52.6320877087135,29.6359329152514,14.6391763216614));
#55838=CARTESIAN_POINT('Ctrl Pts',(52.6124953239584,29.5578714887528,14.6433430209302));
#55839=CARTESIAN_POINT('Ctrl Pts',(52.5967942336395,29.4791161597482,14.6475097201991));
#55840=CARTESIAN_POINT('Ctrl Pts',(52.5809910317977,29.399848648059,14.6517035174591));
#55841=CARTESIAN_POINT('Ctrl Pts',(52.5691299991165,29.3198786600043,14.6558973147192));
#55842=CARTESIAN_POINT('Ctrl Pts',(52.5612452194669,29.2396359122226,14.6600911119793));
#55843=CARTESIAN_POINT('Ctrl Pts',(52.5533604398173,29.1593931644409,14.6642849092394));
#55844=CARTESIAN_POINT('Ctrl Pts',(52.5494518791718,29.07887814682,14.6684787064995));
#55845=CARTESIAN_POINT('Ctrl Pts',(52.5495004475699,28.9985189396232,14.6726725037596));
#55846=CARTESIAN_POINT('',(52.5495009444406,29.0021514419089,15.4726725038256));
#55847=CARTESIAN_POINT('Ctrl Pts',(52.5495004475702,28.9985189390796,14.672672503788));
#55848=CARTESIAN_POINT('Ctrl Pts',(52.5495542816505,28.9094473905506,14.6773209819052));
#55849=CARTESIAN_POINT('Ctrl Pts',(52.5544642569436,28.8205244575737,14.6819694600225));
#55850=CARTESIAN_POINT('Ctrl Pts',(52.5641836615108,28.7321399336424,14.6866179381398));
#55851=CARTESIAN_POINT('Ctrl Pts',(52.5730335449504,28.6516625001486,14.6908505523113));
#55852=CARTESIAN_POINT('Ctrl Pts',(52.5858925348933,28.5714744670663,14.6950831664828));
#55853=CARTESIAN_POINT('Ctrl Pts',(52.6027322144458,28.4920064819864,14.6993157806543));
#55854=CARTESIAN_POINT('Ctrl Pts',(52.6195478737765,28.4126518505255,14.703542357399));
#55855=CARTESIAN_POINT('Ctrl Pts',(52.6403328498171,28.334015677833,14.7077689341438));
#55856=CARTESIAN_POINT('Ctrl Pts',(52.6650070179837,28.2565230172126,14.7119955108886));
#55857=CARTESIAN_POINT('Ctrl Pts',(52.6896538006809,28.179116364472,14.7162173966227));
#55858=CARTESIAN_POINT('Ctrl Pts',(52.7181810582898,28.1028511423937,14.7204392823567));
#55859=CARTESIAN_POINT('Ctrl Pts',(52.7504580308852,28.028140350055,14.7246611680907));
#55860=CARTESIAN_POINT('Ctrl Pts',(52.7827132336635,27.9534799478291,14.7288802062937));
#55861=CARTESIAN_POINT('Ctrl Pts',(52.8187129447186,27.8803723184514,14.7330992444967));
#55862=CARTESIAN_POINT('Ctrl Pts',(52.8582775963539,27.8092122793209,14.7373182826997));
#55863=CARTESIAN_POINT('Ctrl Pts',(52.8978293276164,27.7380754784647,14.7415359431187));
#55864=CARTESIAN_POINT('Ctrl Pts',(52.9409434619016,27.6688854104762,14.7457536035377));
#55865=CARTESIAN_POINT('Ctrl Pts',(52.9873942478509,27.602012755274,14.7499712639566));
#55866=CARTESIAN_POINT('Ctrl Pts',(53.033844067177,27.5351414916665,14.7541888366076));
#55867=CARTESIAN_POINT('Ctrl Pts',(53.083630134129,27.4705879258279,14.7584064092587));
#55868=CARTESIAN_POINT('Ctrl Pts',(53.1364839079387,27.4086929822852,14.7626239819097));
#55869=CARTESIAN_POINT('Ctrl Pts',(53.1894274039829,27.3466929686171,14.766848714126));
#55870=CARTESIAN_POINT('Ctrl Pts',(53.2454487228273,27.2873609621562,14.7710734463423));
#55871=CARTESIAN_POINT('Ctrl Pts',(53.3042392968181,27.2310042714738,14.7752981785586));
#55872=CARTESIAN_POINT('Ctrl Pts',(53.3630151872463,27.1746616564661,14.7795218556036));
#55873=CARTESIAN_POINT('Ctrl Pts',(53.4245585835907,27.1212931605337,14.7837455326487));
#55874=CARTESIAN_POINT('Ctrl Pts',(53.488527630144,27.0711657600608,14.7879692096938));
#55875=CARTESIAN_POINT('Ctrl Pts',(53.5526127389776,27.020947410907,14.7922005499701));
#55876=CARTESIAN_POINT('Ctrl Pts',(53.6191319126329,26.9739821778735,14.7964318902463));
#55877=CARTESIAN_POINT('Ctrl Pts',(53.68771349525,26.9304941702303,14.8006632305225));
#55878=CARTESIAN_POINT('Ctrl Pts',(53.7560979731549,26.8871311479096,14.80488240985));
#55879=CARTESIAN_POINT('Ctrl Pts',(53.8265325839536,26.847225542496,14.8091015891776));
#55880=CARTESIAN_POINT('Ctrl Pts',(53.8986274024896,26.8109525698484,14.8133207685051));
#55881=CARTESIAN_POINT('Ctrl Pts',(53.9709517876213,26.774564095657,14.8175533826766));
#55882=CARTESIAN_POINT('Ctrl Pts',(54.0452159771998,26.7416961109572,14.8217859968481));
#55883=CARTESIAN_POINT('Ctrl Pts',(54.121043262982,26.7125592238376,14.8260186110196));
#55884=CARTESIAN_POINT('Ctrl Pts',(54.1967623882608,26.6834638977515,14.8302451877643));
#55885=CARTESIAN_POINT('Ctrl Pts',(54.274039751417,26.65808926419,14.8344717645091));
#55886=CARTESIAN_POINT('Ctrl Pts',(54.3524751871284,26.6365995119922,14.8386983412539));
#55887=CARTESIAN_POINT('Ctrl Pts',(54.4308235685887,26.6151336109309,14.842920226988));
#55888=CARTESIAN_POINT('Ctrl Pts',(54.5103270228847,26.5975441458926,14.847142112722));
#55889=CARTESIAN_POINT('Ctrl Pts',(54.5905679301628,26.5839462691842,14.851363998456));
#55890=CARTESIAN_POINT('Ctrl Pts',(54.6707547174373,26.570357563822,14.855583036659));
#55891=CARTESIAN_POINT('Ctrl Pts',(54.7516775129992,26.5607551772571,14.8598020748621));
#55892=CARTESIAN_POINT('Ctrl Pts',(54.8329073772553,26.555203422486,14.8640211130651));
#55893=CARTESIAN_POINT('Ctrl Pts',(54.9141107147993,26.5496534807155,14.8682387734841));
#55894=CARTESIAN_POINT('Ctrl Pts',(54.9956204587805,26.5481515754134,14.872456433903));
#55895=CARTESIAN_POINT('Ctrl Pts',(55.0770027743105,26.5507101390916,14.876674094322));
#55896=CARTESIAN_POINT('Ctrl Pts',(55.1583833963052,26.5532686495271,14.8808916669731));
#55897=CARTESIAN_POINT('Ctrl Pts',(55.2396361308393,26.5598874451701,14.8851092396241));
#55898=CARTESIAN_POINT('Ctrl Pts',(55.3203288080082,26.5705268668372,14.8893268122752));
#55899=CARTESIAN_POINT('Ctrl Pts',(55.4011584655055,26.581184349517,14.8935515444915));
#55900=CARTESIAN_POINT('Ctrl Pts',(55.4814257004644,26.5958760528818,14.8977762767078));
#55901=CARTESIAN_POINT('Ctrl Pts',(55.5607047502234,26.6145104416332,14.9020010089241));
#55902=CARTESIAN_POINT('Ctrl Pts',(55.6399639992082,26.6331401762506,14.9062246859692));
#55903=CARTESIAN_POINT('Ctrl Pts',(55.7182351145354,26.6557104774701,14.9104483630143));
#55904=CARTESIAN_POINT('Ctrl Pts',(55.7951080431562,26.682079930259,14.9146720400594));
#55905=CARTESIAN_POINT('Ctrl Pts',(55.872120446224,26.7084972264813,14.9189033803357));
#55906=CARTESIAN_POINT('Ctrl Pts',(55.9477291602737,26.73872727672,14.9231347206119));
#55907=CARTESIAN_POINT('Ctrl Pts',(56.0215438670464,26.7725803319311,14.9273660608881));
#55908=CARTESIAN_POINT('Ctrl Pts',(56.0951464290126,26.8063360928474,14.9315852402157));
#55909=CARTESIAN_POINT('Ctrl Pts',(56.1669649164557,26.8436937775061,14.9358044195432));
#55910=CARTESIAN_POINT('Ctrl Pts',(56.2366400783236,26.8844216945044,14.9400235988707));
#55911=CARTESIAN_POINT('Ctrl Pts',(56.3065371020408,26.9252792986212,14.9442562130422));
#55912=CARTESIAN_POINT('Ctrl Pts',(56.3745370814643,26.969680616962,14.9484888272137));
#55913=CARTESIAN_POINT('Ctrl Pts',(56.4402582729453,27.0174243123621,14.9527214413852));
#55914=CARTESIAN_POINT('Ctrl Pts',(56.5058857193175,27.0650999058637,14.95694801813));
#55915=CARTESIAN_POINT('Ctrl Pts',(56.5692404608935,27.1161081366173,14.9611745948748));
#55916=CARTESIAN_POINT('Ctrl Pts',(56.6299669216089,27.170202720392,14.9654011716195));
#55917=CARTESIAN_POINT('Ctrl Pts',(56.6906259829848,27.2242372654426,14.9696230573536));
#55918=CARTESIAN_POINT('Ctrl Pts',(56.748662214615,27.2813510496237,14.9738449430876));
#55919=CARTESIAN_POINT('Ctrl Pts',(56.8037516712548,27.3412564518752,14.9780668288216));
#55920=CARTESIAN_POINT('Ctrl Pts',(56.8588039717645,27.4011214497907,14.9822858670246));
#55921=CARTESIAN_POINT('Ctrl Pts',(56.9109131310076,27.4637739851927,14.9865049052277));
#55922=CARTESIAN_POINT('Ctrl Pts',(56.9597916865599,27.5288892647762,14.9907239434307));
#55923=CARTESIAN_POINT('Ctrl Pts',(57.008654280158,27.5939832800834,14.9949416038497));
#55924=CARTESIAN_POINT('Ctrl Pts',(57.0542880865565,27.6615380711573,14.9991592642686));
#55925=CARTESIAN_POINT('Ctrl Pts',(57.0964464969875,27.7311964946182,15.0033769246876));
#55926=CARTESIAN_POINT('Ctrl Pts',(57.1386040301179,27.8008534685137,15.0075944973386));
#55927=CARTESIAN_POINT('Ctrl Pts',(57.1772860715491,27.8726135897216,15.0118120699897));
#55928=CARTESIAN_POINT('Ctrl Pts',(57.2122906147601,27.9460927527319,15.0160296426407));
#55929=CARTESIAN_POINT('Ctrl Pts',(57.2473545801392,28.0196966507271,15.020254374857));
#55930=CARTESIAN_POINT('Ctrl Pts',(57.2787283561513,28.095025007502,15.0244791070733));
#55931=CARTESIAN_POINT('Ctrl Pts',(57.3062569393779,28.1716708507053,15.0287038392896));
#55932=CARTESIAN_POINT('Ctrl Pts',(57.3337786470522,28.2482975508056,15.0329275163347));
#55933=CARTESIAN_POINT('Ctrl Pts',(57.3574569672904,28.3262406271011,15.0371511933798));
#55934=CARTESIAN_POINT('Ctrl Pts',(57.3771872893792,28.4050791302922,15.0413748704249));
#55935=CARTESIAN_POINT('Ctrl Pts',(57.3969534091905,28.4840606741717,15.0456062107011));
#55936=CARTESIAN_POINT('Ctrl Pts',(57.4127571253136,28.5639404346521,15.0498375509774));
#55937=CARTESIAN_POINT('Ctrl Pts',(57.4245451144589,28.6442877033983,15.0540688912536));
#55938=CARTESIAN_POINT('Ctrl Pts',(57.4362992247094,28.7244040526358,15.0582880705811));
#55939=CARTESIAN_POINT('Ctrl Pts',(57.4440606988487,28.8049847653453,15.0625072499086));
#55940=CARTESIAN_POINT('Ctrl Pts',(57.4478283089082,28.8856023596947,15.0667264292361));
#55941=CARTESIAN_POINT('Ctrl Pts',(57.4516079159106,28.9664766591326,15.0709590434076));
#55942=CARTESIAN_POINT('Ctrl Pts',(57.4513822135804,29.0476888708402,15.075191657579));
#55943=CARTESIAN_POINT('Ctrl Pts',(57.4471122670599,29.1288091704997,15.0794242717505));
#55944=CARTESIAN_POINT('Ctrl Pts',(57.4428484112173,29.2098137596685,15.0836508484953));
#55945=CARTESIAN_POINT('Ctrl Pts',(57.4345517928504,29.2907262371267,15.0878774252401));
#55946=CARTESIAN_POINT('Ctrl Pts',(57.4222354254891,29.3711142593674,15.0921040019849));
#55947=CARTESIAN_POINT('Ctrl Pts',(57.4099327278693,29.4514130602122,15.0963258877189));
#55948=CARTESIAN_POINT('Ctrl Pts',(57.3936192161576,29.5311881055644,15.1005477734529));
#55949=CARTESIAN_POINT('Ctrl Pts',(57.3733597981023,29.6100110808436,15.104769659187));
#55950=CARTESIAN_POINT('Ctrl Pts',(57.3531140443962,29.6887808924702,15.10898869739));
#55951=CARTESIAN_POINT('Ctrl Pts',(57.3289277854457,29.7665994606097,15.113207735593));
#55952=CARTESIAN_POINT('Ctrl Pts',(57.300916971293,29.8430488367917,15.117426773796));
#55953=CARTESIAN_POINT('Ctrl Pts',(57.272915304451,29.9194732473946,15.121644434215));
#55954=CARTESIAN_POINT('Ctrl Pts',(57.2410917224622,29.994528918152,15.125862094634));
#55955=CARTESIAN_POINT('Ctrl Pts',(57.2056115521912,30.0678145582642,15.130079755053));
#55956=CARTESIAN_POINT('Ctrl Pts',(57.1701321202491,30.1410986733299,15.134297327704));
#55957=CARTESIAN_POINT('Ctrl Pts',(57.1309964548012,30.2126124133733,15.1385149003551));
#55958=CARTESIAN_POINT('Ctrl Pts',(57.0884167807263,30.2819772228791,15.1427324730061));
#55959=CARTESIAN_POINT('Ctrl Pts',(57.0457648252755,30.3514597830249,15.1469572052224));
#55960=CARTESIAN_POINT('Ctrl Pts',(56.9996574082299,30.418785715986,15.1511819374387));
#55961=CARTESIAN_POINT('Ctrl Pts',(56.9503515242788,30.4836034449081,15.155406669655));
#55962=CARTESIAN_POINT('Ctrl Pts',(56.9010579549893,30.5484049849227,15.1596303467001));
#55963=CARTESIAN_POINT('Ctrl Pts',(56.8485678329195,30.6106992308592,15.1638540237452));
#55964=CARTESIAN_POINT('Ctrl Pts',(56.7931773108047,30.6701692674741,15.1680777007903));
#55965=CARTESIAN_POINT('Ctrl Pts',(56.737686290861,30.7297472035878,15.1723090410666));
#55966=CARTESIAN_POINT('Ctrl Pts',(56.6792846884101,30.7864903653685,15.1765403813428));
#55967=CARTESIAN_POINT('Ctrl Pts',(56.6183047632273,30.8401195459306,15.1807717216191));
#55968=CARTESIAN_POINT('Ctrl Pts',(56.557500095456,30.8935945952547,15.1849909009466));
#55969=CARTESIAN_POINT('Ctrl Pts',(56.4941323135716,30.9439733205334,15.1892100802741));
#55970=CARTESIAN_POINT('Ctrl Pts',(56.428559331612,30.9910219702615,15.1934292596016));
#55971=CARTESIAN_POINT('Ctrl Pts',(56.3627775500939,31.038220433785,15.1976618737731));
#55972=CARTESIAN_POINT('Ctrl Pts',(56.2945318256093,31.0822431025086,15.2018944879445));
#55973=CARTESIAN_POINT('Ctrl Pts',(56.2241615094716,31.1228233201866,15.206127102116));
#55974=CARTESIAN_POINT('Ctrl Pts',(56.1538915699823,31.1633456539945,15.2103536788608));
#55975=CARTESIAN_POINT('Ctrl Pts',(56.0815034569499,31.2004350591713,15.2145802556056));
#55976=CARTESIAN_POINT('Ctrl Pts',(56.0073669155911,31.2338670836405,15.2188068323504));
#55977=CARTESIAN_POINT('Ctrl Pts',(55.9333126572084,31.2672620024339,15.2230287180844));
#55978=CARTESIAN_POINT('Ctrl Pts',(55.8575142477203,31.297007416272,15.2272506038184));
#55979=CARTESIAN_POINT('Ctrl Pts',(55.780366304033,31.3229245966088,15.2314724895525));
#55980=CARTESIAN_POINT('Ctrl Pts',(55.7032703942412,31.3488242966111,15.2356915277555));
#55981=CARTESIAN_POINT('Ctrl Pts',(55.6248271972518,31.3709007436843,15.2399105659585));
#55982=CARTESIAN_POINT('Ctrl Pts',(55.5454504220818,31.3890236681646,15.2441296041615));
#55983=CARTESIAN_POINT('Ctrl Pts',(55.4660995684727,31.4071406743586,15.2483472645805));
#55984=CARTESIAN_POINT('Ctrl Pts',(55.3858161946883,31.4213066186349,15.2525649249995));
#55985=CARTESIAN_POINT('Ctrl Pts',(55.3050269176534,31.4314417183035,15.2567825854184));
#55986=CARTESIAN_POINT('Ctrl Pts',(55.2242393218128,31.4415766070646,15.2610001580695));
#55987=CARTESIAN_POINT('Ctrl Pts',(55.1429463047345,31.4476807613341,15.2652177307205));
#55988=CARTESIAN_POINT('Ctrl Pts',(55.0615809437297,31.4497261147666,15.2694353033715));
#55989=CARTESIAN_POINT('Ctrl Pts',(54.9800774604782,31.4517749403008,15.2736600355878));
#55990=CARTESIAN_POINT('Ctrl Pts',(54.8985018544371,31.4497511678989,15.2778847678041));
#55991=CARTESIAN_POINT('Ctrl Pts',(54.8172889452573,31.4436789724665,15.2821095000204));
#55992=CARTESIAN_POINT('Ctrl Pts',(54.7360963198532,31.4376082936285,15.2863331770655));
#55993=CARTESIAN_POINT('Ctrl Pts',(54.6552666700635,31.4274912927601,15.2905568541106));
#55994=CARTESIAN_POINT('Ctrl Pts',(54.5752270581772,31.4134038613326,15.2947805311557));
#55995=CARTESIAN_POINT('Ctrl Pts',(54.4950422263703,31.399290870365,15.299011871432));
#55996=CARTESIAN_POINT('Ctrl Pts',(54.4156507513243,31.3811931559315,15.3032432117082));
#55997=CARTESIAN_POINT('Ctrl Pts',(54.337467721308,31.35923742546,15.3074745519844));
#55998=CARTESIAN_POINT('Ctrl Pts',(54.2595093907386,31.3373447961562,15.311693731312));
#55999=CARTESIAN_POINT('Ctrl Pts',(54.1827529735009,31.3116165207669,15.3159129106395));
#56000=CARTESIAN_POINT('Ctrl Pts',(54.1075893949453,31.2822255721085,15.320132089967));
#56001=CARTESIAN_POINT('Ctrl Pts',(54.0321864781508,31.2527410358638,15.3243647041385));
#56002=CARTESIAN_POINT('Ctrl Pts',(53.9581061256139,31.2194607768503,15.32859731831));
#56003=CARTESIAN_POINT('Ctrl Pts',(53.8857567584493,31.1825242836355,15.3328299324814));
#56004=CARTESIAN_POINT('Ctrl Pts',(53.8135105908636,31.1456404768601,15.3370565092262));
#56005=CARTESIAN_POINT('Ctrl Pts',(53.7429909150328,31.105111003566,15.341283085971));
#56006=CARTESIAN_POINT('Ctrl Pts',(53.6745872966152,31.0611238234774,15.3455096627158));
#56007=CARTESIAN_POINT('Ctrl Pts',(53.6062595982932,31.0171854640652,15.3497315484498));
#56008=CARTESIAN_POINT('Ctrl Pts',(53.5400436795272,30.9697972732653,15.3539534341839));
#56009=CARTESIAN_POINT('Ctrl Pts',(53.4763042920924,30.9191929657291,15.3581753199179));
#56010=CARTESIAN_POINT('Ctrl Pts',(53.4126078948977,30.8686227892289,15.3623943581209));
#56011=CARTESIAN_POINT('Ctrl Pts',(53.3513850744741,30.8148410922616,15.366613396324));
#56012=CARTESIAN_POINT('Ctrl Pts',(53.2929703278242,30.7581239854775,15.370832434527));
#56013=CARTESIAN_POINT('Ctrl Pts',(53.2345746573009,30.7014254004328,15.375050094946));
#56014=CARTESIAN_POINT('Ctrl Pts',(53.178985572454,30.6417936326464,15.3792677553649));
#56015=CARTESIAN_POINT('Ctrl Pts',(53.1265022476143,30.5795431053965,15.3834854157839));
#56016=CARTESIAN_POINT('Ctrl Pts',(53.0740200149327,30.5172938735565,15.387702988435));
#56017=CARTESIAN_POINT('Ctrl Pts',(53.0246437122983,30.4524263465249,15.391920561086));
#56018=CARTESIAN_POINT('Ctrl Pts',(52.9786326501071,30.3852885211345,15.3961381337371));
#56019=CARTESIAN_POINT('Ctrl Pts',(52.932543481567,30.3180367255342,15.4003628659534));
#56020=CARTESIAN_POINT('Ctrl Pts',(52.889831247212,30.2485073059185,15.4045875981696));
#56021=CARTESIAN_POINT('Ctrl Pts',(52.8507123846899,30.1770781608181,15.4088123303859));
#56022=CARTESIAN_POINT('Ctrl Pts',(52.811603292514,30.1056668558956,15.413036007431));
#56023=CARTESIAN_POINT('Ctrl Pts',(52.7760859615526,30.0323572030995,15.4172596844762));
#56024=CARTESIAN_POINT('Ctrl Pts',(52.7443292251793,29.95754874843,15.4214833615213));
#56025=CARTESIAN_POINT('Ctrl Pts',(52.7125148709512,29.8826045649931,15.4257147017975));
#56026=CARTESIAN_POINT('Ctrl Pts',(52.6844749073509,29.8061565825541,15.4299460420738));
#56027=CARTESIAN_POINT('Ctrl Pts',(52.6603290233795,29.7286219672503,15.43417738235));
#56028=CARTESIAN_POINT('Ctrl Pts',(52.6362525351169,29.651310187838,15.4383965616775));
#56029=CARTESIAN_POINT('Ctrl Pts',(52.616047806141,29.572918474828,15.442615741005));
#56030=CARTESIAN_POINT('Ctrl Pts',(52.5997825625659,29.493868912807,15.4468349203325));
#56031=CARTESIAN_POINT('Ctrl Pts',(52.5767052804375,29.3817126431234,15.4528211320508));
#56032=CARTESIAN_POINT('Ctrl Pts',(52.5614830118809,29.2678893779456,15.4588073437692));
#56033=CARTESIAN_POINT('Ctrl Pts',(52.5543005723774,29.1533119686342,15.4647935554875));
#56034=CARTESIAN_POINT('Ctrl Pts',(52.551149438172,29.1030437006629,15.4674198715877));
#56035=CARTESIAN_POINT('Ctrl Pts',(52.5495452631465,29.0526305694615,15.4700461876878));
#56036=CARTESIAN_POINT('Ctrl Pts',(52.5495009444412,29.0021514426317,15.472672503788));
#56037=CARTESIAN_POINT('',(52.5495000114917,28.9997626798325,16.2726725038352));
#56038=CARTESIAN_POINT('Ctrl Pts',(52.5495009444406,29.0021514419089,15.4726725038256));
#56039=CARTESIAN_POINT('Ctrl Pts',(52.549430024194,28.9213730595116,15.4768752224453));
#56040=CARTESIAN_POINT('Ctrl Pts',(52.5533576597404,28.8404682849032,15.4810779410649));
#56041=CARTESIAN_POINT('Ctrl Pts',(52.5612936946831,28.7598712711745,15.4852806596846));
#56042=CARTESIAN_POINT('Ctrl Pts',(52.5691505346619,28.6800785479546,15.4894414387021));
#56043=CARTESIAN_POINT('Ctrl Pts',(52.5809360959679,28.6005879586768,15.4936022177195));
#56044=CARTESIAN_POINT('Ctrl Pts',(52.5966076728007,28.5218205655202,15.497762996737));
#56045=CARTESIAN_POINT('Ctrl Pts',(52.6122717977342,28.4430906265831,15.5019217972869));
#56046=CARTESIAN_POINT('Ctrl Pts',(52.6318181789659,28.3650836706248,15.5060805978368));
#56047=CARTESIAN_POINT('Ctrl Pts',(52.6551526313549,28.2882127651059,15.5102393983867));
#56048=CARTESIAN_POINT('Ctrl Pts',(52.6784836046501,28.2113533207985,15.5143975788724));
#56049=CARTESIAN_POINT('Ctrl Pts',(52.7056013878003,28.1356300487177,15.5185557593582));
#56050=CARTESIAN_POINT('Ctrl Pts',(52.7363617703766,28.0614414161132,15.5227139398439));
#56051=CARTESIAN_POINT('Ctrl Pts',(52.7676927790396,27.9858765337503,15.5269492574151));
#56052=CARTESIAN_POINT('Ctrl Pts',(52.8028027287989,27.9119042896829,15.5311845749863));
#56053=CARTESIAN_POINT('Ctrl Pts',(52.8414884899115,27.839923144436,15.5354198925574));
#56054=CARTESIAN_POINT('Ctrl Pts',(52.8795176709094,27.7691636731909,15.5395833277301));
#56055=CARTESIAN_POINT('Ctrl Pts',(52.9210019170919,27.7003286210923,15.5437467629028));
#56056=CARTESIAN_POINT('Ctrl Pts',(52.9657035541437,27.6337686065764,15.5479101980755));
#56057=CARTESIAN_POINT('Ctrl Pts',(53.0115628629572,27.5654848375327,15.5521814568459));
#56058=CARTESIAN_POINT('Ctrl Pts',(53.0608082015571,27.4995960132654,15.5564527156163));
#56059=CARTESIAN_POINT('Ctrl Pts',(53.113139302838,27.4364441297142,15.5607239743867));
#56060=CARTESIAN_POINT('Ctrl Pts',(53.1654704041189,27.373292246163,15.5649952331571));
#56061=CARTESIAN_POINT('Ctrl Pts',(53.2208868506974,27.3128776476264,15.5692664919275));
#56062=CARTESIAN_POINT('Ctrl Pts',(53.2790499887541,27.2554996965341,15.5735377506979));
#56063=CARTESIAN_POINT('Ctrl Pts',(53.3366868905738,27.1986408776289,15.5777703648694));
#56064=CARTESIAN_POINT('Ctrl Pts',(53.397251858526,27.1445358045864,15.5820029790409));
#56065=CARTESIAN_POINT('Ctrl Pts',(53.4604511639577,27.0935006867453,15.5862355932123));
#56066=CARTESIAN_POINT('Ctrl Pts',(53.5235603215144,27.0425383657077,15.5904621699571));
#56067=CARTESIAN_POINT('Ctrl Pts',(53.5892959949858,26.9946375920394,15.5946887467019));
#56068=CARTESIAN_POINT('Ctrl Pts',(53.6573278653092,26.9500776139754,15.5989153234467));
#56069=CARTESIAN_POINT('Ctrl Pts',(53.7252842281344,26.9055670923271,15.6031372091807));
#56070=CARTESIAN_POINT('Ctrl Pts',(53.7955313372712,26.8643902519524,15.6073590949148));
#56071=CARTESIAN_POINT('Ctrl Pts',(53.8677071906201,26.8267850442659,15.6115809806488));
#56072=CARTESIAN_POINT('Ctrl Pts',(53.9398343635942,26.7892052001257,15.6158000188518));
#56073=CARTESIAN_POINT('Ctrl Pts',(54.0138872862032,26.755192418376,15.6200190570549));
#56074=CARTESIAN_POINT('Ctrl Pts',(54.0894775569006,26.7249397523115,15.6242380952579));
#56075=CARTESIAN_POINT('Ctrl Pts',(54.1650431425715,26.6946969656648,15.6284557556768));
#56076=CARTESIAN_POINT('Ctrl Pts',(54.2421446483471,26.6682120286141,15.6326734160958));
#56077=CARTESIAN_POINT('Ctrl Pts',(54.3203730665648,26.6456301307251,15.6368910765148));
#56078=CARTESIAN_POINT('Ctrl Pts',(54.3985998568789,26.6230487027569,15.6411086491658));
#56079=CARTESIAN_POINT('Ctrl Pts',(54.4779530663593,26.604370280173,15.6453262218169));
#56080=CARTESIAN_POINT('Ctrl Pts',(54.5580092589447,26.5896899712233,15.649543794468));
#56081=CARTESIAN_POINT('Ctrl Pts',(54.6382013513901,26.574984741629,15.6537685266842));
#56082=CARTESIAN_POINT('Ctrl Pts',(54.7190983552261,26.5642912891443,15.6579932589005));
#56083=CARTESIAN_POINT('Ctrl Pts',(54.8002669849083,26.5576533880953,15.6622179911168));
#56084=CARTESIAN_POINT('Ctrl Pts',(54.881415341874,26.5510171449317,15.6664416681619));
#56085=CARTESIAN_POINT('Ctrl Pts',(54.9628347224271,26.5484344211631,15.670665345207));
#56086=CARTESIAN_POINT('Ctrl Pts',(55.0440914571839,26.5498966974016,15.6748890222522));
#56087=CARTESIAN_POINT('Ctrl Pts',(55.125495620149,26.551361626722,15.6791203625284));
#56088=CARTESIAN_POINT('Ctrl Pts',(55.2067360827534,26.5568861912774,15.6833517028047));
#56089=CARTESIAN_POINT('Ctrl Pts',(55.2873830972079,26.5664098115255,15.6875830430809));
#56090=CARTESIAN_POINT('Ctrl Pts',(55.3677983306794,26.5759060607162,15.6918022224084));
#56091=CARTESIAN_POINT('Ctrl Pts',(55.4476230875475,26.5893782517992,15.6960214017359));
#56092=CARTESIAN_POINT('Ctrl Pts',(55.5264442901062,26.6067163437205,15.7002405810634));
#56093=CARTESIAN_POINT('Ctrl Pts',(55.605516477626,26.6241096441414,15.7044731952349));
#56094=CARTESIAN_POINT('Ctrl Pts',(55.6838727952094,26.6454582217696,15.7087058094064));
#56095=CARTESIAN_POINT('Ctrl Pts',(55.7610880923709,26.6706878342199,15.7129384235779));
#56096=CARTESIAN_POINT('Ctrl Pts',(55.8381932491612,26.695881458997,15.7171650003226));
#56097=CARTESIAN_POINT('Ctrl Pts',(55.9141601801648,26.7249449804399,15.7213915770674));
#56098=CARTESIAN_POINT('Ctrl Pts',(55.9885748189535,26.7577533415498,15.7256181538122));
#56099=CARTESIAN_POINT('Ctrl Pts',(56.06290686611,26.790525289178,15.7298400395463));
#56100=CARTESIAN_POINT('Ctrl Pts',(56.1356896214532,26.827033631375,15.7340619252803));
#56101=CARTESIAN_POINT('Ctrl Pts',(56.2065264110986,26.8671042525896,15.7382838110143));
#56102=CARTESIAN_POINT('Ctrl Pts',(56.2773154235262,26.9071478474128,15.7425028492173));
#56103=CARTESIAN_POINT('Ctrl Pts',(56.3461606736869,26.9507487212528,15.7467218874204));
#56104=CARTESIAN_POINT('Ctrl Pts',(56.4126887774916,26.9976861714633,15.7509409256234));
#56105=CARTESIAN_POINT('Ctrl Pts',(56.4791951556432,27.0446082936139,15.7551585860424));
#56106=CARTESIAN_POINT('Ctrl Pts',(56.5433855108962,27.0948645606454,15.7593762464613));
#56107=CARTESIAN_POINT('Ctrl Pts',(56.6049153904789,27.1481909279291,15.7635939068803));
#56108=CARTESIAN_POINT('Ctrl Pts',(56.6664439896479,27.2015161855112,15.7678114795314));
#56109=CARTESIAN_POINT('Ctrl Pts',(56.7253118729403,27.2579111111848,15.7720290521824));
#56110=CARTESIAN_POINT('Ctrl Pts',(56.7812087422233,27.3170722931073,15.7762466248335));
#56111=CARTESIAN_POINT('Ctrl Pts',(56.8372004995652,27.3763339044417,15.7804713570498));
#56112=CARTESIAN_POINT('Ctrl Pts',(56.8902108313902,27.4383708279268,15.784696089266));
#56113=CARTESIAN_POINT('Ctrl Pts',(56.9399671376895,27.5028434434954,15.7889208214823));
#56114=CARTESIAN_POINT('Ctrl Pts',(56.9897110168295,27.5672999563521,15.7931444985274));
#56115=CARTESIAN_POINT('Ctrl Pts',(57.0362022471007,27.634190549858,15.7973681755725));
#56116=CARTESIAN_POINT('Ctrl Pts',(57.0792118848184,27.7031468132322,15.8015918526176));
#56117=CARTESIAN_POINT('Ctrl Pts',(57.1222995570996,27.7722281874466,15.8058231928939));
#56118=CARTESIAN_POINT('Ctrl Pts',(57.1618927863232,27.8433823143637,15.8100545331701));
#56119=CARTESIAN_POINT('Ctrl Pts',(57.1978084330948,27.9162157311451,15.8142858734464));
#56120=CARTESIAN_POINT('Ctrl Pts',(57.2336208576457,27.9888398233648,15.8185050527739));
#56121=CARTESIAN_POINT('Ctrl Pts',(57.2657767058958,28.0631331148853,15.8227242321014));
#56122=CARTESIAN_POINT('Ctrl Pts',(57.2941434032208,28.1386891992674,15.8269434114289));
#56123=CARTESIAN_POINT('Ctrl Pts',(57.3226004266787,28.214485871718,15.8311760256004));
#56124=CARTESIAN_POINT('Ctrl Pts',(57.3473499436632,28.2918353105073,15.8354086397718));
#56125=CARTESIAN_POINT('Ctrl Pts',(57.3682227782928,28.3703404710679,15.8396412539433));
#56126=CARTESIAN_POINT('Ctrl Pts',(57.3890658397837,28.4487336513884,15.8438678306881));
#56127=CARTESIAN_POINT('Ctrl Pts',(57.406043083288,28.5282788340695,15.8480944074329));
#56128=CARTESIAN_POINT('Ctrl Pts',(57.4190339916735,28.6085606086146,15.8523209841777));
#56129=CARTESIAN_POINT('Ctrl Pts',(57.432010481655,28.6887532796861,15.8565428699117));
#56130=CARTESIAN_POINT('Ctrl Pts',(57.4410093539002,28.7696804619158,15.8607647556457));
#56131=CARTESIAN_POINT('Ctrl Pts',(57.4459607113437,28.8509146265958,15.8649866413798));
#56132=CARTESIAN_POINT('Ctrl Pts',(57.4509087292501,28.9320940013509,15.8692056795828));
#56133=CARTESIAN_POINT('Ctrl Pts',(57.451814626031,29.0135794848453,15.8734247177858));
#56134=CARTESIAN_POINT('Ctrl Pts',(57.4486602620347,29.094937722387,15.8776437559888));
#56135=CARTESIAN_POINT('Ctrl Pts',(57.4455069281387,29.1762693912945,15.8818614164078));
#56136=CARTESIAN_POINT('Ctrl Pts',(57.4382959846715,29.2574734329289,15.8860790768268));
#56137=CARTESIAN_POINT('Ctrl Pts',(57.427061398562,29.3381171655067,15.8902967372457));
#56138=CARTESIAN_POINT('Ctrl Pts',(57.41582704624,29.418759219919,15.8945143098968));
#56139=CARTESIAN_POINT('Ctrl Pts',(57.4005692830146,29.4988405285149,15.8987318825478));
#56140=CARTESIAN_POINT('Ctrl Pts',(57.38137369184,29.5779356277409,15.9029494551989));
#56141=CARTESIAN_POINT('Ctrl Pts',(57.3621455150769,29.6571649953173,15.9071741874152));
#56142=CARTESIAN_POINT('Ctrl Pts',(57.3389662460126,29.7354043501289,15.9113989196315));
#56143=CARTESIAN_POINT('Ctrl Pts',(57.3119723628627,29.812240138973,15.9156236518477));
#56144=CARTESIAN_POINT('Ctrl Pts',(57.2849852217183,29.8890567372731,15.9198473288929));
#56145=CARTESIAN_POINT('Ctrl Pts',(57.254185567653,29.964470047114,15.924071005938));
#56146=CARTESIAN_POINT('Ctrl Pts',(57.2197577957976,30.0380874616312,15.9282946829831));
#56147=CARTESIAN_POINT('Ctrl Pts',(57.1852675598924,30.1118384439513,15.9325260232593));
#56148=CARTESIAN_POINT('Ctrl Pts',(57.1471362691119,30.1837866075215,15.9367573635356));
#56149=CARTESIAN_POINT('Ctrl Pts',(57.1055942687773,30.253564128911,15.9409887038118));
#56150=CARTESIAN_POINT('Ctrl Pts',(57.0641716609055,30.3231411084376,15.9452078831393));
#56151=CARTESIAN_POINT('Ctrl Pts',(57.0193582434643,30.3905595729623,15.9494270624668));
#56152=CARTESIAN_POINT('Ctrl Pts',(56.9714227466952,30.4554870675525,15.9536462417943));
#56153=CARTESIAN_POINT('Ctrl Pts',(56.9233346122044,30.5206213063203,15.9578788559658));
#56154=CARTESIAN_POINT('Ctrl Pts',(56.8719256086231,30.5834909223741,15.9621114701373));
#56155=CARTESIAN_POINT('Ctrl Pts',(56.8174366874645,30.643737855334,15.9663440843087));
#56156=CARTESIAN_POINT('Ctrl Pts',(56.7630254896356,30.7038988517011,15.9705706610535));
#56157=CARTESIAN_POINT('Ctrl Pts',(56.7055434087358,30.7614442534303,15.9747972377983));
#56158=CARTESIAN_POINT('Ctrl Pts',(56.6452732919455,30.8160468179017,15.9790238145431));
#56159=CARTESIAN_POINT('Ctrl Pts',(56.5850700680058,30.8705887798493,15.9832457002771));
#56160=CARTESIAN_POINT('Ctrl Pts',(56.5220852992742,30.9221940841614,15.9874675860112));
#56161=CARTESIAN_POINT('Ctrl Pts',(56.4566395555974,30.970571352443,15.9916894717452));
#56162=CARTESIAN_POINT('Ctrl Pts',(56.3912379530452,31.0189159917573,15.9959085099482));
#56163=CARTESIAN_POINT('Ctrl Pts',(56.3233790447604,31.0640366437438,16.0001275481512));
#56164=CARTESIAN_POINT('Ctrl Pts',(56.25341646435,31.1056821737613,16.0043465863543));
#56165=CARTESIAN_POINT('Ctrl Pts',(56.1834767311677,31.1473141038671,16.0085642467732));
#56166=CARTESIAN_POINT('Ctrl Pts',(56.1114350890396,31.1854729283111,16.0127819071922));
#56167=CARTESIAN_POINT('Ctrl Pts',(56.0376729739848,31.2199515870986,16.0169995676112));
#56168=CARTESIAN_POINT('Ctrl Pts',(55.9639123938918,31.2544295283982,16.0212171402622));
#56169=CARTESIAN_POINT('Ctrl Pts',(55.888431833396,31.2852272606572,16.0254347129133));
#56170=CARTESIAN_POINT('Ctrl Pts',(55.8116347734886,31.3121849503152,16.0296522855643));
#56171=CARTESIAN_POINT('Ctrl Pts',(55.7347073462809,31.3391884021577,16.0338770177806));
#56172=CARTESIAN_POINT('Ctrl Pts',(55.6564593889215,31.3623386143548,16.0381017499969));
#56173=CARTESIAN_POINT('Ctrl Pts',(55.5773120991202,31.3815249295797,16.0423264822132));
#56174=CARTESIAN_POINT('Ctrl Pts',(55.4981845771843,31.4007064528212,16.0465501592583));
#56175=CARTESIAN_POINT('Ctrl Pts',(55.4181586339014,31.4159259926763,16.0507738363034));
#56176=CARTESIAN_POINT('Ctrl Pts',(55.3376639826716,31.4271244889388,16.0549975133486));
#56177=CARTESIAN_POINT('Ctrl Pts',(55.2570232859202,31.4383433032001,16.0592288536248));
#56178=CARTESIAN_POINT('Ctrl Pts',(55.175912645807,31.4455264527967,16.0634601939011));
#56179=CARTESIAN_POINT('Ctrl Pts',(55.0947660020834,31.4486669138225,16.0676915341773));
#56180=CARTESIAN_POINT('Ctrl Pts',(55.0138525752865,31.4517983491064,16.0719107135048));
#56181=CARTESIAN_POINT('Ctrl Pts',(54.9329038058637,31.4509103904747,16.0761298928323));
#56182=CARTESIAN_POINT('Ctrl Pts',(54.8523448623591,31.4460474669001,16.0803490721598));
#56183=CARTESIAN_POINT('Ctrl Pts',(54.771529400524,31.4411690586507,16.0845816863313));
#56184=CARTESIAN_POINT('Ctrl Pts',(54.6908056775416,31.4322721592,16.0888143005027));
#56185=CARTESIAN_POINT('Ctrl Pts',(54.6106052176895,31.4193639563963,16.0930469146742));
#56186=CARTESIAN_POINT('Ctrl Pts',(54.5305191562626,31.4064741659317,16.097273491419));
#56187=CARTESIAN_POINT('Ctrl Pts',(54.4509553303829,31.3895845094472,16.1015000681638));
#56188=CARTESIAN_POINT('Ctrl Pts',(54.3723422216486,31.3687540951469,16.1057266449086));
#56189=CARTESIAN_POINT('Ctrl Pts',(54.2938163643621,31.3479468001944,16.1099485306426));
#56190=CARTESIAN_POINT('Ctrl Pts',(54.2162395743571,31.3232075565149,16.1141704163767));
#56191=CARTESIAN_POINT('Ctrl Pts',(54.1400307856651,31.2946466395496,16.1183923021107));
#56192=CARTESIAN_POINT('Ctrl Pts',(54.0638733974379,31.2661049860372,16.1226113403137));
#56193=CARTESIAN_POINT('Ctrl Pts',(53.9890826118921,31.2337469411841,16.1268303785167));
#56194=CARTESIAN_POINT('Ctrl Pts',(53.9160616055209,31.1977324238802,16.1310494167197));
#56195=CARTESIAN_POINT('Ctrl Pts',(53.8430644451482,31.1617296676045,16.1352670771387));
#56196=CARTESIAN_POINT('Ctrl Pts',(53.7718363324972,31.122073015557,16.1394847375576));
#56197=CARTESIAN_POINT('Ctrl Pts',(53.7027586087915,31.0789697022649,16.1437023979766));
#56198=CARTESIAN_POINT('Ctrl Pts',(53.6336823225671,31.0358672859364,16.1479199706277));
#56199=CARTESIAN_POINT('Ctrl Pts',(53.56675672981,30.9893185978865,16.1521375432787));
#56200=CARTESIAN_POINT('Ctrl Pts',(53.5023355583198,30.9395750746302,16.1563551159298));
#56201=CARTESIAN_POINT('Ctrl Pts',(53.4378050282915,30.8897471089638,16.160579848146));
#56202=CARTESIAN_POINT('Ctrl Pts',(53.3757877952056,30.8367137425227,16.1648045803623));
#56203=CARTESIAN_POINT('Ctrl Pts',(53.3166059815924,30.7807680446339,16.1690293125786));
#56204=CARTESIAN_POINT('Ctrl Pts',(53.2574389492577,30.7248363197699,16.1732529896237));
#56205=CARTESIAN_POINT('Ctrl Pts',(53.2011062272324,30.6659940694652,16.1774766666688));
#56206=CARTESIAN_POINT('Ctrl Pts',(53.1478912930289,30.6045695957365,16.1817003437139));
#56207=CARTESIAN_POINT('Ctrl Pts',(53.0945798082758,30.5430336764749,16.1859316839902));
#56208=CARTESIAN_POINT('Ctrl Pts',(53.0443977033076,30.4789065377686,16.1901630242664));
#56209=CARTESIAN_POINT('Ctrl Pts',(52.9975871071046,30.4125483554082,16.1943943645427));
#56210=CARTESIAN_POINT('Ctrl Pts',(52.9509110454044,30.3463808876679,16.1986135438702));
#56211=CARTESIAN_POINT('Ctrl Pts',(52.9075873121655,30.2779956123529,16.2028327231977));
#56212=CARTESIAN_POINT('Ctrl Pts',(52.8678101013429,30.2077733587328,16.2070519025252));
#56213=CARTESIAN_POINT('Ctrl Pts',(52.8261868754805,30.1342921703196,16.2114668891588));
#56214=CARTESIAN_POINT('Ctrl Pts',(52.788303131255,30.0585462817474,16.2158818757924));
#56215=CARTESIAN_POINT('Ctrl Pts',(52.7544002788845,29.9809343212091,16.220296862426));
#56216=CARTESIAN_POINT('Ctrl Pts',(52.7205854081671,29.9035237722959,16.2247003916808));
#56217=CARTESIAN_POINT('Ctrl Pts',(52.6907310153447,29.8242571676171,16.2291039209355));
#56218=CARTESIAN_POINT('Ctrl Pts',(52.6650326032107,29.7435573319732,16.2335074501903));
#56219=CARTESIAN_POINT('Ctrl Pts',(52.639373597316,29.6629812423809,16.2379042270229));
#56220=CARTESIAN_POINT('Ctrl Pts',(52.6178580208794,29.5809766782397,16.2423010038556));
#56221=CARTESIAN_POINT('Ctrl Pts',(52.6006334744758,29.4979864718987,16.2466977806882));
#56222=CARTESIAN_POINT('Ctrl Pts',(52.5834410517142,29.4151510416315,16.2510863575671));
#56223=CARTESIAN_POINT('Ctrl Pts',(52.5705238034113,29.3313340272056,16.2554749344459));
#56224=CARTESIAN_POINT('Ctrl Pts',(52.5619792507151,29.2469920566668,16.2598635113248));
#56225=CARTESIAN_POINT('Ctrl Pts',(52.5536662209177,29.1649354131899,16.2641331754791));
#56226=CARTESIAN_POINT('Ctrl Pts',(52.5494920101768,29.0823822816067,16.2684028396335));
#56227=CARTESIAN_POINT('Ctrl Pts',(52.5495000114916,28.9997626807474,16.2726725037879));
#56228=CARTESIAN_POINT('',(52.5495007998519,28.9980200824703,17.0726725037486));
#56229=CARTESIAN_POINT('Ctrl Pts',(52.5495000114917,28.9997626798325,16.2726725038352));
#56230=CARTESIAN_POINT('Ctrl Pts',(52.5495083514886,28.9136462633258,16.277122878478));
#56231=CARTESIAN_POINT('Ctrl Pts',(52.5540604740065,28.8276303692676,16.2815732531209));
#56232=CARTESIAN_POINT('Ctrl Pts',(52.5630991174095,28.7421932149272,16.2860236277637));
#56233=CARTESIAN_POINT('Ctrl Pts',(52.572165603043,28.6564928838203,16.2904877111404));
#56234=CARTESIAN_POINT('Ctrl Pts',(52.5857461974439,28.5713752385803,16.2949517945171));
#56235=CARTESIAN_POINT('Ctrl Pts',(52.6037321076618,28.4873105831509,16.2994158778938));
#56236=CARTESIAN_POINT('Ctrl Pts',(52.6217470390047,28.4031102853858,16.3038871642821));
#56237=CARTESIAN_POINT('Ctrl Pts',(52.6441813651551,28.3199667357462,16.3083584506705));
#56238=CARTESIAN_POINT('Ctrl Pts',(52.6708765315756,28.2383346411747,16.3128297370589));
#56239=CARTESIAN_POINT('Ctrl Pts',(52.697646299248,28.1564744207934,16.3173135187266));
#56240=CARTESIAN_POINT('Ctrl Pts',(52.728700575226,28.0761344581581,16.3217973003944));
#56241=CARTESIAN_POINT('Ctrl Pts',(52.7638324599678,27.9977500397076,16.3262810820621));
#56242=CARTESIAN_POINT('Ctrl Pts',(52.7833519533301,27.9541991699804,16.328772299005));
#56243=CARTESIAN_POINT('Ctrl Pts',(52.8041293765503,27.9112515299105,16.3312635159478));
#56244=CARTESIAN_POINT('Ctrl Pts',(52.8261233377633,27.8689781136589,16.3337547328906));
#56245=CARTESIAN_POINT('Ctrl Pts',(52.863491400864,27.7971549586266,16.3379873470621));
#56246=CARTESIAN_POINT('Ctrl Pts',(52.9044922481289,27.7270521427378,16.3422199612336));
#56247=CARTESIAN_POINT('Ctrl Pts',(52.948943574148,27.6590608559778,16.3464525754051));
#56248=CARTESIAN_POINT('Ctrl Pts',(52.9933314945241,27.5911665524043,16.3506791521498));
#56249=CARTESIAN_POINT('Ctrl Pts',(53.0411598662639,27.5253781815362,16.3549057288946));
#56250=CARTESIAN_POINT('Ctrl Pts',(53.0922002035034,27.4620630095848,16.3591323056394));
#56251=CARTESIAN_POINT('Ctrl Pts',(53.1431838918788,27.3988181101425,16.3633541913734));
#56252=CARTESIAN_POINT('Ctrl Pts',(53.1973721722039,27.3380413152227,16.3675760771075));
#56253=CARTESIAN_POINT('Ctrl Pts',(53.2544937151468,27.2800703329677,16.3717979628415));
#56254=CARTESIAN_POINT('Ctrl Pts',(53.3115767313805,27.2221384503424,16.3760170010445));
#56255=CARTESIAN_POINT('Ctrl Pts',(53.3715887557567,27.1670089518904,16.3802360392476));
#56256=CARTESIAN_POINT('Ctrl Pts',(53.4342195362188,27.114984936601,16.3844550774506));
#56257=CARTESIAN_POINT('Ctrl Pts',(53.4968298637513,27.0629779104584,16.3886727378696));
#56258=CARTESIAN_POINT('Ctrl Pts',(53.5620568919404,27.0140746500654,16.3928903982885));
#56259=CARTESIAN_POINT('Ctrl Pts',(53.6295560472169,26.9685390423933,16.3971080587075));
#56260=CARTESIAN_POINT('Ctrl Pts',(53.6970537978615,26.9230043823,16.4013256313585));
#56261=CARTESIAN_POINT('Ctrl Pts',(53.7668231958184,26.8808374944166,16.4055432040096));
#56262=CARTESIAN_POINT('Ctrl Pts',(53.8384905429322,26.8422590444768,16.4097607766606));
#56263=CARTESIAN_POINT('Ctrl Pts',(53.9102795493723,26.8036151054626,16.4139855088769));
#56264=CARTESIAN_POINT('Ctrl Pts',(53.9839725399857,26.7685720135591,16.4182102410932));
#56265=CARTESIAN_POINT('Ctrl Pts',(54.0591706641969,26.7373046137643,16.4224349733095));
#56266=CARTESIAN_POINT('Ctrl Pts',(54.134350006888,26.7060450233305,16.4266586503546));
#56267=CARTESIAN_POINT('Ctrl Pts',(54.2110332854379,26.6785593764845,16.4308823273997));
#56268=CARTESIAN_POINT('Ctrl Pts',(54.28880520915,26.6549728744708,16.4351060044448));
#56269=CARTESIAN_POINT('Ctrl Pts',(54.3667182384014,26.6313435782722,16.4393373447211));
#56270=CARTESIAN_POINT('Ctrl Pts',(54.445723408118,26.6116276776904,16.4435686849973));
#56271=CARTESIAN_POINT('Ctrl Pts',(54.5253931562493,26.5958996289953,16.4478000252736));
#56272=CARTESIAN_POINT('Ctrl Pts',(54.6048339320789,26.5802167829975,16.4520192046011));
#56273=CARTESIAN_POINT('Ctrl Pts',(54.6849350089078,26.568498880775,16.4562383839286));
#56274=CARTESIAN_POINT('Ctrl Pts',(54.7652694833726,26.5607681876124,16.4604575632561));
#56275=CARTESIAN_POINT('Ctrl Pts',(54.8458597614063,26.5530128781326,16.4646901774276));
#56276=CARTESIAN_POINT('Ctrl Pts',(54.9269846661948,26.5492413936723,16.4689227915991));
#56277=CARTESIAN_POINT('Ctrl Pts',(55.0082168104974,26.5495137759977,16.4731554057706));
#56278=CARTESIAN_POINT('Ctrl Pts',(55.0893330847734,26.5497857697952,16.4773819825153));
#56279=CARTESIAN_POINT('Ctrl Pts',(55.1705558340651,26.554090172453,16.4816085592601));
#56280=CARTESIAN_POINT('Ctrl Pts',(55.2514525983209,26.5624352642858,16.4858351360049));
#56281=CARTESIAN_POINT('Ctrl Pts',(55.332259576536,26.5707710940329,16.4900570217389));
#56282=CARTESIAN_POINT('Ctrl Pts',(55.412740828855,26.5831386544429,16.494278907473));
#56283=CARTESIAN_POINT('Ctrl Pts',(55.4924653652614,26.5994941962124,16.498500793207));
#56284=CARTESIAN_POINT('Ctrl Pts',(55.5721361299403,26.6158387066761,16.50271983141));
#56285=CARTESIAN_POINT('Ctrl Pts',(55.6510507384723,26.6361657632645,16.5069388696131));
#56286=CARTESIAN_POINT('Ctrl Pts',(55.7287860423086,26.6603801260598,16.5111579078161));
#56287=CARTESIAN_POINT('Ctrl Pts',(55.8064959606288,26.6845865813269,16.515375568235));
#56288=CARTESIAN_POINT('Ctrl Pts',(55.8830268958855,26.7126776836939,16.519593228654));
#56289=CARTESIAN_POINT('Ctrl Pts',(55.957969906901,26.7445080564382,16.523810889073));
#56290=CARTESIAN_POINT('Ctrl Pts',(56.0329113583808,26.7763377668045,16.528028461724));
#56291=CARTESIAN_POINT('Ctrl Pts',(56.1062645241991,26.8119064101505,16.5322460343751));
#56292=CARTESIAN_POINT('Ctrl Pts',(56.1776408627946,26.8510206496394,16.5364636070261));
#56293=CARTESIAN_POINT('Ctrl Pts',(56.2491383667132,26.8902012877354,16.5406883392424));
#56294=CARTESIAN_POINT('Ctrl Pts',(56.3186519197543,26.9329393398588,16.5449130714587));
#56295=CARTESIAN_POINT('Ctrl Pts',(56.3858177229479,26.978995425843,16.549137803675));
#56296=CARTESIAN_POINT('Ctrl Pts',(56.4529667507777,27.0250400088366,16.5533614807201));
#56297=CARTESIAN_POINT('Ctrl Pts',(56.5177688434134,27.074400669101,16.5575851577652));
#56298=CARTESIAN_POINT('Ctrl Pts',(56.5798928943025,27.1267972099817,16.5618088348103));
#56299=CARTESIAN_POINT('Ctrl Pts',(56.6421296600028,27.1792888165596,16.5660401750865));
#56300=CARTESIAN_POINT('Ctrl Pts',(56.7016783328847,27.2348269938406,16.5702715153628));
#56301=CARTESIAN_POINT('Ctrl Pts',(56.7582436920257,27.2930936260439,16.574502855639));
#56302=CARTESIAN_POINT('Ctrl Pts',(56.8146464812982,27.3511927988891,16.5787220349665));
#56303=CARTESIAN_POINT('Ctrl Pts',(56.8680828441032,27.4120043674583,16.5829412142941));
#56304=CARTESIAN_POINT('Ctrl Pts',(56.918301697223,27.4751823556794,16.5871603936216));
#56305=CARTESIAN_POINT('Ctrl Pts',(56.9686804587996,27.5385615172444,16.5913930077931));
#56306=CARTESIAN_POINT('Ctrl Pts',(57.0160085386848,27.6045579347712,16.5956256219645));
#56307=CARTESIAN_POINT('Ctrl Pts',(57.0600029023717,27.6728457918463,16.599858236136));
#56308=CARTESIAN_POINT('Ctrl Pts',(57.1039345122297,27.7410362427052,16.6040848128808));
#56309=CARTESIAN_POINT('Ctrl Pts',(57.1445416008929,27.811511254128,16.6083113896256));
#56310=CARTESIAN_POINT('Ctrl Pts',(57.1815817910237,27.8839125755237,16.6125379663704));
#56311=CARTESIAN_POINT('Ctrl Pts',(57.2185808708324,27.9562335398365,16.6167598521044));
#56312=CARTESIAN_POINT('Ctrl Pts',(57.2520207078107,28.0304761544739,16.6209817378384));
#56313=CARTESIAN_POINT('Ctrl Pts',(57.2817033686652,28.1062550769813,16.6252036235725));
#56314=CARTESIAN_POINT('Ctrl Pts',(57.3113660094856,28.1819828889555,16.6294226617755));
#56315=CARTESIAN_POINT('Ctrl Pts',(57.3372763381311,28.2592445193989,16.6336416999785));
#56316=CARTESIAN_POINT('Ctrl Pts',(57.3592838818366,28.3376331719461,16.6378607381815));
#56317=CARTESIAN_POINT('Ctrl Pts',(57.3812842386806,28.4159962256173,16.6420783986005));
#56318=CARTESIAN_POINT('Ctrl Pts',(57.3993842162074,28.4954851235652,16.6462960590195));
#56319=CARTESIAN_POINT('Ctrl Pts',(57.4134831321724,28.5756776924088,16.6505137194384));
#56320=CARTESIAN_POINT('Ctrl Pts',(57.4275817547442,28.6558685924754,16.6547312920895));
#56321=CARTESIAN_POINT('Ctrl Pts',(57.4376794020145,28.7367626765894,16.6589488647405));
#56322=CARTESIAN_POINT('Ctrl Pts',(57.4437267274599,28.8179287735577,16.6631664373916));
#56323=CARTESIAN_POINT('Ctrl Pts',(57.4497843185781,28.8992326545108,16.6673911696079));
#56324=CARTESIAN_POINT('Ctrl Pts',(57.4517777966085,28.9808090064826,16.6716159018241));
#56325=CARTESIAN_POINT('Ctrl Pts',(57.4497099072213,29.0622223469638,16.6758406340404));
#56326=CARTESIAN_POINT('Ctrl Pts',(57.4476425343112,29.1436153536094,16.6800643110855));
#56327=CARTESIAN_POINT('Ctrl Pts',(57.4415158787183,29.2248449669468,16.6842879881306));
#56328=CARTESIAN_POINT('Ctrl Pts',(57.4313847217911,29.3054809071624,16.6885116651758));
#56329=CARTESIAN_POINT('Ctrl Pts',(57.4212351833929,29.3862631492473,16.692743005452));
#56330=CARTESIAN_POINT('Ctrl Pts',(57.4070667047341,29.4664491068097,16.6969743457282));
#56331=CARTESIAN_POINT('Ctrl Pts',(57.3889854108488,29.5456179586045,16.7012056860045));
#56332=CARTESIAN_POINT('Ctrl Pts',(57.3709560829302,29.6245592776825,16.705424865332));
#56333=CARTESIAN_POINT('Ctrl Pts',(57.349036604091,29.7024889138234,16.7096440446595));
#56334=CARTESIAN_POINT('Ctrl Pts',(57.3233804978824,29.7790079024373,16.713863223987));
#56335=CARTESIAN_POINT('Ctrl Pts',(57.2976426966906,29.8557705452298,16.7180958381585));
#56336=CARTESIAN_POINT('Ctrl Pts',(57.268048681599,29.9313990355144,16.72232845233));
#56337=CARTESIAN_POINT('Ctrl Pts',(57.234717671421,30.0054785820886,16.7265610665014));
#56338=CARTESIAN_POINT('Ctrl Pts',(57.2014342047993,30.0794524611453,16.7307876432462));
#56339=CARTESIAN_POINT('Ctrl Pts',(57.1644245191242,30.1518813645678,16.735014219991));
#56340=CARTESIAN_POINT('Ctrl Pts',(57.1238571736111,30.2223669482199,16.7392407967358));
#56341=CARTESIAN_POINT('Ctrl Pts',(57.083334853154,30.2927743010362,16.7434626824698));
#56342=CARTESIAN_POINT('Ctrl Pts',(57.0392629492597,30.3612422191618,16.7476845682039));
#56343=CARTESIAN_POINT('Ctrl Pts',(56.9918569418559,30.4273948904141,16.7519064539379));
#56344=CARTESIAN_POINT('Ctrl Pts',(56.944482908334,30.4935029437412,16.7561254921409));
#56345=CARTESIAN_POINT('Ctrl Pts',(56.8937795074125,30.5572984749663,16.7603445303439));
#56346=CARTESIAN_POINT('Ctrl Pts',(56.8400060526505,30.6184338034685,16.764563568547));
#56347=CARTESIAN_POINT('Ctrl Pts',(56.7862501583383,30.6795491674013,16.7687812289659));
#56348=CARTESIAN_POINT('Ctrl Pts',(56.7294265077996,30.7380057052982,16.7729988893849));
#56349=CARTESIAN_POINT('Ctrl Pts',(56.6698344192217,30.7934891308236,16.7772165498039));
#56350=CARTESIAN_POINT('Ctrl Pts',(56.6102435707326,30.84897140176,16.7814341224549));
#56351=CARTESIAN_POINT('Ctrl Pts',(56.5478847395449,30.9014803676415,16.785651695106));
#56352=CARTESIAN_POINT('Ctrl Pts',(56.4830927386459,30.9507399054143,16.789869267757));
#56353=CARTESIAN_POINT('Ctrl Pts',(56.4181907497049,31.000083064005,16.7940939999733));
#56354=CARTESIAN_POINT('Ctrl Pts',(56.3508476987579,31.0461654754529,16.7983187321896));
#56355=CARTESIAN_POINT('Ctrl Pts',(56.281430374265,31.0887523658661,16.8025434644059));
#56356=CARTESIAN_POINT('Ctrl Pts',(56.2120303874769,31.1313286197568,16.806767141451));
#56357=CARTESIAN_POINT('Ctrl Pts',(56.1405575823523,31.1704108934794,16.8109908184961));
#56358=CARTESIAN_POINT('Ctrl Pts',(56.067402711464,31.2058108943332,16.8152144955412));
#56359=CARTESIAN_POINT('Ctrl Pts',(55.9941151119893,31.2412751232012,16.8194458358175));
#56360=CARTESIAN_POINT('Ctrl Pts',(55.9191397766967,31.2730435458163,16.8236771760937));
#56361=CARTESIAN_POINT('Ctrl Pts',(55.8428874756168,31.3009760871092,16.8279085163699));
#56362=CARTESIAN_POINT('Ctrl Pts',(55.7668543250338,31.3288283497716,16.8321276956975));
#56363=CARTESIAN_POINT('Ctrl Pts',(55.6895519983229,31.3528666946968,16.836346875025));
#56364=CARTESIAN_POINT('Ctrl Pts',(55.6113987353919,31.3730027046679,16.8405660543525));
#56365=CARTESIAN_POINT('Ctrl Pts',(55.5329966143747,31.3932028323575,16.844798668524));
#56366=CARTESIAN_POINT('Ctrl Pts',(55.4534465231365,31.4095508370058,16.8490312826954));
#56367=CARTESIAN_POINT('Ctrl Pts',(55.3731613018205,31.4219209096962,16.8532638968669));
#56368=CARTESIAN_POINT('Ctrl Pts',(55.2929905998342,31.4342733376394,16.8574904736117));
#56369=CARTESIAN_POINT('Ctrl Pts',(55.2120873057286,31.4426590330567,16.8617170503565));
#56370=CARTESIAN_POINT('Ctrl Pts',(55.1308773243872,31.4470025288016,16.8659436271013));
#56371=CARTESIAN_POINT('Ctrl Pts',(55.0497574767212,31.4513412037691,16.8701655128353));
#56372=CARTESIAN_POINT('Ctrl Pts',(54.9683320797156,31.4516465687934,16.8743873985693));
#56373=CARTESIAN_POINT('Ctrl Pts',(54.8870336815561,31.4478947814188,16.8786092843034));
#56374=CARTESIAN_POINT('Ctrl Pts',(54.8057901166451,31.4441455245083,16.8828283225064));
#56375=CARTESIAN_POINT('Ctrl Pts',(54.7246738433155,31.436344571335,16.8870473607094));
#56376=CARTESIAN_POINT('Ctrl Pts',(54.6441176753538,31.4245201630435,16.8912663989124));
#56377=CARTESIAN_POINT('Ctrl Pts',(54.5635878140997,31.4126996161726,16.8954840593314));
#56378=CARTESIAN_POINT('Ctrl Pts',(54.4836181542365,31.3968582909499,16.8997017197504));
#56379=CARTESIAN_POINT('Ctrl Pts',(54.4046352761339,31.3770761652871,16.9039193801693));
#56380=CARTESIAN_POINT('Ctrl Pts',(54.325654041635,31.3572944512828,16.9081369528204));
#56381=CARTESIAN_POINT('Ctrl Pts',(54.247659998412,31.3335722138928,16.9123545254714));
#56382=CARTESIAN_POINT('Ctrl Pts',(54.1710670379086,31.3060399810841,16.9165720981225));
#56383=CARTESIAN_POINT('Ctrl Pts',(54.0943440565751,31.2784610107718,16.9207968303388));
#56384=CARTESIAN_POINT('Ctrl Pts',(54.0190273560809,31.2470592626936,16.925021562555));
#56385=CARTESIAN_POINT('Ctrl Pts',(53.9455135506227,31.212014597167,16.9292462947713));
#56386=CARTESIAN_POINT('Ctrl Pts',(53.8720181060084,31.176978684413,16.9334699718164));
#56387=CARTESIAN_POINT('Ctrl Pts',(53.8003250561296,31.1383019137261,16.9376936488615));
#56388=CARTESIAN_POINT('Ctrl Pts',(53.7308050716692,31.0962095515238,16.9419173259067));
#56389=CARTESIAN_POINT('Ctrl Pts',(53.6611589535809,31.0540408190173,16.9461486661829));
#56390=CARTESIAN_POINT('Ctrl Pts',(53.593694166273,31.0084443712258,16.9503800064591));
#56391=CARTESIAN_POINT('Ctrl Pts',(53.5287518317834,30.9596885154328,16.9546113467354));
#56392=CARTESIAN_POINT('Ctrl Pts',(53.4639961427416,30.9110727848542,16.9588305260629));
#56393=CARTESIAN_POINT('Ctrl Pts',(53.4017487236058,30.8593161374303,16.9630497053904));
#56394=CARTESIAN_POINT('Ctrl Pts',(53.3423114311109,30.8047212689428,16.9672688847179));
#56395=CARTESIAN_POINT('Ctrl Pts',(53.2835680460246,30.7507637744359,16.9714388067581));
#56396=CARTESIAN_POINT('Ctrl Pts',(53.2273369812938,30.6938201153398,16.9756087287983));
#56397=CARTESIAN_POINT('Ctrl Pts',(53.1739438484535,30.634157024707,16.9797786508385));
#56398=CARTESIAN_POINT('Ctrl Pts',(53.1206398580088,30.5745935444649,16.9839416109939));
#56399=CARTESIAN_POINT('Ctrl Pts',(53.0701647033382,30.512320006737,16.9881045711492));
#56400=CARTESIAN_POINT('Ctrl Pts',(53.0228091583226,30.447641746285,16.9922675313046));
#56401=CARTESIAN_POINT('Ctrl Pts',(52.9754979972637,30.3830241054945,16.9964265897281));
#56402=CARTESIAN_POINT('Ctrl Pts',(52.931300928673,30.3160065967259,17.0005856481515));
#56403=CARTESIAN_POINT('Ctrl Pts',(52.8904694793152,30.2469287198149,17.004744706575));
#56404=CARTESIAN_POINT('Ctrl Pts',(52.8496629348429,30.1778929765201,17.0089012282069));
#56405=CARTESIAN_POINT('Ctrl Pts',(52.8122181796767,30.1067997705884,17.0130577498389));
#56406=CARTESIAN_POINT('Ctrl Pts',(52.7783433561058,30.0340174111884,17.0172142714708));
#56407=CARTESIAN_POINT('Ctrl Pts',(52.7444781103174,29.9612556303046,17.021369617886));
#56408=CARTESIAN_POINT('Ctrl Pts',(52.7141809930965,29.8868060793133,17.0255249643012));
#56409=CARTESIAN_POINT('Ctrl Pts',(52.687613375193,29.8110600146806,17.0296803107164));
#56410=CARTESIAN_POINT('Ctrl Pts',(52.6610324672833,29.7352760593467,17.033837735774));
#56411=CARTESIAN_POINT('Ctrl Pts',(52.6381849466468,29.6581947472086,17.0379951608317));
#56412=CARTESIAN_POINT('Ctrl Pts',(52.6191829795114,29.5802245814782,17.0421525858894));
#56413=CARTESIAN_POINT('Ctrl Pts',(52.6001756703733,29.5022324960787,17.0463111797196));
#56414=CARTESIAN_POINT('Ctrl Pts',(52.5850161616061,29.4233515301268,17.0504697735497));
#56415=CARTESIAN_POINT('Ctrl Pts',(52.5737654496017,29.3440002274034,17.0546283673798));
#56416=CARTESIAN_POINT('Ctrl Pts',(52.5625012777943,29.2645539926524,17.0587919363488));
#56417=CARTESIAN_POINT('Ctrl Pts',(52.5551552817256,29.1846367754754,17.0629555053177));
#56418=CARTESIAN_POINT('Ctrl Pts',(52.5517364939461,29.104671175233,17.0671190742866));
#56419=CARTESIAN_POINT('Ctrl Pts',(52.5502164841563,29.0691180777464,17.0689702174406));
#56420=CARTESIAN_POINT('Ctrl Pts',(52.5494720885549,29.033555406209,17.0708213605946));
#56421=CARTESIAN_POINT('Ctrl Pts',(52.5495007998519,28.9980200824703,17.0726725037486));
#56422=CARTESIAN_POINT('',(52.5495006756093,29.0018196594696,17.8726725038366));
#56423=CARTESIAN_POINT('Ctrl Pts',(52.5495007998525,28.9980200817158,17.0726725037879));
#56424=CARTESIAN_POINT('Ctrl Pts',(52.5496038336256,28.8704975568272,17.0793155401837));
#56425=CARTESIAN_POINT('Ctrl Pts',(52.559664163214,28.7433683178552,17.0859585765795));
#56426=CARTESIAN_POINT('Ctrl Pts',(52.5794817419324,28.617846088125,17.0926016129752));
#56427=CARTESIAN_POINT('Ctrl Pts',(52.580844176456,28.6092165869286,17.0930583136779));
#56428=CARTESIAN_POINT('Ctrl Pts',(52.5822527123098,28.6005946686822,17.0935150143807));
#56429=CARTESIAN_POINT('Ctrl Pts',(52.5837072777295,28.5919807231239,17.0939717150834));
#56430=CARTESIAN_POINT('Ctrl Pts',(52.5971879099513,28.5121483343735,17.0982043292549));
#56431=CARTESIAN_POINT('Ctrl Pts',(52.6146542582931,28.4328362864386,17.1024369434264));
#56432=CARTESIAN_POINT('Ctrl Pts',(52.6360530944036,28.3544728684856,17.1066695575979));
#56433=CARTESIAN_POINT('Ctrl Pts',(52.6574214070836,28.2762212285905,17.1108961343427));
#56434=CARTESIAN_POINT('Ctrl Pts',(52.6827109453337,28.1989159756004,17.1151227110875));
#56435=CARTESIAN_POINT('Ctrl Pts',(52.7118171822583,28.1229768289311,17.1193492878323));
#56436=CARTESIAN_POINT('Ctrl Pts',(52.7408911146304,28.0471219659212,17.1235711735663));
#56437=CARTESIAN_POINT('Ctrl Pts',(52.773773163146,27.9726306280977,17.1277930593003));
#56438=CARTESIAN_POINT('Ctrl Pts',(52.8103089458219,27.8999075778588,17.1320149450344));
#56439=CARTESIAN_POINT('Ctrl Pts',(52.8468200862455,27.8272335770619,17.1362339832374));
#56440=CARTESIAN_POINT('Ctrl Pts',(52.8869798584444,27.7563259091673,17.1404530214404));
#56441=CARTESIAN_POINT('Ctrl Pts',(52.9305862035729,27.687568367816,17.1446720596435));
#56442=CARTESIAN_POINT('Ctrl Pts',(52.9741783084588,27.618833280171,17.1488897200624));
#56443=CARTESIAN_POINT('Ctrl Pts',(53.0212145024397,27.5522473166407,17.1531073804814));
#56444=CARTESIAN_POINT('Ctrl Pts',(53.0714480133359,27.4881675077133,17.1573250409004));
#56445=CARTESIAN_POINT('Ctrl Pts',(53.1216804788918,27.4240890322624,17.1615426135514));
#56446=CARTESIAN_POINT('Ctrl Pts',(53.175109841548,27.3625169725988,17.1657601862025));
#56447=CARTESIAN_POINT('Ctrl Pts',(53.2314483286741,27.3037761834445,17.1699777588535));
#56448=CARTESIAN_POINT('Ctrl Pts',(53.2878824535298,27.2449356785186,17.1742024910698));
#56449=CARTESIAN_POINT('Ctrl Pts',(53.3472352601923,27.1889363973004,17.178427223286));
#56450=CARTESIAN_POINT('Ctrl Pts',(53.4091809563462,27.1360673240837,17.1826519555023));
#56451=CARTESIAN_POINT('Ctrl Pts',(53.4711111809132,27.0832114554722,17.1868756325474));
#56452=CARTESIAN_POINT('Ctrl Pts',(53.5356326177369,27.0334844991816,17.1910993095925));
#56453=CARTESIAN_POINT('Ctrl Pts',(53.6023885701024,26.9871332530394,17.1953229866376));
#56454=CARTESIAN_POINT('Ctrl Pts',(53.6692656411725,26.9406979094844,17.1995543269139));
#56455=CARTESIAN_POINT('Ctrl Pts',(53.7383849344819,26.8976507624229,17.2037856671901));
#56456=CARTESIAN_POINT('Ctrl Pts',(53.809362477328,26.8581940938532,17.2080170074664));
#56457=CARTESIAN_POINT('Ctrl Pts',(53.8801360294271,26.8188508244653,17.2122361867938));
#56458=CARTESIAN_POINT('Ctrl Pts',(53.9527567188956,26.7830775494876,17.2164553661213));
#56459=CARTESIAN_POINT('Ctrl Pts',(54.0268251565367,26.7510266844513,17.2206745454487));
#56460=CARTESIAN_POINT('Ctrl Pts',(54.1011294452352,26.7188737620387,17.2249071596202));
#56461=CARTESIAN_POINT('Ctrl Pts',(54.1771670859999,26.6903474328163,17.2291397737917));
#56462=CARTESIAN_POINT('Ctrl Pts',(54.2545498415163,26.6656362084678,17.2333723879632));
#56463=CARTESIAN_POINT('Ctrl Pts',(54.3318222177978,26.6409602323606,17.237598964708));
#56464=CARTESIAN_POINT('Ctrl Pts',(54.4104354592304,26.6200886929779,17.2418255414527));
#56465=CARTESIAN_POINT('Ctrl Pts',(54.4899805900535,26.6031624061114,17.2460521181975));
#56466=CARTESIAN_POINT('Ctrl Pts',(54.5694374349925,26.5862549054633,17.2502740039316));
#56467=CARTESIAN_POINT('Ctrl Pts',(54.6498236621059,26.5732840529162,17.2544958896656));
#56468=CARTESIAN_POINT('Ctrl Pts',(54.7307157008067,26.5643407019437,17.2587177753996));
#56469=CARTESIAN_POINT('Ctrl Pts',(54.8115531803359,26.5554033829842,17.2629368136026));
#56470=CARTESIAN_POINT('Ctrl Pts',(54.8928953333469,26.5504882214594,17.2671558518057));
#56471=CARTESIAN_POINT('Ctrl Pts',(54.974310223053,26.5496346628798,17.2713748900087));
#56472=CARTESIAN_POINT('Ctrl Pts',(55.0556985256243,26.5487813830412,17.2755925504277));
#56473=CARTESIAN_POINT('Ctrl Pts',(55.1371590535514,26.5519870769218,17.2798102108466));
#56474=CARTESIAN_POINT('Ctrl Pts',(55.2182579776805,26.5592391134774,17.2840278712656));
#56475=CARTESIAN_POINT('Ctrl Pts',(55.2993552141717,26.5664909991208,17.2882454439166));
#56476=CARTESIAN_POINT('Ctrl Pts',(55.3800903992291,26.5777890174768,17.2924630165677));
#56477=CARTESIAN_POINT('Ctrl Pts',(55.4600343728646,26.5930686287758,17.2966805892187));
#56478=CARTESIAN_POINT('Ctrl Pts',(55.5401140558626,26.6083741780688,17.300905321435));
#56479=CARTESIAN_POINT('Ctrl Pts',(55.6193993814666,26.6276747557694,17.3051300536513));
#56480=CARTESIAN_POINT('Ctrl Pts',(55.6974705807617,26.6508544023471,17.3093547858676));
#56481=CARTESIAN_POINT('Ctrl Pts',(55.7755222809558,26.6740282595649,17.3135784629127));
#56482=CARTESIAN_POINT('Ctrl Pts',(55.8523600286027,26.7010790733834,17.3178021399578));
#56483=CARTESIAN_POINT('Ctrl Pts',(55.9275826174791,26.731841994536,17.322025817003));
#56484=CARTESIAN_POINT('Ctrl Pts',(56.0029416865075,26.7626607304141,17.3262571572792));
#56485=CARTESIAN_POINT('Ctrl Pts',(56.0766793184366,26.7972048357748,17.3304884975554));
#56486=CARTESIAN_POINT('Ctrl Pts',(56.1484167989744,26.8352623471115,17.3347198378317));
#56487=CARTESIAN_POINT('Ctrl Pts',(56.219948104692,26.8732104804703,17.3389390171592));
#56488=CARTESIAN_POINT('Ctrl Pts',(56.2894903921097,26.9146515470883,17.3431581964868));
#56489=CARTESIAN_POINT('Ctrl Pts',(56.3566983834342,26.95933350437,17.3473773758143));
#56490=CARTESIAN_POINT('Ctrl Pts',(56.4241203805653,27.0041577393498,17.3516099899858));
#56491=CARTESIAN_POINT('Ctrl Pts',(56.4894439381013,27.0524102740276,17.3558426041573));
#56492=CARTESIAN_POINT('Ctrl Pts',(56.5522995709792,27.1038680710621,17.3600752183287));
#56493=CARTESIAN_POINT('Ctrl Pts',(56.6150655461986,27.1552524683808,17.3643017950735));
#56494=CARTESIAN_POINT('Ctrl Pts',(56.6753702319868,27.209832755635,17.3685283718183));
#56495=CARTESIAN_POINT('Ctrl Pts',(56.7328728617713,27.2673425338699,17.3727549485631));
#56496=CARTESIAN_POINT('Ctrl Pts',(56.7903116702955,27.3247884829104,17.3769768342971));
#56497=CARTESIAN_POINT('Ctrl Pts',(56.8449542754861,27.3851571355647,17.3811987200312));
#56498=CARTESIAN_POINT('Ctrl Pts',(56.8964938749885,27.4481426508434,17.3854206057652));
#56499=CARTESIAN_POINT('Ctrl Pts',(56.9479987126293,27.5110856843453,17.3896396439682));
#56500=CARTESIAN_POINT('Ctrl Pts',(56.9964044077957,27.5766417164459,17.3938586821712));
#56501=CARTESIAN_POINT('Ctrl Pts',(57.0414427258633,27.6444699018392,17.3980777203743));
#56502=CARTESIAN_POINT('Ctrl Pts',(57.0864663360583,27.7122759370201,17.4022953807932));
#56503=CARTESIAN_POINT('Ctrl Pts',(57.1281244962423,27.7823522652168,17.4065130412122));
#56504=CARTESIAN_POINT('Ctrl Pts',(57.1661916247125,27.8543281032401,17.4107307016311));
#56505=CARTESIAN_POINT('Ctrl Pts',(57.2042579610201,27.9263024434734,17.4149482742822));
#56506=CARTESIAN_POINT('Ctrl Pts',(57.2387331980426,28.0001758037414,17.4191658469332));
#56507=CARTESIAN_POINT('Ctrl Pts',(57.2694378383232,28.075553058317,17.4233834195843));
#56508=CARTESIAN_POINT('Ctrl Pts',(57.3001946014463,28.151058269994,17.4276081518006));
#56509=CARTESIAN_POINT('Ctrl Pts',(57.3271677851512,28.2280720513354,17.4318328840168));
#56510=CARTESIAN_POINT('Ctrl Pts',(57.3502261366816,28.3061791611239,17.4360576162331));
#56511=CARTESIAN_POINT('Ctrl Pts',(57.3732787291469,28.3842667628427,17.4402812932782));
#56512=CARTESIAN_POINT('Ctrl Pts',(57.3924183558645,28.4634466888392,17.4445049703233));
#56513=CARTESIAN_POINT('Ctrl Pts',(57.4075648795666,28.5432926531385,17.4487286473685));
#56514=CARTESIAN_POINT('Ctrl Pts',(57.4227388843736,28.6232834860138,17.4529599876447));
#56515=CARTESIAN_POINT('Ctrl Pts',(57.433905243613,28.7039423106955,17.4571913279209));
#56516=CARTESIAN_POINT('Ctrl Pts',(57.4410355852555,28.7848360589776,17.4614226681972));
#56517=CARTESIAN_POINT('Ctrl Pts',(57.4481454341668,28.8654973171592,17.4656418475247));
#56518=CARTESIAN_POINT('Ctrl Pts',(57.4512424993765,28.9463916922957,17.4698610268522));
#56519=CARTESIAN_POINT('Ctrl Pts',(57.4503502310631,29.0270923444712,17.4740802061797));
#56520=CARTESIAN_POINT('Ctrl Pts',(57.4494551215608,29.1080499662103,17.4783128203512));
#56521=CARTESIAN_POINT('Ctrl Pts',(57.4445418755774,29.1891137329985,17.4825454345226));
#56522=CARTESIAN_POINT('Ctrl Pts',(57.4355964344949,29.2698522897355,17.4867780486941));
#56523=CARTESIAN_POINT('Ctrl Pts',(57.4266637532443,29.3504756805022,17.4910046254389));
#56524=CARTESIAN_POINT('Ctrl Pts',(57.4137103509408,29.4307743246597,17.4952312021837));
#56525=CARTESIAN_POINT('Ctrl Pts',(57.3967741761517,29.5103173508045,17.4994577789285));
#56526=CARTESIAN_POINT('Ctrl Pts',(57.3798567985556,29.5897720934011,17.5036796646625));
#56527=CARTESIAN_POINT('Ctrl Pts',(57.3589655280866,29.6684724323045,17.5079015503966));
#56528=CARTESIAN_POINT('Ctrl Pts',(57.3341898884331,29.7459945138784,17.5121234361306));
#56529=CARTESIAN_POINT('Ctrl Pts',(57.3094309591802,29.8234643092124,17.5163424743336));
#56530=CARTESIAN_POINT('Ctrl Pts',(57.2807930051219,29.8997569841993,17.5205615125366));
#56531=CARTESIAN_POINT('Ctrl Pts',(57.2484159087534,29.9744619804101,17.5247805507397));
#56532=CARTESIAN_POINT('Ctrl Pts',(57.2160493855642,30.0491425806927,17.5289982111586));
#56533=CARTESIAN_POINT('Ctrl Pts',(57.1799463296203,30.1222361059529,17.5332158715776));
#56534=CARTESIAN_POINT('Ctrl Pts',(57.1402949563538,30.1933514779002,17.5374335319966));
#56535=CARTESIAN_POINT('Ctrl Pts',(57.1006444082174,30.2644653699635,17.5416511046476));
#56536=CARTESIAN_POINT('Ctrl Pts',(57.0574459168223,30.3336007853902,17.5458686772987));
#56537=CARTESIAN_POINT('Ctrl Pts',(57.0109332050363,30.4003920504211,17.5500862499497));
#56538=CARTESIAN_POINT('Ctrl Pts',(56.9643415353231,30.4672966973563,17.554310982166));
#56539=CARTESIAN_POINT('Ctrl Pts',(56.9144246556321,30.5318488489673,17.5585357143823));
#56540=CARTESIAN_POINT('Ctrl Pts',(56.8614594266659,30.5937123494774,17.5627604465986));
#56541=CARTESIAN_POINT('Ctrl Pts',(56.8085074263209,30.6555603989295,17.5669841236437));
#56542=CARTESIAN_POINT('Ctrl Pts',(56.7525089351073,30.7147208162159,17.5712078006888));
#56543=CARTESIAN_POINT('Ctrl Pts',(56.6937779056618,30.7708943097463,17.5754314777339));
#56544=CARTESIAN_POINT('Ctrl Pts',(56.6349403175358,30.8271697216904,17.5796628180102));
#56545=CARTESIAN_POINT('Ctrl Pts',(56.5733606355525,30.8804470747078,17.5838941582864));
#56546=CARTESIAN_POINT('Ctrl Pts',(56.5093866824929,30.9304668069441,17.5881254985627));
#56547=CARTESIAN_POINT('Ctrl Pts',(56.4455965917354,30.9803427815623,17.5923446778902));
#56548=CARTESIAN_POINT('Ctrl Pts',(56.3794263939126,31.0269796410378,17.5965638572177));
#56549=CARTESIAN_POINT('Ctrl Pts',(56.3112468994102,31.0701646839774,17.6007830365452));
#56550=CARTESIAN_POINT('Ctrl Pts',(56.2428503056097,31.1134872380936,17.6050156507167));
#56551=CARTESIAN_POINT('Ctrl Pts',(56.1721771979242,31.1534970634126,17.6092482648881));
#56552=CARTESIAN_POINT('Ctrl Pts',(56.099581754371,31.1899475371466,17.6134808790596));
#56553=CARTESIAN_POINT('Ctrl Pts',(56.0270898614016,31.2263460177023,17.6177074558044));
#56554=CARTESIAN_POINT('Ctrl Pts',(55.9526814902978,31.2591950236907,17.6219340325492));
#56555=CARTESIAN_POINT('Ctrl Pts',(55.8767387260929,31.2882918205878,17.626160609294));
#56556=CARTESIAN_POINT('Ctrl Pts',(55.8008802495623,31.3173563234097,17.630382495028));
#56557=CARTESIAN_POINT('Ctrl Pts',(55.7234911953972,31.34267672666,17.634604380762));
#56558=CARTESIAN_POINT('Ctrl Pts',(55.6449758394887,31.3640973788057,17.6388262664961));
#56559=CARTESIAN_POINT('Ctrl Pts',(55.5665134397529,31.3855035833857,17.6430453046991));
#56560=CARTESIAN_POINT('Ctrl Pts',(55.4869266940282,31.4030151388351,17.6472643429021));
#56561=CARTESIAN_POINT('Ctrl Pts',(55.4066361412256,31.4165258737802,17.6514833811051));
#56562=CARTESIAN_POINT('Ctrl Pts',(55.3263718083903,31.4300321966118,17.6557010415241));
#56563=CARTESIAN_POINT('Ctrl Pts',(55.2454045826773,31.4395402165839,17.659918701943));
#56564=CARTESIAN_POINT('Ctrl Pts',(55.1641649750556,31.4449949102125,17.664136362362));
#56565=CARTESIAN_POINT('Ctrl Pts',(55.0829270579994,31.450449490331,17.668353935013));
#56566=CARTESIAN_POINT('Ctrl Pts',(55.0014172338872,31.4518508818626,17.6725715076641));
#56567=CARTESIAN_POINT('Ctrl Pts',(54.9200694780109,31.4491960643555,17.6767890803151));
#56568=CARTESIAN_POINT('Ctrl Pts',(54.8385836297736,31.4465367401474,17.6810138125314));
#56569=CARTESIAN_POINT('Ctrl Pts',(54.7572608669687,31.4398074455723,17.6852385447477));
#56570=CARTESIAN_POINT('Ctrl Pts',(54.6765338887316,31.4290574148959,17.689463276964));
#56571=CARTESIAN_POINT('Ctrl Pts',(54.5958270729041,31.4183100691525,17.6936869540091));
#56572=CARTESIAN_POINT('Ctrl Pts',(54.5157161986539,31.4035441008954,17.6979106310542));
#56573=CARTESIAN_POINT('Ctrl Pts',(54.4366232353861,31.3848599269335,17.7021343080993));
#56574=CARTESIAN_POINT('Ctrl Pts',(54.35738676975,31.3661418533287,17.7063656483756));
#56575=CARTESIAN_POINT('Ctrl Pts',(54.2791723534683,31.3434914965236,17.7105969886518));
#56576=CARTESIAN_POINT('Ctrl Pts',(54.2023870685746,31.3170593133588,17.714828328928));
#56577=CARTESIAN_POINT('Ctrl Pts',(54.1258224659828,31.290703096768,17.7190475082555));
#56578=CARTESIAN_POINT('Ctrl Pts',(54.050679182682,31.2605870094316,17.7232666875831));
#56579=CARTESIAN_POINT('Ctrl Pts',(53.9773375074395,31.2269063016458,17.7274858669106));
#56580=CARTESIAN_POINT('Ctrl Pts',(53.9037622953201,31.1931183466874,17.7317184810821));
#56581=CARTESIAN_POINT('Ctrl Pts',(53.831726547693,31.1556173422235,17.7359510952536));
#56582=CARTESIAN_POINT('Ctrl Pts',(53.7616299527723,31.1145661200656,17.740183709425));
#56583=CARTESIAN_POINT('Ctrl Pts',(53.6916333440625,31.0735734536215,17.7444102861698));
#56584=CARTESIAN_POINT('Ctrl Pts',(53.6235707919222,31.0290408601542,17.7486368629146));
#56585=CARTESIAN_POINT('Ctrl Pts',(53.5578203625849,30.9811784733903,17.7528634396594));
#56586=CARTESIAN_POINT('Ctrl Pts',(53.4921429086105,30.9333692083335,17.7570853253934));
#56587=CARTESIAN_POINT('Ctrl Pts',(53.4287728521125,30.882237765319,17.7613072111275));
#56588=CARTESIAN_POINT('Ctrl Pts',(53.3680608456444,30.8280385243427,17.7655290968615));
#56589=CARTESIAN_POINT('Ctrl Pts',(53.3073897875418,30.7738758390736,17.7697481350645));
#56590=CARTESIAN_POINT('Ctrl Pts',(53.249373564519,30.7166497738978,17.7739671732676));
#56591=CARTESIAN_POINT('Ctrl Pts',(53.194330177525,30.6566552876815,17.7781862114706));
#56592=CARTESIAN_POINT('Ctrl Pts',(53.1393047656944,30.5966803934772,17.7824038718896));
#56593=CARTESIAN_POINT('Ctrl Pts',(53.08725057572,30.5339392156945,17.7866215323086));
#56594=CARTESIAN_POINT('Ctrl Pts',(53.0384481332066,30.4687629229658,17.7908391927275));
#56595=CARTESIAN_POINT('Ctrl Pts',(52.9896467062535,30.4035879865311,17.7950567653786));
#56596=CARTESIAN_POINT('Ctrl Pts',(52.944097169718,30.3359784084635,17.7992743380296));
#56597=CARTESIAN_POINT('Ctrl Pts',(52.9020383137302,30.2662965738498,17.8034919106807));
#56598=CARTESIAN_POINT('Ctrl Pts',(52.8599080604843,30.1964964504286,17.807716642897));
#56599=CARTESIAN_POINT('Ctrl Pts',(52.821280584898,30.124617432033,17.8119413751133));
#56600=CARTESIAN_POINT('Ctrl Pts',(52.7863501497853,30.0510492807878,17.8161661073296));
#56601=CARTESIAN_POINT('Ctrl Pts',(52.751428438915,29.9774995039597,17.8203897843747));
#56602=CARTESIAN_POINT('Ctrl Pts',(52.7202020810638,29.9022618766242,17.8246134614198));
#56603=CARTESIAN_POINT('Ctrl Pts',(52.6928165645635,29.8257450243552,17.8288371384649));
#56604=CARTESIAN_POINT('Ctrl Pts',(52.6653813611339,29.7490893436866,17.8330684787412));
#56605=CARTESIAN_POINT('Ctrl Pts',(52.6418010605464,29.6711502456553,17.8372998190174));
#56606=CARTESIAN_POINT('Ctrl Pts',(52.6221710715952,29.5923511097663,17.8415311592937));
#56607=CARTESIAN_POINT('Ctrl Pts',(52.6025974995886,29.5137784440243,17.8457503386212));
#56608=CARTESIAN_POINT('Ctrl Pts',(52.5869515693831,29.4343511400944,17.8499695179486));
#56609=CARTESIAN_POINT('Ctrl Pts',(52.5752765296161,29.3544944882071,17.8541886972761));
#56610=CARTESIAN_POINT('Ctrl Pts',(52.5582274655429,29.2378797955064,17.8603499661134));
#56611=CARTESIAN_POINT('Ctrl Pts',(52.5495884372501,29.1200064603412,17.8665112349507));
#56612=CARTESIAN_POINT('Ctrl Pts',(52.54950067561,29.001819660402,17.872672503788));
#56613=CARTESIAN_POINT('',(52.5495000568352,29.0005277777255,18.6726725037365));
#56614=CARTESIAN_POINT('Ctrl Pts',(52.5495006756093,29.0018196594696,17.8726725038366));
#56615=CARTESIAN_POINT('Ctrl Pts',(52.5494413295004,28.9218994314936,17.8768388744494));
#56616=CARTESIAN_POINT('Ctrl Pts',(52.5532959555911,28.8418332794805,17.8810052450622));
#56617=CARTESIAN_POINT('Ctrl Pts',(52.5610808602745,28.7620426931559,17.8851716156751));
#56618=CARTESIAN_POINT('Ctrl Pts',(52.5688560852825,28.6823513176769,17.8893328058628));
#56619=CARTESIAN_POINT('Ctrl Pts',(52.5805518371758,28.6029353014929,17.8934939960506));
#56620=CARTESIAN_POINT('Ctrl Pts',(52.5961323871062,28.5242156479242,17.8976551862384));
#56621=CARTESIAN_POINT('Ctrl Pts',(52.6117024114061,28.4455491743774,17.9018135652834));
#56622=CARTESIAN_POINT('Ctrl Pts',(52.6311519359377,28.3675785991837,17.9059719443284));
#56623=CARTESIAN_POINT('Ctrl Pts',(52.6543936213352,28.2907179923565,17.9101303233734));
#56624=CARTESIAN_POINT('Ctrl Pts',(52.6776272024671,28.2138841864583,17.9142872524113));
#56625=CARTESIAN_POINT('Ctrl Pts',(52.7046501817746,28.1381600393539,17.9184441814493));
#56626=CARTESIAN_POINT('Ctrl Pts',(52.7353249134837,28.0639460472215,17.9226011104873));
#56627=CARTESIAN_POINT('Ctrl Pts',(52.7659989747984,27.9897336770311,17.9267579486758));
#56628=CARTESIAN_POINT('Ctrl Pts',(52.8003244449853,27.9170318385339,17.9309147868643));
#56629=CARTESIAN_POINT('Ctrl Pts',(52.8381155503269,27.8462210453204,17.9350716250529));
#56630=CARTESIAN_POINT('Ctrl Pts',(52.8759426076556,27.7753428873473,17.9392324177855));
#56631=CARTESIAN_POINT('Ctrl Pts',(52.9172416560433,27.706359789992,17.9433932105182));
#56632=CARTESIAN_POINT('Ctrl Pts',(52.9617813453634,27.6396269019524,17.9475540032508));
#56633=CARTESIAN_POINT('Ctrl Pts',(53.0063433731053,27.5728605447213,17.9517168827861));
#56634=CARTESIAN_POINT('Ctrl Pts',(53.0541489895768,27.508347027116,17.9558797623214));
#56635=CARTESIAN_POINT('Ctrl Pts',(53.1049255277811,27.4464096438429,17.9600426418568));
#56636=CARTESIAN_POINT('Ctrl Pts',(53.1557875461254,27.3843679916224,17.9642125294225));
#56637=CARTESIAN_POINT('Ctrl Pts',(53.2096301480244,27.3249114858323,17.9683824169883));
#56638=CARTESIAN_POINT('Ctrl Pts',(53.2661430915665,27.2683272621314,17.972552304554));
#56639=CARTESIAN_POINT('Ctrl Pts',(53.3038158933783,27.2306069433592,17.9753320455832));
#56640=CARTESIAN_POINT('Ctrl Pts',(53.3426746141094,27.1941622340057,17.9781117866124));
#56641=CARTESIAN_POINT('Ctrl Pts',(53.3826196680679,27.1590678687471,17.9808915276415));
#56642=CARTESIAN_POINT('Ctrl Pts',(53.4434426007408,27.1056309096298,17.985124141813));
#56643=CARTESIAN_POINT('Ctrl Pts',(53.507029759057,27.0551121253094,17.9893567559845));
#56644=CARTESIAN_POINT('Ctrl Pts',(53.573069651168,27.0078102425768,17.9935893701559));
#56645=CARTESIAN_POINT('Ctrl Pts',(53.6390153435737,26.9605758315384,17.9978159469007));
#56646=CARTESIAN_POINT('Ctrl Pts',(53.7074064465877,26.916549476781,18.0020425236455));
#56647=CARTESIAN_POINT('Ctrl Pts',(53.7778970725188,26.8759908934654,18.0062691003903));
#56648=CARTESIAN_POINT('Ctrl Pts',(53.8483094620179,26.8354773254807,18.0104909861243));
#56649=CARTESIAN_POINT('Ctrl Pts',(53.920816343652,26.798424111841,18.0147128718583));
#56650=CARTESIAN_POINT('Ctrl Pts',(53.9950425833535,26.7650479108654,18.0189347575923));
#56651=CARTESIAN_POINT('Ctrl Pts',(54.069218759758,26.7316942211024,18.0231537957954));
#56652=CARTESIAN_POINT('Ctrl Pts',(54.1451115684634,26.7020128084663,18.0273728339984));
#56653=CARTESIAN_POINT('Ctrl Pts',(54.222322111688,26.6761739841308,18.0315918722014));
#56654=CARTESIAN_POINT('Ctrl Pts',(54.299507440764,26.6503435978133,18.0358095326203));
#56655=CARTESIAN_POINT('Ctrl Pts',(54.3780092095653,26.6283534550563,18.0400271930393));
#56656=CARTESIAN_POINT('Ctrl Pts',(54.457410711455,26.6103248936401,18.0442448534582));
#56657=CARTESIAN_POINT('Ctrl Pts',(54.5368105610295,26.5922967073915,18.0484624261093));
#56658=CARTESIAN_POINT('Ctrl Pts',(54.6171096531889,26.5782300402885,18.0526799987603));
#56659=CARTESIAN_POINT('Ctrl Pts',(54.6978797678661,26.5681953994337,18.0568975714114));
#56660=CARTESIAN_POINT('Ctrl Pts',(54.7787869943267,26.5581437242153,18.0611223036277));
#56661=CARTESIAN_POINT('Ctrl Pts',(54.8601663796607,26.5521378272465,18.065347035844));
#56662=CARTESIAN_POINT('Ctrl Pts',(54.9415828339573,26.5501963987471,18.0695717680603));
#56663=CARTESIAN_POINT('Ctrl Pts',(55.0229789536403,26.5482554551399,18.0737954451054));
#56664=CARTESIAN_POINT('Ctrl Pts',(55.1044116583295,26.5503769165849,18.0780191221505));
#56665=CARTESIAN_POINT('Ctrl Pts',(55.1854484935347,26.5565272446279,18.0822427991956));
#56666=CARTESIAN_POINT('Ctrl Pts',(55.2666323579732,26.5626887315225,18.0864741394718));
#56667=CARTESIAN_POINT('Ctrl Pts',(55.347418455313,26.5728936349655,18.090705479748));
#56668=CARTESIAN_POINT('Ctrl Pts',(55.4273812512561,26.5870566695269,18.0949368200243));
#56669=CARTESIAN_POINT('Ctrl Pts',(55.507114232674,26.6011789992701,18.0991559993518));
#56670=CARTESIAN_POINT('Ctrl Pts',(55.5860282135153,26.6192365564029,18.1033751786794));
#56671=CARTESIAN_POINT('Ctrl Pts',(55.6637171569014,26.6410956387266,18.107594358007));
#56672=CARTESIAN_POINT('Ctrl Pts',(55.7416534798717,26.6630243254298,18.1118269721784));
#56673=CARTESIAN_POINT('Ctrl Pts',(55.8186468108733,26.6888603710492,18.1160595863499));
#56674=CARTESIAN_POINT('Ctrl Pts',(55.8942769939244,26.7185051154698,18.1202922005214));
#56675=CARTESIAN_POINT('Ctrl Pts',(55.9697992976208,26.748107574446,18.1245187772662));
#56676=CARTESIAN_POINT('Ctrl Pts',(56.0439618862847,26.7815077739578,18.128745354011));
#56677=CARTESIAN_POINT('Ctrl Pts',(56.1163586027489,26.8185569638268,18.1329719307557));
#56678=CARTESIAN_POINT('Ctrl Pts',(56.1886749672412,26.8555650333853,18.1371938164898));
#56679=CARTESIAN_POINT('Ctrl Pts',(56.2592289424201,26.8962138354806,18.1414157022238));
#56680=CARTESIAN_POINT('Ctrl Pts',(56.3276345665331,26.9403066471568,18.1456375879578));
#56681=CARTESIAN_POINT('Ctrl Pts',(56.3959940531739,26.9843697195989,18.1498566261608));
#56682=CARTESIAN_POINT('Ctrl Pts',(56.4622076771272,27.0318719371499,18.1540756643639));
#56683=CARTESIAN_POINT('Ctrl Pts',(56.5259154168102,27.0825714118276,18.1582947025669));
#56684=CARTESIAN_POINT('Ctrl Pts',(56.5896023518681,27.1332543299053,18.1625123629859));
#56685=CARTESIAN_POINT('Ctrl Pts',(56.6507846645958,27.1871321425254,18.1667300234048));
#56686=CARTESIAN_POINT('Ctrl Pts',(56.7091337183731,27.2439213620342,18.1709476838238));
#56687=CARTESIAN_POINT('Ctrl Pts',(56.7674815579286,27.3007093997806,18.1751652564748));
#56688=CARTESIAN_POINT('Ctrl Pts',(56.822995923674,27.3604083991097,18.1793828291259));
#56689=CARTESIAN_POINT('Ctrl Pts',(56.8753845491235,27.4226975423499,18.1836004017769));
#56690=CARTESIAN_POINT('Ctrl Pts',(56.9278621071921,27.4850924248915,18.1878251339932));
#56691=CARTESIAN_POINT('Ctrl Pts',(56.9772030080718,27.5500858911485,18.1920498662095));
#56692=CARTESIAN_POINT('Ctrl Pts',(57.0231547106364,27.6173231516983,18.1962745984258));
#56693=CARTESIAN_POINT('Ctrl Pts',(57.0690949362814,27.684543619037,18.2004982754709));
#56694=CARTESIAN_POINT('Ctrl Pts',(57.1116474309916,27.7540063513879,18.204721952516));
#56695=CARTESIAN_POINT('Ctrl Pts',(57.1506048990952,27.825330336653,18.2089456295611));
#56696=CARTESIAN_POINT('Ctrl Pts',(57.1896330497057,27.896783728636,18.2131769698373));
#56697=CARTESIAN_POINT('Ctrl Pts',(57.2250529357812,27.9701047027709,18.2174083101136));
#56698=CARTESIAN_POINT('Ctrl Pts',(57.2567044356771,28.0448898806968,18.2216396503898));
#56699=CARTESIAN_POINT('Ctrl Pts',(57.2882649685881,28.1194601246646,18.2258588297173));
#56700=CARTESIAN_POINT('Ctrl Pts',(57.316078668915,28.1954857112511,18.2300780090449));
#56701=CARTESIAN_POINT('Ctrl Pts',(57.3400366426309,28.2725532588947,18.2342971883724));
#56702=CARTESIAN_POINT('Ctrl Pts',(57.3640709040827,28.3498662074554,18.2385298025439));
#56703=CARTESIAN_POINT('Ctrl Pts',(57.384314208715,28.4285153199078,18.2427624167154));
#56704=CARTESIAN_POINT('Ctrl Pts',(57.4006205818658,28.5080944481689,18.2469950308868));
#56705=CARTESIAN_POINT('Ctrl Pts',(57.4169036955065,28.5875600642757,18.2512216076316));
#56706=CARTESIAN_POINT('Ctrl Pts',(57.4292609386188,28.6679526101207,18.2554481843764));
#56707=CARTESIAN_POINT('Ctrl Pts',(57.4375959743156,28.7488504111088,18.2596747611212));
#56708=CARTESIAN_POINT('Ctrl Pts',(57.445921759088,28.8296584249054,18.2638966468553));
#56709=CARTESIAN_POINT('Ctrl Pts',(57.450234159399,28.9109701198137,18.2681185325893));
#56710=CARTESIAN_POINT('Ctrl Pts',(57.4504880735377,28.9923546452433,18.2723404183233));
#56711=CARTESIAN_POINT('Ctrl Pts',(57.4507418164192,29.0736842793345,18.2765594565263));
#56712=CARTESIAN_POINT('Ctrl Pts',(57.4469425082454,29.1550861830391,18.2807784947294));
#56713=CARTESIAN_POINT('Ctrl Pts',(57.439097054718,29.2361266771583,18.2849975329324));
#56714=CARTESIAN_POINT('Ctrl Pts',(57.4312541632297,29.3171407064068,18.2892151933514));
#56715=CARTESIAN_POINT('Ctrl Pts',(57.4193677951843,29.3977930984244,18.2934328537704));
#56716=CARTESIAN_POINT('Ctrl Pts',(57.4034968371366,29.4776538536161,18.2976505141893));
#56717=CARTESIAN_POINT('Ctrl Pts',(57.3876262093575,29.5575129469358,18.3018680868404));
#56718=CARTESIAN_POINT('Ctrl Pts',(57.36777124814,29.636579980775,18.3060856594915));
#56719=CARTESIAN_POINT('Ctrl Pts',(57.34404195333,29.7144351412331,18.3103032321425));
#56720=CARTESIAN_POINT('Ctrl Pts',(57.3202723767163,29.7924224651759,18.3145279643588));
#56721=CARTESIAN_POINT('Ctrl Pts',(57.2926154438239,29.8691933530088,18.3187526965751));
#56722=CARTESIAN_POINT('Ctrl Pts',(57.2612312773784,29.9443428192165,18.3229774287914));
#56723=CARTESIAN_POINT('Ctrl Pts',(57.2298549494574,30.0194735160572,18.3272011058365));
#56724=CARTESIAN_POINT('Ctrl Pts',(57.1947534696254,30.0929831896066,18.3314247828816));
#56725=CARTESIAN_POINT('Ctrl Pts',(57.1561335885112,30.1644905317322,18.3356484599267));
#56726=CARTESIAN_POINT('Ctrl Pts',(57.1174436373911,30.2361276132495,18.339879800203));
#56727=CARTESIAN_POINT('Ctrl Pts',(57.0752227691256,30.3057547046768,18.3441111404792));
#56728=CARTESIAN_POINT('Ctrl Pts',(57.0297221773078,30.3730178924344,18.3483424807555));
#56729=CARTESIAN_POINT('Ctrl Pts',(56.984352355017,30.440087764569,18.352561660083));
#56730=CARTESIAN_POINT('Ctrl Pts',(56.9357219759435,30.5048069887044,18.3567808394104));
#56731=CARTESIAN_POINT('Ctrl Pts',(56.8841185129737,30.566859176528,18.3610000187379));
#56732=CARTESIAN_POINT('Ctrl Pts',(56.832350732628,30.6291089528869,18.3652326329094));
#56733=CARTESIAN_POINT('Ctrl Pts',(56.777398344353,30.6889061877296,18.3694652470808));
#56734=CARTESIAN_POINT('Ctrl Pts',(56.7195225666831,30.7459073264832,18.3736978612523));
#56735=CARTESIAN_POINT('Ctrl Pts',(56.6617293433756,30.8028271584646,18.3779244379971));
#56736=CARTESIAN_POINT('Ctrl Pts',(56.6010213409389,30.8569584925041,18.3821510147419));
#56737=CARTESIAN_POINT('Ctrl Pts',(56.5376998247819,30.9079909588009,18.3863775914867));
#56738=CARTESIAN_POINT('Ctrl Pts',(56.4744485881753,30.9589667849695,18.3905994772207));
#56739=CARTESIAN_POINT('Ctrl Pts',(56.408589961409,31.006850287408,18.3948213629547));
#56740=CARTESIAN_POINT('Ctrl Pts',(56.3404607994197,31.0513690782546,18.3990432486887));
#56741=CARTESIAN_POINT('Ctrl Pts',(56.2723775884375,31.0958578425572,18.4032622868918));
#56742=CARTESIAN_POINT('Ctrl Pts',(56.2020272716181,31.1369861490226,18.4074813250948));
#56743=CARTESIAN_POINT('Ctrl Pts',(56.1297773894836,31.1745236950219,18.4117003632978));
#56744=CARTESIAN_POINT('Ctrl Pts',(56.0575511015265,31.2120489826272,18.4159180237168));
#56745=CARTESIAN_POINT('Ctrl Pts',(55.983426892104,31.24598562449,18.4201356841357));
#56746=CARTESIAN_POINT('Ctrl Pts',(55.9077975136121,31.2761489240117,18.4243533445547));
#56747=CARTESIAN_POINT('Ctrl Pts',(55.8321697089388,31.3063115958466,18.4285709172057));
#56748=CARTESIAN_POINT('Ctrl Pts',(55.7550372294031,31.3327009104592,18.4327884898568));
#56749=CARTESIAN_POINT('Ctrl Pts',(55.6768121095004,31.3551805914693,18.4370060625078));
#56750=CARTESIAN_POINT('Ctrl Pts',(55.5984541980857,31.3776984329939,18.4412307947241));
#56751=CARTESIAN_POINT('Ctrl Pts',(55.5190003840752,31.3962932332051,18.4454555269404));
#56752=CARTESIAN_POINT('Ctrl Pts',(55.4388775504767,31.4108788326433,18.4496802591567));
#56753=CARTESIAN_POINT('Ctrl Pts',(55.3587747283963,31.4254607891751,18.4539039362018));
#56754=CARTESIAN_POINT('Ctrl Pts',(55.278003685843,31.4360355079212,18.4581276132469));
#56755=CARTESIAN_POINT('Ctrl Pts',(55.1969968289068,31.4425688320702,18.462351290292));
#56756=CARTESIAN_POINT('Ctrl Pts',(55.1158429971282,31.44911400996,18.4665826305683));
#56757=CARTESIAN_POINT('Ctrl Pts',(55.0344529616031,31.4516031252468,18.4708139708445));
#56758=CARTESIAN_POINT('Ctrl Pts',(54.953260343965,31.4500542146152,18.4750453111207));
#56759=CARTESIAN_POINT('Ctrl Pts',(54.8723010753831,31.4485097555809,18.4792644904482));
#56760=CARTESIAN_POINT('Ctrl Pts',(54.7915385399024,31.4429505645957,18.4834836697758));
#56761=CARTESIAN_POINT('Ctrl Pts',(54.7113946324922,31.4334455391164,18.4877028491033));
#56762=CARTESIAN_POINT('Ctrl Pts',(54.630995528323,31.4239102474351,18.4919354632748));
#56763=CARTESIAN_POINT('Ctrl Pts',(54.5509199747245,31.4103684607044,18.4961680774462));
#56764=CARTESIAN_POINT('Ctrl Pts',(54.4715983615203,31.3928522642344,18.5004006916177));
#56765=CARTESIAN_POINT('Ctrl Pts',(54.3923898931491,31.375361052974,18.5046272683625));
#56766=CARTESIAN_POINT('Ctrl Pts',(54.31393367909,31.3539067909197,18.5088538451073));
#56767=CARTESIAN_POINT('Ctrl Pts',(54.2366540744935,31.328573221527,18.5130804218521));
#56768=CARTESIAN_POINT('Ctrl Pts',(54.1594602413094,31.3032677694628,18.5173023075861));
#56769=CARTESIAN_POINT('Ctrl Pts',(54.0834408619762,31.274091709223,18.5215241933202));
#56770=CARTESIAN_POINT('Ctrl Pts',(54.0090078064033,31.241179315055,18.5257460790542));
#56771=CARTESIAN_POINT('Ctrl Pts',(53.9346249536182,31.2082891192762,18.5299651172572));
#56772=CARTESIAN_POINT('Ctrl Pts',(53.8618267233971,31.171667781972,18.5341841554602));
#56773=CARTESIAN_POINT('Ctrl Pts',(53.7910063887513,31.1314982284674,18.5384031936632));
#56774=CARTESIAN_POINT('Ctrl Pts',(53.7202091814448,31.0913417928746,18.5426208540822));
#56775=CARTESIAN_POINT('Ctrl Pts',(53.6513889907435,31.0476396712413,18.5468385145012));
#56776=CARTESIAN_POINT('Ctrl Pts',(53.5849145595345,31.0006207652083,18.5510561749201));
#56777=CARTESIAN_POINT('Ctrl Pts',(53.5184415116332,30.9536028376208,18.5552737475712));
#56778=CARTESIAN_POINT('Ctrl Pts',(53.4543145047537,30.9032685320856,18.5594913202222));
#56779=CARTESIAN_POINT('Ctrl Pts',(53.3928721628732,30.8498892845606,18.5637088928733));
#56780=CARTESIAN_POINT('Ctrl Pts',(53.3313255191841,30.7964194227802,18.5679336250896));
#56781=CARTESIAN_POINT('Ctrl Pts',(53.2724730112602,30.7398945834016,18.5721583573059));
#56782=CARTESIAN_POINT('Ctrl Pts',(53.2166193072832,30.6806259413817,18.5763830895222));
#56783=CARTESIAN_POINT('Ctrl Pts',(53.1607795533546,30.6213721023266,18.5806067665673));
#56784=CARTESIAN_POINT('Ctrl Pts',(53.1079373918087,30.5593761996001,18.5848304436124));
#56785=CARTESIAN_POINT('Ctrl Pts',(53.0583568764645,30.4949823513431,18.5890541206575));
#56786=CARTESIAN_POINT('Ctrl Pts',(53.0086864046808,30.4304716700666,18.5932854609337));
#56787=CARTESIAN_POINT('Ctrl Pts',(52.9622896710225,30.3635547313774,18.59751680121));
#56788=CARTESIAN_POINT('Ctrl Pts',(52.9193876098304,30.2946050872265,18.6017481414862));
#56789=CARTESIAN_POINT('Ctrl Pts',(52.8766088499405,30.225853605604,18.6059673208138));
#56790=CARTESIAN_POINT('Ctrl Pts',(52.8373048501513,30.1550815253587,18.6101865001413));
#56791=CARTESIAN_POINT('Ctrl Pts',(52.8016474974991,30.0826802504655,18.6144056794688));
#56792=CARTESIAN_POINT('Ctrl Pts',(52.7633087932116,30.0048345647455,18.6189421314637));
#56793=CARTESIAN_POINT('Ctrl Pts',(52.7290586323875,29.9248486151305,18.6234785834587));
#56794=CARTESIAN_POINT('Ctrl Pts',(52.6991232085006,29.8431584906405,18.6280150354536));
#56795=CARTESIAN_POINT('Ctrl Pts',(52.6692884075535,29.7617429538938,18.632536238921));
#56796=CARTESIAN_POINT('Ctrl Pts',(52.6437395674428,29.6786349946326,18.6370574423884));
#56797=CARTESIAN_POINT('Ctrl Pts',(52.6226552075422,29.5942911641392,18.6415786458558));
#56798=CARTESIAN_POINT('Ctrl Pts',(52.6016158173398,29.5101272260691,18.6460902062913));
#56799=CARTESIAN_POINT('Ctrl Pts',(52.5850220414241,29.4247330115307,18.6506017667268));
#56800=CARTESIAN_POINT('Ctrl Pts',(52.5730034217597,29.3385821306712,18.6551133271622));
#56801=CARTESIAN_POINT('Ctrl Pts',(52.5610198208791,29.2526822685771,18.6596117422147));
#56802=CARTESIAN_POINT('Ctrl Pts',(52.5535848700389,29.1660304884529,18.6641101572671));
#56803=CARTESIAN_POINT('Ctrl Pts',(52.5507773309078,29.0791111067095,18.6686085723195));
#56804=CARTESIAN_POINT('Ctrl Pts',(52.5499318741305,29.0529363761211,18.6699632161252));
#56805=CARTESIAN_POINT('Ctrl Pts',(52.5495057017596,29.026737460879,18.6713178599309));
#56806=CARTESIAN_POINT('Ctrl Pts',(52.5495000568352,29.0005277777256,18.6726725037366));
#56807=CARTESIAN_POINT('',(52.5495009896071,28.9977977140258,19.4726725037492));
#56808=CARTESIAN_POINT('Ctrl Pts',(52.549500056835,29.0005277767301,18.672672503788));
#56809=CARTESIAN_POINT('Ctrl Pts',(52.5494819283997,28.916356332626,18.6770228930965));
#56810=CARTESIAN_POINT('Ctrl Pts',(52.5538049015165,28.8322364052644,18.6813732824049));
#56811=CARTESIAN_POINT('Ctrl Pts',(52.5624270296726,28.7486272402795,18.6857236717134));
#56812=CARTESIAN_POINT('Ctrl Pts',(52.5710574791649,28.664937382924,18.6900782596432));
#56813=CARTESIAN_POINT('Ctrl Pts',(52.5839953011645,28.581759688051,18.6944328475731));
#56814=CARTESIAN_POINT('Ctrl Pts',(52.6011471071535,28.4995451583989,18.6987874355029));
#56815=CARTESIAN_POINT('Ctrl Pts',(52.6183331992217,28.4171662837284,18.7031507281573));
#56816=CARTESIAN_POINT('Ctrl Pts',(52.639750009848,28.33575483198,18.7075140208117));
#56817=CARTESIAN_POINT('Ctrl Pts',(52.665253688106,28.255748759425,18.711877313466));
#56818=CARTESIAN_POINT('Ctrl Pts',(52.6907866110946,28.1756509449646,18.7162456094504));
#56819=CARTESIAN_POINT('Ctrl Pts',(52.720415592244,28.096962114604,18.7206139054347));
#56820=CARTESIAN_POINT('Ctrl Pts',(52.753948715331,28.0201000680494,18.7249822014191));
#56821=CARTESIAN_POINT('Ctrl Pts',(52.787551620376,27.9430780726558,18.729359587766));
#56822=CARTESIAN_POINT('Ctrl Pts',(52.8250747045283,27.8678908291701,18.733736974113));
#56823=CARTESIAN_POINT('Ctrl Pts',(52.8662802307517,27.794931455759,18.7381143604599));
#56824=CARTESIAN_POINT('Ctrl Pts',(52.8756751444272,27.778296623545,18.7391124102513));
#56825=CARTESIAN_POINT('Ctrl Pts',(52.8852613138506,27.7617774819803,18.7401104600428));
#56826=CARTESIAN_POINT('Ctrl Pts',(52.8950356178758,27.7453784634447,18.7411085098342));
#56827=CARTESIAN_POINT('Ctrl Pts',(52.9364873150637,27.6758321153096,18.7453411240057));
#56828=CARTESIAN_POINT('Ctrl Pts',(52.9814664335564,27.6082129377665,18.7495737381772));
#56829=CARTESIAN_POINT('Ctrl Pts',(53.0297683907496,27.5429009450588,18.7538063523487));
#56830=CARTESIAN_POINT('Ctrl Pts',(53.0780014497362,27.4776821137761,18.7580329290935));
#56831=CARTESIAN_POINT('Ctrl Pts',(53.1295476598027,27.4147643014129,18.7622595058383));
#56832=CARTESIAN_POINT('Ctrl Pts',(53.1841577158776,27.3545009725943,18.7664860825831));
#56833=CARTESIAN_POINT('Ctrl Pts',(53.2387071611137,27.2943045290927,18.7707079683171));
#56834=CARTESIAN_POINT('Ctrl Pts',(53.2963133851737,27.2367570576029,18.7749298540511));
#56835=CARTESIAN_POINT('Ctrl Pts',(53.3566860171766,27.1821800408575,18.7791517397851));
#56836=CARTESIAN_POINT('Ctrl Pts',(53.4170179297115,27.1276398346173,18.7833707779882));
#56837=CARTESIAN_POINT('Ctrl Pts',(53.4801122007157,27.0760664147599,18.7875898161912));
#56838=CARTESIAN_POINT('Ctrl Pts',(53.5456415992744,27.0277444657857,18.7918088543942));
#56839=CARTESIAN_POINT('Ctrl Pts',(53.6111495983205,26.9794382969984,18.7960265148132));
#56840=CARTESIAN_POINT('Ctrl Pts',(53.6790907720557,26.9343817658965,18.8002441752322));
#56841=CARTESIAN_POINT('Ctrl Pts',(53.7491058887694,26.8928184291598,18.8044618356511));
#56842=CARTESIAN_POINT('Ctrl Pts',(53.819119548495,26.8512559573404,18.8086794083022));
#56843=CARTESIAN_POINT('Ctrl Pts',(53.8912066653263,26.8131867714811,18.8128969809532));
#56844=CARTESIAN_POINT('Ctrl Pts',(53.9649814264467,26.7788095978958,18.8171145536043));
#56845=CARTESIAN_POINT('Ctrl Pts',(54.0388814243465,26.7443740671375,18.8213392858206));
#56846=CARTESIAN_POINT('Ctrl Pts',(54.1144743751778,26.7136432854959,18.8255640180369));
#56847=CARTESIAN_POINT('Ctrl Pts',(54.191352000615,26.686768783046,18.8297887502531));
#56848=CARTESIAN_POINT('Ctrl Pts',(54.2682104250593,26.6599009927848,18.8340124272983));
#56849=CARTESIAN_POINT('Ctrl Pts',(54.3463524292999,26.6368876669712,18.8382361043434));
#56850=CARTESIAN_POINT('Ctrl Pts',(54.4253561879548,26.6178298257097,18.8424597813885));
#56851=CARTESIAN_POINT('Ctrl Pts',(54.5045032871294,26.5987374068419,18.8466911216648));
#56852=CARTESIAN_POINT('Ctrl Pts',(54.5845148075763,26.5836149013123,18.850922461941));
#56853=CARTESIAN_POINT('Ctrl Pts',(54.6649596022408,26.5725119605095,18.8551538022173));
#56854=CARTESIAN_POINT('Ctrl Pts',(54.7451731971052,26.5614409297601,18.8593729815447));
#56855=CARTESIAN_POINT('Ctrl Pts',(54.8258171182594,26.5543663469128,18.8635921608722));
#56856=CARTESIAN_POINT('Ctrl Pts',(54.9064638889266,26.5512857974183,18.8678113401997));
#56857=CARTESIAN_POINT('Ctrl Pts',(54.9873674575863,26.5481954387409,18.8720439543712));
#56858=CARTESIAN_POINT('Ctrl Pts',(55.0685747979384,26.5491131232658,18.8762765685427));
#56859=CARTESIAN_POINT('Ctrl Pts',(55.1496557695137,26.5540741220039,18.8805091827141));
#56860=CARTESIAN_POINT('Ctrl Pts',(55.2306210866964,26.559028044343,18.8847357594589));
#56861=CARTESIAN_POINT('Ctrl Pts',(55.3114599332799,26.568013797945,18.8889623362037));
#56862=CARTESIAN_POINT('Ctrl Pts',(55.3917400923376,26.5810146858537,18.8931889129485));
#56863=CARTESIAN_POINT('Ctrl Pts',(55.471931149715,26.5940011442824,18.8974107986825));
#56864=CARTESIAN_POINT('Ctrl Pts',(55.5515642953984,26.610993808402,18.9016326844165));
#56865=CARTESIAN_POINT('Ctrl Pts',(55.63021178342,26.6319241232514,18.9058545701506));
#56866=CARTESIAN_POINT('Ctrl Pts',(55.7088062261496,26.6528403212524,18.9100736083536));
#56867=CARTESIAN_POINT('Ctrl Pts',(55.7864158837948,26.6776887761234,18.9142926465566));
#56868=CARTESIAN_POINT('Ctrl Pts',(55.8626238110411,26.7063499807894,18.9185116847596));
#56869=CARTESIAN_POINT('Ctrl Pts',(55.9388068515567,26.7350018257508,18.9227293451786));
#56870=CARTESIAN_POINT('Ctrl Pts',(56.0135886362644,26.7674637844002,18.9269470055975));
#56871=CARTESIAN_POINT('Ctrl Pts',(56.086569297644,26.8035671165689,18.9311646660165));
#56872=CARTESIAN_POINT('Ctrl Pts',(56.1595484403236,26.8396696974409,18.9353822386675));
#56873=CARTESIAN_POINT('Ctrl Pts',(56.2307261183335,26.8794132941344,18.9395998113186));
#56874=CARTESIAN_POINT('Ctrl Pts',(56.2997255982198,26.9225824638913,18.9438173839696));
#56875=CARTESIAN_POINT('Ctrl Pts',(56.368842208579,26.9658249157261,18.9480421161859));
#56876=CARTESIAN_POINT('Ctrl Pts',(56.4357728268587,27.0125043275949,18.9522668484022));
#56877=CARTESIAN_POINT('Ctrl Pts',(56.5001680787598,27.0623607184333,18.9564915806185));
#56878=CARTESIAN_POINT('Ctrl Pts',(56.5645472472712,27.1122046571151,18.9607152576636));
#56879=CARTESIAN_POINT('Ctrl Pts',(56.6263919756417,27.1652236684644,18.9649389347087));
#56880=CARTESIAN_POINT('Ctrl Pts',(56.6853878835814,27.2211189101356,18.9691626117538));
#56881=CARTESIAN_POINT('Ctrl Pts',(56.744490830784,27.2771155653741,18.97339395203));
#56882=CARTESIAN_POINT('Ctrl Pts',(56.8007343061655,27.335998543005,18.9776252923063));
#56883=CARTESIAN_POINT('Ctrl Pts',(56.8538419440844,27.397433216258,18.9818566325825));
#56884=CARTESIAN_POINT('Ctrl Pts',(56.9067969496889,27.458691325146,18.9860758119101));
#56885=CARTESIAN_POINT('Ctrl Pts',(56.9566339039521,27.5224860720422,18.9902949912376));
#56886=CARTESIAN_POINT('Ctrl Pts',(57.0031221135569,27.5884575641593,18.9945141705652));
#56887=CARTESIAN_POINT('Ctrl Pts',(57.0497583523855,27.654639124783,18.9987467847366));
#56888=CARTESIAN_POINT('Ctrl Pts',(57.0931979170176,27.7232574787165,19.0029793989081));
#56889=CARTESIAN_POINT('Ctrl Pts',(57.1331770524215,27.7939710148498,19.0072120130796));
#56890=CARTESIAN_POINT('Ctrl Pts',(57.1730991613426,27.8645836847635,19.0114385898244));
#56891=CARTESIAN_POINT('Ctrl Pts',(57.2095704177916,27.9372852001382,19.0156651665692));
#56892=CARTESIAN_POINT('Ctrl Pts',(57.2423695283531,28.011703916676,19.0198917433139));
#56893=CARTESIAN_POINT('Ctrl Pts',(57.2751322356999,28.0860400370559,19.024113629048));
#56894=CARTESIAN_POINT('Ctrl Pts',(57.304230709071,28.1620891486405,19.028335514782));
#56895=CARTESIAN_POINT('Ctrl Pts',(57.3294895888474,28.2394551259447,19.032557400516));
#56896=CARTESIAN_POINT('Ctrl Pts',(57.3547314322926,28.3167689222964,19.036776438719));
#56897=CARTESIAN_POINT('Ctrl Pts',(57.3761386816807,28.395397379886,19.0409954769221));
#56898=CARTESIAN_POINT('Ctrl Pts',(57.3935845971956,28.4749256947176,19.0452145151251));
#56899=CARTESIAN_POINT('Ctrl Pts',(57.4110248155106,28.554428038501,19.049432175544));
#56900=CARTESIAN_POINT('Ctrl Pts',(57.4245061695532,28.6348292025262,19.053649835963));
#56901=CARTESIAN_POINT('Ctrl Pts',(57.4339525146333,28.715701905546,19.057867496382));
#56902=CARTESIAN_POINT('Ctrl Pts',(57.4433986631386,28.7965729256356,19.062085069033));
#56903=CARTESIAN_POINT('Ctrl Pts',(57.4488099169007,28.8779150036628,19.0663026416841));
#56904=CARTESIAN_POINT('Ctrl Pts',(57.4501619007443,28.9592948388912,19.0705202143351));
#56905=CARTESIAN_POINT('Ctrl Pts',(57.451516179656,29.0408128209371,19.0747449465514));
#56906=CARTESIAN_POINT('Ctrl Pts',(57.4487973939351,29.1223682214935,19.0789696787677));
#56907=CARTESIAN_POINT('Ctrl Pts',(57.4420334226068,29.2035264426833,19.083194410984));
#56908=CARTESIAN_POINT('Ctrl Pts',(57.4352711406513,29.2846643937561,19.0874180880291));
#56909=CARTESIAN_POINT('Ctrl Pts',(57.4244657763874,29.3654049046216,19.0916417650742));
#56910=CARTESIAN_POINT('Ctrl Pts',(57.40969685743,29.4453215751475,19.0958654421193));
#56911=CARTESIAN_POINT('Ctrl Pts',(57.3949011424752,29.5253832425355,19.1000967823955));
#56912=CARTESIAN_POINT('Ctrl Pts',(57.3761276087181,29.6046176290603,19.1043281226718));
#56913=CARTESIAN_POINT('Ctrl Pts',(57.3535064958576,29.6826107411665,19.108559462948));
#56914=CARTESIAN_POINT('Ctrl Pts',(57.3309503964859,29.7603796996537,19.1127786422755));
#56915=CARTESIAN_POINT('Ctrl Pts',(57.304569031496,29.8369141057922,19.116997821603));
#56916=CARTESIAN_POINT('Ctrl Pts',(57.2745386984091,29.9118245222845,19.1212170009306));
#56917=CARTESIAN_POINT('Ctrl Pts',(57.2444127417879,29.986973470889,19.125449615102));
#56918=CARTESIAN_POINT('Ctrl Pts',(57.2105024694546,30.0607675607763,19.1296822292735));
#56919=CARTESIAN_POINT('Ctrl Pts',(57.1729508449742,30.132799574208,19.133914843445));
#56920=CARTESIAN_POINT('Ctrl Pts',(57.1354527843602,30.2047288407361,19.1381414201898));
#56921=CARTESIAN_POINT('Ctrl Pts',(57.0943239006092,30.2749006143076,19.1423679969346));
#56922=CARTESIAN_POINT('Ctrl Pts',(57.0497554660202,30.3429269449677,19.1465945736794));
#56923=CARTESIAN_POINT('Ctrl Pts',(57.0052364972329,30.4108777742778,19.1508164594134));
#56924=CARTESIAN_POINT('Ctrl Pts',(56.957285816278,30.4766875054828,19.1550383451475));
#56925=CARTESIAN_POINT('Ctrl Pts',(56.9061402372876,30.5399933914771,19.1592602308815));
#56926=CARTESIAN_POINT('Ctrl Pts',(56.8550291544041,30.6032565796147,19.1634792690845));
#56927=CARTESIAN_POINT('Ctrl Pts',(56.8007277444122,30.6640189161582,19.1676983072875));
#56928=CARTESIAN_POINT('Ctrl Pts',(56.7435149581103,30.7219482689226,19.1719173454906));
#56929=CARTESIAN_POINT('Ctrl Pts',(56.6863208554184,30.7798587040725,19.1761350059096));
#56930=CARTESIAN_POINT('Ctrl Pts',(56.626217590731,30.8349376624633,19.1803526663285));
#56931=CARTESIAN_POINT('Ctrl Pts',(56.5635221251068,30.8868886597523,19.1845703267475));
#56932=CARTESIAN_POINT('Ctrl Pts',(56.5008279641517,30.9388385759604,19.1887878993986));
#56933=CARTESIAN_POINT('Ctrl Pts',(56.4355420679637,30.9876603649891,19.1930054720496));
#56934=CARTESIAN_POINT('Ctrl Pts',(56.3680146302662,31.0330976910561,19.1972230447007));
#56935=CARTESIAN_POINT('Ctrl Pts',(56.3003725609702,31.0786121495228,19.2014477769169));
#56936=CARTESIAN_POINT('Ctrl Pts',(56.2304817244137,31.1207303892901,19.2056725091332));
#56937=CARTESIAN_POINT('Ctrl Pts',(56.1587218496236,31.1592392005531,19.2098972413495));
#56938=CARTESIAN_POINT('Ctrl Pts',(56.0869798976145,31.1977383938366,19.2141209183946));
#56939=CARTESIAN_POINT('Ctrl Pts',(56.0133702712092,31.2326297809141,19.2183445954397));
#56940=CARTESIAN_POINT('Ctrl Pts',(55.9382939404934,31.2637479389794,19.2225682724848));
#56941=CARTESIAN_POINT('Ctrl Pts',(55.8630813949891,31.2949225562946,19.2267996127611));
#56942=CARTESIAN_POINT('Ctrl Pts',(55.7863972657798,31.3223101064796,19.2310309530373));
#56943=CARTESIAN_POINT('Ctrl Pts',(55.708659723701,31.3457944594538,19.2352622933136));
#56944=CARTESIAN_POINT('Ctrl Pts',(55.6311456007294,31.3692113179712,19.239481472641));
#56945=CARTESIAN_POINT('Ctrl Pts',(55.5525845737257,31.3887473558927,19.2437006519685));
#56946=CARTESIAN_POINT('Ctrl Pts',(55.4733992890323,31.4043384460478,19.247919831296));
#56947=CARTESIAN_POINT('Ctrl Pts',(55.3939618600558,31.4199791818443,19.2521524454675));
#56948=CARTESIAN_POINT('Ctrl Pts',(55.313600736226,31.431707951975,19.2563850596389));
#56949=CARTESIAN_POINT('Ctrl Pts',(55.232735331535,31.4394229882198,19.2606176738104));
#56950=CARTESIAN_POINT('Ctrl Pts',(55.1519852737505,31.4471270196898,19.2648442505552));
#56951=CARTESIAN_POINT('Ctrl Pts',(55.0707328223517,31.4508286445337,19.2690708273));
#56952=CARTESIAN_POINT('Ctrl Pts',(54.9894075283417,31.450477106513,19.2732974040448));
#56953=CARTESIAN_POINT('Ctrl Pts',(54.908172495991,31.4501259586587,19.2775192897789));
#56954=CARTESIAN_POINT('Ctrl Pts',(54.8268652438744,31.4457305885304,19.2817411755129));
#56955=CARTESIAN_POINT('Ctrl Pts',(54.7459189752196,31.4372921619795,19.2859630612469));
#56956=CARTESIAN_POINT('Ctrl Pts',(54.6650273023129,31.4288594268856,19.2901820994499));
#56957=CARTESIAN_POINT('Ctrl Pts',(54.5844965901632,31.4163890993054,19.294401137653));
#56958=CARTESIAN_POINT('Ctrl Pts',(54.5047573006657,31.3999343571765,19.298620175856));
#56959=CARTESIAN_POINT('Ctrl Pts',(54.4250440511127,31.3834849885663,19.302837836275));
#56960=CARTESIAN_POINT('Ctrl Pts',(54.3461221655603,31.3630538832531,19.3070554966939));
#56961=CARTESIAN_POINT('Ctrl Pts',(54.2684128964103,31.3387455098538,19.3112731571129));
#56962=CARTESIAN_POINT('Ctrl Pts',(54.1907052443613,31.3144376423027,19.3154907297639));
#56963=CARTESIAN_POINT('Ctrl Pts',(54.1142106015545,31.2862528068968,19.319708302415));
#56964=CARTESIAN_POINT('Ctrl Pts',(54.0393346346563,31.2543452055595,19.323925875066));
#56965=CARTESIAN_POINT('Ctrl Pts',(53.9643315616201,31.2223834392858,19.3281506072823));
#56966=CARTESIAN_POINT('Ctrl Pts',(53.890953091797,31.1866864461052,19.3323753394986));
#56967=CARTESIAN_POINT('Ctrl Pts',(53.8195847957387,31.1474566807153,19.3366000717149));
#56968=CARTESIAN_POINT('Ctrl Pts',(53.7482343246607,31.1082367133707,19.34082374876));
#56969=CARTESIAN_POINT('Ctrl Pts',(53.678893408997,31.0654860010185,19.3450474258051));
#56970=CARTESIAN_POINT('Ctrl Pts',(53.6119190980081,31.019450831173,19.3492711028502));
#56971=CARTESIAN_POINT('Ctrl Pts',(53.5448232721356,30.9733321373879,19.3535024431265));
#56972=CARTESIAN_POINT('Ctrl Pts',(53.4801030023543,30.9239173596677,19.3577337834027));
#56973=CARTESIAN_POINT('Ctrl Pts',(53.4180833540453,30.871494048949,19.3619651236789));
#56974=CARTESIAN_POINT('Ctrl Pts',(53.3562419513309,30.8192214037765,19.3661843030065));
#56975=CARTESIAN_POINT('Ctrl Pts',(53.2970859434363,30.7639578672298,19.370403482334));
#56976=CARTESIAN_POINT('Ctrl Pts',(53.2408992108594,30.7060230548398,19.3746226616615));
#56977=CARTESIAN_POINT('Ctrl Pts',(53.1852939713217,30.6486878268816,19.3787981754598));
#56978=CARTESIAN_POINT('Ctrl Pts',(53.1323780650783,30.5885105338161,19.3829736892582));
#56979=CARTESIAN_POINT('Ctrl Pts',(53.0824613640708,30.5257771232126,19.3871492030566));
#56980=CARTESIAN_POINT('Ctrl Pts',(53.0326089849624,30.4631245499245,19.3913193363516));
#56981=CARTESIAN_POINT('Ctrl Pts',(52.9857484413835,30.3979227611001,19.3954894696466));
#56982=CARTESIAN_POINT('Ctrl Pts',(52.9421529231358,30.3304945164267,19.3996596029416));
#56983=CARTESIAN_POINT('Ctrl Pts',(52.8985993948141,30.263131216663,19.4038257196864));
#56984=CARTESIAN_POINT('Ctrl Pts',(52.8583049111373,30.1935461143265,19.4079918364312));
#56985=CARTESIAN_POINT('Ctrl Pts',(52.821501474637,30.1220937683594,19.412157953176));
#56986=CARTESIAN_POINT('Ctrl Pts',(52.7847215164527,30.0506870045695,19.416321412196));
#56987=CARTESIAN_POINT('Ctrl Pts',(52.7514284031959,29.9774157853516,19.420484871216));
#56988=CARTESIAN_POINT('Ctrl Pts',(52.7218091490529,29.902660897935,19.424648330236));
#56989=CARTESIAN_POINT('Ctrl Pts',(52.6921886781063,29.827902939475,19.4288119602972));
#56990=CARTESIAN_POINT('Ctrl Pts',(52.6662425610509,29.7516616285719,19.4329755903583));
#56991=CARTESIAN_POINT('Ctrl Pts',(52.6441099351468,29.674338381175,19.4371392204195));
#56992=CARTESIAN_POINT('Ctrl Pts',(52.6219780086933,29.5970175774014,19.4413027188987));
#56993=CARTESIAN_POINT('Ctrl Pts',(52.6036594574649,29.5186153673356,19.445466217378));
#56994=CARTESIAN_POINT('Ctrl Pts',(52.5892431215636,29.4395469520672,19.4496297158572));
#56995=CARTESIAN_POINT('Ctrl Pts',(52.574813058599,29.3604032487958,19.4537971787701));
#56996=CARTESIAN_POINT('Ctrl Pts',(52.5642927093787,29.2805925461025,19.457964641683));
#56997=CARTESIAN_POINT('Ctrl Pts',(52.5577193561152,29.2005380425392,19.4621321045959));
#56998=CARTESIAN_POINT('Ctrl Pts',(52.5521775537746,29.1330464263994,19.4656455709803));
#56999=CARTESIAN_POINT('Ctrl Pts',(52.549440251177,29.065381790129,19.4691590373647));
#57000=CARTESIAN_POINT('Ctrl Pts',(52.5495009896071,28.9977977140258,19.4726725037492));
#57001=CARTESIAN_POINT('',(52.549500306966,29.0012265563159,20.2726725038154));
#57002=CARTESIAN_POINT('Ctrl Pts',(52.5495009896078,28.9977977132792,19.472672503788));
#57003=CARTESIAN_POINT('Ctrl Pts',(52.5495996360256,28.8880331912387,19.4783787881767));
#57004=CARTESIAN_POINT('Ctrl Pts',(52.5570768997099,28.7785906334685,19.4840850725655));
#57005=CARTESIAN_POINT('Ctrl Pts',(52.571782136799,28.6702906449134,19.4897913569543));
#57006=CARTESIAN_POINT('Ctrl Pts',(52.5816900546492,28.5973215806758,19.4936360686452));
#57007=CARTESIAN_POINT('Ctrl Pts',(52.5948782273449,28.5248705095064,19.4974807803361));
#57008=CARTESIAN_POINT('Ctrl Pts',(52.6112889351492,28.4531822070749,19.501325492027));
#57009=CARTESIAN_POINT('Ctrl Pts',(52.6293553598906,28.3742610943379,19.5055581061985));
#57010=CARTESIAN_POINT('Ctrl Pts',(52.6513708184919,28.2960895275474,19.5097907203699));
#57011=CARTESIAN_POINT('Ctrl Pts',(52.6772574486544,28.2190920091532,19.5140233345414));
#57012=CARTESIAN_POINT('Ctrl Pts',(52.7031071539696,28.1422043204892,19.5182499112862));
#57013=CARTESIAN_POINT('Ctrl Pts',(52.7328169169065,28.0664877907818,19.5224764880309));
#57014=CARTESIAN_POINT('Ctrl Pts',(52.7662581568425,27.9923554058462,19.5267030647757));
#57015=CARTESIAN_POINT('Ctrl Pts',(52.7996622808747,27.9183052992732,19.5309249505097));
#57016=CARTESIAN_POINT('Ctrl Pts',(52.8367894626801,27.8458362652206,19.5351468362438));
#57017=CARTESIAN_POINT('Ctrl Pts',(52.8774622130622,27.7753434795744,19.5393687219778));
#57018=CARTESIAN_POINT('Ctrl Pts',(52.9181075309351,27.7048982391265,19.5435877601808));
#57019=CARTESIAN_POINT('Ctrl Pts',(52.9622934363404,27.6364270011302,19.5478067983838));
#57020=CARTESIAN_POINT('Ctrl Pts',(53.0097960531247,27.570301255564,19.5520258365868));
#57021=CARTESIAN_POINT('Ctrl Pts',(53.0572831572861,27.5041971042555,19.5562434970057));
#57022=CARTESIAN_POINT('Ctrl Pts',(53.1080845509981,27.4404373012421,19.5604611574247));
#57023=CARTESIAN_POINT('Ctrl Pts',(53.161933264215,27.3793640369285,19.5646788178436));
#57024=CARTESIAN_POINT('Ctrl Pts',(53.2157808568606,27.3182920435263,19.5688963904946));
#57025=CARTESIAN_POINT('Ctrl Pts',(53.2726753348195,27.2599068253392,19.5731139631456));
#57026=CARTESIAN_POINT('Ctrl Pts',(53.3323106532854,27.2045160839332,19.5773315357967));
#57027=CARTESIAN_POINT('Ctrl Pts',(53.3920472060373,27.1490313136479,19.581556268013));
#57028=CARTESIAN_POINT('Ctrl Pts',(53.4545335661553,27.0965515084368,19.5857810002293));
#57029=CARTESIAN_POINT('Ctrl Pts',(53.5194278031398,27.0473463645888,19.5900057324456));
#57030=CARTESIAN_POINT('Ctrl Pts',(53.5843058321073,26.9981535102421,19.5942294094907));
#57031=CARTESIAN_POINT('Ctrl Pts',(53.6515901382957,26.952233926921,19.5984530865358));
#57032=CARTESIAN_POINT('Ctrl Pts',(53.7209103735222,26.9098134108562,19.6026767635808));
#57033=CARTESIAN_POINT('Ctrl Pts',(53.7903563799615,26.8673159291011,19.6069081038571));
#57034=CARTESIAN_POINT('Ctrl Pts',(53.8618452885203,26.8283304249911,19.6111394441333));
#57035=CARTESIAN_POINT('Ctrl Pts',(53.9349820901553,26.7930366786668,19.6153707844095));
#57036=CARTESIAN_POINT('Ctrl Pts',(54.0079086952979,26.7578443672087,19.6195899637371));
#57037=CARTESIAN_POINT('Ctrl Pts',(54.0824732823083,26.7263227221686,19.6238091430648));
#57038=CARTESIAN_POINT('Ctrl Pts',(54.1582683298632,26.6986008504632,19.6280283223924));
#57039=CARTESIAN_POINT('Ctrl Pts',(54.2343047263982,26.6707907058999,19.6322609365639));
#57040=CARTESIAN_POINT('Ctrl Pts',(54.3118622421014,26.6467011639797,19.6364935507353));
#57041=CARTESIAN_POINT('Ctrl Pts',(54.3905424053107,26.6264980113184,19.6407261649068));
#57042=CARTESIAN_POINT('Ctrl Pts',(54.4691103386549,26.6063236765574,19.6449527416516));
#57043=CARTESIAN_POINT('Ctrl Pts',(54.5487972928023,26.5900248353889,19.6491793183964));
#57044=CARTESIAN_POINT('Ctrl Pts',(54.6291868454381,26.5777184609538,19.6534058951411));
#57045=CARTESIAN_POINT('Ctrl Pts',(54.7094871749796,26.5654257451693,19.6576277808752));
#57046=CARTESIAN_POINT('Ctrl Pts',(54.7904880966581,26.5571167613228,19.6618496666092));
#57047=CARTESIAN_POINT('Ctrl Pts',(54.8717615017094,26.5528577610698,19.6660715523432));
#57048=CARTESIAN_POINT('Ctrl Pts',(54.9529800903693,26.5486016333804,19.6702905905463));
#57049=CARTESIAN_POINT('Ctrl Pts',(55.034470334681,26.5483900883593,19.6745096287493));
#57050=CARTESIAN_POINT('Ctrl Pts',(55.1157987411205,26.5522375724848,19.6787286669523));
#57051=CARTESIAN_POINT('Ctrl Pts',(55.1971005886676,26.5560838001624,19.6829463273713));
#57052=CARTESIAN_POINT('Ctrl Pts',(55.2782402396263,26.5639864026279,19.6871639877902));
#57053=CARTESIAN_POINT('Ctrl Pts',(55.3587853173447,26.5759077274044,19.6913816482092));
#57054=CARTESIAN_POINT('Ctrl Pts',(55.4393287189506,26.5878288041026,19.6955992208602));
#57055=CARTESIAN_POINT('Ctrl Pts',(55.5192771125469,26.60376836766,19.6998167935113));
#57056=CARTESIAN_POINT('Ctrl Pts',(55.5982057792581,26.6236372129529,19.7040343661623));
#57057=CARTESIAN_POINT('Ctrl Pts',(55.6772684317915,26.643539786721,19.7082590983786));
#57058=CARTESIAN_POINT('Ctrl Pts',(55.7553074411604,26.6673848736874,19.7124838305949));
#57059=CARTESIAN_POINT('Ctrl Pts',(55.8319104320743,26.6950324768002,19.7167085628112));
#57060=CARTESIAN_POINT('Ctrl Pts',(55.9084942905876,26.7226731746341,19.7209322398563));
#57061=CARTESIAN_POINT('Ctrl Pts',(55.9836424260476,26.7541142898905,19.7251559169014));
#57062=CARTESIAN_POINT('Ctrl Pts',(56.0569638170305,26.7891680888208,19.7293795939465));
#57063=CARTESIAN_POINT('Ctrl Pts',(56.1304182387257,26.8242854876335,19.7336109342228));
#57064=CARTESIAN_POINT('Ctrl Pts',(56.202038882535,26.8630284477427,19.737842274499));
#57065=CARTESIAN_POINT('Ctrl Pts',(56.2714599010994,26.9051634980514,19.7420736147753));
#57066=CARTESIAN_POINT('Ctrl Pts',(56.3406814023974,26.9471774514613,19.7462927941028));
#57067=CARTESIAN_POINT('Ctrl Pts',(56.407715574752,26.9925636991414,19.7505119734303));
#57068=CARTESIAN_POINT('Ctrl Pts',(56.4722322650878,27.0410506878343,19.7547311527579));
#57069=CARTESIAN_POINT('Ctrl Pts',(56.5369543915045,27.0896920703265,19.7589637669293));
#57070=CARTESIAN_POINT('Ctrl Pts',(56.5993836810645,27.1416349050295,19.7631963811008));
#57071=CARTESIAN_POINT('Ctrl Pts',(56.6591641394782,27.1966351982282,19.7674289952723));
#57072=CARTESIAN_POINT('Ctrl Pts',(56.7188593266812,27.2515570386729,19.7716555720171));
#57073=CARTESIAN_POINT('Ctrl Pts',(56.7759128479175,27.3095273638339,19.7758821487618));
#57074=CARTESIAN_POINT('Ctrl Pts',(56.8299998825219,27.3702605484404,19.7801087255066));
#57075=CARTESIAN_POINT('Ctrl Pts',(56.8840268867811,27.4309263262448,19.7843306112407));
#57076=CARTESIAN_POINT('Ctrl Pts',(56.9350936391157,27.4943485252869,19.7885524969747));
#57077=CARTESIAN_POINT('Ctrl Pts',(56.9829115032094,27.5602041045898,19.7927743827087));
#57078=CARTESIAN_POINT('Ctrl Pts',(57.0306971156364,27.6260152663466,19.7969934209117));
#57079=CARTESIAN_POINT('Ctrl Pts',(57.0752379196429,27.6942561737829,19.8012124591147));
#57080=CARTESIAN_POINT('Ctrl Pts',(57.1162858029343,27.7645710662693,19.8054314973177));
#57081=CARTESIAN_POINT('Ctrl Pts',(57.1573202814835,27.8348629964755,19.8096491577367));
#57082=CARTESIAN_POINT('Ctrl Pts',(57.1948638705751,27.9072271657966,19.8138668181557));
#57083=CARTESIAN_POINT('Ctrl Pts',(57.2287127678591,27.9812803877505,19.8180844785746));
#57084=CARTESIAN_POINT('Ctrl Pts',(57.2625609607603,28.0553320686848,19.8223020512256));
#57085=CARTESIAN_POINT('Ctrl Pts',(57.2927144226679,28.1310723093763,19.8265196238767));
#57086=CARTESIAN_POINT('Ctrl Pts',(57.3190167637917,28.2080962815763,19.8307371965277));
#57087=CARTESIAN_POINT('Ctrl Pts',(57.3453637546093,28.2852510062735,19.834961928744));
#57088=CARTESIAN_POINT('Ctrl Pts',(57.3678463937328,28.3636933806243,19.8391866609603));
#57089=CARTESIAN_POINT('Ctrl Pts',(57.3863576167803,28.4430012793239,19.8434113931766));
#57090=CARTESIAN_POINT('Ctrl Pts',(57.4048642164555,28.5222893700436,19.8476350702217));
#57091=CARTESIAN_POINT('Ctrl Pts',(57.4194013213343,28.6024420903557,19.8518587472668));
#57092=CARTESIAN_POINT('Ctrl Pts',(57.4299135348426,28.6830292392211,19.8560824243119));
#57093=CARTESIAN_POINT('Ctrl Pts',(57.4404448211921,28.7637626014313,19.8603137645881));
#57094=CARTESIAN_POINT('Ctrl Pts',(57.446936585103,28.8449315029823,19.8645451048643));
#57095=CARTESIAN_POINT('Ctrl Pts',(57.4493855004242,28.9261019600266,19.8687764451406));
#57096=CARTESIAN_POINT('Ctrl Pts',(57.4518273775182,29.0070391317058,19.8729956244681));
#57097=CARTESIAN_POINT('Ctrl Pts',(57.4502497054639,29.0879773964062,19.8772148037957));
#57098=CARTESIAN_POINT('Ctrl Pts',(57.4447005343835,29.168491979587,19.8814339831233));
#57099=CARTESIAN_POINT('Ctrl Pts',(57.4391336934574,29.2492629398444,19.8856665972948));
#57100=CARTESIAN_POINT('Ctrl Pts',(57.4295492888961,29.3299079239494,19.8898992114663));
#57101=CARTESIAN_POINT('Ctrl Pts',(57.4159581852052,29.4099954845359,19.8941318256378));
#57102=CARTESIAN_POINT('Ctrl Pts',(57.4023864679476,29.4899688077372,19.8983584023826));
#57103=CARTESIAN_POINT('Ctrl Pts',(57.3848194797224,29.5693858324206,19.9025849791275));
#57104=CARTESIAN_POINT('Ctrl Pts',(57.3633199775803,29.64781859619,19.9068115558723));
#57105=CARTESIAN_POINT('Ctrl Pts',(57.3418443373963,29.7261643086731,19.9110334416063));
#57106=CARTESIAN_POINT('Ctrl Pts',(57.3164449780063,29.8035274851064,19.9152553273403));
#57107=CARTESIAN_POINT('Ctrl Pts',(57.2872357404877,29.8794901462982,19.9194772130743));
#57108=CARTESIAN_POINT('Ctrl Pts',(57.2580462036938,29.9554015730315,19.9236962512774));
#57109=CARTESIAN_POINT('Ctrl Pts',(57.2250520586072,30.0299139281105,19.9279152894805));
#57110=CARTESIAN_POINT('Ctrl Pts',(57.1884166536857,30.1026254123097,19.9321343276835));
#57111=CARTESIAN_POINT('Ctrl Pts',(57.1517932125517,30.1753131515891,19.9363519881025));
#57112=CARTESIAN_POINT('Ctrl Pts',(57.1115310819357,30.2462007733704,19.9405696485215));
#57113=CARTESIAN_POINT('Ctrl Pts',(57.0678407381616,30.3149087160708,19.9447873089405));
#57114=CARTESIAN_POINT('Ctrl Pts',(57.0241513035672,30.383615228985,19.9490048815916));
#57115=CARTESIAN_POINT('Ctrl Pts',(56.9770340479185,30.4501417616265,19.9532224542427));
#57116=CARTESIAN_POINT('Ctrl Pts',(56.9267434126354,30.5141367414689,19.9574400268938));
#57117=CARTESIAN_POINT('Ctrl Pts',(56.8763674061899,30.5782403563641,19.96166475911));
#57118=CARTESIAN_POINT('Ctrl Pts',(56.8228075305529,30.6398034530804,19.9658894913263));
#57119=CARTESIAN_POINT('Ctrl Pts',(56.7663595891434,30.698506417957,19.9701142235425));
#57120=CARTESIAN_POINT('Ctrl Pts',(56.7099257461982,30.7571947211536,19.9743379005877));
#57121=CARTESIAN_POINT('Ctrl Pts',(56.6506056339709,30.813024017022,19.9785615776328));
#57122=CARTESIAN_POINT('Ctrl Pts',(56.5887299580062,30.8657136357259,19.982785254678));
#57123=CARTESIAN_POINT('Ctrl Pts',(56.5267420178696,30.9184988518729,19.9870165949542));
#57124=CARTESIAN_POINT('Ctrl Pts',(56.4621896170737,30.96813272266,19.9912479352305));
#57125=CARTESIAN_POINT('Ctrl Pts',(56.3954349814589,31.0143761968711,19.9954792755068));
#57126=CARTESIAN_POINT('Ctrl Pts',(56.328872199882,31.0604867664955,19.9996984548341));
#57127=CARTESIAN_POINT('Ctrl Pts',(56.2601202556544,31.1032262319335,20.0039176341614));
#57128=CARTESIAN_POINT('Ctrl Pts',(56.189561618902,31.1424036512374,20.0081368134887));
#57129=CARTESIAN_POINT('Ctrl Pts',(56.1187783071086,31.1817058205179,20.0123694276602));
#57130=CARTESIAN_POINT('Ctrl Pts',(56.0459135024077,31.2175693745498,20.0166020418316));
#57131=CARTESIAN_POINT('Ctrl Pts',(55.9713350283798,31.2497685464604,20.0208346560031));
#57132=CARTESIAN_POINT('Ctrl Pts',(55.8968629335426,31.2819217892755,20.0250612327478));
#57133=CARTESIAN_POINT('Ctrl Pts',(55.8206824472001,31.3104208486512,20.0292878094926));
#57134=CARTESIAN_POINT('Ctrl Pts',(55.7431867199957,31.3350853837113,20.0335143862373));
#57135=CARTESIAN_POINT('Ctrl Pts',(55.6657770040739,31.3597225439937,20.0377362719714));
#57136=CARTESIAN_POINT('Ctrl Pts',(55.5870553882782,31.3805334962032,20.0419581577054));
#57137=CARTESIAN_POINT('Ctrl Pts',(55.5074344592735,31.3973861848984,20.0461800434394));
#57138=CARTESIAN_POINT('Ctrl Pts',(55.4278672321169,31.4142275069776,20.0503990816424));
#57139=CARTESIAN_POINT('Ctrl Pts',(55.3474023497371,31.427115771904,20.0546181198454));
#57140=CARTESIAN_POINT('Ctrl Pts',(55.2664657784925,31.4359692606625,20.0588371580484));
#57141=CARTESIAN_POINT('Ctrl Pts',(55.1855556381812,31.4448198581943,20.0630548184674));
#57142=CARTESIAN_POINT('Ctrl Pts',(55.1041745763518,31.4496382457765,20.0672724788863));
#57143=CARTESIAN_POINT('Ctrl Pts',(55.0227555623159,31.4503943426281,20.0714901393053));
#57144=CARTESIAN_POINT('Ctrl Pts',(54.9413382425788,31.4511504237456,20.0757077119563));
#57145=CARTESIAN_POINT('Ctrl Pts',(54.859883436744,31.4478443790698,20.0799252846073));
#57146=CARTESIAN_POINT('Ctrl Pts',(54.7788245708301,31.4404982441156,20.0841428572583));
#57147=CARTESIAN_POINT('Ctrl Pts',(54.6976281029607,31.4331396386869,20.0883675894746));
#57148=CARTESIAN_POINT('Ctrl Pts',(54.6168293848757,31.4217272633144,20.092592321691));
#57149=CARTESIAN_POINT('Ctrl Pts',(54.5368575521966,31.4063352474339,20.0968170539073));
#57150=CARTESIAN_POINT('Ctrl Pts',(54.4569056933225,31.390947075871,20.1010407309524));
#57151=CARTESIAN_POINT('Ctrl Pts',(54.3777807545964,31.3715813829267,20.1052644079975));
#57152=CARTESIAN_POINT('Ctrl Pts',(54.2998982053227,31.3483627758695,20.1094880850425));
#57153=CARTESIAN_POINT('Ctrl Pts',(54.2218743497963,31.3251020421179,20.1137194253188));
#57154=CARTESIAN_POINT('Ctrl Pts',(54.1450978278075,31.297974579116,20.117950765595));
#57155=CARTESIAN_POINT('Ctrl Pts',(54.0699663575865,31.2671540913619,20.1221821058712));
#57156=CARTESIAN_POINT('Ctrl Pts',(53.9950508165709,31.2364221822475,20.1264012851989));
#57157=CARTESIAN_POINT('Ctrl Pts',(53.9217712608793,31.202018716437,20.1306204645265));
#57158=CARTESIAN_POINT('Ctrl Pts',(53.8504960744794,31.1641605705706,20.1348396438542));
#57159=CARTESIAN_POINT('Ctrl Pts',(53.7789939313854,31.1261818756035,20.1390722580256));
#57160=CARTESIAN_POINT('Ctrl Pts',(53.7092430190922,31.0845851869611,20.143304872197));
#57161=CARTESIAN_POINT('Ctrl Pts',(53.6416329600019,31.0395561366746,20.1475374863684));
#57162=CARTESIAN_POINT('Ctrl Pts',(53.5741193403127,30.9945913161002,20.1517640631132));
#57163=CARTESIAN_POINT('Ctrl Pts',(53.5087408921651,30.9462041132224,20.1559906398579));
#57164=CARTESIAN_POINT('Ctrl Pts',(53.4458629215627,30.8946261350004,20.1602172166026));
#57165=CARTESIAN_POINT('Ctrl Pts',(53.3830547382254,30.8431054023605,20.1644391023366));
#57166=CARTESIAN_POINT('Ctrl Pts',(53.3227418753958,30.7884012242506,20.1686609880707));
#57167=CARTESIAN_POINT('Ctrl Pts',(53.2652597170226,30.730787797685,20.1728828738047));
#57168=CARTESIAN_POINT('Ctrl Pts',(53.2078163285839,30.6732132295903,20.1771019120077));
#57169=CARTESIAN_POINT('Ctrl Pts',(53.1532001799829,30.6127336381475,20.1813209502106));
#57170=CARTESIAN_POINT('Ctrl Pts',(53.1017117156202,30.5496618467867,20.1855399884136));
#57171=CARTESIAN_POINT('Ctrl Pts',(53.0502400655128,30.4866106523734,20.1897576488325));
#57172=CARTESIAN_POINT('Ctrl Pts',(53.001894364779,30.4209692987631,20.1939753092514));
#57173=CARTESIAN_POINT('Ctrl Pts',(52.9569355547793,30.3530845955354,20.1981929696703));
#57174=CARTESIAN_POINT('Ctrl Pts',(52.9119776803554,30.2852013049627,20.2024105423212));
#57175=CARTESIAN_POINT('Ctrl Pts',(52.870406812062,30.2150751455486,20.2066281149722));
#57176=CARTESIAN_POINT('Ctrl Pts',(52.832440423427,30.1430816821237,20.2108456876232));
#57177=CARTESIAN_POINT('Ctrl Pts',(52.7944095847245,30.0709660057692,20.2150704198396));
#57178=CARTESIAN_POINT('Ctrl Pts',(52.7599956858202,29.9969770963422,20.219295152056));
#57179=CARTESIAN_POINT('Ctrl Pts',(52.7293701668518,29.9215152797525,20.2235198842723));
#57180=CARTESIAN_POINT('Ctrl Pts',(52.6987522969291,29.8460723105456,20.2277435613174));
#57181=CARTESIAN_POINT('Ctrl Pts',(52.6719210482788,29.7691576169731,20.2319672383624));
#57182=CARTESIAN_POINT('Ctrl Pts',(52.648998079005,29.6911875414659,20.2361909154074));
#57183=CARTESIAN_POINT('Ctrl Pts',(52.6260335194273,29.6130760009028,20.2404222556836));
#57184=CARTESIAN_POINT('Ctrl Pts',(52.6069915192758,29.5339057046566,20.2446535959598));
#57185=CARTESIAN_POINT('Ctrl Pts',(52.5919428889606,29.4541048336809,20.248884936236));
#57186=CARTESIAN_POINT('Ctrl Pts',(52.5769375086802,29.3745333118474,20.2531041155639));
#57187=CARTESIAN_POINT('Ctrl Pts',(52.5659025545103,29.2943352973498,20.2573232948918));
#57188=CARTESIAN_POINT('Ctrl Pts',(52.5588566533828,29.2139378677712,20.2615424742197));
#57189=CARTESIAN_POINT('Ctrl Pts',(52.5526610497839,29.143242779234,20.2652524840758));
#57190=CARTESIAN_POINT('Ctrl Pts',(52.5495358689406,29.0722747171758,20.2689624939319));
#57191=CARTESIAN_POINT('Ctrl Pts',(52.5495003069663,29.0012265568403,20.272672503788));
#57192=CARTESIAN_POINT('',(52.5495003092563,29.0012311234037,21.072672503762));
#57193=CARTESIAN_POINT('Ctrl Pts',(52.549500306966,29.0012265563159,20.2726725038154));
#57194=CARTESIAN_POINT('Ctrl Pts',(52.5494602204554,28.9211389315022,20.276854538593));
#57195=CARTESIAN_POINT('Ctrl Pts',(52.5533505212183,28.8408938744122,20.2810365733706));
#57196=CARTESIAN_POINT('Ctrl Pts',(52.5611912006416,28.7609144710107,20.2852186081482));
#57197=CARTESIAN_POINT('Ctrl Pts',(52.5692395086798,28.6788171372802,20.2895113871664));
#57198=CARTESIAN_POINT('Ctrl Pts',(52.5814504704765,28.5970002272627,20.2938041661846));
#57199=CARTESIAN_POINT('Ctrl Pts',(52.597788511568,28.5159233378427,20.2980969452028));
#57200=CARTESIAN_POINT('Ctrl Pts',(52.6136681749886,28.437121129673,20.3022692866461));
#57201=CARTESIAN_POINT('Ctrl Pts',(52.633446299331,28.3590184693443,20.3064416280894));
#57202=CARTESIAN_POINT('Ctrl Pts',(52.6570377636194,28.2820318886647,20.3106139695326));
#57203=CARTESIAN_POINT('Ctrl Pts',(52.6806175758626,28.2050833323785,20.3147842502174));
#57204=CARTESIAN_POINT('Ctrl Pts',(52.7080068516926,28.129250216667,20.3189545309021));
#57205=CARTESIAN_POINT('Ctrl Pts',(52.7390700458616,28.0549359849833,20.3231248115869));
#57206=CARTESIAN_POINT('Ctrl Pts',(52.7701279301895,27.9806344563317,20.3272943794175));
#57207=CARTESIAN_POINT('Ctrl Pts',(52.8048583016476,27.9078517353656,20.3314639472481));
#57208=CARTESIAN_POINT('Ctrl Pts',(52.8430772801611,27.8369717842447,20.3356335150786));
#57209=CARTESIAN_POINT('Ctrl Pts',(52.8832646755621,27.7624412569391,20.3400178308708));
#57210=CARTESIAN_POINT('Ctrl Pts',(52.9273094397009,27.6900152887277,20.3444021466631));
#57211=CARTESIAN_POINT('Ctrl Pts',(52.9749438292944,27.6201095132267,20.3487864624553));
#57212=CARTESIAN_POINT('Ctrl Pts',(53.020301483121,27.5535449578141,20.3529612252614));
#57213=CARTESIAN_POINT('Ctrl Pts',(53.0689131459155,27.489265569475,20.3571359880676));
#57214=CARTESIAN_POINT('Ctrl Pts',(53.1205052786273,27.4275974299397,20.3613107508737));
#57215=CARTESIAN_POINT('Ctrl Pts',(53.1721317381003,27.3658882595846,20.3654882913531));
#57216=CARTESIAN_POINT('Ctrl Pts',(53.2267422873025,27.3067941411329,20.3696658318325));
#57217=CARTESIAN_POINT('Ctrl Pts',(53.2840263694769,27.2506044617213,20.3738433723119));
#57218=CARTESIAN_POINT('Ctrl Pts',(53.341399074354,27.1943278527288,20.3780273757547));
#57219=CARTESIAN_POINT('Ctrl Pts',(53.4014532028681,27.1409649548513,20.3822113791975));
#57220=CARTESIAN_POINT('Ctrl Pts',(53.4638457085829,27.0907644872984,20.3863953826403));
#57221=CARTESIAN_POINT('Ctrl Pts',(53.4730411491932,27.083365915744,20.3870120232886));
#57222=CARTESIAN_POINT('Ctrl Pts',(53.4822873330595,27.0760359569583,20.3876286639368));
#57223=CARTESIAN_POINT('Ctrl Pts',(53.4915831133027,27.0687753248453,20.3882453045851));
#57224=CARTESIAN_POINT('Ctrl Pts',(53.5553892397709,27.0189384312525,20.3924779187563));
#57225=CARTESIAN_POINT('Ctrl Pts',(53.6217865330381,26.9721744096337,20.3967105329275));
#57226=CARTESIAN_POINT('Ctrl Pts',(53.6904467768475,26.9287635080148,20.4009431470987));
#57227=CARTESIAN_POINT('Ctrl Pts',(53.7590090832661,26.885414527971,20.4051697238432));
#57228=CARTESIAN_POINT('Ctrl Pts',(53.8298275398407,26.8454094146431,20.4093963005877));
#57229=CARTESIAN_POINT('Ctrl Pts',(53.9025418437445,26.8089874840001,20.4136228773322));
#57230=CARTESIAN_POINT('Ctrl Pts',(53.9751754431973,26.7726059774795,20.4178447630663));
#57231=CARTESIAN_POINT('Ctrl Pts',(54.049700295733,26.7397999585165,20.4220666488004));
#57232=CARTESIAN_POINT('Ctrl Pts',(54.1257293863423,26.7107640698052,20.4262885345345));
#57233=CARTESIAN_POINT('Ctrl Pts',(54.2017071976815,26.6817477649029,20.4305075727372));
#57234=CARTESIAN_POINT('Ctrl Pts',(54.2791867992283,26.6564967052678,20.43472661094));
#57235=CARTESIAN_POINT('Ctrl Pts',(54.3577601272413,26.6351578919854,20.4389456491427));
#57236=CARTESIAN_POINT('Ctrl Pts',(54.4363077960701,26.6138260471814,20.4431633095614));
#57237=CARTESIAN_POINT('Ctrl Pts',(54.5159480340786,26.5964040331587,20.4473809699801));
#57238=CARTESIAN_POINT('Ctrl Pts',(54.5962578253218,26.5829889312653,20.4515986303988));
#57239=CARTESIAN_POINT('Ctrl Pts',(54.6765659453488,26.5695741085351,20.4558162030496));
#57240=CARTESIAN_POINT('Ctrl Pts',(54.757543132515,26.5601661075289,20.4600337757003));
#57241=CARTESIAN_POINT('Ctrl Pts',(54.8387578108094,26.5548105990691,20.4642513483511));
#57242=CARTESIAN_POINT('Ctrl Pts',(54.9201103555698,26.5494459993336,20.4684760805677));
#57243=CARTESIAN_POINT('Ctrl Pts',(55.0017007320943,26.5481476868118,20.4727008127844));
#57244=CARTESIAN_POINT('Ctrl Pts',(55.0830934970774,26.5509092052879,20.476925545001));
#57245=CARTESIAN_POINT('Ctrl Pts',(55.1644659333525,26.5536700340454,20.4811492220458));
#57246=CARTESIAN_POINT('Ctrl Pts',(55.2456403940463,26.560488605887,20.4853728990907));
#57247=CARTESIAN_POINT('Ctrl Pts',(55.3261870817444,26.5713064751387,20.4895965761355));
#57248=CARTESIAN_POINT('Ctrl Pts',(55.4068799093768,26.5821439717984,20.4938279164115));
#57249=CARTESIAN_POINT('Ctrl Pts',(55.4869422296769,26.5969951820191,20.4980592566875));
#57250=CARTESIAN_POINT('Ctrl Pts',(55.5659541409433,26.6157503988993,20.5022905969635));
#57251=CARTESIAN_POINT('Ctrl Pts',(55.6447389705763,26.6344517129537,20.5065097762925));
#57252=CARTESIAN_POINT('Ctrl Pts',(55.7224790069256,26.6570344163943,20.5107289556215));
#57253=CARTESIAN_POINT('Ctrl Pts',(55.7987766080229,26.6833415917586,20.5149481349506));
#57254=CARTESIAN_POINT('Ctrl Pts',(55.8753171583144,26.7097325352489,20.5191807491216));
#57255=CARTESIAN_POINT('Ctrl Pts',(55.9506907393684,26.7399698887984,20.5234133632927));
#57256=CARTESIAN_POINT('Ctrl Pts',(56.0244835908758,26.7739309035822,20.5276459774637));
#57257=CARTESIAN_POINT('Ctrl Pts',(56.0981711838093,26.8078434761672,20.5318725542081));
#57258=CARTESIAN_POINT('Ctrl Pts',(56.1702821069487,26.8454689681559,20.5360991309525));
#57259=CARTESIAN_POINT('Ctrl Pts',(56.2404194668725,26.8866354322541,20.5403257076968));
#57260=CARTESIAN_POINT('Ctrl Pts',(56.3104789824573,26.9277562063493,20.544547593431));
#57261=CARTESIAN_POINT('Ctrl Pts',(56.3785688885819,26.9724099095512,20.5487694791651));
#57262=CARTESIAN_POINT('Ctrl Pts',(56.4443152227609,27.0203778675461,20.5529913648992));
#57263=CARTESIAN_POINT('Ctrl Pts',(56.5100172130679,27.0683134726348,20.5572104031018));
#57264=CARTESIAN_POINT('Ctrl Pts',(56.5733783964576,27.119558619795,20.5614294413044));
#57265=CARTESIAN_POINT('Ctrl Pts',(56.6340533144811,27.1738510423755,20.565648479507));
#57266=CARTESIAN_POINT('Ctrl Pts',(56.6947084182886,27.2281257350301,20.5698661399255));
#57267=CARTESIAN_POINT('Ctrl Pts',(56.7526786529445,27.285445417305,20.574083800344));
#57268=CARTESIAN_POINT('Ctrl Pts',(56.8076522939434,27.345508103918,20.5783014607626));
#57269=CARTESIAN_POINT('Ctrl Pts',(56.8626247909617,27.4055695406493,20.5825190334132));
#57270=CARTESIAN_POINT('Ctrl Pts',(56.9146005055265,27.4683735247527,20.5867366060638));
#57271=CARTESIAN_POINT('Ctrl Pts',(56.9633061774716,27.5335829026154,20.5909541787144));
#57272=CARTESIAN_POINT('Ctrl Pts',(57.0120945300272,27.5989029770553,20.5951789109312));
#57273=CARTESIAN_POINT('Ctrl Pts',(57.0576014540899,27.6666362408167,20.599403643148));
#57274=CARTESIAN_POINT('Ctrl Pts',(57.09959530961,27.7364139183008,20.6036283753648));
#57275=CARTESIAN_POINT('Ctrl Pts',(57.1415786767147,27.8061741680626,20.6078520524095));
#57276=CARTESIAN_POINT('Ctrl Pts',(57.1800505284885,27.8779773895188,20.6120757294541));
#57277=CARTESIAN_POINT('Ctrl Pts',(57.214825908578,27.9514312398839,20.6162994064988));
#57278=CARTESIAN_POINT('Ctrl Pts',(57.2496643834006,28.0250183612891,20.6205307467746));
#57279=CARTESIAN_POINT('Ctrl Pts',(57.280792805333,28.1002616661367,20.6247620870504));
#57280=CARTESIAN_POINT('Ctrl Pts',(57.3080746044668,28.1767492057608,20.6289934273262));
#57281=CARTESIAN_POINT('Ctrl Pts',(57.3352779952332,28.2530169188596,20.6332126066561));
#57282=CARTESIAN_POINT('Ctrl Pts',(57.3586567923574,28.3305212645066,20.6374317859861));
#57283=CARTESIAN_POINT('Ctrl Pts',(57.3781261455574,28.4088432645937,20.641650965316));
#57284=CARTESIAN_POINT('Ctrl Pts',(57.3976574936843,28.4874146600572,20.6458835794894));
#57285=CARTESIAN_POINT('Ctrl Pts',(57.41332707702,28.5671011610222,20.6501161936629));
#57286=CARTESIAN_POINT('Ctrl Pts',(57.4250126089298,28.6474888703437,20.6543488078364));
#57287=CARTESIAN_POINT('Ctrl Pts',(57.4366814725256,28.7277619141462,20.6585753845831));
#57288=CARTESIAN_POINT('Ctrl Pts',(57.4443775053466,28.8087337238667,20.6628019613299));
#57289=CARTESIAN_POINT('Ctrl Pts',(57.4480288720224,28.8899777670446,20.6670285380767));
#57290=CARTESIAN_POINT('Ctrl Pts',(57.4516761861019,28.9711316386948,20.6712504238102));
#57291=CARTESIAN_POINT('Ctrl Pts',(57.4512877331433,29.0525566816944,20.6754723095438));
#57292=CARTESIAN_POINT('Ctrl Pts',(57.4468433571991,29.1338201604047,20.6796941952773));
#57293=CARTESIAN_POINT('Ctrl Pts',(57.442401978846,29.2150288294664,20.6839132334823));
#57294=CARTESIAN_POINT('Ctrl Pts',(57.4339101359348,29.2960756880045,20.6881322716873));
#57295=CARTESIAN_POINT('Ctrl Pts',(57.4213997564911,29.3765281785804,20.6923513098923));
#57296=CARTESIAN_POINT('Ctrl Pts',(57.4088934624811,29.4569543963059,20.6965689703133));
#57297=CARTESIAN_POINT('Ctrl Pts',(57.3923713094257,29.5367861728579,20.7007866307342));
#57298=CARTESIAN_POINT('Ctrl Pts',(57.3719169071258,29.6155976248256,20.7050042911551));
#57299=CARTESIAN_POINT('Ctrl Pts',(57.3514629304743,29.6944074367566,20.7092218638082));
#57300=CARTESIAN_POINT('Ctrl Pts',(57.3270769851119,29.7721965169635,20.7134394364612));
#57301=CARTESIAN_POINT('Ctrl Pts',(57.2988931209399,29.848552101226,20.7176570091142));
#57302=CARTESIAN_POINT('Ctrl Pts',(57.2706614131126,29.9250373032813,20.7218817413281));
#57303=CARTESIAN_POINT('Ctrl Pts',(57.2386190488923,30.0000837025487,20.7261064735421));
#57304=CARTESIAN_POINT('Ctrl Pts',(57.2029492615242,30.0732962317784,20.730331205756));
#57305=CARTESIAN_POINT('Ctrl Pts',(57.1672883830236,30.1464904754851,20.734554882803));
#57306=CARTESIAN_POINT('Ctrl Pts',(57.1280021365455,30.2178513669816,20.7387785598501));
#57307=CARTESIAN_POINT('Ctrl Pts',(57.0853189387287,30.2870101684833,20.7430022368971));
#57308=CARTESIAN_POINT('Ctrl Pts',(57.0425582986253,30.3562944482997,20.7472335771752));
#57309=CARTESIAN_POINT('Ctrl Pts',(56.9963886542809,30.4233682697559,20.7514649174534));
#57310=CARTESIAN_POINT('Ctrl Pts',(56.9470812098606,30.4878928093811,20.7556962577315));
#57311=CARTESIAN_POINT('Ctrl Pts',(56.8979154760785,30.5522319041146,20.7599154370481));
#57312=CARTESIAN_POINT('Ctrl Pts',(56.8456303118749,30.6140360569888,20.7641346163648));
#57313=CARTESIAN_POINT('Ctrl Pts',(56.7905309740915,30.6730060014295,20.7683537956815));
#57314=CARTESIAN_POINT('Ctrl Pts',(56.7352561871496,30.732163719944,20.7725864098504));
#57315=CARTESIAN_POINT('Ctrl Pts',(56.6769436737209,30.7886891570702,20.7768190240193));
#57316=CARTESIAN_POINT('Ctrl Pts',(56.6158740482287,30.8422544097548,20.7810516381881));
#57317=CARTESIAN_POINT('Ctrl Pts',(56.5548915328232,30.8957432566359,20.7852782149303));
#57318=CARTESIAN_POINT('Ctrl Pts',(56.4911600626649,30.946280001575,20.7895047916725));
#57319=CARTESIAN_POINT('Ctrl Pts',(56.4249983167076,30.9935721826361,20.7937313684147));
#57320=CARTESIAN_POINT('Ctrl Pts',(56.3589100025761,31.0408118748889,20.7979532541494));
#57321=CARTESIAN_POINT('Ctrl Pts',(56.2903971482431,31.0848138898379,20.8021751398841));
#57322=CARTESIAN_POINT('Ctrl Pts',(56.2198117703657,31.1253257385345,20.8063970256187));
#57323=CARTESIAN_POINT('Ctrl Pts',(56.1492740001902,31.1658102632148,20.8106160638192));
#57324=CARTESIAN_POINT('Ctrl Pts',(56.0766668845959,31.2028090662687,20.8148351020197));
#57325=CARTESIAN_POINT('Ctrl Pts',(56.0023706453165,31.2361134451114,20.8190541402202));
#57326=CARTESIAN_POINT('Ctrl Pts',(55.9280986684798,31.2694069479582,20.8232718006366));
#57327=CARTESIAN_POINT('Ctrl Pts',(55.8521390869959,31.2990082326812,20.827489461053));
#57328=CARTESIAN_POINT('Ctrl Pts',(55.7748946598559,31.3247555820187,20.8317071214695));
#57329=CARTESIAN_POINT('Ctrl Pts',(55.6976518401427,31.3505023955637,20.835924694118));
#57330=CARTESIAN_POINT('Ctrl Pts',(55.6191246690153,31.3723952873945,20.8401422667666));
#57331=CARTESIAN_POINT('Ctrl Pts',(55.5397323603883,31.3903219927762,20.8443598394151));
#57332=CARTESIAN_POINT('Ctrl Pts',(55.4602052787772,31.4082791297655,20.8485845716344));
#57333=CARTESIAN_POINT('Ctrl Pts',(55.3798105768262,31.4222565066309,20.8528093038538));
#57334=CARTESIAN_POINT('Ctrl Pts',(55.2989793992393,31.4321927491115,20.8570340360731));
#57335=CARTESIAN_POINT('Ctrl Pts',(55.2181684101908,31.4421265098985,20.8612577131158));
#57336=CARTESIAN_POINT('Ctrl Pts',(55.1369216299782,31.4480211421537,20.8654813901585));
#57337=CARTESIAN_POINT('Ctrl Pts',(55.0556727153591,31.4498675063694,20.8697050672012));
#57338=CARTESIAN_POINT('Ctrl Pts',(54.9742763867188,31.4517172205371,20.8739364074751));
#57339=CARTESIAN_POINT('Ctrl Pts',(54.8928783816584,31.4495040006416,20.8781677477489));
#57340=CARTESIAN_POINT('Ctrl Pts',(54.8119105576179,31.4432708838081,20.8823990880228));
#57341=CARTESIAN_POINT('Ctrl Pts',(54.7311754362634,31.4370556810417,20.8866182673642));
#57342=CARTESIAN_POINT('Ctrl Pts',(54.6508684676596,31.426843796904,20.8908374467055));
#57343=CARTESIAN_POINT('Ctrl Pts',(54.5714068662368,31.4127283675729,20.8950566260469));
#57344=CARTESIAN_POINT('Ctrl Pts',(54.4916922409749,31.3985679914995,20.8992892402163));
#57345=CARTESIAN_POINT('Ctrl Pts',(54.4125318989979,31.3804264777048,20.9035218543858));
#57346=CARTESIAN_POINT('Ctrl Pts',(54.3343536603774,31.3583607019595,20.9077544685552));
#57347=CARTESIAN_POINT('Ctrl Pts',(54.2562869356745,31.3363264009717,20.9119810452979));
#57348=CARTESIAN_POINT('Ctrl Pts',(54.17919997537,31.3103790807106,20.9162076220406));
#57349=CARTESIAN_POINT('Ctrl Pts',(54.1035115929932,31.2806268406082,20.9204341987833));
#57350=CARTESIAN_POINT('Ctrl Pts',(54.0279072159099,31.2509076220288,20.9246560845179));
#57351=CARTESIAN_POINT('Ctrl Pts',(53.9536987625856,31.2173920438296,20.9288779702524));
#57352=CARTESIAN_POINT('Ctrl Pts',(53.8812896652721,31.1802379312756,20.933099855987));
#57353=CARTESIAN_POINT('Ctrl Pts',(53.808929405695,31.1431088780419,20.9373188941878));
#57354=CARTESIAN_POINT('Ctrl Pts',(53.7383665040388,31.1023463760024,20.9415379323887));
#57355=CARTESIAN_POINT('Ctrl Pts',(53.6699830183152,31.0581557468836,20.9457569705896));
#57356=CARTESIAN_POINT('Ctrl Pts',(53.6016218641454,31.0139795488135,20.9499746310064));
#57357=CARTESIAN_POINT('Ctrl Pts',(53.5354391023518,30.9663776988673,20.9541922914232));
#57358=CARTESIAN_POINT('Ctrl Pts',(53.471789647773,30.9156000024395,20.95840995184));
#57359=CARTESIAN_POINT('Ctrl Pts',(53.4081415177153,30.8648233626764,20.9626275244889));
#57360=CARTESIAN_POINT('Ctrl Pts',(53.3470269524701,30.810871298457,20.9668450971377));
#57361=CARTESIAN_POINT('Ctrl Pts',(53.2887683429225,30.7540343399762,20.9710626697866));
#57362=CARTESIAN_POINT('Ctrl Pts',(53.2304108360649,30.6971008975191,20.9752874020054));
#57363=CARTESIAN_POINT('Ctrl Pts',(53.1749193191843,30.6372730886131,20.9795121342242));
#57364=CARTESIAN_POINT('Ctrl Pts',(53.1225799900837,30.5748791561152,20.9837368664431));
#57365=CARTESIAN_POINT('Ctrl Pts',(53.0702537333381,30.5125008072262,20.987960543486));
#57366=CARTESIAN_POINT('Ctrl Pts',(53.0210783544406,30.4475580008846,20.9921842205289));
#57367=CARTESIAN_POINT('Ctrl Pts',(52.9752976029293,30.3804095237632,20.9964078975718));
#57368=CARTESIAN_POINT('Ctrl Pts',(52.9294337890823,30.3131392157595,21.0006392378458));
#57369=CARTESIAN_POINT('Ctrl Pts',(52.8869771541804,30.2436556369514,21.0048705781199));
#57370=CARTESIAN_POINT('Ctrl Pts',(52.8481267011361,30.1723444697001,21.0091019183939));
#57371=CARTESIAN_POINT('Ctrl Pts',(52.8093879048685,30.1012382517985,21.0133210977334));
#57372=CARTESIAN_POINT('Ctrl Pts',(52.7742347124606,30.0283153826651,21.0175402770729));
#57373=CARTESIAN_POINT('Ctrl Pts',(52.7428161308091,29.9539765356991,21.0217594564124));
#57374=CARTESIAN_POINT('Ctrl Pts',(52.7078707023516,29.8712928904894,21.026452253541));
#57375=CARTESIAN_POINT('Ctrl Pts',(52.6774339914087,29.786596450014,21.0311450506696));
#57376=CARTESIAN_POINT('Ctrl Pts',(52.6517168253079,29.700368746774,21.0358378477981));
#57377=CARTESIAN_POINT('Ctrl Pts',(52.6260780328311,29.6144038243387,21.0405163435252));
#57378=CARTESIAN_POINT('Ctrl Pts',(52.6051302149797,29.5269172078913,21.0451948392523));
#57379=CARTESIAN_POINT('Ctrl Pts',(52.5890358675761,29.4384087158869,21.0498733349793));
#57380=CARTESIAN_POINT('Ctrl Pts',(52.5730253979727,29.3503614974848,21.0545274481129));
#57381=CARTESIAN_POINT('Ctrl Pts',(52.5618180620469,29.2613032944131,21.0591815612465));
#57382=CARTESIAN_POINT('Ctrl Pts',(52.5555258256322,29.1717447549387,21.0638356743802));
#57383=CARTESIAN_POINT('Ctrl Pts',(52.551543440014,29.115062739819,21.0667812841741));
#57384=CARTESIAN_POINT('Ctrl Pts',(52.549528920529,29.0581806662824,21.0697268939681));
#57385=CARTESIAN_POINT('Ctrl Pts',(52.5495003092563,29.0012311234037,21.072672503762));
#57386=CARTESIAN_POINT('',(52.5495009304611,28.9978645400587,21.872672503788));
#57387=CARTESIAN_POINT('Ctrl Pts',(52.549500309256,29.0012311229018,21.072672503788));
#57388=CARTESIAN_POINT('Ctrl Pts',(52.5494587751325,28.9185591518343,21.0769485586139));
#57389=CARTESIAN_POINT('Ctrl Pts',(52.5536052143625,28.8358914090988,21.0812246134398));
#57390=CARTESIAN_POINT('Ctrl Pts',(52.561911940885,28.7536732535821,21.0855006682658));
#57391=CARTESIAN_POINT('Ctrl Pts',(52.5702215590747,28.6714264769786,21.0897782116356));
#57392=CARTESIAN_POINT('Ctrl Pts',(52.5826942985601,28.5896300427903,21.0940557550055));
#57393=CARTESIAN_POINT('Ctrl Pts',(52.5992507594021,28.508722752645,21.0983332983753));
#57394=CARTESIAN_POINT('Ctrl Pts',(52.6158308998912,28.4276997459772,21.1026169596419));
#57395=CARTESIAN_POINT('Ctrl Pts',(52.6365063365672,28.3475688614418,21.1069006209084));
#57396=CARTESIAN_POINT('Ctrl Pts',(52.6611468274167,28.2687571627038,21.111184282175));
#57397=CARTESIAN_POINT('Ctrl Pts',(52.6858051125588,28.1898885495789,21.1154710369157));
#57398=CARTESIAN_POINT('Ctrl Pts',(52.7144340011585,28.1123414389407,21.1197577916565));
#57399=CARTESIAN_POINT('Ctrl Pts',(52.7468546537972,28.0365238462294,21.1240445463972));
#57400=CARTESIAN_POINT('Ctrl Pts',(52.7793422161115,27.9605497813275,21.1283401481335));
#57401=CARTESIAN_POINT('Ctrl Pts',(52.8156369841557,27.8863127692337,21.1326357498698));
#57402=CARTESIAN_POINT('Ctrl Pts',(52.8555135416277,27.8141972845966,21.136931351606));
#57403=CARTESIAN_POINT('Ctrl Pts',(52.8911945340563,27.7496693457663,21.1407749966633));
#57404=CARTESIAN_POINT('Ctrl Pts',(52.9297425079146,27.6868398079593,21.1446186417206));
#57405=CARTESIAN_POINT('Ctrl Pts',(52.9709676970025,27.6259628231403,21.1484622867778));
#57406=CARTESIAN_POINT('Ctrl Pts',(53.0163647916923,27.5589252108114,21.1526949009266));
#57407=CARTESIAN_POINT('Ctrl Pts',(53.0651721812789,27.494015173616,21.1569275150754));
#57408=CARTESIAN_POINT('Ctrl Pts',(53.1171636882252,27.4316002827525,21.1611601292241));
#57409=CARTESIAN_POINT('Ctrl Pts',(53.1690810341687,27.3692744208701,21.1653867059462));
#57410=CARTESIAN_POINT('Ctrl Pts',(53.2241731819283,27.3094369904735,21.1696132826683));
#57411=CARTESIAN_POINT('Ctrl Pts',(53.2821708386307,27.2524264758388,21.1738398593905));
#57412=CARTESIAN_POINT('Ctrl Pts',(53.3401041250387,27.1954792358917,21.1780617451302));
#57413=CARTESIAN_POINT('Ctrl Pts',(53.4009361831773,27.1413530014533,21.1822836308699));
#57414=CARTESIAN_POINT('Ctrl Pts',(53.4643585689652,27.0903519577447,21.1865055166096));
#57415=CARTESIAN_POINT('Ctrl Pts',(53.5277381778993,27.0393853129974,21.1907245547902));
#57416=CARTESIAN_POINT('Ctrl Pts',(53.5937042834803,26.9915399629406,21.1949435929708));
#57417=CARTESIAN_POINT('Ctrl Pts',(53.6619137672141,26.9470812281951,21.1991626311515));
#57418=CARTESIAN_POINT('Ctrl Pts',(53.7301009762197,26.90263701205,21.2033802915482));
#57419=CARTESIAN_POINT('Ctrl Pts',(53.800529719589,26.8615774683478,21.207597951945));
#57420=CARTESIAN_POINT('Ctrl Pts',(53.8728273054669,26.8241250112428,21.2118156123417));
#57421=CARTESIAN_POINT('Ctrl Pts',(53.9451233868624,26.7866733335078,21.2160331849707));
#57422=CARTESIAN_POINT('Ctrl Pts',(54.0192878204168,26.7528288057658,21.2202507575997));
#57423=CARTESIAN_POINT('Ctrl Pts',(54.0949239652938,26.7227675521808,21.2244683302287));
#57424=CARTESIAN_POINT('Ctrl Pts',(54.1706885076261,26.6926552675912,21.2286930624716));
#57425=CARTESIAN_POINT('Ctrl Pts',(54.2479293258799,26.6663392792888,21.2329177947145));
#57426=CARTESIAN_POINT('Ctrl Pts',(54.3262300755266,26.6439472970931,21.2371425269573));
#57427=CARTESIAN_POINT('Ctrl Pts',(54.4045112678511,26.6215609077839,21.2413662039811));
#57428=CARTESIAN_POINT('Ctrl Pts',(54.4838514033151,26.603096649577,21.2455898810048));
#57429=CARTESIAN_POINT('Ctrl Pts',(54.5638235285909,26.5886310245445,21.2498135580286));
#57430=CARTESIAN_POINT('Ctrl Pts',(54.6439407513546,26.574139153794,21.254044898284));
#57431=CARTESIAN_POINT('Ctrl Pts',(54.7246917934493,26.5636604748885,21.2582762385395));
#57432=CARTESIAN_POINT('Ctrl Pts',(54.8056433606426,26.5572196687509,21.2625075787949));
#57433=CARTESIAN_POINT('Ctrl Pts',(54.8863622742927,26.5507973733897,21.2667267582444));
#57434=CARTESIAN_POINT('Ctrl Pts',(54.9672801044456,26.5483897026228,21.2709459376938));
#57435=CARTESIAN_POINT('Ctrl Pts',(55.047970226455,26.5499695701127,21.2751651171433));
#57436=CARTESIAN_POINT('Ctrl Pts',(55.1289172820323,26.5515544682182,21.2793977313082));
#57437=CARTESIAN_POINT('Ctrl Pts',(55.2099362412056,26.5571582613561,21.2836303454731));
#57438=CARTESIAN_POINT('Ctrl Pts',(55.2905956447453,26.5667913321593,21.287862959638));
#57439=CARTESIAN_POINT('Ctrl Pts',(55.3711399952143,26.576410662291,21.292089536376));
#57440=CARTESIAN_POINT('Ctrl Pts',(55.4513253512424,26.5900478004067,21.2963161131139));
#57441=CARTESIAN_POINT('Ctrl Pts',(55.5307211804204,26.6076611279643,21.3005426898519));
#57442=CARTESIAN_POINT('Ctrl Pts',(55.6100288895813,26.6252549068032,21.3047645755876));
#57443=CARTESIAN_POINT('Ctrl Pts',(55.6885483618252,26.6468160061563,21.3089864613233));
#57444=CARTESIAN_POINT('Ctrl Pts',(55.7658565217118,26.6722512940286,21.313208347059));
#57445=CARTESIAN_POINT('Ctrl Pts',(55.8431125394759,26.6976694265333,21.3174273852546));
#57446=CARTESIAN_POINT('Ctrl Pts',(55.9191584273671,26.7269564130436,21.3216464234502));
#57447=CARTESIAN_POINT('Ctrl Pts',(55.9935848337678,26.759968877871,21.3258654616459));
#57448=CARTESIAN_POINT('Ctrl Pts',(56.0679869352143,26.7929705620295,21.3300831220573));
#57449=CARTESIAN_POINT('Ctrl Pts',(56.1407701811375,26.8296951201886,21.3343007824686));
#57450=CARTESIAN_POINT('Ctrl Pts',(56.2115451111847,26.8699510114637,21.33851844288));
#57451=CARTESIAN_POINT('Ctrl Pts',(56.2823185684291,26.9102060650271,21.3427360155233));
#57452=CARTESIAN_POINT('Ctrl Pts',(56.3510833896731,26.9539920749009,21.3469535881666));
#57453=CARTESIAN_POINT('Ctrl Pts',(56.4174759059308,27.0010722108826,21.3511711608098));
#57454=CARTESIAN_POINT('Ctrl Pts',(56.4839811274529,27.0482322682091,21.3553958930347));
#57455=CARTESIAN_POINT('Ctrl Pts',(56.5481056057051,27.0986973697519,21.3596206252596));
#57456=CARTESIAN_POINT('Ctrl Pts',(56.6095155561762,27.1521878005525,21.3638453574845));
#57457=CARTESIAN_POINT('Ctrl Pts',(56.6709101686245,27.205664871345,21.3680690345215));
#57458=CARTESIAN_POINT('Ctrl Pts',(56.7295912880466,27.2621654217142,21.3722927115585));
#57459=CARTESIAN_POINT('Ctrl Pts',(56.7852623088348,27.321372960228,21.3765163885955));
#57460=CARTESIAN_POINT('Ctrl Pts',(56.8410343363732,27.380687921975,21.3807477288634));
#57461=CARTESIAN_POINT('Ctrl Pts',(56.8937850490903,27.4427193322646,21.3849790691314));
#57462=CARTESIAN_POINT('Ctrl Pts',(56.9432578582719,27.507117169278,21.3892104093993));
#57463=CARTESIAN_POINT('Ctrl Pts',(56.9925884822932,27.5713299265086,21.3934295887691));
#57464=CARTESIAN_POINT('Ctrl Pts',(57.0386598283554,27.6378951047047,21.3976487681389));
#57465=CARTESIAN_POINT('Ctrl Pts',(57.081262362369,27.7064400945507,21.4018679475087));
#57466=CARTESIAN_POINT('Ctrl Pts',(57.1240005533097,27.7752033484717,21.4061005617814));
#57467=CARTESIAN_POINT('Ctrl Pts',(57.1634067378801,27.8462148067079,21.4103331760541));
#57468=CARTESIAN_POINT('Ctrl Pts',(57.1992373201145,27.9191182026625,21.4145657903268));
#57469=CARTESIAN_POINT('Ctrl Pts',(57.2350167933919,27.9919176087766,21.4187923671731));
#57470=CARTESIAN_POINT('Ctrl Pts',(57.2672305909045,28.0666031792486,21.4230189440194));
#57471=CARTESIAN_POINT('Ctrl Pts',(57.2956792411472,28.1427911154416,21.4272455208658));
#57472=CARTESIAN_POINT('Ctrl Pts',(57.324096315829,28.2188944895624,21.4314674065745));
#57473=CARTESIAN_POINT('Ctrl Pts',(57.3487563852033,28.2964964830853,21.4356892922832));
#57474=CARTESIAN_POINT('Ctrl Pts',(57.3695072481432,28.375191508543,21.4399111779918));
#57475=CARTESIAN_POINT('Ctrl Pts',(57.3902441158939,28.453833459014,21.4441302162965));
#57476=CARTESIAN_POINT('Ctrl Pts',(57.4070768954282,28.5335665292747,21.4483492546013));
#57477=CARTESIAN_POINT('Ctrl Pts',(57.4199030025417,28.6139692910017,21.452568292906));
#57478=CARTESIAN_POINT('Ctrl Pts',(57.4327249211158,28.6943457961152,21.4567859534264));
#57479=CARTESIAN_POINT('Ctrl Pts',(57.4415426926126,28.77539109998,21.4610036139469));
#57480=CARTESIAN_POINT('Ctrl Pts',(57.4463049638303,28.8566742383964,21.4652212744674));
#57481=CARTESIAN_POINT('Ctrl Pts',(57.4510671359466,28.9379556853355,21.4694388472196));
#57482=CARTESIAN_POINT('Ctrl Pts',(57.4517739495821,29.0194744931645,21.4736564199719));
#57483=CARTESIAN_POINT('Ctrl Pts',(57.4484260821981,29.1007966765922,21.4778739927241));
#57484=CARTESIAN_POINT('Ctrl Pts',(57.4450725317982,29.1822569046934,21.48209872482));
#57485=CARTESIAN_POINT('Ctrl Pts',(57.4376505486444,29.2635193739974,21.4863234569158));
#57486=CARTESIAN_POINT('Ctrl Pts',(57.4262130521348,29.3441518206411,21.4905481890116));
#57487=CARTESIAN_POINT('Ctrl Pts',(57.414778411665,29.4247641326805,21.4947718661561));
#57488=CARTESIAN_POINT('Ctrl Pts',(57.3993303722698,29.5047462829996,21.4989955433006));
#57489=CARTESIAN_POINT('Ctrl Pts',(57.3799729426143,29.583677173122,21.5032192204451));
#57490=CARTESIAN_POINT('Ctrl Pts',(57.3605803918034,29.6627512715168,21.5074505608188));
#57491=CARTESIAN_POINT('Ctrl Pts',(57.3372644090129,29.7407698515431,21.5116819011926));
#57492=CARTESIAN_POINT('Ctrl Pts',(57.3101789142712,29.8173271279338,21.5159132415663));
#57493=CARTESIAN_POINT('Ctrl Pts',(57.2831712679286,29.8936643654639,21.5201324203356));
#57494=CARTESIAN_POINT('Ctrl Pts',(57.2524159990534,29.9685482987032,21.5243515991049));
#57495=CARTESIAN_POINT('Ctrl Pts',(57.2181115911092,30.041600316526,21.5285707778742));
#57496=CARTESIAN_POINT('Ctrl Pts',(57.1836979469842,30.1148849552832,21.5328033918549));
#57497=CARTESIAN_POINT('Ctrl Pts',(57.1455845058485,30.1865985476052,21.5370360058357));
#57498=CARTESIAN_POINT('Ctrl Pts',(57.1039374992242,30.2563428072618,21.5412686198164));
#57499=CARTESIAN_POINT('Ctrl Pts',(57.0623498981447,30.32598758328,21.5454951963707));
#57500=CARTESIAN_POINT('Ctrl Pts',(57.0172389784502,30.3936682102684,21.549721772925));
#57501=CARTESIAN_POINT('Ctrl Pts',(56.968818087626,30.4590084262391,21.5539483494793));
#57502=CARTESIAN_POINT('Ctrl Pts',(56.9204509356576,30.5242761258149,21.558170235261));
#57503=CARTESIAN_POINT('Ctrl Pts',(56.8687813869854,30.5872082041524,21.5623921210426));
#57504=CARTESIAN_POINT('Ctrl Pts',(56.8140668002175,30.6474561889011,21.5666140068243));
#57505=CARTESIAN_POINT('Ctrl Pts',(56.7593891198028,30.7076635348818,21.5708330448388));
#57506=CARTESIAN_POINT('Ctrl Pts',(56.7016707921346,30.7651900400527,21.5750520828532));
#57507=CARTESIAN_POINT('Ctrl Pts',(56.6412094749597,30.819720228305,21.5792711208676));
#57508=CARTESIAN_POINT('Ctrl Pts',(56.5807679022313,30.8742326089998,21.5834887810992));
#57509=CARTESIAN_POINT('Ctrl Pts',(56.5175854636253,30.925750305101,21.5877064413307));
#57510=CARTESIAN_POINT('Ctrl Pts',(56.4519957060219,30.9739956230179,21.5919241015622));
#57511=CARTESIAN_POINT('Ctrl Pts',(56.386407313295,31.0222399369839,21.5961416740272));
#57512=CARTESIAN_POINT('Ctrl Pts',(56.3184120760833,31.067211733845,21.6003592464922));
#57513=CARTESIAN_POINT('Ctrl Pts',(56.2483744009694,31.108675319959,21.6045768189572));
#57514=CARTESIAN_POINT('Ctrl Pts',(56.1782178261752,31.1502092968609,21.6088015513974));
#57515=CARTESIAN_POINT('Ctrl Pts',(56.1060122779705,31.1882229090948,21.6130262838376));
#57516=CARTESIAN_POINT('Ctrl Pts',(56.0321491596884,31.2225252219389,21.6172510162778));
#57517=CARTESIAN_POINT('Ctrl Pts',(55.9583044965698,31.2568189641349,21.6214746931421));
#57518=CARTESIAN_POINT('Ctrl Pts',(55.8828035316091,31.2874031059727,21.6256983700064));
#57519=CARTESIAN_POINT('Ctrl Pts',(55.8060561151941,31.3141356462313,21.6299220468707));
#57520=CARTESIAN_POINT('Ctrl Pts',(55.7291694519662,31.3409166887223,21.6341533869707));
#57521=CARTESIAN_POINT('Ctrl Pts',(55.6510322648193,31.3638320329228,21.6383847270707));
#57522=CARTESIAN_POINT('Ctrl Pts',(55.5720687308181,31.3827898810471,21.6426160671707));
#57523=CARTESIAN_POINT('Ctrl Pts',(55.4933321169684,31.4016932493684,21.646835247527));
#57524=CARTESIAN_POINT('Ctrl Pts',(55.4137743621044,31.4166618343841,21.6510544278833));
#57525=CARTESIAN_POINT('Ctrl Pts',(55.3338211098633,31.4276560128259,21.6552736082396));
#57526=CARTESIAN_POINT('Ctrl Pts',(55.2536132871638,31.438685196636,21.6595062224294));
#57527=CARTESIAN_POINT('Ctrl Pts',(55.1727091253607,31.4457556181,21.6637388366191));
#57528=CARTESIAN_POINT('Ctrl Pts',(55.0915332135982,31.4487898890694,21.6679714508089));
#57529=CARTESIAN_POINT('Ctrl Pts',(55.0104730916868,31.4518198319348,21.6721980275701));
#57530=CARTESIAN_POINT('Ctrl Pts',(54.929142450058,31.4508250416212,21.6764246043314));
#57531=CARTESIAN_POINT('Ctrl Pts',(54.8479730533334,31.4457796420543,21.6806511810926));
#57532=CARTESIAN_POINT('Ctrl Pts',(54.7668937456387,31.4407398423214,21.6848730668223));
#57533=CARTESIAN_POINT('Ctrl Pts',(54.6859757885639,31.4316583950109,21.689094952552));
#57534=CARTESIAN_POINT('Ctrl Pts',(54.6056515956935,31.418561470383,21.6933168382817));
#57535=CARTESIAN_POINT('Ctrl Pts',(54.5253815786919,31.4054733791742,21.6975358764966));
#57536=CARTESIAN_POINT('Ctrl Pts',(54.4457049878306,31.3883752641321,21.7017549147115));
#57537=CARTESIAN_POINT('Ctrl Pts',(54.3670484975769,31.3673450626346,21.7059739529264));
#57538=CARTESIAN_POINT('Ctrl Pts',(54.2884176936976,31.3463217288428,21.7101916133555));
#57539=CARTESIAN_POINT('Ctrl Pts',(54.2108067772946,31.3213689785938,21.7144092737846));
#57540=CARTESIAN_POINT('Ctrl Pts',(54.1346302679803,31.2926154228095,21.7186269342137));
#57541=CARTESIAN_POINT('Ctrl Pts',(54.0584553439017,31.2638624653878,21.7228445068731));
#57542=CARTESIAN_POINT('Ctrl Pts',(53.9837152017648,31.2313090248411,21.7270620795326));
#57543=CARTESIAN_POINT('Ctrl Pts',(53.9108059306148,31.1951324627949,21.731279652192));
#57544=CARTESIAN_POINT('Ctrl Pts',(53.8377728923112,31.1588944892158,21.7355043843931));
#57545=CARTESIAN_POINT('Ctrl Pts',(53.7665773616964,31.11902129613,21.7397291165942));
#57546=CARTESIAN_POINT('Ctrl Pts',(53.6975925798467,31.0757372574412,21.7439538487953));
#57547=CARTESIAN_POINT('Ctrl Pts',(53.6286250273542,31.0324640291971,21.7481775258445));
#57548=CARTESIAN_POINT('Ctrl Pts',(53.5618674893088,30.9857819434466,21.7524012028938));
#57549=CARTESIAN_POINT('Ctrl Pts',(53.4976622028408,30.9359574874534,21.756624879943));
#57550=CARTESIAN_POINT('Ctrl Pts',(53.4333404255097,30.8860426324572,21.7608562202208));
#57551=CARTESIAN_POINT('Ctrl Pts',(53.3715805073717,30.8329743168813,21.7650875604986));
#57552=CARTESIAN_POINT('Ctrl Pts',(53.3126903731069,30.7770583763607,21.7693189007764));
#57553=CARTESIAN_POINT('Ctrl Pts',(53.2539694908919,30.7213031399661,21.7735380800526));
#57554=CARTESIAN_POINT('Ctrl Pts',(53.1981021728646,30.6627170119578,21.7777572593289));
#57555=CARTESIAN_POINT('Ctrl Pts',(53.1453533765797,30.6016354617189,21.7819764386051));
#57556=CARTESIAN_POINT('Ctrl Pts',(53.0928691983639,30.540860331399,21.7861744520699));
#57557=CARTESIAN_POINT('Ctrl Pts',(53.0432691804079,30.4773793757769,21.7903724655347));
#57558=CARTESIAN_POINT('Ctrl Pts',(52.9968478027444,30.41149974305,21.7945704789996));
#57559=CARTESIAN_POINT('Ctrl Pts',(52.9504882732555,30.3457078831388,21.7987628993631));
#57560=CARTESIAN_POINT('Ctrl Pts',(52.9072992512303,30.2775240690775,21.8029553197265));
#57561=CARTESIAN_POINT('Ctrl Pts',(52.8675363449773,30.2072899444654,21.80714774009));
#57562=CARTESIAN_POINT('Ctrl Pts',(52.8278137653434,30.1371270496766,21.8113359085978));
#57563=CARTESIAN_POINT('Ctrl Pts',(52.7915106365121,30.0649183802912,21.8155240771056));
#57564=CARTESIAN_POINT('Ctrl Pts',(52.7588395490466,29.9910348546253,21.8197122456134));
#57565=CARTESIAN_POINT('Ctrl Pts',(52.7261912053985,29.917202762614,21.8238974985482));
#57566=CARTESIAN_POINT('Ctrl Pts',(52.6971700725693,29.8416985607465,21.828082751483));
#57567=CARTESIAN_POINT('Ctrl Pts',(52.6719422981615,29.7649167189378,21.8322680044178));
#57568=CARTESIAN_POINT('Ctrl Pts',(52.6467190670668,29.6881487049025,21.8364525036233));
#57569=CARTESIAN_POINT('Ctrl Pts',(52.6252879935756,29.6101039537651,21.8406370028287));
#57570=CARTESIAN_POINT('Ctrl Pts',(52.6077662033998,29.5311946087863,21.8448215020342));
#57571=CARTESIAN_POINT('Ctrl Pts',(52.5902459033006,29.4522919743648,21.8490056453841));
#57572=CARTESIAN_POINT('Ctrl Pts',(52.5766343209221,29.3725253552373,21.8531897887341));
#57573=CARTESIAN_POINT('Ctrl Pts',(52.5669976351947,29.2923178798019,21.8573739320841));
#57574=CARTESIAN_POINT('Ctrl Pts',(52.5573558623475,29.2120680635605,21.8615602842058));
#57575=CARTESIAN_POINT('Ctrl Pts',(52.5516932194495,29.1313773970183,21.8657466363275));
#57576=CARTESIAN_POINT('Ctrl Pts',(52.5500239961797,29.0506737674197,21.8699329884492));
#57577=CARTESIAN_POINT('Ctrl Pts',(52.5496598873948,29.0330698308851,21.8708461602288));
#57578=CARTESIAN_POINT('Ctrl Pts',(52.5494855924957,29.0154652775853,21.8717593320084));
#57579=CARTESIAN_POINT('Ctrl Pts',(52.5495009304611,28.9978645400587,21.872672503788));
#57580=CARTESIAN_POINT('',(52.5491321430934,29.0004423866234,22.672672503788));
#57581=CARTESIAN_POINT('Ctrl Pts',(52.5506947500799,28.9978548628947,21.8726730601105));
#57582=CARTESIAN_POINT('Ctrl Pts',(52.548747042966,28.7666343434887,21.8846751297305));
#57583=CARTESIAN_POINT('Ctrl Pts',(52.6846919919135,27.7240147216207,21.9389114761391));
#57584=CARTESIAN_POINT('Ctrl Pts',(54.1644763874256,26.2292359076652,22.0353820993358));
#57585=CARTESIAN_POINT('Ctrl Pts',(56.869326740188,26.7907356786193,22.1620849297015));
#57586=CARTESIAN_POINT('Ctrl Pts',(57.870850319864,29.365312819345,22.2887877600669));
#57587=CARTESIAN_POINT('Ctrl Pts',(56.2564582705911,31.6070189140945,22.4154905904323));
#57588=CARTESIAN_POINT('Ctrl Pts',(53.4971863067911,31.4732108227925,22.5421934207978));
#57589=CARTESIAN_POINT('Ctrl Pts',(52.5567672100938,29.8579006357823,22.6279207252497));
#57590=CARTESIAN_POINT('Ctrl Pts',(52.5455403995099,29.0245626904411,22.6714137529131));
#57591=CARTESIAN_POINT('Ctrl Pts',(52.5456007000401,29.000443024056,22.672672503788));
#57592=CARTESIAN_POINT('',(52.5495006321937,29.0017602218196,23.4726725037595));
#57593=CARTESIAN_POINT('Ctrl Pts',(52.5495000399198,29.0004423202172,22.672672503788));
#57594=CARTESIAN_POINT('Ctrl Pts',(52.5494854961293,28.919868209688,22.6768841776903));
#57595=CARTESIAN_POINT('Ctrl Pts',(52.5534492292258,28.8391374882827,22.6810958515925));
#57596=CARTESIAN_POINT('Ctrl Pts',(52.5614115129766,28.7586777238696,22.6853075254948));
#57597=CARTESIAN_POINT('Ctrl Pts',(52.569362527487,28.6783318363859,22.6895132384985));
#57598=CARTESIAN_POINT('Ctrl Pts',(52.5813008096307,28.5982566078266,22.6937189515022));
#57599=CARTESIAN_POINT('Ctrl Pts',(52.597194621011,28.5188798895268,22.6979246645059));
#57600=CARTESIAN_POINT('Ctrl Pts',(52.6130706107374,28.4395921759584,22.7021256616639));
#57601=CARTESIAN_POINT('Ctrl Pts',(52.6328932252952,28.3610018745935,22.706326658822));
#57602=CARTESIAN_POINT('Ctrl Pts',(52.6565790673927,28.2835304733502,22.71052765598));
#57603=CARTESIAN_POINT('Ctrl Pts',(52.6802505614431,28.206106001547,22.7147261083222));
#57604=CARTESIAN_POINT('Ctrl Pts',(52.7077805016829,28.1297995327349,22.7189245606644));
#57605=CARTESIAN_POINT('Ctrl Pts',(52.7390349626928,28.0550199208054,22.7231230130067));
#57606=CARTESIAN_POINT('Ctrl Pts',(52.7702802942635,27.9802621520272,22.7273202389795));
#57607=CARTESIAN_POINT('Ctrl Pts',(52.8052478053248,27.9070307876049,22.7315174649523));
#57608=CARTESIAN_POINT('Ctrl Pts',(52.8437550311147,27.8357157202139,22.7357146909251));
#57609=CARTESIAN_POINT('Ctrl Pts',(52.8822630871812,27.7643991151575,22.7399120073967));
#57610=CARTESIAN_POINT('Ctrl Pts',(52.9243107847905,27.6949993015931,22.7441093238684));
#57611=CARTESIAN_POINT('Ctrl Pts',(52.9696699184124,27.6278811969073,22.74830664034));
#57612=CARTESIAN_POINT('Ctrl Pts',(53.0150744453103,27.5606959235962,22.7525081572875));
#57613=CARTESIAN_POINT('Ctrl Pts',(53.0637967619506,27.495797308667,22.756709674235));
#57614=CARTESIAN_POINT('Ctrl Pts',(53.1155659285187,27.4335203543486,22.7609111911824));
#57615=CARTESIAN_POINT('Ctrl Pts',(53.1673618396172,27.371211227059,22.7651148786806));
#57616=CARTESIAN_POINT('Ctrl Pts',(53.2222074163188,27.311526802737,22.7693185661787));
#57617=CARTESIAN_POINT('Ctrl Pts',(53.2797938234318,27.2547662162058,22.7735222536768));
#57618=CARTESIAN_POINT('Ctrl Pts',(53.3374798801209,27.1979074091279,22.777733215386));
#57619=CARTESIAN_POINT('Ctrl Pts',(53.3979158884207,27.1439828571651,22.7819441770951));
#57620=CARTESIAN_POINT('Ctrl Pts',(53.460759110503,27.0932520528133,22.7861551388043));
#57621=CARTESIAN_POINT('Ctrl Pts',(53.5077387025736,27.0553273186115,22.7893031197124));
#57622=CARTESIAN_POINT('Ctrl Pts',(53.5560628805733,27.01918660076,22.7924511006206));
#57623=CARTESIAN_POINT('Ctrl Pts',(53.605578671413,26.9849219845421,22.7955990815287));
#57624=CARTESIAN_POINT('Ctrl Pts',(53.6721564963022,26.9388505479405,22.7998317862498));
#57625=CARTESIAN_POINT('Ctrl Pts',(53.7411438564632,26.8959965689133,22.8040644909709));
#57626=CARTESIAN_POINT('Ctrl Pts',(53.8121968913307,26.8566208863023,22.808297195692));
#57627=CARTESIAN_POINT('Ctrl Pts',(53.8831485682075,26.8173013735661,22.81252386241));
#57628=CARTESIAN_POINT('Ctrl Pts',(53.9561596643074,26.781450525695,22.816750529128));
#57629=CARTESIAN_POINT('Ctrl Pts',(54.0308566493132,26.7492864651805,22.820977195846));
#57630=CARTESIAN_POINT('Ctrl Pts',(54.1054687422099,26.717158958684,22.8251990590147));
#57631=CARTESIAN_POINT('Ctrl Pts',(54.1817624918819,26.6887100955654,22.8294209221834));
#57632=CARTESIAN_POINT('Ctrl Pts',(54.2593403113337,26.6641118443759,22.8336427853521));
#57633=CARTESIAN_POINT('Ctrl Pts',(54.3368678372452,26.639529540182,22.8378619114955));
#57634=CARTESIAN_POINT('Ctrl Pts',(54.4156773384656,26.6187930314796,22.842081037639));
#57635=CARTESIAN_POINT('Ctrl Pts',(54.4953529332376,26.602025523904,22.8463001637825));
#57636=CARTESIAN_POINT('Ctrl Pts',(54.5750024913493,26.5852634956711,22.8505179111857));
#57637=CARTESIAN_POINT('Ctrl Pts',(54.6555171267196,26.5724679883814,22.8547356585889));
#57638=CARTESIAN_POINT('Ctrl Pts',(54.736468911574,26.563711508168,22.8589534059921));
#57639=CARTESIAN_POINT('Ctrl Pts',(54.8174189913709,26.5549552123892,22.8631710645584));
#57640=CARTESIAN_POINT('Ctrl Pts',(54.8988057403859,26.5502378233306,22.8673887231247));
#57641=CARTESIAN_POINT('Ctrl Pts',(54.9801956520729,26.5495800282802,22.871606381691));
#57642=CARTESIAN_POINT('Ctrl Pts',(55.0617200464984,26.5489211463374,22.875831009208));
#57643=CARTESIAN_POINT('Ctrl Pts',(55.1432471471763,26.5523352820255,22.8800556367249));
#57644=CARTESIAN_POINT('Ctrl Pts',(55.2243426530845,26.5597908646989,22.8842802642418));
#57645=CARTESIAN_POINT('Ctrl Pts',(55.3054214966236,26.5672449155036,22.8885040237414));
#57646=CARTESIAN_POINT('Ctrl Pts',(55.3860684642249,26.5787386663093,22.8927277832411));
#57647=CARTESIAN_POINT('Ctrl Pts',(55.4658578327119,26.5941889663357,22.8969515427407));
#57648=CARTESIAN_POINT('Ctrl Pts',(55.5457919129972,26.6096672881492,22.9011829627575));
#57649=CARTESIAN_POINT('Ctrl Pts',(55.6248648333497,26.6291163886836,22.9054143827744));
#57650=CARTESIAN_POINT('Ctrl Pts',(55.7026637074587,26.6524025123074,22.9096458027913));
#57651=CARTESIAN_POINT('Ctrl Pts',(55.7802287671693,26.6756186525151,22.9138645058256));
#57652=CARTESIAN_POINT('Ctrl Pts',(55.8565270271489,26.7026485535667,22.9180832088599));
#57653=CARTESIAN_POINT('Ctrl Pts',(55.931170698421,26.7333126857897,22.9223019118942));
#57654=CARTESIAN_POINT('Ctrl Pts',(56.0060634968536,26.7640791611592,22.9265346950707));
#57655=CARTESIAN_POINT('Ctrl Pts',(56.0795690231587,26.7986185579771,22.9307674782472));
#57656=CARTESIAN_POINT('Ctrl Pts',(56.1512812722436,26.8367844115343,22.9350002614237));
#57657=CARTESIAN_POINT('Ctrl Pts',(56.2228912622086,26.8748958419399,22.9392270088018));
#57658=CARTESIAN_POINT('Ctrl Pts',(56.2927126471501,26.9166232419716,22.9434537561799));
#57659=CARTESIAN_POINT('Ctrl Pts',(56.3603591041834,26.961772005475,22.947680503558));
#57660=CARTESIAN_POINT('Ctrl Pts',(56.427927663553,27.0068687783296,22.9519023836634));
#57661=CARTESIAN_POINT('Ctrl Pts',(56.493325888301,27.055378827783,22.9561242637689));
#57662=CARTESIAN_POINT('Ctrl Pts',(56.5561930932482,27.1070622549786,22.9603461438744));
#57663=CARTESIAN_POINT('Ctrl Pts',(56.6190205601834,27.1587130133662,22.9645653553529));
#57664=CARTESIAN_POINT('Ctrl Pts',(56.679319825331,27.2135328734199,22.9687845668314));
#57665=CARTESIAN_POINT('Ctrl Pts',(56.7367611320787,27.2712400339837,22.9730037783098));
#57666=CARTESIAN_POINT('Ctrl Pts',(56.7941836897897,27.3289283587352,22.9772216126234));
#57667=CARTESIAN_POINT('Ctrl Pts',(56.8487498142394,27.3895017834338,22.981439446937));
#57668=CARTESIAN_POINT('Ctrl Pts',(56.9001657205332,27.4526408030097,22.9856572812506));
#57669=CARTESIAN_POINT('Ctrl Pts',(56.9515805615183,27.5157785143805,22.989875028173));
#57670=CARTESIAN_POINT('Ctrl Pts',(56.9998450217247,27.5814813540094,22.9940927750954));
#57671=CARTESIAN_POINT('Ctrl Pts',(57.0447057472779,27.6493969283876,22.9983105220178));
#57672=CARTESIAN_POINT('Ctrl Pts',(57.0896384950068,27.7174215386179,23.0025350403713));
#57673=CARTESIAN_POINT('Ctrl Pts',(57.1311563189547,27.7876656008117,23.0067595587248));
#57674=CARTESIAN_POINT('Ctrl Pts',(57.1690492973634,27.859747661433,23.0109840770783));
#57675=CARTESIAN_POINT('Ctrl Pts',(57.2069362845994,27.9318183253237,23.0152079275028));
#57676=CARTESIAN_POINT('Ctrl Pts',(57.2411993949561,28.0057259750564,23.0194317779273));
#57677=CARTESIAN_POINT('Ctrl Pts',(57.2716766127879,28.0810682196636,23.0236556283517));
#57678=CARTESIAN_POINT('Ctrl Pts',(57.3022091107209,28.1565471213279,23.0278871400687));
#57679=CARTESIAN_POINT('Ctrl Pts',(57.3289418398862,28.2334653780283,23.0321186517856));
#57680=CARTESIAN_POINT('Ctrl Pts',(57.3517622218452,28.3114038179733,23.0363501635025));
#57681=CARTESIAN_POINT('Ctrl Pts',(57.374510776033,28.3890969445644,23.0405683564215));
#57682=CARTESIAN_POINT('Ctrl Pts',(57.3933715521117,28.4678033798409,23.0447865493405));
#57683=CARTESIAN_POINT('Ctrl Pts',(57.4082840533503,28.5471002667491,23.0490047422596));
#57684=CARTESIAN_POINT('Ctrl Pts',(57.4232450343868,28.6266549438826,23.0532366483134));
#57685=CARTESIAN_POINT('Ctrl Pts',(57.4342876721786,28.707099976781,23.0574685543673));
#57686=CARTESIAN_POINT('Ctrl Pts',(57.4413137261738,28.7880152354636,23.0617004604211));
#57687=CARTESIAN_POINT('Ctrl Pts',(57.4483297544047,28.868815032849,23.0659263277949));
#57688=CARTESIAN_POINT('Ctrl Pts',(57.4513405422157,28.9500832642489,23.0701521951687));
#57689=CARTESIAN_POINT('Ctrl Pts',(57.4502989434788,29.0313900873962,23.0743780625424));
#57690=CARTESIAN_POINT('Ctrl Pts',(57.4492582824699,29.1126237118335,23.0786001254625));
#57691=CARTESIAN_POINT('Ctrl Pts',(57.4441724786708,29.1938953965611,23.0828221883826));
#57692=CARTESIAN_POINT('Ctrl Pts',(57.4350463452106,29.2747718083732,23.0870442513027));
#57693=CARTESIAN_POINT('Ctrl Pts',(57.4259282784988,29.3555767321143,23.0912625822678));
#57694=CARTESIAN_POINT('Ctrl Pts',(57.412777039292,29.4359866172132,23.0954809132328));
#57695=CARTESIAN_POINT('Ctrl Pts',(57.3956494303402,29.5155715827224,23.0996992441979));
#57696=CARTESIAN_POINT('Ctrl Pts',(57.378527405954,29.5951305990483,23.1039161997494));
#57697=CARTESIAN_POINT('Ctrl Pts',(57.3574316843034,29.6738647759658,23.1081331553008));
#57698=CARTESIAN_POINT('Ctrl Pts',(57.332470278992,29.751353876425,23.1123501108523));
#57699=CARTESIAN_POINT('Ctrl Pts',(57.3075093735703,29.8288414250484,23.1165669819529));
#57700=CARTESIAN_POINT('Ctrl Pts',(57.2786830820212,29.9050835048136,23.1207838530535));
#57701=CARTESIAN_POINT('Ctrl Pts',(57.2461490167081,29.9796758875982,23.1250007241541));
#57702=CARTESIAN_POINT('Ctrl Pts',(57.2135478320734,30.0544221580103,23.12922629486));
#57703=CARTESIAN_POINT('Ctrl Pts',(57.1772237493577,30.1275114901386,23.1334518655659));
#57704=CARTESIAN_POINT('Ctrl Pts',(57.137382692401,30.1985597507946,23.1376774362718));
#57705=CARTESIAN_POINT('Ctrl Pts',(57.0975659613505,30.2695646312428,23.1419004269549));
#57706=CARTESIAN_POINT('Ctrl Pts',(57.0542368184479,30.3385305499311,23.146123417638));
#57707=CARTESIAN_POINT('Ctrl Pts',(57.0076445567346,30.4051026951131,23.150346408321));
#57708=CARTESIAN_POINT('Ctrl Pts',(56.9609675864406,30.4717958739544,23.15457707675));
#57709=CARTESIAN_POINT('Ctrl Pts',(56.911015927208,30.5360862138174,23.158807745179));
#57710=CARTESIAN_POINT('Ctrl Pts',(56.8580798572149,30.5976512429852,23.1630384136079));
#57711=CARTESIAN_POINT('Ctrl Pts',(56.8052390749021,30.6591054518972,23.1672614666136));
#57712=CARTESIAN_POINT('Ctrl Pts',(56.749424987471,30.7178438735892,23.1714845196193));
#57713=CARTESIAN_POINT('Ctrl Pts',(56.6909606339623,30.7735846143869,23.175707572625));
#57714=CARTESIAN_POINT('Ctrl Pts',(56.6323519679936,30.8294629447232,23.1799410497461));
#57715=CARTESIAN_POINT('Ctrl Pts',(56.5708617343952,30.8825367923476,23.1841745268672));
#57716=CARTESIAN_POINT('Ctrl Pts',(56.5067891491679,30.932494944353,23.1884080039883));
#57717=CARTESIAN_POINT('Ctrl Pts',(56.4428079928384,30.9823818081662,23.1926354401147));
#57718=CARTESIAN_POINT('Ctrl Pts',(56.3762521668127,31.0291615235634,23.1968628762411));
#57719=CARTESIAN_POINT('Ctrl Pts',(56.3074568365328,31.0725604624724,23.2010903123675));
#57720=CARTESIAN_POINT('Ctrl Pts',(56.2387408920317,31.1159093215496,23.2053128702804));
#57721=CARTESIAN_POINT('Ctrl Pts',(56.1677909702052,31.1558849113241,23.2095354281933));
#57722=CARTESIAN_POINT('Ctrl Pts',(56.0949731587571,31.1922554667742,23.2137579861062));
#57723=CARTESIAN_POINT('Ctrl Pts',(56.0222014869416,31.228602976708,23.217977868475));
#57724=CARTESIAN_POINT('Ctrl Pts',(55.9475646893086,31.2613497799502,23.2221977508437));
#57725=CARTESIAN_POINT('Ctrl Pts',(55.8714545274654,31.2903094237592,23.2264176332125));
#57726=CARTESIAN_POINT('Ctrl Pts',(55.7953693443882,31.3192595632372,23.2306361306485));
#57727=CARTESIAN_POINT('Ctrl Pts',(55.7178121910653,31.3444248466661,23.2348546280845));
#57728=CARTESIAN_POINT('Ctrl Pts',(55.6391946167058,31.3656670289739,23.2390731255206));
#57729=CARTESIAN_POINT('Ctrl Pts',(55.5605788317492,31.3869087277916,23.24329152694));
#57730=CARTESIAN_POINT('Ctrl Pts',(55.4809031223186,31.4042273830283,23.2475099283594));
#57731=CARTESIAN_POINT('Ctrl Pts',(55.4005926132802,31.4175350686568,23.2517283297788));
#57732=CARTESIAN_POINT('Ctrl Pts',(55.3201849206094,31.4308588578967,23.2559518358798));
#57733=CARTESIAN_POINT('Ctrl Pts',(55.239141352318,31.4401618984881,23.2601753419808));
#57734=CARTESIAN_POINT('Ctrl Pts',(55.1578953815873,31.4454077979906,23.2643988480818));
#57735=CARTESIAN_POINT('Ctrl Pts',(55.0766307334054,31.4506549034611,23.2686233251149));
#57736=CARTESIAN_POINT('Ctrl Pts',(54.9951640556022,31.4518430123114,23.2728478021481));
#57737=CARTESIAN_POINT('Ctrl Pts',(54.9139289520395,31.4489879592809,23.2770722791813));
#57738=CARTESIAN_POINT('Ctrl Pts',(54.8325469465271,31.4461277432995,23.2813043955709));
#57739=CARTESIAN_POINT('Ctrl Pts',(54.7513978161741,31.4392097931619,23.2855365119605));
#57740=CARTESIAN_POINT('Ctrl Pts',(54.6709103675634,31.4283019301196,23.2897686283501));
#57741=CARTESIAN_POINT('Ctrl Pts',(54.590768889633,31.4174409539009,23.2939825532303));
#57742=CARTESIAN_POINT('Ctrl Pts',(54.5112838436527,31.4026244700762,23.2981964781104));
#57743=CARTESIAN_POINT('Ctrl Pts',(54.4328647967604,31.3839689409148,23.3024104029905));
#57744=CARTESIAN_POINT('Ctrl Pts',(54.3540815518368,31.3652267707234,23.3066438984113));
#57745=CARTESIAN_POINT('Ctrl Pts',(54.2760824579198,31.3425403614949,23.3108773938321));
#57746=CARTESIAN_POINT('Ctrl Pts',(54.1992914755943,31.3159913879253,23.3151108892528));
#57747=CARTESIAN_POINT('Ctrl Pts',(54.1226097793403,31.2894801978679,23.3193383597203));
#57748=CARTESIAN_POINT('Ctrl Pts',(54.0471332150036,31.2591175119583,23.3235658301878));
#57749=CARTESIAN_POINT('Ctrl Pts',(53.9732737720535,31.2250356183322,23.3277933006553));
#57750=CARTESIAN_POINT('Ctrl Pts',(53.8994991426381,31.1909928612843,23.3320159166763));
#57751=CARTESIAN_POINT('Ctrl Pts',(53.8273383633754,31.1532395782488,23.3362385326972));
#57752=CARTESIAN_POINT('Ctrl Pts',(53.7571851303894,31.1119567821986,23.3404611487182));
#57753=CARTESIAN_POINT('Ctrl Pts',(53.6870761096498,31.0707000035546,23.3446811035455));
#57754=CARTESIAN_POINT('Ctrl Pts',(53.6189725226876,31.0259183624577,23.3489010583729));
#57755=CARTESIAN_POINT('Ctrl Pts',(53.5532440202676,30.9778390695678,23.3531210132002));
#57756=CARTESIAN_POINT('Ctrl Pts',(53.4875368691057,30.9297753947636,23.3573395972166));
#57757=CARTESIAN_POINT('Ctrl Pts',(53.4242036447361,30.8784164694774,23.3615581812331));
#57758=CARTESIAN_POINT('Ctrl Pts',(53.3635843207133,30.8240323392376,23.3657767652496));
#57759=CARTESIAN_POINT('Ctrl Pts',(53.3029661765759,30.7696492675224,23.3699952671561));
#57760=CARTESIAN_POINT('Ctrl Pts',(53.2450621725797,30.7122414188741,23.3742137690627));
#57761=CARTESIAN_POINT('Ctrl Pts',(53.190177453739,30.6521176111419,23.3784322709693));
#57762=CARTESIAN_POINT('Ctrl Pts',(53.1352288323094,30.5919238009201,23.3826556845015));
#57763=CARTESIAN_POINT('Ctrl Pts',(53.0833068366663,30.5290080549053,23.3868790980337));
#57764=CARTESIAN_POINT('Ctrl Pts',(53.0346778820942,30.463714187562,23.391102511566));
#57765=CARTESIAN_POINT('Ctrl Pts',(52.9860351509877,30.3984018225311,23.3953271215871));
#57766=CARTESIAN_POINT('Ctrl Pts',(52.9406875724281,30.3307103846163,23.3995517316081));
#57767=CARTESIAN_POINT('Ctrl Pts',(52.8988578576523,30.2610122710151,23.4037763416292));
#57768=CARTESIAN_POINT('Ctrl Pts',(52.8569523224409,30.1911878227886,23.4080086091678));
#57769=CARTESIAN_POINT('Ctrl Pts',(52.8185776136158,30.1193498405798,23.4122408767063));
#57770=CARTESIAN_POINT('Ctrl Pts',(52.7839102182845,30.0458949896506,23.4164731442449));
#57771=CARTESIAN_POINT('Ctrl Pts',(52.7493976737093,29.9727682435327,23.4206865072819));
#57772=CARTESIAN_POINT('Ctrl Pts',(52.7185594783011,29.8980394955953,23.424899870319));
#57773=CARTESIAN_POINT('Ctrl Pts',(52.6915207808602,29.8221155300805,23.429113233356));
#57774=CARTESIAN_POINT('Ctrl Pts',(52.6599923408405,29.7335844831239,23.4340262201626));
#57775=CARTESIAN_POINT('Ctrl Pts',(52.6335319134128,29.6431573818611,23.4389392069691));
#57776=CARTESIAN_POINT('Ctrl Pts',(52.6123377738553,29.5513794916768,23.4438521937757));
#57777=CARTESIAN_POINT('Ctrl Pts',(52.5913329406732,29.460421362997,23.4487212977097));
#57778=CARTESIAN_POINT('Ctrl Pts',(52.575500818871,29.3681366175074,23.4535904016438));
#57779=CARTESIAN_POINT('Ctrl Pts',(52.5649881187031,29.2750770581904,23.4584595055778));
#57780=CARTESIAN_POINT('Ctrl Pts',(52.5547592011312,29.1845295731178,23.4631971716384));
#57781=CARTESIAN_POINT('Ctrl Pts',(52.5495663494456,29.0932487390193,23.4679348376989));
#57782=CARTESIAN_POINT('Ctrl Pts',(52.5495006321937,29.0017602218196,23.4726725037595));
#57783=CARTESIAN_POINT('',(57.0573849385052,27.6687909762881,23.799499905797));
#57784=CARTESIAN_POINT('Ctrl Pts',(52.5495006321933,29.001760221269,23.472672503788));
#57785=CARTESIAN_POINT('Ctrl Pts',(52.5494421473559,28.92034031141,23.4768887743692));
#57786=CARTESIAN_POINT('Ctrl Pts',(52.5534458492211,28.8388797722771,23.4811050449504));
#57787=CARTESIAN_POINT('Ctrl Pts',(52.5614972674082,28.7578127312551,23.4853213155316));
#57788=CARTESIAN_POINT('Ctrl Pts',(52.5695478980543,28.6767536197193,23.4895371737028));
#57789=CARTESIAN_POINT('Ctrl Pts',(52.5816454122911,28.5960883915437,23.493753031874));
#57790=CARTESIAN_POINT('Ctrl Pts',(52.5977234365795,28.5162463820906,23.4979688900453));
#57791=CARTESIAN_POINT('Ctrl Pts',(52.6138047898605,28.4363878411622,23.5021856211198));
#57792=CARTESIAN_POINT('Ctrl Pts',(52.6338681970555,28.3573533120643,23.5064023521943));
#57793=CARTESIAN_POINT('Ctrl Pts',(52.6577964014843,28.2795608609326,23.5106190832688));
#57794=CARTESIAN_POINT('Ctrl Pts',(52.6817534461576,28.2016746479262,23.5148408966953));
#57795=CARTESIAN_POINT('Ctrl Pts',(52.7095844488888,28.1250339452557,23.5190627101217));
#57796=CARTESIAN_POINT('Ctrl Pts',(52.741122754398,28.0500400854238,23.5232845235481));
#57797=CARTESIAN_POINT('Ctrl Pts',(52.7726819768628,27.9749964878775,23.5275091369818));
#57798=CARTESIAN_POINT('Ctrl Pts',(52.8079531945684,27.9016023248674,23.5317337504154));
#57799=CARTESIAN_POINT('Ctrl Pts',(52.8467233334473,27.830235131627,23.5359583638491));
#57800=CARTESIAN_POINT('Ctrl Pts',(52.885563189113,27.7587396053051,23.5401905740178));
#57801=CARTESIAN_POINT('Ctrl Pts',(52.9279142852273,27.6892787211411,23.5444227841866));
#57802=CARTESIAN_POINT('Ctrl Pts',(52.9735199245037,27.6222014829386,23.5486549943553));
#57803=CARTESIAN_POINT('Ctrl Pts',(52.9992421148269,27.5843690237346,23.5510420174773));
#57804=CARTESIAN_POINT('Ctrl Pts',(53.0259988654998,27.5472942432224,23.5534290405994));
#57805=CARTESIAN_POINT('Ctrl Pts',(53.0537387209796,27.5110348278802,23.5558160637214));
#57806=CARTESIAN_POINT('Ctrl Pts',(53.1030160851922,27.4466232300167,23.5600563961144));
#57807=CARTESIAN_POINT('Ctrl Pts',(53.1555846095254,27.3845426287641,23.5642967285075));
#57808=CARTESIAN_POINT('Ctrl Pts',(53.2111960290357,27.3251475875581,23.5685370609005));
#57809=CARTESIAN_POINT('Ctrl Pts',(53.2667279960875,27.2658374044997,23.5727713350983));
#57810=CARTESIAN_POINT('Ctrl Pts',(53.325293909279,27.2092054952295,23.5770056092962));
#57811=CARTESIAN_POINT('Ctrl Pts',(53.3866041889151,27.1555748302592,23.581239883494));
#57812=CARTESIAN_POINT('Ctrl Pts',(53.4478429967745,27.10200668464,23.5854692216338));
#57813=CARTESIAN_POINT('Ctrl Pts',(53.5118194654066,27.0514331320413,23.5896985597736));
#57814=CARTESIAN_POINT('Ctrl Pts',(53.5782070003551,27.0041405570129,23.5939278979134));
#57815=CARTESIAN_POINT('Ctrl Pts',(53.644551936521,26.956878328135,23.5981545222206));
#57816=CARTESIAN_POINT('Ctrl Pts',(53.7133044916079,26.9128931648167,23.6023811465278));
#57817=CARTESIAN_POINT('Ctrl Pts',(53.784105685571,26.872430667137,23.606607770835));
#57818=CARTESIAN_POINT('Ctrl Pts',(53.8548828865358,26.8319818813254,23.6108329628303));
#57819=CARTESIAN_POINT('Ctrl Pts',(53.9277069460756,26.7950536195464,23.6150581548256));
#57820=CARTESIAN_POINT('Ctrl Pts',(54.0021918461236,26.7618469359631,23.619283346821));
#57821=CARTESIAN_POINT('Ctrl Pts',(54.0766740573049,26.728641451124,23.623508386289));
#57822=CARTESIAN_POINT('Ctrl Pts',(54.1528165667252,26.6991574647628,23.6277334257571));
#57823=CARTESIAN_POINT('Ctrl Pts',(54.2302121063722,26.6735484426225,23.6319584652252));
#57824=CARTESIAN_POINT('Ctrl Pts',(54.30768071855,26.6479152418789,23.6361874937387));
#57825=CARTESIAN_POINT('Ctrl Pts',(54.3864042842766,26.6261644605585,23.6404165222523));
#57826=CARTESIAN_POINT('Ctrl Pts',(54.4659595540915,26.608399897112,23.6446455507658));
#57827=CARTESIAN_POINT('Ctrl Pts',(54.5455503242964,26.5906274064857,23.6488764664222));
#57828=CARTESIAN_POINT('Ctrl Pts',(54.6259730814925,26.576844757245,23.6531073820787));
#57829=CARTESIAN_POINT('Ctrl Pts',(54.7067959688153,26.5671042673191,23.6573382977351));
#57830=CARTESIAN_POINT('Ctrl Pts',(54.7877612686191,26.5573466143422,23.6615766683986));
#57831=CARTESIAN_POINT('Ctrl Pts',(54.8691276446669,26.5516453877608,23.6658150390621));
#57832=CARTESIAN_POINT('Ctrl Pts',(54.950459840218,26.5500008117208,23.6700534097256));
#57833=CARTESIAN_POINT('Ctrl Pts',(55.0301952929976,26.5483885225862,23.6742085711793));
#57834=CARTESIAN_POINT('Ctrl Pts',(55.1098974842549,26.5506749356976,23.678363732633));
#57835=CARTESIAN_POINT('Ctrl Pts',(55.1891616966146,26.5568118978405,23.6825188940868));
#57836=CARTESIAN_POINT('Ctrl Pts',(55.2690802523531,26.5629995219457,23.6867083573055));
#57837=CARTESIAN_POINT('Ctrl Pts',(55.3488563077395,26.5731252336513,23.6908978205242));
#57838=CARTESIAN_POINT('Ctrl Pts',(55.4280656812847,26.5871779960995,23.695087283743));
#57839=CARTESIAN_POINT('Ctrl Pts',(55.5103202362572,26.6017710129305,23.6994378096619));
#57840=CARTESIAN_POINT('Ctrl Pts',(55.5919631422334,26.6205992052271,23.7037883355808));
#57841=CARTESIAN_POINT('Ctrl Pts',(55.6725214939679,26.6435906361264,23.7081388614997));
#57842=CARTESIAN_POINT('Ctrl Pts',(55.7498998283755,26.6656744870287,23.7123176516829));
#57843=CARTESIAN_POINT('Ctrl Pts',(55.8262771079175,26.6915989493626,23.7164964418661));
#57844=CARTESIAN_POINT('Ctrl Pts',(55.901243442004,26.7212480371386,23.7206752320493));
#57845=CARTESIAN_POINT('Ctrl Pts',(55.9761666697665,26.7508800764194,23.7248516193902));
#57846=CARTESIAN_POINT('Ctrl Pts',(56.0496801212606,26.7842323172225,23.729028006731));
#57847=CARTESIAN_POINT('Ctrl Pts',(56.1213906170083,26.8211394413396,23.7332043940718));
#57848=CARTESIAN_POINT('Ctrl Pts',(56.1930829059465,26.8580371949878,23.7373797210562));
#57849=CARTESIAN_POINT('Ctrl Pts',(56.2629727261088,26.8984878223256,23.7415550480406));
#57850=CARTESIAN_POINT('Ctrl Pts',(56.3306898170856,26.9422792073013,23.7457303750249));
#57851=CARTESIAN_POINT('Ctrl Pts',(56.3984114598277,26.986073535819,23.7499059826638));
#57852=CARTESIAN_POINT('Ctrl Pts',(56.4639596861817,27.033208807563,23.7540815903027));
#57853=CARTESIAN_POINT('Ctrl Pts',(56.526992974048,27.0834294411089,23.7582571979416));
#57854=CARTESIAN_POINT('Ctrl Pts',(56.5900869053925,27.1336983912507,23.7624368228764));
#57855=CARTESIAN_POINT('Ctrl Pts',(56.6506606990727,27.1870583289571,23.7666164478112));
#57856=CARTESIAN_POINT('Ctrl Pts',(56.708406379522,27.2432137601835,23.7707960727461));
#57857=CARTESIAN_POINT('Ctrl Pts',(56.7661851835194,27.2994014027738,23.774978095159));
#57858=CARTESIAN_POINT('Ctrl Pts',(56.8211323240713,27.3583873813232,23.779160117572));
#57859=CARTESIAN_POINT('Ctrl Pts',(56.8729788290211,27.4198416041299,23.783342139985));
#57860=CARTESIAN_POINT('Ctrl Pts',(56.924903432116,27.4813883975123,23.7875304619199));
#57861=CARTESIAN_POINT('Ctrl Pts',(56.9737177969051,27.5454104741242,23.7917187838548));
#57862=CARTESIAN_POINT('Ctrl Pts',(57.0191955923614,27.6115478366943,23.7959071057896));
#57863=CARTESIAN_POINT('Ctrl Pts',(57.0321994179502,27.6304590156364,23.7971047057921));
#57864=CARTESIAN_POINT('Ctrl Pts',(57.0449307307273,27.6495429851411,23.7983023057946));
#57865=CARTESIAN_POINT('Ctrl Pts',(57.0573849385052,27.6687909762881,23.799499905797));
#57866=CARTESIAN_POINT('',(55.2147522011135,26.5589281571169,23.7995));
#57867=CARTESIAN_POINT('Origin',(55.,29.,23.7995));
#57868=CARTESIAN_POINT('',(52.5498441316087,29.0016533468466,23.5883274660079));
#57869=CARTESIAN_POINT('Ctrl Pts',(55.2147522011135,26.5589281571169,23.7995));
#57870=CARTESIAN_POINT('Ctrl Pts',(54.4050310115761,26.4876932984426,23.7572657232115));
#57871=CARTESIAN_POINT('Ctrl Pts',(53.003287825418,27.0942572053241,23.6868748886155));
#57872=CARTESIAN_POINT('Ctrl Pts',(52.5563761394599,28.4582876769929,23.6164840540196));
#57873=CARTESIAN_POINT('Ctrl Pts',(52.5520032102007,29.0016513069589,23.5883274962121));
#57874=CARTESIAN_POINT('',(52.5495000174313,29.0002922856895,22.7883274962497));
#57875=CARTESIAN_POINT('Ctrl Pts',(52.5495005579738,29.0016536714534,23.5883274612015));
#57876=CARTESIAN_POINT('Ctrl Pts',(52.5495642388273,29.0960193905902,23.5834424895806));
#57877=CARTESIAN_POINT('Ctrl Pts',(52.5550827318315,29.1901514168606,23.5785575179597));
#57878=CARTESIAN_POINT('Ctrl Pts',(52.5659516932184,29.2834767896203,23.5736725463388));
#57879=CARTESIAN_POINT('Ctrl Pts',(52.5769354492301,29.3777878362438,23.5687359811511));
#57880=CARTESIAN_POINT('Ctrl Pts',(52.5933831868479,29.4712749581831,23.5637994159634));
#57881=CARTESIAN_POINT('Ctrl Pts',(52.6151379068873,29.5633675947673,23.5588628507757));
#57882=CARTESIAN_POINT('Ctrl Pts',(52.6338942271615,29.6427673288729,23.5546066802735));
#57883=CARTESIAN_POINT('Ctrl Pts',(52.6565946040389,29.7211307824724,23.5503505097713));
#57884=CARTESIAN_POINT('Ctrl Pts',(52.68311033603,29.7981055913782,23.5460943392691));
#57885=CARTESIAN_POINT('Ctrl Pts',(52.7095081791768,29.874738170574,23.5418570916849));
#57886=CARTESIAN_POINT('Ctrl Pts',(52.7397606807718,29.95020067919,23.5376198441007));
#57887=CARTESIAN_POINT('Ctrl Pts',(52.7737445873222,30.0240786529964,23.5333825965165));
#57888=CARTESIAN_POINT('Ctrl Pts',(52.8076799722184,30.0978511450657,23.5291513988037));
#57889=CARTESIAN_POINT('Ctrl Pts',(52.8453359879674,30.1700431784693,23.5249202010908));
#57890=CARTESIAN_POINT('Ctrl Pts',(52.886540194497,30.2402571912806,23.520689003378));
#57891=CARTESIAN_POINT('Ctrl Pts',(52.9276965756498,30.3103897072764,23.5164627167808));
#57892=CARTESIAN_POINT('Ctrl Pts',(52.9723927284683,30.3785483684405,23.5122364301837));
#57893=CARTESIAN_POINT('Ctrl Pts',(53.0204095276617,30.444358616074,23.5080101435865));
#57894=CARTESIAN_POINT('Ctrl Pts',(53.0683956795213,30.5101268594786,23.5037865544706));
#57895=CARTESIAN_POINT('Ctrl Pts',(53.1196979977247,30.5735492917698,23.4995629653547));
#57896=CARTESIAN_POINT('Ctrl Pts',(53.1740537421329,30.6342798148974,23.4953393762388));
#57897=CARTESIAN_POINT('Ctrl Pts',(53.2283913086446,30.694990028246,23.4911171995949));
#57898=CARTESIAN_POINT('Ctrl Pts',(53.2857799645017,30.7530097754057,23.486895022951));
#57899=CARTESIAN_POINT('Ctrl Pts',(53.3459172452173,30.8080266840759,23.482672846307));
#57900=CARTESIAN_POINT('Ctrl Pts',(53.4060526859771,30.8630419094528,23.4784507988445));
#57901=CARTESIAN_POINT('Ctrl Pts',(53.4689362417597,30.9150541670806,23.474228751382));
#57902=CARTESIAN_POINT('Ctrl Pts',(53.5342302610026,30.9637895310444,23.4700067039195));
#57903=CARTESIAN_POINT('Ctrl Pts',(53.5995868324059,31.0125715838526,23.4657806117038));
#57904=CARTESIAN_POINT('Ctrl Pts',(53.6673581086993,31.0580701932019,23.4615545194881));
#57905=CARTESIAN_POINT('Ctrl Pts',(53.7371755937771,31.1000535157581,23.4573284272724));
#57906=CARTESIAN_POINT('Ctrl Pts',(53.8070246807587,31.1420558414754,23.4531004221755));
#57907=CARTESIAN_POINT('Ctrl Pts',(53.8789214131283,31.1805394904803,23.4488724170785));
#57908=CARTESIAN_POINT('Ctrl Pts',(53.9524728912223,31.2153187595414,23.4446444119816));
#57909=CARTESIAN_POINT('Ctrl Pts',(54.0261553873424,31.2501599812824,23.4404088754944));
#57910=CARTESIAN_POINT('Ctrl Pts',(54.1014980905841,31.2812834579993,23.4361733390072));
#57911=CARTESIAN_POINT('Ctrl Pts',(54.1780884412599,31.3085518490191,23.4319378025201));
#57912=CARTESIAN_POINT('Ctrl Pts',(54.2537124722551,31.3354762021454,23.427755704648));
#57913=CARTESIAN_POINT('Ctrl Pts',(54.330552406019,31.358642164411,23.4235736067758));
#57914=CARTESIAN_POINT('Ctrl Pts',(54.4082007613574,31.3779663393627,23.4193915089037));
#57915=CARTESIAN_POINT('Ctrl Pts',(54.4869164102734,31.3975561293133,23.4151519271843));
#57916=CARTESIAN_POINT('Ctrl Pts',(54.5667466705475,31.4132683160261,23.4109123454649));
#57917=CARTESIAN_POINT('Ctrl Pts',(54.6472759233404,31.424981644414,23.4066727637455));
#57918=CARTESIAN_POINT('Ctrl Pts',(54.7276931921117,31.4366786842411,23.4024390775907));
#57919=CARTESIAN_POINT('Ctrl Pts',(54.8088070682774,31.4443878454646,23.3982053914359));
#57920=CARTESIAN_POINT('Ctrl Pts',(54.8901894976013,31.4480383786949,23.3939717052811));
#57921=CARTESIAN_POINT('Ctrl Pts',(54.9714818060851,31.4516848694172,23.389742707403));
#57922=CARTESIAN_POINT('Ctrl Pts',(55.0530416165865,31.4512816445403,23.385513709525));
#57923=CARTESIAN_POINT('Ctrl Pts',(55.1344348921067,31.4468096594922,23.3812847116469));
#57924=CARTESIAN_POINT('Ctrl Pts',(55.2157788324529,31.4423403850631,23.3770582771053));
#57925=CARTESIAN_POINT('Ctrl Pts',(55.2969559773223,31.4338072720591,23.3728318425636));
#57926=CARTESIAN_POINT('Ctrl Pts',(55.3775325749835,31.4212433592736,23.368605408022));
#57927=CARTESIAN_POINT('Ctrl Pts',(55.4580847301207,31.4086832576907,23.3643802555489));
#57928=CARTESIAN_POINT('Ctrl Pts',(55.5380362429751,31.3920948561298,23.3601551030759));
#57929=CARTESIAN_POINT('Ctrl Pts',(55.6169601720937,31.3715628593925,23.3559299506029));
#57930=CARTESIAN_POINT('Ctrl Pts',(55.695884056456,31.3510308742986,23.3517048005259));
#57931=CARTESIAN_POINT('Ctrl Pts',(55.7737799107425,31.3265554162657,23.3474796504489));
#57932=CARTESIAN_POINT('Ctrl Pts',(55.8502340217815,31.298271602358,23.3432545003718));
#57933=CARTESIAN_POINT('Ctrl Pts',(55.9267645865935,31.2699595047615,23.3390251251634));
#57934=CARTESIAN_POINT('Ctrl Pts',(56.0018500929309,31.237831604185,23.334795749955));
#57935=CARTESIAN_POINT('Ctrl Pts',(56.075095441174,31.2020717614026,23.3305663747466));
#57936=CARTESIAN_POINT('Ctrl Pts',(56.1483757047791,31.1662948722427,23.3263349834352));
#57937=CARTESIAN_POINT('Ctrl Pts',(56.2198136567177,31.1268828150247,23.3221035921238));
#57938=CARTESIAN_POINT('Ctrl Pts',(56.2890397269056,31.0840649779839,23.3178722008124));
#57939=CARTESIAN_POINT('Ctrl Pts',(56.3583912791156,31.0411695275706,23.3136331395071));
#57940=CARTESIAN_POINT('Ctrl Pts',(56.4255225550726,30.9948562234326,23.3093940782018));
#57941=CARTESIAN_POINT('Ctrl Pts',(56.4900939366215,30.9453972113797,23.3051550168964));
#57942=CARTESIAN_POINT('Ctrl Pts',(56.5533916522134,30.896913774859,23.300999570777));
#57943=CARTESIAN_POINT('Ctrl Pts',(56.6142292897565,30.8454079401431,23.2968441246576));
#57944=CARTESIAN_POINT('Ctrl Pts',(56.6723214501742,30.7911703484837,23.2926886785382));
#57945=CARTESIAN_POINT('Ctrl Pts',(56.7314235911169,30.7359897911831,23.2884609865319));
#57946=CARTESIAN_POINT('Ctrl Pts',(56.7879040576757,30.6777759052241,23.2842332945255));
#57947=CARTESIAN_POINT('Ctrl Pts',(56.8414349319838,30.6168078553959,23.2800056025192));
#57948=CARTESIAN_POINT('Ctrl Pts',(56.8948884835476,30.5559278709502,23.2757840172083));
#57949=CARTESIAN_POINT('Ctrl Pts',(56.9454005994851,30.4923019703519,23.2715624318975));
#57950=CARTESIAN_POINT('Ctrl Pts',(56.9926786911212,30.4262474834164,23.2673408465866));
#57951=CARTESIAN_POINT('Ctrl Pts',(57.0399740251992,30.3601689062392,23.2631177216527));
#57952=CARTESIAN_POINT('Ctrl Pts',(57.0840326507937,30.2916603080827,23.2588945967188));
#57953=CARTESIAN_POINT('Ctrl Pts',(57.1246007636182,30.2210740539512,23.2546714717848));
#57954=CARTESIAN_POINT('Ctrl Pts',(57.1650804025972,30.1506417393774,23.2504575569442));
#57955=CARTESIAN_POINT('Ctrl Pts',(57.2020844836243,30.0781412129691,23.2462436421036));
#57956=CARTESIAN_POINT('Ctrl Pts',(57.2354040962635,30.0039515807091,23.2420297272629));
#57957=CARTESIAN_POINT('Ctrl Pts',(57.2687125107127,29.9297868824005,23.2378172286518));
#57958=CARTESIAN_POINT('Ctrl Pts',(57.2983387250494,29.8539346300981,23.2336047300407));
#57959=CARTESIAN_POINT('Ctrl Pts',(57.3241207737503,29.7767965493117,23.2293922314296));
#57960=CARTESIAN_POINT('Ctrl Pts',(57.3499020921784,29.6996606534499,23.2251798521369));
#57961=CARTESIAN_POINT('Ctrl Pts',(57.3718393148471,29.6212394436475,23.2209674728442));
#57962=CARTESIAN_POINT('Ctrl Pts',(57.3898199049781,29.5419511710207,23.2167550935515));
#57963=CARTESIAN_POINT('Ctrl Pts',(57.4078789979708,29.4623167275363,23.2125243231032));
#57964=CARTESIAN_POINT('Ctrl Pts',(57.4219467125659,29.3818080914518,23.208293552655));
#57965=CARTESIAN_POINT('Ctrl Pts',(57.4319609652375,29.3008589595823,23.2040627822068));
#57966=CARTESIAN_POINT('Ctrl Pts',(57.4419460760183,29.2201453930455,23.1998443234761));
#57967=CARTESIAN_POINT('Ctrl Pts',(57.4479012922646,29.1389943615875,23.1956258647454));
#57968=CARTESIAN_POINT('Ctrl Pts',(57.4498173277825,29.0578386591885,23.1914074060148));
#57969=CARTESIAN_POINT('Ctrl Pts',(57.4517417513241,28.9763276732072,23.1871704797078));
#57970=CARTESIAN_POINT('Ctrl Pts',(57.4495915665513,28.8948124482751,23.1829335534008));
#57971=CARTESIAN_POINT('Ctrl Pts',(57.443410061242,28.8137272896495,23.1786966270938));
#57972=CARTESIAN_POINT('Ctrl Pts',(57.4372285559327,28.7326421310238,23.1744597007868));
#57973=CARTESIAN_POINT('Ctrl Pts',(57.4270158514712,28.6519874962646,23.1702227744797));
#57974=CARTESIAN_POINT('Ctrl Pts',(57.4128667311383,28.572186503525,23.1659858481727));
#57975=CARTESIAN_POINT('Ctrl Pts',(57.3987289132656,28.4924492566242,23.1617523063652));
#57976=CARTESIAN_POINT('Ctrl Pts',(57.3806080574253,28.4132657080739,23.1575187645578));
#57977=CARTESIAN_POINT('Ctrl Pts',(57.3585610360867,28.3350638458819,23.1532852227503));
#57978=CARTESIAN_POINT('Ctrl Pts',(57.3365454407038,28.2569734530904,23.1490577154585));
#57979=CARTESIAN_POINT('Ctrl Pts',(57.3106149200503,28.1798624106211,23.1448302081668));
#57980=CARTESIAN_POINT('Ctrl Pts',(57.2808775707241,28.1041497014747,23.140602700875));
#57981=CARTESIAN_POINT('Ctrl Pts',(57.2511744714117,28.0285241944964,23.1363800626179));
#57982=CARTESIAN_POINT('Ctrl Pts',(57.2176734265239,27.9542942498791,23.1321574243607));
#57983=CARTESIAN_POINT('Ctrl Pts',(57.1805322388255,27.8818634227239,23.1279347861036));
#57984=CARTESIAN_POINT('Ctrl Pts',(57.1434145361545,27.8094783948568,23.123714817895));
#57985=CARTESIAN_POINT('Ctrl Pts',(57.1026614712074,27.7388906381866,23.1194948496864));
#57986=CARTESIAN_POINT('Ctrl Pts',(57.0584783653688,27.6704823922533,23.1152748814779));
#57987=CARTESIAN_POINT('Ctrl Pts',(57.014309704517,27.6020965113436,23.111056292923));
#57988=CARTESIAN_POINT('Ctrl Pts',(56.9667134815588,27.5358891157875,23.1068377043681));
#57989=CARTESIAN_POINT('Ctrl Pts',(56.9159395072919,27.4722153115056,23.1026191158132));
#57990=CARTESIAN_POINT('Ctrl Pts',(56.8651666276668,27.4085428799743,23.0984006182073));
#57991=CARTESIAN_POINT('Ctrl Pts',(56.8112164233434,27.3474042934087,23.0941821206015));
#57992=CARTESIAN_POINT('Ctrl Pts',(56.7543794388078,27.289122145012,23.0899636229956));
#57993=CARTESIAN_POINT('Ctrl Pts',(56.69747662169,27.2307724901429,23.0857402392299));
#57994=CARTESIAN_POINT('Ctrl Pts',(56.6376806661255,27.1752862200568,23.0815168554642));
#57995=CARTESIAN_POINT('Ctrl Pts',(56.5753193042457,27.1229492975226,23.0772934716985));
#57996=CARTESIAN_POINT('Ctrl Pts',(56.5129402173685,27.0705974992418,23.0730688875186));
#57997=CARTESIAN_POINT('Ctrl Pts',(56.4479946467122,27.0213971071168,23.0688443033387));
#57998=CARTESIAN_POINT('Ctrl Pts',(56.3808414053864,26.9755921203546,23.0646197191588));
#57999=CARTESIAN_POINT('Ctrl Pts',(56.3135666438222,26.9297042450705,23.0603874901881));
#58000=CARTESIAN_POINT('Ctrl Pts',(56.2440766249951,26.8872242972987,23.0561552612175));
#58001=CARTESIAN_POINT('Ctrl Pts',(56.1727570784822,26.8483515424517,23.0519230322469));
#58002=CARTESIAN_POINT('Ctrl Pts',(56.1017558713171,26.8096522986271,23.0477096941003));
#58003=CARTESIAN_POINT('Ctrl Pts',(56.0289418817796,26.7745282251677,23.0434963559538));
#58004=CARTESIAN_POINT('Ctrl Pts',(55.9547139357488,26.7431279276647,23.0392830178073));
#58005=CARTESIAN_POINT('Ctrl Pts',(55.8801328412964,26.7115782394525,23.0350496341955));
#58006=CARTESIAN_POINT('Ctrl Pts',(55.8038480783036,26.6836710384964,23.0308162505837));
#58007=CARTESIAN_POINT('Ctrl Pts',(55.726249631041,26.6595915477394,23.0265828669719));
#58008=CARTESIAN_POINT('Ctrl Pts',(55.6487615440981,26.6355463027746,23.0223555040678));
#58009=CARTESIAN_POINT('Ctrl Pts',(55.569963923485,26.6153180923391,23.0181281411637));
#58010=CARTESIAN_POINT('Ctrl Pts',(55.4902670770494,26.5990442646393,23.0139007782596));
#58011=CARTESIAN_POINT('Ctrl Pts',(55.4106616146491,26.5827890972519,23.0096782626424));
#58012=CARTESIAN_POINT('Ctrl Pts',(55.3301594283528,26.5704793932409,23.0054557470252));
#58013=CARTESIAN_POINT('Ctrl Pts',(55.2491849369823,26.5622024043861,23.001233231408));
#58014=CARTESIAN_POINT('Ctrl Pts',(55.1682613941383,26.5539306233488,22.9970133725651));
#58015=CARTESIAN_POINT('Ctrl Pts',(55.0868665968571,26.5496865675813,22.9927935137223));
#58016=CARTESIAN_POINT('Ctrl Pts',(55.0054329419913,26.549506022627,22.9885736548794));
#58017=CARTESIAN_POINT('Ctrl Pts',(54.9240256515744,26.5493255361249,22.9843551622315));
#58018=CARTESIAN_POINT('Ctrl Pts',(54.8425799925547,26.5532059487735,22.9801366695836));
#58019=CARTESIAN_POINT('Ctrl Pts',(54.7615298097258,26.5611309550633,22.9759181769358));
#58020=CARTESIAN_POINT('Ctrl Pts',(54.6804811119383,26.5690558161471,22.9716997615812));
#58021=CARTESIAN_POINT('Ctrl Pts',(54.5998283379637,26.5810250771506,22.9674813462267));
#58022=CARTESIAN_POINT('Ctrl Pts',(54.5200002233569,26.5969705652193,22.9632629308721));
#58023=CARTESIAN_POINT('Ctrl Pts',(54.440074715967,26.6129355072795,22.9590393689196));
#58024=CARTESIAN_POINT('Ctrl Pts',(54.3609763361036,26.6328862828714,22.954815806967));
#58025=CARTESIAN_POINT('Ctrl Pts',(54.2831233980475,26.6567035638714,22.9505922450145));
#58026=CARTESIAN_POINT('Ctrl Pts',(54.2052524953077,26.6805263407452,22.9463677084687));
#58027=CARTESIAN_POINT('Ctrl Pts',(54.1286280413679,26.708217233255,22.9421431719228));
#58028=CARTESIAN_POINT('Ctrl Pts',(54.0536499864002,26.7396080203293,22.9379186353769));
#58029=CARTESIAN_POINT('Ctrl Pts',(53.9785358691495,26.7710557721003,22.9336864325868));
#58030=CARTESIAN_POINT('Ctrl Pts',(53.9050745417714,26.8062166354433,22.9294542297966));
#58031=CARTESIAN_POINT('Ctrl Pts',(53.83364307309,26.8448754632159,22.9252220270064));
#58032=CARTESIAN_POINT('Ctrl Pts',(53.7625197352201,26.8833675300888,22.9210080804849));
#58033=CARTESIAN_POINT('Ctrl Pts',(53.6934091171587,26.9253271307111,22.9167941339634));
#58034=CARTESIAN_POINT('Ctrl Pts',(53.6266530602894,26.970500447601,22.9125801874418));
#58035=CARTESIAN_POINT('Ctrl Pts',(53.559831201844,27.015718291918,22.9083620872249));
#58036=CARTESIAN_POINT('Ctrl Pts',(53.4951162351161,27.0643270129538,22.904143987008));
#58037=CARTESIAN_POINT('Ctrl Pts',(53.4328743933687,27.1161030858775,22.8999258867911));
#58038=CARTESIAN_POINT('Ctrl Pts',(53.3707216263246,27.1678050617274,22.8957138231248));
#58039=CARTESIAN_POINT('Ctrl Pts',(53.3110353128802,27.2226650915625,22.8915017594585));
#58040=CARTESIAN_POINT('Ctrl Pts',(53.2541527620657,27.2804164248874,22.8872896957922));
#58041=CARTESIAN_POINT('Ctrl Pts',(53.1973355303895,27.338101441437,22.8830824689056));
#58042=CARTESIAN_POINT('Ctrl Pts',(53.1433159903921,27.3986708321606,22.878875242019));
#58043=CARTESIAN_POINT('Ctrl Pts',(53.0923972278155,27.4618186343756,22.8746680151324));
#58044=CARTESIAN_POINT('Ctrl Pts',(53.0415102841336,27.5249269758267,22.8704634173221));
#58045=CARTESIAN_POINT('Ctrl Pts',(52.9937205652041,27.5906101674105,22.8662588195117));
#58046=CARTESIAN_POINT('Ctrl Pts',(52.9492923969959,27.6585274594755,22.8620542217014));
#58047=CARTESIAN_POINT('Ctrl Pts',(52.9048781562321,27.7264234606716,22.8578509419581));
#58048=CARTESIAN_POINT('Ctrl Pts',(52.863823629782,27.7965517801551,22.8536476622147));
#58049=CARTESIAN_POINT('Ctrl Pts',(52.8263502659314,27.8685420539925,22.8494443824714));
#58050=CARTESIAN_POINT('Ctrl Pts',(52.7888769797546,27.9405321786104,22.8452411114405));
#58051=CARTESIAN_POINT('Ctrl Pts',(52.7549850561409,28.0143838338902,22.8410378404096));
#58052=CARTESIAN_POINT('Ctrl Pts',(52.7248496557592,28.0897027072979,22.8368345693787));
#58053=CARTESIAN_POINT('Ctrl Pts',(52.6946846212127,28.1650956468162,22.8326271649889));
#58054=CARTESIAN_POINT('Ctrl Pts',(52.6682836619809,28.2419582504506,22.8284197605991));
#58055=CARTESIAN_POINT('Ctrl Pts',(52.6457732464847,28.3198774793959,22.8242123562093));
#58056=CARTESIAN_POINT('Ctrl Pts',(52.6232517664169,28.3978350080738,22.8200028837489));
#58057=CARTESIAN_POINT('Ctrl Pts',(52.6046247459021,28.4768497402581,22.8157934112885));
#58058=CARTESIAN_POINT('Ctrl Pts',(52.5899677282388,28.5564972389382,22.8115839388282));
#58059=CARTESIAN_POINT('Ctrl Pts',(52.5752850185252,28.6362843504363,22.8073670876513));
#58060=CARTESIAN_POINT('Ctrl Pts',(52.564586274865,28.716705979306,22.8031502364744));
#58061=CARTESIAN_POINT('Ctrl Pts',(52.5578952153805,28.7973316232398,22.7989333852976));
#58062=CARTESIAN_POINT('Ctrl Pts',(52.552285608312,28.8649260278568,22.7953980889483));
#58063=CARTESIAN_POINT('Ctrl Pts',(52.5494919509591,28.9326636235578,22.791862792599));
#58064=CARTESIAN_POINT('Ctrl Pts',(52.5495000174313,29.0002922856895,22.7883274962497));
#58065=CARTESIAN_POINT('',(52.5495008948029,28.9979058586013,21.9883275169164));
#58066=CARTESIAN_POINT('Ctrl Pts',(52.5495000174314,29.0002922864085,22.7883274962121));
#58067=CARTESIAN_POINT('Ctrl Pts',(52.5495018809271,29.015915647263,22.7875107831668));
#58068=CARTESIAN_POINT('Ctrl Pts',(52.5496531545866,29.0315379897785,22.7866940701216));
#58069=CARTESIAN_POINT('Ctrl Pts',(52.54995379109,29.0471574406191,22.7858773570764));
#58070=CARTESIAN_POINT('Ctrl Pts',(52.551511902383,29.1281084976825,22.7816445716218));
#58071=CARTESIAN_POINT('Ctrl Pts',(52.5570892279648,29.2091326985126,22.7774117861671));
#58072=CARTESIAN_POINT('Ctrl Pts',(52.566696269008,29.2897985554489,22.7731790007125));
#58073=CARTESIAN_POINT('Ctrl Pts',(52.5762896098424,29.3703493781018,22.7689522514603));
#58074=CARTESIAN_POINT('Ctrl Pts',(52.589901198119,29.4505424143979,22.7647255022081));
#58075=CARTESIAN_POINT('Ctrl Pts',(52.6074895335361,29.5299470896805,22.7604987529559));
#58076=CARTESIAN_POINT('Ctrl Pts',(52.6250576127034,29.6092603156642,22.7562768715941));
#58077=CARTESIAN_POINT('Ctrl Pts',(52.6465932365051,29.6877865339608,22.7520549902323));
#58078=CARTESIAN_POINT('Ctrl Pts',(52.6720034019218,29.7651026658798,22.7478331088705));
#58079=CARTESIAN_POINT('Ctrl Pts',(52.6973975034608,29.8423699198451,22.7436138965108));
#58080=CARTESIAN_POINT('Ctrl Pts',(52.726661139605,29.9184281659353,22.7393946841512));
#58081=CARTESIAN_POINT('Ctrl Pts',(52.7596510489301,29.9928679808715,22.7351754717915));
#58082=CARTESIAN_POINT('Ctrl Pts',(52.7926301873071,30.0672834917891,22.7309576369717));
#58083=CARTESIAN_POINT('Ctrl Pts',(52.8293329947074,30.1400811965917,22.726739802152));
#58084=CARTESIAN_POINT('Ctrl Pts',(52.8695680384666,30.2108715486281,22.7225219673322));
#58085=CARTESIAN_POINT('Ctrl Pts',(52.9098022449982,30.2816604276293,22.7183042202789));
#58086=CARTESIAN_POINT('Ctrl Pts',(52.9535683112031,30.3504416336603,22.7140864732257));
#58087=CARTESIAN_POINT('Ctrl Pts',(53.000629506976,30.4168513971568,22.7098687261724));
#58088=CARTESIAN_POINT('Ctrl Pts',(53.0477662369107,30.4833677496537,22.7056442095506));
#58089=CARTESIAN_POINT('Ctrl Pts',(53.0982084066648,30.5475046644456,22.7014196929288));
#58090=CARTESIAN_POINT('Ctrl Pts',(53.151676470778,30.6089283331847,22.697195176307));
#58091=CARTESIAN_POINT('Ctrl Pts',(53.2051360931266,30.6703423040945,22.6929713266698));
#58092=CARTESIAN_POINT('Ctrl Pts',(53.2616203165558,30.7290435639711,22.6887474770326));
#58093=CARTESIAN_POINT('Ctrl Pts',(53.3208127308396,30.7847353767687,22.6845236273954));
#58094=CARTESIAN_POINT('Ctrl Pts',(53.3801125017213,30.8405281971637,22.6802921170109));
#58095=CARTESIAN_POINT('Ctrl Pts',(53.4421299247691,30.8933003605444,22.6760606066264));
#58096=CARTESIAN_POINT('Ctrl Pts',(53.5065150453206,30.9427951359179,22.671829096242));
#58097=CARTESIAN_POINT('Ctrl Pts',(53.5706974853756,30.992134104708,22.6676109063983));
#58098=CARTESIAN_POINT('Ctrl Pts',(53.6372323159481,31.0382161003672,22.6633927165546));
#58099=CARTESIAN_POINT('Ctrl Pts',(53.7057472873696,31.0808316043949,22.6591745267109));
#58100=CARTESIAN_POINT('Ctrl Pts',(53.7744978327295,31.1235936326335,22.6549418335321));
#58101=CARTESIAN_POINT('Ctrl Pts',(53.8454977274284,31.1630242160109,22.6507091403532));
#58102=CARTESIAN_POINT('Ctrl Pts',(53.9183907616251,31.1988796477893,22.6464764471744));
#58103=CARTESIAN_POINT('Ctrl Pts',(53.9911798559339,31.2346839524663,22.642249789492));
#58104=CARTESIAN_POINT('Ctrl Pts',(54.065856314865,31.2669230272973,22.6380231318097));
#58105=CARTESIAN_POINT('Ctrl Pts',(54.1420363842115,31.2953972823856,22.6337964741274));
#58106=CARTESIAN_POINT('Ctrl Pts',(54.2181300849763,31.3238392550009,22.6295746083865));
#58107=CARTESIAN_POINT('Ctrl Pts',(54.2957235755163,31.3485247284311,22.6253527426456));
#58108=CARTESIAN_POINT('Ctrl Pts',(54.3744113291554,31.3693013875214,22.6211308769047));
#58109=CARTESIAN_POINT('Ctrl Pts',(54.4530479677455,31.3900645502302,22.6169117536601));
#58110=CARTESIAN_POINT('Ctrl Pts',(54.532777010114,31.4069238218743,22.6126926304155));
#58111=CARTESIAN_POINT('Ctrl Pts',(54.6131770446963,31.4197764878703,22.6084735071709));
#58112=CARTESIAN_POINT('Ctrl Pts',(54.6935508500271,31.4326249608855,22.6042557603491));
#58113=CARTESIAN_POINT('Ctrl Pts',(54.7745947544948,31.4414693507897,22.6000380135274));
#58114=CARTESIAN_POINT('Ctrl Pts',(54.8558777954438,31.4462581711982,22.5958202667056));
#58115=CARTESIAN_POINT('Ctrl Pts',(54.9371591689845,31.4510468933707,22.5916026064051));
#58116=CARTESIAN_POINT('Ctrl Pts',(55.0186792054603,31.4517801853135,22.5873849461045));
#58117=CARTESIAN_POINT('Ctrl Pts',(55.1000039053973,31.4484585904004,22.583167285804));
#58118=CARTESIAN_POINT('Ctrl Pts',(55.1814630420402,31.4451315046058,22.5789426533491));
#58119=CARTESIAN_POINT('Ctrl Pts',(55.2627257296209,31.4377361405835,22.5747180208942));
#58120=CARTESIAN_POINT('Ctrl Pts',(55.34335973163,31.4263252759461,22.5704933884393));
#58121=CARTESIAN_POINT('Ctrl Pts',(55.4239772125173,31.4149167492838,22.5662696215705));
#58122=CARTESIAN_POINT('Ctrl Pts',(55.5039658117012,31.3994944760461,22.5620458547017));
#58123=CARTESIAN_POINT('Ctrl Pts',(55.582904383817,31.3801623325578,22.5578220878329));
#58124=CARTESIAN_POINT('Ctrl Pts',(55.6619861864785,31.3607951117506,22.553590657126));
#58125=CARTESIAN_POINT('Ctrl Pts',(55.7400137081264,31.3375039762578,22.5493592264192));
#58126=CARTESIAN_POINT('Ctrl Pts',(55.8165811004963,31.3104427186823,22.5451277957123));
#58127=CARTESIAN_POINT('Ctrl Pts',(55.8929181279475,31.2834628791128,22.5409090959234));
#58128=CARTESIAN_POINT('Ctrl Pts',(55.9678034109459,31.25273582221,22.5366903961344));
#58129=CARTESIAN_POINT('Ctrl Pts',(56.0408584123792,31.2184598295618,22.5324716963455));
#58130=CARTESIAN_POINT('Ctrl Pts',(56.1141528359076,31.1840715047009,22.5282391706731));
#58131=CARTESIAN_POINT('Ctrl Pts',(56.1858775852503,31.1459830025043,22.5240066450006));
#58132=CARTESIAN_POINT('Ctrl Pts',(56.2556343272889,31.1043603983476,22.5197741193282));
#58133=CARTESIAN_POINT('Ctrl Pts',(56.3252915428871,31.0627971798432,22.5155476324729));
#58134=CARTESIAN_POINT('Ctrl Pts',(56.392985932358,31.0177101101498,22.5113211456177));
#58135=CARTESIAN_POINT('Ctrl Pts',(56.458341168815,30.9693123889671,22.5070946587624));
#58136=CARTESIAN_POINT('Ctrl Pts',(56.5236256017779,30.9209671001212,22.5028727507298));
#58137=CARTESIAN_POINT('Ctrl Pts',(56.5865755447787,30.8693185603639,22.4986508426972));
#58138=CARTESIAN_POINT('Ctrl Pts',(56.6468424163714,30.8146240121965,22.4944289346646));
#58139=CARTESIAN_POINT('Ctrl Pts',(56.707066999848,30.7599678421519,22.4902099890645));
#58140=CARTESIAN_POINT('Ctrl Pts',(56.7646119089447,30.7022702212389,22.4859910434643));
#58141=CARTESIAN_POINT('Ctrl Pts',(56.8191615721865,30.6418286829873,22.4817720978642));
#58142=CARTESIAN_POINT('Ctrl Pts',(56.873693410549,30.5814068948692,22.4775545308646));
#58143=CARTESIAN_POINT('Ctrl Pts',(56.9252316357471,30.5182433146465,22.473336963865));
#58144=CARTESIAN_POINT('Ctrl Pts',(56.9734984458387,30.4526713786236,22.4691193968655));
#58145=CARTESIAN_POINT('Ctrl Pts',(57.0217642435996,30.3871008178829,22.4649019183236));
#58146=CARTESIAN_POINT('Ctrl Pts',(57.0667584882196,30.319122376608,22.4606844397818));
#58147=CARTESIAN_POINT('Ctrl Pts',(57.1082453667274,30.2491003657322,22.45646696124));
#58148=CARTESIAN_POINT('Ctrl Pts',(57.1498046716092,30.1789561128242,22.4522421199683));
#58149=CARTESIAN_POINT('Ctrl Pts',(57.1878441206886,30.1067615537844,22.4480172786966));
#58150=CARTESIAN_POINT('Ctrl Pts',(57.2221726240576,30.0329080689436,22.443792437425));
#58151=CARTESIAN_POINT('Ctrl Pts',(57.2564908969921,29.9590765936043,22.4395688552225));
#58152=CARTESIAN_POINT('Ctrl Pts',(57.2871002806282,29.883587621269,22.4353452730201));
#58153=CARTESIAN_POINT('Ctrl Pts',(57.3138586410326,29.8068509399628,22.4311216908177));
#58154=CARTESIAN_POINT('Ctrl Pts',(57.3406655535197,29.7299750227078,22.4268904450772));
#58155=CARTESIAN_POINT('Ctrl Pts',(57.3636073471398,29.6518473191553,22.4226591993367));
#58156=CARTESIAN_POINT('Ctrl Pts',(57.3825920866213,29.5728919608175,22.4184279535963));
#58157=CARTESIAN_POINT('Ctrl Pts',(57.4015250041914,29.4941521238776,22.4142082577242));
#58158=CARTESIAN_POINT('Ctrl Pts',(57.4165224394577,29.4145896078156,22.4099885618521));
#58159=CARTESIAN_POINT('Ctrl Pts',(57.4275446176907,29.3346302125048,22.40576886598));
#58160=CARTESIAN_POINT('Ctrl Pts',(57.4386006142479,29.2544254852183,22.4015362232076));
#58161=CARTESIAN_POINT('Ctrl Pts',(57.4456980206086,29.1735231071443,22.3973035804351));
#58162=CARTESIAN_POINT('Ctrl Pts',(57.4487593107478,29.0923476476475,22.3930709376626));
#58163=CARTESIAN_POINT('Ctrl Pts',(57.451816234469,29.0112879713552,22.3888443320466));
#58164=CARTESIAN_POINT('Ctrl Pts',(57.450848458447,28.9299564476022,22.3846177264305));
#58165=CARTESIAN_POINT('Ctrl Pts',(57.4458299664352,28.8487848377715,22.3803911208145));
#58166=CARTESIAN_POINT('Ctrl Pts',(57.4408170871408,28.7677040108521,22.3761692422645));
#58167=CARTESIAN_POINT('Ctrl Pts',(57.4317625226274,28.6867832037761,22.3719473637145));
#58168=CARTESIAN_POINT('Ctrl Pts',(57.4186923018831,28.6064548325652,22.3677254851645));
#58169=CARTESIAN_POINT('Ctrl Pts',(57.4056307836308,28.5261799460671,22.3635064176507));
#58170=CARTESIAN_POINT('Ctrl Pts',(57.3885589933099,28.4464971693967,22.359287350137));
#58171=CARTESIAN_POINT('Ctrl Pts',(57.3675547293458,28.3678332074902,22.3550682826232));
#58172=CARTESIAN_POINT('Ctrl Pts',(57.3465573240663,28.2891949323345,22.3508505927941));
#58173=CARTESIAN_POINT('Ctrl Pts',(57.3216301150387,28.2115752597305,22.3466329029651));
#58174=CARTESIAN_POINT('Ctrl Pts',(57.292901578214,28.1353887563629,22.342415213136));
#58175=CARTESIAN_POINT('Ctrl Pts',(57.2641736388151,28.0592038373356,22.3381976110161));
#58176=CARTESIAN_POINT('Ctrl Pts',(57.2316446937954,27.9844524625377,22.3339800088962));
#58177=CARTESIAN_POINT('Ctrl Pts',(57.1954919758804,27.9115307841539,22.3297624067764));
#58178=CARTESIAN_POINT('Ctrl Pts',(57.1592784364919,27.8384864260882,22.3255377091795));
#58179=CARTESIAN_POINT('Ctrl Pts',(57.1194291343123,27.7672783414038,22.3213130115827));
#58180=CARTESIAN_POINT('Ctrl Pts',(57.07616831138,27.6982798331357,22.3170883139859));
#58181=CARTESIAN_POINT('Ctrl Pts',(57.0329176387413,27.6292975139981,22.3128646076306));
#58182=CARTESIAN_POINT('Ctrl Pts',(56.9862573303634,27.5625241045296,22.3086409012752));
#58183=CARTESIAN_POINT('Ctrl Pts',(56.9364537618731,27.498301935099,22.3044171949198));
#58184=CARTESIAN_POINT('Ctrl Pts',(56.8865598367488,27.4339632499399,22.300185825662));
#58185=CARTESIAN_POINT('Ctrl Pts',(56.8335115583894,27.3721854084049,22.2959544564041));
#58186=CARTESIAN_POINT('Ctrl Pts',(56.777614662308,27.3132764416338,22.2917230871462));
#58187=CARTESIAN_POINT('Ctrl Pts',(56.7218809386956,27.2545394400742,22.287504069969));
#58188=CARTESIAN_POINT('Ctrl Pts',(56.663315592898,27.1986548403543,22.2832850527918));
#58189=CARTESIAN_POINT('Ctrl Pts',(56.6022539625235,27.1458876815096,22.2790660356146));
#58190=CARTESIAN_POINT('Ctrl Pts',(56.5409954399236,27.0929503758269,22.2748334142857));
#58191=CARTESIAN_POINT('Ctrl Pts',(56.4769966705314,27.042953795681,22.2706007929569));
#58192=CARTESIAN_POINT('Ctrl Pts',(56.4105715839815,26.9961941070892,22.266368171628));
#58193=CARTESIAN_POINT('Ctrl Pts',(56.3442412430922,26.9495011143471,22.2621415875138));
#58194=CARTESIAN_POINT('Ctrl Pts',(56.2754918353231,26.9060361084803,22.2579150033995));
#58195=CARTESIAN_POINT('Ctrl Pts',(56.2046713653864,26.8660559633819,22.2536884192853));
#58196=CARTESIAN_POINT('Ctrl Pts',(56.1339296517423,26.8261202784234,22.2494665353671));
#58197=CARTESIAN_POINT('Ctrl Pts',(56.0611218548132,26.7896619810227,22.2452446514489));
#58198=CARTESIAN_POINT('Ctrl Pts',(55.98662486943,26.7568946487019,22.2410227675307));
#58199=CARTESIAN_POINT('Ctrl Pts',(55.912177959732,26.7241493420591,22.2368037214956));
#58200=CARTESIAN_POINT('Ctrl Pts',(55.8360445407491,26.6950902596719,22.2325846754605));
#58201=CARTESIAN_POINT('Ctrl Pts',(55.7586248930801,26.6698844402907,22.2283656294253));
#58202=CARTESIAN_POINT('Ctrl Pts',(55.6812305249085,26.6446868512551,22.2241479610167));
#58203=CARTESIAN_POINT('Ctrl Pts',(55.602551203505,26.6233401702427,22.2199302926081));
#58204=CARTESIAN_POINT('Ctrl Pts',(55.5230046165781,26.6059623183755,22.2157126241996));
#58205=CARTESIAN_POINT('Ctrl Pts',(55.443459682209,26.5885848275282,22.2114950434119));
#58206=CARTESIAN_POINT('Ctrl Pts',(55.3630479722324,26.5751760998911,22.2072774626241));
#58207=CARTESIAN_POINT('Ctrl Pts',(55.2821982710643,26.565803133309,22.2030598818364));
#58208=CARTESIAN_POINT('Ctrl Pts',(55.201211654988,26.5564142940788,22.1988351587875));
#58209=CARTESIAN_POINT('Ctrl Pts',(55.119786027606,26.5510749435566,22.1946104357385));
#58210=CARTESIAN_POINT('Ctrl Pts',(55.0383566131692,26.5498002081001,22.1903857126896));
#58211=CARTESIAN_POINT('Ctrl Pts',(54.9569471977203,26.5485257857175,22.1861620272287));
#58212=CARTESIAN_POINT('Ctrl Pts',(54.8755344622266,26.5513139449561,22.1819383417678));
#58213=CARTESIAN_POINT('Ctrl Pts',(54.7945505732901,26.5581276071292,22.1777146563068));
#58214=CARTESIAN_POINT('Ctrl Pts',(54.7134197495079,26.5649536318155,22.1734833075122));
#58215=CARTESIAN_POINT('Ctrl Pts',(54.632719788992,26.5758196935741,22.1692519587175));
#58216=CARTESIAN_POINT('Ctrl Pts',(54.5528755146421,26.5906370251468,22.1650206099228));
#58217=CARTESIAN_POINT('Ctrl Pts',(54.4732617129635,26.6054115860886,22.1608014750316));
#58218=CARTESIAN_POINT('Ctrl Pts',(54.3944990878205,26.6241144503633,22.1565823401403));
#58219=CARTESIAN_POINT('Ctrl Pts',(54.3169925537467,26.6466086006865,22.1523632052491));
#58220=CARTESIAN_POINT('Ctrl Pts',(54.239238611905,26.6691745543434,22.1481306025031));
#58221=CARTESIAN_POINT('Ctrl Pts',(54.1624596057763,26.6956399943221,22.1438979997571));
#58222=CARTESIAN_POINT('Ctrl Pts',(54.0870748679564,26.7259028267721,22.1396653970111));
#58223=CARTESIAN_POINT('Ctrl Pts',(54.011797663029,26.7561224906709,22.13543883188));
#58224=CARTESIAN_POINT('Ctrl Pts',(53.9379112038061,26.7901286169372,22.1312122667489));
#58225=CARTESIAN_POINT('Ctrl Pts',(53.8658204147616,26.8277691378612,22.1269857016178));
#58226=CARTESIAN_POINT('Ctrl Pts',(53.7938093911539,26.8653680111262,22.1227638130039));
#58227=CARTESIAN_POINT('Ctrl Pts',(53.7235904996973,26.9065930749595,22.1185419243899));
#58228=CARTESIAN_POINT('Ctrl Pts',(53.6555480816002,26.9512444535496,22.114320035776));
#58229=CARTESIAN_POINT('Ctrl Pts',(53.5875517955472,26.9958655589746,22.1101010095582));
#58230=CARTESIAN_POINT('Ctrl Pts',(53.5217294394126,27.0439081110724,22.1058819833403));
#58231=CARTESIAN_POINT('Ctrl Pts',(53.4584390414731,27.0951272847916,22.1016629571225));
#58232=CARTESIAN_POINT('Ctrl Pts',(53.3951693136296,27.146329730772,22.0974453088021));
#58233=CARTESIAN_POINT('Ctrl Pts',(53.3344302626156,27.2007064460319,22.0932276604817));
#58234=CARTESIAN_POINT('Ctrl Pts',(53.2765481923684,27.2579712640799,22.0890100121613));
#58235=CARTESIAN_POINT('Ctrl Pts',(53.2186673279599,27.3152348891483,22.0847924517058));
#58236=CARTESIAN_POINT('Ctrl Pts',(53.1636436553973,27.3753861698215,22.0805748912503));
#58237=CARTESIAN_POINT('Ctrl Pts',(53.111766804186,27.4381019085018,22.0763573307949));
#58238=CARTESIAN_POINT('Ctrl Pts',(53.0598015653069,27.5009245021229,22.0721325844689));
#58239=CARTESIAN_POINT('Ctrl Pts',(53.0109941727395,27.5663199359595,22.067907838143));
#58240=CARTESIAN_POINT('Ctrl Pts',(52.965594258439,27.6339313601785,22.0636830918171));
#58241=CARTESIAN_POINT('Ctrl Pts',(52.9202059671091,27.7015254749906,22.0594594270813));
#58242=CARTESIAN_POINT('Ctrl Pts',(52.8782236315398,27.7713340352223,22.0552357623456));
#58243=CARTESIAN_POINT('Ctrl Pts',(52.8398514202671,27.8429743462318,22.0510120976099));
#58244=CARTESIAN_POINT('Ctrl Pts',(52.8014095878862,27.9147446387481,22.0467807696144));
#58245=CARTESIAN_POINT('Ctrl Pts',(52.7665911691204,27.988352902704,22.042549441619));
#58246=CARTESIAN_POINT('Ctrl Pts',(52.7355529769454,28.0633944641531,22.0383181136236));
#58247=CARTESIAN_POINT('Ctrl Pts',(52.7046034083988,28.1382217587587,22.034098867377));
#58248=CARTESIAN_POINT('Ctrl Pts',(52.6774125823483,28.2144737199589,22.0298796211303));
#58249=CARTESIAN_POINT('Ctrl Pts',(52.654086009428,28.2917360669646,22.0256603748837));
#58250=CARTESIAN_POINT('Ctrl Pts',(52.6254336649508,28.3866384510008,22.02047781775));
#58251=CARTESIAN_POINT('Ctrl Pts',(52.6025235371786,28.4833492873121,22.0152952606162));
#58252=CARTESIAN_POINT('Ctrl Pts',(52.5855453264011,28.5812412638087,22.0101127034825));
#58253=CARTESIAN_POINT('Ctrl Pts',(52.5688012110521,28.6777835065506,22.0050016034033));
#58254=CARTESIAN_POINT('Ctrl Pts',(52.5578265961228,28.7754745670536,21.9998905033241));
#58255=CARTESIAN_POINT('Ctrl Pts',(52.5527573617204,28.8736919662633,21.9947794032449));
#58256=CARTESIAN_POINT('Ctrl Pts',(52.5506243490207,28.9150195008028,21.9926287744687));
#58257=CARTESIAN_POINT('Ctrl Pts',(52.5495363306197,28.9564399683349,21.9904781456926));
#58258=CARTESIAN_POINT('Ctrl Pts',(52.5495008948029,28.9979058586013,21.9883275169164));
#58259=CARTESIAN_POINT('',(52.5526951386847,29.0013429706744,21.1883274962121));
#58260=CARTESIAN_POINT('Ctrl Pts',(52.5509293928096,28.9979074783278,21.9883274962121));
#58261=CARTESIAN_POINT('Ctrl Pts',(52.555637109855,29.5719524683613,21.9585375123141));
#58262=CARTESIAN_POINT('Ctrl Pts',(53.0429452071781,30.9670398873744,21.8865132516278));
#58263=CARTESIAN_POINT('Ctrl Pts',(55.3643553567281,31.8709715157123,21.7722547141527));
#58264=CARTESIAN_POINT('Ctrl Pts',(57.6065987423142,30.257328552056,21.6455518837873));
#58265=CARTESIAN_POINT('Ctrl Pts',(57.4737133360388,27.498009992113,21.5188490534219));
#58266=CARTESIAN_POINT('Ctrl Pts',(55.0867844397265,26.1073022273406,21.3921462230564));
#58267=CARTESIAN_POINT('Ctrl Pts',(52.9424797866962,27.1899851156092,21.2819723706532));
#58268=CARTESIAN_POINT('Ctrl Pts',(52.5551788087165,28.5051077036468,21.2140327950384));
#58269=CARTESIAN_POINT('Ctrl Pts',(52.5526951386847,29.0013429706744,21.1883274962121));
#58270=CARTESIAN_POINT('',(52.546116949762,29.0010979606402,20.3883274962121));
#58271=CARTESIAN_POINT('Ctrl Pts',(52.5526951386847,29.0013429706744,21.1883274962121));
#58272=CARTESIAN_POINT('Ctrl Pts',(52.5510980933635,29.3204313363915,21.1717985182499));
#58273=CARTESIAN_POINT('Ctrl Pts',(52.7571740168711,30.4528613238408,21.1130352634992));
#58274=CARTESIAN_POINT('Ctrl Pts',(54.4641895190608,31.8439653680504,21.0120377319602));
#58275=CARTESIAN_POINT('Ctrl Pts',(57.0938942397928,30.9977083845063,20.8853349015945));
#58276=CARTESIAN_POINT('Ctrl Pts',(57.8156459017858,28.3311427450632,20.7586320712293));
#58277=CARTESIAN_POINT('Ctrl Pts',(55.9717855603786,26.2740387563892,20.6319292408637));
#58278=CARTESIAN_POINT('Ctrl Pts',(53.3128323054721,26.6898183773978,20.5084943825248));
#58279=CARTESIAN_POINT('Ctrl Pts',(52.5503076068562,28.2540245866119,20.4272938009741));
#58280=CARTESIAN_POINT('Ctrl Pts',(52.546116949762,29.0010979606402,20.3883274962121));
#58281=CARTESIAN_POINT('',(52.5495689100241,28.9977886599613,19.5883274962121));
#58282=CARTESIAN_POINT('Ctrl Pts',(52.546116949762,29.0010979606402,20.3883274962121));
#58283=CARTESIAN_POINT('Ctrl Pts',(52.5457654935425,29.0637524746597,20.3850595241856));
#58284=CARTESIAN_POINT('Ctrl Pts',(52.5762972871919,29.9357868722756,20.3395572753712));
#58285=CARTESIAN_POINT('Ctrl Pts',(53.6159095712962,31.541559670917,20.2518207497671));
#58286=CARTESIAN_POINT('Ctrl Pts',(56.3784244236166,31.5446371025649,20.125117919402));
#58287=CARTESIAN_POINT('Ctrl Pts',(57.8849211638169,29.2290453097147,19.9984150890365));
#58288=CARTESIAN_POINT('Ctrl Pts',(56.7626823916054,26.704747799967,19.871712258671));
#58289=CARTESIAN_POINT('Ctrl Pts',(54.0342902665226,26.2718803937405,19.7450094283056));
#58290=CARTESIAN_POINT('Ctrl Pts',(52.6562115032221,27.8024599995536,19.6505478408193));
#58291=CARTESIAN_POINT('Ctrl Pts',(52.547821720126,28.8054976079726,19.5983205301214));
#58292=CARTESIAN_POINT('Ctrl Pts',(52.5495689100241,28.9977886599613,19.5883274962121));
#58293=CARTESIAN_POINT('',(52.553285085785,29.0006607136179,18.7883274962121));
#58294=CARTESIAN_POINT('Ctrl Pts',(52.5495689100241,28.9977886599613,19.5883274962121));
#58295=CARTESIAN_POINT('Ctrl Pts',(52.5552059942539,29.6181910889828,19.5560862533329));
#58296=CARTESIAN_POINT('Ctrl Pts',(53.1089152944742,31.0602443464707,19.4816107336654));
#58297=CARTESIAN_POINT('Ctrl Pts',(55.529472822231,31.8451520883635,19.3649009372091));
#58298=CARTESIAN_POINT('Ctrl Pts',(57.6748307788521,30.1047679303366,19.2381981068439));
#58299=CARTESIAN_POINT('Ctrl Pts',(57.3828872430288,27.3577210156594,19.1114952764783));
#58300=CARTESIAN_POINT('Ctrl Pts',(54.9196606938342,26.1071160632887,18.9847924461128));
#58301=CARTESIAN_POINT('Ctrl Pts',(52.8876672972278,27.2849697601211,18.8770698526908));
#58302=CARTESIAN_POINT('Ctrl Pts',(52.5543748892619,28.5514755235239,18.8115815360572));
#58303=CARTESIAN_POINT('Ctrl Pts',(52.553285085785,29.0006607136179,18.7883274962121));
#58304=CARTESIAN_POINT('',(52.5471787931917,29.0017322249443,17.9883274962121));
#58305=CARTESIAN_POINT('Ctrl Pts',(52.553285085785,29.0006607136179,18.7883274962121));
#58306=CARTESIAN_POINT('Ctrl Pts',(52.552395574614,29.3672912602337,18.7693472592687));
#58307=CARTESIAN_POINT('Ctrl Pts',(52.8014692833217,30.5485894345094,18.7081327455369));
#58308=CARTESIAN_POINT('Ctrl Pts',(54.6292489299202,31.8701525254662,18.6046839550165));
#58309=CARTESIAN_POINT('Ctrl Pts',(57.2057191633969,30.8735086996375,18.477981124651));
#58310=CARTESIAN_POINT('Ctrl Pts',(57.7723416519745,28.1697267677909,18.3512782942857));
#58311=CARTESIAN_POINT('Ctrl Pts',(55.8128108977569,26.2224884662913,18.2245754639201));
#58312=CARTESIAN_POINT('Ctrl Pts',(53.2345306382145,26.779769950788,18.1035918645624));
#58313=CARTESIAN_POINT('Ctrl Pts',(52.5528064276185,28.3008580228539,18.0248425419929));
#58314=CARTESIAN_POINT('Ctrl Pts',(52.5471787931917,29.0017322249443,17.9883274962121));
#58315=CARTESIAN_POINT('',(52.5495008502318,28.9979586805009,17.1883274962121));
#58316=CARTESIAN_POINT('Ctrl Pts',(52.5471787931917,29.0017322249443,17.9883274962121));
#58317=CARTESIAN_POINT('Ctrl Pts',(52.5462973554,29.1115078361563,17.9826082652045));
#58318=CARTESIAN_POINT('Ctrl Pts',(52.602769458379,30.0310210786956,17.9346547574086));
#58319=CARTESIAN_POINT('Ctrl Pts',(53.7649272708013,31.6172174592488,17.8444669728237));
#58320=CARTESIAN_POINT('Ctrl Pts',(56.5230134408625,31.4608254579201,17.7177641424583));
#58321=CARTESIAN_POINT('Ctrl Pts',(57.893332219512,29.0621332674915,17.5910613120929));
#58322=CARTESIAN_POINT('Ctrl Pts',(56.6272513453282,26.6068253439157,17.4643584817274));
#58323=CARTESIAN_POINT('Ctrl Pts',(53.8784216692723,26.3321743078981,17.3376556513621));
#58324=CARTESIAN_POINT('Ctrl Pts',(52.624400967416,27.898034156911,17.2456453228568));
#58325=CARTESIAN_POINT('Ctrl Pts',(52.5468627294195,28.8530496528172,17.1958692711402));
#58326=CARTESIAN_POINT('Ctrl Pts',(52.5481572452887,28.9979575612485,17.1883274962121));
#58327=CARTESIAN_POINT('',(52.549500001991,28.9999012170075,16.3883274962515));
#58328=CARTESIAN_POINT('Ctrl Pts',(52.5495008502318,28.9979586805009,17.1883274962121));
#58329=CARTESIAN_POINT('Ctrl Pts',(52.5494314790664,29.0812351994276,17.1839909334796));
#58330=CARTESIAN_POINT('Ctrl Pts',(52.5536121190673,29.1646579537596,17.179654370747));
#58331=CARTESIAN_POINT('Ctrl Pts',(52.5620561956239,29.247750391935,17.1753178080145));
#58332=CARTESIAN_POINT('Ctrl Pts',(52.5701546732359,29.3274420249732,17.1711587320081));
#58333=CARTESIAN_POINT('Ctrl Pts',(52.5821743818546,29.4068293158971,17.1669996560017));
#58334=CARTESIAN_POINT('Ctrl Pts',(52.5980740820284,29.4854916421281,17.1628405799952));
#58335=CARTESIAN_POINT('Ctrl Pts',(52.6139649341711,29.5641101935265,17.1586838184749));
#58336=CARTESIAN_POINT('Ctrl Pts',(52.6337314001425,29.6420041114002,17.1545270569545));
#58337=CARTESIAN_POINT('Ctrl Pts',(52.6572807298755,29.7187605104534,17.1503702954342));
#58338=CARTESIAN_POINT('Ctrl Pts',(52.6808246581083,29.7954993039226,17.1462144873485));
#58339=CARTESIAN_POINT('Ctrl Pts',(52.7081495867769,29.8711006382324,17.1420586792628));
#58340=CARTESIAN_POINT('Ctrl Pts',(52.739112672509,29.9451659866872,17.1379028711772));
#58341=CARTESIAN_POINT('Ctrl Pts',(52.7700787847425,30.0192385746946,17.1337466568801));
#58342=CARTESIAN_POINT('Ctrl Pts',(52.8046835721578,30.0917744375175,17.129590442583));
#58343=CARTESIAN_POINT('Ctrl Pts',(52.8427363862768,30.1623957806642,17.1254342282859));
#58344=CARTESIAN_POINT('Ctrl Pts',(52.880828258598,30.2330896110309,17.1212737479638));
#58345=CARTESIAN_POINT('Ctrl Pts',(52.9223749893459,30.3018645791274,17.1171132676416));
#58346=CARTESIAN_POINT('Ctrl Pts',(52.9671408046875,30.3683690079921,17.1129527873195));
#58347=CARTESIAN_POINT('Ctrl Pts',(53.0119338967066,30.4349139592923,17.1087897719361));
#58348=CARTESIAN_POINT('Ctrl Pts',(53.0599496859862,30.4991852374112,17.1046267565528));
#58349=CARTESIAN_POINT('Ctrl Pts',(53.1109116253203,30.5608636592124,17.1004637411695));
#58350=CARTESIAN_POINT('Ctrl Pts',(53.1619539794875,30.6226394058027,17.0962941568017));
#58351=CARTESIAN_POINT('Ctrl Pts',(53.2159514314526,30.6818137848235,17.092124572434));
#58352=CARTESIAN_POINT('Ctrl Pts',(53.2725906863439,30.7381045173102,17.0879549880662));
#58353=CARTESIAN_POINT('Ctrl Pts',(53.2893668024256,30.7547774037091,17.0867199889211));
#58354=CARTESIAN_POINT('Ctrl Pts',(53.3063744677791,30.771197581093,17.0854849897761));
#58355=CARTESIAN_POINT('Ctrl Pts',(53.3236050203222,30.7873584201584,17.0842499906311));
#58356=CARTESIAN_POINT('Ctrl Pts',(53.3826579202126,30.8427451762758,17.0800173764596));
#58357=CARTESIAN_POINT('Ctrl Pts',(53.4445684874815,30.895305198464,17.0757847622881));
#58358=CARTESIAN_POINT('Ctrl Pts',(53.5090351101451,30.9447297877134,17.0715521481166));
#58359=CARTESIAN_POINT('Ctrl Pts',(53.5734097772245,30.994083877427,17.0673255713719));
#58360=CARTESIAN_POINT('Ctrl Pts',(53.6403328927217,31.0403111366677,17.0630989946271));
#58361=CARTESIAN_POINT('Ctrl Pts',(53.7094671982809,31.0831407388093,17.0588724178823));
#58362=CARTESIAN_POINT('Ctrl Pts',(53.7785247727665,31.1259228050521,17.0546505321483));
#58363=CARTESIAN_POINT('Ctrl Pts',(53.8497882679766,31.1653144637599,17.0504286464142));
#58364=CARTESIAN_POINT('Ctrl Pts',(53.9228897943695,31.2010869712318,17.0462067606802));
#58365=CARTESIAN_POINT('Ctrl Pts',(53.9959420160496,31.2368353512569,17.0419877224772));
#58366=CARTESIAN_POINT('Ctrl Pts',(54.0708293905801,31.2689692244317,17.0377686842742));
#58367=CARTESIAN_POINT('Ctrl Pts',(54.1471587699883,31.2973053968491,17.0335496460711));
#58368=CARTESIAN_POINT('Ctrl Pts',(54.223463223004,31.3256323157057,17.0293319856522));
#58369=CARTESIAN_POINT('Ctrl Pts',(54.3012083105334,31.3501638351956,17.0251143252332));
#58370=CARTESIAN_POINT('Ctrl Pts',(54.3799814924724,31.3707651297257,17.0208966648142));
#58371=CARTESIAN_POINT('Ctrl Pts',(54.4587530351714,31.3913659955506,17.0166790921632));
#58372=CARTESIAN_POINT('Ctrl Pts',(54.5385521800133,31.4080366826258,17.0124615195121));
#58373=CARTESIAN_POINT('Ctrl Pts',(54.6189532264553,31.4206927947121,17.0082439468611));
#58374=CARTESIAN_POINT('Ctrl Pts',(54.6994907581661,31.4333703912559,17.0040192146448));
#58375=CARTESIAN_POINT('Ctrl Pts',(54.7806317744697,31.4420197050398,16.9997944824285));
#58376=CARTESIAN_POINT('Ctrl Pts',(54.8619420234416,31.4466079058788,16.9955697502122));
#58377=CARTESIAN_POINT('Ctrl Pts',(54.9432319643261,31.4511949607665,16.9913460731671));
#58378=CARTESIAN_POINT('Ctrl Pts',(55.0246905870729,31.4517229492961,16.987122396122));
#58379=CARTESIAN_POINT('Ctrl Pts',(55.1058845752201,31.4482113280374,16.9828987190769));
#58380=CARTESIAN_POINT('Ctrl Pts',(55.1872258777314,31.4446933354664,16.9786673788007));
#58381=CARTESIAN_POINT('Ctrl Pts',(55.2683011222209,31.4371211291395,16.9744360385244));
#58382=CARTESIAN_POINT('Ctrl Pts',(55.3486822258607,31.4255661102862,16.9702046982482));
#58383=CARTESIAN_POINT('Ctrl Pts',(55.4288323127503,31.4140443007667,16.9659855189207));
#58384=CARTESIAN_POINT('Ctrl Pts',(55.5082918124677,31.3985627102043,16.9617663395931));
#58385=CARTESIAN_POINT('Ctrl Pts',(55.5866505546961,31.3792417650745,16.9575471602656));
#58386=CARTESIAN_POINT('Ctrl Pts',(55.6652588093043,31.3598592975815,16.9533145460941));
#58387=CARTESIAN_POINT('Ctrl Pts',(55.7430516446065,31.3365408703696,16.9490819319227));
#58388=CARTESIAN_POINT('Ctrl Pts',(55.8196059182785,31.3093714271903,16.9448493177512));
#58389=CARTESIAN_POINT('Ctrl Pts',(55.8960509944673,31.2822407386705,16.9406227410064));
#58390=CARTESIAN_POINT('Ctrl Pts',(55.9712605837468,31.2512700982966,16.9363961642616));
#58391=CARTESIAN_POINT('Ctrl Pts',(56.0448239061901,31.216594968652,16.9321695875168));
#58392=CARTESIAN_POINT('Ctrl Pts',(56.1183055818639,31.1819583243861,16.9279477017828));
#58393=CARTESIAN_POINT('Ctrl Pts',(56.1901442031871,31.1436255575711,16.9237258160488));
#58394=CARTESIAN_POINT('Ctrl Pts',(56.2599476148098,31.1017807349805,16.9195039303147));
#58395=CARTESIAN_POINT('Ctrl Pts',(56.329703946196,31.0599641354251,16.9152848921117));
#58396=CARTESIAN_POINT('Ctrl Pts',(56.397427396743,31.0146404229193,16.9110658539087));
#58397=CARTESIAN_POINT('Ctrl Pts',(56.4627502687065,30.9660396489896,16.9068468157057));
#58398=CARTESIAN_POINT('Ctrl Pts',(56.5280518086015,30.9174547463009,16.9026291552867));
#58399=CARTESIAN_POINT('Ctrl Pts',(56.5909539543505,30.8655951845633,16.8984114948677));
#58400=CARTESIAN_POINT('Ctrl Pts',(56.6511190236793,30.8107336136617,16.8941938344488));
#58401=CARTESIAN_POINT('Ctrl Pts',(56.7112828409957,30.7558731844087,16.8899762617977));
#58402=CARTESIAN_POINT('Ctrl Pts',(56.7687093526638,30.6980111840744,16.8857586891467));
#58403=CARTESIAN_POINT('Ctrl Pts',(56.8230960132702,30.6374587556327,16.8815411164956));
#58404=CARTESIAN_POINT('Ctrl Pts',(56.8775749982719,30.5768035360603,16.8773163842793));
#58405=CARTESIAN_POINT('Ctrl Pts',(56.9290034955704,30.513449098005,16.8730916520631));
#58406=CARTESIAN_POINT('Ctrl Pts',(56.9771175592805,30.4477418301565,16.8688669198468));
#58407=CARTESIAN_POINT('Ctrl Pts',(57.0252196059986,30.3820509733872,16.8646432428017));
#58408=CARTESIAN_POINT('Ctrl Pts',(57.0700086359976,30.3140088630182,16.8604195657566));
#58409=CARTESIAN_POINT('Ctrl Pts',(57.1112650721079,30.2439895680017,16.8561958887114));
#58410=CARTESIAN_POINT('Ctrl Pts',(57.1525963618593,30.1738432334328,16.8519645484352));
#58411=CARTESIAN_POINT('Ctrl Pts',(57.1903820326334,30.101712957807,16.847733208159));
#58412=CARTESIAN_POINT('Ctrl Pts',(57.224448928946,30.0279966986867,16.8435018678827));
#58413=CARTESIAN_POINT('Ctrl Pts',(57.2584179163805,29.9544923014329,16.8392826885552));
#58414=CARTESIAN_POINT('Ctrl Pts',(57.2886893833677,29.8794114781285,16.8350635092277));
#58415=CARTESIAN_POINT('Ctrl Pts',(57.3151410496224,29.803163850253,16.8308443299002));
#58416=CARTESIAN_POINT('Ctrl Pts',(57.3416769441076,29.7266734322744,16.8266117157287));
#58417=CARTESIAN_POINT('Ctrl Pts',(57.364467341359,29.6487242689363,16.8223791015573));
#58418=CARTESIAN_POINT('Ctrl Pts',(57.3833531353155,29.5697175461417,16.8181464873858));
#58419=CARTESIAN_POINT('Ctrl Pts',(57.4022119904603,29.4908235190188,16.813919910641));
#58420=CARTESIAN_POINT('Ctrl Pts',(57.4171771970483,29.4108753765981,16.8096933338962));
#58421=CARTESIAN_POINT('Ctrl Pts',(57.4281387555884,29.330291437385,16.8054667571514));
#58422=CARTESIAN_POINT('Ctrl Pts',(57.4390881480678,29.2497969370128,16.8012448714174));
#58423=CARTESIAN_POINT('Ctrl Pts',(57.4460426595963,29.1686684999841,16.7970229856834));
#58424=CARTESIAN_POINT('Ctrl Pts',(57.4489432003383,29.0873352821995,16.7928010999493));
#58425=CARTESIAN_POINT('Ctrl Pts',(57.4518417847555,29.0060569211481,16.7885820617463));
#58426=CARTESIAN_POINT('Ctrl Pts',(57.4506918123866,28.924574516711,16.7843630235433));
#58427=CARTESIAN_POINT('Ctrl Pts',(57.4454860813073,28.8433217432689,16.7801439853403));
#58428=CARTESIAN_POINT('Ctrl Pts',(57.44028205023,28.7620955040202,16.7759263249213));
#58429=CARTESIAN_POINT('Ctrl Pts',(57.4310249204237,28.6810992100852,16.7717086645023));
#58430=CARTESIAN_POINT('Ctrl Pts',(57.4177595629877,28.6007645486916,16.7674910040833));
#58431=CARTESIAN_POINT('Ctrl Pts',(57.4044944815989,28.5204315590319,16.7632734314323));
#58432=CARTESIAN_POINT('Ctrl Pts',(57.3872214152632,28.4407606326884,16.7590558587812));
#58433=CARTESIAN_POINT('Ctrl Pts',(57.3660366525896,28.3621749388721,16.7548382861302));
#58434=CARTESIAN_POINT('Ctrl Pts',(57.3448159275976,28.2834558414496,16.7506135539139));
#58435=CARTESIAN_POINT('Ctrl Pts',(57.3196703420827,28.2058261133501,16.7463888216976));
#58436=CARTESIAN_POINT('Ctrl Pts',(57.2907467632637,28.1296957333227,16.7421640894813));
#58437=CARTESIAN_POINT('Ctrl Pts',(57.2618304084119,28.0535843676561,16.7379404124362));
#58438=CARTESIAN_POINT('Ctrl Pts',(57.2291381537515,27.9789720196369,16.7337167353911));
#58439=CARTESIAN_POINT('Ctrl Pts',(57.1928642397683,27.9062465195734,16.729493058346));
#58440=CARTESIAN_POINT('Ctrl Pts',(57.1565245121863,27.8333890699528,16.7252617180697));
#58441=CARTESIAN_POINT('Ctrl Pts',(57.1165903669661,27.7624257158661,16.7210303777935));
#58442=CARTESIAN_POINT('Ctrl Pts',(57.0733013549653,27.6937183529197,16.7167990375172));
#58443=CARTESIAN_POINT('Ctrl Pts',(57.0301367563706,27.6252084561811,16.7125798581897));
#58444=CARTESIAN_POINT('Ctrl Pts',(56.9836368787229,27.5589419252595,16.7083606788622));
#58445=CARTESIAN_POINT('Ctrl Pts',(56.9340787533669,27.4952443302068,16.7041414995347));
#58446=CARTESIAN_POINT('Ctrl Pts',(56.8843628234641,27.4313439072617,16.6999088853632));
#58447=CARTESIAN_POINT('Ctrl Pts',(56.8313842094394,27.3697911597357,16.6956762711918));
#58448=CARTESIAN_POINT('Ctrl Pts',(56.7753928186813,27.3109379557355,16.6914436570203));
#58449=CARTESIAN_POINT('Ctrl Pts',(56.7194812943846,27.2521687003047,16.6872170802755));
#58450=CARTESIAN_POINT('Ctrl Pts',(56.6605658461699,27.196091674292,16.6829905035307));
#58451=CARTESIAN_POINT('Ctrl Pts',(56.5989374863409,27.1430268809771,16.6787639267859));
#58452=CARTESIAN_POINT('Ctrl Pts',(56.537377526855,27.090020983438,16.6745420410519));
#58453=CARTESIAN_POINT('Ctrl Pts',(56.4731109888984,27.0400209771942,16.6703201553179));
#58454=CARTESIAN_POINT('Ctrl Pts',(56.4064656907128,26.9933100611087,16.6660982695838));
#58455=CARTESIAN_POINT('Ctrl Pts',(56.3398653427142,26.9466306500875,16.6618792313808));
#58456=CARTESIAN_POINT('Ctrl Pts',(56.2708898003976,26.9032361892494,16.6576601931778));
#58457=CARTESIAN_POINT('Ctrl Pts',(56.1998989200406,26.8633688124327,16.6534411549748));
#58458=CARTESIAN_POINT('Ctrl Pts',(56.1289312227169,26.8235144548477,16.6492234945558));
#58459=CARTESIAN_POINT('Ctrl Pts',(56.0559498991074,26.78718512114,16.6450058341369));
#58460=CARTESIAN_POINT('Ctrl Pts',(55.9813414872116,26.7545781831742,16.6407881737179));
#58461=CARTESIAN_POINT('Ctrl Pts',(55.9067346278885,26.7219719237464,16.6365706010668));
#58462=CARTESIAN_POINT('Ctrl Pts',(55.8305011737406,26.6930880910062,16.6323530284158));
#58463=CARTESIAN_POINT('Ctrl Pts',(55.7530485093739,26.668076289299,16.6281354557647));
#58464=CARTESIAN_POINT('Ctrl Pts',(55.6754643647819,26.6430220286609,16.6239107235484));
#58465=CARTESIAN_POINT('Ctrl Pts',(55.5966573134268,26.6218530935813,16.6196859913322));
#58466=CARTESIAN_POINT('Ctrl Pts',(55.5170512104585,26.6046694808934,16.6154612591159));
#58467=CARTESIAN_POINT('Ctrl Pts',(55.4374649899492,26.5874901599931,16.6112375820708));
#58468=CARTESIAN_POINT('Ctrl Pts',(55.3570805803588,26.5742942255241,16.6070139050257));
#58469=CARTESIAN_POINT('Ctrl Pts',(55.2763290482109,26.5651298787995,16.6027902279805));
#58470=CARTESIAN_POINT('Ctrl Pts',(55.1954310044693,26.5559489047366,16.5985588877043));
#58471=CARTESIAN_POINT('Ctrl Pts',(55.1141649719844,26.5508141660023,16.5943275474281));
#58472=CARTESIAN_POINT('Ctrl Pts',(55.0329649296005,26.5497217375538,16.5900962071518));
#58473=CARTESIAN_POINT('Ctrl Pts',(54.9519982576119,26.5486324487644,16.5858770278243));
#58474=CARTESIAN_POINT('Ctrl Pts',(54.8710976488593,26.5515621663447,16.5816578484968));
#58475=CARTESIAN_POINT('Ctrl Pts',(54.7906870158031,26.5584557500126,16.5774386691693));
#58476=CARTESIAN_POINT('Ctrl Pts',(54.7100203366712,26.5653712844472,16.5732060549978));
#58477=CARTESIAN_POINT('Ctrl Pts',(54.6295467390401,26.5763017170233,16.5689734408263));
#58478=CARTESIAN_POINT('Ctrl Pts',(54.5496974285382,26.5912289764,16.5647408266549));
#58479=CARTESIAN_POINT('Ctrl Pts',(54.4699620155803,26.6061349434429,16.5605142499101));
#58480=CARTESIAN_POINT('Ctrl Pts',(54.3908495739733,26.6250263295152,16.5562876731653));
#58481=CARTESIAN_POINT('Ctrl Pts',(54.3127869578739,26.6478332361987,16.5520610964205));
#58482=CARTESIAN_POINT('Ctrl Pts',(54.2348109822389,26.6706148298567,16.5478392106865));
#58483=CARTESIAN_POINT('Ctrl Pts',(54.1578829605515,26.6973031794606,16.5436173249524));
#58484=CARTESIAN_POINT('Ctrl Pts',(54.0824189116775,26.7277774764885,16.5393954392184));
#58485=CARTESIAN_POINT('Ctrl Pts',(54.0070057609643,26.7582312195481,16.5351764010154));
#58486=CARTESIAN_POINT('Ctrl Pts',(53.9330550516337,26.7924656650499,16.5309573628124));
#58487=CARTESIAN_POINT('Ctrl Pts',(53.8609657977053,26.8303107743267,16.5267383246093));
#58488=CARTESIAN_POINT('Ctrl Pts',(53.788900085499,26.8681435247706,16.5225206641903));
#58489=CARTESIAN_POINT('Ctrl Pts',(53.7186950324747,26.9095843815824,16.5183030037714));
#58490=CARTESIAN_POINT('Ctrl Pts',(53.6507266307302,26.9544165563392,16.5140853433524));
#58491=CARTESIAN_POINT('Ctrl Pts',(53.5827596433824,26.9992477981553,16.5098677707014));
#58492=CARTESIAN_POINT('Ctrl Pts',(53.5170296019134,27.0474699608352,16.5056501980503));
#58493=CARTESIAN_POINT('Ctrl Pts',(53.45388377873,27.0988227646204,16.5014326253993));
#58494=CARTESIAN_POINT('Ctrl Pts',(53.3906307619834,27.1502627426593,16.497207893183));
#58495=CARTESIAN_POINT('Ctrl Pts',(53.3299711029042,27.2048437001086,16.4929831609667));
#58496=CARTESIAN_POINT('Ctrl Pts',(53.2722194284441,27.2622645349324,16.4887584287504));
#58497=CARTESIAN_POINT('Ctrl Pts',(53.2144821780702,27.3196710283005,16.4845347517053));
#58498=CARTESIAN_POINT('Ctrl Pts',(53.1596517579463,27.3799156215909,16.4803110746602));
#58499=CARTESIAN_POINT('Ctrl Pts',(53.1080032735126,27.4426629661628,16.4760873976151));
#58500=CARTESIAN_POINT('Ctrl Pts',(53.0562610806182,27.5055241564192,16.4718560573388));
#58501=CARTESIAN_POINT('Ctrl Pts',(53.007712638625,27.570896798692,16.4676247170626));
#58502=CARTESIAN_POINT('Ctrl Pts',(52.9625909135407,27.6384147237822,16.4633933767863));
#58503=CARTESIAN_POINT('Ctrl Pts',(52.9175988691131,27.7057386011304,16.4591741974588));
#58504=CARTESIAN_POINT('Ctrl Pts',(52.8760140334964,27.7751950132776,16.4549550181313));
#58505=CARTESIAN_POINT('Ctrl Pts',(52.8380209319162,27.8463983533439,16.4507358388038));
#58506=CARTESIAN_POINT('Ctrl Pts',(52.7978259282973,27.921728305167,16.4462721356239));
#58507=CARTESIAN_POINT('Ctrl Pts',(52.7615146012321,27.9992682907874,16.441808432444));
#58508=CARTESIAN_POINT('Ctrl Pts',(52.7293216506219,28.0786042741223,16.4373447292641));
#58509=CARTESIAN_POINT('Ctrl Pts',(52.6972217088438,28.1577110474281,16.4328939221938));
#58510=CARTESIAN_POINT('Ctrl Pts',(52.6692165851757,28.2386031219828,16.4284431151235));
#58511=CARTESIAN_POINT('Ctrl Pts',(52.6454942862122,28.3208438370001,16.4239923080532));
#58512=CARTESIAN_POINT('Ctrl Pts',(52.6218134302734,28.4029408769049,16.4195492765744));
#58513=CARTESIAN_POINT('Ctrl Pts',(52.6024006204135,28.4863814977593,16.4151062450956));
#58514=CARTESIAN_POINT('Ctrl Pts',(52.5873954735558,28.5707102971405,16.4106632136169));
#58515=CARTESIAN_POINT('Ctrl Pts',(52.5724246591913,28.6548461481984,16.4062303480064));
#58516=CARTESIAN_POINT('Ctrl Pts',(52.5618414865605,28.7398657476831,16.401797482396));
#58517=CARTESIAN_POINT('Ctrl Pts',(52.5557351608016,28.8253012711598,16.3973646167856));
#58518=CARTESIAN_POINT('Ctrl Pts',(52.5515855800147,28.883359360547,16.3943522432743));
#58519=CARTESIAN_POINT('Ctrl Pts',(52.5495023518216,28.9416092003001,16.3913398697629));
#58520=CARTESIAN_POINT('Ctrl Pts',(52.549500001991,28.9999012170075,16.3883274962515));
#58521=CARTESIAN_POINT('',(52.549500910706,29.0021126687846,15.5883274962626));
#58522=CARTESIAN_POINT('Ctrl Pts',(52.549500001991,28.9999012177705,16.3883274962121));
#58523=CARTESIAN_POINT('Ctrl Pts',(52.5494965672996,29.0851059289342,16.3839243475573));
#58524=CARTESIAN_POINT('Ctrl Pts',(52.5539413361584,29.1702316435544,16.3795211989024));
#58525=CARTESIAN_POINT('Ctrl Pts',(52.5627838559111,29.2548091776064,16.3751180502476));
#58526=CARTESIAN_POINT('Ctrl Pts',(52.5716489821169,29.3396029393975,16.3707036446687));
#58527=CARTESIAN_POINT('Ctrl Pts',(52.5849342869729,29.423845318605,16.3662892390898));
#58528=CARTESIAN_POINT('Ctrl Pts',(52.6025376868597,29.5070746563101,16.3618748335109));
#58529=CARTESIAN_POINT('Ctrl Pts',(52.62016388412,29.5904117805969,16.3574547110334));
#58530=CARTESIAN_POINT('Ctrl Pts',(52.6421192227754,29.6727328593025,16.3530345885559));
#58531=CARTESIAN_POINT('Ctrl Pts',(52.6682516765415,29.753591405238,16.3486144660783));
#58532=CARTESIAN_POINT('Ctrl Pts',(52.6944539806234,29.8346660807041,16.3441825289066));
#58533=CARTESIAN_POINT('Ctrl Pts',(52.7248555799906,29.9142700303812,16.3397505917348));
#58534=CARTESIAN_POINT('Ctrl Pts',(52.7592558778403,29.9919758207773,16.3353186545631));
#58535=CARTESIAN_POINT('Ctrl Pts',(52.7884552680145,30.0579334384259,16.3315567725215));
#58536=CARTESIAN_POINT('Ctrl Pts',(52.8205347695802,30.1225237429707,16.3277948904799));
#58537=CARTESIAN_POINT('Ctrl Pts',(52.8553466886114,30.1855009168913,16.3240330084383));
#58538=CARTESIAN_POINT('Ctrl Pts',(52.8945146955292,30.2563585556664,16.3198003942668));
#58539=CARTESIAN_POINT('Ctrl Pts',(52.9372709326651,30.3254047609059,16.3155677800953));
#58540=CARTESIAN_POINT('Ctrl Pts',(52.9834232843317,30.3922530660137,16.3113351659239));
#58541=CARTESIAN_POINT('Ctrl Pts',(53.0295098040021,30.459006018291,16.3071085891791));
#58542=CARTESIAN_POINT('Ctrl Pts',(53.0789825551811,30.5235669180335,16.3028820124343));
#58543=CARTESIAN_POINT('Ctrl Pts',(53.131603859933,30.5855743797699,16.2986554356895));
#58544=CARTESIAN_POINT('Ctrl Pts',(53.1841667611299,30.6475130204039,16.2944335499555));
#58545=CARTESIAN_POINT('Ctrl Pts',(53.2398709732091,30.7069035018126,16.2902116642214));
#58546=CARTESIAN_POINT('Ctrl Pts',(53.2984367340434,30.763415067971,16.2859897784874));
#58547=CARTESIAN_POINT('Ctrl Pts',(53.3569629940884,30.8198885188307,16.2817707402844));
#58548=CARTESIAN_POINT('Ctrl Pts',(53.4183466362554,30.8734865891656,16.2775517020814));
#58549=CARTESIAN_POINT('Ctrl Pts',(53.4822698611413,30.9239141029682,16.2733326638783));
#58550=CARTESIAN_POINT('Ctrl Pts',(53.5461722110325,30.9743251489833,16.2691150034594));
#58551=CARTESIAN_POINT('Ctrl Pts',(53.6126121321914,31.0215674071835,16.2648973430404));
#58552=CARTESIAN_POINT('Ctrl Pts',(53.6812385038008,31.0653857669071,16.2606796826214));
#58553=CARTESIAN_POINT('Ctrl Pts',(53.7498634473213,31.1092032147872,16.2564621099704));
#58554=CARTESIAN_POINT('Ctrl Pts',(53.8206743586554,31.1495966568427,16.2522445373193));
#58555=CARTESIAN_POINT('Ctrl Pts',(53.8932920919819,31.1863549246017,16.2480269646683));
#58556=CARTESIAN_POINT('Ctrl Pts',(53.9660330979681,31.2231755915741,16.243802232452));
#58557=CARTESIAN_POINT('Ctrl Pts',(54.0405866460044,31.2563485267905,16.2395775002357));
#58558=CARTESIAN_POINT('Ctrl Pts',(54.1165496017435,31.2857090024368,16.2353527680194));
#58559=CARTESIAN_POINT('Ctrl Pts',(54.192493584938,31.3150621449964,16.2311290909743));
#58560=CARTESIAN_POINT('Ctrl Pts',(54.2698458225861,31.3406046061649,16.2269054139292));
#58561=CARTESIAN_POINT('Ctrl Pts',(54.3481879977817,31.3622217008071,16.2226817368841));
#58562=CARTESIAN_POINT('Ctrl Pts',(54.4266723131526,31.3838780164388,16.2184503966079));
#58563=CARTESIAN_POINT('Ctrl Pts',(54.5061497007664,31.4015946311211,16.2142190563316));
#58564=CARTESIAN_POINT('Ctrl Pts',(54.5861908563781,31.4153078981064,16.2099877160554));
#58565=CARTESIAN_POINT('Ctrl Pts',(54.6660019722557,31.4289817529133,16.2057685367279));
#58566=CARTESIAN_POINT('Ctrl Pts',(54.7463731579651,31.4386752687481,16.2015493574004));
#58567=CARTESIAN_POINT('Ctrl Pts',(54.8268770843264,31.4443769566228,16.1973301780729));
#58568=CARTESIAN_POINT('Ctrl Pts',(54.9076373538314,31.4500967999921,16.1930975639015));
#58569=CARTESIAN_POINT('Ctrl Pts',(54.9888315826127,31.4518205994553,16.18886494973));
#58570=CARTESIAN_POINT('Ctrl Pts',(55.0700310048049,31.4494991137712,16.1846323355585));
#58571=CARTESIAN_POINT('Ctrl Pts',(55.1511146036455,31.4471809394685,16.1804057588137));
#58572=CARTESIAN_POINT('Ctrl Pts',(55.2322029206835,31.4408289535834,16.1761791820689));
#58573=CARTESIAN_POINT('Ctrl Pts',(55.312863424609,31.4304457878221,16.1719526053242));
#58574=CARTESIAN_POINT('Ctrl Pts',(55.3934344047154,31.4200741461724,16.1677307195901));
#58575=CARTESIAN_POINT('Ctrl Pts',(55.4735780567573,31.4056802737708,16.1635088338561));
#58576=CARTESIAN_POINT('Ctrl Pts',(55.5528646315092,31.3873187783005,16.1592869481221));
#58577=CARTESIAN_POINT('Ctrl Pts',(55.6320977299251,31.3689696670896,16.1550679099191));
#58578=CARTESIAN_POINT('Ctrl Pts',(55.7104744477495,31.3466583521943,16.1508488717161));
#58579=CARTESIAN_POINT('Ctrl Pts',(55.7875741736494,31.3204907177148,16.146629833513));
#58580=CARTESIAN_POINT('Ctrl Pts',(55.8646487215899,31.2943316286306,16.1424121730941));
#58581=CARTESIAN_POINT('Ctrl Pts',(55.940446666215,31.2643188701095,16.1381945126751));
#58582=CARTESIAN_POINT('Ctrl Pts',(56.01456286381,31.2306080887008,16.1339768522561));
#58583=CARTESIAN_POINT('Ctrl Pts',(56.088677519075,31.1968980088007,16.1297592796051));
#58584=CARTESIAN_POINT('Ctrl Pts',(56.1611100745158,31.1594902524207,16.125541706954));
#58585=CARTESIAN_POINT('Ctrl Pts',(56.2314769894,31.1185878963541,16.121324134303));
#58586=CARTESIAN_POINT('Ctrl Pts',(56.301963356054,31.0776161062527,16.1170994020867));
#58587=CARTESIAN_POINT('Ctrl Pts',(56.3703766626418,31.033138082045,16.1128746698704));
#58588=CARTESIAN_POINT('Ctrl Pts',(56.4363592646534,30.9854023050365,16.1086499376541));
#58589=CARTESIAN_POINT('Ctrl Pts',(56.5023253868182,30.937678450539,16.104426260609));
#58590=CARTESIAN_POINT('Ctrl Pts',(56.5658616681585,30.8866987786574,16.1002025835639));
#58591=CARTESIAN_POINT('Ctrl Pts',(56.6266441758287,30.8327517494856,16.0959789065188));
#58592=CARTESIAN_POINT('Ctrl Pts',(56.6875369642803,30.7787068414873,16.0917475662425));
#58593=CARTESIAN_POINT('Ctrl Pts',(56.7456656615169,30.7216841430657,16.0875162259663));
#58594=CARTESIAN_POINT('Ctrl Pts',(56.8007431654636,30.662009116111,16.08328488569));
#58595=CARTESIAN_POINT('Ctrl Pts',(56.8556623756647,30.6025055962665,16.0790657063625));
#58596=CARTESIAN_POINT('Ctrl Pts',(56.9075476795902,30.5403653759723,16.074846527035));
#58597=CARTESIAN_POINT('Ctrl Pts',(56.9561568016372,30.4759406551106,16.0706273477075));
#58598=CARTESIAN_POINT('Ctrl Pts',(57.0049207063848,30.4113107910195,16.066394733536));
#58599=CARTESIAN_POINT('Ctrl Pts',(57.0505688764742,30.3441414614153,16.0621621193645));
#58600=CARTESIAN_POINT('Ctrl Pts',(57.092826586627,30.2747655189514,16.0579295051931));
#58601=CARTESIAN_POINT('Ctrl Pts',(57.1350240201241,30.2054885347552,16.0537029284483));
#58602=CARTESIAN_POINT('Ctrl Pts',(57.1738403592937,30.1340115825381,16.0494763517035));
#58603=CARTESIAN_POINT('Ctrl Pts',(57.2090423412836,30.0606989131776,16.0452497749587));
#58604=CARTESIAN_POINT('Ctrl Pts',(57.2442052531498,29.9874676123909,16.0410278892247));
#58605=CARTESIAN_POINT('Ctrl Pts',(57.2757615786477,29.9124050595007,16.0368060034906));
#58606=CARTESIAN_POINT('Ctrl Pts',(57.3035231682552,29.8359014674657,16.0325841177566));
#58607=CARTESIAN_POINT('Ctrl Pts',(57.3312660335314,29.7594494747312,16.0283650795536));
#58608=CARTESIAN_POINT('Ctrl Pts',(57.3552190881166,29.6815588087606,16.0241460413506));
#58609=CARTESIAN_POINT('Ctrl Pts',(57.3752421691163,29.6026399323407,16.0199270031475));
#58610=CARTESIAN_POINT('Ctrl Pts',(57.3952587113078,29.5237468279485,16.0157093427286));
#58611=CARTESIAN_POINT('Ctrl Pts',(57.4113477144833,29.4438266298739,16.0114916823096));
#58612=CARTESIAN_POINT('Ctrl Pts',(57.42341917833,29.3633039169929,16.0072740218906));
#58613=CARTESIAN_POINT('Ctrl Pts',(57.4354903909741,29.2827828797592,16.0030564492396));
#58614=CARTESIAN_POINT('Ctrl Pts',(57.4435441628035,29.2016598122362,15.9988388765885));
#58615=CARTESIAN_POINT('Ctrl Pts',(57.4475420398717,29.1203669932358,15.9946213039375));
#58616=CARTESIAN_POINT('Ctrl Pts',(57.4515467035597,29.0389361751326,15.9903965717212));
#58617=CARTESIAN_POINT('Ctrl Pts',(57.4514816740545,28.9573354954365,15.9861718395049));
#58618=CARTESIAN_POINT('Ctrl Pts',(57.4473606817844,28.876000228808,15.9819471072886));
#58619=CARTESIAN_POINT('Ctrl Pts',(57.4432407187754,28.7946852765152,15.9777234302435));
#58620=CARTESIAN_POINT('Ctrl Pts',(57.4350668867047,28.7136360663957,15.9734997531984));
#58621=CARTESIAN_POINT('Ctrl Pts',(57.4229048038741,28.6332813593999,15.9692760761533));
#58622=CARTESIAN_POINT('Ctrl Pts',(57.4107206547609,28.5527808607906,15.965044735877));
#58623=CARTESIAN_POINT('Ctrl Pts',(57.3945338864326,28.472977840116,15.9608133956008));
#58624=CARTESIAN_POINT('Ctrl Pts',(57.3744612059323,28.3942903075546,15.9565820553245));
#58625=CARTESIAN_POINT('Ctrl Pts',(57.3544462146801,28.3158289243897,15.952362875997));
#58626=CARTESIAN_POINT('Ctrl Pts',(57.3305678315509,28.2384770364956,15.9481436966695));
#58627=CARTESIAN_POINT('Ctrl Pts',(57.3029895956575,28.1626296086599,15.943924517342));
#58628=CARTESIAN_POINT('Ctrl Pts',(57.2753235442751,28.0865406650506,15.9396919031705));
#58629=CARTESIAN_POINT('Ctrl Pts',(57.2438311166961,28.0116827912019,15.9354592889991));
#58630=CARTESIAN_POINT('Ctrl Pts',(57.2086419574601,27.9384676388604,15.9312266748276));
#58631=CARTESIAN_POINT('Ctrl Pts',(57.1735029922558,27.8653569210592,15.9270000980828));
#58632=CARTESIAN_POINT('Ctrl Pts',(57.134677967898,27.7938846861118,15.922773521338));
#58633=CARTESIAN_POINT('Ctrl Pts',(57.0923454387272,27.7244448992547,15.9185469445932));
#58634=CARTESIAN_POINT('Ctrl Pts',(57.0500598937618,27.6550821825201,15.9143250588592));
#58635=CARTESIAN_POINT('Ctrl Pts',(57.0042748198077,27.5877478262943,15.9101031731252));
#58636=CARTESIAN_POINT('Ctrl Pts',(56.9552151085869,27.5228120873925,15.9058812873912));
#58637=CARTESIAN_POINT('Ctrl Pts',(56.9061884866198,27.4579201456329,15.9016622491881));
#58638=CARTESIAN_POINT('Ctrl Pts',(56.8538918932527,27.3954239778184,15.8974432109851));
#58639=CARTESIAN_POINT('Ctrl Pts',(56.7985933302329,27.3356646123928,15.8932241727821));
#58640=CARTESIAN_POINT('Ctrl Pts',(56.7433128257078,27.2759247621973,15.8890065123631));
#58641=CARTESIAN_POINT('Ctrl Pts',(56.6850326136842,27.2189202801812,15.8847888519442));
#58642=CARTESIAN_POINT('Ctrl Pts',(56.6240598453912,27.1649578019598,15.8805711915252));
#58643=CARTESIAN_POINT('Ctrl Pts',(56.5630883459184,27.1109964466773,15.8763536188742));
#58644=CARTESIAN_POINT('Ctrl Pts',(56.4994247502327,27.0600772763247,15.8721360462231));
#58645=CARTESIAN_POINT('Ctrl Pts',(56.4334107303472,27.0124678799764,15.8679184735721));
#58646=CARTESIAN_POINT('Ctrl Pts',(56.3672846479743,26.9647776640175,15.8636937413558));
#58647=CARTESIAN_POINT('Ctrl Pts',(56.2988005371564,26.9204087365886,15.8594690091395));
#58648=CARTESIAN_POINT('Ctrl Pts',(56.2283309921159,26.8795865441364,15.8552442769232));
#58649=CARTESIAN_POINT('Ctrl Pts',(56.1578790475833,26.8387745474548,15.8510205998781));
#58650=CARTESIAN_POINT('Ctrl Pts',(56.0854430847041,26.8015077086641,15.846796922833));
#58651=CARTESIAN_POINT('Ctrl Pts',(56.0114184816362,26.7679644032846,15.8425732457879));
#58652=CARTESIAN_POINT('Ctrl Pts',(55.9372595719828,26.7343602385877,15.8383419055116));
#58653=CARTESIAN_POINT('Ctrl Pts',(55.8615066952888,26.704493279414,15.8341105652354));
#58654=CARTESIAN_POINT('Ctrl Pts',(55.7845740244455,26.6784931940299,15.8298792249592));
#58655=CARTESIAN_POINT('Ctrl Pts',(55.7078624594941,26.652567833363,15.8256600456316));
#58656=CARTESIAN_POINT('Ctrl Pts',(55.6299783335128,26.6304871933858,15.8214408663041));
#58657=CARTESIAN_POINT('Ctrl Pts',(55.5513419837542,26.6123291125136,15.8172216869766));
#58658=CARTESIAN_POINT('Ctrl Pts',(55.4724552376491,26.5941132121073,15.8129890728051));
#58659=CARTESIAN_POINT('Ctrl Pts',(55.3925180616294,26.5797771679544,15.8087564586337));
#58660=CARTESIAN_POINT('Ctrl Pts',(55.311946338157,26.5694363344873,15.8045238444622));
#58661=CARTESIAN_POINT('Ctrl Pts',(55.2314895426829,26.5591102512482,15.8002972677174));
#58662=CARTESIAN_POINT('Ctrl Pts',(55.1504004543862,26.5527681188034,15.7960706909726));
#58663=CARTESIAN_POINT('Ctrl Pts',(55.0691067463729,26.55047463626,15.7918441142278));
#58664=CARTESIAN_POINT('Ctrl Pts',(54.9879032649618,26.5481836992166,15.7876222284938));
#58665=CARTESIAN_POINT('Ctrl Pts',(54.9064960771127,26.5499324964694,15.7834003427598));
#58666=CARTESIAN_POINT('Ctrl Pts',(54.8253181948176,26.5557339512774,15.7791784570258));
#58667=CARTESIAN_POINT('Ctrl Pts',(54.744195064487,26.5615314931839,15.7749594188227));
#58668=CARTESIAN_POINT('Ctrl Pts',(54.663301394714,26.5713762308611,15.7707403806197));
#58669=CARTESIAN_POINT('Ctrl Pts',(54.5830691491281,26.5852290138419,15.7665213424167));
#58670=CARTESIAN_POINT('Ctrl Pts',(54.5028631044684,26.5990772730088,15.7623036819977));
#58671=CARTESIAN_POINT('Ctrl Pts',(54.4233185124632,26.6169308991426,15.7580860215788));
#58672=CARTESIAN_POINT('Ctrl Pts',(54.3448598001788,26.6386991787199,15.7538683611598));
#58673=CARTESIAN_POINT('Ctrl Pts',(54.2664027205901,26.6604670053076,15.7496507885088));
#58674=CARTESIAN_POINT('Ctrl Pts',(54.1890319231182,26.6861491980422,15.7454332158577));
#58675=CARTESIAN_POINT('Ctrl Pts',(54.1131578747488,26.7156048295271,15.7412156432066));
#58676=CARTESIAN_POINT('Ctrl Pts',(54.0371550259428,26.7451104635923,15.7369909109903));
#58677=CARTESIAN_POINT('Ctrl Pts',(53.9626544451567,26.7784021835576,15.732766178774));
#58678=CARTESIAN_POINT('Ctrl Pts',(53.8900480831524,26.8152901812171,15.7285414465578));
#58679=CARTESIAN_POINT('Ctrl Pts',(53.8174598553484,26.8521689657124,15.7243177695126));
#58680=CARTESIAN_POINT('Ctrl Pts',(53.7467652942307,26.8926419816627,15.7200940924675));
#58681=CARTESIAN_POINT('Ctrl Pts',(53.678329269874,26.9364746836716,15.7158704154224));
#58682=CARTESIAN_POINT('Ctrl Pts',(53.6097690785732,26.9803869135711,15.7116390751462));
#58683=CARTESIAN_POINT('Ctrl Pts',(53.5434759926032,27.027670740936,15.7074077348699));
#58684=CARTESIAN_POINT('Ctrl Pts',(53.4797842570331,27.0780493386053,15.7031763945937));
#58685=CARTESIAN_POINT('Ctrl Pts',(53.4162755726665,27.1282831472709,15.6989572152661));
#58686=CARTESIAN_POINT('Ctrl Pts',(53.3553535938367,27.1815935987523,15.6947380359386));
#58687=CARTESIAN_POINT('Ctrl Pts',(53.2973124453094,27.2376704788543,15.6905188566111));
#58688=CARTESIAN_POINT('Ctrl Pts',(53.2387376267668,27.2942629681442,15.6862608832632));
#58689=CARTESIAN_POINT('Ctrl Pts',(53.1828605070431,27.3539018189101,15.6820029099154));
#58690=CARTESIAN_POINT('Ctrl Pts',(53.1300199241262,27.4162939774583,15.6777449365675));
#58691=CARTESIAN_POINT('Ctrl Pts',(53.0783432331251,27.477311856524,15.6735807513742));
#58692=CARTESIAN_POINT('Ctrl Pts',(53.0295710384744,27.540962630188,15.6694165661809));
#58693=CARTESIAN_POINT('Ctrl Pts',(52.9839856291495,27.6069327702783,15.6652523809876));
#58694=CARTESIAN_POINT('Ctrl Pts',(52.9384430373197,27.6728409458896,15.6610921071331));
#58695=CARTESIAN_POINT('Ctrl Pts',(52.8960815645859,27.7410637747401,15.6569318332785));
#58696=CARTESIAN_POINT('Ctrl Pts',(52.8571433024632,27.8112546850474,15.652771559424));
#58697=CARTESIAN_POINT('Ctrl Pts',(52.8182288838058,27.881402614635,15.6486138330726));
#58698=CARTESIAN_POINT('Ctrl Pts',(52.782733747793,27.9535158159383,15.6444561067212));
#58699=CARTESIAN_POINT('Ctrl Pts',(52.7508558078707,28.0272201415473,15.6402983803698));
#58700=CARTESIAN_POINT('Ctrl Pts',(52.71765006469,28.1039944536092,15.6359674733609));
#58701=CARTESIAN_POINT('Ctrl Pts',(52.6883697254216,28.182494867485,15.631636566352));
#58702=CARTESIAN_POINT('Ctrl Pts',(52.6631838951662,28.262273260489,15.627305659343));
#58703=CARTESIAN_POINT('Ctrl Pts',(52.6390015006805,28.3388731800271,15.6231473012222));
#58704=CARTESIAN_POINT('Ctrl Pts',(52.6185936465048,28.416650678846,15.6189889431015));
#58705=CARTESIAN_POINT('Ctrl Pts',(52.602059037614,28.4951937095169,15.6148305849807));
#58706=CARTESIAN_POINT('Ctrl Pts',(52.5855195668995,28.5737598349202,15.6106710041395));
#58707=CARTESIAN_POINT('Ctrl Pts',(52.5728556877415,28.6530914674989,15.6065114232983));
#58708=CARTESIAN_POINT('Ctrl Pts',(52.5641146513142,28.7327682315704,15.6023518424571));
#58709=CARTESIAN_POINT('Ctrl Pts',(52.5553646363121,28.8125268376292,15.5981879889981));
#58710=CARTESIAN_POINT('Ctrl Pts',(52.5505455299891,28.892630804583,15.594024135539));
#58711=CARTESIAN_POINT('Ctrl Pts',(52.5496525457875,28.9726576585775,15.58986028208));
#58712=CARTESIAN_POINT('Ctrl Pts',(52.5495429715248,28.9824774107231,15.5893493534742));
#58713=CARTESIAN_POINT('Ctrl Pts',(52.5494924473865,28.9922960060854,15.5888384248684));
#58714=CARTESIAN_POINT('Ctrl Pts',(52.549500910706,29.0021126687846,15.5883274962626));
#58715=CARTESIAN_POINT('',(52.5495005156126,28.9984103405398,14.7883274961845));
#58716=CARTESIAN_POINT('Ctrl Pts',(52.5495009107069,29.0021126697551,15.5883274962121));
#58717=CARTESIAN_POINT('Ctrl Pts',(52.5496027197749,29.1202016554576,15.5821813096032));
#58718=CARTESIAN_POINT('Ctrl Pts',(52.5582439368934,29.2379333721702,15.5760351229943));
#58719=CARTESIAN_POINT('Ctrl Pts',(52.5752507941987,29.354318414658,15.5698889363854));
#58720=CARTESIAN_POINT('Ctrl Pts',(52.5808521598771,29.3926509043574,15.5678646330055));
#58721=CARTESIAN_POINT('Ctrl Pts',(52.5873606589403,29.4308375654985,15.5658403296256));
#58722=CARTESIAN_POINT('Ctrl Pts',(52.5947690610642,29.4688436630541,15.5638160262457));
#58723=CARTESIAN_POINT('Ctrl Pts',(52.6102592826036,29.5483105792856,15.5595834120742));
#58724=CARTESIAN_POINT('Ctrl Pts',(52.6297208255725,29.6271567752449,15.5553507979027));
#58725=CARTESIAN_POINT('Ctrl Pts',(52.653089674389,29.7049554408191,15.5511181837313));
#58726=CARTESIAN_POINT('Ctrl Pts',(52.6764251897368,29.7826431339017,15.5468916069865));
#58727=CARTESIAN_POINT('Ctrl Pts',(52.7036568089021,29.8592858230665,15.5426650302417));
#58728=CARTESIAN_POINT('Ctrl Pts',(52.734669450267,29.9344665592981,15.5384384534969));
#58729=CARTESIAN_POINT('Ctrl Pts',(52.7656476711912,30.0095638536182,15.5342165677629));
#58730=CARTESIAN_POINT('Ctrl Pts',(52.8003983996278,30.0832019918242,15.5299946820288));
#58731=CARTESIAN_POINT('Ctrl Pts',(52.8387570920477,30.1549802348204,15.5257727962948));
#58732=CARTESIAN_POINT('Ctrl Pts',(52.8770899127191,30.2267100656178,15.5215537580918));
#58733=CARTESIAN_POINT('Ctrl Pts',(52.9190256459222,30.2965820839802,15.5173347198887));
#58734=CARTESIAN_POINT('Ctrl Pts',(52.9643526154026,30.3642177156091,15.5131156816857));
#58735=CARTESIAN_POINT('Ctrl Pts',(53.0096647827474,30.4318312599067,15.5088980212667));
#58736=CARTESIAN_POINT('Ctrl Pts',(53.058365728613,30.4972094822384,15.5046803608478));
#58737=CARTESIAN_POINT('Ctrl Pts',(53.1101997527774,30.5600016908957,15.5004627004288));
#58738=CARTESIAN_POINT('Ctrl Pts',(53.1620326982953,30.6227925928708,15.4962451277777));
#58739=CARTESIAN_POINT('Ctrl Pts',(53.2169982958419,30.6829972306607,15.4920275551267));
#58740=CARTESIAN_POINT('Ctrl Pts',(53.2748006694688,30.7402981123747,15.4878099824756));
#58741=CARTESIAN_POINT('Ctrl Pts',(53.3327011658547,30.7976962655371,15.4835852502593));
#58742=CARTESIAN_POINT('Ctrl Pts',(53.3934477415336,30.852180471496,15.479360518043));
#58743=CARTESIAN_POINT('Ctrl Pts',(53.4567074178512,30.9034700564718,15.4751357858268));
#58744=CARTESIAN_POINT('Ctrl Pts',(53.5199512944015,30.9547468313359,15.4709121087816));
#58745=CARTESIAN_POINT('Ctrl Pts',(53.585706627575,31.0028303227957,15.4666884317365));
#58746=CARTESIAN_POINT('Ctrl Pts',(53.6536106083631,31.0474828097172,15.4624647546914));
#58747=CARTESIAN_POINT('Ctrl Pts',(53.7216377907818,31.0922163119068,15.4582334144152));
#58748=CARTESIAN_POINT('Ctrl Pts',(53.7918210100753,31.1335061327748,15.4540020741389));
#58749=CARTESIAN_POINT('Ctrl Pts',(53.863771312899,31.1711597409239,15.4497707338627));
#58750=CARTESIAN_POINT('Ctrl Pts',(53.9355148292464,31.2087051319198,15.4455515545352));
#58751=CARTESIAN_POINT('Ctrl Pts',(54.0090148372316,31.2426350680789,15.4413323752077));
#58752=CARTESIAN_POINT('Ctrl Pts',(54.0838682298706,31.2728072575033,15.4371131958802));
#58753=CARTESIAN_POINT('Ctrl Pts',(54.1589599730452,31.3030755221656,15.4328805817087));
#58754=CARTESIAN_POINT('Ctrl Pts',(54.2356930309845,31.3296746216102,15.4286479675372));
#58755=CARTESIAN_POINT('Ctrl Pts',(54.313674534464,31.3524258979523,15.4244153533658));
#58756=CARTESIAN_POINT('Ctrl Pts',(54.3915448046509,31.375144721735,15.420188776621));
#58757=CARTESIAN_POINT('Ctrl Pts',(54.4706595412482,31.3940264943716,15.4159621998762));
#58758=CARTESIAN_POINT('Ctrl Pts',(54.5506063463779,31.4089407618462,15.4117356231314));
#58759=CARTESIAN_POINT('Ctrl Pts',(54.6304644198115,31.4238384762109,15.4075137373974));
#58760=CARTESIAN_POINT('Ctrl Pts',(54.7111522724174,31.4347773503387,15.4032918516633));
#58761=CARTESIAN_POINT('Ctrl Pts',(54.7922441765024,31.4416772448059,15.3990699659293));
#58762=CARTESIAN_POINT('Ctrl Pts',(54.8732813866128,31.4485724855083,15.3948509277263));
#58763=CARTESIAN_POINT('Ctrl Pts',(54.9547216452721,31.4514341176995,15.3906318895233));
#58764=CARTESIAN_POINT('Ctrl Pts',(55.0361321580848,31.4502336046084,15.3864128513202));
#58765=CARTESIAN_POINT('Ctrl Pts',(55.1175160851921,31.449033483561,15.3821951909013));
#58766=CARTESIAN_POINT('Ctrl Pts',(55.1988698216021,31.4437738585199,15.3779775304823));
#58767=CARTESIAN_POINT('Ctrl Pts',(55.2797599948554,31.4344783004329,15.3737598700633));
#58768=CARTESIAN_POINT('Ctrl Pts',(55.3606484848149,31.4251829357829,15.3695422974123));
#58769=CARTESIAN_POINT('Ctrl Pts',(55.4410729694212,31.411851859275,15.3653247247612));
#58770=CARTESIAN_POINT('Ctrl Pts',(55.5206060533622,31.3945604162774,15.3611071521102));
#58771=CARTESIAN_POINT('Ctrl Pts',(55.6002741491573,31.3772396200892,15.3568824198939));
#58772=CARTESIAN_POINT('Ctrl Pts',(55.6790473603885,31.3559451055838,15.3526576876776));
#58773=CARTESIAN_POINT('Ctrl Pts',(55.756508976961,31.3308033846246,15.3484329554613));
#58774=CARTESIAN_POINT('Ctrl Pts',(55.8339512466824,31.3056679430738,15.3442092784162));
#58775=CARTESIAN_POINT('Ctrl Pts',(55.9100821487366,31.27668740229,15.3399856013711));
#58776=CARTESIAN_POINT('Ctrl Pts',(55.9845047631225,31.2440366800454,15.335761924326));
#58777=CARTESIAN_POINT('Ctrl Pts',(56.0590624062261,31.2113267179421,15.3315305840498));
#58778=CARTESIAN_POINT('Ctrl Pts',(56.131905150775,31.1749334748291,15.3272992437735));
#58779=CARTESIAN_POINT('Ctrl Pts',(56.2026597500616,31.1350784003361,15.3230679034973));
#58780=CARTESIAN_POINT('Ctrl Pts',(56.2732109993462,31.0953378700503,15.3188487241698));
#58781=CARTESIAN_POINT('Ctrl Pts',(56.341685749369,31.0521556937388,15.3146295448422));
#58782=CARTESIAN_POINT('Ctrl Pts',(56.4077451903292,31.0057925438851,15.3104103655147));
#58783=CARTESIAN_POINT('Ctrl Pts',(56.474014979846,30.9592817630265,15.3061777513432));
#58784=CARTESIAN_POINT('Ctrl Pts',(56.5381005140958,30.9093967094343,15.3019451371718));
#58785=CARTESIAN_POINT('Ctrl Pts',(56.5996380520154,30.8563696702286,15.2977125230003));
#58786=CARTESIAN_POINT('Ctrl Pts',(56.6610878124152,30.8034182691153,15.2934859462555));
#58787=CARTESIAN_POINT('Ctrl Pts',(56.719996446032,30.7473340844447,15.2892593695107));
#58788=CARTESIAN_POINT('Ctrl Pts',(56.776030015009,30.688392026689,15.2850327927659));
#58789=CARTESIAN_POINT('Ctrl Pts',(56.8320013932129,30.6295153877923,15.2808109070319));
#58790=CARTESIAN_POINT('Ctrl Pts',(56.8851037288051,30.5677875133758,15.2765890212979));
#58791=CARTESIAN_POINT('Ctrl Pts',(56.9350380323161,30.5035218866017,15.2723671355638));
#58792=CARTESIAN_POINT('Ctrl Pts',(56.9849386566879,30.439299605,15.2681480973608));
#58793=CARTESIAN_POINT('Ctrl Pts',(57.031675208438,30.3725433363819,15.2639290591578));
#58794=CARTESIAN_POINT('Ctrl Pts',(57.074988136585,30.3036005841635,15.2597100209548));
#58795=CARTESIAN_POINT('Ctrl Pts',(57.1182869203088,30.2346803461345,15.2554923605358));
#58796=CARTESIAN_POINT('Ctrl Pts',(57.1581640538318,30.1635754355767,15.2512747001168));
#58797=CARTESIAN_POINT('Ctrl Pts',(57.1944033807436,30.090662208285,15.2470570396979));
#58798=CARTESIAN_POINT('Ctrl Pts',(57.2306419535287,30.0177504982899,15.2428394670468));
#58799=CARTESIAN_POINT('Ctrl Pts',(57.2632426645084,29.9430309629015,15.2386218943958));
#58800=CARTESIAN_POINT('Ctrl Pts',(57.292036040926,29.8669031301688,15.2344043217447));
#58801=CARTESIAN_POINT('Ctrl Pts',(57.3208782957089,29.7906460661862,15.2301795895285));
#58802=CARTESIAN_POINT('Ctrl Pts',(57.3459001194426,29.7129763584957,15.2259548573122));
#58803=CARTESIAN_POINT('Ctrl Pts',(57.3669807761582,29.6343124271978,15.2217301250959));
#58804=CARTESIAN_POINT('Ctrl Pts',(57.3880561677587,29.5556681430415,15.2175064480508));
#58805=CARTESIAN_POINT('Ctrl Pts',(57.4051922835052,29.4760305920444,15.2132827710057));
#58806=CARTESIAN_POINT('Ctrl Pts',(57.4183197652693,29.3958279460926,15.2090590939606));
#58807=CARTESIAN_POINT('Ctrl Pts',(57.4314710648882,29.3154797844192,15.2048277536843));
#58808=CARTESIAN_POINT('Ctrl Pts',(57.4405991433208,29.2345649417645,15.2005964134081));
#58809=CARTESIAN_POINT('Ctrl Pts',(57.4456865622944,29.1535170642398,15.1963650731318));
#58810=CARTESIAN_POINT('Ctrl Pts',(57.4507593599335,29.0727021197859,15.1921458938043));
#58811=CARTESIAN_POINT('Ctrl Pts',(57.4518147701902,28.9917553604263,15.1879267144768));
#58812=CARTESIAN_POINT('Ctrl Pts',(57.4488870033909,28.9111028986792,15.1837075351493));
#58813=CARTESIAN_POINT('Ctrl Pts',(57.4459499139042,28.830193620818,15.1794749209778));
#58814=CARTESIAN_POINT('Ctrl Pts',(57.4389932889958,28.7492795945812,15.1752423068064));
#58815=CARTESIAN_POINT('Ctrl Pts',(57.4280139560343,28.6687923924442,15.1710096926349));
#58816=CARTESIAN_POINT('Ctrl Pts',(57.4170502840602,28.5884199977437,15.1667831158901));
#58817=CARTESIAN_POINT('Ctrl Pts',(57.4020753627368,28.5084736744004,15.1625565391453));
#58818=CARTESIAN_POINT('Ctrl Pts',(57.383137997865,28.4293831993957,15.1583299624005));
#58819=CARTESIAN_POINT('Ctrl Pts',(57.3642216512753,28.3503805056598,15.1541080766665));
#58820=CARTESIAN_POINT('Ctrl Pts',(57.3413517072913,28.2722322223294,15.1498861909324));
#58821=CARTESIAN_POINT('Ctrl Pts',(57.3146283533897,28.1953598098003,15.1456643051984));
#58822=CARTESIAN_POINT('Ctrl Pts',(57.2879230235615,28.1185392453296,15.1414452669954));
#58823=CARTESIAN_POINT('Ctrl Pts',(57.2573695978118,28.0429932802206,15.1372262287924));
#58824=CARTESIAN_POINT('Ctrl Pts',(57.223118271009,27.9691288135242,15.1330071905893));
#58825=CARTESIAN_POINT('Ctrl Pts',(57.1888781294407,27.8952884682696,15.1287895301704));
#58826=CARTESIAN_POINT('Ctrl Pts',(57.1509426803136,27.8231289520367,15.1245718697514));
#58827=CARTESIAN_POINT('Ctrl Pts',(57.1095099446389,27.7530364706737,15.1203542093324));
#58828=CARTESIAN_POINT('Ctrl Pts',(57.0680780711636,27.6829454479088,15.1161366366814));
#58829=CARTESIAN_POINT('Ctrl Pts',(57.0231492932417,27.6149217737984,15.1119190640304));
#58830=CARTESIAN_POINT('Ctrl Pts',(56.9749664839744,27.5493251097582,15.1077014913793));
#58831=CARTESIAN_POINT('Ctrl Pts',(56.9267018816959,27.4836170917155,15.103476759163));
#58832=CARTESIAN_POINT('Ctrl Pts',(56.8751724724945,27.4203447032426,15.0992520269467));
#58833=CARTESIAN_POINT('Ctrl Pts',(56.8206635089471,27.3598370089566,15.0950272947304));
#58834=CARTESIAN_POINT('Ctrl Pts',(56.766168159585,27.2993444271018,15.0908036176853));
#58835=CARTESIAN_POINT('Ctrl Pts',(56.7086950879882,27.2416154739421,15.0865799406402));
#58836=CARTESIAN_POINT('Ctrl Pts',(56.6485656969155,27.1869414259453,15.0823562635951));
#58837=CARTESIAN_POINT('Ctrl Pts',(56.588327210044,27.1321681800548,15.0781249233189));
#58838=CARTESIAN_POINT('Ctrl Pts',(56.5254231320117,27.0804612120078,15.0738935830426));
#58839=CARTESIAN_POINT('Ctrl Pts',(56.4602077227072,27.0320712267599,15.0696622427664));
#58840=CARTESIAN_POINT('Ctrl Pts',(56.3951797436721,26.9838203152075,15.0654430634389));
#58841=CARTESIAN_POINT('Ctrl Pts',(56.3278541260386,26.9388675293988,15.0612238841113));
#58842=CARTESIAN_POINT('Ctrl Pts',(56.2586069278663,26.8974161488476,15.0570047047838));
#58843=CARTESIAN_POINT('Ctrl Pts',(56.1891392305801,26.8558327775022,15.0527720906123));
#58844=CARTESIAN_POINT('Ctrl Pts',(56.1174793119124,26.8176185088514,15.0485394764409));
#58845=CARTESIAN_POINT('Ctrl Pts',(56.0439874585597,26.7830109525823,15.0443068622694));
#58846=CARTESIAN_POINT('Ctrl Pts',(55.9706004344353,26.7484527607427,15.0400802855246));
#58847=CARTESIAN_POINT('Ctrl Pts',(55.895387082334,26.7174912596412,15.0358537087798));
#58848=CARTESIAN_POINT('Ctrl Pts',(55.8187344799474,26.6903194806759,15.031627132035));
#58849=CARTESIAN_POINT('Ctrl Pts',(55.7421669530735,26.6631778592389,15.027405246301));
#58850=CARTESIAN_POINT('Ctrl Pts',(55.6641637855931,26.6398177567488,15.023183360567));
#58851=CARTESIAN_POINT('Ctrl Pts',(55.5851330512618,26.6203845768022,15.0189614748329));
#58852=CARTESIAN_POINT('Ctrl Pts',(55.5061556207098,26.6009645039328,15.0147424366299));
#58853=CARTESIAN_POINT('Ctrl Pts',(55.4261524497351,26.5854662039199,15.0105233984269));
#58854=CARTESIAN_POINT('Ctrl Pts',(55.3455466217338,26.5739852056905,15.0063043602239));
#58855=CARTESIAN_POINT('Ctrl Pts',(55.2649671166572,26.5625079567366,15.0020866998049));
#58856=CARTESIAN_POINT('Ctrl Pts',(55.1837858049525,26.5550454696606,14.9978690393859));
#58857=CARTESIAN_POINT('Ctrl Pts',(55.1024344486264,26.5516418902181,14.993651378967));
#58858=CARTESIAN_POINT('Ctrl Pts',(55.0210847851912,26.5482383816029,14.9894338063159));
#58859=CARTESIAN_POINT('Ctrl Pts',(54.939565548361,26.5488936309297,14.9852162336649));
#58860=CARTESIAN_POINT('Ctrl Pts',(54.8583106515168,26.5535997100788,14.9809986610138));
#58861=CARTESIAN_POINT('Ctrl Pts',(54.7769178199451,26.5583137780603,14.9767739287975));
#58862=CARTESIAN_POINT('Ctrl Pts',(54.6957906923802,26.5670924071531,14.9725491965812));
#58863=CARTESIAN_POINT('Ctrl Pts',(54.6153605882569,26.579875463342,14.968324464365));
#58864=CARTESIAN_POINT('Ctrl Pts',(54.5349505723956,26.5926553268287,14.9641007873199));
#58865=CARTESIAN_POINT('Ctrl Pts',(54.4552376836173,26.6094375005358,14.9598771102747));
#58866=CARTESIAN_POINT('Ctrl Pts',(54.3766412238928,26.6301109548652,14.9556534332296));
#58867=CARTESIAN_POINT('Ctrl Pts',(54.2979021626316,26.6508219180895,14.9514220929534));
#58868=CARTESIAN_POINT('Ctrl Pts',(54.2202840226028,26.6754381305557,14.9471907526771));
#58869=CARTESIAN_POINT('Ctrl Pts',(54.1441899608165,26.7037989141121,14.9429594124009));
#58870=CARTESIAN_POINT('Ctrl Pts',(54.0683145947448,26.7320781882619,14.9387402330734));
#58871=CARTESIAN_POINT('Ctrl Pts',(53.9939549434447,26.7640802819455,14.9345210537459));
#58872=CARTESIAN_POINT('Ctrl Pts',(53.9214862492111,26.7996004137068,14.9303018744184));
#58873=CARTESIAN_POINT('Ctrl Pts',(53.848786797874,26.8352336497928,14.9260692602469));
#58874=CARTESIAN_POINT('Ctrl Pts',(53.7777199877831,26.8745399187011,14.9218366460755));
#58875=CARTESIAN_POINT('Ctrl Pts',(53.7086812723065,26.9173463577666,14.917604031904));
#58876=CARTESIAN_POINT('Ctrl Pts',(53.6397410340751,26.9600917374661,14.9133774551592));
#58877=CARTESIAN_POINT('Ctrl Pts',(53.572823536347,27.0063271284838,14.9091508784144));
#58878=CARTESIAN_POINT('Ctrl Pts',(53.5083014241358,27.0558329267358,14.9049243016696));
#58879=CARTESIAN_POINT('Ctrl Pts',(53.4438509239977,27.1052837792844,14.9007024159356));
#58880=CARTESIAN_POINT('Ctrl Pts',(53.3817908934466,27.1579975453547,14.8964805302015));
#58881=CARTESIAN_POINT('Ctrl Pts',(53.3224654563689,27.2137110802213,14.8922586444675));
#58882=CARTESIAN_POINT('Ctrl Pts',(53.2631800324587,27.2693870380363,14.8880396062645));
#58883=CARTESIAN_POINT('Ctrl Pts',(53.2066258766436,27.3280584291,14.8838205680615));
#58884=CARTESIAN_POINT('Ctrl Pts',(53.1531134479394,27.3894223664108,14.8796015298584));
#58885=CARTESIAN_POINT('Ctrl Pts',(53.0996184944434,27.450766264497,14.8753838694395));
#58886=CARTESIAN_POINT('Ctrl Pts',(53.0491636004792,27.5148006127681,14.8711662090205));
#58887=CARTESIAN_POINT('Ctrl Pts',(53.0020208482047,27.5811872713458,14.8669485486015));
#58888=CARTESIAN_POINT('Ctrl Pts',(52.954879076953,27.6475725484422,14.8627309759505));
#58889=CARTESIAN_POINT('Ctrl Pts',(52.9110495783621,27.7163096590762,14.8585134032994));
#58890=CARTESIAN_POINT('Ctrl Pts',(52.8707619249197,27.7870303096827,14.8542958306484));
#58891=CARTESIAN_POINT('Ctrl Pts',(52.8304058809345,27.8578710125452,14.8500710984321));
#58892=CARTESIAN_POINT('Ctrl Pts',(52.7936039428232,27.93070158653,14.8458463662158));
#58893=CARTESIAN_POINT('Ctrl Pts',(52.7605404793052,28.0051274930076,14.8416216339995));
#58894=CARTESIAN_POINT('Ctrl Pts',(52.7274852737339,28.0795348108345,14.8373979569544));
#58895=CARTESIAN_POINT('Ctrl Pts',(52.6981668234897,28.1555362217884,14.8331742799093));
#58896=CARTESIAN_POINT('Ctrl Pts',(52.6727202624752,28.2327195601955,14.8289506028642));
#58897=CARTESIAN_POINT('Ctrl Pts',(52.6472275324766,28.3100429362417,14.8247192625879));
#58898=CARTESIAN_POINT('Ctrl Pts',(52.625620854484,28.3885520761161,14.8204879223117));
#58899=CARTESIAN_POINT('Ctrl Pts',(52.6079849266118,28.4678213282329,14.8162565820354));
#58900=CARTESIAN_POINT('Ctrl Pts',(52.5903996847164,28.5468627590806,14.8120374027079));
#58901=CARTESIAN_POINT('Ctrl Pts',(52.5767623941067,28.6266594760962,14.8078182233804));
#58902=CARTESIAN_POINT('Ctrl Pts',(52.5671055611392,28.7067852333864,14.8035990440529));
#58903=CARTESIAN_POINT('Ctrl Pts',(52.5554544180134,28.8034584045383,14.798508528106));
#58904=CARTESIAN_POINT('Ctrl Pts',(52.5495638106476,28.9008395066439,14.793418012159));
#58905=CARTESIAN_POINT('Ctrl Pts',(52.549500515613,28.9984103400116,14.7883274962121));
#58906=CARTESIAN_POINT('',(52.5495001466462,28.9991522304455,13.9883274962515));
#58907=CARTESIAN_POINT('Ctrl Pts',(52.5495005156126,28.9984103405398,14.7883274961845));
#58908=CARTESIAN_POINT('Ctrl Pts',(52.5494486476381,29.0783661096744,14.7841560024729));
#58909=CARTESIAN_POINT('Ctrl Pts',(52.5533142347253,29.1584742115312,14.7799845087613));
#58910=CARTESIAN_POINT('Ctrl Pts',(52.5611155699173,29.2383127917256,14.7758130150497));
#58911=CARTESIAN_POINT('Ctrl Pts',(52.5689063467647,29.318043318207,14.7716471670471));
#58912=CARTESIAN_POINT('Ctrl Pts',(52.5806222456023,29.3975045747558,14.7674813190444));
#58913=CARTESIAN_POINT('Ctrl Pts',(52.5962295353568,29.4762749240818,14.7633154710417));
#58914=CARTESIAN_POINT('Ctrl Pts',(52.6118251610571,29.5549864046583,14.7591527363712));
#58915=CARTESIAN_POINT('Ctrl Pts',(52.6313063172899,29.6330075345443,14.7549900017007));
#58916=CARTESIAN_POINT('Ctrl Pts',(52.654587629556,29.7099232793536,14.7508272670302));
#58917=CARTESIAN_POINT('Ctrl Pts',(52.6778591264256,29.7868065965009,14.7466662873678));
#58918=CARTESIAN_POINT('Ctrl Pts',(52.7049274619381,29.862584995857,14.7425053077053));
#58919=CARTESIAN_POINT('Ctrl Pts',(52.7356568709464,29.9368566826937,14.7383443280429));
#58920=CARTESIAN_POINT('Ctrl Pts',(52.7663833333954,30.0111212478207,14.7341837473655));
#58921=CARTESIAN_POINT('Ctrl Pts',(52.8007699881503,30.0838789456754,14.730023166688));
#58922=CARTESIAN_POINT('Ctrl Pts',(52.8386328050145,30.1547476340918,14.7258625860106));
#58923=CARTESIAN_POINT('Ctrl Pts',(52.8765298797931,30.2256804438194,14.7216982408796));
#58924=CARTESIAN_POINT('Ctrl Pts',(52.9179091736609,30.2947204068032,14.7175338957486));
#58925=CARTESIAN_POINT('Ctrl Pts',(52.9625408723203,30.3615103940237,14.7133695506176));
#58926=CARTESIAN_POINT('Ctrl Pts',(53.0071919011386,30.4283293082424,14.7092034018928));
#58927=CARTESIAN_POINT('Ctrl Pts',(53.0550978534665,30.4928959221122,14.7050372531681));
#58928=CARTESIAN_POINT('Ctrl Pts',(53.1059873434397,30.554884660285,14.7008711044433));
#58929=CARTESIAN_POINT('Ctrl Pts',(53.1569665143059,30.6169826391947,14.6966976138501));
#58930=CARTESIAN_POINT('Ctrl Pts',(53.2109394031175,30.6764933129995,14.692524123257));
#58931=CARTESIAN_POINT('Ctrl Pts',(53.2675966059561,30.7331268650348,14.6883506326638));
#58932=CARTESIAN_POINT('Ctrl Pts',(53.3194297437781,30.7849383657958,14.684532493005));
#58933=CARTESIAN_POINT('Ctrl Pts',(53.3735088997252,30.8343421090488,14.6807143533463));
#58934=CARTESIAN_POINT('Ctrl Pts',(53.4295743626424,30.8811468755868,14.6768962136875));
#58935=CARTESIAN_POINT('Ctrl Pts',(53.4917259584669,30.9330324889603,14.672663599516));
#58936=CARTESIAN_POINT('Ctrl Pts',(53.5565672853796,30.981931124894,14.6684309853445));
#58937=CARTESIAN_POINT('Ctrl Pts',(53.6237794148746,31.0275520094629,14.664198371173));
#58938=CARTESIAN_POINT('Ctrl Pts',(53.690895672578,31.0731078201237,14.6599717944283));
#58939=CARTESIAN_POINT('Ctrl Pts',(53.7603756351425,31.115394906649,14.6557452176835));
#58940=CARTESIAN_POINT('Ctrl Pts',(53.8318669732864,31.1541623620101,14.6515186409387));
#58941=CARTESIAN_POINT('Ctrl Pts',(53.9032789643233,31.1928867899848,14.6472967552046));
#58942=CARTESIAN_POINT('Ctrl Pts',(53.9766974888646,31.2280991284402,14.6430748694706));
#58943=CARTESIAN_POINT('Ctrl Pts',(54.0517420667263,31.2595922512665,14.6388529837366));
#58944=CARTESIAN_POINT('Ctrl Pts',(54.1267360293474,31.2910641329581,14.6346339455336));
#58945=CARTESIAN_POINT('Ctrl Pts',(54.2033534398501,31.3188216018119,14.6304149073305));
#58946=CARTESIAN_POINT('Ctrl Pts',(54.2811912310675,31.342704463586,14.6261958691275));
#58947=CARTESIAN_POINT('Ctrl Pts',(54.3590036033,31.3665795260882,14.6219782087085));
#58948=CARTESIAN_POINT('Ctrl Pts',(54.4380351210145,31.3865823581674,14.6177605482896));
#58949=CARTESIAN_POINT('Ctrl Pts',(54.5178661492761,31.4026021726424,14.6135428878706));
#58950=CARTESIAN_POINT('Ctrl Pts',(54.5976955162842,31.4186216537512,14.6093253152196));
#58951=CARTESIAN_POINT('Ctrl Pts',(54.6783239050611,31.4306581918046,14.6051077425685));
#58952=CARTESIAN_POINT('Ctrl Pts',(54.7593214531776,31.438652104565,14.6008901699174));
#58953=CARTESIAN_POINT('Ctrl Pts',(54.8404564991578,31.446659587439,14.5966654377012));
#58954=CARTESIAN_POINT('Ctrl Pts',(54.921961493559,31.4506106687288,14.5924407054849));
#58955=CARTESIAN_POINT('Ctrl Pts',(55.0034010134452,31.4504976398902,14.5882159732686));
#58956=CARTESIAN_POINT('Ctrl Pts',(55.0848201929573,31.4503846392818,14.5839922962235));
#58957=CARTESIAN_POINT('Ctrl Pts',(55.1661734662046,31.4462096035141,14.5797686191784));
#58958=CARTESIAN_POINT('Ctrl Pts',(55.2470293623713,31.4380169696141,14.5755449421332));
#58959=CARTESIAN_POINT('Ctrl Pts',(55.3280319594846,31.4298094714036,14.571313601857));
#58960=CARTESIAN_POINT('Ctrl Pts',(55.4085349154643,31.4175698776105,14.5670822615808));
#58961=CARTESIAN_POINT('Ctrl Pts',(55.4881149828723,31.4013941811988,14.5628509213045));
#58962=CARTESIAN_POINT('Ctrl Pts',(55.5674663357224,31.3852649740322,14.558631741977));
#58963=CARTESIAN_POINT('Ctrl Pts',(55.6458996772294,31.3652224521933,14.5544125626495));
#58964=CARTESIAN_POINT('Ctrl Pts',(55.7230124725475,31.341410518158,14.550193383322));
#58965=CARTESIAN_POINT('Ctrl Pts',(55.8003708128623,31.3175227614107,14.5459607691505));
#58966=CARTESIAN_POINT('Ctrl Pts',(55.87668789292,31.2897526774452,14.5417281549791));
#58967=CARTESIAN_POINT('Ctrl Pts',(55.9515461792811,31.2582094939787,14.5374955408076));
#58968=CARTESIAN_POINT('Ctrl Pts',(56.0262976873254,31.2267113039017,14.5332689640628));
#58969=CARTESIAN_POINT('Ctrl Pts',(56.0995941099357,31.1914508825021,14.529042387318));
#58970=CARTESIAN_POINT('Ctrl Pts',(56.1710331716213,31.1525871784814,14.5248158105732));
#58971=CARTESIAN_POINT('Ctrl Pts',(56.2423929442211,31.1137666086717,14.5205939248392));
#58972=CARTESIAN_POINT('Ctrl Pts',(56.3118990459886,31.0713509235728,14.5163720391052));
#58973=CARTESIAN_POINT('Ctrl Pts',(56.3791706005989,31.0255465199406,14.5121501533712));
#58974=CARTESIAN_POINT('Ctrl Pts',(56.4463967826319,30.9797730099582,14.5079311151681));
#58975=CARTESIAN_POINT('Ctrl Pts',(56.5113910278071,30.9306155815937,14.5037120769651));
#58976=CARTESIAN_POINT('Ctrl Pts',(56.5737995310625,30.8783251278805,14.4994930387621));
#58977=CARTESIAN_POINT('Ctrl Pts',(56.636187653976,30.8260517503232,14.4952753783431));
#58978=CARTESIAN_POINT('Ctrl Pts',(56.6959913561078,30.7706476774154,14.4910577179242));
#58979=CARTESIAN_POINT('Ctrl Pts',(56.7528892567785,30.712404596896,14.4868400575052));
#58980=CARTESIAN_POINT('Ctrl Pts',(56.8097859734253,30.6541627283931,14.4826224848542));
#58981=CARTESIAN_POINT('Ctrl Pts',(56.8637766850532,30.5930823028627,14.4784049122031));
#58982=CARTESIAN_POINT('Ctrl Pts',(56.9145773112425,30.5294914086962,14.4741873395521));
#58983=CARTESIAN_POINT('Ctrl Pts',(56.9654641743332,30.4657925654337,14.4699626073358));
#58984=CARTESIAN_POINT('Ctrl Pts',(57.0131498256613,30.3995750918099,14.4657378751195));
#58985=CARTESIAN_POINT('Ctrl Pts',(57.057390754508,30.3312000350304,14.4615131429032));
#58986=CARTESIAN_POINT('Ctrl Pts',(57.1016206337188,30.2628420556384,14.4572894658581));
#58987=CARTESIAN_POINT('Ctrl Pts',(57.1424072959396,30.1923279848682,14.453065788813));
#58988=CARTESIAN_POINT('Ctrl Pts',(57.1795531230098,30.1200439428783,14.4488421117679));
#58989=CARTESIAN_POINT('Ctrl Pts',(57.2167663456349,30.0476287522909,14.4446107714916));
#58990=CARTESIAN_POINT('Ctrl Pts',(57.2503253397301,29.9734375972048,14.4403794312154));
#58991=CARTESIAN_POINT('Ctrl Pts',(57.2800802103686,29.8978777668957,14.4361480909392));
#58992=CARTESIAN_POINT('Ctrl Pts',(57.309749564969,29.8225350969098,14.4319289116116));
#58993=CARTESIAN_POINT('Ctrl Pts',(57.3356365663843,29.7458320663347,14.4277097322841));
#58994=CARTESIAN_POINT('Ctrl Pts',(57.3576427833466,29.668184672178,14.4234905529566));
#58995=CARTESIAN_POINT('Ctrl Pts',(57.3797190731995,29.5902900307384,14.4192579387851));
#58996=CARTESIAN_POINT('Ctrl Pts',(57.3979719061172,29.511155282603,14.4150253246137));
#58997=CARTESIAN_POINT('Ctrl Pts',(57.4122655995232,29.4311901290114,14.4107927104422));
#58998=CARTESIAN_POINT('Ctrl Pts',(57.4265389043178,29.3513390382027,14.4065661336974));
#58999=CARTESIAN_POINT('Ctrl Pts',(57.4368642048842,29.2706603479988,14.4023395569526));
#59000=CARTESIAN_POINT('Ctrl Pts',(57.4431558323015,29.1895780290307,14.3981129802078));
#59001=CARTESIAN_POINT('Ctrl Pts',(57.4494404767409,29.1085857020479,14.3938910944737));
#59002=CARTESIAN_POINT('Ctrl Pts',(57.4517003078846,29.0271910972604,14.3896692087397));
#59003=CARTESIAN_POINT('Ctrl Pts',(57.44990110716,28.9458260658984,14.3854473230057));
#59004=CARTESIAN_POINT('Ctrl Pts',(57.4481031199405,28.8645159127267,14.3812282848027));
#59005=CARTESIAN_POINT('Ctrl Pts',(57.4422515483897,28.7832357566018,14.3770092465996));
#59006=CARTESIAN_POINT('Ctrl Pts',(57.4323642361525,28.7024189645048,14.3727902083966));
#59007=CARTESIAN_POINT('Ctrl Pts',(57.4224801527509,28.6216285642256,14.3685725479776));
#59008=CARTESIAN_POINT('Ctrl Pts',(57.4085630023528,28.5413016882235,14.3643548875586));
#59009=CARTESIAN_POINT('Ctrl Pts',(57.3906825000909,28.4618667137601,14.3601372271397));
#59010=CARTESIAN_POINT('Ctrl Pts',(57.3728023699155,28.3824333923088,14.3559196544886));
#59011=CARTESIAN_POINT('Ctrl Pts',(57.3509591550207,28.303892388444,14.3517020818376));
#59012=CARTESIAN_POINT('Ctrl Pts',(57.3252734106166,28.2266606075731,14.3474845091865));
#59013=CARTESIAN_POINT('Ctrl Pts',(57.2995440632262,28.1492977214387,14.3432597769703));
#59014=CARTESIAN_POINT('Ctrl Pts',(57.2699592828855,28.0732489480897,14.339035044754));
#59015=CARTESIAN_POINT('Ctrl Pts',(57.2366893576674,27.99891510485,14.3348103125377));
#59016=CARTESIAN_POINT('Ctrl Pts',(57.203427741962,27.9245998272672,14.3305866354926));
#59017=CARTESIAN_POINT('Ctrl Pts',(57.1664830523105,27.8519990290742,14.3263629584475));
#59018=CARTESIAN_POINT('Ctrl Pts',(57.1260715925566,27.7814886814954,14.3221392814024));
#59019=CARTESIAN_POINT('Ctrl Pts',(57.085586812245,27.7108504034226,14.3179079411261));
#59020=CARTESIAN_POINT('Ctrl Pts',(57.041622943151,27.6423105479224,14.3136766008499));
#59021=CARTESIAN_POINT('Ctrl Pts',(56.9944400268748,27.576216579251,14.3094452605736));
#59022=CARTESIAN_POINT('Ctrl Pts',(56.9473927151562,27.510312565845,14.3052260812461));
#59023=CARTESIAN_POINT('Ctrl Pts',(56.8971451825335,27.4468407043081,14.3010069019186));
#59024=CARTESIAN_POINT('Ctrl Pts',(56.8439927917296,27.3861100303772,14.2967877225911));
#59025=CARTESIAN_POINT('Ctrl Pts',(56.7906711514053,27.3251859759175,14.2925551084196));
#59026=CARTESIAN_POINT('Ctrl Pts',(56.7342277852616,27.266794018506,14.2883224942482));
#59027=CARTESIAN_POINT('Ctrl Pts',(56.67493249533,27.2112710137957,14.2840898800767));
#59028=CARTESIAN_POINT('Ctrl Pts',(56.6157217845621,27.1558272074384,14.2798633033319));
#59029=CARTESIAN_POINT('Ctrl Pts',(56.5536675658583,27.1032445408476,14.2756367265871));
#59030=CARTESIAN_POINT('Ctrl Pts',(56.4890788382501,27.0538256852286,14.2714101498423));
#59031=CARTESIAN_POINT('Ctrl Pts',(56.4245617966502,27.0044616788168,14.2671882641083));
#59032=CARTESIAN_POINT('Ctrl Pts',(56.3575162026761,26.9582547869718,14.2629663783743));
#59033=CARTESIAN_POINT('Ctrl Pts',(56.2882856754156,26.9154688132534,14.2587444926403));
#59034=CARTESIAN_POINT('Ctrl Pts',(56.2191018419988,26.8727116973476,14.2545254544372));
#59035=CARTESIAN_POINT('Ctrl Pts',(56.1477363962833,26.8333711606566,14.2503064162342));
#59036=CARTESIAN_POINT('Ctrl Pts',(56.0745625715205,26.7976681608152,14.2460873780312));
#59037=CARTESIAN_POINT('Ctrl Pts',(56.0014126426609,26.7619768202718,14.2418697176122));
#59038=CARTESIAN_POINT('Ctrl Pts',(55.9264559247337,26.7299208610591,14.2376520571933));
#59039=CARTESIAN_POINT('Ctrl Pts',(55.8500897043675,26.7016750132916,14.2334343967743));
#59040=CARTESIAN_POINT('Ctrl Pts',(55.7737250731538,26.6734297533096,14.2292168241233));
#59041=CARTESIAN_POINT('Ctrl Pts',(55.695951433926,26.6489946071822,14.2249992514722));
#59042=CARTESIAN_POINT('Ctrl Pts',(55.6171841278108,26.6284954137977,14.2207816788212));
#59043=CARTESIAN_POINT('Ctrl Pts',(55.5382831097919,26.607961421887,14.2165569466049));
#59044=CARTESIAN_POINT('Ctrl Pts',(55.4583855019225,26.5913768684574,14.2123322143886));
#59045=CARTESIAN_POINT('Ctrl Pts',(55.3779202248495,26.5788171168518,14.2081074821723));
#59046=CARTESIAN_POINT('Ctrl Pts',(55.2974750448233,26.5662605021759,14.2038838051272));
#59047=CARTESIAN_POINT('Ctrl Pts',(55.2164629449355,26.5577267068027,14.1996601280821));
#59048=CARTESIAN_POINT('Ctrl Pts',(55.1353170553205,26.5532389686487,14.195436451037));
#59049=CARTESIAN_POINT('Ctrl Pts',(55.0540239386093,26.5487430881641,14.1912051107608));
#59050=CARTESIAN_POINT('Ctrl Pts',(54.9725970129515,26.5483079380591,14.1869737704845));
#59051=CARTESIAN_POINT('Ctrl Pts',(54.8914693069877,26.5519045487003,14.1827424302083));
#59052=CARTESIAN_POINT('Ctrl Pts',(54.8105747635226,26.5554908226172,14.1785232508808));
#59053=CARTESIAN_POINT('Ctrl Pts',(54.7299781675619,26.5630855880005,14.1743040715532));
#59054=CARTESIAN_POINT('Ctrl Pts',(54.6500995417821,26.5746093264509,14.1700848922257));
#59055=CARTESIAN_POINT('Ctrl Pts',(54.5699665639614,26.586169759153,14.1658522780542));
#59056=CARTESIAN_POINT('Ctrl Pts',(54.4902581029698,26.6017272499,14.1616196638828));
#59057=CARTESIAN_POINT('Ctrl Pts',(54.4114036022708,26.6212388664306,14.1573870497113));
#59058=CARTESIAN_POINT('Ctrl Pts',(54.3326615801128,26.6407226514724,14.1531604729665));
#59059=CARTESIAN_POINT('Ctrl Pts',(54.2547715461571,26.6641492495008,14.1489338962217));
#59060=CARTESIAN_POINT('Ctrl Pts',(54.1781556079684,26.6914242387814,14.1447073194769));
#59061=CARTESIAN_POINT('Ctrl Pts',(54.1016247045994,26.7186689559821,14.1404854337428));
#59062=CARTESIAN_POINT('Ctrl Pts',(54.0263655226236,26.7497534224188,14.1362635480088));
#59063=CARTESIAN_POINT('Ctrl Pts',(53.9527864136307,26.7845330166027,14.1320416622748));
#59064=CARTESIAN_POINT('Ctrl Pts',(53.879256931465,26.8192891530289,14.1278226240718));
#59065=CARTESIAN_POINT('Ctrl Pts',(53.8074056906419,26.8577352693669,14.1236035858687));
#59066=CARTESIAN_POINT('Ctrl Pts',(53.7376212244823,26.8996785776643,14.1193845476657));
#59067=CARTESIAN_POINT('Ctrl Pts',(53.6678595473853,26.9416081888063,14.1151668872468));
#59068=CARTESIAN_POINT('Ctrl Pts',(53.6001637024346,26.9870324847263,14.1109492268278));
#59069=CARTESIAN_POINT('Ctrl Pts',(53.534896540819,27.035713334593,14.1067315664088));
#59070=CARTESIAN_POINT('Ctrl Pts',(53.4696307373884,27.0843931714296,14.1025139937578));
#59071=CARTESIAN_POINT('Ctrl Pts',(53.4067938884794,27.1363291487885,14.0982964211067));
#59072=CARTESIAN_POINT('Ctrl Pts',(53.3467176629704,27.1912413748468,14.0940788484557));
#59073=CARTESIAN_POINT('Ctrl Pts',(53.2865394547117,27.2462468174773,14.0898541162394));
#59074=CARTESIAN_POINT('Ctrl Pts',(53.229131590767,27.3042383023091,14.0856293840231));
#59075=CARTESIAN_POINT('Ctrl Pts',(53.1747907925554,27.3648970677479,14.0814046518068));
#59076=CARTESIAN_POINT('Ctrl Pts',(53.1204635665281,27.4255406830238,14.0771809747617));
#59077=CARTESIAN_POINT('Ctrl Pts',(53.0692021511873,27.4888498710534,14.0729572977166));
#59078=CARTESIAN_POINT('Ctrl Pts',(53.0212618354783,27.5544739620937,14.0687336206715));
#59079=CARTESIAN_POINT('Ctrl Pts',(52.973234539227,27.6202171182451,14.0645022803952));
#59080=CARTESIAN_POINT('Ctrl Pts',(52.9285406403615,27.6882831816093,14.060270940119));
#59081=CARTESIAN_POINT('Ctrl Pts',(52.8873915795634,27.7582931457465,14.0560395998428));
#59082=CARTESIAN_POINT('Ctrl Pts',(52.8463607819126,27.8281018999764,14.0518204205153));
#59083=CARTESIAN_POINT('Ctrl Pts',(52.8088546108891,27.8998429543094,14.0476012411877));
#59084=CARTESIAN_POINT('Ctrl Pts',(52.7750350251377,27.9731206932477,14.0433820618602));
#59085=CARTESIAN_POINT('Ctrl Pts',(52.7381980024279,28.0529363880121,14.0387864406765));
#59086=CARTESIAN_POINT('Ctrl Pts',(52.70561483382,28.134833249766,14.0341908194928));
#59087=CARTESIAN_POINT('Ctrl Pts',(52.6775044184427,28.2183578033098,14.029595198309));
#59088=CARTESIAN_POINT('Ctrl Pts',(52.6494634471717,28.3016760173919,14.0250109301701));
#59089=CARTESIAN_POINT('Ctrl Pts',(52.625873331223,28.38661360295,14.0204266620313));
#59090=CARTESIAN_POINT('Ctrl Pts',(52.6069054817936,28.4726965987871,14.0158423938924));
#59091=CARTESIAN_POINT('Ctrl Pts',(52.5879312268089,28.5588086653633,14.0112565776189));
#59092=CARTESIAN_POINT('Ctrl Pts',(52.5735825333524,28.646066617719,14.0066707613454));
#59093=CARTESIAN_POINT('Ctrl Pts',(52.5639823990412,28.7339765088965,14.0020849450719));
#59094=CARTESIAN_POINT('Ctrl Pts',(52.55438226473,28.8218864000741,13.9974991287985));
#59095=CARTESIAN_POINT('Ctrl Pts',(52.5495308345984,28.9104479100502,13.992913312525));
#59096=CARTESIAN_POINT('Ctrl Pts',(52.5495001466462,28.9991522304455,13.9883274962515));
#59097=CARTESIAN_POINT('',(52.5495009948596,29.0022081227281,13.1883274961606));
#59098=CARTESIAN_POINT('Ctrl Pts',(52.549500146646,28.9991522312078,13.9883274962121));
#59099=CARTESIAN_POINT('Ctrl Pts',(52.549471270417,29.0826197940372,13.9840124086693));
#59100=CARTESIAN_POINT('Ctrl Pts',(52.5537112764691,29.1660567928118,13.9796973211265));
#59101=CARTESIAN_POINT('Ctrl Pts',(52.5621845880863,29.2490105769558,13.9753822335838));
#59102=CARTESIAN_POINT('Ctrl Pts',(52.5706635607001,29.3320197822995,13.9710642631426));
#59103=CARTESIAN_POINT('Ctrl Pts',(52.5833814218345,29.4145446995457,13.9667462927015));
#59104=CARTESIAN_POINT('Ctrl Pts',(52.6002510244919,29.4961402065424,13.9624283222603));
#59105=CARTESIAN_POINT('Ctrl Pts',(52.6171497683524,29.5778766647692,13.9581028927903));
#59106=CARTESIAN_POINT('Ctrl Pts',(52.6382144862426,29.6586800814982,13.9537774633202));
#59107=CARTESIAN_POINT('Ctrl Pts',(52.6633074022456,29.7381178453335,13.9494520338502));
#59108=CARTESIAN_POINT('Ctrl Pts',(52.6884241060414,29.8176309152461,13.9451225039233));
#59109=CARTESIAN_POINT('Ctrl Pts',(52.7175764641308,29.8957753472051,13.9407929739963));
#59110=CARTESIAN_POINT('Ctrl Pts',(52.7505784092967,29.9721382397982,13.9364634440694));
#59111=CARTESIAN_POINT('Ctrl Pts',(52.7836484656787,30.0486587342979,13.9321249786222));
#59112=CARTESIAN_POINT('Ctrl Pts',(52.8205837872558,30.123389956217,13.9277865131751));
#59113=CARTESIAN_POINT('Ctrl Pts',(52.8611521724728,30.195943234724,13.9234480477279));
#59114=CARTESIAN_POINT('Ctrl Pts',(52.8822502579406,30.2336754555833,13.9211917756502));
#59115=CARTESIAN_POINT('Ctrl Pts',(52.904330240533,30.2708190947748,13.9189355035725));
#59116=CARTESIAN_POINT('Ctrl Pts',(52.9273550057654,30.3073228284835,13.9166792314947));
#59117=CARTESIAN_POINT('Ctrl Pts',(52.9705479117009,30.3758013697613,13.9124466173232));
#59118=CARTESIAN_POINT('Ctrl Pts',(53.017218500924,30.4422643697956,13.9082140031518));
#59119=CARTESIAN_POINT('Ctrl Pts',(53.0671526695653,30.506337096148,13.9039813889803));
#59120=CARTESIAN_POINT('Ctrl Pts',(53.1170156118037,30.5703184287723,13.8997548122355));
#59121=CARTESIAN_POINT('Ctrl Pts',(53.1701326044661,30.6319158960519,13.8955282354907));
#59122=CARTESIAN_POINT('Ctrl Pts',(53.2262455051986,30.6907824349016,13.8913016587459));
#59123=CARTESIAN_POINT('Ctrl Pts',(53.282296127109,30.7495836387098,13.8870797730119));
#59124=CARTESIAN_POINT('Ctrl Pts',(53.3413357311895,30.8056596021463,13.8828578872779));
#59125=CARTESIAN_POINT('Ctrl Pts',(53.4030659291315,30.8586962697814,13.8786360015438));
#59126=CARTESIAN_POINT('Ctrl Pts',(53.4647544919693,30.9116971658289,13.8744169633408));
#59127=CARTESIAN_POINT('Ctrl Pts',(53.5291296930227,30.9616625354226,13.8701979251378));
#59128=CARTESIAN_POINT('Ctrl Pts',(53.5958572239643,31.0083160394985,13.8659788869348));
#59129=CARTESIAN_POINT('Ctrl Pts',(53.662562964127,31.0549543082407,13.8617612265158));
#59130=CARTESIAN_POINT('Ctrl Pts',(53.7316191281786,31.0982825933431,13.8575435660968));
#59131=CARTESIAN_POINT('Ctrl Pts',(53.802660454684,31.1380664777369,13.8533259056779));
#59132=CARTESIAN_POINT('Ctrl Pts',(53.8737003028462,31.1778495342431,13.8491083330268));
#59133=CARTESIAN_POINT('Ctrl Pts',(53.9467248254334,31.2140881107318,13.8448907603758));
#59134=CARTESIAN_POINT('Ctrl Pts',(54.0213433192699,31.2465932767776,13.8406731877248));
#59135=CARTESIAN_POINT('Ctrl Pts',(54.0960884821692,31.2791536221591,13.8364484555085));
#59136=CARTESIAN_POINT('Ctrl Pts',(54.1724326019667,31.3079676903907,13.8322237232922));
#59137=CARTESIAN_POINT('Ctrl Pts',(54.2499637077153,31.3328942989891,13.8279989910759));
#59138=CARTESIAN_POINT('Ctrl Pts',(54.3274754492571,31.3578146819056,13.8237753140308));
#59139=CARTESIAN_POINT('Ctrl Pts',(54.4061731280681,31.3788494469736,13.8195516369857));
#59140=CARTESIAN_POINT('Ctrl Pts',(54.4856325046381,31.395908247349,13.8153279599406));
#59141=CARTESIAN_POINT('Ctrl Pts',(54.5652360483783,31.4129979983697,13.8110966196644));
#59142=CARTESIAN_POINT('Ctrl Pts',(54.6456035919012,31.4260972932283,13.8068652793881));
#59143=CARTESIAN_POINT('Ctrl Pts',(54.726302872835,31.4351673726012,13.8026339391119));
#59144=CARTESIAN_POINT('Ctrl Pts',(54.8067702225712,31.4442113844015,13.7984147597844));
#59145=CARTESIAN_POINT('Ctrl Pts',(54.8875669458817,31.4492493645495,13.7941955804569));
#59146=CARTESIAN_POINT('Ctrl Pts',(54.9682657629379,31.4502945105024,13.7899764011293));
#59147=CARTESIAN_POINT('Ctrl Pts',(55.0492215437141,31.451342984442,13.7857437869579));
#59148=CARTESIAN_POINT('Ctrl Pts',(55.130379891234,31.4483770276291,13.7815111727864));
#59149=CARTESIAN_POINT('Ctrl Pts',(55.2113099121558,31.4413722311489,13.7772785586149));
#59150=CARTESIAN_POINT('Ctrl Pts',(55.2921244940016,31.4343774263531,13.7730519818701));
#59151=CARTESIAN_POINT('Ctrl Pts',(55.3727109371319,31.4233552637546,13.7688254051253));
#59152=CARTESIAN_POINT('Ctrl Pts',(55.4526375833698,31.4083333382489,13.7645988283806));
#59153=CARTESIAN_POINT('Ctrl Pts',(55.5324755202858,31.393328085341,13.7603769426465));
#59154=CARTESIAN_POINT('Ctrl Pts',(55.6116546611306,31.374331975729,13.7561550569125));
#59155=CARTESIAN_POINT('Ctrl Pts',(55.6897491254512,31.3514243330244,13.7519331711785));
#59156=CARTESIAN_POINT('Ctrl Pts',(55.7677909174774,31.3285321408145,13.7477141329755));
#59157=CARTESIAN_POINT('Ctrl Pts',(55.8447490413464,31.3017337856434,13.7434950947724));
#59158=CARTESIAN_POINT('Ctrl Pts',(55.9202096991569,31.2711592545609,13.7392760565694));
#59159=CARTESIAN_POINT('Ctrl Pts',(55.9956457142676,31.2405947080055,13.7350583961504));
#59160=CARTESIAN_POINT('Ctrl Pts',(56.0695848042591,31.2062566088348,13.7308407357315));
#59161=CARTESIAN_POINT('Ctrl Pts',(56.1416314855606,31.1683237307138,13.7266230753125));
#59162=CARTESIAN_POINT('Ctrl Pts',(56.213676667598,31.1303916419617,13.7224055026615));
#59163=CARTESIAN_POINT('Ctrl Pts',(56.2838291087358,31.0888651404542,13.7181879300104));
#59164=CARTESIAN_POINT('Ctrl Pts',(56.351717630243,31.043969103996,13.7139703573594));
#59165=CARTESIAN_POINT('Ctrl Pts',(56.419721396309,30.9989968540072,13.7097456251431));
#59166=CARTESIAN_POINT('Ctrl Pts',(56.4854531640172,30.9506438823338,13.7055208929268));
#59167=CARTESIAN_POINT('Ctrl Pts',(56.5485702286235,30.8991789007413,13.7012961607105));
#59168=CARTESIAN_POINT('Ctrl Pts',(56.6116715290809,30.8477267730678,13.6970724836654));
#59169=CARTESIAN_POINT('Ctrl Pts',(56.6721591004684,30.7931645178053,13.6928488066203));
#59170=CARTESIAN_POINT('Ctrl Pts',(56.7297262012426,30.7357988128625,13.6886251295752));
#59171=CARTESIAN_POINT('Ctrl Pts',(56.7873977489227,30.6783290264165,13.6843937892989));
#59172=CARTESIAN_POINT('Ctrl Pts',(56.8421379234027,30.6180459701271,13.6801624490227));
#59173=CARTESIAN_POINT('Ctrl Pts',(56.8936788884007,30.5552911359696,13.6759311087465));
#59174=CARTESIAN_POINT('Ctrl Pts',(56.9450717237301,30.492716660344,13.6717119294189));
#59175=CARTESIAN_POINT('Ctrl Pts',(56.9932835098872,30.4276850109937,13.6674927500914));
#59176=CARTESIAN_POINT('Ctrl Pts',(57.0380927057488,30.3605617857244,13.6632735707639));
#59177=CARTESIAN_POINT('Ctrl Pts',(57.083044584466,30.2932248245629,13.6590409565924));
#59178=CARTESIAN_POINT('Ctrl Pts',(57.1247393348929,30.223532485968,13.6548083424209));
#59179=CARTESIAN_POINT('Ctrl Pts',(57.1629219035332,30.1518329259126,13.6505757282495));
#59180=CARTESIAN_POINT('Ctrl Pts',(57.2010500083245,30.0802356385473,13.6463491515047));
#59181=CARTESIAN_POINT('Ctrl Pts',(57.2356756648905,30.0066372228569,13.6421225747599));
#59182=CARTESIAN_POINT('Ctrl Pts',(57.2665870254661,29.9314147872933,13.6378959980151));
#59183=CARTESIAN_POINT('Ctrl Pts',(57.297464078011,29.8562758399226,13.6336741122811));
#59184=CARTESIAN_POINT('Ctrl Pts',(57.324634850161,29.7795168817087,13.629452226547));
#59185=CARTESIAN_POINT('Ctrl Pts',(57.3479340309009,29.7015383357576,13.625230340813));
#59186=CARTESIAN_POINT('Ctrl Pts',(57.3712174970659,29.6236123839176,13.62101130261));
#59187=CARTESIAN_POINT('Ctrl Pts',(57.3906344253783,29.5444689220006,13.616792264407));
#59188=CARTESIAN_POINT('Ctrl Pts',(57.4060685803433,29.4645258191797,13.6125732262039));
#59189=CARTESIAN_POINT('Ctrl Pts',(57.4214976950761,29.3846088228616,13.608355565785));
#59190=CARTESIAN_POINT('Ctrl Pts',(57.4329465314363,29.3038931600108,13.604137905366));
#59191=CARTESIAN_POINT('Ctrl Pts',(57.4403497477094,29.2228078967508,13.599920244947));
#59192=CARTESIAN_POINT('Ctrl Pts',(57.4477528099245,29.1417243208446,13.595702672296));
#59193=CARTESIAN_POINT('Ctrl Pts',(57.4511103783708,29.0602716225518,13.5914850996449));
#59194=CARTESIAN_POINT('Ctrl Pts',(57.4504090162236,28.978883579614,13.5872675269939));
#59195=CARTESIAN_POINT('Ctrl Pts',(57.449706463475,28.8973573759256,13.5830427947776));
#59196=CARTESIAN_POINT('Ctrl Pts',(57.4449311983527,28.8158965141655,13.5788180625613));
#59197=CARTESIAN_POINT('Ctrl Pts',(57.4361220543256,28.7349347506204,13.574593330345));
#59198=CARTESIAN_POINT('Ctrl Pts',(57.4273151104745,28.6539932081249,13.5703696532999));
#59199=CARTESIAN_POINT('Ctrl Pts',(57.4144763969283,28.5735509715438,13.5661459762548));
#59200=CARTESIAN_POINT('Ctrl Pts',(57.39769617251,28.4940322991229,13.5619222992097));
#59201=CARTESIAN_POINT('Ctrl Pts',(57.3808855028808,28.414369351948,13.5576909589334));
#59202=CARTESIAN_POINT('Ctrl Pts',(57.360119149602,28.3356337681933,13.5534596186572));
#59203=CARTESIAN_POINT('Ctrl Pts',(57.3355377544693,28.2582361241957,13.549228278381));
#59204=CARTESIAN_POINT('Ctrl Pts',(57.3110270067123,28.1810609224311,13.5450090990535));
#59205=CARTESIAN_POINT('Ctrl Pts',(57.2827233539127,28.1052163776052,13.5407899197259));
#59206=CARTESIAN_POINT('Ctrl Pts',(57.2508128615668,28.0310873557408,13.5365707403984));
#59207=CARTESIAN_POINT('Ctrl Pts',(57.2188007588242,27.9567222899056,13.5323381262269));
#59208=CARTESIAN_POINT('Ctrl Pts',(57.1830397228031,27.8838071160754,13.5281055120555));
#59209=CARTESIAN_POINT('Ctrl Pts',(57.1436829441875,27.8127453159495,13.523872897884));
#59210=CARTESIAN_POINT('Ctrl Pts',(57.1043823043211,27.7417848788093,13.5196463211392));
#59211=CARTESIAN_POINT('Ctrl Pts',(57.0614963318947,27.6726729677245,13.5154197443944));
#59212=CARTESIAN_POINT('Ctrl Pts',(57.0152260248969,27.6057925840901,13.5111931676496));
#59213=CARTESIAN_POINT('Ctrl Pts',(56.9690070725819,27.538986429937,13.5069712819156));
#59214=CARTESIAN_POINT('Ctrl Pts',(56.9194115122677,27.4744072620696,13.5027493961816));
#59215=CARTESIAN_POINT('Ctrl Pts',(56.8666852335074,27.4124117381999,13.4985275104476));
#59216=CARTESIAN_POINT('Ctrl Pts',(56.8139945169869,27.3504580283884,13.4943084722445));
#59217=CARTESIAN_POINT('Ctrl Pts',(56.7581775759748,27.291084854603,13.4900894340415));
#59218=CARTESIAN_POINT('Ctrl Pts',(56.6995216509783,27.2346172064235,13.4858703958385));
#59219=CARTESIAN_POINT('Ctrl Pts',(56.6408848808684,27.1781679985193,13.4816527354195));
#59220=CARTESIAN_POINT('Ctrl Pts',(56.5794113023675,27.1246227538218,13.4774350750006));
#59221=CARTESIAN_POINT('Ctrl Pts',(56.5154252548821,27.074269866553,13.4732174145816));
#59222=CARTESIAN_POINT('Ctrl Pts',(56.4514405389221,27.0239180271089,13.4689998419305));
#59223=CARTESIAN_POINT('Ctrl Pts',(56.3849438237229,26.9767586993703,13.4647822692795));
#59224=CARTESIAN_POINT('Ctrl Pts',(56.316291657979,26.9330393034373,13.4605646966285));
#59225=CARTESIAN_POINT('Ctrl Pts',(56.2475229513475,26.8892456913867,13.4563399644122));
#59226=CARTESIAN_POINT('Ctrl Pts',(56.1765918672738,26.8489039454176,13.4521152321959));
#59227=CARTESIAN_POINT('Ctrl Pts',(56.1038833924458,26.8122176283089,13.4478904999796));
#59228=CARTESIAN_POINT('Ctrl Pts',(56.0311930773219,26.7755404739926,13.4436668229345));
#59229=CARTESIAN_POINT('Ctrl Pts',(55.9567266939224,26.7425170923501,13.4394431458894));
#59230=CARTESIAN_POINT('Ctrl Pts',(55.8808892577429,26.7133027385347,13.4352194688443));
#59231=CARTESIAN_POINT('Ctrl Pts',(55.8049142258629,26.6840353796378,13.430988128568));
#59232=CARTESIAN_POINT('Ctrl Pts',(55.7275636124464,26.6585910053715,13.4267567882918));
#59233=CARTESIAN_POINT('Ctrl Pts',(55.6492583847897,26.6370751599384,13.4225254480155));
#59234=CARTESIAN_POINT('Ctrl Pts',(55.5711782077782,26.6156211514354,13.418306268688));
#59235=CARTESIAN_POINT('Ctrl Pts',(55.4921493588124,26.5980731380775,13.4140870893605));
#59236=CARTESIAN_POINT('Ctrl Pts',(55.4125959674281,26.5844845648057,13.409867910033));
#59237=CARTESIAN_POINT('Ctrl Pts',(55.3327892596243,26.57085272237,13.4056352958615));
#59238=CARTESIAN_POINT('Ctrl Pts',(55.2521578355119,26.5611549021207,13.40140268169));
#59239=CARTESIAN_POINT('Ctrl Pts',(55.1711235428509,26.5554822596099,13.3971700675186));
#59240=CARTESIAN_POINT('Ctrl Pts',(55.0902048379992,26.5498177085909,13.3929434907738));
#59241=CARTESIAN_POINT('Ctrl Pts',(55.0088848655,26.5481669640471,13.3887169140289));
#59242=CARTESIAN_POINT('Ctrl Pts',(54.9275943200526,26.550569930063,13.3844903372841));
#59243=CARTESIAN_POINT('Ctrl Pts',(54.8463939976978,26.5529702290649,13.3802684515501));
#59244=CARTESIAN_POINT('Ctrl Pts',(54.7652234995034,26.5594152851691,13.3760465658161));
#59245=CARTESIAN_POINT('Ctrl Pts',(54.6845158614266,26.5698930047612,13.3718246800821));
#59246=CARTESIAN_POINT('Ctrl Pts',(54.6038626581489,26.5803636574564,13.367605641879));
#59247=CARTESIAN_POINT('Ctrl Pts',(54.5236721544562,26.5948615120148,13.363386603676));
#59248=CARTESIAN_POINT('Ctrl Pts',(54.4443733337705,26.6133225484421,13.359167565473));
#59249=CARTESIAN_POINT('Ctrl Pts',(54.3651004091885,26.6317775561681,13.354949905054));
#59250=CARTESIAN_POINT('Ctrl Pts',(54.2867190414284,26.6541930702489,13.350732244635));
#59251=CARTESIAN_POINT('Ctrl Pts',(54.2096477134736,26.6804540286551,13.3465145842161));
#59252=CARTESIAN_POINT('Ctrl Pts',(54.132577989344,26.7067144405806,13.342297011565));
#59253=CARTESIAN_POINT('Ctrl Pts',(54.0568186901607,26.7368199867859,13.338079438914));
#59254=CARTESIAN_POINT('Ctrl Pts',(53.982771463542,26.770606280933,13.3338618662629));
#59255=CARTESIAN_POINT('Ctrl Pts',(53.9085985376188,26.8044499292022,13.3296371340466));
#59256=CARTESIAN_POINT('Ctrl Pts',(53.8361439240233,26.8419866328989,13.3254124018303));
#59257=CARTESIAN_POINT('Ctrl Pts',(53.7657879634133,26.8830042752182,13.3211876696141));
#59258=CARTESIAN_POINT('Ctrl Pts',(53.695449574942,26.9240116729513,13.3169639925689));
#59259=CARTESIAN_POINT('Ctrl Pts',(53.6272091701636,26.968497998349,13.3127403155238));
#59260=CARTESIAN_POINT('Ctrl Pts',(53.5614174717795,27.0162080352268,13.3085166384787));
#59261=CARTESIAN_POINT('Ctrl Pts',(53.4955064041858,27.0640046348403,13.3042852982025));
#59262=CARTESIAN_POINT('Ctrl Pts',(53.4320532848467,27.1150363428642,13.3000539579262));
#59263=CARTESIAN_POINT('Ctrl Pts',(53.3713758218373,27.1690074996593,13.29582261765));
#59264=CARTESIAN_POINT('Ctrl Pts',(53.3108727469579,27.2228235423703,13.2916034383225));
#59265=CARTESIAN_POINT('Ctrl Pts',(53.2531296615676,27.2795617819552,13.287384258995));
#59266=CARTESIAN_POINT('Ctrl Pts',(53.1984222930922,27.3388955433288,13.2831650796675));
#59267=CARTESIAN_POINT('Ctrl Pts',(53.1441786834718,27.397726327535,13.2789816666697));
#59268=CARTESIAN_POINT('Ctrl Pts',(53.0927073678689,27.4593391010681,13.2747982536718));
#59269=CARTESIAN_POINT('Ctrl Pts',(53.0443115060476,27.5234388720333,13.2706148406739));
#59270=CARTESIAN_POINT('Ctrl Pts',(52.9959787824364,27.5874550171542,13.2664368854404));
#59271=CARTESIAN_POINT('Ctrl Pts',(52.9507138383018,27.6539513481805,13.2622589302069));
#59272=CARTESIAN_POINT('Ctrl Pts',(52.9087821854626,27.7225970478501,13.2580809749733));
#59273=CARTESIAN_POINT('Ctrl Pts',(52.8668916944516,27.7911753620887,13.2539071209918));
#59274=CARTESIAN_POINT('Ctrl Pts',(52.8283282490237,27.8618984545656,13.2497332670103));
#59275=CARTESIAN_POINT('Ctrl Pts',(52.7933153586562,27.9344047937151,13.2455594130288));
#59276=CARTESIAN_POINT('Ctrl Pts',(52.7583255353572,28.006863364495,13.241388308851));
#59277=CARTESIAN_POINT('Ctrl Pts',(52.7268818296577,28.0811024219658,13.2372172046732));
#59278=CARTESIAN_POINT('Ctrl Pts',(52.6991621075189,28.1567353662561,13.2330461004954));
#59279=CARTESIAN_POINT('Ctrl Pts',(52.6714438038877,28.2323644401648,13.2288752097664));
#59280=CARTESIAN_POINT('Ctrl Pts',(52.6474492835787,28.3093868176467,13.2247043190374));
#59281=CARTESIAN_POINT('Ctrl Pts',(52.6273080105467,28.3873965612371,13.2205334283085));
#59282=CARTESIAN_POINT('Ctrl Pts',(52.6071677410357,28.4654024180612,13.2163627453904));
#59283=CARTESIAN_POINT('Ctrl Pts',(52.5908804484917,28.5443950799622,13.2121920624724));
#59284=CARTESIAN_POINT('Ctrl Pts',(52.5785249940676,28.6239560588911,13.2080213795544));
#59285=CARTESIAN_POINT('Ctrl Pts',(52.5661601393466,28.7035775695332,13.2038475234906));
#59286=CARTESIAN_POINT('Ctrl Pts',(52.5577331587781,28.7837677880482,13.1996736674268));
#59287=CARTESIAN_POINT('Ctrl Pts',(52.5532711845619,28.8641016788011,13.195499811363));
#59288=CARTESIAN_POINT('Ctrl Pts',(52.550715379667,28.9101166805143,13.193109039646));
#59289=CARTESIAN_POINT('Ctrl Pts',(52.5494595182279,28.9561787562162,13.1907182679291));
#59290=CARTESIAN_POINT('Ctrl Pts',(52.5495009948587,29.0022081217367,13.1883274962121));
#59291=CARTESIAN_POINT('',(52.5495001658419,28.9990984507376,12.3883274961653));
#59292=CARTESIAN_POINT('Ctrl Pts',(52.5495009948596,29.0022081227281,13.1883274961606));
#59293=CARTESIAN_POINT('Ctrl Pts',(52.5495956779836,29.107284212101,13.1828698293045));
#59294=CARTESIAN_POINT('Ctrl Pts',(52.5564525380247,29.2120617946342,13.1774121624485));
#59295=CARTESIAN_POINT('Ctrl Pts',(52.5699345169715,29.3158037336601,13.1719544955924));
#59296=CARTESIAN_POINT('Ctrl Pts',(52.582691258624,29.4139650733196,13.1667904134956));
#59297=CARTESIAN_POINT('Ctrl Pts',(52.6013790218718,29.511199695907,13.1616263313989));
#59298=CARTESIAN_POINT('Ctrl Pts',(52.6258433201928,29.6069022241902,13.1564622493021));
#59299=CARTESIAN_POINT('Ctrl Pts',(52.6458948867304,29.6853424716276,13.1522296351306));
#59300=CARTESIAN_POINT('Ctrl Pts',(52.6698753221035,29.7629337919622,13.1479970209591));
#59301=CARTESIAN_POINT('Ctrl Pts',(52.6976960801471,29.8392537820171,13.1437644067877));
#59302=CARTESIAN_POINT('Ctrl Pts',(52.7254771544916,29.9154649087722,13.1395378300429));
#59303=CARTESIAN_POINT('Ctrl Pts',(52.7570875139937,29.9904078741316,13.1353112532981));
#59304=CARTESIAN_POINT('Ctrl Pts',(52.7923882008275,30.0636730673259,13.1310846765533));
#59305=CARTESIAN_POINT('Ctrl Pts',(52.8276497079867,30.1368569446398,13.1268627908193));
#59306=CARTESIAN_POINT('Ctrl Pts',(52.8665932034325,30.2083663334484,13.1226409050853));
#59307=CARTESIAN_POINT('Ctrl Pts',(52.9090312856088,30.2778106610282,13.1184190193512));
#59308=CARTESIAN_POINT('Ctrl Pts',(52.9514407446146,30.3472081505623,13.1141999811482));
#59309=CARTESIAN_POINT('Ctrl Pts',(52.9973398675489,30.4145429497611,13.1099809429452));
#59310=CARTESIAN_POINT('Ctrl Pts',(53.0464954781693,30.4794493344441,13.1057619047422));
#59311=CARTESIAN_POINT('Ctrl Pts',(53.0956350363595,30.5443345230683,13.1015442443232));
#59312=CARTESIAN_POINT('Ctrl Pts',(53.1480286900404,30.6067925020412,13.0973265839043));
#59313=CARTESIAN_POINT('Ctrl Pts',(53.2034009219129,30.6664879245337,13.0931089234853));
#59314=CARTESIAN_POINT('Ctrl Pts',(53.2587720015101,30.726182104787,13.0888913508343));
#59315=CARTESIAN_POINT('Ctrl Pts',(53.3171212192789,30.7831135030728,13.0846737781832));
#59316=CARTESIAN_POINT('Ctrl Pts',(53.3781348656214,30.8369822361381,13.0804562055322));
#59317=CARTESIAN_POINT('Ctrl Pts',(53.4392520860381,30.8909424143881,13.0762314733159));
#59318=CARTESIAN_POINT('Ctrl Pts',(53.5030424344527,30.9418292162612,13.0720067410996));
#59319=CARTESIAN_POINT('Ctrl Pts',(53.5691572857285,30.9893816569518,13.0677820088833));
#59320=CARTESIAN_POINT('Ctrl Pts',(53.6352556241266,31.0369222209214,13.0635583318382));
#59321=CARTESIAN_POINT('Ctrl Pts',(53.7036769013223,31.0811298539567,13.0593346547931));
#59322=CARTESIAN_POINT('Ctrl Pts',(53.7740451909773,31.1217881742139,13.055110977748));
#59323=CARTESIAN_POINT('Ctrl Pts',(53.8445411533833,31.1625202629204,13.0508796374718));
#59324=CARTESIAN_POINT('Ctrl Pts',(53.9169907734289,31.1996899566632,13.0466482971955));
#59325=CARTESIAN_POINT('Ctrl Pts',(53.9909946325807,31.2331274971481,13.0424169569193));
#59326=CARTESIAN_POINT('Ctrl Pts',(54.0647858032994,31.2664689375354,13.0381977775917));
#59327=CARTESIAN_POINT('Ctrl Pts',(54.140121837128,31.2960995593441,13.0339785982642));
#59328=CARTESIAN_POINT('Ctrl Pts',(54.2165920855353,31.3219005770175,13.0297594189366));
#59329=CARTESIAN_POINT('Ctrl Pts',(54.2933058329201,31.3477837511053,13.0255268047651));
#59330=CARTESIAN_POINT('Ctrl Pts',(54.3714463581967,31.3699091342994,13.0212941905937));
#59331=CARTESIAN_POINT('Ctrl Pts',(54.4506111343204,31.3881210447269,13.0170615764222));
#59332=CARTESIAN_POINT('Ctrl Pts',(54.5296629893242,31.4063069775741,13.0128349996774));
#59333=CARTESIAN_POINT('Ctrl Pts',(54.6097357444841,31.4205904213417,13.0086084229326));
#59334=CARTESIAN_POINT('Ctrl Pts',(54.6904101592007,31.4308649449268,13.0043818461878));
#59335=CARTESIAN_POINT('Ctrl Pts',(54.7709950346588,31.4411280649804,13.0001599604538));
#59336=CARTESIAN_POINT('Ctrl Pts',(54.8521797843075,31.4473910474798,12.9959380747198));
#59337=CARTESIAN_POINT('Ctrl Pts',(54.9335347643349,31.4495984614724,12.9917161889857));
#59338=CARTESIAN_POINT('Ctrl Pts',(55.0148348729512,31.4518043866327,12.9874971507827));
#59339=CARTESIAN_POINT('Ctrl Pts',(55.0963045207342,31.4499601633729,12.9832781125797));
#59340=CARTESIAN_POINT('Ctrl Pts',(55.1775099876806,31.4440622852689,12.9790590743767));
#59341=CARTESIAN_POINT('Ctrl Pts',(55.2586889358821,31.4381663331968,12.9748414139577));
#59342=CARTESIAN_POINT('Ctrl Pts',(55.3396034116048,31.4282193888435,12.9706237535387));
#59343=CARTESIAN_POINT('Ctrl Pts',(55.4198221256285,31.4142699999861,12.9664060931198));
#59344=CARTESIAN_POINT('Ctrl Pts',(55.5000391703312,31.4003209014101,12.9621885204687));
#59345=CARTESIAN_POINT('Ctrl Pts',(55.5795600246435,31.3823696046746,12.9579709478177));
#59346=CARTESIAN_POINT('Ctrl Pts',(55.6579623551695,31.3605160006193,12.9537533751666));
#59347=CARTESIAN_POINT('Ctrl Pts',(55.7364977780323,31.3386252988501,12.9495286429503));
#59348=CARTESIAN_POINT('Ctrl Pts',(55.8139104282942,31.3128191613027,12.9453039107341));
#59349=CARTESIAN_POINT('Ctrl Pts',(55.8897915935107,31.283247943198,12.9410791785178));
#59350=CARTESIAN_POINT('Ctrl Pts',(55.9656538066105,31.2536841108151,12.9368555014727));
#59351=CARTESIAN_POINT('Ctrl Pts',(56.0399848829157,31.220357288479,12.9326318244276));
#59352=CARTESIAN_POINT('Ctrl Pts',(56.1123986612753,31.183465014236,12.9284081473824));
#59353=CARTESIAN_POINT('Ctrl Pts',(56.1849438236198,31.1465058044719,12.9241768071062));
#59354=CARTESIAN_POINT('Ctrl Pts',(56.2555643319928,31.1059684467035,12.91994546683));
#59355=CARTESIAN_POINT('Ctrl Pts',(56.3239003450831,31.0620955667206,12.9157141265537));
#59356=CARTESIAN_POINT('Ctrl Pts',(56.3920399592316,31.0183487781911,12.9114949472262));
#59357=CARTESIAN_POINT('Ctrl Pts',(56.4579078698647,30.9712859468861,12.9072757678987));
#59358=CARTESIAN_POINT('Ctrl Pts',(56.5211808792693,30.9211868682004,12.9030565885712));
#59359=CARTESIAN_POINT('Ctrl Pts',(56.5846553645874,30.870928262447,12.8988239743997));
#59360=CARTESIAN_POINT('Ctrl Pts',(56.6457544591394,30.8174270950118,12.8945913602282));
#59361=CARTESIAN_POINT('Ctrl Pts',(56.7041284369947,30.7609362623974,12.8903587460568));
#59362=CARTESIAN_POINT('Ctrl Pts',(56.7624191498517,30.7045260086514,12.886132169312));
#59363=CARTESIAN_POINT('Ctrl Pts',(56.8179921352872,30.6451348798985,12.8819055925672));
#59364=CARTESIAN_POINT('Ctrl Pts',(56.8705298812866,30.5830566045514,12.8776790158224));
#59365=CARTESIAN_POINT('Ctrl Pts',(56.9230093164717,30.5210472289015,12.8734571300884));
#59366=CARTESIAN_POINT('Ctrl Pts',(56.9724599073562,30.4563569855376,12.8692352443543));
#59367=CARTESIAN_POINT('Ctrl Pts',(57.0186012586211,30.3893160938725,12.8650133586203));
#59368=CARTESIAN_POINT('Ctrl Pts',(57.0647114889755,30.3223204192099,12.8607943204173));
#59369=CARTESIAN_POINT('Ctrl Pts',(57.1075166499194,30.2529776267519,12.8565752822142));
#59370=CARTESIAN_POINT('Ctrl Pts',(57.1467776826562,30.1816496228786,12.8523562440112));
#59371=CARTESIAN_POINT('Ctrl Pts',(57.1860258941712,30.1103449121308,12.8481385835922));
#59372=CARTESIAN_POINT('Ctrl Pts',(57.221732052134,30.0370566841063,12.8439209231733));
#59373=CARTESIAN_POINT('Ctrl Pts',(57.2537020854455,29.9621731445319,12.8397032627543));
#59374=CARTESIAN_POINT('Ctrl Pts',(57.2856714534728,29.8872911632557,12.8354856901033));
#59375=CARTESIAN_POINT('Ctrl Pts',(57.3139046701088,29.8108143641371,12.8312681174522));
#59376=CARTESIAN_POINT('Ctrl Pts',(57.3382556076688,29.7331513917367,12.8270505448012));
#59377=CARTESIAN_POINT('Ctrl Pts',(57.3626478823059,29.6553565821013,12.8228258125849));
#59378=CARTESIAN_POINT('Ctrl Pts',(57.3831445523268,29.5763720160536,12.8186010803686));
#59379=CARTESIAN_POINT('Ctrl Pts',(57.3996492360996,29.4966223854064,12.8143763481523));
#59380=CARTESIAN_POINT('Ctrl Pts',(57.4161497976545,29.4168926730656,12.8101526711072));
#59381=CARTESIAN_POINT('Ctrl Pts',(57.4286603162007,29.3363987421303,12.8059289940621));
#59382=CARTESIAN_POINT('Ctrl Pts',(57.4371362651929,29.2555720541874,12.8017053170169));
#59383=CARTESIAN_POINT('Ctrl Pts',(57.4456275925285,29.1745987182919,12.7974739767407));
#59384=CARTESIAN_POINT('Ctrl Pts',(57.450069695877,29.0932918840432,12.7932426364645));
#59385=CARTESIAN_POINT('Ctrl Pts',(57.4504701979716,29.0120854810866,12.7890112961882));
#59386=CARTESIAN_POINT('Ctrl Pts',(57.4508695490159,28.9311124668059,12.7847921168607));
#59387=CARTESIAN_POINT('Ctrl Pts',(57.4472506024997,28.8502397583826,12.7805729375332));
#59388=CARTESIAN_POINT('Ctrl Pts',(57.4396721087627,28.7698907830503,12.7763537582057));
#59389=CARTESIAN_POINT('Ctrl Pts',(57.4320694833468,28.6892859579748,12.7721211440342));
#59390=CARTESIAN_POINT('Ctrl Pts',(57.4204537507425,28.608908417405,12.7678885298628));
#59391=CARTESIAN_POINT('Ctrl Pts',(57.4048466558375,28.5291891973339,12.7636559156913));
#59392=CARTESIAN_POINT('Ctrl Pts',(57.389261822988,28.449583689245,12.7594293389465));
#59393=CARTESIAN_POINT('Ctrl Pts',(57.3696970239834,28.3706350887212,12.7552027622017));
#59394=CARTESIAN_POINT('Ctrl Pts',(57.3462257918297,28.2927696388353,12.7509761854569));
#59395=CARTESIAN_POINT('Ctrl Pts',(57.3227806100257,28.2149906105821,12.7467542997229));
#59396=CARTESIAN_POINT('Ctrl Pts',(57.2954377434726,28.138292786793,12.7425324139889));
#59397=CARTESIAN_POINT('Ctrl Pts',(57.2643215411068,28.0630911418501,12.7383105282549));
#59398=CARTESIAN_POINT('Ctrl Pts',(57.2332263256545,27.9879402180846,12.7340914900518));
#59399=CARTESIAN_POINT('Ctrl Pts',(57.1983630061319,27.9142838970988,12.7298724518488));
#59400=CARTESIAN_POINT('Ctrl Pts',(57.159905014939,27.8425197295671,12.7256534136458));
#59401=CARTESIAN_POINT('Ctrl Pts',(57.121459582724,27.7707789975962,12.7214357532268));
#59402=CARTESIAN_POINT('Ctrl Pts',(57.0794220293684,27.7009296010969,12.7172180928079));
#59403=CARTESIAN_POINT('Ctrl Pts',(57.0340123391669,27.6333456713138,12.7130004323889));
#59404=CARTESIAN_POINT('Ctrl Pts',(56.9886035939239,27.5657631479268,12.7087828597379));
#59405=CARTESIAN_POINT('Ctrl Pts',(56.9398231114118,27.5004463824609,12.7045652870868));
#59406=CARTESIAN_POINT('Ctrl Pts',(56.8879341209679,27.4377404169328,12.7003477144358));
#59407=CARTESIAN_POINT('Ctrl Pts',(56.8359570460632,27.3749280045244,12.6961229822195));
#59408=CARTESIAN_POINT('Ctrl Pts',(56.7808612031716,27.3147356191941,12.6918982500032));
#59409=CARTESIAN_POINT('Ctrl Pts',(56.7229503642611,27.2574753108514,12.6876735177869));
#59410=CARTESIAN_POINT('Ctrl Pts',(56.66505398919,27.2002293038712,12.6834498407418));
#59411=CARTESIAN_POINT('Ctrl Pts',(56.6043443856516,27.145914204406,12.6792261636967));
#59412=CARTESIAN_POINT('Ctrl Pts',(56.5411592342224,27.0948022504813,12.6750024866516));
#59413=CARTESIAN_POINT('Ctrl Pts',(56.4778594427736,27.0435975615506,12.6707711463753));
#59414=CARTESIAN_POINT('Ctrl Pts',(56.4120755036895,26.9956079070793,12.6665398060991));
#59415=CARTESIAN_POINT('Ctrl Pts',(56.3441755579257,26.9510631245753,12.6623084658229));
#59416=CARTESIAN_POINT('Ctrl Pts',(56.2764707578379,26.9066463645844,12.6580892864954));
#59417=CARTESIAN_POINT('Ctrl Pts',(56.2066625324019,26.8656548605482,12.6538701071678));
#59418=CARTESIAN_POINT('Ctrl Pts',(56.1351380467958,26.8282698453268,12.6496509278403));
#59419=CARTESIAN_POINT('Ctrl Pts',(56.0633858106653,26.7907657875603,12.6454183136688));
#59420=CARTESIAN_POINT('Ctrl Pts',(55.9896394877231,26.7567517592118,12.6411856994974));
#59421=CARTESIAN_POINT('Ctrl Pts',(55.9142724797684,26.7264441764632,12.6369530853259));
#59422=CARTESIAN_POINT('Ctrl Pts',(55.8390129757738,26.6961798246356,12.6327265085811));
#59423=CARTESIAN_POINT('Ctrl Pts',(55.7621378056333,26.6696115898312,12.6284999318363));
#59424=CARTESIAN_POINT('Ctrl Pts',(55.6840445442169,26.646909837782,12.6242733550915));
#59425=CARTESIAN_POINT('Ctrl Pts',(55.6060379572776,26.6242332820488,12.6200514693575));
#59426=CARTESIAN_POINT('Ctrl Pts',(55.5268164091989,26.6054148111937,12.6158295836235));
#59427=CARTESIAN_POINT('Ctrl Pts',(55.4467956866222,26.59057603058,12.6116076978894));
#59428=CARTESIAN_POINT('Ctrl Pts',(55.3668289355414,26.5757472582636,12.6073886596864));
#59429=CARTESIAN_POINT('Ctrl Pts',(55.2860645360832,26.5648929296592,12.6031696214834));
#59430=CARTESIAN_POINT('Ctrl Pts',(55.2049303805208,26.5580839922021,12.5989505832803));
#59431=CARTESIAN_POINT('Ctrl Pts',(55.1238227204157,26.5512772782957,12.5947329228614));
#59432=CARTESIAN_POINT('Ctrl Pts',(55.0423460065726,26.5485133707775,12.5905152624424));
#59433=CARTESIAN_POINT('Ctrl Pts',(54.9609338293452,26.549811418623,12.5862976020234));
#59434=CARTESIAN_POINT('Ctrl Pts',(54.8795233462743,26.5511094394565,12.5820800293724));
#59435=CARTESIAN_POINT('Ctrl Pts',(54.7981778616191,26.5564692390106,12.5778624567213));
#59436=CARTESIAN_POINT('Ctrl Pts',(54.7173301075911,26.5658578550287,12.5736448840703));
#59437=CARTESIAN_POINT('Ctrl Pts',(54.6363451099832,26.5752624087471,12.569420151854));
#59438=CARTESIAN_POINT('Ctrl Pts',(54.5558599973781,26.5887094085851,12.5651954196377));
#59439=CARTESIAN_POINT('Ctrl Pts',(54.4763018988166,26.6061139231749,12.5609706874214));
#59440=CARTESIAN_POINT('Ctrl Pts',(54.3967636707247,26.6235140908047,12.5567470103763));
#59441=CARTESIAN_POINT('Ctrl Pts',(54.3181524379497,26.6448696538575,12.5525233333312));
#59442=CARTESIAN_POINT('Ctrl Pts',(54.2408803941934,26.6700455639476,12.5482996562861));
#59443=CARTESIAN_POINT('Ctrl Pts',(54.1634681518555,26.6952671519662,12.5440683160098));
#59444=CARTESIAN_POINT('Ctrl Pts',(54.0874003895536,26.7243227730418,12.5398369757336));
#59445=CARTESIAN_POINT('Ctrl Pts',(54.0130703170206,26.7570287449782,12.5356056354573));
#59446=CARTESIAN_POINT('Ctrl Pts',(53.9389538704648,26.7896407193577,12.5313864561298));
#59447=CARTESIAN_POINT('Ctrl Pts',(53.8665655085587,26.8258818120867,12.5271672768023));
#59448=CARTESIAN_POINT('Ctrl Pts',(53.7962680270324,26.8655259225619,12.5229480974748));
#59449=CARTESIAN_POINT('Ctrl Pts',(53.7257467020468,26.9052962690647,12.5187154833033));
#59450=CARTESIAN_POINT('Ctrl Pts',(53.6570673193136,26.9486392807201,12.5144828691319));
#59451=CARTESIAN_POINT('Ctrl Pts',(53.5906146944258,26.9953595558226,12.5102502549604));
#59452=CARTESIAN_POINT('Ctrl Pts',(53.5242568579679,27.0420131888395,12.5060236782156));
#59453=CARTESIAN_POINT('Ctrl Pts',(53.46011984776,27.0920342524662,12.5017971014708));
#59454=CARTESIAN_POINT('Ctrl Pts',(53.3985630109559,27.1451819981138,12.497570524726));
#59455=CARTESIAN_POINT('Ctrl Pts',(53.3370744951124,27.198270755918,12.493348638992));
#59456=CARTESIAN_POINT('Ctrl Pts',(53.2781608123703,27.2544789982947,12.489126753258));
#59457=CARTESIAN_POINT('Ctrl Pts',(53.2221503229588,27.3135241549774,12.4849048675239));
#59458=CARTESIAN_POINT('Ctrl Pts',(53.1661776108856,27.372529487533,12.4806858293209));
#59459=CARTESIAN_POINT('Ctrl Pts',(53.1131045220431,27.4343675980315,12.4764667911179));
#59460=CARTESIAN_POINT('Ctrl Pts',(53.0632235138284,27.4987181834802,12.4722477529149));
#59461=CARTESIAN_POINT('Ctrl Pts',(53.0133587949325,27.563047754374,12.4680300924959));
#59462=CARTESIAN_POINT('Ctrl Pts',(52.966684370872,27.6298878039107,12.4638124320769));
#59463=CARTESIAN_POINT('Ctrl Pts',(52.9234523512287,27.698885050281,12.459594771658));
#59464=CARTESIAN_POINT('Ctrl Pts',(52.8802212312274,27.7678808608447,12.4553771990069));
#59465=CARTESIAN_POINT('Ctrl Pts',(52.840432618875,27.8390333847079,12.4511596263559));
#59466=CARTESIAN_POINT('Ctrl Pts',(52.8042944443639,27.9119616904958,12.4469420537048));
#59467=CARTESIAN_POINT('Ctrl Pts',(52.7680949232823,27.9850137961579,12.4427173214885));
#59468=CARTESIAN_POINT('Ctrl Pts',(52.7355584457849,28.0598472965956,12.4384925892723));
#59469=CARTESIAN_POINT('Ctrl Pts',(52.7068462986919,28.136057668489,12.434267857056));
#59470=CARTESIAN_POINT('Ctrl Pts',(52.6781413227587,28.2122490060427,12.4300441800109));
#59471=CARTESIAN_POINT('Ctrl Pts',(52.6532588892888,28.2898160769963,12.4258205029657));
#59472=CARTESIAN_POINT('Ctrl Pts',(52.6323101148727,28.368339602424,12.4215968259206));
#59473=CARTESIAN_POINT('Ctrl Pts',(52.6113233320345,28.44700559706,12.4173654856444));
#59474=CARTESIAN_POINT('Ctrl Pts',(52.5942845688628,28.5266310586114,12.4131341453681));
#59475=CARTESIAN_POINT('Ctrl Pts',(52.5812538117933,28.6067861560991,12.4089028050919));
#59476=CARTESIAN_POINT('Ctrl Pts',(52.568260505356,28.6867108863821,12.4046836257644));
#59477=CARTESIAN_POINT('Ctrl Pts',(52.55925216562,28.7671617506215,12.4004644464369));
#59478=CARTESIAN_POINT('Ctrl Pts',(52.5542366399835,28.8477113372554,12.3962452671094));
#59479=CARTESIAN_POINT('Ctrl Pts',(52.5510992381463,28.8980981639606,12.3936060101436));
#59480=CARTESIAN_POINT('Ctrl Pts',(52.5495187507328,28.9485829339407,12.3909667531778));
#59481=CARTESIAN_POINT('Ctrl Pts',(52.5495001658422,28.9990984498427,12.3883274962121));
#59482=CARTESIAN_POINT('',(52.5495004573641,28.9985028222904,11.5883274962406));
#59483=CARTESIAN_POINT('Ctrl Pts',(52.5495001658419,28.9990984507376,12.3883274961653));
#59484=CARTESIAN_POINT('Ctrl Pts',(52.5494706380201,29.079357983368,12.3841342195694));
#59485=CARTESIAN_POINT('Ctrl Pts',(52.5533883882208,29.1597762288156,12.3799409429735));
#59486=CARTESIAN_POINT('Ctrl Pts',(52.561273989113,29.2399285181527,12.3757476663776));
#59487=CARTESIAN_POINT('Ctrl Pts',(52.5691487625614,29.3199707531757,12.3715601474236));
#59488=CARTESIAN_POINT('Ctrl Pts',(52.5809805248543,29.3997472893288,12.3673726284697));
#59489=CARTESIAN_POINT('Ctrl Pts',(52.5967378291866,29.4788331529219,12.3631851095157));
#59490=CARTESIAN_POINT('Ctrl Pts',(52.6124785576057,29.5578358220559,12.3590019956267));
#59491=CARTESIAN_POINT('Ctrl Pts',(52.6321365331142,29.6361487992951,12.3548188817378));
#59492=CARTESIAN_POINT('Ctrl Pts',(52.6556286436803,29.7133534843733,12.3506357678489));
#59493=CARTESIAN_POINT('Ctrl Pts',(52.6791077142574,29.7905153147137,12.3464549759207));
#59494=CARTESIAN_POINT('Ctrl Pts',(52.7064165592587,29.8665696211731,12.3422741839925));
#59495=CARTESIAN_POINT('Ctrl Pts',(52.7374215575929,29.941110536523,12.3380933920643));
#59496=CARTESIAN_POINT('Ctrl Pts',(52.7684192578951,30.0156339062507,12.3339135842211));
#59497=CARTESIAN_POINT('Ctrl Pts',(52.8031112019664,30.0886441548573,12.3297337763779));
#59498=CARTESIAN_POINT('Ctrl Pts',(52.8413152866402,30.159754525021,12.3255539685347));
#59499=CARTESIAN_POINT('Ctrl Pts',(52.8795225924527,30.2308708907836,12.3213738082753));
#59500=CARTESIAN_POINT('Ctrl Pts',(52.9212424003766,30.3000866437562,12.3171936480158));
#59501=CARTESIAN_POINT('Ctrl Pts',(52.9662469752236,30.3670401911476,12.3130134877564));
#59502=CARTESIAN_POINT('Ctrl Pts',(53.0112979745108,30.4340628044276,12.3088290154553));
#59503=CARTESIAN_POINT('Ctrl Pts',(53.0596402376615,30.4988181613851,12.3046445431542));
#59504=CARTESIAN_POINT('Ctrl Pts',(53.1110034996619,30.5609748465977,12.3004600708532));
#59505=CARTESIAN_POINT('Ctrl Pts',(53.1623967487656,30.6231678203726,12.2962731555569));
#59506=CARTESIAN_POINT('Ctrl Pts',(53.2168141858928,30.6827587546492,12.2920862402606));
#59507=CARTESIAN_POINT('Ctrl Pts',(53.2739479068017,30.739452333801,12.2878993249643));
#59508=CARTESIAN_POINT('Ctrl Pts',(53.331175189797,30.7962387542637,12.2837055531825));
#59509=CARTESIAN_POINT('Ctrl Pts',(53.3911272805342,30.8501180359065,12.2795117814007));
#59510=CARTESIAN_POINT('Ctrl Pts',(53.4534628821636,30.900834867408,12.2753180096189));
#59511=CARTESIAN_POINT('Ctrl Pts',(53.4820786349711,30.9241169129084,12.2733928186606));
#59512=CARTESIAN_POINT('Ctrl Pts',(53.5111962723062,30.946733117978,12.2714676277022));
#59513=CARTESIAN_POINT('Ctrl Pts',(53.5407808827152,30.9686619358718,12.2695424367439));
#59514=CARTESIAN_POINT('Ctrl Pts',(53.6058239064903,31.016873374316,12.2653098225724));
#59515=CARTESIAN_POINT('Ctrl Pts',(53.6733797551386,31.0619475530149,12.261077208401));
#59516=CARTESIAN_POINT('Ctrl Pts',(53.7431132472199,31.1036125928236,12.2568445942295));
#59517=CARTESIAN_POINT('Ctrl Pts',(53.8127472710226,31.1452182013652,12.2526180174847));
#59518=CARTESIAN_POINT('Ctrl Pts',(53.8845523734627,31.1834240929048,12.2483914407399));
#59519=CARTESIAN_POINT('Ctrl Pts',(53.9581623293075,31.2180001167552,12.2441648639951));
#59520=CARTESIAN_POINT('Ctrl Pts',(54.0316905866251,31.2525377652229,12.2399429782611));
#59521=CARTESIAN_POINT('Ctrl Pts',(54.1070192986825,31.2834533545764,12.2357210925271));
#59522=CARTESIAN_POINT('Ctrl Pts',(54.1837566635088,31.3105620670378,12.231499206793));
#59523=CARTESIAN_POINT('Ctrl Pts',(54.2604422713623,31.3376524955132,12.22728016859));
#59524=CARTESIAN_POINT('Ctrl Pts',(54.3385342081279,31.3609409922764,12.223061130387));
#59525=CARTESIAN_POINT('Ctrl Pts',(54.4176208316246,31.3802908969793,12.218842092184));
#59526=CARTESIAN_POINT('Ctrl Pts',(54.4966816283134,31.3996344827087,12.214624431765));
#59527=CARTESIAN_POINT('Ctrl Pts',(54.576736015751,31.4150419203746,12.210406771346));
#59528=CARTESIAN_POINT('Ctrl Pts',(54.6573586636032,31.4264268306694,12.2061891109271));
#59529=CARTESIAN_POINT('Ctrl Pts',(54.7379796337285,31.4378115040484,12.201971538276));
#59530=CARTESIAN_POINT('Ctrl Pts',(54.8191683806081,31.4451737526953,12.197753965625));
#59531=CARTESIAN_POINT('Ctrl Pts',(54.9004923134657,31.4484788074069,12.193536392974));
#59532=CARTESIAN_POINT('Ctrl Pts',(54.9819542982437,31.4517894726335,12.1893116607577));
#59533=CARTESIAN_POINT('Ctrl Pts',(55.0635514615379,31.4510291450554,12.1850869285414));
#59534=CARTESIAN_POINT('Ctrl Pts',(55.1448486614833,31.4462152634767,12.1808621963251));
#59535=CARTESIAN_POINT('Ctrl Pts',(55.2261255566005,31.4414025842154,12.17663851928));
#59536=CARTESIAN_POINT('Ctrl Pts',(55.307102177115,31.432538447385,12.1724148422349));
#59537=CARTESIAN_POINT('Ctrl Pts',(55.3873503367598,31.4196921222776,12.1681911651898));
#59538=CARTESIAN_POINT('Ctrl Pts',(55.467744094704,31.406822489432,12.1639598249135));
#59539=CARTESIAN_POINT('Ctrl Pts',(55.5474062946451,31.3899563257236,12.1597284846373));
#59540=CARTESIAN_POINT('Ctrl Pts',(55.6259199360131,31.3692138957261,12.155497144361));
#59541=CARTESIAN_POINT('Ctrl Pts',(55.7042079277511,31.3485310798487,12.1512779650335));
#59542=CARTESIAN_POINT('Ctrl Pts',(55.7813535454311,31.3239944660964,12.147058785706));
#59543=CARTESIAN_POINT('Ctrl Pts',(55.8569632320824,31.295770953048,12.1428396063785));
#59544=CARTESIAN_POINT('Ctrl Pts',(55.9328136774842,31.2674575697986,12.138606992207));
#59545=CARTESIAN_POINT('Ctrl Pts',(56.0074004941536,31.2353284389188,12.1343743780356));
#59546=CARTESIAN_POINT('Ctrl Pts',(56.0803131499589,31.1995167078306,12.1301417638641));
#59547=CARTESIAN_POINT('Ctrl Pts',(56.1531218027069,31.1637560588142,12.1259151871193));
#59548=CARTESIAN_POINT('Ctrl Pts',(56.2242606240282,31.1243234455889,12.1216886103745));
#59549=CARTESIAN_POINT('Ctrl Pts',(56.2933371844084,31.0814007728995,12.1174620336297));
#59550=CARTESIAN_POINT('Ctrl Pts',(56.3623370778054,31.0385257394064,12.1132401478957));
#59551=CARTESIAN_POINT('Ctrl Pts',(56.4292788656544,30.9921685871546,12.1090182621617));
#59552=CARTESIAN_POINT('Ctrl Pts',(56.4937942208316,30.9425573545742,12.1047963764276));
#59553=CARTESIAN_POINT('Ctrl Pts',(56.5582660624024,30.8929795832316,12.1005773382246));
#59554=CARTESIAN_POINT('Ctrl Pts',(56.6203143543339,30.8401523730299,12.0963583000216));
#59555=CARTESIAN_POINT('Ctrl Pts',(56.679600364143,30.7843466218117,12.0921392618185));
#59556=CARTESIAN_POINT('Ctrl Pts',(56.7388670133027,30.7285590947172,12.0879216013996));
#59557=CARTESIAN_POINT('Ctrl Pts',(56.7953728337728,30.6697952764575,12.0837039409806));
#59558=CARTESIAN_POINT('Ctrl Pts',(56.8488138182338,30.6083649198823,12.0794862805616));
#59559=CARTESIAN_POINT('Ctrl Pts',(56.902253690608,30.5469358416496,12.0752687079106));
#59560=CARTESIAN_POINT('Ctrl Pts',(56.9526285497644,30.4828406866846,12.0710511352595));
#59561=CARTESIAN_POINT('Ctrl Pts',(56.9996737276507,30.4164233946612,12.0668335626085));
#59562=CARTESIAN_POINT('Ctrl Pts',(57.0467987673553,30.3498933555733,12.0626088303922));
#59563=CARTESIAN_POINT('Ctrl Pts',(57.0905825468881,30.2810336735705,12.0583840981759));
#59564=CARTESIAN_POINT('Ctrl Pts',(57.1308028027755,30.2102188503258,12.0541593659596));
#59565=CARTESIAN_POINT('Ctrl Pts',(57.1710130132322,30.1394217138259,12.0499356889145));
#59566=CARTESIAN_POINT('Ctrl Pts',(57.2076612891364,30.0666708384707,12.0457120118694));
#59567=CARTESIAN_POINT('Ctrl Pts',(57.2405726303686,29.9923631079616,12.0414883348243));
#59568=CARTESIAN_POINT('Ctrl Pts',(57.2735436843137,29.9179205571743,12.037256994548));
#59569=CARTESIAN_POINT('Ctrl Pts',(57.3027640865823,29.8419159410713,12.0330256542718));
#59570=CARTESIAN_POINT('Ctrl Pts',(57.3281077026861,29.7647645223816,12.0287943139956));
#59571=CARTESIAN_POINT('Ctrl Pts',(57.3533784807775,29.687834838269,12.024575134668));
#59572=CARTESIAN_POINT('Ctrl Pts',(57.3747946866316,29.609765395665,12.0203559553405));
#59573=CARTESIAN_POINT('Ctrl Pts',(57.392282066255,29.5309771798061,12.016136776013));
#59574=CARTESIAN_POINT('Ctrl Pts',(57.4098251297444,29.4519380840238,12.0119041618415));
#59575=CARTESIAN_POINT('Ctrl Pts',(57.4234795273592,29.3718816558138,12.00767154767));
#59576=CARTESIAN_POINT('Ctrl Pts',(57.4331334524926,29.2912247454487,12.0034389334986));
#59577=CARTESIAN_POINT('Ctrl Pts',(57.4427736072081,29.210682884593,11.9992123567538));
#59578=CARTESIAN_POINT('Ctrl Pts',(57.4484245681362,29.1295427001877,11.994985780009));
#59579=CARTESIAN_POINT('Ctrl Pts',(57.4500252826214,29.0482324010992,11.9907592032642));
#59580=CARTESIAN_POINT('Ctrl Pts',(57.451624220499,28.9670123470269,11.9865373175302));
#59581=CARTESIAN_POINT('Ctrl Pts',(57.4491818349971,28.8856230155492,11.9823154317961));
#59582=CARTESIAN_POINT('Ctrl Pts',(57.4426888929207,28.8044975130547,11.9780935460621));
#59583=CARTESIAN_POINT('Ctrl Pts',(57.4362003301324,28.7234267271958,11.9738745078591));
#59584=CARTESIAN_POINT('Ctrl Pts',(57.4256666736764,28.6426198787795,11.9696554696561));
#59585=CARTESIAN_POINT('Ctrl Pts',(57.4111307532604,28.5625085821617,11.965436431453));
#59586=CARTESIAN_POINT('Ctrl Pts',(57.3965995797459,28.4824234469727,11.9612187710341));
#59587=CARTESIAN_POINT('Ctrl Pts',(57.3780688207534,28.4030338692272,11.9570011106151));
#59588=CARTESIAN_POINT('Ctrl Pts',(57.3556328029574,28.324763487635,11.9527834501961));
#59589=CARTESIAN_POINT('Ctrl Pts',(57.3331972520466,28.24649473482,11.9485658775451));
#59590=CARTESIAN_POINT('Ctrl Pts',(57.3068567330474,28.1693455780917,11.944348304894));
#59591=CARTESIAN_POINT('Ctrl Pts',(57.2767556657342,28.0937252687251,11.940130732243));
#59592=CARTESIAN_POINT('Ctrl Pts',(57.2466035001772,28.0179765896579,11.9359060000267));
#59593=CARTESIAN_POINT('Ctrl Pts',(57.2126781866408,27.943762384433,11.9316812678104));
#59594=CARTESIAN_POINT('Ctrl Pts',(57.175172866162,27.8714729722719,11.9274565355941));
#59595=CARTESIAN_POINT('Ctrl Pts',(57.1376769130302,27.7992016151496,11.923232858549));
#59596=CARTESIAN_POINT('Ctrl Pts',(57.0966029944165,27.7288544815802,11.9190091815039));
#59597=CARTESIAN_POINT('Ctrl Pts',(57.052188756176,27.6607944298858,11.9147855044588));
#59598=CARTESIAN_POINT('Ctrl Pts',(57.007693934934,27.5926108933933,11.9105541641825));
#59599=CARTESIAN_POINT('Ctrl Pts',(56.9598469561017,27.5267231085291,11.9063228239063));
#59600=CARTESIAN_POINT('Ctrl Pts',(56.9089274848149,27.4634629494482,11.9020914836301));
#59601=CARTESIAN_POINT('Ctrl Pts',(56.8581543570125,27.4003846012124,11.8978723043025));
#59602=CARTESIAN_POINT('Ctrl Pts',(56.8043267388008,27.3399190799684,11.893653124975));
#59603=CARTESIAN_POINT('Ctrl Pts',(56.7477573392823,27.2823578565414,11.8894339456475));
#59604=CARTESIAN_POINT('Ctrl Pts',(56.6910078096964,27.2246133448501,11.885201331476));
#59605=CARTESIAN_POINT('Ctrl Pts',(56.6312879231681,27.1695769076014,11.8809687173046));
#59606=CARTESIAN_POINT('Ctrl Pts',(56.5688864766152,27.1175692646225,11.8767361031331));
#59607=CARTESIAN_POINT('Ctrl Pts',(56.5065740398665,27.0656358056629,11.8725095263883));
#59608=CARTESIAN_POINT('Ctrl Pts',(56.441587993916,27.0167228552666,11.8682829496435));
#59609=CARTESIAN_POINT('Ctrl Pts',(56.3742542940485,26.9711147431929,11.8640563728987));
#59610=CARTESIAN_POINT('Ctrl Pts',(56.3069953267909,26.9255572508424,11.8598344871647));
#59611=CARTESIAN_POINT('Ctrl Pts',(56.2373942656691,26.8832975677387,11.8556126014307));
#59612=CARTESIAN_POINT('Ctrl Pts',(56.165809384689,26.8445792223858,11.8513907156966));
#59613=CARTESIAN_POINT('Ctrl Pts',(56.0942727854914,26.8058869913562,11.8471716774936));
#59614=CARTESIAN_POINT('Ctrl Pts',(56.0207554314249,26.7707315746989,11.8429526392906));
#59615=CARTESIAN_POINT('Ctrl Pts',(55.9456426880273,26.7393120169779,11.8387336010876));
#59616=CARTESIAN_POINT('Ctrl Pts',(55.8705544737131,26.707902719739,11.8345159406686));
#59617=CARTESIAN_POINT('Ctrl Pts',(55.7938723329707,26.6802270377313,11.8302982802497));
#59618=CARTESIAN_POINT('Ctrl Pts',(55.7160029761548,26.6564364766157,11.8260806198307));
#59619=CARTESIAN_POINT('Ctrl Pts',(55.6381352397707,26.6326464105726,11.8218630471797));
#59620=CARTESIAN_POINT('Ctrl Pts',(55.5590807810528,26.6127414392866,11.8176454745286));
#59621=CARTESIAN_POINT('Ctrl Pts',(55.4792615125366,26.5968232165317,11.8134279018775));
#59622=CARTESIAN_POINT('Ctrl Pts',(55.3993067463523,26.5808779717043,11.8092031696613));
#59623=CARTESIAN_POINT('Ctrl Pts',(55.3185850307356,26.5689331073856,11.804978437445));
#59624=CARTESIAN_POINT('Ctrl Pts',(55.2375289214324,26.5610391021004,11.8007537052287));
#59625=CARTESIAN_POINT('Ctrl Pts',(55.1564930567426,26.5531470684259,11.7965300281836));
#59626=CARTESIAN_POINT('Ctrl Pts',(55.0751234320191,26.549303871314,11.7923063511385));
#59627=CARTESIAN_POINT('Ctrl Pts',(54.9938537965713,26.5495077077894,11.7880826740934));
#59628=CARTESIAN_POINT('Ctrl Pts',(54.9124367095087,26.5497119140958,11.7838513338171));
#59629=CARTESIAN_POINT('Ctrl Pts',(54.8311204395328,26.5539778037926,11.7796199935409));
#59630=CARTESIAN_POINT('Ctrl Pts',(54.7503356209827,26.5622514592662,11.7753886532646));
#59631=CARTESIAN_POINT('Ctrl Pts',(54.669782979467,26.5705013361038,11.7711694739371));
#59632=CARTESIAN_POINT('Ctrl Pts',(54.5897591761054,26.5827358216747,11.7669502946096));
#59633=CARTESIAN_POINT('Ctrl Pts',(54.5106789430665,26.598851284647,11.7627311152821));
#59634=CARTESIAN_POINT('Ctrl Pts',(54.4313469002539,26.615018062985,11.7584985011107));
#59635=CARTESIAN_POINT('Ctrl Pts',(54.352669393887,26.6351507295708,11.7542658869392));
#59636=CARTESIAN_POINT('Ctrl Pts',(54.2750726731228,26.6591816343965,11.7500332727677));
#59637=CARTESIAN_POINT('Ctrl Pts',(54.197586636795,26.6831782613928,11.7458066960229));
#59638=CARTESIAN_POINT('Ctrl Pts',(54.1211787642444,26.7110619465329,11.7415801192782));
#59639=CARTESIAN_POINT('Ctrl Pts',(54.0462650087663,26.7427140596512,11.7373535425334));
#59640=CARTESIAN_POINT('Ctrl Pts',(53.9714343988815,26.7743310425893,11.7331316567994));
#59641=CARTESIAN_POINT('Ctrl Pts',(53.8980950368,26.8097079629586,11.7289097710654));
#59642=CARTESIAN_POINT('Ctrl Pts',(53.8266462450325,26.8486768685984,11.7246878853313));
#59643=CARTESIAN_POINT('Ctrl Pts',(53.7552456432594,26.8876194909198,11.7204688471283));
#59644=CARTESIAN_POINT('Ctrl Pts',(53.6857334860588,26.9301490649902,11.7162498089253));
#59645=CARTESIAN_POINT('Ctrl Pts',(53.6184865303419,26.9760506964963,11.7120307707223));
#59646=CARTESIAN_POINT('Ctrl Pts',(53.5512615350292,27.0219373382029,11.7078131103033));
#59647=CARTESIAN_POINT('Ctrl Pts',(53.4863006555292,27.0711935887503,11.7035954498844));
#59648=CARTESIAN_POINT('Ctrl Pts',(53.4239523920575,27.1235607690366,11.6993777894654));
#59649=CARTESIAN_POINT('Ctrl Pts',(53.3616054260292,27.1759268595818,11.6951602168144));
#59650=CARTESIAN_POINT('Ctrl Pts',(53.3018713228988,27.2314034514767,11.6909426441633));
#59651=CARTESIAN_POINT('Ctrl Pts',(53.2450650419408,27.2896919742392,11.6867250715122));
#59652=CARTESIAN_POINT('Ctrl Pts',(53.1881623291467,27.3480794450261,11.682500339296));
#59653=CARTESIAN_POINT('Ctrl Pts',(53.1341977085533,27.4092880627194,11.6782756070797));
#59654=CARTESIAN_POINT('Ctrl Pts',(53.0834490065173,27.4729824691968,11.6740508748634));
#59655=CARTESIAN_POINT('Ctrl Pts',(53.032712979502,27.5366609673279,11.6698271978183));
#59656=CARTESIAN_POINT('Ctrl Pts',(52.9851915195056,27.6028236216844,11.6656035207732));
#59657=CARTESIAN_POINT('Ctrl Pts',(52.9411192476209,27.6711056108619,11.661379843728));
#59658=CARTESIAN_POINT('Ctrl Pts',(52.8969670131816,27.7395114875099,11.6571485034518));
#59659=CARTESIAN_POINT('Ctrl Pts',(52.8562767061392,27.8100439799548,11.6529171631756));
#59660=CARTESIAN_POINT('Ctrl Pts',(52.8192375367207,27.8823125084568,11.6486858228993));
#59661=CARTESIAN_POINT('Ctrl Pts',(52.7823048185469,27.9543733358971,11.6444666435718));
#59662=CARTESIAN_POINT('Ctrl Pts',(52.7490023906174,28.0281597847597,11.6402474642442));
#59663=CARTESIAN_POINT('Ctrl Pts',(52.7194691048837,28.1032675502581,11.6360282849167));
#59664=CARTESIAN_POINT('Ctrl Pts',(52.6860019559815,28.1883797451664,11.631247106687));
#59665=CARTESIAN_POINT('Ctrl Pts',(52.65726976131,28.2754529496787,11.6264659284574));
#59666=CARTESIAN_POINT('Ctrl Pts',(52.6334774315741,28.3639802022492,11.6216847502278));
#59667=CARTESIAN_POINT('Ctrl Pts',(52.6097729953872,28.4521804177246,11.6169212346115));
#59668=CARTESIAN_POINT('Ctrl Pts',(52.5909721282548,28.5418237490575,11.6121577189953));
#59669=CARTESIAN_POINT('Ctrl Pts',(52.5772307427071,28.6323869209124,11.6073942033791));
#59670=CARTESIAN_POINT('Ctrl Pts',(52.5635760436512,28.722378781845,11.602660738041));
#59671=CARTESIAN_POINT('Ctrl Pts',(52.554917305081,28.8132786888873,11.5979272727028));
#59672=CARTESIAN_POINT('Ctrl Pts',(52.5513594669747,28.9045547799749,11.5931938073647));
#59673=CARTESIAN_POINT('Ctrl Pts',(52.5501402370929,28.9358340384533,11.5915717036567));
#59674=CARTESIAN_POINT('Ctrl Pts',(52.5495196084685,28.9671573297734,11.5899495999486));
#59675=CARTESIAN_POINT('Ctrl Pts',(52.5495004573641,28.9985028222904,11.5883274962406));
#59676=CARTESIAN_POINT('',(52.5495008325386,29.0020199680429,10.7883274961659));
#59677=CARTESIAN_POINT('Ctrl Pts',(52.5495004573637,28.9985028228412,11.5883274962121));
#59678=CARTESIAN_POINT('Ctrl Pts',(52.5494502760639,29.0806368920414,11.5840771250261));
#59679=CARTESIAN_POINT('Ctrl Pts',(52.5535337966699,29.162786480375,11.5798267538401));
#59680=CARTESIAN_POINT('Ctrl Pts',(52.5617291806368,29.2445110660934,11.575576382654));
#59681=CARTESIAN_POINT('Ctrl Pts',(52.5699256911786,29.3262468860455,11.5713254271926));
#59682=CARTESIAN_POINT('Ctrl Pts',(52.5822351423506,29.4075571352908,11.5670744717312));
#59683=CARTESIAN_POINT('Ctrl Pts',(52.598583889012,29.4880070818006,11.5628235162698));
#59684=CARTESIAN_POINT('Ctrl Pts',(52.6157295688845,29.5723786276551,11.5583653444599));
#59685=CARTESIAN_POINT('Ctrl Pts',(52.6373182619213,29.6558033196536,11.5539071726501));
#59686=CARTESIAN_POINT('Ctrl Pts',(52.6632053716463,29.7377947647533,11.5494490008402));
#59687=CARTESIAN_POINT('Ctrl Pts',(52.6879344924561,29.816118547237,11.5451902531295));
#59688=CARTESIAN_POINT('Ctrl Pts',(52.7165854932329,29.8931341456156,11.5409315054189));
#59689=CARTESIAN_POINT('Ctrl Pts',(52.7489826375331,29.9684374444808,11.5366727577082));
#59690=CARTESIAN_POINT('Ctrl Pts',(52.781406914166,30.0438038092182,11.5324104433326));
#59691=CARTESIAN_POINT('Ctrl Pts',(52.817583379001,30.1174546134316,11.528148128957));
#59692=CARTESIAN_POINT('Ctrl Pts',(52.8572903621785,30.1890103691671,11.5238858145813));
#59693=CARTESIAN_POINT('Ctrl Pts',(52.8970653766748,30.260688723802,11.5196161974381));
#59694=CARTESIAN_POINT('Ctrl Pts',(52.9403827378663,30.3302644848842,11.515346580295));
#59695=CARTESIAN_POINT('Ctrl Pts',(52.9869778522888,30.3973875921963,11.5110769631518));
#59696=CARTESIAN_POINT('Ctrl Pts',(52.9933493637473,30.4065661434816,11.5104931269516));
#59697=CARTESIAN_POINT('Ctrl Pts',(52.9997821040668,30.4156988867582,11.5099092907514));
#59698=CARTESIAN_POINT('Ctrl Pts',(53.0062753409067,30.4247849780663,11.5093254545513));
#59699=CARTESIAN_POINT('Ctrl Pts',(53.0533491027925,30.4906560542727,11.5050928403798));
#59700=CARTESIAN_POINT('Ctrl Pts',(53.1037784033861,30.5543142031118,11.5008602262083));
#59701=CARTESIAN_POINT('Ctrl Pts',(53.1573278646467,30.6153976759896,11.4966276120368));
#59702=CARTESIAN_POINT('Ctrl Pts',(53.2108009426289,30.6763940190287,11.492401035292));
#59703=CARTESIAN_POINT('Ctrl Pts',(53.2673850380899,30.734822633813,11.4881744585472));
#59704=CARTESIAN_POINT('Ctrl Pts',(53.3268024051304,30.7903519370567,11.4839478818025));
#59705=CARTESIAN_POINT('Ctrl Pts',(53.3861538257739,30.8458196092039,11.4797259960684));
#59706=CARTESIAN_POINT('Ctrl Pts',(53.4483319319848,30.898394048177,11.4755041103344));
#59707=CARTESIAN_POINT('Ctrl Pts',(53.5130207043615,30.9477789464779,11.4712822246004));
#59708=CARTESIAN_POINT('Ctrl Pts',(53.5776658461673,30.9971305361963,11.4670631863973));
#59709=CARTESIAN_POINT('Ctrl Pts',(53.6448179226719,31.0432965766419,11.4628441481943));
#59710=CARTESIAN_POINT('Ctrl Pts',(53.7141272315008,31.0860204872513,11.4586251099913));
#59711=CARTESIAN_POINT('Ctrl Pts',(53.7834139064364,31.1287304457891,11.4544074495723));
#59712=CARTESIAN_POINT('Ctrl Pts',(53.8548560195054,31.1680002632532,11.4501897891534));
#59713=CARTESIAN_POINT('Ctrl Pts',(53.9280753867571,31.2036169979205,11.4459721287344));
#59714=CARTESIAN_POINT('Ctrl Pts',(54.0012932303415,31.239232991417,11.4417545560833));
#59715=CARTESIAN_POINT('Ctrl Pts',(54.0762878363156,31.2711958511109,11.4375369834323));
#59716=CARTESIAN_POINT('Ctrl Pts',(54.1526582470961,31.2993395146837,11.4333194107812));
#59717=CARTESIAN_POINT('Ctrl Pts',(54.2291583009165,31.327530953698,11.4290946785649));
#59718=CARTESIAN_POINT('Ctrl Pts',(54.3070383941571,31.3518900635452,11.4248699463486));
#59719=CARTESIAN_POINT('Ctrl Pts',(54.3858790931439,31.3722996778995,11.4206452141324));
#59720=CARTESIAN_POINT('Ctrl Pts',(54.4647001008393,31.3927041947387,11.4164215370872));
#59721=CARTESIAN_POINT('Ctrl Pts',(54.5444807736633,31.409161115333,11.4121978600421));
#59722=CARTESIAN_POINT('Ctrl Pts',(54.6247923642888,31.4216047324252,11.407974182997));
#59723=CARTESIAN_POINT('Ctrl Pts',(54.7052496682997,31.4340709266019,11.4037428427208));
#59724=CARTESIAN_POINT('Ctrl Pts',(54.7862393517869,31.4425092170877,11.3995115024445));
#59725=CARTESIAN_POINT('Ctrl Pts',(54.8673276357942,31.4469058612411,11.3952801621683));
#59726=CARTESIAN_POINT('Ctrl Pts',(54.9481828706022,31.4512898693594,11.3910609828408));
#59727=CARTESIAN_POINT('Ctrl Pts',(55.0291356843062,31.4516555127718,11.3868418035132));
#59728=CARTESIAN_POINT('Ctrl Pts',(55.109760271355,31.4480406313687,11.3826226241857));
#59729=CARTESIAN_POINT('Ctrl Pts',(55.1906415857582,31.4444142393462,11.3783900100142));
#59730=CARTESIAN_POINT('Ctrl Pts',(55.2714933988372,31.436768417361,11.3741573958427));
#59731=CARTESIAN_POINT('Ctrl Pts',(55.3518841267503,31.4251036702255,11.3699247816713));
#59732=CARTESIAN_POINT('Ctrl Pts',(55.4321601848385,31.4134555617565,11.3656982049265));
#59733=CARTESIAN_POINT('Ctrl Pts',(55.511976008113,31.3977999800111,11.3614716281817));
#59734=CARTESIAN_POINT('Ctrl Pts',(55.5909022510574,31.3781893910484,11.3572450514369));
#59735=CARTESIAN_POINT('Ctrl Pts',(55.6697408950114,31.3586005675686,11.3530231657028));
#59736=CARTESIAN_POINT('Ctrl Pts',(55.7476914718922,31.3350655704522,11.3488012799688));
#59737=CARTESIAN_POINT('Ctrl Pts',(55.8243333902782,31.3076881747048,11.3445793942348));
#59738=CARTESIAN_POINT('Ctrl Pts',(55.9009236160669,31.2803292441618,11.3403603560318));
#59739=CARTESIAN_POINT('Ctrl Pts',(55.9762065000338,31.2491332179575,11.3361413178288));
#59740=CARTESIAN_POINT('Ctrl Pts',(56.0497764376747,31.2142537526,11.3319222796257));
#59741=CARTESIAN_POINT('Ctrl Pts',(56.1233223500562,31.1793856776042,11.3277046192068));
#59742=CARTESIAN_POINT('Ctrl Pts',(56.195156007577,31.1408367511517,11.3234869587878));
#59743=CARTESIAN_POINT('Ctrl Pts',(56.2648929057,31.0988082778352,11.3192692983688));
#59744=CARTESIAN_POINT('Ctrl Pts',(56.3346283526245,31.0567806791155,11.3150517257178));
#59745=CARTESIAN_POINT('Ctrl Pts',(56.4022667296338,31.0112739182926,11.3108341530667));
#59746=CARTESIAN_POINT('Ctrl Pts',(56.4674504578341,30.9625339242424,11.3066165804157));
#59747=CARTESIAN_POINT('Ctrl Pts',(56.5327448390552,30.913711191329,11.3023918481994));
#59748=CARTESIAN_POINT('Ctrl Pts',(56.5955758604643,30.8616445234465,11.2981671159831));
#59749=CARTESIAN_POINT('Ctrl Pts',(56.6556168999613,30.8066219666999,11.2939423837669));
#59750=CARTESIAN_POINT('Ctrl Pts',(56.715642943579,30.7516131524138,11.2897187067217));
#59751=CARTESIAN_POINT('Ctrl Pts',(56.7728800863489,30.6936502722294,11.2854950296766));
#59752=CARTESIAN_POINT('Ctrl Pts',(56.8270398009749,30.6330571991371,11.2812713526315));
#59753=CARTESIAN_POINT('Ctrl Pts',(56.8812977803136,30.5723541889642,11.2770400123553));
#59754=CARTESIAN_POINT('Ctrl Pts',(56.9324668802389,30.5090118114391,11.272808672079));
#59755=CARTESIAN_POINT('Ctrl Pts',(56.9802994234629,30.4433864497883,11.2685773318028));
#59756=CARTESIAN_POINT('Ctrl Pts',(57.0279944950895,30.377949696618,11.2643581524753));
#59757=CARTESIAN_POINT('Ctrl Pts',(57.0723719830576,30.3102434908223,11.2601389731478));
#59758=CARTESIAN_POINT('Ctrl Pts',(57.1132318195364,30.2406456089065,11.2559197938203));
#59759=CARTESIAN_POINT('Ctrl Pts',(57.1542217631962,30.1708261112182,11.2516871796488));
#59760=CARTESIAN_POINT('Ctrl Pts',(57.1918240470589,30.0988431790726,11.2474545654774));
#59761=CARTESIAN_POINT('Ctrl Pts',(57.2258041399824,30.0250591107039,11.2432219513059));
#59762=CARTESIAN_POINT('Ctrl Pts',(57.2597357634939,29.9513802883808,11.2389953745611));
#59763=CARTESIAN_POINT('Ctrl Pts',(57.2900552651194,29.8759058509472,11.2347687978163));
#59764=CARTESIAN_POINT('Ctrl Pts',(57.3165729186675,29.7990245068183,11.2305422210715));
#59765=CARTESIAN_POINT('Ctrl Pts',(57.3430611406908,29.7222284920788,11.2263203353375));
#59766=CARTESIAN_POINT('Ctrl Pts',(57.3657557482853,29.6440291102945,11.2220984496035));
#59767=CARTESIAN_POINT('Ctrl Pts',(57.3845148202347,29.564835659357,11.2178765638694));
#59768=CARTESIAN_POINT('Ctrl Pts',(57.4032612397717,29.4856956219463,11.2136575256664));
#59769=CARTESIAN_POINT('Ctrl Pts',(57.4180772887261,29.4055632978649,11.2094384874634));
#59770=CARTESIAN_POINT('Ctrl Pts',(57.4288710466342,29.3248625691302,11.2052194492604));
#59771=CARTESIAN_POINT('Ctrl Pts',(57.4396612796946,29.2441881943112,11.2010017888414));
#59772=CARTESIAN_POINT('Ctrl Pts',(57.446431768768,29.1629462435645,11.1967841284224));
#59773=CARTESIAN_POINT('Ctrl Pts',(57.4491420486453,29.0815688393782,11.1925664680035));
#59774=CARTESIAN_POINT('Ctrl Pts',(57.4518522721227,29.0001931286248,11.1883488953524));
#59775=CARTESIAN_POINT('Ctrl Pts',(57.4505024401052,28.9186824343659,11.1841313227014));
#59776=CARTESIAN_POINT('Ctrl Pts',(57.4451041776997,28.8374705866766,11.1799137500503));
#59777=CARTESIAN_POINT('Ctrl Pts',(57.4396967514422,28.756120877338,11.175689017834));
#59778=CARTESIAN_POINT('Ctrl Pts',(57.4302271756289,28.6750714955413,11.1714642856177));
#59779=CARTESIAN_POINT('Ctrl Pts',(57.4167592572644,28.5947532326757,11.1672395534014));
#59780=CARTESIAN_POINT('Ctrl Pts',(57.4032947026538,28.5144550301386,11.1630158763563));
#59781=CARTESIAN_POINT('Ctrl Pts',(57.3858339231741,28.4348880321328,11.1587921993112));
#59782=CARTESIAN_POINT('Ctrl Pts',(57.3644915171676,28.3564705793497,11.1545685222661));
#59783=CARTESIAN_POINT('Ctrl Pts',(57.3431103885532,28.2779108498114,11.1503371819898));
#59784=CARTESIAN_POINT('Ctrl Pts',(57.3178337035763,28.2005052765348,11.1461058417136));
#59785=CARTESIAN_POINT('Ctrl Pts',(57.2888255697627,28.1246556327933,11.1418745014374));
#59786=CARTESIAN_POINT('Ctrl Pts',(57.2599008058519,28.0490239823041,11.1376553221098));
#59787=CARTESIAN_POINT('Ctrl Pts',(57.2272662726081,27.9749397128427,11.1334361427823));
#59788=CARTESIAN_POINT('Ctrl Pts',(57.1911299414055,27.9027763081868,11.1292169634548));
#59789=CARTESIAN_POINT('Ctrl Pts',(57.1548785437568,27.8303831185404,11.1249843492833));
#59790=CARTESIAN_POINT('Ctrl Pts',(57.1149681579824,27.7596538079307,11.1207517351119));
#59791=CARTESIAN_POINT('Ctrl Pts',(57.0715750100384,27.6909823424474,11.1165191209404));
#59792=CARTESIAN_POINT('Ctrl Pts',(57.0282437583455,27.6224088303617,11.1122925441956));
#59793=CARTESIAN_POINT('Ctrl Pts',(56.9814398573322,27.5558877229245,11.1080659674508));
#59794=CARTESIAN_POINT('Ctrl Pts',(56.9313860783316,27.4917897804263,11.103839390706));
#59795=CARTESIAN_POINT('Ctrl Pts',(56.8813878532297,27.4277629792217,11.099617504972));
#59796=CARTESIAN_POINT('Ctrl Pts',(56.8281472016935,27.3661543633525,11.095395619238));
#59797=CARTESIAN_POINT('Ctrl Pts',(56.7719301910955,27.3073058020173,11.091173733504));
#59798=CARTESIAN_POINT('Ctrl Pts',(56.7157510971278,27.2484969322118,11.0869546953009));
#59799=CARTESIAN_POINT('Ctrl Pts',(56.6565999511539,27.1924447547406,11.0827356570979));
#59800=CARTESIAN_POINT('Ctrl Pts',(56.5947822745287,27.1394571365193,11.0785166188949));
#59801=CARTESIAN_POINT('Ctrl Pts',(56.5329847853029,27.0864868221223,11.0742989584759));
#59802=CARTESIAN_POINT('Ctrl Pts',(56.468522847203,27.0365793815965,11.070081298057));
#59803=CARTESIAN_POINT('Ctrl Pts',(56.4017369061809,26.9900040060114,11.065863637638));
#59804=CARTESIAN_POINT('Ctrl Pts',(56.334952354949,26.9434295996422,11.061646064987));
#59805=CARTESIAN_POINT('Ctrl Pts',(56.2658442786624,26.9001873851175,11.0574284923359));
#59806=CARTESIAN_POINT('Ctrl Pts',(56.1947829136503,26.8605037884471,11.0532109196849));
#59807=CARTESIAN_POINT('Ctrl Pts',(56.1236009180002,26.8207528266538,11.0489861874686));
#59808=CARTESIAN_POINT('Ctrl Pts',(56.0504594071755,26.7845727969416,11.0447614552523));
#59809=CARTESIAN_POINT('Ctrl Pts',(55.9757544764458,26.7521446995645,11.040536723036));
#59810=CARTESIAN_POINT('Ctrl Pts',(55.9010682040559,26.7197247014448,11.0363130459909));
#59811=CARTESIAN_POINT('Ctrl Pts',(55.8248197364326,26.6910549058961,11.0320893689458));
#59812=CARTESIAN_POINT('Ctrl Pts',(55.7474223757313,26.6662669299476,11.0278656919007));
#59813=CARTESIAN_POINT('Ctrl Pts',(55.6698845890796,26.6414339799192,11.0236343516245));
#59814=CARTESIAN_POINT('Ctrl Pts',(55.5911941937921,26.6204970444419,11.0194030113482));
#59815=CARTESIAN_POINT('Ctrl Pts',(55.5117775476953,26.6035371916771,11.015171671072));
#59816=CARTESIAN_POINT('Ctrl Pts',(55.4325891464803,26.5866260818368,11.0109524917445));
#59817=CARTESIAN_POINT('Ctrl Pts',(55.3526791260918,26.5736692155802,11.0067333124169));
#59818=CARTESIAN_POINT('Ctrl Pts',(55.2724739939285,26.5646954661413,11.0025141330894));
#59819=CARTESIAN_POINT('Ctrl Pts',(55.1920134700522,26.5556931422063,10.9982815189179));
#59820=CARTESIAN_POINT('Ctrl Pts',(55.1109566938016,26.5506658869071,10.9940489047465));
#59821=CARTESIAN_POINT('Ctrl Pts',(55.029730071424,26.5496803529227,10.989816290575));
#59822=CARTESIAN_POINT('Ctrl Pts',(54.9486193111962,26.54869622471,10.9855897138302));
#59823=CARTESIAN_POINT('Ctrl Pts',(54.8673396466744,26.5517423730987,10.9813631370854));
#59824=CARTESIAN_POINT('Ctrl Pts',(54.7863233578371,26.5588337740756,10.9771365603406));
#59825=CARTESIAN_POINT('Ctrl Pts',(54.7053969876991,26.5659173044185,10.9729146746066));
#59826=CARTESIAN_POINT('Ctrl Pts',(54.6247338728599,26.5770371258987,10.9686927888725));
#59827=CARTESIAN_POINT('Ctrl Pts',(54.5447656291199,26.5921561683595,10.9644709031385));
#59828=CARTESIAN_POINT('Ctrl Pts',(54.4648513214803,26.6072650134949,10.9602518649355));
#59829=CARTESIAN_POINT('Ctrl Pts',(54.3856314094065,26.6263676363598,10.9560328267325));
#59830=CARTESIAN_POINT('Ctrl Pts',(54.3075304655059,26.6493753609312,10.9518137885294));
#59831=CARTESIAN_POINT('Ctrl Pts',(54.2294550265261,26.6723755720185,10.9475961281105));
#59832=CARTESIAN_POINT('Ctrl Pts',(54.1524982753025,26.6992782210437,10.9433784676915));
#59833=CARTESIAN_POINT('Ctrl Pts',(54.0770713551459,26.7299442811887,10.9391608072725));
#59834=CARTESIAN_POINT('Ctrl Pts',(54.0016460045951,26.7606097031846,10.9349432346215));
#59835=CARTESIAN_POINT('Ctrl Pts',(53.9277508517128,26.7950382045397,10.9307256619704));
#59836=CARTESIAN_POINT('Ctrl Pts',(53.8557773853043,26.8330424881832,10.9265080893194));
#59837=CARTESIAN_POINT('Ctrl Pts',(53.7836817399151,26.8711112862218,10.9222833571031));
#59838=CARTESIAN_POINT('Ctrl Pts',(53.7135147207998,26.9127677933263,10.9180586248868));
#59839=CARTESIAN_POINT('Ctrl Pts',(53.6456437901219,26.9577782914765,10.9138338926705));
#59840=CARTESIAN_POINT('Ctrl Pts',(53.5777898109206,27.0027775477829,10.9096102156254));
#59841=CARTESIAN_POINT('Ctrl Pts',(53.512231135899,27.0511288261646,10.9053865385803));
#59842=CARTESIAN_POINT('Ctrl Pts',(53.4493031707684,27.1025570907637,10.9011628615351));
#59843=CARTESIAN_POINT('Ctrl Pts',(53.3862610322444,27.1540786642673,10.8969315212589));
#59844=CARTESIAN_POINT('Ctrl Pts',(53.3258594879415,27.2086880684349,10.8927001809826));
#59845=CARTESIAN_POINT('Ctrl Pts',(53.2683986494233,27.2660717971378,10.8884688407064));
#59846=CARTESIAN_POINT('Ctrl Pts',(53.2111029543979,27.3232906039629,10.8842496613789));
#59847=CARTESIAN_POINT('Ctrl Pts',(53.1567313285859,27.3832674165504,10.8800304820514));
#59848=CARTESIAN_POINT('Ctrl Pts',(53.1055401825562,27.4456601883466,10.8758113027239));
#59849=CARTESIAN_POINT('Ctrl Pts',(53.0544250736637,27.50796028459,10.8715983903848));
#59850=CARTESIAN_POINT('Ctrl Pts',(53.0062851429247,27.5729079792855,10.8673854780457));
#59851=CARTESIAN_POINT('Ctrl Pts',(52.9614081126638,27.6401862749307,10.8631725657066));
#59852=CARTESIAN_POINT('Ctrl Pts',(52.9165921463314,27.7073730253686,10.8589653858542));
#59853=CARTESIAN_POINT('Ctrl Pts',(52.8750305270319,27.7768836970744,10.8547582060018));
#59854=CARTESIAN_POINT('Ctrl Pts',(52.8369711761229,27.8483678725058,10.8505510261493));
#59855=CARTESIAN_POINT('Ctrl Pts',(52.7989517092293,27.919777136624,10.8463482551799));
#59856=CARTESIAN_POINT('Ctrl Pts',(52.76442744343,27.9931553871588,10.8421454842105));
#59857=CARTESIAN_POINT('Ctrl Pts',(52.7336025250028,28.0681240772901,10.8379427132411));
#59858=CARTESIAN_POINT('Ctrl Pts',(52.7027967376404,28.1430462391272,10.8337425506642));
#59859=CARTESIAN_POINT('Ctrl Pts',(52.6756859210305,28.2195564499582,10.8295423880872));
#59860=CARTESIAN_POINT('Ctrl Pts',(52.6524272465736,28.2972536607209,10.8253422255102));
#59861=CARTESIAN_POINT('Ctrl Pts',(52.6291779684574,28.3749194823579,10.8211437597693));
#59862=CARTESIAN_POINT('Ctrl Pts',(52.6097778731808,28.4537709017236,10.8169452940285));
#59863=CARTESIAN_POINT('Ctrl Pts',(52.594334617116,28.5333906177609,10.8127468282876));
#59864=CARTESIAN_POINT('Ctrl Pts',(52.5788858380369,28.613038808417,10.8085468610378));
#59865=CARTESIAN_POINT('Ctrl Pts',(52.567396821711,28.6934553850803,10.804346893788));
#59866=CARTESIAN_POINT('Ctrl Pts',(52.5599241172339,28.77421263024,10.8001469265382));
#59867=CARTESIAN_POINT('Ctrl Pts',(52.5529142919454,28.8499675568645,10.7962071164295));
#59868=CARTESIAN_POINT('Ctrl Pts',(52.5494381866502,28.9260218523768,10.7922673063208));
#59869=CARTESIAN_POINT('Ctrl Pts',(52.5495008325378,29.0020199671524,10.7883274962121));
#59870=CARTESIAN_POINT('',(52.5495000009021,28.9999335093135,9.98832749618066));
#59871=CARTESIAN_POINT('Ctrl Pts',(52.5495008325386,29.0020199680429,10.7883274961659));
#59872=CARTESIAN_POINT('Ctrl Pts',(52.5495806928346,29.0989014953011,10.7833050713127));
#59873=CARTESIAN_POINT('Ctrl Pts',(52.5554097972367,29.195537660279,10.7782826464595));
#59874=CARTESIAN_POINT('Ctrl Pts',(52.5668780804804,29.2913210853217,10.7732602216063));
#59875=CARTESIAN_POINT('Ctrl Pts',(52.578489456825,29.3882996279791,10.7681751304994));
#59876=CARTESIAN_POINT('Ctrl Pts',(52.5958815310451,29.4844039715165,10.7630900393925));
#59877=CARTESIAN_POINT('Ctrl Pts',(52.6188909492805,29.5790249896004,10.7580049482857));
#59878=CARTESIAN_POINT('Ctrl Pts',(52.6323094394725,29.6342054896082,10.75503945631));
#59879=CARTESIAN_POINT('Ctrl Pts',(52.6476374345984,29.6888819236266,10.7520739643342));
#59880=CARTESIAN_POINT('Ctrl Pts',(52.6648351019657,29.7429368405111,10.7491084723585));
#59881=CARTESIAN_POINT('Ctrl Pts',(52.6893811439755,29.8200888305072,10.744875858187));
#59882=CARTESIAN_POINT('Ctrl Pts',(52.717800499929,29.8961665176382,10.7406432440155));
#59883=CARTESIAN_POINT('Ctrl Pts',(52.7499803883688,29.970753314326,10.736410629844));
#59884=CARTESIAN_POINT('Ctrl Pts',(52.7821143752193,30.0452337199517,10.7321840530992));
#59885=CARTESIAN_POINT('Ctrl Pts',(52.8179980583693,30.1182270358674,10.7279574763544));
#59886=CARTESIAN_POINT('Ctrl Pts',(52.8574690671919,30.189332355551,10.7237308996096));
#59887=CARTESIAN_POINT('Ctrl Pts',(52.8968962677652,30.2603587565634,10.7195090138756));
#59888=CARTESIAN_POINT('Ctrl Pts',(52.9399026584179,30.3295009208941,10.7152871281416));
#59889=CARTESIAN_POINT('Ctrl Pts',(52.9862786045282,30.3963797447038,10.7110652424076));
#59890=CARTESIAN_POINT('Ctrl Pts',(53.032623271501,30.4632134608209,10.7068462042045));
#59891=CARTESIAN_POINT('Ctrl Pts',(53.0823327161962,30.5277864875226,10.7026271660015));
#59892=CARTESIAN_POINT('Ctrl Pts',(53.1351530399975,30.5897471703921,10.6984081277985));
#59893=CARTESIAN_POINT('Ctrl Pts',(53.1879561146069,30.6516876191615,10.6941904673795));
#59894=CARTESIAN_POINT('Ctrl Pts',(53.2438677496658,30.7110170650421,10.6899728069605));
#59895=CARTESIAN_POINT('Ctrl Pts',(53.3025935296144,30.7674166244248,10.6857551465415));
#59896=CARTESIAN_POINT('Ctrl Pts',(53.3613180875018,30.823815010154,10.6815375738905));
#59897=CARTESIAN_POINT('Ctrl Pts',(53.4228563379765,30.8772833096742,10.6773200012394));
#59898=CARTESIAN_POINT('Ctrl Pts',(53.4868777839744,30.9275402484436,10.6731024285884));
#59899=CARTESIAN_POINT('Ctrl Pts',(53.551007909954,30.9778825011745,10.6688776963721));
#59900=CARTESIAN_POINT('Ctrl Pts',(53.6176292980807,31.0250021976902,10.6646529641558));
#59901=CARTESIAN_POINT('Ctrl Pts',(53.6863788393578,31.0686589125114,10.6604282319395));
#59902=CARTESIAN_POINT('Ctrl Pts',(53.7551112097162,31.1123047236105,10.6562045548944));
#59903=CARTESIAN_POINT('Ctrl Pts',(53.8259702543295,31.152489071163,10.6519808778493));
#59904=CARTESIAN_POINT('Ctrl Pts',(53.8985681831979,31.1890176342222,10.6477572008042));
#59905=CARTESIAN_POINT('Ctrl Pts',(53.9712978301646,31.2256124729031,10.6435258605279));
#59906=CARTESIAN_POINT('Ctrl Pts',(54.0457722403259,31.2585380831304,10.6392945202517));
#59907=CARTESIAN_POINT('Ctrl Pts',(54.1215828619718,31.2876480458363,10.6350631799754));
#59908=CARTESIAN_POINT('Ctrl Pts',(54.1971756025148,31.3166743459808,10.630844000648));
#59909=CARTESIAN_POINT('Ctrl Pts',(54.2740964257098,31.3419068389321,10.6266248213205));
#59910=CARTESIAN_POINT('Ctrl Pts',(54.351928510941,31.3632506416097,10.622405641993));
#59911=CARTESIAN_POINT('Ctrl Pts',(54.4300084315551,31.3846624078977,10.6181730278216));
#59912=CARTESIAN_POINT('Ctrl Pts',(54.5092958350579,31.40224028939,10.6139404136501));
#59913=CARTESIAN_POINT('Ctrl Pts',(54.5893798789632,31.415852099405,10.6097077994786));
#59914=CARTESIAN_POINT('Ctrl Pts',(54.6693496904995,31.4294444934512,10.6054812227338));
#59915=CARTESIAN_POINT('Ctrl Pts',(54.7501134313602,31.439081974809,10.601254645989));
#59916=CARTESIAN_POINT('Ctrl Pts',(54.8312464163408,31.4446824902228,10.5970280692442));
#59917=CARTESIAN_POINT('Ctrl Pts',(54.912289353103,31.4502767897131,10.5928061835102));
#59918=CARTESIAN_POINT('Ctrl Pts',(54.9937002585672,31.4518429943024,10.5885842977762));
#59919=CARTESIAN_POINT('Ctrl Pts',(55.075047005612,31.4493505663642,10.5843624120422));
#59920=CARTESIAN_POINT('Ctrl Pts',(55.1563388867985,31.4468598194914,10.5801433738391));
#59921=CARTESIAN_POINT('Ctrl Pts',(55.237566232377,31.44031589104,10.5759243356361));
#59922=CARTESIAN_POINT('Ctrl Pts',(55.3182958431399,31.4297403166264,10.5717052974331));
#59923=CARTESIAN_POINT('Ctrl Pts',(55.3989990905552,31.4191681958099,10.5674876370141));
#59924=CARTESIAN_POINT('Ctrl Pts',(55.4792044656936,31.4045671039895,10.5632699765952));
#59925=CARTESIAN_POINT('Ctrl Pts',(55.558484200871,31.3860104038703,10.5590523161762));
#59926=CARTESIAN_POINT('Ctrl Pts',(55.6377622862671,31.3674540899091,10.5548347435252));
#59927=CARTESIAN_POINT('Ctrl Pts',(55.7161143179457,31.3449424383288,10.5506171708741));
#59928=CARTESIAN_POINT('Ctrl Pts',(55.7931244328572,31.3185995523171,10.5463995982231));
#59929=CARTESIAN_POINT('Ctrl Pts',(55.8702652767418,31.2922119477844,10.5421748660068));
#59930=CARTESIAN_POINT('Ctrl Pts',(55.9460592042979,31.2619802475128,10.5379501337905));
#59931=CARTESIAN_POINT('Ctrl Pts',(56.0201068637376,31.2280781486643,10.5337254015742));
#59932=CARTESIAN_POINT('Ctrl Pts',(56.0941360289977,31.1941845172206,10.5295017245291));
#59933=CARTESIAN_POINT('Ctrl Pts',(56.1664193944902,31.1566225542158,10.525278047484));
#59934=CARTESIAN_POINT('Ctrl Pts',(56.2365828457144,31.1156117592047,10.5210543704389));
#59935=CARTESIAN_POINT('Ctrl Pts',(56.3068735980408,31.0745265562315,10.5168230301626));
#59936=CARTESIAN_POINT('Ctrl Pts',(56.3750363594652,31.0299802709464,10.5125916898864));
#59937=CARTESIAN_POINT('Ctrl Pts',(56.4407258940992,30.9822358961718,10.5083603496102));
#59938=CARTESIAN_POINT('Ctrl Pts',(56.5062266358189,30.9346287395965,10.5041411702826));
#59939=CARTESIAN_POINT('Ctrl Pts',(56.5692680456235,30.8838422020938,10.4999219909551));
#59940=CARTESIAN_POINT('Ctrl Pts',(56.6295436157121,30.8301742688859,10.4957028116276));
#59941=CARTESIAN_POINT('Ctrl Pts',(56.6900111171732,30.7763354445514,10.4914701974561));
#59942=CARTESIAN_POINT('Ctrl Pts',(56.747920014007,30.7193965831343,10.4872375832847));
#59943=CARTESIAN_POINT('Ctrl Pts',(56.8029357617094,30.6596303471404,10.4830049691132));
#59944=CARTESIAN_POINT('Ctrl Pts',(56.8578730346133,30.5999493620705,10.4787783923684));
#59945=CARTESIAN_POINT('Ctrl Pts',(56.9099250427466,30.5374493513981,10.4745518156236));
#59946=CARTESIAN_POINT('Ctrl Pts',(56.9587917588003,30.4724418819282,10.4703252388788));
#59947=CARTESIAN_POINT('Ctrl Pts',(57.0076042384578,30.4075065632217,10.4661033531448));
#59948=CARTESIAN_POINT('Ctrl Pts',(57.0532381729521,30.3400696849732,10.4618814674108));
#59949=CARTESIAN_POINT('Ctrl Pts',(57.0954326961982,30.2704771016053,10.4576595816767));
#59950=CARTESIAN_POINT('Ctrl Pts',(57.137598760547,30.2009314562767,10.4534405434737));
#59951=CARTESIAN_POINT('Ctrl Pts',(57.1763297806992,30.129233389725,10.4492215052707));
#59952=CARTESIAN_POINT('Ctrl Pts',(57.2114079872756,30.0557580043807,10.4450024670676));
#59953=CARTESIAN_POINT('Ctrl Pts',(57.2464747385885,29.9823066134184,10.4407848066487));
#59954=CARTESIAN_POINT('Ctrl Pts',(57.277890845314,29.9070794752191,10.4365671462297));
#59955=CARTESIAN_POINT('Ctrl Pts',(57.3054849688676,29.8304753508235,10.4323494858107));
#59956=CARTESIAN_POINT('Ctrl Pts',(57.333078518198,29.7538728205307,10.4281319131597));
#59957=CARTESIAN_POINT('Ctrl Pts',(57.3568500861601,29.6758937984692,10.4239143405086));
#59958=CARTESIAN_POINT('Ctrl Pts',(57.3766773774591,29.5969546829317,10.4196967678576));
#59959=CARTESIAN_POINT('Ctrl Pts',(57.396538326693,29.5178815638347,10.4154720356413));
#59960=CARTESIAN_POINT('Ctrl Pts',(57.4124414891092,29.4378455433135,10.411247303425));
#59961=CARTESIAN_POINT('Ctrl Pts',(57.424315158834,29.3572761685977,10.4070225712087));
#59962=CARTESIAN_POINT('Ctrl Pts',(57.4361858629852,29.2767269169283,10.4027988941636));
#59963=CARTESIAN_POINT('Ctrl Pts',(57.4440290632794,29.1956450434864,10.3985752171185));
#59964=CARTESIAN_POINT('Ctrl Pts',(57.4478252132447,29.1144638606878,10.3943515400734));
#59965=CARTESIAN_POINT('Ctrl Pts',(57.4516282507571,29.0331353867587,10.3901201997971));
#59966=CARTESIAN_POINT('Ctrl Pts',(57.4513695651493,28.9517077092808,10.3858888595209));
#59967=CARTESIAN_POINT('Ctrl Pts',(57.4470818147394,28.870613594331,10.3816575192447));
#59968=CARTESIAN_POINT('Ctrl Pts',(57.4428063874019,28.789752545339,10.3774383399172));
#59969=CARTESIAN_POINT('Ctrl Pts',(57.4345251528575,28.7092235884595,10.3732191605896));
#59970=CARTESIAN_POINT('Ctrl Pts',(57.4223212055342,28.6294460535637,10.3689999812621));
#59971=CARTESIAN_POINT('Ctrl Pts',(57.4100783980166,28.5494144885236,10.3647673670906));
#59972=CARTESIAN_POINT('Ctrl Pts',(57.3938422947662,28.4698414829047,10.3605347529192));
#59973=CARTESIAN_POINT('Ctrl Pts',(57.3736594856737,28.3911560987647,10.3563021387477));
#59974=CARTESIAN_POINT('Ctrl Pts',(57.3535054654632,28.3125829519369,10.3520755620029));
#59975=CARTESIAN_POINT('Ctrl Pts',(57.3294160349933,28.2348953581758,10.3478489852581));
#59976=CARTESIAN_POINT('Ctrl Pts',(57.301489209251,28.1585146051766,10.3436224085133));
#59977=CARTESIAN_POINT('Ctrl Pts',(57.2735933790515,28.0822186259686,10.3394005227793));
#59978=CARTESIAN_POINT('Ctrl Pts',(57.2418687750507,28.0072270395985,10.3351786370453));
#59979=CARTESIAN_POINT('Ctrl Pts',(57.2064634929563,27.9339469505456,10.3309567513112));
#59980=CARTESIAN_POINT('Ctrl Pts',(57.1710820906267,27.8607162866402,10.3267377131082));
#59981=CARTESIAN_POINT('Ctrl Pts',(57.1320251422449,27.7891952446147,10.3225186749052));
#59982=CARTESIAN_POINT('Ctrl Pts',(57.089488739367,27.7197707009841,10.3182996367022));
#59983=CARTESIAN_POINT('Ctrl Pts',(57.0469662273274,27.6503688288784,10.3140819762832));
#59984=CARTESIAN_POINT('Ctrl Pts',(57.000966759851,27.5830624913214,10.3098643158642));
#59985=CARTESIAN_POINT('Ctrl Pts',(56.9517315508951,27.5182124972721,10.3056466554453));
#59986=CARTESIAN_POINT('Ctrl Pts',(56.9024973665053,27.4533638527268,10.3014290827942));
#59987=CARTESIAN_POINT('Ctrl Pts',(56.8500278563562,27.3909718193431,10.2972115101432));
#59988=CARTESIAN_POINT('Ctrl Pts',(56.7946057281832,27.3313656690658,10.2929939374921));
#59989=CARTESIAN_POINT('Ctrl Pts',(56.7390895178508,27.2716583340179,10.2887692052759));
#59990=CARTESIAN_POINT('Ctrl Pts',(56.6806109791777,27.2147466860857,10.2845444730596));
#59991=CARTESIAN_POINT('Ctrl Pts',(56.6194913904811,27.1609247198231,10.2803197408433));
#59992=CARTESIAN_POINT('Ctrl Pts',(56.5583870670427,27.1071161961611,10.2760960637982));
#59993=CARTESIAN_POINT('Ctrl Pts',(56.4946433906778,27.0563960846154,10.2718723867531));
#59994=CARTESIAN_POINT('Ctrl Pts',(56.4286131936573,27.0090166768884,10.267648709708));
#59995=CARTESIAN_POINT('Ctrl Pts',(56.3624631947068,26.9615513063029,10.2634173694317));
#59996=CARTESIAN_POINT('Ctrl Pts',(56.2940187759755,26.9174390050455,10.2591860291555));
#59997=CARTESIAN_POINT('Ctrl Pts',(56.2236607317809,26.8768879766962,10.2549546888792));
#59998=CARTESIAN_POINT('Ctrl Pts',(56.1535048978822,26.8364534927382,10.2507355095517));
#59999=CARTESIAN_POINT('Ctrl Pts',(56.0814468665521,26.7995599721353,10.2465163302242));
#60000=CARTESIAN_POINT('Ctrl Pts',(56.0078836189387,26.7663659967051,10.2422971508967));
#60001=CARTESIAN_POINT('Ctrl Pts',(55.9340861289105,26.7330663239707,10.2380645367252));
#60002=CARTESIAN_POINT('Ctrl Pts',(55.8584993366765,26.7033659685561,10.2338319225538));
#60003=CARTESIAN_POINT('Ctrl Pts',(55.7815085138889,26.6774594314159,10.2295993083823));
#60004=CARTESIAN_POINT('Ctrl Pts',(55.7046275112808,26.6515898475183,10.2253727316375));
#60005=CARTESIAN_POINT('Ctrl Pts',(55.626346892407,26.62950348083,10.2211461548927));
#60006=CARTESIAN_POINT('Ctrl Pts',(55.5470734034523,26.6113474632682,10.2169195781479));
#60007=CARTESIAN_POINT('Ctrl Pts',(55.4678878988907,26.5932115967835,10.2126976924139));
#60008=CARTESIAN_POINT('Ctrl Pts',(55.3877121644035,26.5789975148659,10.2084758066798));
#60009=CARTESIAN_POINT('Ctrl Pts',(55.3069683129208,26.5688026191067,10.2042539209458));
#60010=CARTESIAN_POINT('Ctrl Pts',(55.2262789206621,26.5586145994885,10.2000348827428));
#60011=CARTESIAN_POINT('Ctrl Pts',(55.1450226321312,26.5524404401531,10.1958158445398));
#60012=CARTESIAN_POINT('Ctrl Pts',(55.0636307215102,26.5503262704433,10.1915968063367));
#60013=CARTESIAN_POINT('Ctrl Pts',(54.9822653905197,26.5482127911443,10.1873791459178));
#60014=CARTESIAN_POINT('Ctrl Pts',(54.9007649894306,26.550156680478,10.1831614854988));
#60015=CARTESIAN_POINT('Ctrl Pts',(54.8195634909725,26.5561520267803,10.1789438250798));
#60016=CARTESIAN_POINT('Ctrl Pts',(54.7383636822869,26.5621472483217,10.1747262524288));
#60017=CARTESIAN_POINT('Ctrl Pts',(54.6574632270658,26.572193723826,10.1705086797777));
#60018=CARTESIAN_POINT('Ctrl Pts',(54.5772922332422,26.5862335668249,10.1662911071267));
#60019=CARTESIAN_POINT('Ctrl Pts',(54.4969851446769,26.6002972432419,10.1620663749104));
#60020=CARTESIAN_POINT('Ctrl Pts',(54.4174104550551,26.6183677697227,10.1578416426941));
#60021=CARTESIAN_POINT('Ctrl Pts',(54.3389896786002,26.6403357007822,10.1536169104778));
#60022=CARTESIAN_POINT('Ctrl Pts',(54.2605884885567,26.6622981451206,10.1493932334327));
#60023=CARTESIAN_POINT('Ctrl Pts',(54.1833410706479,26.6881558793239,10.1451695563876));
#60024=CARTESIAN_POINT('Ctrl Pts',(54.107651135691,26.7177502865886,10.1409458793425));
#60025=CARTESIAN_POINT('Ctrl Pts',(54.0318238726525,26.7473983884849,10.1367145390662));
#60026=CARTESIAN_POINT('Ctrl Pts',(53.9575601647771,26.7807965212213,10.13248319879));
#60027=CARTESIAN_POINT('Ctrl Pts',(53.8852419632136,26.8177386111146,10.1282518585138));
#60028=CARTESIAN_POINT('Ctrl Pts',(53.8131316054736,26.8545745287712,10.1240326791862));
#60029=CARTESIAN_POINT('Ctrl Pts',(53.7429559393099,26.8949337609263,10.1198134998587));
#60030=CARTESIAN_POINT('Ctrl Pts',(53.6750641040087,26.9385696418473,10.1155943205312));
#60031=CARTESIAN_POINT('Ctrl Pts',(53.6069560853829,26.9823444695174,10.1113617063597));
#60032=CARTESIAN_POINT('Ctrl Pts',(53.5408931673629,27.0295796802682,10.1071290921883));
#60033=CARTESIAN_POINT('Ctrl Pts',(53.4772482444542,27.0800579849948,10.1028964780168));
#60034=CARTESIAN_POINT('Ctrl Pts',(53.413694105052,27.1304642871594,10.098669901272));
#60035=CARTESIAN_POINT('Ctrl Pts',(53.3525514714623,27.1841042092555,10.0944433245272));
#60036=CARTESIAN_POINT('Ctrl Pts',(53.2941651945998,27.2407166610562,10.0902167477824));
#60037=CARTESIAN_POINT('Ctrl Pts',(53.2358437197436,27.297266279591,10.0859948620484));
#60038=CARTESIAN_POINT('Ctrl Pts',(53.180272854749,27.3567815506487,10.0817729763144));
#60039=CARTESIAN_POINT('Ctrl Pts',(53.1277641011473,27.4189614207594,10.0775510905803));
#60040=CARTESIAN_POINT('Ctrl Pts',(53.0752907630715,27.481099352476,10.0733320523773));
#60041=CARTESIAN_POINT('Ctrl Pts',(53.0258757334726,27.5458979598612,10.0691130141743));
#60042=CARTESIAN_POINT('Ctrl Pts',(52.9797924928195,27.6130205921026,10.0648939759713));
#60043=CARTESIAN_POINT('Ctrl Pts',(52.9337243012726,27.6801213045395,10.0606763155523));
#60044=CARTESIAN_POINT('Ctrl Pts',(52.8909860006212,27.7495441519376,10.0564586551333));
#60045=CARTESIAN_POINT('Ctrl Pts',(52.8518088871162,27.8209218887084,10.0522409947144));
#60046=CARTESIAN_POINT('Ctrl Pts',(52.812632588872,27.8922981401356,10.0480234220633));
#60047=CARTESIAN_POINT('Ctrl Pts',(52.777017552922,27.9656287922486,10.0438058494123));
#60048=CARTESIAN_POINT('Ctrl Pts',(52.7451493737418,28.0405215462227,10.0395882767612));
#60049=CARTESIAN_POINT('Ctrl Pts',(52.7132270965467,28.1155414348316,10.035363544545));
#60050=CARTESIAN_POINT('Ctrl Pts',(52.685064584843,28.1921283011353,10.0311388123287));
#60051=CARTESIAN_POINT('Ctrl Pts',(52.6607995056797,28.2698689861594,10.0269140801124));
#60052=CARTESIAN_POINT('Ctrl Pts',(52.6365404869745,28.3475902546322,10.0226904030673));
#60053=CARTESIAN_POINT('Ctrl Pts',(52.6161770501565,28.4264643088748,10.0184667260222));
#60054=CARTESIAN_POINT('Ctrl Pts',(52.5997959239436,28.5060661549535,10.014243048977));
#60055=CARTESIAN_POINT('Ctrl Pts',(52.5833850766241,28.5858124266921,10.0100117087008));
#60056=CARTESIAN_POINT('Ctrl Pts',(52.5709710504681,28.6662886687285,10.0057803684246));
#60057=CARTESIAN_POINT('Ctrl Pts',(52.562588920185,28.7470623041239,10.0015490281483));
#60058=CARTESIAN_POINT('Ctrl Pts',(52.5542308802965,28.8276037946254,9.99732984882081));
#60059=CARTESIAN_POINT('Ctrl Pts',(52.5498815331473,28.9084405122791,9.99311066949331));
#60060=CARTESIAN_POINT('Ctrl Pts',(52.5495240410073,28.9891453052202,9.9888914901658));
#60061=CARTESIAN_POINT('Ctrl Pts',(52.5495081118901,28.9927413454074,9.98870349218122));
#60062=CARTESIAN_POINT('Ctrl Pts',(52.5495000984775,28.9963374206841,9.98851549419664));
#60063=CARTESIAN_POINT('Ctrl Pts',(52.5495000009021,28.999933508713,9.98832749621206));
#60064=CARTESIAN_POINT('',(52.5495007901279,28.9980321543788,9.18832749626153));
#60065=CARTESIAN_POINT('Ctrl Pts',(52.5495000009021,28.9999335093135,9.98832749618066));
#60066=CARTESIAN_POINT('Ctrl Pts',(52.5494978058378,29.0808321322443,9.98409823984876));
#60067=CARTESIAN_POINT('Ctrl Pts',(52.5535059878827,29.1618824777843,9.97986898351686));
#60068=CARTESIAN_POINT('Ctrl Pts',(52.5615436641983,29.2426539684173,9.97563972718495));
#60069=CARTESIAN_POINT('Ctrl Pts',(52.569569873288,29.3233102236385,9.97141650466635));
#60070=CARTESIAN_POINT('Ctrl Pts',(52.5816141135454,29.4036879548487,9.96719328214775));
#60071=CARTESIAN_POINT('Ctrl Pts',(52.5976434925847,29.4833564536443,9.96297005962915));
#60072=CARTESIAN_POINT('Ctrl Pts',(52.613654441598,29.5629333523532,9.95875169282585));
#60073=CARTESIAN_POINT('Ctrl Pts',(52.633641331911,29.6418021853624,9.95453332602254));
#60074=CARTESIAN_POINT('Ctrl Pts',(52.6575196292917,29.7195387153213,9.95031495921924));
#60075=CARTESIAN_POINT('Ctrl Pts',(52.6813828891315,29.7972262901045,9.94609924896478));
#60076=CARTESIAN_POINT('Ctrl Pts',(52.7091325551766,29.8737825336235,9.94188353871032));
#60077=CARTESIAN_POINT('Ctrl Pts',(52.7406335763444,29.9487958756537,9.93766782845585));
#60078=CARTESIAN_POINT('Ctrl Pts',(52.7721244336861,30.0237850145779,9.93345347840319));
#60079=CARTESIAN_POINT('Ctrl Pts',(52.8073640624274,30.0972318118537,9.92923912835052));
#60080=CARTESIAN_POINT('Ctrl Pts',(52.8461688640155,30.1687436364163,9.92502477829785));
#60081=CARTESIAN_POINT('Ctrl Pts',(52.8849730622045,30.2402543489988,9.92081049377664));
#60082=CARTESIAN_POINT('Ctrl Pts',(52.9273420999318,30.3098297402525,9.91659620925541));
#60083=CARTESIAN_POINT('Ctrl Pts',(52.9730465961936,30.3771020836516,9.9123819247342));
#60084=CARTESIAN_POINT('Ctrl Pts',(53.0187960794113,30.4444406432481,9.90816349209086));
#60085=CARTESIAN_POINT('Ctrl Pts',(53.067887317589,30.5094712406044,9.90394505944751));
#60086=CARTESIAN_POINT('Ctrl Pts',(53.1200480822684,30.5718559212018,9.89972662680417));
#60087=CARTESIAN_POINT('Ctrl Pts',(53.1722334319942,30.6342700057062,9.89550620587781));
#60088=CARTESIAN_POINT('Ctrl Pts',(53.227490874146,30.6940353467502,9.89128578495145));
#60089=CARTESIAN_POINT('Ctrl Pts',(53.2855101318628,30.7508497200088,9.88706536402509));
#60090=CARTESIAN_POINT('Ctrl Pts',(53.3436339422809,30.8077664747253,9.88283733775483));
#60091=CARTESIAN_POINT('Ctrl Pts',(53.4045291642281,30.8617213258825,9.87860931148456));
#60092=CARTESIAN_POINT('Ctrl Pts',(53.467851266408,30.9124514394233,9.87438128521429));
#60093=CARTESIAN_POINT('Ctrl Pts',(53.5287199099901,30.961215979666,9.87031707674297));
#60094=CARTESIAN_POINT('Ctrl Pts',(53.5918304998814,31.0070008999972,9.86625286827166));
#60095=CARTESIAN_POINT('Ctrl Pts',(53.6568537203743,31.0496117489729,9.86218865980035));
#60096=CARTESIAN_POINT('Ctrl Pts',(53.7245712615576,31.0939882332272,9.85795604562887));
#60097=CARTESIAN_POINT('Ctrl Pts',(53.7946163414348,31.1350876378089,9.85372343145738));
#60098=CARTESIAN_POINT('Ctrl Pts',(53.8666386434207,31.1726578850369,9.8494908172859));
#60099=CARTESIAN_POINT('Ctrl Pts',(53.9385582123553,31.2101745418348,9.84526424054112));
#60100=CARTESIAN_POINT('Ctrl Pts',(54.0124489934216,31.2441718264052,9.84103766379634));
#60101=CARTESIAN_POINT('Ctrl Pts',(54.0879320867521,31.274441111927,9.83681108705155));
#60102=CARTESIAN_POINT('Ctrl Pts',(54.1633314025899,31.304676802047,9.83258920131752));
#60103=CARTESIAN_POINT('Ctrl Pts',(54.2403190901064,31.3311925425831,9.8283673155835));
#60104=CARTESIAN_POINT('Ctrl Pts',(54.3184933321552,31.3538264404333,9.82414542984947));
#60105=CARTESIAN_POINT('Ctrl Pts',(54.3966148481019,31.3764450724214,9.81992639164645));
#60106=CARTESIAN_POINT('Ctrl Pts',(54.4759208840565,31.3951869328009,9.81570735344342));
#60107=CARTESIAN_POINT('Ctrl Pts',(54.5559925955995,31.4099393508629,9.8114883152404));
#60108=CARTESIAN_POINT('Ctrl Pts',(54.6360381586408,31.4246869513231,9.80727065482143));
#60109=CARTESIAN_POINT('Ctrl Pts',(54.716848444194,31.4354476126523,9.80305299440246));
#60110=CARTESIAN_POINT('Ctrl Pts',(54.7979938449502,31.442159651481,9.7988353339835));
#60111=CARTESIAN_POINT('Ctrl Pts',(54.8791375571012,31.4488715506348,9.79461776133245));
#60112=CARTESIAN_POINT('Ctrl Pts',(54.9606159075262,31.4515349576749,9.7904001886814));
#60113=CARTESIAN_POINT('Ctrl Pts',(55.0419950197388,31.4501401323837,9.78618261603036));
#60114=CARTESIAN_POINT('Ctrl Pts',(55.1235122775416,31.4487429392986,9.78195788381407));
#60115=CARTESIAN_POINT('Ctrl Pts',(55.2049294931523,31.4432737384524,9.77773315159778));
#60116=CARTESIAN_POINT('Ctrl Pts',(55.2858132569215,31.4337750578408,9.77350841938149));
#60117=CARTESIAN_POINT('Ctrl Pts',(55.3666768191224,31.4242787496243,9.76928474233638));
#60118=CARTESIAN_POINT('Ctrl Pts',(55.447006739762,31.4107550725452,9.76506106529126));
#60119=CARTESIAN_POINT('Ctrl Pts',(55.5263795450707,31.393297897156,9.76083738824615));
#60120=CARTESIAN_POINT('Ctrl Pts',(55.6058963604791,31.3758090483295,9.75660604796991));
#60121=CARTESIAN_POINT('Ctrl Pts',(55.6844521406715,31.3543725613023,9.75237470769367));
#60122=CARTESIAN_POINT('Ctrl Pts',(55.761637522592,31.3291325711904,9.74814336741743));
#60123=CARTESIAN_POINT('Ctrl Pts',(55.8386010723243,31.303965121268,9.74392418808991));
#60124=CARTESIAN_POINT('Ctrl Pts',(55.9142016949616,31.2750162422132,9.7397050087624));
#60125=CARTESIAN_POINT('Ctrl Pts',(55.9880561238729,31.2424752721217,9.73548582943489));
#60126=CARTESIAN_POINT('Ctrl Pts',(56.0621457223876,31.2098306840463,9.7312532152634));
#60127=CARTESIAN_POINT('Ctrl Pts',(56.1347535377424,31.1734496529806,9.72702060109192));
#60128=CARTESIAN_POINT('Ctrl Pts',(56.2054774081875,31.1334888020212,9.72278798692043));
#60129=CARTESIAN_POINT('Ctrl Pts',(56.2761003976719,31.0935849514636,9.71856141017565));
#60130=CARTESIAN_POINT('Ctrl Pts',(56.3448443784209,31.0501116493631,9.71433483343087));
#60131=CARTESIAN_POINT('Ctrl Pts',(56.4113280756007,31.0032731498778,9.71010825668609));
#60132=CARTESIAN_POINT('Ctrl Pts',(56.4777379835754,30.956486635703,9.70588637095206));
#60133=CARTESIAN_POINT('Ctrl Pts',(56.5418922148169,30.9063426117408,9.70166448521803));
#60134=CARTESIAN_POINT('Ctrl Pts',(56.6034362197288,30.8530899976153,9.69744259948401));
#60135=CARTESIAN_POINT('Ctrl Pts',(56.6649387151179,30.7998733007266,9.69322356128098));
#60136=CARTESIAN_POINT('Ctrl Pts',(56.7238341303281,30.7435524809836,9.68900452307796));
#60137=CARTESIAN_POINT('Ctrl Pts',(56.7797999350869,30.6844175376268,9.68478548487493));
#60138=CARTESIAN_POINT('Ctrl Pts',(56.8357474634543,30.6253019055865,9.68056782445596));
#60139=CARTESIAN_POINT('Ctrl Pts',(56.8887669622505,30.5633743121338,9.67635016403699));
#60140=CARTESIAN_POINT('Ctrl Pts',(56.9385728113438,30.4989615422414,9.67213250361803));
#60141=CARTESIAN_POINT('Ctrl Pts',(56.9883776239961,30.4345501127544,9.66791493096698));
#60142=CARTESIAN_POINT('Ctrl Pts',(57.0349686366767,30.3676539778703,9.66369735831594));
#60143=CARTESIAN_POINT('Ctrl Pts',(57.0781014763362,30.2986317815491,9.6594797856649));
#60144=CARTESIAN_POINT('Ctrl Pts',(57.1213075364012,30.2294924161929,9.65525505344861));
#60145=CARTESIAN_POINT('Ctrl Pts',(57.1610434305799,30.1582201644429,9.65103032123232));
#60146=CARTESIAN_POINT('Ctrl Pts',(57.1971088838655,30.0852017335222,9.64680558901603));
#60147=CARTESIAN_POINT('Ctrl Pts',(57.2331653294258,30.0122015397203,9.64258191197092));
#60148=CARTESIAN_POINT('Ctrl Pts',(57.2655530014879,29.9374564750665,9.63835823492581));
#60149=CARTESIAN_POINT('Ctrl Pts',(57.2941201015777,29.8613728632464,9.6341345578807));
#60150=CARTESIAN_POINT('Ctrl Pts',(57.3227390324036,29.7851512090768,9.62990321760446));
#60151=CARTESIAN_POINT('Ctrl Pts',(57.3475233963717,29.7075865980716,9.62567187732821));
#60152=CARTESIAN_POINT('Ctrl Pts',(57.3683712400756,29.6291008815624,9.62144053705197));
#60153=CARTESIAN_POINT('Ctrl Pts',(57.3891591666985,29.5508407344265,9.61722135772446));
#60154=CARTESIAN_POINT('Ctrl Pts',(57.4060331565599,29.4716652318527,9.61300217839695));
#60155=CARTESIAN_POINT('Ctrl Pts',(57.4189433805684,29.3919989433716,9.60878299906944));
#60156=CARTESIAN_POINT('Ctrl Pts',(57.4318947137196,29.3120789789805,9.60455038489796));
#60157=CARTESIAN_POINT('Ctrl Pts',(57.4409051402828,29.231367849109,9.60031777072648));
#60158=CARTESIAN_POINT('Ctrl Pts',(57.4458871024818,29.1502881629185,9.596085156555));
#60159=CARTESIAN_POINT('Ctrl Pts',(57.4508619583795,29.0693241292871,9.59185857981021));
#60160=CARTESIAN_POINT('Ctrl Pts',(57.4518197344045,28.9879930432876,9.58763200306542));
#60161=CARTESIAN_POINT('Ctrl Pts',(57.4487241977703,28.9067259239975,9.58340542632063));
#60162=CARTESIAN_POINT('Ctrl Pts',(57.4456320968234,28.8255490017993,9.5791835405866));
#60163=CARTESIAN_POINT('Ctrl Pts',(57.4384956397333,28.7444363671145,9.57496165485257));
#60164=CARTESIAN_POINT('Ctrl Pts',(57.4273306094741,28.663820937133,9.57073976911855));
#60165=CARTESIAN_POINT('Ctrl Pts',(57.4161731096816,28.583259879759,9.56652073091552));
#60166=CARTESIAN_POINT('Ctrl Pts',(57.4009924967785,28.5031958200244,9.5623016927125));
#60167=CARTESIAN_POINT('Ctrl Pts',(57.3818564437034,28.4240571802786,9.55808265450948));
#60168=CARTESIAN_POINT('Ctrl Pts',(57.3627266397655,28.3449443843274,9.55386499409051));
#60169=CARTESIAN_POINT('Ctrl Pts',(57.3396440699972,28.2667568593869,9.54964733367155));
#60170=CARTESIAN_POINT('Ctrl Pts',(57.3127273580472,28.1899120928318,9.54542967325259));
#60171=CARTESIAN_POINT('Ctrl Pts',(57.2858112062238,28.1130689253872,9.54121210060154));
#60172=CARTESIAN_POINT('Ctrl Pts',(57.2550612255348,28.0375688988133,9.5369945279505));
#60173=CARTESIAN_POINT('Ctrl Pts',(57.2206452186966,27.9638122454497,9.53277695529945));
#60174=CARTESIAN_POINT('Ctrl Pts',(57.1861707887636,27.8899303860456,9.52855222308317));
#60175=CARTESIAN_POINT('Ctrl Pts',(57.14801807881,27.8177982442578,9.52432749086688));
#60176=CARTESIAN_POINT('Ctrl Pts',(57.1064024387348,27.7477943395385,9.52010275865059));
#60177=CARTESIAN_POINT('Ctrl Pts',(57.0647971926022,27.6778079190285,9.51587908160548));
#60178=CARTESIAN_POINT('Ctrl Pts',(57.01973102153,27.6099490491839,9.51165540456037));
#60179=CARTESIAN_POINT('Ctrl Pts',(56.9714621208644,27.5445662653363,9.50743172751526));
#60180=CARTESIAN_POINT('Ctrl Pts',(56.9231056434881,27.4790648541933,9.50320038723902));
#60181=CARTESIAN_POINT('Ctrl Pts',(56.8715351187498,27.4160488676827,9.49896904696278));
#60182=CARTESIAN_POINT('Ctrl Pts',(56.8170489026719,27.3558334830989,9.49473770668654));
#60183=CARTESIAN_POINT('Ctrl Pts',(56.7627192809676,27.2957911586229,9.49051852735902));
#60184=CARTESIAN_POINT('Ctrl Pts',(56.7054910857013,27.2385336228024,9.48629934803151));
#60185=CARTESIAN_POINT('Ctrl Pts',(56.6456933295085,27.1843338095312,9.48208016870399));
#60186=CARTESIAN_POINT('Ctrl Pts',(56.5857051634132,27.1299614115042,9.47784755453251));
#60187=CARTESIAN_POINT('Ctrl Pts',(56.5229079150301,27.0784640342167,9.47361494036103));
#60188=CARTESIAN_POINT('Ctrl Pts',(56.4576084130609,27.0301451921083,9.46938232618954));
#60189=CARTESIAN_POINT('Ctrl Pts',(56.3924020546999,26.9818952722912,9.46515574944476));
#60190=CARTESIAN_POINT('Ctrl Pts',(56.3247009020312,26.9368151568067,9.46092917269997));
#60191=CARTESIAN_POINT('Ctrl Pts',(56.2548467795724,26.8951698857635,9.45670259595518));
#60192=CARTESIAN_POINT('Ctrl Pts',(56.1850701871006,26.8535708361487,9.45248071022115));
#60193=CARTESIAN_POINT('Ctrl Pts',(56.1131457698716,26.8153992926695,9.44825882448713));
#60194=CARTESIAN_POINT('Ctrl Pts',(56.0394452620096,26.7808776966364,9.4440369387531));
#60195=CARTESIAN_POINT('Ctrl Pts',(55.9657944628546,26.7463793843492,9.43981790055008));
#60196=CARTESIAN_POINT('Ctrl Pts',(55.8903703718364,26.7155263267475,9.43559886234706));
#60197=CARTESIAN_POINT('Ctrl Pts',(55.813569201632,26.6884949915356,9.43137982414403));
#60198=CARTESIAN_POINT('Ctrl Pts',(55.7367931118897,26.6614724837724,9.42716216372507));
#60199=CARTESIAN_POINT('Ctrl Pts',(55.6586412739084,26.63826937399,9.4229445033061));
#60200=CARTESIAN_POINT('Ctrl Pts',(55.57952846544,26.6190134381428,9.41872684288714));
#60201=CARTESIAN_POINT('Ctrl Pts',(55.5004173032792,26.5997579030042,9.41450927023609));
#60202=CARTESIAN_POINT('Ctrl Pts',(55.4203456620391,26.5844494872086,9.41029169758504));
#60203=CARTESIAN_POINT('Ctrl Pts',(55.3397406186372,26.5731653204126,9.40607412493399));
#60204=CARTESIAN_POINT('Ctrl Pts',(55.2589987436701,26.561861998113,9.40184939271771));
#60205=CARTESIAN_POINT('Ctrl Pts',(55.1777221173716,26.5545966575692,9.39762466050142));
#60206=CARTESIAN_POINT('Ctrl Pts',(55.0963454880657,26.5513947241482,9.39339992828513));
#60207=CARTESIAN_POINT('Ctrl Pts',(55.0149891834263,26.5481935904436,9.38917625124002));
#60208=CARTESIAN_POINT('Ctrl Pts',(54.9335333916301,26.5490538081861,9.3849525741949));
#60209=CARTESIAN_POINT('Ctrl Pts',(54.8524110346605,26.5539485395213,9.38072889714979));
#60210=CARTESIAN_POINT('Ctrl Pts',(54.771141493291,26.5588521516154,9.37649755687354));
#60211=CARTESIAN_POINT('Ctrl Pts',(54.6902070588287,26.5678048548927,9.3722662165973));
#60212=CARTESIAN_POINT('Ctrl Pts',(54.6100345351985,26.5807279635679,9.36803487632105));
#60213=CARTESIAN_POINT('Ctrl Pts',(54.530092428856,26.5936139309943,9.36381569699355));
#60214=CARTESIAN_POINT('Ctrl Pts',(54.4509082877067,26.6104473362374,9.35959651766604));
#60215=CARTESIAN_POINT('Ctrl Pts',(54.3728901703299,26.6311007806301,9.35537733833854));
#60216=CARTESIAN_POINT('Ctrl Pts',(54.2946236252016,26.6518199903724,9.35114472416706));
#60217=CARTESIAN_POINT('Ctrl Pts',(54.2172394533364,26.6764606928121,9.34691210999558));
#60218=CARTESIAN_POINT('Ctrl Pts',(54.1411592880959,26.7049307457996,9.3426794958241));
#60219=CARTESIAN_POINT('Ctrl Pts',(54.0651876440677,26.7333601889296,9.33845291907931));
#60220=CARTESIAN_POINT('Ctrl Pts',(53.9905167438469,26.7656079724965,9.33422634233453));
#60221=CARTESIAN_POINT('Ctrl Pts',(53.9175549993061,26.8015316535204,9.32999976558974));
#60222=CARTESIAN_POINT('Ctrl Pts',(53.8446742338529,26.8374154634183,9.32577787985571));
#60223=CARTESIAN_POINT('Ctrl Pts',(53.7734992694838,26.8769668600102,9.32155599412169));
#60224=CARTESIAN_POINT('Ctrl Pts',(53.7044190679385,26.9199951205637,9.31733410838766));
#60225=CARTESIAN_POINT('Ctrl Pts',(53.6353854588469,26.9629943598899,9.31311507018463));
#60226=CARTESIAN_POINT('Ctrl Pts',(53.5684441998257,27.0094655607562,9.30889603198161));
#60227=CARTESIAN_POINT('Ctrl Pts',(53.503959014938,27.0591724391346,9.30467699377858));
#60228=CARTESIAN_POINT('Ctrl Pts',(53.4394948885609,27.1088630850585,9.30045933335962));
#60229=CARTESIAN_POINT('Ctrl Pts',(53.3774856111131,27.1617870266523,9.29624167294066));
#60230=CARTESIAN_POINT('Ctrl Pts',(53.318264169631,27.217665899206,9.2920240125217));
#60231=CARTESIAN_POINT('Ctrl Pts',(53.2590439605247,27.2735436089417,9.28780643987066));
#60232=CARTESIAN_POINT('Ctrl Pts',(53.2026118091136,27.3323758077121,9.28358886721961));
#60233=CARTESIAN_POINT('Ctrl Pts',(53.1492649147178,27.3938462420722,9.27937129456856));
#60234=CARTESIAN_POINT('Ctrl Pts',(53.095827460988,27.4554210259295,9.27514656235227));
#60235=CARTESIAN_POINT('Ctrl Pts',(53.0454860491666,27.5196426532177,9.27092183013599));
#60236=CARTESIAN_POINT('Ctrl Pts',(52.9984986840313,27.586160287665,9.2666970979197));
#60237=CARTESIAN_POINT('Ctrl Pts',(52.9515230544833,27.6526613086354,9.26247342087459));
#60238=CARTESIAN_POINT('Ctrl Pts',(52.907900028098,27.7214567849452,9.25824974382948));
#60239=CARTESIAN_POINT('Ctrl Pts',(52.867842775683,27.7921689601633,9.25402606678437));
#60240=CARTESIAN_POINT('Ctrl Pts',(52.8277128453667,27.8630094320616,9.24979472650813));
#60241=CARTESIAN_POINT('Ctrl Pts',(52.7911618273533,27.935773136337,9.24556338623189));
#60242=CARTESIAN_POINT('Ctrl Pts',(52.7583560704221,28.0100592224852,9.24133204595565));
#60243=CARTESIAN_POINT('Ctrl Pts',(52.7256445978314,28.0841318090742,9.23711286662813));
#60244=CARTESIAN_POINT('Ctrl Pts',(52.6966569725273,28.1597175836678,9.23289368730061));
#60245=CARTESIAN_POINT('Ctrl Pts',(52.6715084767136,28.2364049004982,9.22867450797309));
#60246=CARTESIAN_POINT('Ctrl Pts',(52.6414535836778,28.328053686239,9.22363217922602));
#60247=CARTESIAN_POINT('Ctrl Pts',(52.6167895085714,28.4215518952709,9.21858985047894));
#60248=CARTESIAN_POINT('Ctrl Pts',(52.5977094991824,28.5163155990923,9.21354752173187));
#60249=CARTESIAN_POINT('Ctrl Pts',(52.5788396119689,28.6100356998838,9.20856072257414));
#60250=CARTESIAN_POINT('Ctrl Pts',(52.5654315328359,28.7049935042304,9.20357392341642));
#60251=CARTESIAN_POINT('Ctrl Pts',(52.5576258895964,28.8006035235255,9.1985871242587));
#60252=CARTESIAN_POINT('Ctrl Pts',(52.5522728903824,28.8661715161226,9.19516724825964));
#60253=CARTESIAN_POINT('Ctrl Pts',(52.5495537797068,28.9320458190386,9.19174737226059));
#60254=CARTESIAN_POINT('Ctrl Pts',(52.5495007901279,28.9980321543788,9.18832749626153));
#60255=CARTESIAN_POINT('',(52.5495005111529,29.0015827696721,8.38832749618323));
#60256=CARTESIAN_POINT('Ctrl Pts',(52.5495007901272,28.9980321553333,9.18832749621206));
#60257=CARTESIAN_POINT('Ctrl Pts',(52.5494356333114,29.0791700257587,9.18412236109965));
#60258=CARTESIAN_POINT('Ctrl Pts',(52.5534045814512,29.1603656797671,9.17991722598724));
#60259=CARTESIAN_POINT('Ctrl Pts',(52.5613981666387,29.241187371823,9.17571209087484));
#60260=CARTESIAN_POINT('Ctrl Pts',(52.5693897025857,29.3219883443796,9.17150803379349));
#60261=CARTESIAN_POINT('Ctrl Pts',(52.5814037806911,29.402415080424,9.16730397671214));
#60262=CARTESIAN_POINT('Ctrl Pts',(52.5973789763346,29.4820399015032,9.16309991963079));
#60263=CARTESIAN_POINT('Ctrl Pts',(52.613355033272,29.5616690155106,9.15889563589004));
#60264=CARTESIAN_POINT('Ctrl Pts',(52.6332925383797,29.6404956706803,9.15469135214927));
#60265=CARTESIAN_POINT('Ctrl Pts',(52.6570790391625,29.7181027929679,9.15048706840852));
#60266=CARTESIAN_POINT('Ctrl Pts',(52.6808909100591,29.7957926891591,9.14627830047911));
#60267=CARTESIAN_POINT('Ctrl Pts',(52.7085598373744,29.8722600070486,9.1420695325497));
#60268=CARTESIAN_POINT('Ctrl Pts',(52.7399237536216,29.947103801363,9.13786076462029));
#60269=CARTESIAN_POINT('Ctrl Pts',(52.771304532971,30.0219878361418,9.13364973380753));
#60270=CARTESIAN_POINT('Ctrl Pts',(52.806384054545,30.095246187559,9.12943870299477));
#60271=CARTESIAN_POINT('Ctrl Pts',(52.8449535347726,30.1665011713286,9.12522767218202));
#60272=CARTESIAN_POINT('Ctrl Pts',(52.883593346088,30.237886087897,9.12100896259382));
#60273=CARTESIAN_POINT('Ctrl Pts',(52.9257355850283,30.3072599395976,9.11679025300563));
#60274=CARTESIAN_POINT('Ctrl Pts',(52.9711273947103,30.3742729719765,9.11257154341743));
#60275=CARTESIAN_POINT('Ctrl Pts',(53.0091443191936,30.4303982820091,9.10903825481416));
#60276=CARTESIAN_POINT('Ctrl Pts',(53.0494398132988,30.4848680186467,9.1055049662109));
#60277=CARTESIAN_POINT('Ctrl Pts',(53.0918445043536,30.5374956437123,9.10197167760763));
#60278=CARTESIAN_POINT('Ctrl Pts',(53.1426421369415,30.6005395828511,9.09773906343615));
#60279=CARTESIAN_POINT('Ctrl Pts',(53.1966619733455,30.6611805883413,9.09350644926467));
#60280=CARTESIAN_POINT('Ctrl Pts',(53.2536481463105,30.7190711018208,9.08927383509319));
#60281=CARTESIAN_POINT('Ctrl Pts',(53.3105530338507,30.7768790399185,9.0850472583484));
#60282=CARTESIAN_POINT('Ctrl Pts',(53.3704155310609,30.8319439499115,9.08082068160361));
#60283=CARTESIAN_POINT('Ctrl Pts',(53.4329392147453,30.8839508341029,9.07659410485882));
#60284=CARTESIAN_POINT('Ctrl Pts',(53.4953935043809,30.9358999966751,9.07237221912479));
#60285=CARTESIAN_POINT('Ctrl Pts',(53.5605027563299,30.9847975818501,9.06815033339076));
#60286=CARTESIAN_POINT('Ctrl Pts',(53.6279343739839,31.0303660182108,9.06392844765674));
#60287=CARTESIAN_POINT('Ctrl Pts',(53.6953205111029,31.0759037200742,9.05970940945372));
#60288=CARTESIAN_POINT('Ctrl Pts',(53.7650255190825,31.1181164732636,9.05549037125071));
#60289=CARTESIAN_POINT('Ctrl Pts',(53.8366854677165,31.1567683113812,9.05127133304769));
#60290=CARTESIAN_POINT('Ctrl Pts',(53.908322014824,31.1954075272177,9.04705367262872));
#60291=CARTESIAN_POINT('Ctrl Pts',(53.9819118261865,31.2304879169971,9.04283601220975));
#60292=CARTESIAN_POINT('Ctrl Pts',(54.057065056535,31.2618187244765,9.03861835179079));
#60293=CARTESIAN_POINT('Ctrl Pts',(54.132216722973,31.2931488799736,9.03440077913975));
#60294=CARTESIAN_POINT('Ctrl Pts',(54.2089313144798,31.3207294306384,9.03018320648871));
#60295=CARTESIAN_POINT('Ctrl Pts',(54.2867989562092,31.3444177360564,9.02596563383767));
#60296=CARTESIAN_POINT('Ctrl Pts',(54.3647987826116,31.3681462536965,9.02174090162138));
#60297=CARTESIAN_POINT('Ctrl Pts',(54.4439551286935,31.3879691705021,9.01751616940509));
#60298=CARTESIAN_POINT('Ctrl Pts',(54.5238424968138,31.4037937270405,9.0132914371888));
#60299=CARTESIAN_POINT('Ctrl Pts',(54.603709912226,31.41961433123,9.00906776014369));
#60300=CARTESIAN_POINT('Ctrl Pts',(54.6843075202604,31.4314385255299,9.00484408309858));
#60301=CARTESIAN_POINT('Ctrl Pts',(54.7652034955927,31.4392254613951,9.00062040605347));
#60302=CARTESIAN_POINT('Ctrl Pts',(54.8462462445892,31.4470265254923,8.99638906577723));
#60303=CARTESIAN_POINT('Ctrl Pts',(54.9275879773352,31.450775670937,8.99215772550099));
#60304=CARTESIAN_POINT('Ctrl Pts',(55.0087948448896,31.4504842175993,8.98792638522476));
#60305=CARTESIAN_POINT('Ctrl Pts',(55.0897683224335,31.4501936019038,8.98370720589723));
#60306=CARTESIAN_POINT('Ctrl Pts',(55.1706072587814,31.4458856892045,8.97948802656971));
#60307=CARTESIAN_POINT('Ctrl Pts',(55.2508887426691,31.4376228356335,8.97526884724219));
#60308=CARTESIAN_POINT('Ctrl Pts',(55.3314258613909,31.4293336712234,8.97103623307072));
#60309=CARTESIAN_POINT('Ctrl Pts',(55.4117015091039,31.4170334819488,8.96680361889926));
#60310=CARTESIAN_POINT('Ctrl Pts',(55.4912848507461,31.4007476846656,8.96257100472779));
#60311=CARTESIAN_POINT('Ctrl Pts',(55.5707546742239,31.3844851175431,8.95834442798302));
#60312=CARTESIAN_POINT('Ctrl Pts',(55.6495337016168,31.3642483261047,8.95411785123825));
#60313=CARTESIAN_POINT('Ctrl Pts',(55.7271963318837,31.3401144726049,8.94989127449347));
#60314=CARTESIAN_POINT('Ctrl Pts',(55.8047727656244,31.3160074048878,8.94566938875944));
#60315=CARTESIAN_POINT('Ctrl Pts',(55.8812348228851,31.2880120066089,8.94144750302541));
#60316=CARTESIAN_POINT('Ctrl Pts',(55.9561686038967,31.2562561580907,8.93722561729138));
#60317=CARTESIAN_POINT('Ctrl Pts',(56.0310518443965,31.2245217279077,8.93300657908837));
#60318=CARTESIAN_POINT('Ctrl Pts',(56.1044084292349,31.1890320656087,8.92878754088536));
#60319=CARTESIAN_POINT('Ctrl Pts',(56.1758422999468,31.1499639847346,8.92456850268235));
#60320=CARTESIAN_POINT('Ctrl Pts',(56.247252842961,31.1109086620713,8.92035084226339));
#60321=CARTESIAN_POINT('Ctrl Pts',(56.3167415115339,31.0682774643003,8.91613318184443));
#60322=CARTESIAN_POINT('Ctrl Pts',(56.3839360624377,31.0222935556156,8.91191552142547));
#60323=CARTESIAN_POINT('Ctrl Pts',(56.4511292150484,30.9763106038386,8.90769794877443));
#60324=CARTESIAN_POINT('Ctrl Pts',(56.5160279622005,30.9269753431916,8.90348037612339));
#60325=CARTESIAN_POINT('Ctrl Pts',(56.5782895173192,30.8745539334787,8.89926280347235));
#60326=CARTESIAN_POINT('Ctrl Pts',(56.6406567649069,30.8220435354934,8.89503807125605));
#60327=CARTESIAN_POINT('Ctrl Pts',(56.7003775062325,30.7664368073819,8.89081333903975));
#60328=CARTESIAN_POINT('Ctrl Pts',(56.7571422910847,30.7080401689894,8.88658860682345));
#60329=CARTESIAN_POINT('Ctrl Pts',(56.8138928983363,30.6496581157702,8.88236492977835));
#60330=CARTESIAN_POINT('Ctrl Pts',(56.8676887336057,30.5884879097927,8.87814125273325));
#60331=CARTESIAN_POINT('Ctrl Pts',(56.918260446048,30.5248695390517,8.87391757568816));
#60332=CARTESIAN_POINT('Ctrl Pts',(56.9689239133089,30.4611357422793,8.86968623541193));
#60333=CARTESIAN_POINT('Ctrl Pts',(57.016351295979,30.3949452826139,8.8654548951357));
#60334=CARTESIAN_POINT('Ctrl Pts',(57.0603159017376,30.3266682460385,8.86122355485947));
#60335=CARTESIAN_POINT('Ctrl Pts',(57.1041541524224,30.2585874389039,8.85700437553189));
#60336=CARTESIAN_POINT('Ctrl Pts',(57.1445493486987,30.1884324685906,8.85278519620431));
#60337=CARTESIAN_POINT('Ctrl Pts',(57.1813235632301,30.1165920304647,8.84856601687674));
#60338=CARTESIAN_POINT('Ctrl Pts',(57.2182148753756,30.0445228357491,8.84433340270522));
#60339=CARTESIAN_POINT('Ctrl Pts',(57.2515992936489,29.9704893643416,8.84010078853371));
#60340=CARTESIAN_POINT('Ctrl Pts',(57.2812635913947,29.8948668485181,8.83586817436219));
#60341=CARTESIAN_POINT('Ctrl Pts',(57.3108855758052,29.8193522011129,8.83164159761737));
#60342=CARTESIAN_POINT('Ctrl Pts',(57.3367978106545,29.7422534399687,8.82741502087254));
#60343=CARTESIAN_POINT('Ctrl Pts',(57.3588333240383,29.6639695771694,8.82318844412772));
#60344=CARTESIAN_POINT('Ctrl Pts',(57.3808443805536,29.5857726003937,8.8189665583937));
#60345=CARTESIAN_POINT('Ctrl Pts',(57.3989871398471,29.5063935804293,8.81474467265968));
#60346=CARTESIAN_POINT('Ctrl Pts',(57.4131435437912,29.426249324995,8.81052278692566));
#60347=CARTESIAN_POINT('Ctrl Pts',(57.4272903996801,29.3461591243747,8.8063037487226));
#60348=CARTESIAN_POINT('Ctrl Pts',(57.4374561595622,29.265305169645,8.80208471051954));
#60349=CARTESIAN_POINT('Ctrl Pts',(57.4435735245486,29.1841159420724,8.79786567231648));
#60350=CARTESIAN_POINT('Ctrl Pts',(57.4496888918266,29.1029532279416,8.79364801189748));
#60351=CARTESIAN_POINT('Ctrl Pts',(57.4517584548587,29.0214559212844,8.78943035147848));
#60352=CARTESIAN_POINT('Ctrl Pts',(57.4497667598874,28.940057759878,8.78521269105948));
#60353=CARTESIAN_POINT('Ctrl Pts',(57.4477751063625,28.8586612923366,8.78099511840841));
#60354=CARTESIAN_POINT('Ctrl Pts',(57.4417223754058,28.7773644303241,8.77677754575734));
#60355=CARTESIAN_POINT('Ctrl Pts',(57.4316452152877,28.696599609479,8.77255997310626));
#60356=CARTESIAN_POINT('Ctrl Pts',(57.4215509486275,28.615697685839,8.76833524089001));
#60357=CARTESIAN_POINT('Ctrl Pts',(57.4074186420021,28.535330073799,8.76411050867376));
#60358=CARTESIAN_POINT('Ctrl Pts',(57.3893368631636,28.4559231632135,8.75988577645752));
#60359=CARTESIAN_POINT('Ctrl Pts',(57.3712596004387,28.3765360853354,8.75566209941237));
#60360=CARTESIAN_POINT('Ctrl Pts',(57.3492349845927,28.2981096721276,8.75143842236722));
#60361=CARTESIAN_POINT('Ctrl Pts',(57.3234015713157,28.2210549516122,8.74721474532208));
#60362=CARTESIAN_POINT('Ctrl Pts',(57.2975212871689,28.1438604268158,8.7429834050458));
#60363=CARTESIAN_POINT('Ctrl Pts',(57.2678185651516,28.0680430021525,8.73875206476953));
#60364=CARTESIAN_POINT('Ctrl Pts',(57.2344804312408,27.9939943079674,8.73452072449325));
#60365=CARTESIAN_POINT('Ctrl Pts',(57.2012381117335,27.9201584310769,8.73030154516593));
#60366=CARTESIAN_POINT('Ctrl Pts',(57.1643815302306,27.8480814989764,8.7260823658386));
#60367=CARTESIAN_POINT('Ctrl Pts',(57.1241398704255,27.7781243676753,8.72186318651128));
#60368=CARTESIAN_POINT('Ctrl Pts',(57.0837700718557,27.7079444766663,8.71763057233982));
#60369=CARTESIAN_POINT('Ctrl Pts',(57.0398434325917,27.6396369028923,8.71339795816837));
#60370=CARTESIAN_POINT('Ctrl Pts',(56.9925586261697,27.5735847830044,8.70916534399691));
#60371=CARTESIAN_POINT('Ctrl Pts',(56.9453412670842,27.5076268802634,8.70493876725215));
#60372=CARTESIAN_POINT('Ctrl Pts',(56.8947755227792,27.443918416245,8.70071219050739));
#60373=CARTESIAN_POINT('Ctrl Pts',(56.8411051950176,27.382816673695,8.69648561376262));
#60374=CARTESIAN_POINT('Ctrl Pts',(56.7874944351046,27.3217827470032,8.69226372802859));
#60375=CARTESIAN_POINT('Ctrl Pts',(56.7307862434185,27.2633501403435,8.68804184229456));
#60376=CARTESIAN_POINT('Ctrl Pts',(56.6712659778491,27.2078447943094,8.68381995656052));
#60377=CARTESIAN_POINT('Ctrl Pts',(56.6117858568535,27.1523768849103,8.67960091835753));
#60378=CARTESIAN_POINT('Ctrl Pts',(56.5494977677676,27.0998326309214,8.67538188015453));
#60379=CARTESIAN_POINT('Ctrl Pts',(56.4847244939177,27.0505017498954,8.67116284195153));
#60380=CARTESIAN_POINT('Ctrl Pts',(56.4199723726575,27.0011869785367,8.6669451815326));
#60381=CARTESIAN_POINT('Ctrl Pts',(56.3527370476518,26.9550837774033,8.66272752111366));
#60382=CARTESIAN_POINT('Ctrl Pts',(56.2833739360523,26.9124412366926,8.65850986069472));
#60383=CARTESIAN_POINT('Ctrl Pts',(56.2140122678729,26.8697995833571,8.65429228804371));
#60384=CARTESIAN_POINT('Ctrl Pts',(56.1425232974958,26.8306186895519,8.65007471539269));
#60385=CARTESIAN_POINT('Ctrl Pts',(56.0692897141918,26.7951032320937,8.64585714274168));
#60386=CARTESIAN_POINT('Ctrl Pts',(55.995931812787,26.7595274851614,8.64163241052536));
#60387=CARTESIAN_POINT('Ctrl Pts',(55.9208237932188,26.7276298276872,8.63740767830904));
#60388=CARTESIAN_POINT('Ctrl Pts',(55.8443715384095,26.6995680937867,8.63318294609272));
#60389=CARTESIAN_POINT('Ctrl Pts',(55.7679383783536,26.671513368599,8.62895926904763));
#60390=CARTESIAN_POINT('Ctrl Pts',(55.6901621058367,26.6472927694118,8.62473559200254));
#60391=CARTESIAN_POINT('Ctrl Pts',(55.6114629313621,26.6270138362034,8.62051191495746));
#60392=CARTESIAN_POINT('Ctrl Pts',(55.5326209689902,26.6066981098997,8.61628057468124));
#60393=CARTESIAN_POINT('Ctrl Pts',(55.4528532146922,26.5903384353346,8.61204923440502));
#60394=CARTESIAN_POINT('Ctrl Pts',(55.3725899949738,26.5779911342761,8.6078178941288));
#60395=CARTESIAN_POINT('Ctrl Pts',(55.2925574532021,26.5656793195844,8.60359871480114));
#60396=CARTESIAN_POINT('Ctrl Pts',(55.2120327515495,26.5573568099956,8.59937953547349));
#60397=CARTESIAN_POINT('Ctrl Pts',(55.1314433529275,26.5530278107483,8.59516035614583));
#60398=CARTESIAN_POINT('Ctrl Pts',(55.0505973390032,26.5486850269653,8.59092774197442));
#60399=CARTESIAN_POINT('Ctrl Pts',(54.9693855250677,26.5483451018986,8.58669512780302));
#60400=CARTESIAN_POINT('Ctrl Pts',(54.8882374538426,26.552049963076,8.58246251363161));
#60401=CARTESIAN_POINT('Ctrl Pts',(54.807205132722,26.5557495396167,8.57823593688691));
#60402=CARTESIAN_POINT('Ctrl Pts',(54.7262368339361,26.5634824224046,8.57400936014221));
#60403=CARTESIAN_POINT('Ctrl Pts',(54.6457649811417,26.5752386093856,8.56978278339751));
#60404=CARTESIAN_POINT('Ctrl Pts',(54.5653824427835,26.5869817483606,8.56556089766346));
#60405=CARTESIAN_POINT('Ctrl Pts',(54.4854957129381,26.6027392519697,8.56133901192941));
#60406=CARTESIAN_POINT('Ctrl Pts',(54.4065335478631,26.6224491971384,8.55711712619536));
#60407=CARTESIAN_POINT('Ctrl Pts',(54.3276246403217,26.6421458485597,8.55289808799242));
#60408=CARTESIAN_POINT('Ctrl Pts',(54.2496395086022,26.6657895348154,8.54867904978947));
#60409=CARTESIAN_POINT('Ctrl Pts',(54.1729968985998,26.6932672195778,8.54446001158653));
#60410=CARTESIAN_POINT('Ctrl Pts',(54.0963793172795,26.7207359311301,8.54024235116764));
#60411=CARTESIAN_POINT('Ctrl Pts',(54.0211038239627,26.7520359980488,8.53602469074875));
#60412=CARTESIAN_POINT('Ctrl Pts',(53.9475728511745,26.7870048923653,8.53180703032986));
#60413=CARTESIAN_POINT('Ctrl Pts',(53.8740434085379,26.8219730589925,8.52758945767888));
#60414=CARTESIAN_POINT('Ctrl Pts',(53.8022588332697,26.860609700648,8.5233718850279));
#60415=CARTESIAN_POINT('Ctrl Pts',(53.7325991497947,26.9027052341412,8.51915431237692));
#60416=CARTESIAN_POINT('Ctrl Pts',(53.662821215112,26.9448722271562,8.51492958016054));
#60417=CARTESIAN_POINT('Ctrl Pts',(53.5951757889163,26.9905096183042,8.51070484794416));
#60418=CARTESIAN_POINT('Ctrl Pts',(53.5300162294356,27.0393628677704,8.50648011572778));
#60419=CARTESIAN_POINT('Ctrl Pts',(53.4648729442408,27.0882039156235,8.50225643868274));
#60420=CARTESIAN_POINT('Ctrl Pts',(53.4022146291533,27.1402589013781,8.49803276163769));
#60421=CARTESIAN_POINT('Ctrl Pts',(53.3423602543571,27.1952338867141,8.49380908459265));
#60422=CARTESIAN_POINT('Ctrl Pts',(53.2823972827381,27.2503086159496,8.48957774431648));
#60423=CARTESIAN_POINT('Ctrl Pts',(53.2252487452473,27.3083136005641,8.48534640404031));
#60424=CARTESIAN_POINT('Ctrl Pts',(53.1711961561012,27.3689185334445,8.48111506376414));
#60425=CARTESIAN_POINT('Ctrl Pts',(53.1172989150709,27.429349286655,8.47689588443622));
#60426=CARTESIAN_POINT('Ctrl Pts',(53.0664800715651,27.4923646569045,8.4726767051083));
#60427=CARTESIAN_POINT('Ctrl Pts',(53.0189758641979,27.557608366854,8.46845752578038));
#60428=CARTESIAN_POINT('Ctrl Pts',(52.9710150013666,27.6234792611793,8.46419778770196));
#60429=CARTESIAN_POINT('Ctrl Pts',(52.9262542749234,27.691866689358,8.45993804962353));
#60430=CARTESIAN_POINT('Ctrl Pts',(52.8849658519662,27.7624294756859,8.45567831154511));
#60431=CARTESIAN_POINT('Ctrl Pts',(52.8437376019429,27.8328894251997,8.45142478152501));
#60432=CARTESIAN_POINT('Ctrl Pts',(52.8059718335822,27.9055180461353,8.4471712515049));
#60433=CARTESIAN_POINT('Ctrl Pts',(52.7718988642993,27.9799433451571,8.4429177214848));
#60434=CARTESIAN_POINT('Ctrl Pts',(52.7378655894756,28.054281939907,8.4386691467585));
#60435=CARTESIAN_POINT('Ctrl Pts',(52.7075167558013,28.130412641639,8.4344205720322));
#60436=CARTESIAN_POINT('Ctrl Pts',(52.6810372815973,28.2079380323115,8.4301719973059));
#60437=CARTESIAN_POINT('Ctrl Pts',(52.6545822678531,28.2853918087714,8.4259273472078));
#60438=CARTESIAN_POINT('Ctrl Pts',(52.6319896538309,28.3642372819011,8.42168269710969));
#60439=CARTESIAN_POINT('Ctrl Pts',(52.6133961035504,28.4440574746867,8.41743804701158));
#60440=CARTESIAN_POINT('Ctrl Pts',(52.594812424493,28.5238352913302,8.41319565037704));
#60441=CARTESIAN_POINT('Ctrl Pts',(52.5802236919809,28.6045863549805,8.40895325374249));
#60442=CARTESIAN_POINT('Ctrl Pts',(52.5697162820903,28.685880117689,8.40471085710795));
#60443=CARTESIAN_POINT('Ctrl Pts',(52.5592102493312,28.7671632258017,8.40046901649419));
#60444=CARTESIAN_POINT('Ctrl Pts',(52.5527845372909,28.8489884393477,8.39622717588043));
#60445=CARTESIAN_POINT('Ctrl Pts',(52.5504739432897,28.9309178206984,8.39198533526666));
#60446=CARTESIAN_POINT('Ctrl Pts',(52.5498097834161,28.9544676990108,8.3907660555818));
#60447=CARTESIAN_POINT('Ctrl Pts',(52.5494852960204,28.9780261599311,8.38954677589693));
#60448=CARTESIAN_POINT('Ctrl Pts',(52.5495005111525,29.0015827691152,8.38832749621206));
#60449=CARTESIAN_POINT('',(52.5495001241791,29.000780129339,7.58832749625521));
#60450=CARTESIAN_POINT('Ctrl Pts',(52.5495005111528,29.0015827696721,8.38832749618324));
#60451=CARTESIAN_POINT('Ctrl Pts',(52.54956003669,29.093742292839,8.38355735997699));
#60452=CARTESIAN_POINT('Ctrl Pts',(52.5548225910511,29.185703809808,8.37878722377074));
#60453=CARTESIAN_POINT('Ctrl Pts',(52.5651971369812,29.2769210505458,8.3740170875645));
#60454=CARTESIAN_POINT('Ctrl Pts',(52.5756211608251,29.3685733212895,8.36922420179507));
#60455=CARTESIAN_POINT('Ctrl Pts',(52.5912059224144,29.4594739912179,8.36443131602564));
#60456=CARTESIAN_POINT('Ctrl Pts',(52.6118095392283,29.5490870359779,8.3596384302562));
#60457=CARTESIAN_POINT('Ctrl Pts',(52.6325284203184,29.6392014093562,8.35481873130564));
#60458=CARTESIAN_POINT('Ctrl Pts',(52.6583223494864,29.7280135082775,8.34999903235508));
#60459=CARTESIAN_POINT('Ctrl Pts',(52.6889989463192,29.8149996195619,8.34517933340452));
#60460=CARTESIAN_POINT('Ctrl Pts',(52.696264700189,29.8356022854357,8.34403778740799));
#60461=CARTESIAN_POINT('Ctrl Pts',(52.7038041549949,29.8561026184683,8.34289624141145));
#60462=CARTESIAN_POINT('Ctrl Pts',(52.7116143735494,29.8764938531754,8.34175469541492));
#60463=CARTESIAN_POINT('Ctrl Pts',(52.7405730329762,29.9521002932589,8.33752208124372));
#60464=CARTESIAN_POINT('Ctrl Pts',(52.7733365344255,30.0264106373841,8.33328946707252));
#60465=CARTESIAN_POINT('Ctrl Pts',(52.8097682372598,30.0990155028406,8.32905685290132));
#60466=CARTESIAN_POINT('Ctrl Pts',(52.8461479736908,30.1715168042739,8.3248302761568));
#60467=CARTESIAN_POINT('Ctrl Pts',(52.8861853127835,30.2423170469457,8.32060369941229));
#60468=CARTESIAN_POINT('Ctrl Pts',(52.9296950125962,30.3110253655558,8.31637712266778));
#60469=CARTESIAN_POINT('Ctrl Pts',(52.9731564216839,30.3796574258942,8.31215523693368));
#60470=CARTESIAN_POINT('Ctrl Pts',(53.0200822864821,30.4462017850736,8.30793335119959));
#60471=CARTESIAN_POINT('Ctrl Pts',(53.0702414384091,30.5102920724041,8.30371146546549));
#60472=CARTESIAN_POINT('Ctrl Pts',(53.1203667595396,30.5743391328181,8.29949242726274));
#60473=CARTESIAN_POINT('Ctrl Pts',(53.173720751063,30.6359350438601,8.29527338905999));
#60474=CARTESIAN_POINT('Ctrl Pts',(53.2300296387102,30.6947433936014,8.29105435085723));
#60475=CARTESIAN_POINT('Ctrl Pts',(53.2863201379277,30.7535325386799,8.28683669043854));
#60476=CARTESIAN_POINT('Ctrl Pts',(53.3455632958838,30.8095355950081,8.28261903001984));
#60477=CARTESIAN_POINT('Ctrl Pts',(53.4074467805978,30.8624512056351,8.27840136960114));
#60478=CARTESIAN_POINT('Ctrl Pts',(53.4693289775399,30.9153657151083,8.27418379695036));
#60479=CARTESIAN_POINT('Ctrl Pts',(53.5338510381637,30.9651926056109,8.26996622429957));
#60480=CARTESIAN_POINT('Ctrl Pts',(53.6006667801059,31.0116701493289,8.26574865164879));
#60481=CARTESIAN_POINT('Ctrl Pts',(53.6675959455129,31.0582265912808,8.26152391943218));
#60482=CARTESIAN_POINT('Ctrl Pts',(53.7368261991617,31.1014220440101,8.25729918721557));
#60483=CARTESIAN_POINT('Ctrl Pts',(53.8079811591194,31.1410374431536,8.25307445499896));
#60484=CARTESIAN_POINT('Ctrl Pts',(53.8791183473698,31.1806429479302,8.24885077795411));
#60485=CARTESIAN_POINT('Ctrl Pts',(53.9521788531332,31.2166700001067,8.24462710090925));
#60486=CARTESIAN_POINT('Ctrl Pts',(54.0267643159805,31.2489469876702,8.2404034238644));
#60487=CARTESIAN_POINT('Ctrl Pts',(54.1014851030099,31.2812825370068,8.23617208358841));
#60488=CARTESIAN_POINT('Ctrl Pts',(54.1777359402165,31.3098542608292,8.23194074331241));
#60489=CARTESIAN_POINT('Ctrl Pts',(54.2551005051838,31.3345395675856,8.22770940303642));
#60490=CARTESIAN_POINT('Ctrl Pts',(54.332242723019,31.3591539283325,8.22349022370744));
#60491=CARTESIAN_POINT('Ctrl Pts',(54.4104918140557,31.3799041451524,8.21927104437846));
#60492=CARTESIAN_POINT('Ctrl Pts',(54.4894261756389,31.3967195538647,8.21505186504948));
#60493=CARTESIAN_POINT('Ctrl Pts',(54.5686118824718,31.4135885067245,8.21081925087842));
#60494=CARTESIAN_POINT('Ctrl Pts',(54.6487817503826,31.4265602664254,8.20658663670737));
#60495=CARTESIAN_POINT('Ctrl Pts',(54.7295179915529,31.4355265823034,8.20235402253631));
#60496=CARTESIAN_POINT('Ctrl Pts',(54.8101390700559,31.4444801085737,8.19812744579195));
#60497=CARTESIAN_POINT('Ctrl Pts',(54.8913244593947,31.4494394876987,8.19390086904759));
#60498=CARTESIAN_POINT('Ctrl Pts',(54.9726454460324,31.4503473179077,8.18967429230322));
#60499=CARTESIAN_POINT('Ctrl Pts',(55.053876175802,31.4512541405303,8.18545240656909));
#60500=CARTESIAN_POINT('Ctrl Pts',(55.1352417416545,31.4481183441097,8.18123052083496));
#60501=CARTESIAN_POINT('Ctrl Pts',(55.2163089742501,31.4409343861847,8.17700863510082));
#60502=CARTESIAN_POINT('Ctrl Pts',(55.2973215295009,31.4337552736175,8.17278959689824));
#60503=CARTESIAN_POINT('Ctrl Pts',(55.3780356895875,31.4225334631796,8.16857055869565));
#60504=CARTESIAN_POINT('Ctrl Pts',(55.4580202207648,31.4073154607094,8.16435152049306));
#60505=CARTESIAN_POINT('Ctrl Pts',(55.5379786319102,31.392102427884,8.16013386007453));
#60506=CARTESIAN_POINT('Ctrl Pts',(55.6172074313242,31.3728958814592,8.15591619965601));
#60507=CARTESIAN_POINT('Ctrl Pts',(55.6952837994118,31.3497937544124,8.15169853923748));
#60508=CARTESIAN_POINT('Ctrl Pts',(55.7733585427597,31.3266921081121,8.14748096658687));
#60509=CARTESIAN_POINT('Ctrl Pts',(55.8502804573394,31.299695175302,8.14326339393626));
#60510=CARTESIAN_POINT('Ctrl Pts',(55.9256415373002,31.2689508576487,8.13904582128565));
#60511=CARTESIAN_POINT('Ctrl Pts',(56.0011305469222,31.2381543497912,8.13482108906885));
#60512=CARTESIAN_POINT('Ctrl Pts',(56.0750529882894,31.2035979058228,8.13059635685204));
#60513=CARTESIAN_POINT('Ctrl Pts',(56.1470202020595,31.1654779855882,8.12637162463524));
#60514=CARTESIAN_POINT('Ctrl Pts',(56.2189694412471,31.1273675862121,8.12214794759057));
#60515=CARTESIAN_POINT('Ctrl Pts',(56.2889640397234,31.0856957471054,8.11792427054589));
#60516=CARTESIAN_POINT('Ctrl Pts',(56.3566431772644,31.0407031973273,8.11370059350122));
#60517=CARTESIAN_POINT('Ctrl Pts',(56.4244451084916,30.9956290152879,8.10946925322541));
#60518=CARTESIAN_POINT('Ctrl Pts',(56.4899228084764,30.9472223589163,8.10523791294961));
#60519=CARTESIAN_POINT('Ctrl Pts',(56.5527467980732,30.8957657110185,8.1010065726738));
#60520=CARTESIAN_POINT('Ctrl Pts',(56.6153902304262,30.8444569504258,8.09678739334387));
#60521=CARTESIAN_POINT('Ctrl Pts',(56.6753949040331,30.7901160735973,8.09256821401394));
#60522=CARTESIAN_POINT('Ctrl Pts',(56.7324720231711,30.7330582618393,8.08834903468401));
#60523=CARTESIAN_POINT('Ctrl Pts',(56.7897308890671,30.6758187648024,8.08411642051055));
#60524=CARTESIAN_POINT('Ctrl Pts',(56.8442564691055,30.6156320935251,8.07988380633709));
#60525=CARTESIAN_POINT('Ctrl Pts',(56.8957305158735,30.5527897672209,8.07565119216363));
#60526=CARTESIAN_POINT('Ctrl Pts',(56.947131139747,30.4900370795945,8.07142461541686));
#60527=CARTESIAN_POINT('Ctrl Pts',(56.9954885835029,30.4246366168747,8.06719803867008));
#60528=CARTESIAN_POINT('Ctrl Pts',(57.0405213050927,30.3569167452216,8.06297146192331));
#60529=CARTESIAN_POINT('Ctrl Pts',(57.0855040455498,30.2892720348241,8.05874957618978));
#60530=CARTESIAN_POINT('Ctrl Pts',(57.1271691400413,30.2193134154538,8.05452769045625));
#60531=CARTESIAN_POINT('Ctrl Pts',(57.1652761216738,30.14740122316,8.05030580472271));
#60532=CARTESIAN_POINT('Ctrl Pts',(57.2033574013513,30.0755375333677,8.04608676651771));
#60533=CARTESIAN_POINT('Ctrl Pts',(57.2378851174962,30.0017232969852,8.04186772831271));
#60534=CARTESIAN_POINT('Ctrl Pts',(57.26866351638,29.9263455615732,8.03764869010771));
#60535=CARTESIAN_POINT('Ctrl Pts',(57.2994318641608,29.8509924417816,8.03343102968677));
#60536=CARTESIAN_POINT('Ctrl Pts',(57.3264531507695,29.7740772666921,8.02921336926582));
#60537=CARTESIAN_POINT('Ctrl Pts',(57.3495793415295,29.69600802284,8.02499570884488));
#60538=CARTESIAN_POINT('Ctrl Pts',(57.3727050510423,29.6179404035795,8.02077813619187));
#60539=CARTESIAN_POINT('Ctrl Pts',(57.3919356950475,29.5387192090555,8.01656056353886));
#60540=CARTESIAN_POINT('Ctrl Pts',(57.4071732184801,29.4587672026555,8.01234299088585));
#60541=CARTESIAN_POINT('Ctrl Pts',(57.4224366084445,29.3786794733389,8.00811825867191));
#60542=CARTESIAN_POINT('Ctrl Pts',(57.4336932281304,29.2978589087463,8.00389352645796));
#60543=CARTESIAN_POINT('Ctrl Pts',(57.4408962865524,29.2167384790355,7.99966879424403));
#60544=CARTESIAN_POINT('Ctrl Pts',(57.4480975459424,29.1356383099208,7.99544511719699));
#60545=CARTESIAN_POINT('Ctrl Pts',(57.451247271857,29.0542388920839,7.99122144014996));
#60546=CARTESIAN_POINT('Ctrl Pts',(57.4503509630831,28.9729739437261,7.98699776310293));
#60547=CARTESIAN_POINT('Ctrl Pts',(57.4494530280908,28.8915615522583,7.9827664228248));
#60548=CARTESIAN_POINT('Ctrl Pts',(57.4444944161923,28.8102845828779,7.97853508254668));
#60549=CARTESIAN_POINT('Ctrl Pts',(57.435532712379,28.7295731948718,7.97430374226855));
#60550=CARTESIAN_POINT('Ctrl Pts',(57.426596764692,28.6490937731021,7.97008456295189));
#60551=CARTESIAN_POINT('Ctrl Pts',(57.4136808590501,28.5691771222106,7.96586538363523));
#60552=CARTESIAN_POINT('Ctrl Pts',(57.3968921568583,28.4902370762884,7.96164620431857));
#60553=CARTESIAN_POINT('Ctrl Pts',(57.3800499955182,28.4110456668256,7.95741359014969));
#60554=CARTESIAN_POINT('Ctrl Pts',(57.3592476670589,28.3325425624581,7.95318097598081));
#60555=CARTESIAN_POINT('Ctrl Pts',(57.3345564510021,28.2551534204384,7.94894836181193));
#60556=CARTESIAN_POINT('Ctrl Pts',(57.3099004546465,28.1778746667632,7.94472178506973));
#60557=CARTESIAN_POINT('Ctrl Pts',(57.2813667280436,28.1017071584427,7.94049520832754));
#60558=CARTESIAN_POINT('Ctrl Pts',(57.2490774412937,28.0270658228514,7.93626863158534));
#60559=CARTESIAN_POINT('Ctrl Pts',(57.2168239918883,27.9525073304422,7.93204674585066));
#60560=CARTESIAN_POINT('Ctrl Pts',(57.1808234481206,27.8794720692538,7.92782486011599));
#60561=CARTESIAN_POINT('Ctrl Pts',(57.1412471585885,27.8083579162195,7.92360297438131));
#60562=CARTESIAN_POINT('Ctrl Pts',(57.1016975620664,27.73729172753,7.91938393618084));
#60563=CARTESIAN_POINT('Ctrl Pts',(57.0585772350112,27.6681444784381,7.91516489798036));
#60564=CARTESIAN_POINT('Ctrl Pts',(57.012104274193,27.6012910811129,7.91094585977989));
#60565=CARTESIAN_POINT('Ctrl Pts',(56.9656464897493,27.5344595156696,7.90672819936345));
#60566=CARTESIAN_POINT('Ctrl Pts',(56.9158385107976,27.4699206954975,7.90251053894701));
#60567=CARTESIAN_POINT('Ctrl Pts',(56.8629419765386,27.4080209040159,7.89829287853057));
#60568=CARTESIAN_POINT('Ctrl Pts',(56.8100465430362,27.3461224006452,7.89407530588203));
#60569=CARTESIAN_POINT('Ctrl Pts',(56.7540629847037,27.2868631691755,7.88985773323349));
#60570=CARTESIAN_POINT('Ctrl Pts',(56.6952925448785,27.2305556133975,7.88564016058495));
#60571=CARTESIAN_POINT('Ctrl Pts',(56.6364223388707,27.1741524723232,7.88141542836563));
#60572=CARTESIAN_POINT('Ctrl Pts',(56.5747561231674,27.1207113551315,7.87719069614631));
#60573=CARTESIAN_POINT('Ctrl Pts',(56.5106316110116,27.0705072205855,7.87296596392699));
#60574=CARTESIAN_POINT('Ctrl Pts',(56.4465231147079,27.0203156251134,7.8687422868843));
#60575=CARTESIAN_POINT('Ctrl Pts',(56.3799579429414,26.9733596468785,7.86451860984161));
#60576=CARTESIAN_POINT('Ctrl Pts',(56.3113029030241,26.9298707898973,7.86029493279892));
#60577=CARTESIAN_POINT('Ctrl Pts',(56.2425232987904,26.88630302888,7.85606359252503));
#60578=CARTESIAN_POINT('Ctrl Pts',(56.1716466542426,26.8462151899789,7.85183225225114));
#60579=CARTESIAN_POINT('Ctrl Pts',(56.0990651471578,26.8097931485125,7.84760091197725));
#60580=CARTESIAN_POINT('Ctrl Pts',(56.0266922403633,26.7734757845145,7.84338173263587));
#60581=CARTESIAN_POINT('Ctrl Pts',(55.9526247076398,26.7408032826157,7.83916255329449));
#60582=CARTESIAN_POINT('Ctrl Pts',(55.8772680222262,26.7119110447408,7.83494337395311));
#60583=CARTESIAN_POINT('Ctrl Pts',(55.8016713839619,26.6829268073995,7.83071075978369));
#60584=CARTESIAN_POINT('Ctrl Pts',(55.7244961952023,26.6576391719911,7.82647814561427));
#60585=CARTESIAN_POINT('Ctrl Pts',(55.6461383126182,26.6362200756063,7.82224553144485));
#60586=CARTESIAN_POINT('Ctrl Pts',(55.567892200197,26.6148315315514,7.81801895470215));
#60587=CARTESIAN_POINT('Ctrl Pts',(55.4884671889393,26.59730068832,7.81379237795946));
#60588=CARTESIAN_POINT('Ctrl Pts',(55.4082778398956,26.5837509533473,7.80956580121676));
#60589=CARTESIAN_POINT('Ctrl Pts',(55.3281774916941,26.570216257003,7.80534391548222));
#60590=CARTESIAN_POINT('Ctrl Pts',(55.2473149470752,26.5606539662429,7.80112202974767));
#60591=CARTESIAN_POINT('Ctrl Pts',(55.1661172375628,26.5551369540638,7.79690014401313));
#60592=CARTESIAN_POINT('Ctrl Pts',(55.0849742934391,26.5496236629418,7.79268110581226));
#60593=CARTESIAN_POINT('Ctrl Pts',(55.0034970956777,26.5481502629355,7.7884620676114));
#60594=CARTESIAN_POINT('Ctrl Pts',(54.9221188621217,26.5507379114593,7.78424302941054));
#60595=CARTESIAN_POINT('Ctrl Pts',(54.8407672037304,26.5533247149514,7.78002536899375));
#60596=CARTESIAN_POINT('Ctrl Pts',(54.7595149093206,26.559969918488,7.77580770857697));
#60597=CARTESIAN_POINT('Ctrl Pts',(54.678794886752,26.5706425694799,7.77159004816019));
#60598=CARTESIAN_POINT('Ctrl Pts',(54.5980765439369,26.5813149983779,7.76737247551134));
#60599=CARTESIAN_POINT('Ctrl Pts',(54.5178909113262,26.5960146460401,7.76315490286249));
#60600=CARTESIAN_POINT('Ctrl Pts',(54.4386640382166,26.614658894831,7.75893733021364));
#60601=CARTESIAN_POINT('Ctrl Pts',(54.3593026729739,26.6333347932971,7.75471259799481));
#60602=CARTESIAN_POINT('Ctrl Pts',(54.2809037781545,26.6559685834207,7.75048786577598));
#60603=CARTESIAN_POINT('Ctrl Pts',(54.2038818474671,26.6824266705868,7.74626313355715));
#60604=CARTESIAN_POINT('Ctrl Pts',(54.1268791539015,26.7088781495383,7.74203945651425));
#60605=CARTESIAN_POINT('Ctrl Pts',(54.0512531615973,26.7391518224769,7.73781577947137));
#60606=CARTESIAN_POINT('Ctrl Pts',(53.9773977521605,26.7730660331493,7.73359210242848));
#60607=CARTESIAN_POINT('Ctrl Pts',(53.9034083431144,26.8070417760914,7.72936076215445));
#60608=CARTESIAN_POINT('Ctrl Pts',(53.8311963500906,26.8446710417584,7.72512942188042));
#60609=CARTESIAN_POINT('Ctrl Pts',(53.7611311918934,26.8857260522107,7.72089808160639));
#60610=CARTESIAN_POINT('Ctrl Pts',(53.6912674019958,26.9266630699565,7.71667890226682));
#60611=CARTESIAN_POINT('Ctrl Pts',(53.6235384586531,26.971005848546,7.71245972292724));
#60612=CARTESIAN_POINT('Ctrl Pts',(53.5582786803735,27.0184879797149,7.70824054358767));
#60613=CARTESIAN_POINT('Ctrl Pts',(53.493336088166,27.0657393305918,7.70404187098223));
#60614=CARTESIAN_POINT('Ctrl Pts',(53.4305885577082,27.1162817178861,7.69984319837678));
#60615=CARTESIAN_POINT('Ctrl Pts',(53.3703926384257,27.1698824909031,7.69564452577134));
#60616=CARTESIAN_POINT('Ctrl Pts',(53.3102828322357,27.2234065854944,7.69145185956444));
#60617=CARTESIAN_POINT('Ctrl Pts',(53.2527177405871,27.2799800682008,7.68725919335755));
#60618=CARTESIAN_POINT('Ctrl Pts',(53.1980236960905,27.3393279522589,7.68306652715065));
#60619=CARTESIAN_POINT('Ctrl Pts',(53.1433919473746,27.3986082398757,7.67887863633415));
#60620=CARTESIAN_POINT('Ctrl Pts',(53.0916250678718,27.4606563049205,7.67469074551765));
#60621=CARTESIAN_POINT('Ctrl Pts',(53.0430139528752,27.5251590386218,7.67050285470115));
#60622=CARTESIAN_POINT('Ctrl Pts',(52.9944325484566,27.5896223489628,7.66631752347739));
#60623=CARTESIAN_POINT('Ctrl Pts',(52.9490033651089,27.6565369742822,7.66213219225362));
#60624=CARTESIAN_POINT('Ctrl Pts',(52.9069774212357,27.7255563038005,7.65794686102986));
#60625=CARTESIAN_POINT('Ctrl Pts',(52.864963787464,27.7945554164032,7.65376275575959));
#60626=CARTESIAN_POINT('Ctrl Pts',(52.8263516595754,27.8656576054518,7.64957865048931));
#60627=CARTESIAN_POINT('Ctrl Pts',(52.791348199437,27.9384881188277,7.64539454521904));
#60628=CARTESIAN_POINT('Ctrl Pts',(52.7563438519329,28.0113204785156,7.64121033387833));
#60629=CARTESIAN_POINT('Ctrl Pts',(52.724948556607,28.0858808223611,7.63702612253763));
#60630=CARTESIAN_POINT('Ctrl Pts',(52.6973223782933,28.1617720951368,7.63284191119692));
#60631=CARTESIAN_POINT('Ctrl Pts',(52.6696696439529,28.2377363193953,7.62865367772811));
#60632=CARTESIAN_POINT('Ctrl Pts',(52.6457934207092,28.3150335811986,7.6244654442593));
#60633=CARTESIAN_POINT('Ctrl Pts',(52.6258044213698,28.3932499654614,7.62027721079048));
#60634=CARTESIAN_POINT('Ctrl Pts',(52.6058048288362,28.4715078005907,7.61608675776233));
#60635=CARTESIAN_POINT('Ctrl Pts',(52.5896966540588,28.5506852641807,7.61189630473417));
#60636=CARTESIAN_POINT('Ctrl Pts',(52.5775393163813,28.6303589764087,7.60770585170601));
#60637=CARTESIAN_POINT('Ctrl Pts',(52.5653624033685,28.7101609765624,7.60350865135165));
#60638=CARTESIAN_POINT('Ctrl Pts',(52.5571490730172,28.7904603501842,7.59931145099729));
#60639=CARTESIAN_POINT('Ctrl Pts',(52.5529067564705,28.8708299281092,7.59511425064293));
#60640=CARTESIAN_POINT('Ctrl Pts',(52.5506201878051,28.9141483737054,7.59285199918035));
#60641=CARTESIAN_POINT('Ctrl Pts',(52.5494863416593,28.9574872273925,7.59058974771779));
#60642=CARTESIAN_POINT('Ctrl Pts',(52.5495001241791,29.000780129339,7.58832749625521));
#60643=CARTESIAN_POINT('',(52.5495009849895,28.9978028581341,6.78832749625012));
#60644=CARTESIAN_POINT('Ctrl Pts',(52.5495001241794,29.000780130165,7.58832749621205));
#60645=CARTESIAN_POINT('Ctrl Pts',(52.5495139128642,29.0440923516512,7.58606423521544));
#60646=CARTESIAN_POINT('Ctrl Pts',(52.5506759352354,29.0873847550339,7.58380097421883));
#60647=CARTESIAN_POINT('Ctrl Pts',(52.5529834801352,29.1306154719347,7.58153771322222));
#60648=CARTESIAN_POINT('Ctrl Pts',(52.5572989113675,29.2114629501035,7.5773050990735));
#60649=CARTESIAN_POINT('Ctrl Pts',(52.5656333752337,29.2922466793995,7.57307248492477));
#60650=CARTESIAN_POINT('Ctrl Pts',(52.5779826895163,29.3725350959535,7.56883987077604));
#60651=CARTESIAN_POINT('Ctrl Pts',(52.5903143886615,29.4527089886203,7.56461329405396));
#60652=CARTESIAN_POINT('Ctrl Pts',(52.6066494940107,29.5323885164452,7.56038671733188));
#60653=CARTESIAN_POINT('Ctrl Pts',(52.626931883058,29.6111447965527,7.5561601406098));
#60654=CARTESIAN_POINT('Ctrl Pts',(52.6471917611382,29.6898136668373,7.55193825487009));
#60655=CARTESIAN_POINT('Ctrl Pts',(52.6713901026035,29.7675608778629,7.54771636913039));
#60656=CARTESIAN_POINT('Ctrl Pts',(52.6994195524536,29.8439667377138,7.54349448339068));
#60657=CARTESIAN_POINT('Ctrl Pts',(52.7274300971225,29.9203210636733,7.53927544521007));
#60658=CARTESIAN_POINT('Ctrl Pts',(52.759266458567,29.9953354002865,7.53505640702946));
#60659=CARTESIAN_POINT('Ctrl Pts',(52.7947715297969,30.0686054670483,7.53083736884884));
#60660=CARTESIAN_POINT('Ctrl Pts',(52.8302650063662,30.1418516064803,7.52661970845213));
#60661=CARTESIAN_POINT('Ctrl Pts',(52.8694246110104,30.21335418955,7.52240204805542));
#60662=CARTESIAN_POINT('Ctrl Pts',(52.9120457701724,30.282730440952,7.51818438765871));
#60663=CARTESIAN_POINT('Ctrl Pts',(52.954666042406,30.3521052486634,7.51396681502973));
#60664=CARTESIAN_POINT('Ctrl Pts',(53.0007474817649,30.4193534174791,7.50974924240076));
#60665=CARTESIAN_POINT('Ctrl Pts',(53.0500411214562,30.4841194769924,7.50553166977178));
#60666=CARTESIAN_POINT('Ctrl Pts',(53.0994184404249,30.5489954812591,7.50130693752886));
#60667=CARTESIAN_POINT('Ctrl Pts',(53.1520185869289,30.6113805742921,7.49708220528594));
#60668=CARTESIAN_POINT('Ctrl Pts',(53.2075507422407,30.6709506002148,7.49285747304302));
#60669=CARTESIAN_POINT('Ctrl Pts',(53.2630690271832,30.7305057472218,7.4886337960193));
#60670=CARTESIAN_POINT('Ctrl Pts',(53.3215175071784,30.7872469237406,7.48441011899559));
#60671=CARTESIAN_POINT('Ctrl Pts',(53.3825698625209,30.8408883726002,7.48018644197187));
#60672=CARTESIAN_POINT('Ctrl Pts',(53.443732988252,30.8946271458644,7.47595510171645));
#60673=CARTESIAN_POINT('Ctrl Pts',(53.5075090658685,30.9452546624414,7.47172376146103));
#60674=CARTESIAN_POINT('Ctrl Pts',(53.5735396146827,30.9925262906974,7.46749242120561));
#60675=CARTESIAN_POINT('Ctrl Pts',(53.6393803927309,31.0396620610321,7.46327324175599));
#60676=CARTESIAN_POINT('Ctrl Pts',(53.7074622727845,31.0834610304722,7.45905406230637));
#60677=CARTESIAN_POINT('Ctrl Pts',(53.7774057872843,31.1237263573808,7.45483488285675));
#60678=CARTESIAN_POINT('Ctrl Pts',(53.8475720159899,31.164119897182,7.45060226869189));
#60679=CARTESIAN_POINT('Ctrl Pts',(53.9198727351502,31.2011074660635,7.44636965452703));
#60680=CARTESIAN_POINT('Ctrl Pts',(53.9939436613002,31.2344576284553,7.44213704036217));
#60681=CARTESIAN_POINT('Ctrl Pts',(54.0679089322243,31.2677602199697,7.43791046362427));
#60682=CARTESIAN_POINT('Ctrl Pts',(54.143638975022,31.2974355207267,7.43368388688636));
#60683=CARTESIAN_POINT('Ctrl Pts',(54.2207434787784,31.3232971235151,7.42945731014846));
#60684=CARTESIAN_POINT('Ctrl Pts',(54.2977624056204,31.3491300229715,7.42523542441274));
#60685=CARTESIAN_POINT('Ctrl Pts',(54.3761523240618,31.3711574879541,7.42101353867703));
#60686=CARTESIAN_POINT('Ctrl Pts',(54.4555027417914,31.3892410899286,7.41679165294131));
#60687=CARTESIAN_POINT('Ctrl Pts',(54.5347996399532,31.4073124950353,7.41257261474574));
#60688=CARTESIAN_POINT('Ctrl Pts',(54.6150552989914,31.4214452172141,7.40835357655017));
#60689=CARTESIAN_POINT('Ctrl Pts',(54.6958450690456,31.4315509511372,7.4041345383546));
#60690=CARTESIAN_POINT('Ctrl Pts',(54.7766084561026,31.4416533848955,7.39991687794328));
#60691=CARTESIAN_POINT('Ctrl Pts',(54.8579051471828,31.4477313844269,7.39569921753196));
#60692=CARTESIAN_POINT('Ctrl Pts',(54.9393026906921,31.4497481680048,7.39148155712065));
#60693=CARTESIAN_POINT('Ctrl Pts',(55.0206985403457,31.4517649096141,7.38726398447743));
#60694=CARTESIAN_POINT('Ctrl Pts',(55.1021947738211,31.4497205929703,7.38304641183422));
#60695=CARTESIAN_POINT('Ctrl Pts',(55.1833576758483,31.4436305393221,7.378828839191));
#60696=CARTESIAN_POINT('Ctrl Pts',(55.264658356755,31.4375301474437,7.37460410696603));
#60697=CARTESIAN_POINT('Ctrl Pts',(55.3456241083945,31.4273703124783,7.37037937474106));
#60698=CARTESIAN_POINT('Ctrl Pts',(55.4258246986973,31.4132185097872,7.36615464251609));
#60699=CARTESIAN_POINT('Ctrl Pts',(55.5060052577411,31.3990702417137,7.36193096547917));
#60700=CARTESIAN_POINT('Ctrl Pts',(55.5854205879014,31.3809321242811,7.35770728844226));
#60701=CARTESIAN_POINT('Ctrl Pts',(55.6636533401404,31.3589223162539,7.35348361140535));
#60702=CARTESIAN_POINT('Ctrl Pts',(55.7420280340206,31.3368725747182,7.34925227113746));
#60703=CARTESIAN_POINT('Ctrl Pts',(55.8192154204152,31.310937252548,7.34502093086957));
#60704=CARTESIAN_POINT('Ctrl Pts',(55.8948151389593,31.281283874727,7.34078959060168));
#60705=CARTESIAN_POINT('Ctrl Pts',(55.9701975834504,31.2517157208949,7.33657041123156));
#60706=CARTESIAN_POINT('Ctrl Pts',(56.0440010929758,31.2184511171995,7.33235123186144));
#60707=CARTESIAN_POINT('Ctrl Pts',(56.1158539693795,31.1817012098406,7.32813205249133));
#60708=CARTESIAN_POINT('Ctrl Pts',(56.1879356429818,31.1448342817545,7.32389943821827));
#60709=CARTESIAN_POINT('Ctrl Pts',(56.2583223204356,31.1043226757462,7.31966682394521));
#60710=CARTESIAN_POINT('Ctrl Pts',(56.3266215515227,31.0603459682867,7.31543420967216));
#60711=CARTESIAN_POINT('Ctrl Pts',(56.3948233601778,31.016431989466,7.31120763282544));
#60712=CARTESIAN_POINT('Ctrl Pts',(56.4609432489158,30.9690629753186,7.30698105597871));
#60713=CARTESIAN_POINT('Ctrl Pts',(56.5246123690791,30.9184648482709,7.30275447913199));
#60714=CARTESIAN_POINT('Ctrl Pts',(56.5882108219746,30.8679228808087,7.2985325934234));
#60715=CARTESIAN_POINT('Ctrl Pts',(56.6493635493592,30.8141592094933,7.29431070771481));
#60716=CARTESIAN_POINT('Ctrl Pts',(56.707730961565,30.7574428050187,7.29008882200622));
#60717=CARTESIAN_POINT('Ctrl Pts',(56.7660590085238,30.7007646522876,7.28586978370114));
#60718=CARTESIAN_POINT('Ctrl Pts',(56.8216051389128,30.6411380444694,7.28165074539606));
#60719=CARTESIAN_POINT('Ctrl Pts',(56.8740641002604,30.5788711151057,7.27743170709098));
#60720=CARTESIAN_POINT('Ctrl Pts',(56.926505930422,30.5166245198532,7.27321404657014));
#60721=CARTESIAN_POINT('Ctrl Pts',(56.9758622945986,30.4517396703964,7.2689963860493));
#60722=CARTESIAN_POINT('Ctrl Pts',(57.0218669123456,30.3845592940579,7.26477872552846));
#60723=CARTESIAN_POINT('Ctrl Pts',(57.0678705727504,30.3173803157227,7.26056115277585));
#60724=CARTESIAN_POINT('Ctrl Pts',(57.1105223638987,30.2479062894376,7.25634358002325));
#60725=CARTESIAN_POINT('Ctrl Pts',(57.1495990226901,30.1765093674297,7.25212600727065));
#60726=CARTESIAN_POINT('Ctrl Pts',(57.1887420142307,30.1049912489257,7.24790127517525));
#60727=CARTESIAN_POINT('Ctrl Pts',(57.2242975069586,30.0315441136056,7.24367654307985));
#60728=CARTESIAN_POINT('Ctrl Pts',(57.2560878822445,29.9565655845731,7.23945181098445));
#60729=CARTESIAN_POINT('Ctrl Pts',(57.2878703192107,29.8816057782994,7.2352281338396));
#60730=CARTESIAN_POINT('Ctrl Pts',(57.3158893784778,29.8051157880412,7.23100445669475));
#60731=CARTESIAN_POINT('Ctrl Pts',(57.3400169694353,29.7275100224429,7.2267807795499));
#60732=CARTESIAN_POINT('Ctrl Pts',(57.364188336291,29.6497634528124,7.2225494391758));
#60733=CARTESIAN_POINT('Ctrl Pts',(57.3844540087452,29.5708975133715,7.21831809880169));
#60734=CARTESIAN_POINT('Ctrl Pts',(57.4007365544642,29.4913392372477,7.21408675842759));
#60735=CARTESIAN_POINT('Ctrl Pts',(57.41697230132,29.412009625422,7.20986757966034));
#60736=CARTESIAN_POINT('Ctrl Pts',(57.4292478004427,29.3319921139886,7.2056484008931));
#60737=CARTESIAN_POINT('Ctrl Pts',(57.4375378138133,29.2517134407027,7.20142922212585));
#60738=CARTESIAN_POINT('Ctrl Pts',(57.4458542252345,29.1711791344779,7.19719660814569));
#60739=CARTESIAN_POINT('Ctrl Pts',(57.4501906321446,29.0900824681324,7.19296399416552));
#60740=CARTESIAN_POINT('Ctrl Pts',(57.4504840175798,29.0088504003319,7.18873138018536));
#60741=CARTESIAN_POINT('Ctrl Pts',(57.4507769845281,28.9277342024496,7.18450480363166));
#60742=CARTESIAN_POINT('Ctrl Pts',(57.4470383823237,28.8464834473939,7.18027822707797));
#60743=CARTESIAN_POINT('Ctrl Pts',(57.4392569188675,28.7655305270256,7.17605165052427));
#60744=CARTESIAN_POINT('Ctrl Pts',(57.4314840914952,28.6846674504533,7.17182976474244));
#60745=CARTESIAN_POINT('Ctrl Pts',(57.4196773625136,28.6041020118625,7.16760787896062));
#60746=CARTESIAN_POINT('Ctrl Pts',(57.4038774784267,28.5242654955621,7.16338599317879));
#60747=CARTESIAN_POINT('Ctrl Pts',(57.3880882517584,28.4444828309965,7.15916695516493));
#60748=CARTESIAN_POINT('Ctrl Pts',(57.3683113094349,28.3654285667424,7.15494791715107));
#60749=CARTESIAN_POINT('Ctrl Pts',(57.3446389419345,28.2875265043777,7.1507288791372));
#60750=CARTESIAN_POINT('Ctrl Pts',(57.3209743049602,28.2096498819664,7.14651121890626));
#60751=CARTESIAN_POINT('Ctrl Pts',(57.2934169040895,28.1329251583408,7.14229355867531));
#60752=CARTESIAN_POINT('Ctrl Pts',(57.2621092643398,28.057762277242,7.13807589844436));
#60753=CARTESIAN_POINT('Ctrl Pts',(57.2308022760799,27.9826009602296,7.13385832597994));
#60754=CARTESIAN_POINT('Ctrl Pts',(57.1957453838109,27.9090018495065,7.12964075351552));
#60755=CARTESIAN_POINT('Ctrl Pts',(57.1571292135792,27.8373548237217,7.1254231810511));
#60756=CARTESIAN_POINT('Ctrl Pts',(57.1184474864727,27.7655861661161,7.12119844861021));
#60757=CARTESIAN_POINT('Ctrl Pts',(57.0761946134957,27.6957766350037,7.11697371616932));
#60758=CARTESIAN_POINT('Ctrl Pts',(57.0306074353041,27.6282916878259,7.11274898372843));
#60759=CARTESIAN_POINT('Ctrl Pts',(56.9850316473682,27.5608236022051,7.10852530686467));
#60760=CARTESIAN_POINT('Ctrl Pts',(56.9361235170756,27.4956792990654,7.10430163000091));
#60761=CARTESIAN_POINT('Ctrl Pts',(56.8841609282059,27.4331918283905,7.10007795313715));
#60762=CARTESIAN_POINT('Ctrl Pts',(56.8321040609197,27.3705909834609,7.09584661303768));
#60763=CARTESIAN_POINT('Ctrl Pts',(56.7769819752198,27.3106569473758,7.09161527293821));
#60764=CARTESIAN_POINT('Ctrl Pts',(56.7191107230254,27.2536871494548,7.08738393283874));
#60765=CARTESIAN_POINT('Ctrl Pts',(56.6614057773356,27.1968810675,7.08316475247929));
#60766=CARTESIAN_POINT('Ctrl Pts',(56.6009678400075,27.1430224503848,7.07894557211985));
#60767=CARTESIAN_POINT('Ctrl Pts',(56.5381411302798,27.0923647850436,7.07472639176041));
#60768=CARTESIAN_POINT('Ctrl Pts',(56.4751143809048,27.041545826177,7.07049377757077));
#60769=CARTESIAN_POINT('Ctrl Pts',(56.4094491918281,26.9937592464748,7.06626116338113));
#60770=CARTESIAN_POINT('Ctrl Pts',(56.3414694002919,26.9492903428129,7.06202854919149));
#60771=CARTESIAN_POINT('Ctrl Pts',(56.2735865755749,26.904884869886,7.0578019724304));
#60772=CARTESIAN_POINT('Ctrl Pts',(56.2033960912588,26.8637879261263,7.05357539566932));
#60773=CARTESIAN_POINT('Ctrl Pts',(56.1312545011445,26.8262443781234,7.04934881890823));
#60774=CARTESIAN_POINT('Ctrl Pts',(56.0591929801929,26.7887424992942,7.04512693317851));
#60775=CARTESIAN_POINT('Ctrl Pts',(55.9851850663174,26.7547863931242,7.04090504744879));
#60776=CARTESIAN_POINT('Ctrl Pts',(55.9096147140627,26.7245766719222,7.03668316171907));
#60777=CARTESIAN_POINT('Ctrl Pts',(55.8340953313802,26.6943873261256,7.03246412350433));
#60778=CARTESIAN_POINT('Ctrl Pts',(55.7570160335231,26.6679395188327,7.02824508528959));
#60779=CARTESIAN_POINT('Ctrl Pts',(55.6787825589831,26.6453865523997,7.02402604707484));
#60780=CARTESIAN_POINT('Ctrl Pts',(55.6005746326758,26.6228409509526,7.0198083866459));
#60781=CARTESIAN_POINT('Ctrl Pts',(55.5212137242396,26.604187793001,7.01559072621695));
#60782=CARTESIAN_POINT('Ctrl Pts',(55.4411212955882,26.5895306986857,7.011373065788));
#60783=CARTESIAN_POINT('Ctrl Pts',(55.3610305336629,26.574873909385,7.00715549312872));
#60784=CARTESIAN_POINT('Ctrl Pts',(55.2802087389603,26.56421310085,7.00293792046943));
#60785=CARTESIAN_POINT('Ctrl Pts',(55.1990867285295,26.5576006214127,6.99872034781014));
#60786=CARTESIAN_POINT('Ctrl Pts',(55.1178270094009,26.5509769169587,6.99449561560887));
#60787=CARTESIAN_POINT('Ctrl Pts',(55.0362665203414,26.5484153292952,6.99027088340761));
#60788=CARTESIAN_POINT('Ctrl Pts',(54.9548407524154,26.5499161458518,6.98604615120634));
#60789=CARTESIAN_POINT('Ctrl Pts',(54.8734353210632,26.5514165875706,6.98182247415728));
#60790=CARTESIAN_POINT('Ctrl Pts',(54.7921650071736,26.5569773515209,6.97759879710821));
#60791=CARTESIAN_POINT('Ctrl Pts',(54.7114604616645,26.5665466544811,6.97337512005915));
#60792=CARTESIAN_POINT('Ctrl Pts',(54.6306094898613,26.5761333195064,6.96914377978153));
#60793=CARTESIAN_POINT('Ctrl Pts',(54.5503267972118,26.5897429803003,6.9649124395039));
#60794=CARTESIAN_POINT('Ctrl Pts',(54.4710339338915,26.607272445324,6.96068109922628));
#60795=CARTESIAN_POINT('Ctrl Pts',(54.3919689606695,26.6247515301327,6.95646191994917));
#60796=CARTESIAN_POINT('Ctrl Pts',(54.3138885519046,26.6461277175504,6.95224274067206));
#60797=CARTESIAN_POINT('Ctrl Pts',(54.2371927317533,26.6712502664498,6.94802356139495));
#60798=CARTESIAN_POINT('Ctrl Pts',(54.1602526807823,26.6964528158069,6.9437909465276));
#60799=CARTESIAN_POINT('Ctrl Pts',(54.0844198979967,26.7255193857952,6.93955833166025));
#60800=CARTESIAN_POINT('Ctrl Pts',(54.0101099949605,26.7583336492861,6.93532571679289));
#60801=CARTESIAN_POINT('Ctrl Pts',(53.9359060879517,26.791101106343,6.93109913934912));
#60802=CARTESIAN_POINT('Ctrl Pts',(53.863221167765,26.8276054534984,6.92687256190536));
#60803=CARTESIAN_POINT('Ctrl Pts',(53.7924547429285,26.867680909872,6.92264598446159));
#60804=CARTESIAN_POINT('Ctrl Pts',(53.7217668752385,26.9077118788563,6.91842409890192));
#60805=CARTESIAN_POINT('Ctrl Pts',(53.6529936733689,26.9513058523189,6.91420221334225));
#60806=CARTESIAN_POINT('Ctrl Pts',(53.58651244099,26.9982499730176,6.90998032778258));
#60807=CARTESIAN_POINT('Ctrl Pts',(53.520076034353,27.0451624410985,6.90576128887821));
#60808=CARTESIAN_POINT('Ctrl Pts',(53.4559289064382,27.0954203028341,6.90154224997385));
#60809=CARTESIAN_POINT('Ctrl Pts',(53.3944205355582,27.1487666723606,6.89732321106948));
#60810=CARTESIAN_POINT('Ctrl Pts',(53.3329322510764,27.202095620902,6.89310554994986));
#60811=CARTESIAN_POINT('Ctrl Pts',(53.2740813629766,27.2585107700868,6.88888788883023));
#60812=CARTESIAN_POINT('Ctrl Pts',(53.2181842347152,27.3177149978132,6.88467022771061));
#60813=CARTESIAN_POINT('Ctrl Pts',(53.1622882696734,27.3769179934993,6.88045265436053));
#60814=CARTESIAN_POINT('Ctrl Pts',(53.1093462603175,27.4389096137375,6.87623508101046));
#60815=CARTESIAN_POINT('Ctrl Pts',(53.0596366549587,27.5033569766908,6.87201750766039));
#60816=CARTESIAN_POINT('Ctrl Pts',(53.0098426828071,27.5679137192554,6.86779277627448));
#60817=CARTESIAN_POINT('Ctrl Pts',(52.963292376095,27.634934173688,6.86356804488858));
#60818=CARTESIAN_POINT('Ctrl Pts',(52.9202230574265,27.7040531958682,6.85934331350267));
#60819=CARTESIAN_POINT('Ctrl Pts',(52.8771644802957,27.7731549796846,6.85511963576964));
#60820=CARTESIAN_POINT('Ctrl Pts',(52.8375853630188,27.8443538668529,6.85089595803661));
#60821=CARTESIAN_POINT('Ctrl Pts',(52.8016767153071,27.9172604255977,6.84667228030358));
#60822=CARTESIAN_POINT('Ctrl Pts',(52.7657029168312,27.990299262173,6.84244093935153));
#60823=CARTESIAN_POINT('Ctrl Pts',(52.7334130814668,28.0650515344894,6.83820959839948));
#60824=CARTESIAN_POINT('Ctrl Pts',(52.7049501418823,28.1411074579705,6.83397825744744));
#60825=CARTESIAN_POINT('Ctrl Pts',(52.6765690357659,28.2169447139463,6.82975908197479));
#60826=CARTESIAN_POINT('Ctrl Pts',(52.6519929084458,28.2940776758606,6.82553990650215));
#60827=CARTESIAN_POINT('Ctrl Pts',(52.6313130877515,28.3720887309958,6.82132073102951));
#60828=CARTESIAN_POINT('Ctrl Pts',(52.6043609741696,28.4737609287255,6.81582185856627));
#60829=CARTESIAN_POINT('Ctrl Pts',(52.583942728695,28.577232327224,6.81032298610304));
#60830=CARTESIAN_POINT('Ctrl Pts',(52.570251424349,28.6817672092287,6.80482411363981));
#60831=CARTESIAN_POINT('Ctrl Pts',(52.5565601200031,28.7863020912335,6.79932524117658));
#60832=CARTESIAN_POINT('Ctrl Pts',(52.5495959378341,28.8919007970249,6.79382636871335));
#60833=CARTESIAN_POINT('Ctrl Pts',(52.5495009849895,28.9978028581341,6.78832749625011));
#60834=CARTESIAN_POINT('',(52.5495001872432,29.0009579555037,5.9883274961685));
#60835=CARTESIAN_POINT('Ctrl Pts',(52.5495009849888,28.9978028588672,6.78832749621205));
#60836=CARTESIAN_POINT('Ctrl Pts',(52.5494288600355,29.078244722314,6.78415062238013));
#60837=CARTESIAN_POINT('Ctrl Pts',(52.5533219557559,29.1587813112267,6.77997374854822));
#60838=CARTESIAN_POINT('Ctrl Pts',(52.5611815322018,29.2389868848418,6.7757968747163));
#60839=CARTESIAN_POINT('Ctrl Pts',(52.5690366754036,29.3191472179931,6.77162235687663));
#60840=CARTESIAN_POINT('Ctrl Pts',(52.5808538141535,29.3989764342918,6.76744783903695));
#60841=CARTESIAN_POINT('Ctrl Pts',(52.5965821798488,29.4780512857214,6.76327332119728));
#60842=CARTESIAN_POINT('Ctrl Pts',(52.6123067321063,29.5571069649721,6.75909981549485));
#60843=CARTESIAN_POINT('Ctrl Pts',(52.6319405357407,29.6354081765147,6.75492630979243));
#60844=CARTESIAN_POINT('Ctrl Pts',(52.6553815221646,29.7125408362983,6.75075280409001));
#60845=CARTESIAN_POINT('Ctrl Pts',(52.6788243637717,29.7896796005698,6.74657896808502));
#60846=CARTESIAN_POINT('Ctrl Pts',(52.7060748458035,29.8656491754188,6.74240513208003));
#60847=CARTESIAN_POINT('Ctrl Pts',(52.7369812040606,29.94005115777,6.73823129607504));
#60848=CARTESIAN_POINT('Ctrl Pts',(52.7679195171146,30.0145300660479,6.73405314464468));
#60849=CARTESIAN_POINT('Ctrl Pts',(52.8025210667272,30.0874377078138,6.72987499321432));
#60850=CARTESIAN_POINT('Ctrl Pts',(52.8405864519799,30.1583969003011,6.72569684178396));
#60851=CARTESIAN_POINT('Ctrl Pts',(52.8786740011369,30.2293974094004,6.7215162575883));
#60852=CARTESIAN_POINT('Ctrl Pts',(52.9202291526092,30.2984468056787,6.71733567339264));
#60853=CARTESIAN_POINT('Ctrl Pts',(52.965008511472,30.365195916936,6.71315508919698));
#60854=CARTESIAN_POINT('Ctrl Pts',(53.0098618370269,30.4320552845945,6.70896759949861));
#60855=CARTESIAN_POINT('Ctrl Pts',(53.0579497132379,30.4966064052028,6.70478010980025));
#60856=CARTESIAN_POINT('Ctrl Pts',(53.1089881508435,30.558532783213,6.70059262010189));
#60857=CARTESIAN_POINT('Ctrl Pts',(53.133262068887,30.5879850136314,6.69860104695594));
#60858=CARTESIAN_POINT('Ctrl Pts',(53.158202847914,30.6168440727045,6.69660947381));
#60859=CARTESIAN_POINT('Ctrl Pts',(53.1837771558477,30.6450789739035,6.69461790066405));
#60860=CARTESIAN_POINT('Ctrl Pts',(53.2381292618132,30.7050855377514,6.69038528584816));
#60861=CARTESIAN_POINT('Ctrl Pts',(53.2955594916946,30.7625071746051,6.68615267103227));
#60862=CARTESIAN_POINT('Ctrl Pts',(53.3557923422701,30.8170116753236,6.68192005621637));
#60863=CARTESIAN_POINT('Ctrl Pts',(53.4159392761671,30.8714384303332,6.67769347884023));
#60864=CARTESIAN_POINT('Ctrl Pts',(53.4788805492502,30.9229560044402,6.67346690146409));
#60865=CARTESIAN_POINT('Ctrl Pts',(53.5443020495218,30.9712670359374,6.66924032408795));
#60866=CARTESIAN_POINT('Ctrl Pts',(53.6096509272737,31.0195244387526,6.66501843851339));
#60867=CARTESIAN_POINT('Ctrl Pts',(53.6774741897334,31.0645820970959,6.66079655293884));
#60868=CARTESIAN_POINT('Ctrl Pts',(53.7474237724054,31.1061821013542,6.65657466736428));
#60869=CARTESIAN_POINT('Ctrl Pts',(53.8173261887602,31.1477540551379,6.65235562856574));
#60870=CARTESIAN_POINT('Ctrl Pts',(53.8893516795222,31.1858727484733,6.64813658976719));
#60871=CARTESIAN_POINT('Ctrl Pts',(53.9631233002723,31.2203236159537,6.64391755096865));
#60872=CARTESIAN_POINT('Ctrl Pts',(54.0368708296467,31.2547632329183,6.63969988996888));
#60873=CARTESIAN_POINT('Ctrl Pts',(54.1123629359801,31.2855372063541,6.63548222896912));
#60874=CARTESIAN_POINT('Ctrl Pts',(54.1891994127194,31.3124776015489,6.63126456796936));
#60875=CARTESIAN_POINT('Ctrl Pts',(54.2660342902399,31.3394174360258,6.62704699475293));
#60876=CARTESIAN_POINT('Ctrl Pts',(54.3442130437623,31.362523698306,6.62282942153651));
#60877=CARTESIAN_POINT('Ctrl Pts',(54.4233182479969,31.3816776454648,6.61861184832009));
#60878=CARTESIAN_POINT('Ctrl Pts',(54.5025577137125,31.4008641017023,6.6143871168183));
#60879=CARTESIAN_POINT('Ctrl Pts',(54.5827263223072,31.4160847116326,6.61016238531651));
#60880=CARTESIAN_POINT('Ctrl Pts',(54.6633939314659,31.4272714320047,6.60593765381472));
#60881=CARTESIAN_POINT('Ctrl Pts',(54.7440414166564,31.4384553616506,6.60171397624726));
#60882=CARTESIAN_POINT('Ctrl Pts',(54.8251871872543,31.4456073943768,6.59749029867979));
#60883=CARTESIAN_POINT('Ctrl Pts',(54.9063977799338,31.4487116764533,6.59326662111233));
#60884=CARTESIAN_POINT('Ctrl Pts',(54.9877557165144,31.4518215907634,6.58903528034344));
#60885=CARTESIAN_POINT('Ctrl Pts',(55.0691782443495,31.4508690831215,6.58480393957455));
#60886=CARTESIAN_POINT('Ctrl Pts',(55.1502328912408,31.4458904980374,6.58057259880565));
#60887=CARTESIAN_POINT('Ctrl Pts',(55.2310545156928,31.4409262257913,6.57635342263664));
#60888=CARTESIAN_POINT('Ctrl Pts',(55.3115099283703,31.4319591272632,6.57213424646762));
#60889=CARTESIAN_POINT('Ctrl Pts',(55.3911805236031,31.4190758665147,6.56791507029861));
#60890=CARTESIAN_POINT('Ctrl Pts',(55.4711049550331,31.4061515587787,6.56368245153347));
#60891=CARTESIAN_POINT('Ctrl Pts',(55.5505368141948,31.3892379989933,6.55944983276834));
#60892=CARTESIAN_POINT('Ctrl Pts',(55.629047450847,31.3683854320154,6.55521721400321));
#60893=CARTESIAN_POINT('Ctrl Pts',(55.707446100048,31.347562609107,6.55099063263896));
#60894=CARTESIAN_POINT('Ctrl Pts',(55.7849256913231,31.3228120565172,6.54676405127471));
#60895=CARTESIAN_POINT('Ctrl Pts',(55.8610657867765,31.294235376077,6.54253746991046));
#60896=CARTESIAN_POINT('Ctrl Pts',(55.9371212716691,31.2656904514277,6.53831558532807));
#60897=CARTESIAN_POINT('Ctrl Pts',(56.0118397857047,31.233328009683,6.53409370074568));
#60898=CARTESIAN_POINT('Ctrl Pts',(56.0848155021396,31.1972996100481,6.52987181616329));
#60899=CARTESIAN_POINT('Ctrl Pts',(56.1577420989467,31.1612954609677,6.5256527733125));
#60900=CARTESIAN_POINT('Ctrl Pts',(56.2289278124649,31.1216304597929,6.5214337304617));
#60901=CARTESIAN_POINT('Ctrl Pts',(56.2979874505031,31.0785039880492,6.51721468761091));
#60902=CARTESIAN_POINT('Ctrl Pts',(56.3670245362098,31.0353915998211,6.51299702254395));
#60903=CARTESIAN_POINT('Ctrl Pts',(56.4339365315444,30.9888202317808,6.50877935747699));
#60904=CARTESIAN_POINT('Ctrl Pts',(56.4983646954293,30.9390341640856,6.50456169241003));
#60905=CARTESIAN_POINT('Ctrl Pts',(56.5627915184957,30.8892491324913,6.50034411511716));
#60906=CARTESIAN_POINT('Ctrl Pts',(56.6247342460189,30.8362498192367,6.49612653782428));
#60907=CARTESIAN_POINT('Ctrl Pts',(56.683866026361,30.780321728022,6.4919089605314));
#60908=CARTESIAN_POINT('Ctrl Pts',(56.7430980439055,30.7242988303367,6.48768423381488));
#60909=CARTESIAN_POINT('Ctrl Pts',(56.7995092414239,30.6653375423788,6.48345950709836));
#60910=CARTESIAN_POINT('Ctrl Pts',(56.8528083740854,30.6037616340713,6.47923478038184));
#60911=CARTESIAN_POINT('Ctrl Pts',(56.9060943218714,30.5422009581071,6.47501109875729));
#60912=CARTESIAN_POINT('Ctrl Pts',(56.956269473905,30.4780273355217,6.47078741713273));
#60913=CARTESIAN_POINT('Ctrl Pts',(57.0030845534015,30.411595736011,6.46656373550818));
#60914=CARTESIAN_POINT('Ctrl Pts',(57.0499845709571,30.3450436075769,6.4623323907263));
#60915=CARTESIAN_POINT('Ctrl Pts',(57.0935120837138,30.2762257088127,6.45810104594442));
#60916=CARTESIAN_POINT('Ctrl Pts',(57.1334621396473,30.20552459481,6.45386970116254));
#60917=CARTESIAN_POINT('Ctrl Pts',(57.1732970944237,30.1350271796465,6.44965054741941));
#60918=CARTESIAN_POINT('Ctrl Pts',(57.2095750493838,30.0626578305374,6.44543139367628));
#60919=CARTESIAN_POINT('Ctrl Pts',(57.2421408135098,29.9888148574904,6.44121223993315));
#60920=CARTESIAN_POINT('Ctrl Pts',(57.2748103779279,29.9147365169531,6.43697963803664));
#60921=CARTESIAN_POINT('Ctrl Pts',(57.3038655318623,29.8388996131088,6.43274703614012));
#60922=CARTESIAN_POINT('Ctrl Pts',(57.3291150640083,29.7616910585072,6.42851443424361));
#60923=CARTESIAN_POINT('Ctrl Pts',(57.3543285799335,29.6845926350686,6.42428786977873));
#60924=CARTESIAN_POINT('Ctrl Pts',(57.3757471123381,29.6061268846802,6.42006130531384));
#60925=CARTESIAN_POINT('Ctrl Pts',(57.3932270001455,29.5267017901758,6.41583474084896));
#60926=CARTESIAN_POINT('Ctrl Pts',(57.4106875507256,29.4473645601437,6.41161285204557));
#60927=CARTESIAN_POINT('Ctrl Pts',(57.4242180148205,29.3670705461218,6.40739096324219));
#60928=CARTESIAN_POINT('Ctrl Pts',(57.4337245898435,29.2862426781441,6.40316907443881));
#60929=CARTESIAN_POINT('Ctrl Pts',(57.4432247185924,29.2054696184003,6.39895004843849));
#60930=CARTESIAN_POINT('Ctrl Pts',(57.4487063234812,29.1241638838749,6.39473102243817));
#60931=CARTESIAN_POINT('Ctrl Pts',(57.4501269514733,29.0427571241308,6.39051199643785));
#60932=CARTESIAN_POINT('Ctrl Pts',(57.4515471155577,28.9613769478611,6.38629434816551));
#60933=CARTESIAN_POINT('Ctrl Pts',(57.4489089282322,28.8798962760132,6.38207669989316));
#60934=CARTESIAN_POINT('Ctrl Pts',(57.4422219985723,28.7987490131965,6.37785905162082));
#60935=CARTESIAN_POINT('Ctrl Pts',(57.4355352079506,28.7176034376365,6.37364149104405));
#60936=CARTESIAN_POINT('Ctrl Pts',(57.4247998816956,28.6367917202094,6.36942393046728));
#60937=CARTESIAN_POINT('Ctrl Pts',(57.4100775688688,28.556743457989,6.36520636989052));
#60938=CARTESIAN_POINT('Ctrl Pts',(57.3953301713377,28.4765588050395,6.36098162319695));
#60939=CARTESIAN_POINT('Ctrl Pts',(57.3765822798807,28.3971406692574,6.35675687650338));
#60940=CARTESIAN_POINT('Ctrl Pts',(57.3539469297499,28.3189096227952,6.35253212980982));
#60941=CARTESIAN_POINT('Ctrl Pts',(57.3313173736756,28.2406986014307,6.34830846454068));
#60942=CARTESIAN_POINT('Ctrl Pts',(57.3048025207277,28.1636744955753,6.34408479927155));
#60943=CARTESIAN_POINT('Ctrl Pts',(57.2745644219918,28.0882396475998,6.33986113400242));
#60944=CARTESIAN_POINT('Ctrl Pts',(57.2442714586458,28.0126679291299,6.33562980523069));
#60945=CARTESIAN_POINT('Ctrl Pts',(57.2102419435187,27.9386916545432,6.33139847645896));
#60946=CARTESIAN_POINT('Ctrl Pts',(57.1726851973896,27.86669100284,6.32716714768723));
#60947=CARTESIAN_POINT('Ctrl Pts',(57.135235696081,27.7948959519343,6.32294790164739));
#60948=CARTESIAN_POINT('Ctrl Pts',(57.0942793833322,27.7250656066502,6.31872865560755));
#60949=CARTESIAN_POINT('Ctrl Pts',(57.0500659050149,27.6575470082363,6.31450940956771));
#60950=CARTESIAN_POINT('Ctrl Pts',(57.0057122524442,27.5898143490996,6.31027678684532));
#60951=CARTESIAN_POINT('Ctrl Pts',(56.9579157577534,27.5241562099011,6.30604416412293));
#60952=CARTESIAN_POINT('Ctrl Pts',(56.9068968804013,27.4609436210731,6.30181154140054));
#60953=CARTESIAN_POINT('Ctrl Pts',(56.8559507776077,27.397821200208,6.2975849561934));
#60954=CARTESIAN_POINT('Ctrl Pts',(56.8017917107017,27.3371377598075,6.29335837098627));
#60955=CARTESIAN_POINT('Ctrl Pts',(56.7446836997035,27.2792359144877,6.28913178577912));
#60956=CARTESIAN_POINT('Ctrl Pts',(56.6876392149322,27.2213984784462,6.28490990217175));
#60957=CARTESIAN_POINT('Ctrl Pts',(56.6276526288117,27.1663368182792,6.28068801856439));
#60958=CARTESIAN_POINT('Ctrl Pts',(56.5650276366769,27.1143598576511,6.27646613495702));
#60959=CARTESIAN_POINT('Ctrl Pts',(56.5024447301628,27.0624178268901,6.27224708856505));
#60960=CARTESIAN_POINT('Ctrl Pts',(56.4372272955657,27.0135566745421,6.26802804217309));
#60961=CARTESIAN_POINT('Ctrl Pts',(56.3697143025282,26.9680470036318,6.26380899578113));
#60962=CARTESIAN_POINT('Ctrl Pts',(56.3022233586583,26.9225521957918,6.25959132729372));
#60963=CARTESIAN_POINT('Ctrl Pts',(56.2324387301324,26.8804069551102,6.25537365880631));
#60964=CARTESIAN_POINT('Ctrl Pts',(56.1607296208659,26.8418394412731,6.2511559903189));
#60965=CARTESIAN_POINT('Ctrl Pts',(56.0890220060584,26.803272731205,6.24693840973012));
#60966=CARTESIAN_POINT('Ctrl Pts',(56.0153903999367,26.7682838187407,6.24272082914134));
#60967=CARTESIAN_POINT('Ctrl Pts',(55.9402286694053,26.7370549500201,6.23850324855256));
#60968=CARTESIAN_POINT('Ctrl Pts',(55.8649396634547,26.7057731997689,6.2342785261067));
#60969=CARTESIAN_POINT('Ctrl Pts',(55.788115780296,26.6782644114158,6.23005380366084));
#60970=CARTESIAN_POINT('Ctrl Pts',(55.7101713327564,26.6546627261456,6.22582908121498));
#60971=CARTESIAN_POINT('Ctrl Pts',(55.6322460333196,26.631066838947,6.22160539662906));
#60972=CARTESIAN_POINT('Ctrl Pts',(55.5532011774512,26.6113762274964,6.21738171204314));
#60973=CARTESIAN_POINT('Ctrl Pts',(55.4734624837417,26.5956739974602,6.21315802745723));
#60974=CARTESIAN_POINT('Ctrl Pts',(55.393579121926,26.5799432792236,6.20892667993601));
#60975=CARTESIAN_POINT('Ctrl Pts',(55.3129998676101,26.5682154704624,6.2046953324148));
#60976=CARTESIAN_POINT('Ctrl Pts',(55.2321575821357,26.56052196012,6.20046398489359));
#60977=CARTESIAN_POINT('Ctrl Pts',(55.1515486193776,26.552850654379,6.19624484966314));
#60978=CARTESIAN_POINT('Ctrl Pts',(55.0706786002372,26.5491903285429,6.19202571443269));
#60979=CARTESIAN_POINT('Ctrl Pts',(54.9899745035598,26.5495205082635,6.18780657920225));
#60980=CARTESIAN_POINT('Ctrl Pts',(54.9090120275628,26.5498517450756,6.18357393614091));
#60981=CARTESIAN_POINT('Ctrl Pts',(54.8279154383746,26.554200339424,6.17934129307957));
#60982=CARTESIAN_POINT('Ctrl Pts',(54.7471159881272,26.5625833498273,6.17510865001823));
#60983=CARTESIAN_POINT('Ctrl Pts',(54.6664317859521,26.570954403147,6.17088204417561));
#60984=CARTESIAN_POINT('Ctrl Pts',(54.586044339172,26.5833483958408,6.16665543833299));
#60985=CARTESIAN_POINT('Ctrl Pts',(54.5063847778751,26.5997303771271,6.16242883249037));
#60986=CARTESIAN_POINT('Ctrl Pts',(54.426814313883,26.616094035561,6.1582069540048));
#60987=CARTESIAN_POINT('Ctrl Pts',(54.3479705703504,26.6364367260928,6.15398507551924));
#60988=CARTESIAN_POINT('Ctrl Pts',(54.270278007529,26.660671877717,6.14976319703367));
#60989=CARTESIAN_POINT('Ctrl Pts',(54.192637171885,26.6848908937428,6.14554412944595));
#60990=CARTESIAN_POINT('Ctrl Pts',(54.1161464371773,26.712997086288,6.14132506185822));
#60991=CARTESIAN_POINT('Ctrl Pts',(54.041217330246,26.7448534322179,6.1371059942705));
#60992=CARTESIAN_POINT('Ctrl Pts',(53.9663126915176,26.7766993754142,6.1328883044251));
#60993=CARTESIAN_POINT('Ctrl Pts',(53.8929690950125,26.8122928583612,6.12867061457969));
#60994=CARTESIAN_POINT('Ctrl Pts',(53.8215789243146,26.8514483905709,6.12445292473428));
#60995=CARTESIAN_POINT('Ctrl Pts',(53.7501902391895,26.890603107985,6.12023532265566));
#60996=CARTESIAN_POINT('Ctrl Pts',(53.6807553057858,26.9333195028628,6.11601772057704));
#60997=CARTESIAN_POINT('Ctrl Pts',(53.6136414206032,26.9793664015134,6.11180011849842));
#60998=CARTESIAN_POINT('Ctrl Pts',(53.5464146278028,27.025490766185,6.10757542102661));
#60999=CARTESIAN_POINT('Ctrl Pts',(53.4815170806266,27.0749565805098,6.10335072355481));
#61000=CARTESIAN_POINT('Ctrl Pts',(53.4192868435943,27.1274893412411,6.09912602608301));
#61001=CARTESIAN_POINT('Ctrl Pts',(53.3570712084832,27.1800097755009,6.09490231990905));
#61002=CARTESIAN_POINT('Ctrl Pts',(53.297521958275,27.2355953835484,6.09067861373509));
#61003=CARTESIAN_POINT('Ctrl Pts',(53.2409405682616,27.2939343020821,6.08645490756113));
#61004=CARTESIAN_POINT('Ctrl Pts',(53.1842565259842,27.3523790614596,6.08222353856728));
#61005=CARTESIAN_POINT('Ctrl Pts',(53.13055141174,27.4135867638002,6.07799216957343));
#61006=CARTESIAN_POINT('Ctrl Pts',(53.080087208073,27.4772113996372,6.07376080057958));
#61007=CARTESIAN_POINT('Ctrl Pts',(53.0297703139504,27.5406503094458,6.06954178333199));
#61008=CARTESIAN_POINT('Ctrl Pts',(52.9826756319443,27.6064916426494,6.06532276608439));
#61009=CARTESIAN_POINT('Ctrl Pts',(52.9390184174073,27.6743661266346,6.0611037488368));
#61010=CARTESIAN_POINT('Ctrl Pts',(52.8942488691094,27.7439699715248,6.05677723606133));
#61011=CARTESIAN_POINT('Ctrl Pts',(52.8529333346666,27.8159616604484,6.05245072328586));
#61012=CARTESIAN_POINT('Ctrl Pts',(52.8153283562073,27.8899729468124,6.04812421051039));
#61013=CARTESIAN_POINT('Ctrl Pts',(52.7777843730217,27.963864186873,6.04380471533846));
#61014=CARTESIAN_POINT('Ctrl Pts',(52.7439391787127,28.0397681264347,6.03948522016654));
#61015=CARTESIAN_POINT('Ctrl Pts',(52.7140055440341,28.1172884971333,6.03516572499462));
#61016=CARTESIAN_POINT('Ctrl Pts',(52.6841225849363,28.1946776311863,6.03085354243036));
#61017=CARTESIAN_POINT('Ctrl Pts',(52.6581381619751,28.2736773444822,6.0265413598661));
#61018=CARTESIAN_POINT('Ctrl Pts',(52.636218034592,28.353869154109,6.02222917730185));
#61019=CARTESIAN_POINT('Ctrl Pts',(52.614319784242,28.4339809295804,6.01792129844256));
#61020=CARTESIAN_POINT('Ctrl Pts',(52.5964778819453,28.5152820169277,6.01361341958326));
#61021=CARTESIAN_POINT('Ctrl Pts',(52.5828089271904,28.5973369056775,6.00930554072397));
#61022=CARTESIAN_POINT('Ctrl Pts',(52.5691514667886,28.6793227936964,6.0050012844007));
#61023=CARTESIAN_POINT('Ctrl Pts',(52.5596600446458,28.7620607920093,6.00069702807742));
#61024=CARTESIAN_POINT('Ctrl Pts',(52.5544003556719,28.845104455641,5.99639277175415));
#61025=CARTESIAN_POINT('Ctrl Pts',(52.5511151702141,28.8969732709803,5.99370434657345));
#61026=CARTESIAN_POINT('Ctrl Pts',(52.549479860527,28.9489611166896,5.99101592139276));
#61027=CARTESIAN_POINT('Ctrl Pts',(52.5495001872428,29.0009579546612,5.98832749621206));
#61028=CARTESIAN_POINT('Ctrl Pts',(52.5495001872432,29.0009579555037,5.9883274961685));
#61029=CARTESIAN_POINT('Ctrl Pts',(52.5495348804631,29.0897050095589,5.98373895147723));
#61030=CARTESIAN_POINT('Ctrl Pts',(52.5543948630893,29.1783029161916,5.97915040678597));
#61031=CARTESIAN_POINT('Ctrl Pts',(52.5640065805463,29.2662448316463,5.97456186209471));
#61032=CARTESIAN_POINT('Ctrl Pts',(52.5736441829486,29.354423580079,5.96996096017084));
#61033=CARTESIAN_POINT('Ctrl Pts',(52.5880590237614,29.4419424892432,5.96536005824698));
#61034=CARTESIAN_POINT('Ctrl Pts',(52.6071265666039,29.5283057653925,5.96075915632312));
#61035=CARTESIAN_POINT('Ctrl Pts',(52.6262757077358,29.6150386274747,5.95613856514353));
#61036=CARTESIAN_POINT('Ctrl Pts',(52.6501173215307,29.700605641685,5.95151797396394));
#61037=CARTESIAN_POINT('Ctrl Pts',(52.6784764616596,29.7845245126389,5.94689738278434));
#61038=CARTESIAN_POINT('Ctrl Pts',(52.7040423808818,29.8601778316844,5.94273189468001));
#61039=CARTESIAN_POINT('Ctrl Pts',(52.7332790280157,29.9344918007638,5.93856640657567));
#61040=CARTESIAN_POINT('Ctrl Pts',(52.7660259964594,30.0071297838435,5.93440091847134));
#61041=CARTESIAN_POINT('Ctrl Pts',(52.7993013887138,30.0809398949598,5.9301682136687));
#61042=CARTESIAN_POINT('Ctrl Pts',(52.8363005913983,30.1532363580626,5.92593550886607));
#61043=CARTESIAN_POINT('Ctrl Pts',(52.8768635501333,30.2236183495059,5.92170280406344));
#61044=CARTESIAN_POINT('Ctrl Pts',(52.9173686453212,30.2938999401942,5.91747613726498));
#61045=CARTESIAN_POINT('Ctrl Pts',(52.9614271695572,30.3622720842524,5.91324947046653));
#61046=CARTESIAN_POINT('Ctrl Pts',(53.0088316173746,30.4283552506408,5.90902280366807));
#61047=CARTESIAN_POINT('Ctrl Pts',(53.0561821895524,30.4943633128349,5.90480094051965));
#61048=CARTESIAN_POINT('Ctrl Pts',(53.1068708588622,30.5580871916842,5.90057907737122));
#61049=CARTESIAN_POINT('Ctrl Pts',(53.1606457045262,30.6191744889672,5.8963572142228));
#61050=CARTESIAN_POINT('Ctrl Pts',(53.2143856893116,30.6802221848933,5.89213808800196));
#61051=CARTESIAN_POINT('Ctrl Pts',(53.2712075719737,30.7386363451589,5.88791896178113));
#61052=CARTESIAN_POINT('Ctrl Pts',(53.3308186070495,30.7940969113813,5.8836998355603));
#61053=CARTESIAN_POINT('Ctrl Pts',(53.3904101622112,30.8495393539951,5.87948208808111));
#61054=CARTESIAN_POINT('Ctrl Pts',(53.4527887198652,30.9020298031947,5.87526434060193));
#61055=CARTESIAN_POINT('Ctrl Pts',(53.5176250644263,30.9512854225825,5.87104659312274));
#61056=CARTESIAN_POINT('Ctrl Pts',(53.5824600433415,31.0005400045007,5.86682893448183));
#61057=CARTESIAN_POINT('Ctrl Pts',(53.6497523356319,31.046559612006,5.86261127584092));
#61058=CARTESIAN_POINT('Ctrl Pts',(53.71914121885,31.0891029253608,5.85839361720001));
#61059=CARTESIAN_POINT('Ctrl Pts',(53.7886447524352,31.1317165324899,5.8541689897755));
#61060=CARTESIAN_POINT('Ctrl Pts',(53.8602514094746,31.1708421100769,5.84994436235099));
#61061=CARTESIAN_POINT('Ctrl Pts',(53.9335728330193,31.2062826989136,5.84571973492648));
#61062=CARTESIAN_POINT('Ctrl Pts',(54.0068791943299,31.24171600728,5.84149597535647));
#61063=CARTESIAN_POINT('Ctrl Pts',(54.0818991803267,31.2734656782613,5.83727221578646));
#61064=CARTESIAN_POINT('Ctrl Pts',(54.1582251784986,31.3013833665616,5.83304845621645));
#61065=CARTESIAN_POINT('Ctrl Pts',(54.2346896069915,31.3293516883897,5.82881703613224));
#61066=CARTESIAN_POINT('Ctrl Pts',(54.3124643364177,31.3534740002599,5.82458561604803));
#61067=CARTESIAN_POINT('Ctrl Pts',(54.3911266505643,31.3736519320126,5.82035419596382));
#61068=CARTESIAN_POINT('Ctrl Pts',(54.4695525463929,31.3937692193164,5.81613549334452));
#61069=CARTESIAN_POINT('Ctrl Pts',(54.5488602366159,31.409965794223,5.81191679072521));
#61070=CARTESIAN_POINT('Ctrl Pts',(54.6286248968841,31.4221954468593,5.8076980881059));
#61071=CARTESIAN_POINT('Ctrl Pts',(54.7086557912035,31.4344659189505,5.80346530453539));
#61072=CARTESIAN_POINT('Ctrl Pts',(54.7894442047976,31.442788526944,5.79923252096488));
#61073=CARTESIAN_POINT('Ctrl Pts',(54.8705667614793,31.4470793380612,5.79499973739437));
#61074=CARTESIAN_POINT('Ctrl Pts',(54.9515736403356,31.4513640306373,5.79077298961981));
#61075=CARTESIAN_POINT('Ctrl Pts',(55.0329132559281,31.4516283206803,5.78654624184525));
#61076=CARTESIAN_POINT('Ctrl Pts',(55.1141542634911,31.4478396708377,5.78231949407068));
#61077=CARTESIAN_POINT('Ctrl Pts',(55.1953017187549,31.4440553837783,5.77809761356678));
#61078=CARTESIAN_POINT('Ctrl Pts',(55.2763503300436,31.4362274541488,5.77387573306287));
#61079=CARTESIAN_POINT('Ctrl Pts',(55.3568673555319,31.4243753712154,5.76965385255896));
#61080=CARTESIAN_POINT('Ctrl Pts',(55.4373334866782,31.4125307799145,5.76543464068109));
#61081=CARTESIAN_POINT('Ctrl Pts',(55.5172682407257,31.3966671521891,5.76121542880322));
#61082=CARTESIAN_POINT('Ctrl Pts',(55.5962437602841,31.3768558282576,5.75699621692535));
#61083=CARTESIAN_POINT('Ctrl Pts',(55.6751935019768,31.3570509708066,5.75277838221191));
#61084=CARTESIAN_POINT('Ctrl Pts',(55.7531841807739,31.3333010890549,5.74856054749848));
#61085=CARTESIAN_POINT('Ctrl Pts',(55.8297993097425,31.3057283785283,5.74434271278505));
#61086=CARTESIAN_POINT('Ctrl Pts',(55.9064128512869,31.2781562392935,5.74012496546289));
#61087=CARTESIAN_POINT('Ctrl Pts',(55.9816504630053,31.2467615871665,5.73590721814072));
#61088=CARTESIAN_POINT('Ctrl Pts',(56.055113332537,31.211715647524,5.73168947081855));
#61089=CARTESIAN_POINT('Ctrl Pts',(56.1286941265191,31.1766134512557,5.72746495306204));
#61090=CARTESIAN_POINT('Ctrl Pts',(56.2004940578778,31.1378484432521,5.72324043530553));
#61091=CARTESIAN_POINT('Ctrl Pts',(56.2701365348185,31.0956391466374,5.71901591754902));
#61092=CARTESIAN_POINT('Ctrl Pts',(56.3397680171007,31.0534365137261,5.71479206672931));
#61093=CARTESIAN_POINT('Ctrl Pts',(56.4072423515412,31.0077909577052,5.7105682159096));
#61094=CARTESIAN_POINT('Ctrl Pts',(56.4722131888498,30.9589636486104,5.70634436508989));
#61095=CARTESIAN_POINT('Ctrl Pts',(56.5373018712743,30.9100477757823,5.70211285298382));
#61096=CARTESIAN_POINT('Ctrl Pts',(56.5998776237771,30.8579389146044,5.69788134087774));
#61097=CARTESIAN_POINT('Ctrl Pts',(56.6596277954745,30.8029381105541,5.69364982877167));
#61098=CARTESIAN_POINT('Ctrl Pts',(56.7191898600446,30.7481104615418,5.68943163842792));
#61099=CARTESIAN_POINT('Ctrl Pts',(56.7759438507384,30.6904094356497,5.68521344808418));
#61100=CARTESIAN_POINT('Ctrl Pts',(56.8296198357287,30.6301660978895,5.68099525774043));
#61101=CARTESIAN_POINT('Ctrl Pts',(56.8834703391349,30.5697268890729,5.67676335266193));
#61102=CARTESIAN_POINT('Ctrl Pts',(56.9344231637771,30.5065038715945,5.67253144758343));
#61103=CARTESIAN_POINT('Ctrl Pts',(56.9821774481714,30.4408063068853,5.66829954250492));
#61104=CARTESIAN_POINT('Ctrl Pts',(57.0298635899893,30.3752024887663,5.66407367610795));
#61105=CARTESIAN_POINT('Ctrl Pts',(57.0743599854588,30.3071315092119,5.65984780971098));
#61106=CARTESIAN_POINT('Ctrl Pts',(57.1154045371144,30.236937304133,5.65562194331401));
#61107=CARTESIAN_POINT('Ctrl Pts',(57.1564121491291,30.1668062730595,5.65139988014988));
#61108=CARTESIAN_POINT('Ctrl Pts',(57.1939738470693,30.0945562067714,5.64717781698576));
#61109=CARTESIAN_POINT('Ctrl Pts',(57.2278702471078,30.0205608321172,5.64295575382163));
#61110=CARTESIAN_POINT('Ctrl Pts',(57.2617366757566,29.9466308845941,5.63873742382978));
#61111=CARTESIAN_POINT('Ctrl Pts',(57.2919440611223,29.870959120572,5.63451909383792));
#61112=CARTESIAN_POINT('Ctrl Pts',(57.3183193406169,29.793943124488,5.63030076384607));
#61113=CARTESIAN_POINT('Ctrl Pts',(57.3446860203039,29.7169522399008,5.62608380926432));
#61114=CARTESIAN_POINT('Ctrl Pts',(57.3672229250302,29.6386184329849,5.62186685468258));
#61115=CARTESIAN_POINT('Ctrl Pts',(57.3858058396285,29.5593574399207,5.61764990010084));
#61116=CARTESIAN_POINT('Ctrl Pts',(57.4043883820968,29.4800980340881,5.61343302996522));
#61117=CARTESIAN_POINT('Ctrl Pts',(57.419016986936,29.3999119317448,5.6092161598296));
#61118=CARTESIAN_POINT('Ctrl Pts',(57.4296181882844,29.319226736283,5.60499928969398));
#61119=CARTESIAN_POINT('Ctrl Pts',(57.4402412657466,29.2383750428492,5.60077371783407));
#61120=CARTESIAN_POINT('Ctrl Pts',(57.4468202434313,29.1570226586364,5.59654814597415));
#61121=CARTESIAN_POINT('Ctrl Pts',(57.44933340943,29.0756048903831,5.59232257411424));
#61122=CARTESIAN_POINT('Ctrl Pts',(57.4518450397081,28.9942368740935,5.58809958437494));
#61123=CARTESIAN_POINT('Ctrl Pts',(57.4502958591789,28.9128040196171,5.58387659463564));
#61124=CARTESIAN_POINT('Ctrl Pts',(57.44471643472,28.8317388820619,5.57965360489633));
#61125=CARTESIAN_POINT('Ctrl Pts',(57.4391268663778,28.7505263609714,5.57542293739102));
#61126=CARTESIAN_POINT('Ctrl Pts',(57.4294924658969,28.6696833556457,5.57119226988571));
#61127=CARTESIAN_POINT('Ctrl Pts',(57.4158955933696,28.5896358544689,5.5669616023804));
#61128=CARTESIAN_POINT('Ctrl Pts',(57.4023231758288,28.5097323246766,5.56273854404527));
#61129=CARTESIAN_POINT('Ctrl Pts',(57.3848027010076,28.4306218705929,5.55851548571013));
#61130=CARTESIAN_POINT('Ctrl Pts',(57.3634655259986,28.3527126160536,5.55429242737499));
#61131=CARTESIAN_POINT('Ctrl Pts',(57.3420757069462,28.2746111402772,5.5500589497193));
#61132=CARTESIAN_POINT('Ctrl Pts',(57.3167706850182,28.1974260423424,5.5458254720636));
#61133=CARTESIAN_POINT('Ctrl Pts',(57.2876462846144,28.121578275263,5.54159199440791));
#61134=CARTESIAN_POINT('Ctrl Pts',(57.2585634435399,28.0458387398479,5.53736455775184));
#61135=CARTESIAN_POINT('Ctrl Pts',(57.2256722137725,27.9714331749786,5.53313712109577));
#61136=CARTESIAN_POINT('Ctrl Pts',(57.1891186039552,27.8987688762948,5.5289096844397));
#61137=CARTESIAN_POINT('Ctrl Pts',(57.15260717494,27.8261884281094,5.52468712600687));
#61138=CARTESIAN_POINT('Ctrl Pts',(57.1124419730094,27.7553456652756,5.52046456757404));
#61139=CARTESIAN_POINT('Ctrl Pts',(57.0688170908201,27.6866279678892,5.51624200914121));
#61140=CARTESIAN_POINT('Ctrl Pts',(57.0252198507741,27.6179538122696,5.51202212625866));
#61141=CARTESIAN_POINT('Ctrl Pts',(56.9781675304111,27.5514024400632,5.50780224337611));
#61142=CARTESIAN_POINT('Ctrl Pts',(56.9278995891057,27.4873356537797,5.50358236049356));
#61143=CARTESIAN_POINT('Ctrl Pts',(56.8776481454277,27.4232898938192,5.49936386255047));
#61144=CARTESIAN_POINT('Ctrl Pts',(56.8241834631045,27.3617274654113,5.49514536460738));
#61145=CARTESIAN_POINT('Ctrl Pts',(56.7677868187332,27.3029790768782,5.49092686666429));
#61146=CARTESIAN_POINT('Ctrl Pts',(56.7113914580959,27.2442320256109,5.48670846474516));
#61147=CARTESIAN_POINT('Ctrl Pts',(56.652064590513,27.188299221033,5.48249006282603));
#61148=CARTESIAN_POINT('Ctrl Pts',(56.5901250769412,27.135475264395,5.47827166090691));
#61149=CARTESIAN_POINT('Ctrl Pts',(56.5281106291953,27.0825874015471,5.47404815558213));
#61150=CARTESIAN_POINT('Ctrl Pts',(56.4634775713136,27.0328162076375,5.46982465025735));
#61151=CARTESIAN_POINT('Ctrl Pts',(56.3965784963801,26.986416439914,5.46560114493257));
#61152=CARTESIAN_POINT('Ctrl Pts',(56.3296640223232,26.9400059916878,5.46137666742276));
#61153=CARTESIAN_POINT('Ctrl Pts',(56.2604828922113,26.8969687536104,5.45715218991294));
#61154=CARTESIAN_POINT('Ctrl Pts',(56.1894147494465,26.8575148066325,5.45292771240313));
#61155=CARTESIAN_POINT('Ctrl Pts',(56.1182180905243,26.8179895130642,5.44869559555457));
#61156=CARTESIAN_POINT('Ctrl Pts',(56.0451280173098,26.7820606658857,5.444463478706));
#61157=CARTESIAN_POINT('Ctrl Pts',(55.9705468772094,26.7498913339265,5.44023136185744));
#61158=CARTESIAN_POINT('Ctrl Pts',(55.8962863854371,26.7178603082803,5.43601744024147));
#61159=CARTESIAN_POINT('Ctrl Pts',(55.8205480775728,26.6895566078653,5.4318035186255));
#61160=CARTESIAN_POINT('Ctrl Pts',(55.7437429055251,26.6650917061946,5.42758959700954));
#61161=CARTESIAN_POINT('Ctrl Pts',(55.6665809343043,26.6405131525855,5.42335609957976));
#61162=CARTESIAN_POINT('Ctrl Pts',(55.5880563758273,26.6197181557584,5.41912260214997));
#61163=CARTESIAN_POINT('Ctrl Pts',(55.5085745716469,26.6028554163184,5.41488910472019));
#61164=CARTESIAN_POINT('Ctrl Pts',(55.4292058827146,26.5860166752384,5.41066163223054));
#61165=CARTESIAN_POINT('Ctrl Pts',(55.3488831043022,26.5730991721212,5.4064341597409));
#61166=CARTESIAN_POINT('Ctrl Pts',(55.2680274277603,26.5642020716061,5.40220668725125));
#61167=CARTESIAN_POINT('Ctrl Pts',(55.1872645983554,26.5553151876935,5.39798406919772));
#61168=CARTESIAN_POINT('Ctrl Pts',(55.1059705462059,26.5504395813525,5.39376145114421));
#61169=CARTESIAN_POINT('Ctrl Pts',(55.0245759219857,26.5496232383451,5.38953883309069));
#61170=CARTESIAN_POINT('Ctrl Pts',(54.9432325944776,26.5488074098153,5.38531887622548));
#61171=CARTESIAN_POINT('Ctrl Pts',(54.8617892837758,26.5520457708118,5.38109891936026));
#61172=CARTESIAN_POINT('Ctrl Pts',(54.7806798685637,26.5593343264702,5.37687896249505));
#61173=CARTESIAN_POINT('Ctrl Pts',(54.6995968008861,26.5666205145185,5.37266037643814));
#61174=CARTESIAN_POINT('Ctrl Pts',(54.6188478753948,26.577954242836,5.36844179038123));
#61175=CARTESIAN_POINT('Ctrl Pts',(54.5388636393897,26.5932795120906,5.36422320432431));
#61176=CARTESIAN_POINT('Ctrl Pts',(54.4588809601898,26.6086044830556,5.36000470037754));
#61177=CARTESIAN_POINT('Ctrl Pts',(54.3796633966782,26.6279207519469,5.35578619643076));
#61178=CARTESIAN_POINT('Ctrl Pts',(54.3016316561382,26.6511211384382,5.35156769248399));
#61179=CARTESIAN_POINT('Ctrl Pts',(54.2235091569189,26.6743485092878,5.34734428199733));
#61180=CARTESIAN_POINT('Ctrl Pts',(54.146575683951,26.7014688949003,5.34312087151067));
#61181=CARTESIAN_POINT('Ctrl Pts',(54.0712368133841,26.7323251570855,5.33889746102401));
#61182=CARTESIAN_POINT('Ctrl Pts',(53.9958765090544,26.7631901978176,5.33467284898524));
#61183=CARTESIAN_POINT('Ctrl Pts',(53.9221121290926,26.7977930283744,5.33044823694648));
#61184=CARTESIAN_POINT('Ctrl Pts',(53.8503265516765,26.8359294807655,5.32622362490771));
#61185=CARTESIAN_POINT('Ctrl Pts',(53.7784108564861,26.8741350588847,5.32199135538208));
#61186=CARTESIAN_POINT('Ctrl Pts',(53.7084815316927,26.9158868203423,5.31775908585645));
#61187=CARTESIAN_POINT('Ctrl Pts',(53.6408943715873,26.9609359645129,5.31352681633082));
#61188=CARTESIAN_POINT('Ctrl Pts',(53.5736093482096,27.005783724264,5.30931346643524));
#61189=CARTESIAN_POINT('Ctrl Pts',(53.5086458998363,27.0538991039601,5.30510011653967));
#61190=CARTESIAN_POINT('Ctrl Pts',(53.4463210542274,27.1049981573985,5.30088676664409));
#61191=CARTESIAN_POINT('Ctrl Pts',(53.3846040832502,27.1555988250329,5.29671451092999));
#61192=CARTESIAN_POINT('Ctrl Pts',(53.3252305756237,27.2093254374529,5.29254225521589));
#61193=CARTESIAN_POINT('Ctrl Pts',(53.2685409160821,27.2659297330505,5.2883699995018));
#61194=CARTESIAN_POINT('Ctrl Pts',(53.2119031338706,27.3224822294356,5.28420156186472));
#61195=CARTESIAN_POINT('Ctrl Pts',(53.1579446829156,27.3819068699599,5.28003312422765));
#61196=CARTESIAN_POINT('Ctrl Pts',(53.1069740353159,27.4439142224698,5.27586468659057));
#61197=CARTESIAN_POINT('Ctrl Pts',(53.0560883838579,27.5058181745725,5.27170320003482));
#61198=CARTESIAN_POINT('Ctrl Pts',(53.0081809220524,27.5702958977824,5.26754171347906));
#61199=CARTESIAN_POINT('Ctrl Pts',(52.9635221819285,27.6370222501806,5.2633802269233));
#61200=CARTESIAN_POINT('Ctrl Pts',(52.9188903880555,27.7037083411422,5.25922125133092));
#61201=CARTESIAN_POINT('Ctrl Pts',(52.877503692765,27.7726399724987,5.25506227573853));
#61202=CARTESIAN_POINT('Ctrl Pts',(52.8395909509523,27.843460769886,5.25090330014614));
#61203=CARTESIAN_POINT('Ctrl Pts',(52.8016887096749,27.9142619523298,5.24674547644802));
#61204=CARTESIAN_POINT('Ctrl Pts',(52.7672587371688,27.9869508397116,5.24258765274991));
#61205=CARTESIAN_POINT('Ctrl Pts',(52.7364844969214,28.0611454759534,5.23842982905179));
#61206=CARTESIAN_POINT('Ctrl Pts',(52.7055816869476,28.1356500852116,5.23425463464848));
#61207=CARTESIAN_POINT('Ctrl Pts',(52.6783654327688,28.2116726133079,5.23007944024517));
#61208=CARTESIAN_POINT('Ctrl Pts',(52.6549724545473,28.2888065937679,5.22590424584186));
#61209=CARTESIAN_POINT('Ctrl Pts',(52.6316551638009,28.3656910089022,5.22174256018975));
#61210=CARTESIAN_POINT('Ctrl Pts',(52.6121365308147,28.4436792188454,5.21758087453763));
#61211=CARTESIAN_POINT('Ctrl Pts',(52.5965011928653,28.5223560592845,5.21341918888552));
#61212=CARTESIAN_POINT('Ctrl Pts',(52.5807897269088,28.6014159749789,5.2092372401066));
#61213=CARTESIAN_POINT('Ctrl Pts',(52.5689995442004,28.6811707622526,5.2050552913277));
#61214=CARTESIAN_POINT('Ctrl Pts',(52.5611638549431,28.761193577214,5.20087334254879));
#61215=CARTESIAN_POINT('Ctrl Pts',(52.5533281656857,28.8412163921755,5.19669139376987));
#61216=CARTESIAN_POINT('Ctrl Pts',(52.5494469351108,28.9215067478683,5.19250944499096));
#61217=CARTESIAN_POINT('Ctrl Pts',(52.5495005484666,29.0016395226469,5.18832749621205));
#61218=CARTESIAN_POINT('Origin',(55.,29.,3.45145488139523));
#61219=CARTESIAN_POINT('',(53.1796208058588,29.8156268460748,23.7995000000001));
#61220=CARTESIAN_POINT('Ctrl Pts',(53.0466869607994,29.4044696940301,23.0258937941419));
#61221=CARTESIAN_POINT('Ctrl Pts',(53.0269937965999,29.3093651287642,23.0326584916325));
#61222=CARTESIAN_POINT('Ctrl Pts',(53.0142625475846,29.21290049674,23.0393919029704));
#61223=CARTESIAN_POINT('Ctrl Pts',(53.0077245142915,29.1005080488077,23.0468431679078));
#61224=CARTESIAN_POINT('Ctrl Pts',(53.0070096342023,29.08516404734,23.047851829735));
#61225=CARTESIAN_POINT('Ctrl Pts',(53.0062705156584,29.0640582609184,23.0492260649345));
#61226=CARTESIAN_POINT('Ctrl Pts',(53.0060939086745,29.0583028169952,23.0495994647139));
#61227=CARTESIAN_POINT('Ctrl Pts',(53.0058343146134,29.0484516465045,23.0502361882818));
#61228=CARTESIAN_POINT('Ctrl Pts',(53.0057390190016,29.0443563211459,23.0505001779298));
#61229=CARTESIAN_POINT('Ctrl Pts',(53.0055672213574,29.0358461944791,23.0510472377948));
#61230=CARTESIAN_POINT('Ctrl Pts',(53.0054927613474,29.0314314097092,23.0513301832163));
#61231=CARTESIAN_POINT('Ctrl Pts',(53.0053480779659,29.0207497161521,23.0520127872558));
#61232=CARTESIAN_POINT('Ctrl Pts',(53.0052927287307,29.0144825850596,23.0524116274026));
#61233=CARTESIAN_POINT('Ctrl Pts',(53.0052021000396,28.992477019324,23.0538065749029));
#61234=CARTESIAN_POINT('Ctrl Pts',(53.0053235413239,28.9767380484583,23.0547944262847));
#61235=CARTESIAN_POINT('Ctrl Pts',(53.0072294407947,28.8792708253711,23.0608599701355));
#61236=CARTESIAN_POINT('Ctrl Pts',(53.0138504254682,28.7977057763332,23.0657111526208));
#61237=CARTESIAN_POINT('Ctrl Pts',(53.0284238550768,28.6961073179405,23.0717176928971));
#61238=CARTESIAN_POINT('Ctrl Pts',(53.0317117769336,28.6754930727361,23.0729344098968));
#61239=CARTESIAN_POINT('Ctrl Pts',(53.0634162678052,28.4949794853208,23.0835974444499));
#61240=CARTESIAN_POINT('Ctrl Pts',(53.110933483601,28.3390733782184,23.0929288342571));
#61241=CARTESIAN_POINT('Ctrl Pts',(53.1853969964351,28.171332104408,23.104242425343));
#61242=CARTESIAN_POINT('Ctrl Pts',(53.1942814473479,28.1521468299178,23.105555364071));
#61243=CARTESIAN_POINT('Ctrl Pts',(53.2084123863968,28.1228621667007,23.1075906217099));
#61244=CARTESIAN_POINT('Ctrl Pts',(53.2134433262879,28.1126600432109,23.1083055677231));
#61245=CARTESIAN_POINT('Ctrl Pts',(53.2217855759446,28.0961015639035,23.1094758719722));
#61246=CARTESIAN_POINT('Ctrl Pts',(53.2250444165549,28.0897189470692,23.1099294012262));
#61247=CARTESIAN_POINT('Ctrl Pts',(53.2319649715542,28.0763431305161,23.1108850256121));
#61248=CARTESIAN_POINT('Ctrl Pts',(53.2356339379979,28.0693538423847,23.111387368638));
#61249=CARTESIAN_POINT('Ctrl Pts',(53.2445224864398,28.0526628758661,23.1125943046141));
#61250=CARTESIAN_POINT('Ctrl Pts',(53.2497810989011,28.0429823838635,23.1133002642427));
#61251=CARTESIAN_POINT('Ctrl Pts',(53.2681715927985,28.0097862072837,23.1157420511611));
#61252=CARTESIAN_POINT('Ctrl Pts',(53.2816989131776,27.98649408225,23.117491853158));
#61253=CARTESIAN_POINT('Ctrl Pts',(53.3155064269025,27.9309055810656,23.1217591266877));
#61254=CARTESIAN_POINT('Ctrl Pts',(53.3362485980348,27.8989039857857,23.1242924895472));
#61255=CARTESIAN_POINT('Ctrl Pts',(53.4216929830226,27.775009081462,23.1344084990309));
#61256=CARTESIAN_POINT('Ctrl Pts',(53.4931887835824,27.6880660864639,23.1422137902668));
#61257=CARTESIAN_POINT('Ctrl Pts',(53.6473467165213,27.5299224298756,23.1576074858563));
#61258=CARTESIAN_POINT('Ctrl Pts',(53.7292996110698,27.4585318490359,23.1651655992862));
#61259=CARTESIAN_POINT('Ctrl Pts',(53.8295922485481,27.3846265671882,23.1734194324104));
#61260=CARTESIAN_POINT('Ctrl Pts',(53.8426399155792,27.3752528485534,23.174475171916));
#61261=CARTESIAN_POINT('Ctrl Pts',(53.861127967449,27.3623063885016,23.1759443698658));
#61262=CARTESIAN_POINT('Ctrl Pts',(53.8664743567736,27.3586013614416,23.1763661392876));
#61263=CARTESIAN_POINT('Ctrl Pts',(53.8751523361516,27.3526501773608,23.1770456192352));
#61264=CARTESIAN_POINT('Ctrl Pts',(53.8784727030794,27.3503878552904,23.1773043996749));
#61265=CARTESIAN_POINT('Ctrl Pts',(53.8855193801861,27.3456177332947,23.1778510190905));
#61266=CARTESIAN_POINT('Ctrl Pts',(53.8892473727873,27.3431124545434,23.1781386836943));
#61267=CARTESIAN_POINT('Ctrl Pts',(53.8985088657935,27.3369338691558,23.178849656092));
#61268=CARTESIAN_POINT('Ctrl Pts',(53.9040523658649,27.3332755295128,23.1792719759884));
#61269=CARTESIAN_POINT('Ctrl Pts',(53.9248696230127,27.3196862975788,23.1808462374057));
#61270=CARTESIAN_POINT('Ctrl Pts',(53.9402614664818,27.3099367580645,23.1819868582589));
#61271=CARTESIAN_POINT('Ctrl Pts',(53.9795955272188,27.2857703779029,23.1848488145544));
#61272=CARTESIAN_POINT('Ctrl Pts',(54.0037116932348,27.2716429037138,23.1865548134304));
#61273=CARTESIAN_POINT('Ctrl Pts',(54.1153955260518,27.209332257933,23.1942723266549));
#61274=CARTESIAN_POINT('Ctrl Pts',(54.2062160544311,27.1672626624804,23.2000480025739));
#61275=CARTESIAN_POINT('Ctrl Pts',(54.4232766365216,27.0858936953332,23.2135099583196));
#61276=CARTESIAN_POINT('Ctrl Pts',(54.5510086944361,27.0519717573984,23.221200619581));
#61277=CARTESIAN_POINT('Ctrl Pts',(54.7051792221558,27.027007086802,23.2308154270356));
#61278=CARTESIAN_POINT('Ctrl Pts',(54.7292812957294,27.023555811542,23.2323269565471));
#61279=CARTESIAN_POINT('Ctrl Pts',(54.7631637726224,27.019335417538,23.2344661364921));
#61280=CARTESIAN_POINT('Ctrl Pts',(54.7728964799116,27.018195879373,23.2350822549687));
#61281=CARTESIAN_POINT('Ctrl Pts',(54.7898217301219,27.0163405289065,23.2361567060718));
#61282=CARTESIAN_POINT('Ctrl Pts',(54.797010557825,27.0155920060299,23.2366140117171));
#61283=CARTESIAN_POINT('Ctrl Pts',(54.8120235351367,27.0141112409155,23.2375710778735));
#61284=CARTESIAN_POINT('Ctrl Pts',(54.8198482478452,27.0133861326082,23.238071052261));
#61285=CARTESIAN_POINT('Ctrl Pts',(54.8384151345723,27.0117761520964,23.2392602479254));
#61286=CARTESIAN_POINT('Ctrl Pts',(54.8491605116404,27.0109320827679,23.239950726404));
#61287=CARTESIAN_POINT('Ctrl Pts',(54.885285171777,27.0083888286327,23.2422798574794));
#61288=CARTESIAN_POINT('Ctrl Pts',(54.910689137617,27.0070880548499,23.243930776762));
#61289=CARTESIAN_POINT('Ctrl Pts',(54.9714639187638,27.0051404984673,23.2479131143175));
#61290=CARTESIAN_POINT('Ctrl Pts',(55.0068397008295,27.0049481950451,23.2502577455333));
#61291=CARTESIAN_POINT('Ctrl Pts',(55.1452925243451,27.0078779066466,23.2595387027066));
#61292=CARTESIAN_POINT('Ctrl Pts',(55.248049560848,27.018049589813,23.266664843371));
#61293=CARTESIAN_POINT('Ctrl Pts',(55.4705398563118,27.057650285062,23.2824051829382));
#61294=CARTESIAN_POINT('Ctrl Pts',(55.5892924061433,27.0903220407767,23.2910124544846));
#61295=CARTESIAN_POINT('Ctrl Pts',(55.7190341513746,27.1392835284934,23.3001951079177));
#61296=CARTESIAN_POINT('Ctrl Pts',(55.7337120060112,27.1450222030181,23.301230345357));
#61297=CARTESIAN_POINT('Ctrl Pts',(55.7543099648585,27.1533582416038,23.3026765027001));
#61298=CARTESIAN_POINT('Ctrl Pts',(55.760287375528,27.1558111766054,23.3030953751033));
#61299=CARTESIAN_POINT('Ctrl Pts',(55.7703298121838,27.1599893908685,23.303797640786));
#61300=CARTESIAN_POINT('Ctrl Pts',(55.7744011863436,27.1616991907608,23.3040819427536));
#61301=CARTESIAN_POINT('Ctrl Pts',(55.7827168361507,27.1652239309213,23.3046617376676));
#61302=CARTESIAN_POINT('Ctrl Pts',(55.7869605300156,27.1670401001385,23.3049571553129));
#61303=CARTESIAN_POINT('Ctrl Pts',(55.7977757553531,27.1717131646593,23.305708940068));
#61304=CARTESIAN_POINT('Ctrl Pts',(55.8043383341192,27.1745907976322,23.3061640769284));
#61305=CARTESIAN_POINT('Ctrl Pts',(55.8310940166077,27.1864952348645,23.3080159818504));
#61306=CARTESIAN_POINT('Ctrl Pts',(55.8511526922929,27.1958226286283,23.30939572661));
#61307=CARTESIAN_POINT('Ctrl Pts',(56.0261601913642,27.2807706915851,23.3213929464275));
#61308=CARTESIAN_POINT('Ctrl Pts',(56.1708713746678,27.3758599743514,23.3310817786555));
#61309=CARTESIAN_POINT('Ctrl Pts',(56.372195455831,27.5492087654979,23.3466972653289));
#61310=CARTESIAN_POINT('Ctrl Pts',(56.4384711079166,27.6148959523822,23.35227580554));
#61311=CARTESIAN_POINT('Ctrl Pts',(56.5100495467407,27.6965374580077,23.3590179190276));
#61312=CARTESIAN_POINT('Ctrl Pts',(56.5200570380525,27.7082218408238,23.3599784346568));
#61313=CARTESIAN_POINT('Ctrl Pts',(56.5361859839426,27.7275003759686,23.3615567948436));
#61314=CARTESIAN_POINT('Ctrl Pts',(56.5423887730352,27.7350258746334,23.3621713492577));
#61315=CARTESIAN_POINT('Ctrl Pts',(56.5534026539198,27.7485898505873,23.3632763954362));
#61316=CARTESIAN_POINT('Ctrl Pts',(56.5582343730027,27.7546113846124,23.3637660508649));
#61317=CARTESIAN_POINT('Ctrl Pts',(56.568419601323,27.7674567997589,23.3648087602921));
#61318=CARTESIAN_POINT('Ctrl Pts',(56.5737637907646,27.7742878342497,23.3653621682558));
#61319=CARTESIAN_POINT('Ctrl Pts',(56.5879892300069,27.7927174445258,23.3668524385846));
#61320=CARTESIAN_POINT('Ctrl Pts',(56.5967877644377,27.8043789145247,23.3677924956758));
#61321=CARTESIAN_POINT('Ctrl Pts',(56.6405830399055,27.8637703861967,23.3725664991025));
#61322=CARTESIAN_POINT('Ctrl Pts',(56.6735680910811,27.9129401615652,23.3764760805458));
#61323=CARTESIAN_POINT('Ctrl Pts',(56.7684776016419,28.0689997145327,23.3887640361049));
#61324=CARTESIAN_POINT('Ctrl Pts',(56.8226980836196,28.1802196279707,23.397374778849));
#61325=CARTESIAN_POINT('Ctrl Pts',(56.8841831293861,28.3431504683717,23.4095042681128));
#61326=CARTESIAN_POINT('Ctrl Pts',(56.9002673620794,28.3912457921987,23.4130254420823));
#61327=CARTESIAN_POINT('Ctrl Pts',(56.9298778868938,28.4924593881586,23.4202565067685));
#61328=CARTESIAN_POINT('Ctrl Pts',(56.9430843746261,28.5456318536107,23.4239560146763));
#61329=CARTESIAN_POINT('Ctrl Pts',(56.9558963189699,28.6081093374627,23.4281392119864));
#61330=CARTESIAN_POINT('Ctrl Pts',(56.95764608585,28.6169458109699,23.4287270780151));
#61331=CARTESIAN_POINT('Ctrl Pts',(56.96037778546,28.6312489427348,23.4296721905237));
#61332=CARTESIAN_POINT('Ctrl Pts',(56.9613968287197,28.63670826318,23.4300314166702));
#61333=CARTESIAN_POINT('Ctrl Pts',(56.9631650278105,28.6464053806947,23.4306667265646));
#61334=CARTESIAN_POINT('Ctrl Pts',(56.9639232897444,28.6506414525974,23.4309433170164));
#61335=CARTESIAN_POINT('Ctrl Pts',(56.9655277203487,28.6597750112247,23.4315376344174));
#61336=CARTESIAN_POINT('Ctrl Pts',(56.9663692987154,28.6646732268088,23.4318551013414));
#61337=CARTESIAN_POINT('Ctrl Pts',(56.9686708131002,28.6783753272465,23.4327397866297));
#61338=CARTESIAN_POINT('Ctrl Pts',(56.9700900114112,28.6871860704638,23.4333047559333));
#61339=CARTESIAN_POINT('Ctrl Pts',(56.9781906316498,28.739719938627,23.4366517527509));
#61340=CARTESIAN_POINT('Ctrl Pts',(56.9834759991016,28.7836495542177,23.4393615630364));
#61341=CARTESIAN_POINT('Ctrl Pts',(56.9963859202443,28.9325708719677,23.4483575379999));
#61342=CARTESIAN_POINT('Ctrl Pts',(56.9971640112668,29.0379823119999,23.4544142480253));
#61343=CARTESIAN_POINT('Ctrl Pts',(56.9806647011903,29.2675935326576,23.4677755473257));
#61344=CARTESIAN_POINT('Ctrl Pts',(56.9600220017781,29.3910849872229,23.4750825923943));
#61345=CARTESIAN_POINT('Ctrl Pts',(56.9217309019719,29.5353211833679,23.484266788313));
#61346=CARTESIAN_POINT('Ctrl Pts',(56.915065151186,29.5586983227218,23.4857754975631));
#61347=CARTESIAN_POINT('Ctrl Pts',(56.9051284679641,29.5912767747246,23.4879089592227));
#61348=CARTESIAN_POINT('Ctrl Pts',(56.9022144792804,29.6005853587795,23.4885221173801));
#61349=CARTESIAN_POINT('Ctrl Pts',(56.8970361774662,29.6167113612844,23.4895907140938));
#61350=CARTESIAN_POINT('Ctrl Pts',(56.8948030734968,29.6235386693897,23.490045124005));
#61351=CARTESIAN_POINT('Ctrl Pts',(56.8900687174059,29.6377527939192,23.4909954224819));
#61352=CARTESIAN_POINT('Ctrl Pts',(56.8875609284246,29.6451372887339,23.4914915198569));
#61353=CARTESIAN_POINT('Ctrl Pts',(56.8815177860186,29.6625951656407,23.4926701442732));
#61354=CARTESIAN_POINT('Ctrl Pts',(56.8779447685756,29.6726551653545,23.4933539081129));
#61355=CARTESIAN_POINT('Ctrl Pts',(56.8657054623858,29.7062577726948,23.4956535222178));
#61356=CARTESIAN_POINT('Ctrl Pts',(56.8566761286016,29.7296646984661,23.4972813705041));
#61357=CARTESIAN_POINT('Ctrl Pts',(56.8340726161987,29.785121876564,23.5012023012756));
#61358=CARTESIAN_POINT('Ctrl Pts',(56.8200966915207,29.8169984779811,23.5035082162291));
#61359=CARTESIAN_POINT('Ctrl Pts',(56.7625488991183,29.9394401404017,23.5125711797984));
#61360=CARTESIAN_POINT('Ctrl Pts',(56.7129959541922,30.0270185615008,23.519509994011));
#61361=CARTESIAN_POINT('Ctrl Pts',(56.5863504229899,30.2159991613256,23.5353575152376));
#61362=CARTESIAN_POINT('Ctrl Pts',(56.5057156092179,30.3145294081862,23.5442725769919));
#61363=CARTESIAN_POINT('Ctrl Pts',(56.4053126561713,30.4157560492814,23.5537134968081));
#61364=CARTESIAN_POINT('Ctrl Pts',(56.3942449034619,30.4266569445521,23.5547339758985));
#61365=CARTESIAN_POINT('Ctrl Pts',(56.3784386814168,30.4418652238573,23.5561616570567));
#61366=CARTESIAN_POINT('Ctrl Pts',(56.3738054175832,30.4462804705647,23.5565766220354));
#61367=CARTESIAN_POINT('Ctrl Pts',(56.3659606293862,30.4536844105377,23.5572731705885));
#61368=CARTESIAN_POINT('Ctrl Pts',(56.362760378524,30.4566849208744,23.5575556453886));
#61369=CARTESIAN_POINT('Ctrl Pts',(56.3561756278052,30.4628179981053,23.5581333839986));
#61370=CARTESIAN_POINT('Ctrl Pts',(56.3527901458667,30.4659494027158,23.558428564128));
#61371=CARTESIAN_POINT('Ctrl Pts',(56.3441132951714,30.4739194081151,23.5591804599885));
#61372=CARTESIAN_POINT('Ctrl Pts',(56.3388065881791,30.4787413212083,23.5596359397828));
#61373=CARTESIAN_POINT('Ctrl Pts',(56.31695192135,30.4983853711532,23.5614944693113));
#61374=CARTESIAN_POINT('Ctrl Pts',(56.3001821923403,30.5129598299847,23.5628803043307));
#61375=CARTESIAN_POINT('Ctrl Pts',(56.1521480754288,30.6373356444658,23.5748039478997));
#61376=CARTESIAN_POINT('Ctrl Pts',(56.0074867602964,30.7301155604524,23.5844238475882));
#61377=CARTESIAN_POINT('Ctrl Pts',(55.7655181453883,30.8445373607581,23.6001335628644));
#61378=CARTESIAN_POINT('Ctrl Pts',(55.6754310293716,30.8793949850743,23.605899824467));
#61379=CARTESIAN_POINT('Ctrl Pts',(55.5683294707553,30.9121376584505,23.612854367207));
#61380=CARTESIAN_POINT('Ctrl Pts',(55.5534236850307,30.9165048958821,23.6138241994013));
#61381=CARTESIAN_POINT('Ctrl Pts',(55.5290198806953,30.9233465175018,23.6154158610411));
#61382=CARTESIAN_POINT('Ctrl Pts',(55.5195517425197,30.9259257103851,23.6160343276561));
#61383=CARTESIAN_POINT('Ctrl Pts',(55.5025751192138,30.9304159749629,23.6171450926423));
#61384=CARTESIAN_POINT('Ctrl Pts',(55.4950737554998,30.9323533736677,23.6176365387527));
#61385=CARTESIAN_POINT('Ctrl Pts',(55.4791429887171,30.9363690069521,23.6186816677031));
#61386=CARTESIAN_POINT('Ctrl Pts',(55.4707109442223,30.9384360030261,23.6192356970079));
#61387=CARTESIAN_POINT('Ctrl Pts',(55.4480919170739,30.9438244509622,23.6207242885064));
#61388=CARTESIAN_POINT('Ctrl Pts',(55.4338817994746,30.9470455639079,23.6216620043055));
#61389=CARTESIAN_POINT('Ctrl Pts',(55.3626139068295,30.9623814701046,23.6263784521179));
#61390=CARTESIAN_POINT('Ctrl Pts',(55.3050844080902,30.9721440726963,23.6302301539382));
#61391=CARTESIAN_POINT('Ctrl Pts',(55.1336318920188,30.993557701073,23.6418458428476));
#61392=CARTESIAN_POINT('Ctrl Pts',(55.0190501218361,30.9979393475764,23.6497985991136));
#61393=CARTESIAN_POINT('Ctrl Pts',(54.8001909402524,30.9874755624655,23.6650546666023));
#61394=CARTESIAN_POINT('Ctrl Pts',(54.6961882118609,30.9742556737258,23.6723277967546));
#61395=CARTESIAN_POINT('Ctrl Pts',(54.5779959171746,30.9496659336828,23.6803221828443));
#61396=CARTESIAN_POINT('Ctrl Pts',(54.5623359725929,30.9462104039463,23.6813756071969));
#61397=CARTESIAN_POINT('Ctrl Pts',(54.5404432024905,30.9411019139186,23.6828385873551));
#61398=CARTESIAN_POINT('Ctrl Pts',(54.5341746046335,30.9396071236522,23.6832563622914));
#61399=CARTESIAN_POINT('Ctrl Pts',(54.5236203829862,30.9370362787557,23.6839577353699));
#61400=CARTESIAN_POINT('Ctrl Pts',(54.519330942291,30.9359763281572,23.6842422203313));
#61401=CARTESIAN_POINT('Ctrl Pts',(54.5106107827195,30.9337907470628,23.6848193751251));
#61402=CARTESIAN_POINT('Ctrl Pts',(54.5061804006559,30.9326641362935,23.6851119901684));
#61403=CARTESIAN_POINT('Ctrl Pts',(54.4949803460138,30.9297750245215,23.6858502565804));
#61404=CARTESIAN_POINT('Ctrl Pts',(54.4882159346453,30.9279921083906,23.6862947823126));
#61405=CARTESIAN_POINT('Ctrl Pts',(54.4621253596635,30.9209683476557,23.6880045728139));
#61406=CARTESIAN_POINT('Ctrl Pts',(54.4428684186382,30.9154720025348,23.6892564236563));
#61407=CARTESIAN_POINT('Ctrl Pts',(54.2912854644196,30.8697274444191,23.6990539728212));
#61408=CARTESIAN_POINT('Ctrl Pts',(54.1633721998504,30.8161004049785,23.7069985486325));
#61409=CARTESIAN_POINT('Ctrl Pts',(54.0258782399295,30.740819710466,23.7161584189659));
#61410=CARTESIAN_POINT('Ctrl Pts',(54.0098540500527,30.731755599347,23.7172357677195));
#61411=CARTESIAN_POINT('Ctrl Pts',(53.9038475038053,30.6698404423495,23.7244399152103));
#61412=CARTESIAN_POINT('Ctrl Pts',(53.8180171704275,30.6102266877487,23.7306586870503));
#61413=CARTESIAN_POINT('Ctrl Pts',(53.7250642332943,30.5342144919913,23.7381142867862));
#61414=CARTESIAN_POINT('Ctrl Pts',(53.7129980410297,30.5241067064651,23.7390969735459));
#61415=CARTESIAN_POINT('Ctrl Pts',(53.6935228361529,30.5073962427245,23.7407083149328));
#61416=CARTESIAN_POINT('Ctrl Pts',(53.6860411059779,30.5008790862246,23.741333555631));
#61417=CARTESIAN_POINT('Ctrl Pts',(53.6727481960419,30.4891243761616,23.742455799945));
#61418=CARTESIAN_POINT('Ctrl Pts',(53.6669185808696,30.4839079102067,23.7429519385613));
#61419=CARTESIAN_POINT('Ctrl Pts',(53.6546291352255,30.4727801836509,23.7440064174553));
#61420=CARTESIAN_POINT('Ctrl Pts',(53.6481772574697,30.4668604234792,23.7445651032287));
#61421=CARTESIAN_POINT('Ctrl Pts',(53.6310172363931,30.4509063047845,23.7460648860278));
#61422=CARTESIAN_POINT('Ctrl Pts',(53.6203806593805,30.4407960884781,23.7470091508639));
#61423=CARTESIAN_POINT('Ctrl Pts',(53.5679022930759,30.3898007086786,23.751742653849));
#61424=CARTESIAN_POINT('Ctrl Pts',(53.5277654489043,30.3472097564735,23.755604899916));
#61425=CARTESIAN_POINT('Ctrl Pts',(53.3631004050786,30.1563181795977,23.7725527284527));
#61426=CARTESIAN_POINT('Ctrl Pts',(53.2587174625726,29.992160893355,23.7863691355466));
#61427=CARTESIAN_POINT('Ctrl Pts',(53.1796208058588,29.8156268460748,23.7995000000001));
#61428=CARTESIAN_POINT('',(55.1572109533382,30.9885452669352,23.7995));
#61429=CARTESIAN_POINT('Origin',(55.,29.,23.7995));
#61430=CARTESIAN_POINT('',(53.0052505146164,29.0014328510003,23.2095451186048));
#61431=CARTESIAN_POINT('Ctrl Pts',(53.0052505146164,29.0014328510003,23.2095451186048));
#61432=CARTESIAN_POINT('Ctrl Pts',(53.0052003937452,28.9316568713932,23.213983964139));
#61433=CARTESIAN_POINT('Ctrl Pts',(53.008815721088,28.8618442511641,23.2184228096733));
#61434=CARTESIAN_POINT('Ctrl Pts',(53.0160814449356,28.7924072993311,23.2228616552075));
#61435=CARTESIAN_POINT('Ctrl Pts',(53.0233464821315,28.7229769096794,23.2273000812459));
#61436=CARTESIAN_POINT('Ctrl Pts',(53.0342611791721,28.6539226036702,23.2317385072843));
#61437=CARTESIAN_POINT('Ctrl Pts',(53.0487586209827,28.5856515436127,23.2361769333228));
#61438=CARTESIAN_POINT('Ctrl Pts',(53.0632595914515,28.5173638664694,23.2406164396682));
#61439=CARTESIAN_POINT('Ctrl Pts',(53.0813449337531,28.4498602909106,23.2450559460137));
#61440=CARTESIAN_POINT('Ctrl Pts',(53.1028970159024,28.3835360268208,23.2494954523591));
#61441=CARTESIAN_POINT('Ctrl Pts',(53.1244760897302,28.3171286986818,23.2539405187116));
#61442=CARTESIAN_POINT('Ctrl Pts',(53.1495304120609,28.2519040931028,23.2583855850641));
#61443=CARTESIAN_POINT('Ctrl Pts',(53.1778933430144,28.1882396332238,23.2628306514166));
#61444=CARTESIAN_POINT('Ctrl Pts',(53.2062775865753,28.1245273342959,23.2672790579018));
#61445=CARTESIAN_POINT('Ctrl Pts',(53.237975161805,28.0623779471762,23.271727464387));
#61446=CARTESIAN_POINT('Ctrl Pts',(53.2727736951244,28.0021438709685,23.2761758708722));
#61447=CARTESIAN_POINT('Ctrl Pts',(53.3076334738165,27.9418037828661,23.280632106547));
#61448=CARTESIAN_POINT('Ctrl Pts',(53.3456048299077,27.8833861368431,23.2850883422217));
#61449=CARTESIAN_POINT('Ctrl Pts',(53.3864329442855,27.8272131825379,23.2895445778965));
#61450=CARTESIAN_POINT('Ctrl Pts',(53.3960350471951,27.814002224937,23.2905926114437));
#61451=CARTESIAN_POINT('Ctrl Pts',(53.4057949933653,27.8009152710909,23.291640644991));
#61452=CARTESIAN_POINT('Ctrl Pts',(53.4157091669753,27.787956222369,23.2926886785382));
#61453=CARTESIAN_POINT('Ctrl Pts',(53.4579393336063,27.7327561816565,23.2971528560961));
#61454=CARTESIAN_POINT('Ctrl Pts',(53.5031392396318,27.6796594619913,23.3016170336539));
#61455=CARTESIAN_POINT('Ctrl Pts',(53.5510719652676,27.6290021470963,23.3060812112118));
#61456=CARTESIAN_POINT('Ctrl Pts',(53.5989330395069,27.5784205564024,23.310538715572));
#61457=CARTESIAN_POINT('Ctrl Pts',(53.6495184920662,27.5302714830558,23.3149962199321));
#61458=CARTESIAN_POINT('Ctrl Pts',(53.7025503019092,27.4848591341317,23.3194537242923));
#61459=CARTESIAN_POINT('Ctrl Pts',(53.7555194471414,27.4395004463438,23.3239059614783));
#61460=CARTESIAN_POINT('Ctrl Pts',(53.8109288390678,27.3968723744137,23.3283581986643));
#61461=CARTESIAN_POINT('Ctrl Pts',(53.8684639171322,27.3572420581023,23.3328104358503));
#61462=CARTESIAN_POINT('Ctrl Pts',(53.925962550079,27.3176368452857,23.3372598528037));
#61463=CARTESIAN_POINT('Ctrl Pts',(53.9855837973,27.2810258960868,23.341709269757));
#61464=CARTESIAN_POINT('Ctrl Pts',(54.0469815372319,27.2476349204224,23.3461586867104));
#61465=CARTESIAN_POINT('Ctrl Pts',(54.1083609907082,27.2142538897917,23.3506067784673));
#61466=CARTESIAN_POINT('Ctrl Pts',(54.1715154586615,27.1840911611187,23.3550548702242));
#61467=CARTESIAN_POINT('Ctrl Pts',(54.2360729823614,27.1573271928468,23.3595029619811));
#61468=CARTESIAN_POINT('Ctrl Pts',(54.300632943392,27.1305622141173,23.3639512216731));
#61469=CARTESIAN_POINT('Ctrl Pts',(54.3665956144681,27.1071964348777,23.368399481365));
#61470=CARTESIAN_POINT('Ctrl Pts',(54.4335693888397,27.0873620506639,23.372847741057));
#61471=CARTESIAN_POINT('Ctrl Pts',(54.5006111469935,27.0675075329506,23.3773005160913));
#61472=CARTESIAN_POINT('Ctrl Pts',(54.5686655890589,27.051191703632,23.3817532911256));
#61473=CARTESIAN_POINT('Ctrl Pts',(54.6373272168936,27.0384964912359,23.3862060661599));
#61474=CARTESIAN_POINT('Ctrl Pts',(54.7060278406712,27.0257940686732,23.39066137012));
#61475=CARTESIAN_POINT('Ctrl Pts',(54.7753358536369,27.0167164203056,23.3951166740801));
#61476=CARTESIAN_POINT('Ctrl Pts',(54.8448395772272,27.0112936854063,23.3995719780401));
#61477=CARTESIAN_POINT('Ctrl Pts',(54.9144593687262,27.0058618947979,23.4040347221457));
#61478=CARTESIAN_POINT('Ctrl Pts',(54.9842750363814,27.0040972136788,23.4084974662512));
#61479=CARTESIAN_POINT('Ctrl Pts',(55.0538746652478,27.0059776623758,23.4129602103568));
#61480=CARTESIAN_POINT('Ctrl Pts',(55.0873082045986,27.0068809725878,23.4151039765391));
#61481=CARTESIAN_POINT('Ctrl Pts',(55.1206919650002,27.0086246434188,23.4172477427214));
#61482=CARTESIAN_POINT('Ctrl Pts',(55.1539809403483,27.0112020131473,23.4193915089037));
#61483=CARTESIAN_POINT('Ctrl Pts',(55.223243451322,27.0165646023299,23.4238519234155));
#61484=CARTESIAN_POINT('Ctrl Pts',(55.2923578402198,27.0255599757434,23.4283123379274));
#61485=CARTESIAN_POINT('Ctrl Pts',(55.3609135802758,27.0381720386149,23.4327727524393));
#61486=CARTESIAN_POINT('Ctrl Pts',(55.429368653755,27.0507655820569,23.4372266173222));
#61487=CARTESIAN_POINT('Ctrl Pts',(55.4972662306628,27.0669651856091,23.4416804822051));
#61488=CARTESIAN_POINT('Ctrl Pts',(55.564200204765,27.0867029265054,23.446134347088));
#61489=CARTESIAN_POINT('Ctrl Pts',(55.6310579929409,27.1064182014104,23.4505831424703));
#61490=CARTESIAN_POINT('Ctrl Pts',(55.6969538910947,27.1296634772005,23.4550319378526));
#61491=CARTESIAN_POINT('Ctrl Pts',(55.7614930396604,27.15632000796,23.459480733235));
#61492=CARTESIAN_POINT('Ctrl Pts',(55.8259930789442,27.1829603854574,23.4639268327467));
#61493=CARTESIAN_POINT('Ctrl Pts',(55.8891375499583,27.213007730801,23.4683729322584));
#61494=CARTESIAN_POINT('Ctrl Pts',(55.950549236786,27.2462942918079,23.4728190317701));
#61495=CARTESIAN_POINT('Ctrl Pts',(56.0119443912701,27.2795718919005,23.4772639343688));
#61496=CARTESIAN_POINT('Ctrl Pts',(56.0716072591108,27.3160867439157,23.4817088369676));
#61497=CARTESIAN_POINT('Ctrl Pts',(56.1291845935455,27.3556248249869,23.4861537395663));
#61498=CARTESIAN_POINT('Ctrl Pts',(56.1867658175742,27.3951655770237,23.4905989424371));
#61499=CARTESIAN_POINT('Ctrl Pts',(56.2422608277492,27.4377296854861,23.4950441453079));
#61500=CARTESIAN_POINT('Ctrl Pts',(56.295346242923,27.4830604252492,23.4994893481787));
#61501=CARTESIAN_POINT('Ctrl Pts',(56.3484881889734,27.5284394379032,23.5039392847643));
#61502=CARTESIAN_POINT('Ctrl Pts',(56.3992150471316,27.5765906445625,23.50838922135));
#61503=CARTESIAN_POINT('Ctrl Pts',(56.447238100391,27.6272183555726,23.5128391579356));
#61504=CARTESIAN_POINT('Ctrl Pts',(56.495289745305,27.6778762089817,23.5172917438956));
#61505=CARTESIAN_POINT('Ctrl Pts',(56.5406340643731,27.7310131305015,23.5217443298557));
#61506=CARTESIAN_POINT('Ctrl Pts',(56.5830224948326,27.7863001428055,23.5261969158157));
#61507=CARTESIAN_POINT('Ctrl Pts',(56.6254837756589,27.841682173469,23.5306571541591));
#61508=CARTESIAN_POINT('Ctrl Pts',(56.6649787517476,27.899221268783,23.5351173925025));
#61509=CARTESIAN_POINT('Ctrl Pts',(56.7013025072247,27.9585599674437,23.5395776308459));
#61510=CARTESIAN_POINT('Ctrl Pts',(56.7189929910849,27.9874592449867,23.541749866987));
#61511=CARTESIAN_POINT('Ctrl Pts',(56.7359319909526,28.0167850081694,23.5439221031281));
#61512=CARTESIAN_POINT('Ctrl Pts',(56.7520999247469,28.0464941446421,23.5460943392691));
#61513=CARTESIAN_POINT('Ctrl Pts',(56.7849370585255,28.1068335115155,23.5505061589654));
#61514=CARTESIAN_POINT('Ctrl Pts',(56.8147250413319,28.1690028022865,23.5549179786618));
#61515=CARTESIAN_POINT('Ctrl Pts',(56.8412533880425,28.2326581442915,23.5593297983581));
#61516=CARTESIAN_POINT('Ctrl Pts',(56.8677416371924,28.2962172713323,23.5637349495949));
#61517=CARTESIAN_POINT('Ctrl Pts',(56.8909798325664,28.3612575373282,23.5681401008316));
#61518=CARTESIAN_POINT('Ctrl Pts',(56.9108030193091,28.4274099338102,23.5725452520684));
#61519=CARTESIAN_POINT('Ctrl Pts',(56.9306036107021,28.4934869268492,23.5769453821179));
#61520=CARTESIAN_POINT('Ctrl Pts',(56.9469967761192,28.5606730584504,23.5813455121674));
#61521=CARTESIAN_POINT('Ctrl Pts',(56.9598661039142,28.6285805373597,23.5857456422169));
#61522=CARTESIAN_POINT('Ctrl Pts',(56.9727276878521,28.6964471543194,23.5901431245773));
#61523=CARTESIAN_POINT('Ctrl Pts',(56.982069544642,28.765033768377,23.5945406069377));
#61524=CARTESIAN_POINT('Ctrl Pts',(56.9878258834181,28.8339403128002,23.5989380892981));
#61525=CARTESIAN_POINT('Ctrl Pts',(56.9935808038825,28.9028298792501,23.6033344881571));
#61526=CARTESIAN_POINT('Ctrl Pts',(56.9957519173905,28.9720387219498,23.6077308870161));
#61527=CARTESIAN_POINT('Ctrl Pts',(56.9943252738296,29.0411614463345,23.612127285875));
#61528=CARTESIAN_POINT('Ctrl Pts',(56.9928984748356,29.1102917016561,23.6165241637227));
#61529=CARTESIAN_POINT('Ctrl Pts',(56.987873153928,29.1793353205475,23.6209210415703));
#61530=CARTESIAN_POINT('Ctrl Pts',(56.9792874447691,29.2478886312022,23.625317919418));
#61531=CARTESIAN_POINT('Ctrl Pts',(56.9706913314874,29.3165250144432,23.629720125382));
#61532=CARTESIAN_POINT('Ctrl Pts',(56.9585262831637,29.3846694070833,23.634122331346));
#61533=CARTESIAN_POINT('Ctrl Pts',(56.9428819981594,29.4519259936409,23.63852453731));
#61534=CARTESIAN_POINT('Ctrl Pts',(56.9272273849109,29.5192269825121,23.6429296495786));
#61535=CARTESIAN_POINT('Ctrl Pts',(56.9080891071294,29.5856385203148,23.6473347618472));
#61536=CARTESIAN_POINT('Ctrl Pts',(56.8856065793176,29.6507806009204,23.6517398741159));
#61537=CARTESIAN_POINT('Ctrl Pts',(56.8630803356331,29.7160493462374,23.6561535518505));
#61538=CARTESIAN_POINT('Ctrl Pts',(56.8371970534577,29.780043246305,23.6605672295851));
#61539=CARTESIAN_POINT('Ctrl Pts',(56.8081437043812,29.8424036483816,23.6649809073197));
#61540=CARTESIAN_POINT('Ctrl Pts',(56.7909933359761,29.8792153724512,23.6675863280913));
#61541=CARTESIAN_POINT('Ctrl Pts',(56.7727391922468,29.9154583669337,23.6701917488629));
#61542=CARTESIAN_POINT('Ctrl Pts',(56.7534268006312,29.9510636242272,23.6727971696346));
#61543=CARTESIAN_POINT('Ctrl Pts',(56.7194988970924,30.0136147447188,23.6773743585389));
#61544=CARTESIAN_POINT('Ctrl Pts',(56.6821654181802,30.0744490461571,23.6819515474432));
#61545=CARTESIAN_POINT('Ctrl Pts',(56.6416212702106,30.1331845249968,23.6865287363475));
#61546=CARTESIAN_POINT('Ctrl Pts',(56.5999260677838,30.1935875129124,23.691235872333));
#61547=CARTESIAN_POINT('Ctrl Pts',(56.5548352799137,30.2517702301202,23.6959430083185));
#61548=CARTESIAN_POINT('Ctrl Pts',(56.5066120605671,30.3073437426529,23.700650144304));
#61549=CARTESIAN_POINT('Ctrl Pts',(56.4598751211621,30.3612044330623,23.7052122024227));
#61550=CARTESIAN_POINT('Ctrl Pts',(56.4101963491268,30.4126140338595,23.7097742605413));
#61551=CARTESIAN_POINT('Ctrl Pts',(56.3578584746602,30.4612487554464,23.7143363186599));
#61552=CARTESIAN_POINT('Ctrl Pts',(56.3055697505126,30.5098378043324,23.7188940925654));
#61553=CARTESIAN_POINT('Ctrl Pts',(56.2506272201341,30.5556568431123,23.7234518664708));
#61554=CARTESIAN_POINT('Ctrl Pts',(56.193351055624,30.5984182245398,23.7280096403763));
#61555=CARTESIAN_POINT('Ctrl Pts',(56.1361132473686,30.6411509698593,23.7325643620673));
#61556=CARTESIAN_POINT('Ctrl Pts',(56.0765452772435,30.6808298560183,23.7371190837583));
#61557=CARTESIAN_POINT('Ctrl Pts',(56.0149999893189,30.7172077871308,23.7416738054493));
#61558=CARTESIAN_POINT('Ctrl Pts',(55.9534793501874,30.7535711489379,23.7462267029812));
#61559=CARTESIAN_POINT('Ctrl Pts',(55.8899833615618,30.7866359535699,23.7507796005132));
#61560=CARTESIAN_POINT('Ctrl Pts',(55.824892246756,30.8161994228999,23.7553324980452));
#61561=CARTESIAN_POINT('Ctrl Pts',(55.7597915763966,30.845767232228,23.7598860639549));
#61562=CARTESIAN_POINT('Ctrl Pts',(55.6930957255118,30.8718324847587,23.7644396298647));
#61563=CARTESIAN_POINT('Ctrl Pts',(55.6252069064563,30.8942396592352,23.7689931957745));
#61564=CARTESIAN_POINT('Ctrl Pts',(55.5573127849839,30.916648583811,23.7735471173379));
#61565=CARTESIAN_POINT('Ctrl Pts',(55.4882259463757,30.9353987263845,23.7781010389013));
#61566=CARTESIAN_POINT('Ctrl Pts',(55.4183641249596,30.9503843266,23.7826549604647));
#61567=CARTESIAN_POINT('Ctrl Pts',(55.3484544890822,30.9653801831813,23.7872119987992));
#61568=CARTESIAN_POINT('Ctrl Pts',(55.2777692603935,30.9766062679254,23.7917690371337));
#61569=CARTESIAN_POINT('Ctrl Pts',(55.2067358047839,30.9840080316169,23.7963260754682));
#61570=CARTESIAN_POINT('Ctrl Pts',(55.1902444778306,30.9857264459052,23.7973840503121));
#61571=CARTESIAN_POINT('Ctrl Pts',(55.17373440234,30.9872389516035,23.7984420251561));
#61572=CARTESIAN_POINT('Ctrl Pts',(55.1572109533382,30.9885452669352,23.7995));
#61573=CARTESIAN_POINT('Ctrl Pts',(53.0052505724191,29.0015111801821,23.2106966576448));
#61574=CARTESIAN_POINT('Ctrl Pts',(53.0053532058501,29.1369867378291,23.2014815125057));
#61575=CARTESIAN_POINT('Ctrl Pts',(53.0192563134189,29.2719984182957,23.1919432329457));
#61576=CARTESIAN_POINT('Ctrl Pts',(53.0466869980277,29.4044698738173,23.182578193545));
#61577=CARTESIAN_POINT('Origin',(55.,29.,23.7995));
#61578=CARTESIAN_POINT('',(57.0818213830407,27.7073399599607,23.7995));
#61579=CARTESIAN_POINT('',(52.5495,29.,23.7995));
#61580=CARTESIAN_POINT('Origin',(55.,29.,23.7995));
#61581=CARTESIAN_POINT('Ctrl Pts',(57.0818213830407,27.7073399599607,23.7995));
#61582=CARTESIAN_POINT('Ctrl Pts',(57.1030396553067,27.7491534849406,23.7995));
#61583=CARTESIAN_POINT('Ctrl Pts',(57.1229432336361,27.7915806564359,23.7995));
#61584=CARTESIAN_POINT('Ctrl Pts',(57.1414767532722,27.834592368553,23.7995));
#61585=CARTESIAN_POINT('Ctrl Pts',(57.1752210883004,27.9129046185899,23.7995));
#61586=CARTESIAN_POINT('Ctrl Pts',(57.204426630953,27.9931545233241,23.7995));
#61587=CARTESIAN_POINT('Ctrl Pts',(57.2291348926794,28.0749451167352,23.7995));
#61588=CARTESIAN_POINT('Ctrl Pts',(57.2415707567772,28.1161109711122,23.7995));
#61589=CARTESIAN_POINT('Ctrl Pts',(57.2528665481713,28.1576672136207,23.7995));
#61590=CARTESIAN_POINT('Ctrl Pts',(57.2630226514886,28.1995631640058,23.7995));
#61591=CARTESIAN_POINT('Ctrl Pts',(57.2679451975272,28.219869647522,23.7995));
#61592=CARTESIAN_POINT('Ctrl Pts',(57.2725999564407,28.2402559300432,23.7995));
#61593=CARTESIAN_POINT('Ctrl Pts',(57.2769867024841,28.2607161878036,23.7995));
#61594=CARTESIAN_POINT('Ctrl Pts',(57.2803633605224,28.2764652859161,23.7995));
#61595=CARTESIAN_POINT('Ctrl Pts',(57.283579417055,28.2922499240532,23.7995));
#61596=CARTESIAN_POINT('Ctrl Pts',(57.2866346383619,28.3080640271147,23.7995));
#61597=CARTESIAN_POINT('Ctrl Pts',(57.3027426818727,28.3914407237968,23.7995));
#61598=CARTESIAN_POINT('Ctrl Pts',(57.3143907517678,28.4756669169532,23.7995));
#61599=CARTESIAN_POINT('Ctrl Pts',(57.3216193457988,28.560349030643,23.7995));
#61600=CARTESIAN_POINT('Ctrl Pts',(57.3272123451589,28.625870348572,23.7995));
#61601=CARTESIAN_POINT('Ctrl Pts',(57.3301584584012,28.6916648728046,23.7995));
#61602=CARTESIAN_POINT('Ctrl Pts',(57.3304553643523,28.7575465748756,23.7995));
#61603=CARTESIAN_POINT('Ctrl Pts',(57.3306021462004,28.7901166124713,23.7995));
#61604=CARTESIAN_POINT('Ctrl Pts',(57.3301011767369,28.8227078729075,23.7995));
#61605=CARTESIAN_POINT('Ctrl Pts',(57.3289505854467,28.8552972137907,23.7995));
#61606=CARTESIAN_POINT('Ctrl Pts',(57.3282547843989,28.8750050785456,23.7995));
#61607=CARTESIAN_POINT('Ctrl Pts',(57.3273209535759,28.8947175616372,23.7995));
#61608=CARTESIAN_POINT('Ctrl Pts',(57.3261507382989,28.9143980333835,23.7995));
#61609=CARTESIAN_POINT('Ctrl Pts',(57.321219325461,28.9973336546602,23.7995));
#61610=CARTESIAN_POINT('Ctrl Pts',(57.3120931008026,29.0797939101152,23.7995));
#61611=CARTESIAN_POINT('Ctrl Pts',(57.2988083985721,29.1614134126558,23.7995));
#61612=CARTESIAN_POINT('Ctrl Pts',(57.2856622806402,29.2421814710828,23.7995));
#61613=CARTESIAN_POINT('Ctrl Pts',(57.2684436947102,29.3221271630888,23.7995));
#61614=CARTESIAN_POINT('Ctrl Pts',(57.2471404962224,29.4008787730705,23.7995));
#61615=CARTESIAN_POINT('Ctrl Pts',(57.2264556547298,29.4773445005381,23.7995));
#61616=CARTESIAN_POINT('Ctrl Pts',(57.2019195046976,29.5526851565708,23.7995));
#61617=CARTESIAN_POINT('Ctrl Pts',(57.1734812055056,29.6265319791042,23.7995));
#61618=CARTESIAN_POINT('Ctrl Pts',(57.1631231693767,29.653429088901,23.7995));
#61619=CARTESIAN_POINT('Ctrl Pts',(57.1522471027555,29.6801276936848,23.7995));
#61620=CARTESIAN_POINT('Ctrl Pts',(57.1408493279597,29.7066087272485,23.7995));
#61621=CARTESIAN_POINT('Ctrl Pts',(57.1357954958359,29.7183505540957,23.7995));
#61622=CARTESIAN_POINT('Ctrl Pts',(57.1306390832675,29.7300495949142,23.7995));
#61623=CARTESIAN_POINT('Ctrl Pts',(57.125379729995,29.7417041391356,23.7995));
#61624=CARTESIAN_POINT('Ctrl Pts',(57.1196168749922,29.7544744257074,23.7995));
#61625=CARTESIAN_POINT('Ctrl Pts',(57.1137336869214,29.7671839514575,23.7995));
#61626=CARTESIAN_POINT('Ctrl Pts',(57.1077332174747,29.7798243326649,23.7995));
#61627=CARTESIAN_POINT('Ctrl Pts',(57.0742497329774,29.8503594819485,23.7995));
#61628=CARTESIAN_POINT('Ctrl Pts',(57.0370888487061,29.9188081298351,23.7995));
#61629=CARTESIAN_POINT('Ctrl Pts',(56.9962424222594,29.9848386006808,23.7995));
#61630=CARTESIAN_POINT('Ctrl Pts',(56.9810932635781,30.00932803997,23.7995));
#61631=CARTESIAN_POINT('Ctrl Pts',(56.9654367357015,30.0334845581951,23.7995));
#61632=CARTESIAN_POINT('Ctrl Pts',(56.9492709954722,30.0572900658797,23.7995));
#61633=CARTESIAN_POINT('Ctrl Pts',(56.904600395496,30.1230715454731,23.7995));
#61634=CARTESIAN_POINT('Ctrl Pts',(56.8560436870518,30.1861759538499,23.7995));
#61635=CARTESIAN_POINT('Ctrl Pts',(56.8039291296095,30.2464231547475,23.7995));
#61636=CARTESIAN_POINT('Ctrl Pts',(56.753493550458,30.3047293674193,23.7995));
#61637=CARTESIAN_POINT('Ctrl Pts',(56.6997246599247,30.3603596510879,23.7995));
#61638=CARTESIAN_POINT('Ctrl Pts',(56.6429003401567,30.4131086059567,23.7995));
#61639=CARTESIAN_POINT('Ctrl Pts',(56.631007338023,30.4241486577403,23.7995));
#61640=CARTESIAN_POINT('Ctrl Pts',(56.6189775044667,30.4350648031822,23.7995));
#61641=CARTESIAN_POINT('Ctrl Pts',(56.6068336367285,30.4458373588959,23.7995));
#61642=CARTESIAN_POINT('Ctrl Pts',(56.548571484007,30.4975204222927,23.7995));
#61643=CARTESIAN_POINT('Ctrl Pts',(56.4876029081873,30.5459827779286,23.7995));
#61644=CARTESIAN_POINT('Ctrl Pts',(56.4242546407422,30.5910801684579,23.7995));
#61645=CARTESIAN_POINT('Ctrl Pts',(56.3610994478872,30.6360401099214,23.7995));
#61646=CARTESIAN_POINT('Ctrl Pts',(56.2955780376467,30.6776559088237,23.7995));
#61647=CARTESIAN_POINT('Ctrl Pts',(56.2279927066909,30.7157377301824,23.7995));
#61648=CARTESIAN_POINT('Ctrl Pts',(56.1614582290472,30.7532274347675,23.7995));
#61649=CARTESIAN_POINT('Ctrl Pts',(56.0929225858511,30.7872924132189,23.7995));
#61650=CARTESIAN_POINT('Ctrl Pts',(56.0226677290349,30.8177021134375,23.7995));
#61651=CARTESIAN_POINT('Ctrl Pts',(55.9956814080747,30.8293830984625,23.7995));
#61652=CARTESIAN_POINT('Ctrl Pts',(55.9684414235731,30.8405242122541,23.7995));
#61653=CARTESIAN_POINT('Ctrl Pts',(55.9409639301567,30.8511103048716,23.7995));
#61654=CARTESIAN_POINT('Ctrl Pts',(55.9293858895887,30.8555709086074,23.7995));
#61655=CARTESIAN_POINT('Ctrl Pts',(55.9177654819835,30.859932941087,23.7995));
#61656=CARTESIAN_POINT('Ctrl Pts',(55.9061177979359,30.8641903960764,23.7995));
#61657=CARTESIAN_POINT('Ctrl Pts',(55.8355459925781,30.8899857630871,23.7995));
#61658=CARTESIAN_POINT('Ctrl Pts',(55.7638488209893,30.9119951518818,23.7995));
#61659=CARTESIAN_POINT('Ctrl Pts',(55.6913062742255,30.9300521964143,23.7995));
#61660=CARTESIAN_POINT('Ctrl Pts',(55.620784624429,30.9476062061325,23.7995));
#61661=CARTESIAN_POINT('Ctrl Pts',(55.5494632169023,30.9614250473839,23.7995));
#61662=CARTESIAN_POINT('Ctrl Pts',(55.4775979949367,30.9713078399483,23.7995));
#61663=CARTESIAN_POINT('Ctrl Pts',(55.4067390150588,30.9810522556797,23.7995));
#61664=CARTESIAN_POINT('Ctrl Pts',(55.3353506394514,30.9869701931208,23.7995));
#61665=CARTESIAN_POINT('Ctrl Pts',(55.263688103798,30.9888204486881,23.7995));
#61666=CARTESIAN_POINT('Ctrl Pts',(55.2282516842486,30.989735381881,23.7995));
#61667=CARTESIAN_POINT('Ctrl Pts',(55.1927484456801,30.9896549180268,23.7995));
#61668=CARTESIAN_POINT('Ctrl Pts',(55.1572109533382,30.9885452669352,23.7995));
#61669=CARTESIAN_POINT('',(53.1673064968656,29.7915239329253,23.80042507898));
#61670=CARTESIAN_POINT('Ctrl Pts',(53.1796208058588,29.8156268460748,23.7995000000001));
#61671=CARTESIAN_POINT('Ctrl Pts',(53.1759393605194,29.8074103111085,23.79980835966));
#61672=CARTESIAN_POINT('Ctrl Pts',(53.1723135457441,29.7991688506918,23.80011671932));
#61673=CARTESIAN_POINT('Ctrl Pts',(53.1687436939319,29.7909032203662,23.80042507898));
#61674=CARTESIAN_POINT('Ctrl Pts',(53.165787664683,29.7920814616361,23.7995));
#61675=CARTESIAN_POINT('Ctrl Pts',(53.1401820698082,29.7477636700476,23.7995));
#61676=CARTESIAN_POINT('Ctrl Pts',(53.1164423925447,29.7024883184289,23.7995));
#61677=CARTESIAN_POINT('Ctrl Pts',(53.0946595038619,29.6563380756085,23.7995));
#61678=CARTESIAN_POINT('Ctrl Pts',(53.0640455095737,29.5914778410146,23.7995));
#61679=CARTESIAN_POINT('Ctrl Pts',(53.037294163456,29.524890812006,23.7995));
#61680=CARTESIAN_POINT('Ctrl Pts',(53.0142981560509,29.456912722762,23.7995));
#61681=CARTESIAN_POINT('Ctrl Pts',(53.0009606170863,29.4174858606089,23.7995));
#61682=CARTESIAN_POINT('Ctrl Pts',(52.9888871151828,29.3775904012731,23.7995));
#61683=CARTESIAN_POINT('Ctrl Pts',(52.9780631887975,29.3372874974198,23.7995));
#61684=CARTESIAN_POINT('Ctrl Pts',(52.9745837243386,29.3243317070202,23.7995));
#61685=CARTESIAN_POINT('Ctrl Pts',(52.9712330997116,29.3113324732422,23.7995));
#61686=CARTESIAN_POINT('Ctrl Pts',(52.9680119647507,29.2982959373246,23.7995));
#61687=CARTESIAN_POINT('Ctrl Pts',(52.9500851274445,29.2257426723206,23.7995));
#61688=CARTESIAN_POINT('Ctrl Pts',(52.9362078481641,29.1522120659674,23.7995));
#61689=CARTESIAN_POINT('Ctrl Pts',(52.9262598407908,29.0780700769049,23.7995));
#61690=CARTESIAN_POINT('Ctrl Pts',(52.9178400915168,29.0153181171246,23.7995));
#61691=CARTESIAN_POINT('Ctrl Pts',(52.9122358150479,28.9521272587033,23.7995));
#61692=CARTESIAN_POINT('Ctrl Pts',(52.9093993969571,28.8887050743856,23.7995));
#61693=CARTESIAN_POINT('Ctrl Pts',(52.9080492667043,28.8585162210475,23.7995));
#61694=CARTESIAN_POINT('Ctrl Pts',(52.907326603863,28.8282748042801,23.7995));
#61695=CARTESIAN_POINT('Ctrl Pts',(52.9072281478651,28.7980025837903,23.7995));
#61696=CARTESIAN_POINT('Ctrl Pts',(52.9071800358105,28.7832095924427,23.7995));
#61697=CARTESIAN_POINT('Ctrl Pts',(52.9072810447628,28.7684067535663,23.7995));
#61698=CARTESIAN_POINT('Ctrl Pts',(52.9075307536315,28.7536046094758,23.7995));
#61699=CARTESIAN_POINT('Ctrl Pts',(52.9088393982126,28.6760312907818,23.7995));
#61700=CARTESIAN_POINT('Ctrl Pts',(52.9142236191172,28.5986682948975,23.7995));
#61701=CARTESIAN_POINT('Ctrl Pts',(52.9235643439375,28.5218879125633,23.7995));
#61702=CARTESIAN_POINT('Ctrl Pts',(52.9332602936395,28.4421875959892,23.7995));
#61703=CARTESIAN_POINT('Ctrl Pts',(52.9472190372289,28.3631140585917,23.7995));
#61704=CARTESIAN_POINT('Ctrl Pts',(52.9653613277415,28.2850644949545,23.7995));
#61705=CARTESIAN_POINT('Ctrl Pts',(52.9831194474831,28.2086676642516,23.7995));
#61706=CARTESIAN_POINT('Ctrl Pts',(53.0048859614684,28.1332507805631,23.7995));
#61707=CARTESIAN_POINT('Ctrl Pts',(53.0306380316024,28.0591843708784,23.7995));
#61708=CARTESIAN_POINT('Ctrl Pts',(53.0394167579217,28.0339355758613,23.7995));
#61709=CARTESIAN_POINT('Ctrl Pts',(53.0486590790892,28.0088437755125,23.7995));
#61710=CARTESIAN_POINT('Ctrl Pts',(53.0583654557726,27.983923948249,23.7995));
#61711=CARTESIAN_POINT('Ctrl Pts',(53.0630790096306,27.9718225275264,23.7995));
#61712=CARTESIAN_POINT('Ctrl Pts',(53.0679020080437,27.9597616651288,23.7995));
#61713=CARTESIAN_POINT('Ctrl Pts',(53.0728345632088,27.9477430987234,23.7995));
#61714=CARTESIAN_POINT('Ctrl Pts',(53.0780479523345,27.9350402578415,23.7995));
#61715=CARTESIAN_POINT('Ctrl Pts',(53.0833805561955,27.9223925031397,23.7995));
#61716=CARTESIAN_POINT('Ctrl Pts',(53.0888294627625,27.909807514102,23.7995));
#61717=CARTESIAN_POINT('Ctrl Pts',(53.1210151517875,27.8354702982651,23.7995));
#61718=CARTESIAN_POINT('Ctrl Pts',(53.1572806186558,27.7632594115094,23.7995));
#61719=CARTESIAN_POINT('Ctrl Pts',(53.1975435690432,27.6935631803969,23.7995));
#61720=CARTESIAN_POINT('Ctrl Pts',(53.2111784159906,27.6699609000155,23.7995));
#61721=CARTESIAN_POINT('Ctrl Pts',(53.2252721371432,27.6466469888357,23.7995));
#61722=CARTESIAN_POINT('Ctrl Pts',(53.2398228910682,27.6236366097474,23.7995));
#61723=CARTESIAN_POINT('Ctrl Pts',(53.2817577761606,27.5573213103493,23.7995));
#61724=CARTESIAN_POINT('Ctrl Pts',(53.3274848540066,27.4935254236365,23.7995));
#61725=CARTESIAN_POINT('Ctrl Pts',(53.3766655016659,27.4323469456169,23.7995));
#61726=CARTESIAN_POINT('Ctrl Pts',(53.4258461493252,27.3711684675974,23.7995));
#61727=CARTESIAN_POINT('Ctrl Pts',(53.4784810156533,27.3126068943904,23.7995000000001));
#61728=CARTESIAN_POINT('Ctrl Pts',(53.5342771578376,27.2567856770345,23.7995));
#61729=CARTESIAN_POINT('Ctrl Pts',(53.5477935777438,27.2432631827559,23.7995));
#61730=CARTESIAN_POINT('Ctrl Pts',(53.5615006180451,27.2298971458495,23.7995));
#61731=CARTESIAN_POINT('Ctrl Pts',(53.5753681819369,27.2167140140831,23.7995));
#61732=CARTESIAN_POINT('Ctrl Pts',(53.633752056695,27.1612116691885,23.7995));
#61733=CARTESIAN_POINT('Ctrl Pts',(53.6950394894952,27.108883136901,23.7995));
#61734=CARTESIAN_POINT('Ctrl Pts',(53.7588597602439,27.0598159162569,23.7995));
#61735=CARTESIAN_POINT('Ctrl Pts',(53.8246617759526,27.0092250618821,23.7995));
#61736=CARTESIAN_POINT('Ctrl Pts',(53.8931568786773,26.9621005359295,23.7995));
#61737=CARTESIAN_POINT('Ctrl Pts',(53.9639880369228,26.9185657891014,23.7995));
#61738=CARTESIAN_POINT('Ctrl Pts',(54.0348191951683,26.8750310422733,23.7995));
#61739=CARTESIAN_POINT('Ctrl Pts',(54.107987210922,26.8350855029082,23.7995));
#61740=CARTESIAN_POINT('Ctrl Pts',(54.1831732887653,26.7988889473287,23.7995));
#61741=CARTESIAN_POINT('Ctrl Pts',(54.2150841291888,26.7835262293614,23.7995));
#61742=CARTESIAN_POINT('Ctrl Pts',(54.2473588964334,26.7688393372961,23.7995));
#61743=CARTESIAN_POINT('Ctrl Pts',(54.279974752017,26.754842857782,23.7995));
#61744=CARTESIAN_POINT('Ctrl Pts',(54.2965159643313,26.7477445083702,23.7995));
#61745=CARTESIAN_POINT('Ctrl Pts',(54.313149574602,26.7408220047297,23.7995));
#61746=CARTESIAN_POINT('Ctrl Pts',(54.3298442609607,26.7340884936375,23.7995));
#61747=CARTESIAN_POINT('Ctrl Pts',(54.4093433274494,26.7020239292294,23.7995));
#61748=CARTESIAN_POINT('Ctrl Pts',(54.4903303509709,26.6741939381907,23.7995));
#61749=CARTESIAN_POINT('Ctrl Pts',(54.5724341788774,26.6507190230252,23.7995));
#61750=CARTESIAN_POINT('Ctrl Pts',(54.6544887625027,26.6272581876579,23.7995));
#61751=CARTESIAN_POINT('Ctrl Pts',(54.7376596641008,26.6081466518036,23.7995));
#61752=CARTESIAN_POINT('Ctrl Pts',(54.8216091428745,26.5935443949621,23.7995));
#61753=CARTESIAN_POINT('Ctrl Pts',(54.9045672100692,26.5791145852487,23.7995));
#61754=CARTESIAN_POINT('Ctrl Pts',(54.9882864392925,26.5690877150561,23.7995));
#61755=CARTESIAN_POINT('Ctrl Pts',(55.0724600567375,26.5636643588097,23.7995));
#61756=CARTESIAN_POINT('Ctrl Pts',(55.1197647546895,26.5606164889794,23.7995));
#61757=CARTESIAN_POINT('Ctrl Pts',(55.167213237544,26.5590234297658,23.7995));
#61758=CARTESIAN_POINT('Ctrl Pts',(55.2147522011135,26.5589281571169,23.7995));
#61759=CARTESIAN_POINT('Origin',(55.,29.,23.7995));
#61760=CARTESIAN_POINT('Ctrl Pts',(54.1264195366494,30.7893316856308,4.66531914574752));
#61761=CARTESIAN_POINT('Ctrl Pts',(53.5328852721049,30.4995587262633,4.707553422536));
#61762=CARTESIAN_POINT('Ctrl Pts',(52.6669803260193,29.287877577452,4.79202197611296));
#61763=CARTESIAN_POINT('Ctrl Pts',(53.4895592866451,27.1957792326284,4.91872480647843));
#61764=CARTESIAN_POINT('Ctrl Pts',(55.6906360859252,26.7527320219417,5.04542763684387));
#61765=CARTESIAN_POINT('Ctrl Pts',(57.2612985360137,28.3549210763986,5.17213046720934));
#61766=CARTESIAN_POINT('Ctrl Pts',(56.7720339725362,30.5461560293319,5.29883329757478));
#61767=CARTESIAN_POINT('Ctrl Pts',(54.6678069104706,31.3278986568886,5.42553612794023));
#61768=CARTESIAN_POINT('Ctrl Pts',(52.8664205998243,29.9887889527256,5.55223895830568));
#61769=CARTESIAN_POINT('Ctrl Pts',(53.009073421732,27.7485304409038,5.67894178867113));
#61770=CARTESIAN_POINT('Ctrl Pts',(54.9658935874079,26.648693626069,5.80564461903658));
#61771=CARTESIAN_POINT('Ctrl Pts',(56.9537719413826,27.6913201942627,5.93234744940203));
#61772=CARTESIAN_POINT('Ctrl Pts',(57.1613864127378,29.9264357302167,6.05905027976748));
#61773=CARTESIAN_POINT('Ctrl Pts',(55.3995439881701,31.317373277448,6.18575311013294));
#61774=CARTESIAN_POINT('Ctrl Pts',(53.2736403188764,30.5967297689046,6.31245594049839));
#61775=CARTESIAN_POINT('Ctrl Pts',(52.720791484149,28.4211457420414,6.43915877086384));
#61776=CARTESIAN_POINT('Ctrl Pts',(54.2447544488578,26.7730142754301,6.56586160122929));
#61777=CARTESIAN_POINT('Ctrl Pts',(56.4568955974548,27.1541078477562,6.69256443159474));
#61778=CARTESIAN_POINT('Ctrl Pts',(57.3415160026948,29.2171757615622,6.8192672619602));
#61779=CARTESIAN_POINT('Ctrl Pts',(56.0925507123657,31.0823532731961,6.94597009232564));
#61780=CARTESIAN_POINT('Ctrl Pts',(53.848055020457,31.0500939414026,7.0726729226911));
#61781=CARTESIAN_POINT('Ctrl Pts',(52.6532097130149,29.1497922643776,7.19937575305655));
#61782=CARTESIAN_POINT('Ctrl Pts',(53.5967559427171,27.113000143957,7.32607858342201));
#61783=CARTESIAN_POINT('Ctrl Pts',(55.8189358885639,26.7956392360687,7.45278141378746));
#61784=CARTESIAN_POINT('Ctrl Pts',(57.2949027764116,28.4868883085401,7.5794842441529));
#61785=CARTESIAN_POINT('Ctrl Pts',(56.6797579534097,30.64568392336,7.70618707451836));
#61786=CARTESIAN_POINT('Ctrl Pts',(54.5340203927282,31.3049350027155,7.83288990488381));
#61787=CARTESIAN_POINT('Ctrl Pts',(52.8128826983748,29.8639330234614,7.95959273524927));
#61788=CARTESIAN_POINT('Ctrl Pts',(53.0846427626806,27.6357166668124,8.08629556561471));
#61789=CARTESIAN_POINT('Ctrl Pts',(55.1016732529539,26.6506330831788,8.21299839598018));
#61790=CARTESIAN_POINT('Ctrl Pts',(57.0260592391414,27.8062888458497,8.3397012263456));
#61791=CARTESIAN_POINT('Ctrl Pts',(57.1043033136765,30.0496522872255,8.46640405671108));
#61792=CARTESIAN_POINT('Ctrl Pts',(55.2651096020556,31.3365742571087,8.59310688707651));
#61793=CARTESIAN_POINT('Ctrl Pts',(53.1843484485316,30.4944135316941,8.71980971744197));
#61794=CARTESIAN_POINT('Ctrl Pts',(52.758006060917,28.2905456059944,8.84651254780742));
#61795=CARTESIAN_POINT('Ctrl Pts',(54.3745649353107,26.7331313800921,8.97321537817288));
#61796=CARTESIAN_POINT('Ctrl Pts',(56.5610192321176,27.2412841852587,9.09991820853831));
#61797=CARTESIAN_POINT('Ctrl Pts',(57.3250753218085,29.3519760048347,9.22662103890378));
#61798=CARTESIAN_POINT('Ctrl Pts',(55.9705265275212,31.1419478563778,9.35332386926922));
#61799=CARTESIAN_POINT('Ctrl Pts',(53.7316355263593,30.9801802751439,9.48002669963468));
#61800=CARTESIAN_POINT('Ctrl Pts',(52.6484761883034,29.014075620299,9.60672953000012));
#61801=CARTESIAN_POINT('Ctrl Pts',(53.708021555563,27.0351452829349,9.73343236036558));
#61802=CARTESIAN_POINT('Ctrl Pts',(55.9448155980397,26.8465873953736,9.86013519073104));
#61803=CARTESIAN_POINT('Ctrl Pts',(57.3206951911261,28.6202156007059,9.98683802109648));
#61804=CARTESIAN_POINT('Ctrl Pts',(56.5819610682486,30.7399027382612,10.1135408514619));
#61805=CARTESIAN_POINT('Ctrl Pts',(54.4017465709424,31.2741933063581,10.2402436818274));
#61806=CARTESIAN_POINT('Ctrl Pts',(52.766659633492,29.7362426009061,10.3669465121928));
#61807=CARTESIAN_POINT('Ctrl Pts',(53.1665888366757,27.5274288247217,10.4936493425583));
#61808=CARTESIAN_POINT('Ctrl Pts',(55.2371193354502,26.6604195288858,10.6203521729237));
#61809=CARTESIAN_POINT('Ctrl Pts',(57.0915870781246,27.925232185686,10.7470550032892));
#61810=CARTESIAN_POINT('Ctrl Pts',(57.0402040479584,30.1693715417937,10.8737578336547));
#61811=CARTESIAN_POINT('Ctrl Pts',(55.1297903791825,31.3479814346657,11.0004606640201));
#61812=CARTESIAN_POINT('Ctrl Pts',(53.1011119261864,30.3871144304603,11.1271634943856));
#61813=CARTESIAN_POINT('Ctrl Pts',(52.8026972240355,28.162310993983,11.253866324751));
#61814=CARTESIAN_POINT('Ctrl Pts',(54.5064612681272,26.7008084289898,11.3805691551165));
#61815=CARTESIAN_POINT('Ctrl Pts',(56.6599370088555,27.3343255159861,11.5072719854819));
#61816=CARTESIAN_POINT('Ctrl Pts',(57.3008808238125,29.485602506866,11.6339748158474));
#61817=CARTESIAN_POINT('Ctrl Pts',(55.8452657423508,31.1943992765382,11.7606776462128));
#61818=CARTESIAN_POINT('Ctrl Pts',(53.6194458794751,30.9036629639631,11.8873804765783));
#61819=CARTESIAN_POINT('Ctrl Pts',(52.6515847050371,28.8783120283382,12.0140833069437));
#61820=CARTESIAN_POINT('Ctrl Pts',(53.8235957604794,26.9638429762661,12.1407861373092));
#61821=CARTESIAN_POINT('Ctrl Pts',(56.0675444619859,26.9047169208562,12.2674889676746));
#61822=CARTESIAN_POINT('Ctrl Pts',(57.3387483711783,28.7548094284558,12.3941917980401));
#61823=CARTESIAN_POINT('Ctrl Pts',(56.4788885358544,30.8283191894692,12.5208946284055));
#61824=CARTESIAN_POINT('Ctrl Pts',(54.2714678514121,31.2358674532577,12.647597458771));
#61825=CARTESIAN_POINT('Ctrl Pts',(52.7278844859831,29.6060968990407,12.7743002891364));
#61826=CARTESIAN_POINT('Ctrl Pts',(53.2546491130723,27.4240518277673,12.9010031195019));
#61827=CARTESIAN_POINT('Ctrl Pts',(55.3717746538996,26.6780081897687,13.0277059498673));
#61828=CARTESIAN_POINT('Ctrl Pts',(57.1501397295913,28.0477597449719,13.1544087802328));
#61829=CARTESIAN_POINT('Ctrl Pts',(56.9693009508439,30.2851910850408,13.2811116105982));
#61830=CARTESIAN_POINT('Ctrl Pts',(54.9940383212441,31.3515583808295,13.4078144409637));
#61831=CARTESIAN_POINT('Ctrl Pts',(53.0242079637134,30.2751894719645,13.5345172713291));
#61832=CARTESIAN_POINT('Ctrl Pts',(52.8547161236231,28.0368699725265,13.6612201016946));
#61833=CARTESIAN_POINT('Ctrl Pts',(54.6400034923536,26.6761530010465,13.7879229320601));
#61834=CARTESIAN_POINT('Ctrl Pts',(56.7533190983459,27.4329216677402,13.9146257624255));
#61835=CARTESIAN_POINT('Ctrl Pts',(57.2690131692052,29.6176095838284,14.041328592791));
#61836=CARTESIAN_POINT('Ctrl Pts',(55.7171860991359,31.2395326430462,14.1680314231564));
#61837=CARTESIAN_POINT('Ctrl Pts',(53.5118602120182,30.8207971692334,14.2947342535218));
#61838=CARTESIAN_POINT('Ctrl Pts',(52.6625249000395,28.742954250905,14.4214370838873));
#61839=CARTESIAN_POINT('Ctrl Pts',(53.9430931298965,26.899331004658,14.5481399142527));
#61840=CARTESIAN_POINT('Ctrl Pts',(56.186713195498,26.9698339595752,14.6748427446182));
#61841=CARTESIAN_POINT('Ctrl Pts',(57.349002110972,28.890220936824,14.8015455749836));
#61842=CARTESIAN_POINT('Ctrl Pts',(56.3708840907646,30.9106384194169,14.9282484053491));
#61843=CARTESIAN_POINT('Ctrl Pts',(54.1436186976438,31.1900852551985,15.0549512357145));
#61844=CARTESIAN_POINT('Ctrl Pts',(52.6966865662897,29.4739299380211,15.18165406608));
#61845=CARTESIAN_POINT('Ctrl Pts',(53.3485299215708,27.325930425545,15.3083568964455));
#61846=CARTESIAN_POINT('Ctrl Pts',(55.5051901492716,26.7033404098252,15.4350597268109));
#61847=CARTESIAN_POINT('Ctrl Pts',(57.2015219275906,28.1734629092404,15.5617625571764));
#61848=CARTESIAN_POINT('Ctrl Pts',(56.8918304755086,30.39672467294,15.6884653875418));
#61849=CARTESIAN_POINT('Ctrl Pts',(54.8583061447766,31.3472931669169,15.8151682179073));
#61850=CARTESIAN_POINT('Ctrl Pts',(52.9538930264383,30.1590119122794,15.9418710482727));
#61851=CARTESIAN_POINT('Ctrl Pts',(52.913889283001,27.9146408721142,16.0685738786382));
#61852=CARTESIAN_POINT('Ctrl Pts',(54.7747462609773,26.6592473191046,16.1952767090036));
#61853=CARTESIAN_POINT('Ctrl Pts',(56.8408540827227,27.5367438343933,16.3219795393691));
#61854=CARTESIAN_POINT('Ctrl Pts',(57.2295786327234,29.7475570082386,16.4486823697345));
#61855=CARTESIAN_POINT('Ctrl Pts',(55.5867147278486,31.2771974416349,16.5753852000999));
#61856=CARTESIAN_POINT('Ctrl Pts',(53.4092373090532,30.7318592382624,16.7020880304655));
#61857=CARTESIAN_POINT('Ctrl Pts',(52.6812602890962,28.6084536896598,16.8287908608308));
#61858=CARTESIAN_POINT('Ctrl Pts',(54.0661151546778,26.8418245076593,16.9554936911964));
#61859=CARTESIAN_POINT('Ctrl Pts',(56.3019243853996,27.041721354157,17.0821965215618));
#61860=CARTESIAN_POINT('Ctrl Pts',(57.3514222155374,29.0259985449642,17.2088993519273));
#61861=CARTESIAN_POINT('Ctrl Pts',(56.2583079146159,30.9865859035235,17.3356021822927));
#61862=CARTESIAN_POINT('Ctrl Pts',(54.0186254709554,31.1369993902211,17.4623050126582));
#61863=CARTESIAN_POINT('Ctrl Pts',(52.6731699156649,29.3401824785247,17.5890078430236));
#61864=CARTESIAN_POINT('Ctrl Pts',(53.4479181811372,27.2333918409509,17.715710673389));
#61865=CARTESIAN_POINT('Ctrl Pts',(55.6369208971794,26.7363317091943,17.8424135037545));
#61866=CARTESIAN_POINT('Ctrl Pts',(57.2455623187654,28.3019224737871,17.9691163341199));
#61867=CARTESIAN_POINT('Ctrl Pts',(56.8080509765289,30.5036003545943,18.0958191644854));
#61868=CARTESIAN_POINT('Ctrl Pts',(54.7230465000152,31.3352000168956,18.2225219948509));
#61869=CARTESIAN_POINT('Ctrl Pts',(52.890401606092,30.0389691893815,18.3492248252163));
#61870=CARTESIAN_POINT('Ctrl Pts',(52.9800193669072,27.7960313118718,18.4759276555818));
#61871=CARTESIAN_POINT('Ctrl Pts',(54.9102402233175,26.650147761549,18.6026304859472));
#61872=CARTESIAN_POINT('Ctrl Pts',(56.9222500435006,27.645445781696,18.7293333163127));
#61873=CARTESIAN_POINT('Ctrl Pts',(57.1827087237314,29.8750114213024,18.8560361466781));
#61874=CARTESIAN_POINT('Ctrl Pts',(55.4542867345813,31.3072680648001,18.9827389770436));
#61875=CARTESIAN_POINT('Ctrl Pts',(53.3119194054314,30.6371457681906,19.109441807409));
#61876=CARTESIAN_POINT('Ctrl Pts',(52.7077283919724,28.4752588875521,19.2361446377745));
#61877=CARTESIAN_POINT('Ctrl Pts',(54.1922515713913,26.7915152624158,19.3628474681399));
#61878=CARTESIAN_POINT('Ctrl Pts',(56.4127938164408,27.1201393689178,19.4895502985054));
#61879=CARTESIAN_POINT('Ctrl Pts',(57.3460006141201,29.1616894511321,19.6162531288708));
#61880=CARTESIAN_POINT('Ctrl Pts',(56.1415354352125,31.0559083662008,19.7429559592363));
#61881=CARTESIAN_POINT('Ctrl Pts',(53.8969050084927,31.0767868932071,19.8696587896017));
#61882=CARTESIAN_POINT('Ctrl Pts',(52.6574129592736,29.2053005519918,19.9963616199672));
#61883=CARTESIAN_POINT('Ctrl Pts',(53.5524824440479,27.1467446788788,20.1230644503326));
#61884=CARTESIAN_POINT('Ctrl Pts',(55.7665275916892,26.7768720658948,20.2497672806981));
#61885=CARTESIAN_POINT('Ctrl Pts',(57.2821140337366,28.4327100416997,20.3764701110635));
#61886=CARTESIAN_POINT('Ctrl Pts',(56.7182418484071,30.6054617125546,20.503172941429));
#61887=CARTESIAN_POINT('Ctrl Pts',(54.5887104611592,31.3153192601402,20.6298757717944));
#61888=CARTESIAN_POINT('Ctrl Pts',(52.8339454392039,29.9154616307104,20.7565786021598));
#61889=CARTESIAN_POINT('Ctrl Pts',(53.0528858388122,27.681436840953,20.8832814325254));
#61890=CARTESIAN_POINT('Ctrl Pts',(55.0460335250711,26.6488846728187,21.0099842628908));
#61891=CARTESIAN_POINT('Ctrl Pts',(56.9972355321144,27.7586650048169,21.1366870932563));
#61892=CARTESIAN_POINT('Ctrl Pts',(57.1285597534825,29.99954777245,21.2633899236217));
#61893=CARTESIAN_POINT('Ctrl Pts',(55.3203437390977,31.3296442417868,21.3900927539872));
#61894=CARTESIAN_POINT('Ctrl Pts',(53.2202310668697,30.5369725951186,21.5167955843526));
#61895=CARTESIAN_POINT('Ctrl Pts',(52.7418408968943,28.343814075626,21.643498414718));
#61896=CARTESIAN_POINT('Ctrl Pts',(54.3210818164914,26.7485709605453,21.7702012450835));
#61897=CARTESIAN_POINT('Ctrl Pts',(56.518951584052,27.2048266531433,21.8969040754489));
#61898=CARTESIAN_POINT('Ctrl Pts',(57.3327557174393,29.2968408217187,22.0236069058144));
#61899=CARTESIAN_POINT('Ctrl Pts',(56.0209554270959,31.1183752546229,22.1503097361798));
#61900=CARTESIAN_POINT('Ctrl Pts',(53.7788645019832,31.0096473324931,22.2770125665453));
#61901=CARTESIAN_POINT('Ctrl Pts',(52.6494657578868,29.0697363896565,22.4037153969107));
#61902=CARTESIAN_POINT('Ctrl Pts',(53.6618788749301,27.0662731610901,22.5304182272762));
#61903=CARTESIAN_POINT('Ctrl Pts',(55.8935684586045,26.8248355645479,22.6571210576416));
#61904=CARTESIAN_POINT('Ctrl Pts',(57.3110738969302,28.565371261504,22.7838238880071));
#61905=CARTESIAN_POINT('Ctrl Pts',(56.6226659052376,30.7020047032443,22.9105267183726));
#61906=CARTESIAN_POINT('Ctrl Pts',(54.4558179268847,31.2876473235127,23.037229548738));
#61907=CARTESIAN_POINT('Ctrl Pts',(52.7845718724283,29.7890380715951,23.1639323791035));
#61908=CARTESIAN_POINT('Ctrl Pts',(53.1325219577503,27.5709710820395,23.2906352094689));
#61909=CARTESIAN_POINT('Ctrl Pts',(55.1811312054231,26.6559899627326,23.4173380398344));
#61910=CARTESIAN_POINT('Ctrl Pts',(57.0666303447483,27.8749743362302,23.5440408701998));
#61911=CARTESIAN_POINT('Ctrl Pts',(57.065134231683,30.1232847911398,23.6707611309521));
#61912=CARTESIAN_POINT('Ctrl Pts',(55.8148535333292,30.9332788394173,23.7552471149158));
#61913=CARTESIAN_POINT('Ctrl Pts',(55.1561153962245,30.9850638875332,23.7974988220912));
#61914=CARTESIAN_POINT('Ctrl Pts',(54.0587888680759,30.9278577897226,4.75431987392162));
#61915=CARTESIAN_POINT('Ctrl Pts',(53.4193044926757,30.6156512483342,4.7965541507101));
#61916=CARTESIAN_POINT('Ctrl Pts',(52.4863630995982,29.3101644231945,4.88102270428707));
#61917=CARTESIAN_POINT('Ctrl Pts',(53.3726243051861,27.0561004487379,5.00772553465252));
#61918=CARTESIAN_POINT('Ctrl Pts',(55.7441036051655,26.5787535022794,5.13442836501797));
#61919=CARTESIAN_POINT('Ctrl Pts',(57.4363632704608,28.3049804919693,5.26113119538342));
#61920=CARTESIAN_POINT('Ctrl Pts',(56.909220925914,30.665856011611,5.38783402574887));
#61921=CARTESIAN_POINT('Ctrl Pts',(54.6420892557349,31.5081194254857,5.51453685611433));
#61922=CARTESIAN_POINT('Ctrl Pts',(52.7012435985727,30.0653388078979,5.64123968647978));
#61923=CARTESIAN_POINT('Ctrl Pts',(52.8549402866429,27.6516444337965,5.76794251684523));
#61924=CARTESIAN_POINT('Ctrl Pts',(54.9632531443315,26.4666606837572,5.89464534721069));
#61925=CARTESIAN_POINT('Ctrl Pts',(57.105028646608,27.5900050963139,6.02134817757613));
#61926=CARTESIAN_POINT('Ctrl Pts',(57.3287161714393,29.9981583367233,6.14805100794159));
#61927=CARTESIAN_POINT('Ctrl Pts',(55.4304758006111,31.4967791944333,6.27475383830703));
#61928=CARTESIAN_POINT('Ctrl Pts',(53.1399893681846,30.7203450583168,6.4014566686725));
#61929=CARTESIAN_POINT('Ctrl Pts',(52.54434019865,28.3763321248479,6.52815949903794));
#61930=CARTESIAN_POINT('Ctrl Pts',(54.1862850076286,26.6006059630024,6.65486232940339));
#61931=CARTESIAN_POINT('Ctrl Pts',(56.5696852343928,27.0112029573562,6.78156515976885));
#61932=CARTESIAN_POINT('Ctrl Pts',(57.5227909961055,29.2339890289928,6.90826799013429));
#61933=CARTESIAN_POINT('Ctrl Pts',(56.1771335736217,31.2435644609235,7.03497082049975));
#61934=CARTESIAN_POINT('Ctrl Pts',(53.7588739863169,31.2088076829662,7.16167365086519));
#61935=CARTESIAN_POINT('Ctrl Pts',(52.4715263961725,29.1613888503957,7.28837648123066));
#61936=CARTESIAN_POINT('Ctrl Pts',(53.4881198894316,26.9669127859905,7.4150793115961));
#61937=CARTESIAN_POINT('Ctrl Pts',(55.8823360949398,26.6249824980852,7.54178214196155));
#61938=CARTESIAN_POINT('Ctrl Pts',(57.4725690768737,28.4471643355324,7.66848497232701));
#61939=CARTESIAN_POINT('Ctrl Pts',(56.8098011013468,30.7730891352056,7.79518780269245));
#61940=CARTESIAN_POINT('Ctrl Pts',(54.4979452815009,31.4833779759637,7.92189063305792));
#61941=CARTESIAN_POINT('Ctrl Pts',(52.6435609111293,29.9308168085626,8.04859346342335));
#61942=CARTESIAN_POINT('Ctrl Pts',(52.9363600389347,27.5300968666704,8.17529629378881));
#61943=CARTESIAN_POINT('Ctrl Pts',(55.1095445714663,26.4687502893497,8.30199912415426));
#61944=CARTESIAN_POINT('Ctrl Pts',(57.1829122671806,27.7138743667884,8.42870195451973));
#61945=CARTESIAN_POINT('Ctrl Pts',(57.2672138250211,30.1309140472269,8.55540478488516));
#61946=CARTESIAN_POINT('Ctrl Pts',(55.2856338014677,31.5174666714988,8.68210761525061));
#61947=CARTESIAN_POINT('Ctrl Pts',(53.0437847186021,30.6101077241741,8.80881044561607));
#61948=CARTESIAN_POINT('Ctrl Pts',(52.5844358456948,28.2356212149373,8.93551327598151));
#61949=CARTESIAN_POINT('Ctrl Pts',(54.326145135019,26.5576354220616,9.06221610634698));
#61950=CARTESIAN_POINT('Ctrl Pts',(56.681869890704,27.1051282942199,9.18891893671242));
#61951=CARTESIAN_POINT('Ctrl Pts',(57.5050775140442,29.3792252091466,9.31562176707788));
#61952=CARTESIAN_POINT('Ctrl Pts',(56.0456625461001,31.3077727250115,9.44232459744333));
#61953=CARTESIAN_POINT('Ctrl Pts',(53.6334415523114,31.133481455198,9.56902742780878));
#61954=CARTESIAN_POINT('Ctrl Pts',(52.4664264124404,29.0151653237108,9.69573025817422));
#61955=CARTESIAN_POINT('Ctrl Pts',(53.6079994400906,26.8830305737127,9.82243308853968));
#61956=CARTESIAN_POINT('Ctrl Pts',(56.0179611332878,26.6798749512714,9.94913591890513));
#61957=CARTESIAN_POINT('Ctrl Pts',(57.5003582833259,28.5908135319605,10.0758387492706));
#61958=CARTESIAN_POINT('Ctrl Pts',(56.7044329974998,30.8746021625019,10.202541579636));
#61959=CARTESIAN_POINT('Ctrl Pts',(54.355431112801,31.4502563254235,10.3292444100015));
#61960=CARTESIAN_POINT('Ctrl Pts',(52.5937593587313,29.7932408757307,10.4559472403669));
#61961=CARTESIAN_POINT('Ctrl Pts',(53.0246501968509,27.4134256191966,10.5826500707324));
#61962=CARTESIAN_POINT('Ctrl Pts',(55.2554765902893,26.4792943800521,10.7093529010978));
#61963=CARTESIAN_POINT('Ctrl Pts',(57.2535131266198,27.842026037091,10.8360557314633));
#61964=CARTESIAN_POINT('Ctrl Pts',(57.1981521358314,30.2599017018651,10.9627585618287));
#61965=CARTESIAN_POINT('Ctrl Pts',(55.1398384634595,31.5297569675287,11.0894613921942));
#61966=CARTESIAN_POINT('Ctrl Pts',(52.9541042086769,30.494501763689,11.2161642225596));
#61967=CARTESIAN_POINT('Ctrl Pts',(52.6325868998799,28.0974589627044,11.3428670529251));
#61968=CARTESIAN_POINT('Ctrl Pts',(54.468252590388,26.5228100995293,11.4695698832905));
#61969=CARTESIAN_POINT('Ctrl Pts',(56.7884456630761,27.2053726791204,11.596272713656));
#61970=CARTESIAN_POINT('Ctrl Pts',(57.4790099314911,29.5231967796068,11.7229755440215));
#61971=CARTESIAN_POINT('Ctrl Pts',(55.9107043478092,31.3642848181859,11.8496783743869));
#61972=CARTESIAN_POINT('Ctrl Pts',(53.5125664309413,31.0510403429139,11.9763812047524));
#61973=CARTESIAN_POINT('Ctrl Pts',(52.4697755836688,28.8688912145425,12.1030840351178));
#61974=CARTESIAN_POINT('Ctrl Pts',(53.7325211444948,26.8062082000632,12.2297868654833));
#61975=CARTESIAN_POINT('Ctrl Pts',(56.1501913946096,26.7425047361315,12.3564896958487));
#61976=CARTESIAN_POINT('Ctrl Pts',(57.5198091006742,28.7358273163583,12.4831925262142));
#61977=CARTESIAN_POINT('Ctrl Pts',(56.5933808174717,30.9698636199331,12.6098953565796));
#61978=CARTESIAN_POINT('Ctrl Pts',(54.2150665027632,31.4089633694888,12.7365981869451));
#61979=CARTESIAN_POINT('Ctrl Pts',(52.5519823250081,29.6530195812916,12.8633010173105));
#61980=CARTESIAN_POINT('Ctrl Pts',(53.1195279052041,27.3020454036351,12.990003847676));
#61981=CARTESIAN_POINT('Ctrl Pts',(55.4005566258606,26.4982447161838,13.1167066780414));
#61982=CARTESIAN_POINT('Ctrl Pts',(57.3165987949426,27.9740394091908,13.2434095084069));
#61983=CARTESIAN_POINT('Ctrl Pts',(57.1217598776575,30.384687738151,13.3701123387723));
#61984=CARTESIAN_POINT('Ctrl Pts',(54.9935767812522,31.5336108329584,13.4968151691378));
#61985=CARTESIAN_POINT('Ctrl Pts',(52.8712465114121,30.3739118222972,13.6235179995032));
#61986=CARTESIAN_POINT('Ctrl Pts',(52.6886329876949,27.9623065746326,13.7502208298687));
#61987=CARTESIAN_POINT('Ctrl Pts',(54.6121333584417,26.4962459028513,13.8769236602341));
#61988=CARTESIAN_POINT('Ctrl Pts',(56.8890571875299,27.3116019270135,14.0036264905996));
#61989=CARTESIAN_POINT('Ctrl Pts',(57.444675153502,29.6654235526888,14.1303293209651));
#61990=CARTESIAN_POINT('Ctrl Pts',(55.7727090617147,31.4129123101694,14.2570321513305));
#61991=CARTESIAN_POINT('Ctrl Pts',(53.3966517189094,30.9617592615168,14.3837349816959));
#61992=CARTESIAN_POINT('Ctrl Pts',(52.4815627443869,28.7230543371655,14.5104378120614));
#61993=CARTESIAN_POINT('Ctrl Pts',(53.8612697361237,26.7367018542058,14.6371406424268));
#61994=CARTESIAN_POINT('Ctrl Pts',(56.2785859080682,26.8126629920581,14.7638434727923));
#61995=CARTESIAN_POINT('Ctrl Pts',(57.5308566623387,28.8817220844006,14.8905463031577));
#61996=CARTESIAN_POINT('Ctrl Pts',(56.4770149069683,31.0585558227109,15.0172491335232));
#61997=CARTESIAN_POINT('Ctrl Pts',(54.0773195500988,31.3596368148496,15.1439519638886));
#61998=CARTESIAN_POINT('Ctrl Pts',(52.5183691313298,29.5106205462822,15.2706547942541));
#61999=CARTESIAN_POINT('Ctrl Pts',(53.2206767583889,27.1963276593334,15.3973576246195));
#62000=CARTESIAN_POINT('Ctrl Pts',(55.5443008539925,26.5255381007245,15.524060454985));
#62001=CARTESIAN_POINT('Ctrl Pts',(57.3719588891393,28.1094742345918,15.6507632853505));
#62002=CARTESIAN_POINT('Ctrl Pts',(57.0382918093569,30.5048560098996,15.7774661157159));
#62003=CARTESIAN_POINT('Ctrl Pts',(54.8473365196951,31.5290154156122,15.9041689460814));
#62004=CARTESIAN_POINT('Ctrl Pts',(52.7954879471124,30.2487400527318,16.0308717764468));
#62005=CARTESIAN_POINT('Ctrl Pts',(52.7523872022796,27.8306147674328,16.1575746068123));
#62006=CARTESIAN_POINT('Ctrl Pts',(54.7573076143868,26.4780314203805,16.2842774371777));
#62007=CARTESIAN_POINT('Ctrl Pts',(56.9833689369161,27.4234617763278,16.4109802675432));
#62008=CARTESIAN_POINT('Ctrl Pts',(57.402187682369,29.8054312194704,16.5376830979086));
#62009=CARTESIAN_POINT('Ctrl Pts',(55.6321368852467,31.4534930342133,16.6643859282741));
#62010=CARTESIAN_POINT('Ctrl Pts',(53.2860839776272,30.865935952512,16.7910887586395));
#62011=CARTESIAN_POINT('Ctrl Pts',(52.501748585853,28.578141039759,16.917791589005));
#62012=CARTESIAN_POINT('Ctrl Pts',(53.9938158541446,26.6747433313176,17.0444944193704));
#62013=CARTESIAN_POINT('Ctrl Pts',(56.4027164936376,26.8901157498337,17.1711972497359));
#62014=CARTESIAN_POINT('Ctrl Pts',(57.5334641260503,29.0280112948501,17.2979000801013));
#62015=CARTESIAN_POINT('Ctrl Pts',(56.3557233320924,31.1403829931681,17.4246029104668));
#62016=CARTESIAN_POINT('Ctrl Pts',(53.9426496240763,31.3024411595428,17.5513057408322));
#62017=CARTESIAN_POINT('Ctrl Pts',(52.4930318735928,29.3665186540973,17.6780085711977));
#62018=CARTESIAN_POINT('Ctrl Pts',(53.3277594373305,27.0966249420605,17.8047114015631));
#62019=CARTESIAN_POINT('Ctrl Pts',(55.686229905235,26.5610835135692,17.9314142319286));
#62020=CARTESIAN_POINT('Ctrl Pts',(57.4194087900553,28.2478788546879,18.058117062294));
#62021=CARTESIAN_POINT('Ctrl Pts',(56.9480262867464,30.6200057705973,18.1848198926595));
#62022=CARTESIAN_POINT('Ctrl Pts',(54.7016053722045,31.5159860406461,18.3115227230249));
#62023=CARTESIAN_POINT('Ctrl Pts',(52.7270811613398,30.1194038875609,18.4382255533904));
#62024=CARTESIAN_POINT('Ctrl Pts',(52.8236369311127,27.7028227172024,18.5649283837558));
#62025=CARTESIAN_POINT('Ctrl Pts',(54.9032912198053,26.468227395192,18.6916312141213));
#62026=CARTESIAN_POINT('Ctrl Pts',(57.0710663930656,27.5405791881239,18.8183340444868));
#62027=CARTESIAN_POINT('Ctrl Pts',(57.3516892086208,29.9427528714775,18.9450368748522));
#62028=CARTESIAN_POINT('Ctrl Pts',(55.48945660945,31.4858916585581,19.0717397052177));
#62029=CARTESIAN_POINT('Ctrl Pts',(53.1812319370115,30.7638899749351,19.1984425355831));
#62030=CARTESIAN_POINT('Ctrl Pts',(52.5302657907506,28.4346345904763,19.3251453659486));
#62031=CARTESIAN_POINT('Ctrl Pts',(54.1297174734372,26.6205392555073,19.451848196314));
#62032=CARTESIAN_POINT('Ctrl Pts',(56.5221691909721,26.9746047139677,19.5785510266795));
#62033=CARTESIAN_POINT('Ctrl Pts',(57.5276227962348,29.1742070910521,19.7052538570449));
#62034=CARTESIAN_POINT('Ctrl Pts',(56.229910585439,31.2150722476805,19.8319566874103));
#62035=CARTESIAN_POINT('Ctrl Pts',(53.8115058324518,31.2375671440993,19.9586595177758));
#62036=CARTESIAN_POINT('Ctrl Pts',(52.4760550484659,29.2211944669454,20.0853623481413));
#62037=CARTESIAN_POINT('Ctrl Pts',(53.4404188343545,27.0032697482195,20.2120651785067));
#62038=CARTESIAN_POINT('Ctrl Pts',(55.8258704635605,26.6047624150779,20.3387680088722));
#62039=CARTESIAN_POINT('Ctrl Pts',(57.4587902580083,28.3887917070251,20.4654708392376));
#62040=CARTESIAN_POINT('Ctrl Pts',(56.8512643344329,30.7297530097437,20.5921736696031));
#62041=CARTESIAN_POINT('Ctrl Pts',(54.5568693341469,31.4945661596456,20.7188764999685));
#62042=CARTESIAN_POINT('Ctrl Pts',(52.6662542827978,29.9863346466896,20.845579330334));
#62043=CARTESIAN_POINT('Ctrl Pts',(52.9021445642136,27.5793565956363,20.9722821606994));
#62044=CARTESIAN_POINT('Ctrl Pts',(55.0495973388329,26.4668665209239,21.0989849910649));
#62045=CARTESIAN_POINT('Ctrl Pts',(57.1518570924653,27.6625635932472,21.2256878214303));
#62046=CARTESIAN_POINT('Ctrl Pts',(57.2933481447822,30.0769305516647,21.3523906517957));
#62047=CARTESIAN_POINT('Ctrl Pts',(55.3451440433139,31.5100001497084,21.4790934821613));
#62048=CARTESIAN_POINT('Ctrl Pts',(53.0824452899396,30.6559616162193,21.6057963125266));
#62049=CARTESIAN_POINT('Ctrl Pts',(52.5670192104037,28.293013611747,21.7324991428922));
#62050=CARTESIAN_POINT('Ctrl Pts',(54.268521471356,26.574270300707,21.8592019732576));
#62051=CARTESIAN_POINT('Ctrl Pts',(56.6365454583084,27.0658483005513,21.985904803623));
#62052=CARTESIAN_POINT('Ctrl Pts',(57.5133525089284,29.3198215820206,22.1126076339885));
#62053=CARTESIAN_POINT('Ctrl Pts',(56.0999955396154,31.282375184532,22.2393104643539));
#62054=CARTESIAN_POINT('Ctrl Pts',(53.6843268908365,31.1652297869952,22.3660132947194));
#62055=CARTESIAN_POINT('Ctrl Pts',(52.4674925923137,29.0751352268033,22.4927161250848));
#62056=CARTESIAN_POINT('Ctrl Pts',(53.5582844951136,26.916568303392,22.6194189554503));
#62057=CARTESIAN_POINT('Ctrl Pts',(55.9627465535904,26.6564391417817,22.7461217858157));
#62058=CARTESIAN_POINT('Ctrl Pts',(57.4899921297994,28.5317232652417,22.8728246161812));
#62059=CARTESIAN_POINT('Ctrl Pts',(56.7482891129976,30.8337701453811,22.9995274465467));
#62060=CARTESIAN_POINT('Ctrl Pts',(54.4136885536048,31.4647519228485,23.1262302769121));
#62061=CARTESIAN_POINT('Ctrl Pts',(52.6130583236143,29.8501236550651,23.2529331072776));
#62062=CARTESIAN_POINT('Ctrl Pts',(52.987945935458,27.4603388218333,23.379635937643));
#62063=CARTESIAN_POINT('Ctrl Pts',(55.1951539829876,26.4745218866781,23.5063387680084));
#62064=CARTESIAN_POINT('Ctrl Pts',(57.2266242981082,27.7878773360167,23.6330415983739));
#62065=CARTESIAN_POINT('Ctrl Pts',(57.2250123592762,30.2102470168422,23.7597618591261));
#62066=CARTESIAN_POINT('Ctrl Pts',(55.8779376927861,31.0829490139849,23.8442478430899));
#62067=CARTESIAN_POINT('Ctrl Pts',(55.1682015051339,31.138743146064,23.8864995502653));
#62068=CARTESIAN_POINT('Ctrl Pts',(53.9911581995026,31.0663838938146,4.84332060209571));
#62069=CARTESIAN_POINT('Ctrl Pts',(53.3057237132466,30.7317437704051,4.88555487888419));
#62070=CARTESIAN_POINT('Ctrl Pts',(52.3057458731769,29.332451268937,4.97002343246116));
#62071=CARTESIAN_POINT('Ctrl Pts',(53.2556893237274,26.9164216648475,5.09672626282661));
#62072=CARTESIAN_POINT('Ctrl Pts',(55.7975711244056,26.4047749826171,5.22342909319206));
#62073=CARTESIAN_POINT('Ctrl Pts',(57.6114280049078,28.2550399075399,5.35013192355752));
#62074=CARTESIAN_POINT('Ctrl Pts',(57.0464078792917,30.7855559938902,5.47683475392296));
#62075=CARTESIAN_POINT('Ctrl Pts',(54.6163716009993,31.6883401940828,5.60353758428842));
#62076=CARTESIAN_POINT('Ctrl Pts',(52.5360665973209,30.1418886630702,5.73024041465387));
#62077=CARTESIAN_POINT('Ctrl Pts',(52.700807151554,27.5547584266893,5.85694324501931));
#62078=CARTESIAN_POINT('Ctrl Pts',(54.9606127012548,26.2846277414455,5.98364607538478));
#62079=CARTESIAN_POINT('Ctrl Pts',(57.2562853518332,27.4886899983651,6.11034890575021));
#62080=CARTESIAN_POINT('Ctrl Pts',(57.4960459301408,30.0698809432301,6.23705173611568));
#62081=CARTESIAN_POINT('Ctrl Pts',(55.461407613052,31.6761851114186,6.36375456648113));
#62082=CARTESIAN_POINT('Ctrl Pts',(53.006338417493,30.8439603477291,6.49045739684658));
#62083=CARTESIAN_POINT('Ctrl Pts',(52.3678889131507,28.3315185076544,6.61716022721203));
#62084=CARTESIAN_POINT('Ctrl Pts',(54.1278155663995,26.4281976505747,6.74386305757748));
#62085=CARTESIAN_POINT('Ctrl Pts',(56.6824748713308,26.8682980669564,6.87056588794293));
#62086=CARTESIAN_POINT('Ctrl Pts',(57.7040659895162,29.2508022964232,6.99726871830839));
#62087=CARTESIAN_POINT('Ctrl Pts',(56.2617164348777,31.404775648651,7.12397154867383));
#62088=CARTESIAN_POINT('Ctrl Pts',(53.6696929521768,31.3675214245298,7.25067437903929));
#62089=CARTESIAN_POINT('Ctrl Pts',(52.2898430793299,29.1729854364138,7.37737720940473));
#62090=CARTESIAN_POINT('Ctrl Pts',(53.3794838361463,26.8208254280239,7.5040800397702));
#62091=CARTESIAN_POINT('Ctrl Pts',(55.9457363013156,26.4543257601017,7.63078287013563));
#62092=CARTESIAN_POINT('Ctrl Pts',(57.6502353773361,28.4074403625246,7.7574857005011));
#62093=CARTESIAN_POINT('Ctrl Pts',(56.9398442492839,30.900494347051,7.88418853086654));
#62094=CARTESIAN_POINT('Ctrl Pts',(54.4618701702737,31.6618209492118,8.01089136123201));
#62095=CARTESIAN_POINT('Ctrl Pts',(52.4742391238837,29.9977005936638,8.13759419159744));
#62096=CARTESIAN_POINT('Ctrl Pts',(52.7880773151889,27.4244770665284,8.2642970219629));
#62097=CARTESIAN_POINT('Ctrl Pts',(55.1174158899787,26.2868674955205,8.39099985232835));
#62098=CARTESIAN_POINT('Ctrl Pts',(57.3397652952198,27.621459887727,8.51770268269381));
#62099=CARTESIAN_POINT('Ctrl Pts',(57.4301243363657,30.2121758072282,8.64440551305926));
#62100=CARTESIAN_POINT('Ctrl Pts',(55.3061580008797,31.6983590858891,8.7711083434247));
#62101=CARTESIAN_POINT('Ctrl Pts',(52.9032209886726,30.7258019166539,8.89781117379017));
#62102=CARTESIAN_POINT('Ctrl Pts',(52.4108656304726,28.1806968238802,9.0245140041556));
#62103=CARTESIAN_POINT('Ctrl Pts',(54.2777253347274,26.3821394640313,9.15121683452108));
#62104=CARTESIAN_POINT('Ctrl Pts',(56.8027205492901,26.9689724031812,9.2779196648865));
#62105=CARTESIAN_POINT('Ctrl Pts',(57.68507970628,29.4064744134585,9.40462249525197));
#62106=CARTESIAN_POINT('Ctrl Pts',(56.1207985646789,31.4735975936453,9.53132532561742));
#62107=CARTESIAN_POINT('Ctrl Pts',(53.5352475782635,31.286782635252,9.65802815598287));
#62108=CARTESIAN_POINT('Ctrl Pts',(52.2843766365773,29.0162550271226,9.78473098634831));
#62109=CARTESIAN_POINT('Ctrl Pts',(53.5079773246182,26.7309158644907,9.91143381671377));
#62110=CARTESIAN_POINT('Ctrl Pts',(56.0911066685357,26.513162507169,10.0381366470792));
#62111=CARTESIAN_POINT('Ctrl Pts',(57.6800213755258,28.5614114632152,10.1648394774447));
#62112=CARTESIAN_POINT('Ctrl Pts',(56.8269049267509,31.0093015867427,10.2915423078101));
#62113=CARTESIAN_POINT('Ctrl Pts',(54.3091156546596,31.626319344489,10.4182451381756));
#62114=CARTESIAN_POINT('Ctrl Pts',(52.4208590839707,29.8502391505553,10.544947968541));
#62115=CARTESIAN_POINT('Ctrl Pts',(52.8827115570261,27.2994224136717,10.6716507989065));
#62116=CARTESIAN_POINT('Ctrl Pts',(55.2738338451284,26.2981692312182,10.7983536292719));
#62117=CARTESIAN_POINT('Ctrl Pts',(57.415439175115,27.758819888496,10.9250564596374));
#62118=CARTESIAN_POINT('Ctrl Pts',(57.3561002237046,30.3504318619362,11.0517592900028));
#62119=CARTESIAN_POINT('Ctrl Pts',(55.1498865477365,31.7115325003918,11.1784621203683));
#62120=CARTESIAN_POINT('Ctrl Pts',(52.8070964911674,30.6018890969175,11.3051649507338));
#62121=CARTESIAN_POINT('Ctrl Pts',(52.4624765757242,28.032606931426,11.4318677810992));
#62122=CARTESIAN_POINT('Ctrl Pts',(54.4300439126487,26.3448117700689,11.5585706114646));
#62123=CARTESIAN_POINT('Ctrl Pts',(56.9169543172966,27.0764198422547,11.6852734418301));
#62124=CARTESIAN_POINT('Ctrl Pts',(57.6571390391698,29.5607910523476,11.8119762721955));
#62125=CARTESIAN_POINT('Ctrl Pts',(55.9761429532675,31.5341703598337,11.938679102561));
#62126=CARTESIAN_POINT('Ctrl Pts',(53.4056869824076,31.1984177218646,12.0653819329264));
#62127=CARTESIAN_POINT('Ctrl Pts',(52.2879664623005,28.8594704007468,12.1920847632919));
#62128=CARTESIAN_POINT('Ctrl Pts',(53.6414465285101,26.6485734238602,12.3187875936574));
#62129=CARTESIAN_POINT('Ctrl Pts',(56.2328383272333,26.5802925514067,12.4454904240228));
#62130=CARTESIAN_POINT('Ctrl Pts',(57.7008698301702,28.7168452042609,12.5721932543883));
#62131=CARTESIAN_POINT('Ctrl Pts',(56.707873099089,31.111408050397,12.6988960847537));
#62132=CARTESIAN_POINT('Ctrl Pts',(54.1586651541145,31.5820592857199,12.8255989151192));
#62133=CARTESIAN_POINT('Ctrl Pts',(52.376080164033,29.6999422635425,12.9523017454846));
#62134=CARTESIAN_POINT('Ctrl Pts',(52.9844066973359,27.180038979503,13.0790045758501));
#62135=CARTESIAN_POINT('Ctrl Pts',(55.4293385978216,26.3184812425989,13.2057074062155));
#62136=CARTESIAN_POINT('Ctrl Pts',(57.4830578602938,27.9003190734096,13.332410236581));
#62137=CARTESIAN_POINT('Ctrl Pts',(57.2742188044711,30.4841843912612,13.4591130669464));
#62138=CARTESIAN_POINT('Ctrl Pts',(54.9931152412601,31.7156632850872,13.5858158973119));
#62139=CARTESIAN_POINT('Ctrl Pts',(52.718285059111,30.47263417263,13.7125187276773));
#62140=CARTESIAN_POINT('Ctrl Pts',(52.5225498517664,27.8877431767388,13.8392215580428));
#62141=CARTESIAN_POINT('Ctrl Pts',(54.5842632245302,26.316338804656,13.9659243884082));
#62142=CARTESIAN_POINT('Ctrl Pts',(57.0247952767137,27.1902821862869,14.0926272187737));
#62143=CARTESIAN_POINT('Ctrl Pts',(57.6203371377989,29.7132375215492,14.2193300491391));
#62144=CARTESIAN_POINT('Ctrl Pts',(55.8282320242933,31.5862919772926,14.3460328795046));
#62145=CARTESIAN_POINT('Ctrl Pts',(53.2814432258008,31.1027213538002,14.47273570987));
#62146=CARTESIAN_POINT('Ctrl Pts',(52.3006005887342,28.7031544234258,14.5994385402355));
#62147=CARTESIAN_POINT('Ctrl Pts',(53.7794463423511,26.5740727037537,14.7261413706009));
#62148=CARTESIAN_POINT('Ctrl Pts',(56.3704586206384,26.6554920245408,14.8528442009664));
#62149=CARTESIAN_POINT('Ctrl Pts',(57.7127112137053,28.8732232319774,14.9795470313318));
#62150=CARTESIAN_POINT('Ctrl Pts',(56.5831457231721,31.2064732260048,15.1062498616973));
#62151=CARTESIAN_POINT('Ctrl Pts',(54.0110204025537,31.5291883745005,15.2329526920627));
#62152=CARTESIAN_POINT('Ctrl Pts',(52.3400516963698,29.5473111545432,15.3596555224282));
#62153=CARTESIAN_POINT('Ctrl Pts',(53.0928235952072,27.0667248931217,15.4863583527936));
#62154=CARTESIAN_POINT('Ctrl Pts',(55.5834115587132,26.3477357916238,15.6130611831591));
#62155=CARTESIAN_POINT('Ctrl Pts',(57.5423958506882,28.0454855599432,15.7397640135245));
#62156=CARTESIAN_POINT('Ctrl Pts',(57.1847531432053,30.6129873468592,15.86646684389));
#62157=CARTESIAN_POINT('Ctrl Pts',(54.8363668946136,31.7107376643075,15.9931696742555));
#62158=CARTESIAN_POINT('Ctrl Pts',(52.6370828677864,30.3384681931841,16.1198725046209));
#62159=CARTESIAN_POINT('Ctrl Pts',(52.5908851215582,27.7465886627514,16.2465753349864));
#62160=CARTESIAN_POINT('Ctrl Pts',(54.7398689677963,26.2968155216564,16.3732781653518));
#62161=CARTESIAN_POINT('Ctrl Pts',(57.1258837911094,27.3101797182624,16.4999809957173));
#62162=CARTESIAN_POINT('Ctrl Pts',(57.5747967320147,29.8633054307021,16.6266838260827));
#62163=CARTESIAN_POINT('Ctrl Pts',(55.6775590426448,31.6297886267918,16.7533866564481));
#62164=CARTESIAN_POINT('Ctrl Pts',(53.1629306462013,31.0000126667616,16.8800894868136));
#62165=CARTESIAN_POINT('Ctrl Pts',(52.3222368826097,28.5478283898582,17.006792317179));
#62166=CARTESIAN_POINT('Ctrl Pts',(53.9215165536116,26.5076621549759,17.1334951475445));
#62167=CARTESIAN_POINT('Ctrl Pts',(56.5035086018754,26.7385101455104,17.2601979779099));
#62168=CARTESIAN_POINT('Ctrl Pts',(57.7155060365633,29.0300240447358,17.3869008082754));
#62169=CARTESIAN_POINT('Ctrl Pts',(56.4531387495689,31.2941800828128,17.5136036386409));
#62170=CARTESIAN_POINT('Ctrl Pts',(53.8666737771972,31.4678829288644,17.6403064690063));
#62171=CARTESIAN_POINT('Ctrl Pts',(52.3128938315209,29.39285482967,17.7670092993718));
#62172=CARTESIAN_POINT('Ctrl Pts',(53.2076006935238,26.9598580431702,17.8937121297372));
#62173=CARTESIAN_POINT('Ctrl Pts',(55.7355389132906,26.3858353179441,18.0204149601027));
#62174=CARTESIAN_POINT('Ctrl Pts',(57.5932552613452,28.1938352355886,18.1471177904681));
#62175=CARTESIAN_POINT('Ctrl Pts',(57.0880015969638,30.7364111866002,18.2738206208336));
#62176=CARTESIAN_POINT('Ctrl Pts',(54.6801642443937,31.6967720643965,18.400523451199));
#62177=CARTESIAN_POINT('Ctrl Pts',(52.5637607165875,30.1998385857402,18.5272262815645));
#62178=CARTESIAN_POINT('Ctrl Pts',(52.667254495318,27.609614122533,18.6539291119299));
#62179=CARTESIAN_POINT('Ctrl Pts',(54.8963422162931,26.2863070288349,18.7806319422954));
#62180=CARTESIAN_POINT('Ctrl Pts',(57.2198827426306,27.4357125945517,18.9073347726609));
#62181=CARTESIAN_POINT('Ctrl Pts',(57.5206696935102,30.0104943216526,19.0340376030263));
#62182=CARTESIAN_POINT('Ctrl Pts',(55.5246264843186,31.6645152523161,19.1607404333918));
#62183=CARTESIAN_POINT('Ctrl Pts',(53.0505444685914,30.8906341816795,19.2874432637572));
#62184=CARTESIAN_POINT('Ctrl Pts',(52.3528031895289,28.3940102934005,19.4141460941227));
#62185=CARTESIAN_POINT('Ctrl Pts',(54.0671833754831,26.4495632485988,19.5408489244881));
#62186=CARTESIAN_POINT('Ctrl Pts',(56.6315445655035,26.8290700590176,19.6675517548536));
#62187=CARTESIAN_POINT('Ctrl Pts',(57.7092449783493,29.1867247309721,19.794254585219));
#62188=CARTESIAN_POINT('Ctrl Pts',(56.3182857356656,31.3742361291603,19.9209574155844));
#62189=CARTESIAN_POINT('Ctrl Pts',(53.7261066564109,31.3983473949914,20.0476602459499));
#62190=CARTESIAN_POINT('Ctrl Pts',(52.2946971376583,29.2370883818991,20.1743630763153));
#62191=CARTESIAN_POINT('Ctrl Pts',(53.328355224661,26.8597948175601,20.3010659066808));
#62192=CARTESIAN_POINT('Ctrl Pts',(55.8852133354318,26.4326527642611,20.4277687370462));
#62193=CARTESIAN_POINT('Ctrl Pts',(57.6354664822799,28.3448733723503,20.5544715674117));
#62194=CARTESIAN_POINT('Ctrl Pts',(56.9842868204588,30.854044306933,20.6811743977772));
#62195=CARTESIAN_POINT('Ctrl Pts',(54.5250282071345,31.6738130591511,20.8078772281426));
#62196=CARTESIAN_POINT('Ctrl Pts',(52.4985631263916,30.0572076626689,20.9345800585081));
#62197=CARTESIAN_POINT('Ctrl Pts',(52.7514032896153,27.4772763503198,21.0612828888735));
#62198=CARTESIAN_POINT('Ctrl Pts',(55.0531611525946,26.2848483690293,21.1879857192389));
#62199=CARTESIAN_POINT('Ctrl Pts',(57.3064786528164,27.5664621816773,21.3146885496044));
#62200=CARTESIAN_POINT('Ctrl Pts',(57.4581365360819,30.1543133308796,21.4413913799699));
#62201=CARTESIAN_POINT('Ctrl Pts',(55.3699443475302,31.69035605763,21.5680942103353));
#62202=CARTESIAN_POINT('Ctrl Pts',(52.9446595130096,30.7749506373201,21.6947970407008));
#62203=CARTESIAN_POINT('Ctrl Pts',(52.3921975239131,28.242213147868,21.8214998710662));
#62204=CARTESIAN_POINT('Ctrl Pts',(54.2159611262207,26.3999696408687,21.9482027014317));
#62205=CARTESIAN_POINT('Ctrl Pts',(56.7541393325647,26.9268699479593,22.0749055317971));
#62206=CARTESIAN_POINT('Ctrl Pts',(57.6939493004178,29.3428023423225,22.2016083621626));
#62207=CARTESIAN_POINT('Ctrl Pts',(56.1790356521349,31.4463751144411,22.328311192528));
#62208=CARTESIAN_POINT('Ctrl Pts',(53.58978927969,31.3208122414973,22.4550140228935));
#62209=CARTESIAN_POINT('Ctrl Pts',(52.2855194267405,29.0805340639504,22.5817168532589));
#62210=CARTESIAN_POINT('Ctrl Pts',(53.4546901152972,26.7668634456938,22.7084196836244));
#62211=CARTESIAN_POINT('Ctrl Pts',(56.0319246485763,26.4880427190156,22.8351225139898));
#62212=CARTESIAN_POINT('Ctrl Pts',(57.6689103626689,28.4980752689794,22.9618253443553));
#62213=CARTESIAN_POINT('Ctrl Pts',(56.8739123207573,30.9655355875179,23.0885281747208));
#62214=CARTESIAN_POINT('Ctrl Pts',(54.371559180325,31.6418565221842,23.2152310050862));
#62215=CARTESIAN_POINT('Ctrl Pts',(52.4415447748001,29.9112092385352,23.3419338354517));
#62216=CARTESIAN_POINT('Ctrl Pts',(52.8433699131658,27.3497065616273,23.4686366658171));
#62217=CARTESIAN_POINT('Ctrl Pts',(55.209176760552,26.2930538106234,23.5953394961826));
#62218=CARTESIAN_POINT('Ctrl Pts',(57.386618251468,27.7007803358032,23.722042326548));
#62219=CARTESIAN_POINT('Ctrl Pts',(57.3848904868694,30.2972092425445,23.8487625873002));
#62220=CARTESIAN_POINT('Ctrl Pts',(55.9410218522429,31.2326191885525,23.933248571264));
#62221=CARTESIAN_POINT('Ctrl Pts',(55.1802876140434,31.2924224045949,23.9755002784394));
#62222=CARTESIAN_POINT('Ctrl Pts',(53.9235275309291,31.2049099979065,4.93232133026981));
#62223=CARTESIAN_POINT('Ctrl Pts',(53.1921429338175,30.847836292476,4.97455560705829));
#62224=CARTESIAN_POINT('Ctrl Pts',(52.1251286467557,29.3547381146796,5.05902416063525));
#62225=CARTESIAN_POINT('Ctrl Pts',(53.1387543422687,26.7767428809569,5.18572699100072));
#62226=CARTESIAN_POINT('Ctrl Pts',(55.8510386436457,26.2307964629548,5.31242982136615));
#62227=CARTESIAN_POINT('Ctrl Pts',(57.786492739355,28.2050993231106,5.43913265173162));
#62228=CARTESIAN_POINT('Ctrl Pts',(57.1835948326693,30.9052559761693,5.56583548209706));
#62229=CARTESIAN_POINT('Ctrl Pts',(54.5906539462635,31.8685609626798,5.69253831246252));
#62230=CARTESIAN_POINT('Ctrl Pts',(52.3708895960694,30.2184385182424,5.81924114282797));
#62231=CARTESIAN_POINT('Ctrl Pts',(52.5466740164649,27.4578724195821,5.94594397319342));
#62232=CARTESIAN_POINT('Ctrl Pts',(54.9579722581784,26.1025947991337,6.07264680355888));
#62233=CARTESIAN_POINT('Ctrl Pts',(57.4075420570585,27.3873749004164,6.19934963392432));
#62234=CARTESIAN_POINT('Ctrl Pts',(57.6633756888425,30.1416035497367,6.32605246428978));
#62235=CARTESIAN_POINT('Ctrl Pts',(55.4923394254929,31.855591028404,6.45275529465523));
#62236=CARTESIAN_POINT('Ctrl Pts',(52.8726874668012,30.9675756371415,6.57945812502068));
#62237=CARTESIAN_POINT('Ctrl Pts',(52.1914376276516,28.2867048904611,6.70616095538613));
#62238=CARTESIAN_POINT('Ctrl Pts',(54.0693461251703,26.2557893381471,6.83286378575158));
#62239=CARTESIAN_POINT('Ctrl Pts',(56.7952645082689,26.7253931765565,6.95956661611704));
#62240=CARTESIAN_POINT('Ctrl Pts',(57.8853409829267,29.2676155638537,7.08626944648249));
#62241=CARTESIAN_POINT('Ctrl Pts',(56.3462992961339,31.5659868363783,7.21297227684794));
#62242=CARTESIAN_POINT('Ctrl Pts',(53.5805119180366,31.5262351660934,7.33967510721339));
#62243=CARTESIAN_POINT('Ctrl Pts',(52.1081597624875,29.1845820224319,7.46637793757883));
#62244=CARTESIAN_POINT('Ctrl Pts',(53.2708477828606,26.6747380700575,7.5930807679443));
#62245=CARTESIAN_POINT('Ctrl Pts',(56.0091365076915,26.2836690221182,7.71978359830973));
#62246=CARTESIAN_POINT('Ctrl Pts',(57.8279016777983,28.3677163895168,7.84648642867521));
#62247=CARTESIAN_POINT('Ctrl Pts',(57.0698873972211,31.0278995588966,7.97318925904064));
#62248=CARTESIAN_POINT('Ctrl Pts',(54.4257950590463,31.84026392246,8.09989208940611));
#62249=CARTESIAN_POINT('Ctrl Pts',(52.3049173366382,30.0645843787649,8.22659491977155));
#62250=CARTESIAN_POINT('Ctrl Pts',(52.6397945914431,27.3188572663865,8.353297750137));
#62251=CARTESIAN_POINT('Ctrl Pts',(55.1252872084912,26.1049847016914,8.48000058050245));
#62252=CARTESIAN_POINT('Ctrl Pts',(57.496618323259,27.5290454086657,8.6067034108679));
#62253=CARTESIAN_POINT('Ctrl Pts',(57.5930348477102,30.2934375672296,8.73340624123336));
#62254=CARTESIAN_POINT('Ctrl Pts',(55.3266822002917,31.8792515002793,8.8601090715988));
#62255=CARTESIAN_POINT('Ctrl Pts',(52.7626572587432,30.8414961091338,8.98681190196427));
#62256=CARTESIAN_POINT('Ctrl Pts',(52.2372954152504,28.1257724328231,9.1135147323297));
#62257=CARTESIAN_POINT('Ctrl Pts',(54.2293055344357,26.2066435060008,9.24021756269518));
#62258=CARTESIAN_POINT('Ctrl Pts',(56.9235712078764,26.8328165121425,9.36692039306061));
#62259=CARTESIAN_POINT('Ctrl Pts',(57.8650818985156,29.4337236177705,9.49362322342607));
#62260=CARTESIAN_POINT('Ctrl Pts',(56.1959345832578,31.639422462279,9.6203260537915));
#62261=CARTESIAN_POINT('Ctrl Pts',(53.4370536042156,31.4400838153061,9.74702888415697));
#62262=CARTESIAN_POINT('Ctrl Pts',(52.1023268607143,29.0173447305344,9.87373171452243));
#62263=CARTESIAN_POINT('Ctrl Pts',(53.4079552091459,26.5788011552687,10.0004345448879));
#62264=CARTESIAN_POINT('Ctrl Pts',(56.1642522037837,26.3464500630666,10.1271373752533));
#62265=CARTESIAN_POINT('Ctrl Pts',(57.8596844677255,28.5320093944699,10.2538402056188));
#62266=CARTESIAN_POINT('Ctrl Pts',(56.9493768560022,31.1440010109833,10.3805430359842));
#62267=CARTESIAN_POINT('Ctrl Pts',(54.2628001965182,31.8023823635544,10.5072458663497));
#62268=CARTESIAN_POINT('Ctrl Pts',(52.24795880921,29.90723742538,10.6339486967151));
#62269=CARTESIAN_POINT('Ctrl Pts',(52.7407729172013,27.1854192081467,10.7606515270806));
#62270=CARTESIAN_POINT('Ctrl Pts',(55.2921910999675,26.1170440823845,10.887354357446));
#62271=CARTESIAN_POINT('Ctrl Pts',(57.5773652236103,27.675613739901,11.0140571878115));
#62272=CARTESIAN_POINT('Ctrl Pts',(57.5140483115778,30.4409620220074,11.1407600181769));
#62273=CARTESIAN_POINT('Ctrl Pts',(55.1599346320135,31.8933080332549,11.2674628485424));
#62274=CARTESIAN_POINT('Ctrl Pts',(52.660088773658,30.7092764301462,11.3941656789078));
#62275=CARTESIAN_POINT('Ctrl Pts',(52.2923662515686,27.9677549001475,11.5208685092733));
#62276=CARTESIAN_POINT('Ctrl Pts',(54.3918352349096,26.1668134406084,11.6475713396387));
#62277=CARTESIAN_POINT('Ctrl Pts',(57.0454629715172,26.9474670053891,11.7742741700042));
#62278=CARTESIAN_POINT('Ctrl Pts',(57.8352681468484,29.5983853250884,11.9009770003696));
#62279=CARTESIAN_POINT('Ctrl Pts',(56.0415815587258,31.7040559014815,12.0276798307351));
#62280=CARTESIAN_POINT('Ctrl Pts',(53.2988075338738,31.3457951008154,12.1543826611005));
#62281=CARTESIAN_POINT('Ctrl Pts',(52.1061573409321,28.8500495869511,12.281085491466));
#62282=CARTESIAN_POINT('Ctrl Pts',(53.5503719125255,26.4909386476573,12.4077883218315));
#62283=CARTESIAN_POINT('Ctrl Pts',(56.3154852598571,26.418080366682,12.5344911521969));
#62284=CARTESIAN_POINT('Ctrl Pts',(57.8819305596662,28.6978630921634,12.6611939825623));
#62285=CARTESIAN_POINT('Ctrl Pts',(56.8223653807064,31.2529524808608,12.7878968129278));
#62286=CARTESIAN_POINT('Ctrl Pts',(54.1022638054657,31.755155201951,12.9145996432933));
#62287=CARTESIAN_POINT('Ctrl Pts',(52.200178003058,29.7468649457934,13.0413024736587));
#62288=CARTESIAN_POINT('Ctrl Pts',(52.8492854894676,27.058032555371,13.1680053040242));
#62289=CARTESIAN_POINT('Ctrl Pts',(55.4581205697826,26.1387177690139,13.2947081343896));
#62290=CARTESIAN_POINT('Ctrl Pts',(57.6495169256451,27.8265987376286,13.4214109647551));
#62291=CARTESIAN_POINT('Ctrl Pts',(57.4266777312847,30.5836810443714,13.5481137951205));
#62292=CARTESIAN_POINT('Ctrl Pts',(54.9926537012681,31.8977157372161,13.674816625486));
#62293=CARTESIAN_POINT('Ctrl Pts',(52.5653236068099,30.5713565229626,13.8015194558514));
#62294=CARTESIAN_POINT('Ctrl Pts',(52.356466715838,27.8131797788449,13.9282222862168));
#62295=CARTESIAN_POINT('Ctrl Pts',(54.5563930906184,26.1364317064607,14.0549251165823));
#62296=CARTESIAN_POINT('Ctrl Pts',(57.1605333658978,27.0689624455601,14.1816279469477));
#62297=CARTESIAN_POINT('Ctrl Pts',(57.7959991220958,29.7610514904095,14.3083307773132));
#62298=CARTESIAN_POINT('Ctrl Pts',(55.8837549868721,31.7596716444159,14.4350336076787));
#62299=CARTESIAN_POINT('Ctrl Pts',(53.1662347326919,31.2436834460835,14.5617364380441));
#62300=CARTESIAN_POINT('Ctrl Pts',(52.1196384330817,28.6832545096864,14.6884392684096));
#62301=CARTESIAN_POINT('Ctrl Pts',(53.6976229485782,26.4114435533014,14.815142098775));
#62302=CARTESIAN_POINT('Ctrl Pts',(56.4623313332087,26.4983210570238,14.9418449291405));
#62303=CARTESIAN_POINT('Ctrl Pts',(57.894565765072,28.864724379554,15.0685477595059));
#62304=CARTESIAN_POINT('Ctrl Pts',(56.6892765393757,31.3543906292988,15.1952505898714));
#62305=CARTESIAN_POINT('Ctrl Pts',(53.9447212550088,31.6987399341516,15.3219534202368));
#62306=CARTESIAN_POINT('Ctrl Pts',(52.1617342614096,29.5840017628043,15.4486562506023));
#62307=CARTESIAN_POINT('Ctrl Pts',(52.9649704320257,26.9371221269099,15.5753590809677));
#62308=CARTESIAN_POINT('Ctrl Pts',(55.6225222634338,26.1699334825232,15.7020619113332));
#62309=CARTESIAN_POINT('Ctrl Pts',(57.712832812237,27.9814968852945,15.8287647416986));
#62310=CARTESIAN_POINT('Ctrl Pts',(57.3312144770535,30.7211186838188,15.9554675720641));
#62311=CARTESIAN_POINT('Ctrl Pts',(54.825397269532,31.8924599130027,16.0821704024296));
#62312=CARTESIAN_POINT('Ctrl Pts',(52.4786777884606,30.4281963336365,16.208873232795));
#62313=CARTESIAN_POINT('Ctrl Pts',(52.4293830408368,27.6625625580699,16.3355760631605));
#62314=CARTESIAN_POINT('Ctrl Pts',(54.7224303212057,26.1155996229323,16.4622788935259));
#62315=CARTESIAN_POINT('Ctrl Pts',(57.2683986453028,27.196897660197,16.5889817238913));
#62316=CARTESIAN_POINT('Ctrl Pts',(57.7474057816604,29.9211796419339,16.7156845542568));
#62317=CARTESIAN_POINT('Ctrl Pts',(55.7229812000429,31.8060842193703,16.8423873846222));
#62318=CARTESIAN_POINT('Ctrl Pts',(53.0397773147751,31.1340893810111,16.9690902149877));
#62319=CARTESIAN_POINT('Ctrl Pts',(52.1427251793666,28.5175157399575,17.0957930453531));
#62320=CARTESIAN_POINT('Ctrl Pts',(53.8492172530783,26.3405809786343,17.2224958757186));
#62321=CARTESIAN_POINT('Ctrl Pts',(56.6043007101135,26.586904541187,17.3491987060841));
#62322=CARTESIAN_POINT('Ctrl Pts',(57.8975479470761,29.0320367946217,17.4759015364495));
#62323=CARTESIAN_POINT('Ctrl Pts',(56.5505541670455,31.4479771724574,17.602604366815));
#62324=CARTESIAN_POINT('Ctrl Pts',(53.790697930318,31.6333246981861,17.7293071971804));
#62325=CARTESIAN_POINT('Ctrl Pts',(52.132755789449,29.4191910052424,17.8560100275459));
#62326=CARTESIAN_POINT('Ctrl Pts',(53.0874419497171,26.8230911442798,17.9827128579113));
#62327=CARTESIAN_POINT('Ctrl Pts',(55.7848479213462,26.2105871223189,18.1094156882768));
#62328=CARTESIAN_POINT('Ctrl Pts',(57.7671017326352,28.1397916164894,18.2361185186422));
#62329=CARTESIAN_POINT('Ctrl Pts',(57.2279769071813,30.8528166026031,18.3628213490077));
#62330=CARTESIAN_POINT('Ctrl Pts',(54.6587231165829,31.8775580881469,18.4895241793731));
#62331=CARTESIAN_POINT('Ctrl Pts',(52.4004402718352,30.2802732839195,18.6162270097386));
#62332=CARTESIAN_POINT('Ctrl Pts',(52.5108720595234,27.5164055278637,18.742929840104));
#62333=CARTESIAN_POINT('Ctrl Pts',(54.8893932127809,26.1043866624779,18.8696326704694));
#62334=CARTESIAN_POINT('Ctrl Pts',(57.3686990921956,27.3308460009795,18.996335500835));
#62335=CARTESIAN_POINT('Ctrl Pts',(57.6896501783996,30.0782357718278,19.1230383312003));
#62336=CARTESIAN_POINT('Ctrl Pts',(55.5597963591873,31.8431388460741,19.2497411615659));
#62337=CARTESIAN_POINT('Ctrl Pts',(52.9198570001715,31.0173783884239,19.3764439919313));
#62338=CARTESIAN_POINT('Ctrl Pts',(52.1753405883074,28.3533859963246,19.5031468222967));
#62339=CARTESIAN_POINT('Ctrl Pts',(54.004649277529,26.2785872416904,19.6298496526622));
#62340=CARTESIAN_POINT('Ctrl Pts',(56.7409199400349,26.6835354040676,19.7565524830276));
#62341=CARTESIAN_POINT('Ctrl Pts',(57.890867160464,29.199242370892,19.8832553133931));
#62342=CARTESIAN_POINT('Ctrl Pts',(56.4066608858923,31.53340001064,20.0099581437585));
#62343=CARTESIAN_POINT('Ctrl Pts',(53.6407074803699,31.5591276458837,20.136660974124));
#62344=CARTESIAN_POINT('Ctrl Pts',(52.1133392268507,29.2529822968528,20.2633638044895));
#62345=CARTESIAN_POINT('Ctrl Pts',(53.2162916149675,26.7163198869008,20.3900666348549));
#62346=CARTESIAN_POINT('Ctrl Pts',(55.944556207303,26.2605431134443,20.5167694652203));
#62347=CARTESIAN_POINT('Ctrl Pts',(57.8121427065516,28.3009550376753,20.6434722955858));
#62348=CARTESIAN_POINT('Ctrl Pts',(57.1173093064847,30.9783356041222,20.7701751259513));
#62349=CARTESIAN_POINT('Ctrl Pts',(54.4931870801222,31.8530599586564,20.8968779563167));
#62350=CARTESIAN_POINT('Ctrl Pts',(52.3308719699855,30.1280806786482,21.0235807866821));
#62351=CARTESIAN_POINT('Ctrl Pts',(52.6006620150167,27.3751961050032,21.1502836170476));
#62352=CARTESIAN_POINT('Ctrl Pts',(55.0567249663564,26.1028302171346,21.276986447413));
#62353=CARTESIAN_POINT('Ctrl Pts',(57.4611002131674,27.4703607701076,21.4036892777785));
#62354=CARTESIAN_POINT('Ctrl Pts',(57.6229249273816,30.2316961100944,21.5303921081439));
#62355=CARTESIAN_POINT('Ctrl Pts',(55.3947446517464,31.8707119655516,21.6570949385094));
#62356=CARTESIAN_POINT('Ctrl Pts',(52.8068737360795,30.8939396584208,21.7837977688749));
#62357=CARTESIAN_POINT('Ctrl Pts',(52.2173758374226,28.1914126839889,21.9105005992403));
#62358=CARTESIAN_POINT('Ctrl Pts',(54.1634007810851,26.2256689810304,22.0372034296058));
#62359=CARTESIAN_POINT('Ctrl Pts',(56.8717332068209,26.7878915953673,22.1639062599712));
#62360=CARTESIAN_POINT('Ctrl Pts',(57.874546091907,29.3657831026244,22.2906090903367));
#62361=CARTESIAN_POINT('Ctrl Pts',(56.2580757646544,31.6103750443502,22.4173119207021));
#62362=CARTESIAN_POINT('Ctrl Pts',(53.4952516685433,31.4763946959995,22.5440147510676));
#62363=CARTESIAN_POINT('Ctrl Pts',(52.1035462611674,29.0859329010972,22.6707175814331));
#62364=CARTESIAN_POINT('Ctrl Pts',(53.3510957354806,26.6171585879957,22.7974204117984));
#62365=CARTESIAN_POINT('Ctrl Pts',(56.1011027435622,26.3196462962494,22.924123242164));
#62366=CARTESIAN_POINT('Ctrl Pts',(57.847828595538,28.4644272727171,23.0508260725294));
#62367=CARTESIAN_POINT('Ctrl Pts',(56.9995355285173,31.0973010296546,23.1775289028948));
#62368=CARTESIAN_POINT('Ctrl Pts',(54.3294298070452,31.81896112152,23.3042317332603));
#62369=CARTESIAN_POINT('Ctrl Pts',(52.2700312259861,29.9722948220053,23.4309345636257));
#62370=CARTESIAN_POINT('Ctrl Pts',(52.6987938908735,27.2390743014212,23.5576373939912));
#62371=CARTESIAN_POINT('Ctrl Pts',(55.2231995381166,26.1115857345688,23.6843402243566));
#62372=CARTESIAN_POINT('Ctrl Pts',(57.5466122048277,27.6136833355897,23.8110430547221));
#62373=CARTESIAN_POINT('Ctrl Pts',(57.5447686144626,30.384171468247,23.9377633154743));
#62374=CARTESIAN_POINT('Ctrl Pts',(56.0041060116998,31.3822893631201,24.0222492994381));
#62375=CARTESIAN_POINT('Ctrl Pts',(55.192373722953,31.4461016631257,24.0645010066135));
#62376=CARTESIAN_POINT('Ctrl Pts',(57.0573849385052,27.6687909762881,23.7995));
#62377=CARTESIAN_POINT('Ctrl Pts',(57.065530420017,27.6816406375123,23.7995));
#62378=CARTESIAN_POINT('Ctrl Pts',(57.0736759015289,27.6944902987365,23.7995));
#62379=CARTESIAN_POINT('Ctrl Pts',(57.0818213830407,27.7073399599607,23.7995));
#62380=CARTESIAN_POINT('',(53.8384899895517,27.376374413452,4.92960110781498));
#62381=CARTESIAN_POINT('Ctrl Pts',(53.8371424194197,27.3753492875172,4.9305));
#62382=CARTESIAN_POINT('Ctrl Pts',(53.7923471686059,27.4001101047657,4.93049999999997));
#62383=CARTESIAN_POINT('Ctrl Pts',(53.7486565878578,27.4266536903292,4.9305));
#62384=CARTESIAN_POINT('Ctrl Pts',(53.7061911675431,27.4549560897793,4.9305));
#62385=CARTESIAN_POINT('Ctrl Pts',(53.6465096071238,27.4947327209836,4.9305));
#62386=CARTESIAN_POINT('Ctrl Pts',(53.5892465950656,27.5379810208987,4.9305));
#62387=CARTESIAN_POINT('Ctrl Pts',(53.5344833636967,27.5843580131219,4.9305));
#62388=CARTESIAN_POINT('Ctrl Pts',(53.5027210288969,27.6112563811908,4.93049999999999));
#62389=CARTESIAN_POINT('Ctrl Pts',(53.4717999231724,27.6392081762248,4.93049999999999));
#62390=CARTESIAN_POINT('Ctrl Pts',(53.441739198632,27.668153548885,4.93050000000001));
#62391=CARTESIAN_POINT('Ctrl Pts',(53.4320758759555,27.6774583304657,4.93050000000001));
#62392=CARTESIAN_POINT('Ctrl Pts',(53.422500525095,27.6868667842346,4.93049999999999));
#62393=CARTESIAN_POINT('Ctrl Pts',(53.4130168704631,27.6963739839462,4.9305));
#62394=CARTESIAN_POINT('Ctrl Pts',(53.3601668251658,27.7493552401086,4.93050000000002));
#62395=CARTESIAN_POINT('Ctrl Pts',(53.3102898631553,27.805270243235,4.93049999999999));
#62396=CARTESIAN_POINT('Ctrl Pts',(53.2634720446863,27.863741969491,4.93049999999999));
#62397=CARTESIAN_POINT('Ctrl Pts',(53.2239608869098,27.9130882585135,4.93049999999999));
#62398=CARTESIAN_POINT('Ctrl Pts',(53.1866286810685,27.9642566970573,4.93050000000001));
#62399=CARTESIAN_POINT('Ctrl Pts',(53.1515413985246,28.0170458610233,4.93049999999999));
#62400=CARTESIAN_POINT('Ctrl Pts',(53.1348137264051,28.042212809338,4.93049999999999));
#62401=CARTESIAN_POINT('Ctrl Pts',(53.1185965065014,28.0677484290916,4.93049999999998));
#62402=CARTESIAN_POINT('Ctrl Pts',(53.1028981687538,28.0936323966796,4.9305));
#62403=CARTESIAN_POINT('Ctrl Pts',(53.0952269344716,28.1062809957042,4.93050000000001));
#62404=CARTESIAN_POINT('Ctrl Pts',(53.0876783757228,28.1190149460074,4.93050000000001));
#62405=CARTESIAN_POINT('Ctrl Pts',(53.0802575695615,28.1318249982112,4.93050000000001));
#62406=CARTESIAN_POINT('Ctrl Pts',(53.0406280389758,28.20023486428,4.93050000000001));
#62407=CARTESIAN_POINT('Ctrl Pts',(53.0047367242393,28.2706403069767,4.93050000000001));
#62408=CARTESIAN_POINT('Ctrl Pts',(52.9726791564584,28.342639293023,4.9305));
#62409=CARTESIAN_POINT('Ctrl Pts',(52.9406215886776,28.4146382790693,4.93049999999999));
#62410=CARTESIAN_POINT('Ctrl Pts',(52.9123971908107,28.4882317069565,4.93049999999998));
#62411=CARTESIAN_POINT('Ctrl Pts',(52.8881358995463,28.5630593264738,4.93049999999998));
#62412=CARTESIAN_POINT('Ctrl Pts',(52.8639452198436,28.6376691630622,4.93049999999997));
#62413=CARTESIAN_POINT('Ctrl Pts',(52.8436940427735,28.7135069395457,4.9305));
#62414=CARTESIAN_POINT('Ctrl Pts',(52.8275539142239,28.7902434418759,4.93050000000001));
#62415=CARTESIAN_POINT('Ctrl Pts',(52.8220518507206,28.8164024100368,4.93050000000001));
#62416=CARTESIAN_POINT('Ctrl Pts',(52.8170279307067,28.842665994242,4.93050000000001));
#62417=CARTESIAN_POINT('Ctrl Pts',(52.8124902744209,28.8690215999907,4.93050000000001));
#62418=CARTESIAN_POINT('Ctrl Pts',(52.8102866450664,28.8818207153985,4.93050000000001));
#62419=CARTESIAN_POINT('Ctrl Pts',(52.8081977059568,28.8946415354413,4.9305));
#62420=CARTESIAN_POINT('Ctrl Pts',(52.8062244495756,28.9074826291637,4.93049999999999));
#62421=CARTESIAN_POINT('Ctrl Pts',(52.8041389781676,28.9210539694416,4.93049999999998));
#62422=CARTESIAN_POINT('Ctrl Pts',(52.8021840453567,28.9346396035822,4.93049999999998));
#62423=CARTESIAN_POINT('Ctrl Pts',(52.8003611168859,28.948231453112,4.93049999999998));
#62424=CARTESIAN_POINT('Ctrl Pts',(52.7895931013731,29.0285183370621,4.93049999999999));
#62425=CARTESIAN_POINT('Ctrl Pts',(52.7834170296039,29.1090878588739,4.9305));
#62426=CARTESIAN_POINT('Ctrl Pts',(52.7819626910031,29.1895648886972,4.9305));
#62427=CARTESIAN_POINT('Ctrl Pts',(52.7814701883797,29.2168179288706,4.9305));
#62428=CARTESIAN_POINT('Ctrl Pts',(52.7815195434031,29.2440606003883,4.93050000000001));
#62429=CARTESIAN_POINT('Ctrl Pts',(52.7821169991807,29.2712789634107,4.9305));
#62430=CARTESIAN_POINT('Ctrl Pts',(52.7838212494952,29.3489196951292,4.93049999999997));
#62431=CARTESIAN_POINT('Ctrl Pts',(52.7899813526817,29.4263621040423,4.93049999999998));
#62432=CARTESIAN_POINT('Ctrl Pts',(52.8003647568699,29.5033553971092,4.9305));
#62433=CARTESIAN_POINT('Ctrl Pts',(52.8109627235699,29.5819396784545,4.93050000000002));
#62434=CARTESIAN_POINT('Ctrl Pts',(52.8259604552607,29.6600568668912,4.93049999999998));
#62435=CARTESIAN_POINT('Ctrl Pts',(52.8451645866725,29.7374421551003,4.93049999999999));
#62436=CARTESIAN_POINT('Ctrl Pts',(52.8497696158219,29.7559986573601,4.93049999999999));
#62437=CARTESIAN_POINT('Ctrl Pts',(52.8546186499929,29.7745194397526,4.93049999999997));
#62438=CARTESIAN_POINT('Ctrl Pts',(52.8596995461917,29.792966320632,4.93049999999997));
#62439=CARTESIAN_POINT('Ctrl Pts',(52.8810906976902,29.8706297894632,4.93049999999997));
#62440=CARTESIAN_POINT('Ctrl Pts',(52.9066063850458,29.9470718181813,4.93050000000001));
#62441=CARTESIAN_POINT('Ctrl Pts',(52.9359741374881,30.0220262297436,4.93049999999999));
#62442=CARTESIAN_POINT('Ctrl Pts',(52.9662538136702,30.0993081162269,4.93049999999998));
#62443=CARTESIAN_POINT('Ctrl Pts',(53.0006285871345,30.1750093988147,4.93049999999999));
#62444=CARTESIAN_POINT('Ctrl Pts',(53.0388562578731,30.2488401603755,4.93049999999998));
#62445=CARTESIAN_POINT('Ctrl Pts',(53.0770839286116,30.3226709219363,4.93049999999997));
#62446=CARTESIAN_POINT('Ctrl Pts',(53.119164888844,30.3946320658828,4.93050000000001));
#62447=CARTESIAN_POINT('Ctrl Pts',(53.1649084323202,30.4644222759714,4.93050000000002));
#62448=CARTESIAN_POINT('Ctrl Pts',(53.1843231359478,30.4940429861746,4.93050000000002));
#62449=CARTESIAN_POINT('Ctrl Pts',(53.2043982041861,30.5232724122283,4.9305));
#62450=CARTESIAN_POINT('Ctrl Pts',(53.2251215945603,30.55208627748,4.9305));
#62451=CARTESIAN_POINT('Ctrl Pts',(53.2367479306124,30.5682515706257,4.93049999999999));
#62452=CARTESIAN_POINT('Ctrl Pts',(53.2485813425571,30.584289696419,4.93049999999999));
#62453=CARTESIAN_POINT('Ctrl Pts',(53.2605971587666,30.6001671053542,4.93049999999999));
#62454=CARTESIAN_POINT('Ctrl Pts',(53.3124157578432,30.6686389489339,4.9305));
#62455=CARTESIAN_POINT('Ctrl Pts',(53.3676995807456,30.734233482485,4.93049999999999));
#62456=CARTESIAN_POINT('Ctrl Pts',(53.4261926153321,30.796654168762,4.93049999999999));
#62457=CARTESIAN_POINT('Ctrl Pts',(53.4847629333864,30.8591573278859,4.93049999999999));
#62458=CARTESIAN_POINT('Ctrl Pts',(53.546551385425,30.9184791823246,4.93049999999999));
#62459=CARTESIAN_POINT('Ctrl Pts',(53.6113499889526,30.9743043144675,4.9305));
#62460=CARTESIAN_POINT('Ctrl Pts',(53.6747669431677,31.0289391315226,4.93050000000001));
#62461=CARTESIAN_POINT('Ctrl Pts',(53.7410676106959,31.080225534543,4.93049999999999));
#62462=CARTESIAN_POINT('Ctrl Pts',(53.8100963515205,31.1278383728564,4.93049999999999));
#62463=CARTESIAN_POINT('Ctrl Pts',(53.8475703604045,31.1536862139821,4.93049999999998));
#62464=CARTESIAN_POINT('Ctrl Pts',(53.8858490074175,31.1784508229889,4.93049999999998));
#62465=CARTESIAN_POINT('Ctrl Pts',(53.9249115396487,31.2020751695661,4.9305));
#62466=CARTESIAN_POINT('Ctrl Pts',(53.8393993796462,27.3776456112999,4.92960110781498));
#62467=CARTESIAN_POINT('Ctrl Pts',(53.8466111964845,27.3724864184906,4.92990073854331));
#62468=CARTESIAN_POINT('Ctrl Pts',(53.853857414901,27.3673753141965,4.93020036927164));
#62469=CARTESIAN_POINT('Ctrl Pts',(53.8611373905627,27.3623127528964,4.93049999999996));
#62470=CARTESIAN_POINT('Origin',(55.,29.,4.9305));
#62471=CARTESIAN_POINT('',(52.5495,29.,4.9305));
#62472=CARTESIAN_POINT('Origin',(55.,29.,4.9305));
#62473=CARTESIAN_POINT('',(56.1167974000718,31.181218424916,4.9305));
#62474=CARTESIAN_POINT('Origin',(55.,29.,4.9305));
#62475=CARTESIAN_POINT('Ctrl Pts',(56.1167974000718,31.181218424916,4.9305));
#62476=CARTESIAN_POINT('Ctrl Pts',(56.156542077517,31.1563402429025,4.93049999999999));
#62477=CARTESIAN_POINT('Ctrl Pts',(56.1954769538157,31.1302582487305,4.93049999999999));
#62478=CARTESIAN_POINT('Ctrl Pts',(56.2335395857427,31.1029688213438,4.93049999999999));
#62479=CARTESIAN_POINT('Ctrl Pts',(56.3028413187012,31.0532821729542,4.9305));
#62480=CARTESIAN_POINT('Ctrl Pts',(56.3692540097722,30.9995944471324,4.9305));
#62481=CARTESIAN_POINT('Ctrl Pts',(56.4326084716472,30.9422671449757,4.9305));
#62482=CARTESIAN_POINT('Ctrl Pts',(56.4644952752616,30.9134138586953,4.9305));
#62483=CARTESIAN_POINT('Ctrl Pts',(56.4956067164715,30.8836380847701,4.93049999999998));
#62484=CARTESIAN_POINT('Ctrl Pts',(56.5259169844523,30.8529834405448,4.93049999999998));
#62485=CARTESIAN_POINT('Ctrl Pts',(56.5406079272072,30.8381255836702,4.93049999999998));
#62486=CARTESIAN_POINT('Ctrl Pts',(56.5551106138877,30.8230612430467,4.9305));
#62487=CARTESIAN_POINT('Ctrl Pts',(56.569421847319,30.8077952915011,4.93050000000001));
#62488=CARTESIAN_POINT('Ctrl Pts',(56.5804379355535,30.7960443079108,4.93050000000001));
#62489=CARTESIAN_POINT('Ctrl Pts',(56.5913347634252,30.7841800385731,4.93050000000001));
#62490=CARTESIAN_POINT('Ctrl Pts',(56.6021089968716,30.7722075680246,4.9305));
#62491=CARTESIAN_POINT('Ctrl Pts',(56.6589136001418,30.7090855424019,4.93049999999999));
#62492=CARTESIAN_POINT('Ctrl Pts',(56.7123354273433,30.6429353418224,4.93049999999999));
#62493=CARTESIAN_POINT('Ctrl Pts',(56.7622061712803,30.5741150402067,4.9305));
#62494=CARTESIAN_POINT('Ctrl Pts',(56.8007927973022,30.5208665215059,4.9305));
#62495=CARTESIAN_POINT('Ctrl Pts',(56.8372527063867,30.4660187139076,4.93049999999998));
#62496=CARTESIAN_POINT('Ctrl Pts',(56.8714879584134,30.4097297951466,4.93049999999998));
#62497=CARTESIAN_POINT('Ctrl Pts',(56.88841288161,30.3819021738949,4.93049999999997));
#62498=CARTESIAN_POINT('Ctrl Pts',(56.9047938120668,30.3537222699618,4.9305));
#62499=CARTESIAN_POINT('Ctrl Pts',(56.9206172107038,30.3252089451577,4.9305));
#62500=CARTESIAN_POINT('Ctrl Pts',(56.9301861753971,30.3079659365857,4.9305));
#62501=CARTESIAN_POINT('Ctrl Pts',(56.9395535970338,30.2905961984367,4.93050000000001));
#62502=CARTESIAN_POINT('Ctrl Pts',(56.948701992001,30.2731319608337,4.93050000000001));
#62503=CARTESIAN_POINT('Ctrl Pts',(56.9872728773672,30.1995003446863,4.93050000000001));
#62504=CARTESIAN_POINT('Ctrl Pts',(57.0220010953548,30.1241106605415,4.93050000000001));
#62505=CARTESIAN_POINT('Ctrl Pts',(57.0527290708383,30.0472951628104,4.93050000000001));
#62506=CARTESIAN_POINT('Ctrl Pts',(57.0828377959204,29.9720277015854,4.9305));
#62507=CARTESIAN_POINT('Ctrl Pts',(57.1091060242923,29.8953903735951,4.93049999999997));
#62508=CARTESIAN_POINT('Ctrl Pts',(57.1313374504974,29.8176867055421,4.93049999999999));
#62509=CARTESIAN_POINT('Ctrl Pts',(57.1531068495254,29.7415979229254,4.9305));
#62510=CARTESIAN_POINT('Ctrl Pts',(57.1710055955889,29.6644858782793,4.93050000000001));
#62511=CARTESIAN_POINT('Ctrl Pts',(57.1848010612909,29.5866393720501,4.93050000000001));
#62512=CARTESIAN_POINT('Ctrl Pts',(57.1899692544381,29.5574757476596,4.93050000000001));
#62513=CARTESIAN_POINT('Ctrl Pts',(57.1945610611568,29.5282091413259,4.93050000000002));
#62514=CARTESIAN_POINT('Ctrl Pts',(57.1985624054365,29.4988552147064,4.9305));
#62515=CARTESIAN_POINT('Ctrl Pts',(57.2002889244207,29.4861894433988,4.93049999999999));
#62516=CARTESIAN_POINT('Ctrl Pts',(57.2019054985971,29.4735074191975,4.93049999999999));
#62517=CARTESIAN_POINT('Ctrl Pts',(57.2034109371338,29.4608104216605,4.93049999999999));
#62518=CARTESIAN_POINT('Ctrl Pts',(57.2050605906204,29.4468971028871,4.93049999999999));
#62519=CARTESIAN_POINT('Ctrl Pts',(57.206575805631,29.4329737711374,4.93050000000001));
#62520=CARTESIAN_POINT('Ctrl Pts',(57.2079548720302,29.4190491854131,4.93050000000001));
#62521=CARTESIAN_POINT('Ctrl Pts',(57.2156500436978,29.3413501873025,4.93050000000002));
#62522=CARTESIAN_POINT('Ctrl Pts',(57.2191185329822,29.2635419889306,4.93049999999998));
#62523=CARTESIAN_POINT('Ctrl Pts',(57.2181822895949,29.1859045445621,4.93049999999998));
#62524=CARTESIAN_POINT('Ctrl Pts',(57.2178350531444,29.1571101616343,4.93049999999998));
#62525=CARTESIAN_POINT('Ctrl Pts',(57.2168814224251,29.1283393057487,4.93050000000001));
#62526=CARTESIAN_POINT('Ctrl Pts',(57.2153104878672,29.0996065241017,4.9305));
#62527=CARTESIAN_POINT('Ctrl Pts',(57.2109695624812,29.0202099250287,4.93049999999998));
#62528=CARTESIAN_POINT('Ctrl Pts',(57.2019185379677,28.9411024317745,4.93050000000001));
#62529=CARTESIAN_POINT('Ctrl Pts',(57.1883457297054,28.8626076791341,4.93049999999999));
#62530=CARTESIAN_POINT('Ctrl Pts',(57.1752101981451,28.7866418008357,4.93049999999998));
#62531=CARTESIAN_POINT('Ctrl Pts',(57.15783874972,28.7112491714072,4.9305));
#62532=CARTESIAN_POINT('Ctrl Pts',(57.136363509946,28.6367490856546,4.93050000000001));
#62533=CARTESIAN_POINT('Ctrl Pts',(57.1318688602108,28.621156626887,4.93050000000001));
#62534=CARTESIAN_POINT('Ctrl Pts',(57.1271930748425,28.6055997454899,4.93049999999999));
#62535=CARTESIAN_POINT('Ctrl Pts',(57.122345532269,28.5901070630992,4.9305));
#62536=CARTESIAN_POINT('Ctrl Pts',(57.0991415837965,28.5159475485739,4.9305));
#62537=CARTESIAN_POINT('Ctrl Pts',(57.0719758581837,28.4431451575644,4.93050000000001));
#62538=CARTESIAN_POINT('Ctrl Pts',(57.0410525219349,28.3719899830229,4.93050000000001));
#62539=CARTESIAN_POINT('Ctrl Pts',(57.010229889292,28.3010665293603,4.93050000000002));
#62540=CARTESIAN_POINT('Ctrl Pts',(56.9756733982571,28.2317787781305,4.93050000000002));
#62541=CARTESIAN_POINT('Ctrl Pts',(56.9375430523185,28.1644427906323,4.9305));
#62542=CARTESIAN_POINT('Ctrl Pts',(56.8997300162386,28.0976671540083,4.93049999999999));
#62543=CARTESIAN_POINT('Ctrl Pts',(56.8584017016581,28.0328102169304,4.9305));
#62544=CARTESIAN_POINT('Ctrl Pts',(56.8136826037627,27.9702198192552,4.93050000000001));
#62545=CARTESIAN_POINT('Ctrl Pts',(56.7965878517277,27.9462934124539,4.93050000000001));
#62546=CARTESIAN_POINT('Ctrl Pts',(56.7789973254977,27.9226986854038,4.93050000000004));
#62547=CARTESIAN_POINT('Ctrl Pts',(56.7609170509524,27.8994569494047,4.93050000000003));
#62548=CARTESIAN_POINT('Ctrl Pts',(56.7532986544245,27.889663693202,4.93050000000002));
#62549=CARTESIAN_POINT('Ctrl Pts',(56.745593119741,27.8799330323037,4.93050000000001));
#62550=CARTESIAN_POINT('Ctrl Pts',(56.7378102773488,27.8702778958364,4.93050000000001));
#62551=CARTESIAN_POINT('Ctrl Pts',(56.6906550139252,27.8117786380373,4.93050000000002));
#62552=CARTESIAN_POINT('Ctrl Pts',(56.6405828747768,27.7559424449364,4.93050000000003));
#62553=CARTESIAN_POINT('Ctrl Pts',(56.5877479254413,27.703056258697,4.93050000000003));
#62554=CARTESIAN_POINT('Ctrl Pts',(56.5363848379517,27.6516433616474,4.93050000000003));
#62555=CARTESIAN_POINT('Ctrl Pts',(56.4824100357581,27.6030179442244,4.93050000000002));
#62556=CARTESIAN_POINT('Ctrl Pts',(56.4259391803423,27.5574841144824,4.93050000000001));
#62557=CARTESIAN_POINT('Ctrl Pts',(56.3702590108002,27.5125878340689,4.93050000000001));
#62558=CARTESIAN_POINT('Ctrl Pts',(56.3121516549929,27.4706967082956,4.93050000000002));
#62559=CARTESIAN_POINT('Ctrl Pts',(56.2517113699718,27.432149026189,4.93050000000001));
#62560=CARTESIAN_POINT('Ctrl Pts',(56.2218244016619,27.4130876774026,4.9305));
#62561=CARTESIAN_POINT('Ctrl Pts',(56.1913667829791,27.3948446290381,4.9305));
#62562=CARTESIAN_POINT('Ctrl Pts',(56.1603489846691,27.3774656255483,4.9305));
#62563=CARTESIAN_POINT('Ctrl Pts',(56.426474702112,27.0036056037862,4.66549903655386));
#62564=CARTESIAN_POINT('Ctrl Pts',(57.0889864356691,27.4769547815182,4.70775074246383));
#62565=CARTESIAN_POINT('Ctrl Pts',(57.8940851946881,29.1267095489036,4.79223672516228));
#62566=CARTESIAN_POINT('Ctrl Pts',(56.4666838667935,31.5011894340363,4.91895698464923));
#62567=CARTESIAN_POINT('Ctrl Pts',(53.7014160468368,31.5896772934095,5.04565981501467));
#62568=CARTESIAN_POINT('Ctrl Pts',(52.1202558948328,29.321686656546,5.17236264538012));
#62569=CARTESIAN_POINT('Ctrl Pts',(53.1626841165763,26.7589385357385,5.29906547574558));
#62570=CARTESIAN_POINT('Ctrl Pts',(55.8794910541278,26.2390763871994,5.42576830611103));
#62571=CARTESIAN_POINT('Ctrl Pts',(57.7947951629564,28.2345376750715,5.55247113647648));
#62572=CARTESIAN_POINT('Ctrl Pts',(57.1635435827332,30.9277042403169,5.67917396684193));
#62573=CARTESIAN_POINT('Ctrl Pts',(54.5608454099514,31.8642389468711,5.80587679720738));
#62574=CARTESIAN_POINT('Ctrl Pts',(52.3583190771025,30.1909403202993,5.93257962757283));
#62575=CARTESIAN_POINT('Ctrl Pts',(52.5628805448572,27.4324299216987,6.05928245793829));
#62576=CARTESIAN_POINT('Ctrl Pts',(54.9881452069412,26.1023015851809,6.18598528830373));
#62577=CARTESIAN_POINT('Ctrl Pts',(57.4242099589407,27.4125438522027,6.31268811866919));
#62578=CARTESIAN_POINT('Ctrl Pts',(57.6513395150985,30.1692774386449,6.43939094903464));
#62579=CARTESIAN_POINT('Ctrl Pts',(55.4625722652183,31.8605653501733,6.5660937794001));
#62580=CARTESIAN_POINT('Ctrl Pts',(52.8523101761262,30.9453117267534,6.69279660976554));
#62581=CARTESIAN_POINT('Ctrl Pts',(52.1990194571466,28.2574926847764,6.81949944013099));
#62582=CARTESIAN_POINT('Ctrl Pts',(54.0979777606297,26.2462453713895,6.94620227049645));
#62583=CARTESIAN_POINT('Ctrl Pts',(56.8188572391422,26.744214702256,7.0729051008619));
#62584=CARTESIAN_POINT('Ctrl Pts',(57.8823969521443,29.2976520266901,7.19960793122735));
#62585=CARTESIAN_POINT('Ctrl Pts',(56.3195012012023,31.5798692697846,7.3263107615928));
#62586=CARTESIAN_POINT('Ctrl Pts',(53.5542780881045,31.5113138120211,7.45301359195826));
#62587=CARTESIAN_POINT('Ctrl Pts',(52.1063944474859,29.1544532493034,7.57971642232369));
#62588=CARTESIAN_POINT('Ctrl Pts',(53.2951595215023,26.6568551394786,7.70641925268916));
#62589=CARTESIAN_POINT('Ctrl Pts',(56.0373724898025,26.2943268458236,7.8331220830546));
#62590=CARTESIAN_POINT('Ctrl Pts',(57.8343333185037,28.3972035684727,7.95982491342006));
#62591=CARTESIAN_POINT('Ctrl Pts',(57.0486541976706,31.0493474268912,8.0865277437855));
#62592=CARTESIAN_POINT('Ctrl Pts',(54.3962446755182,31.8341292148724,8.21323057415097));
#62593=CARTESIAN_POINT('Ctrl Pts',(52.2939760314182,30.0364570322204,8.33993340451641));
#62594=CARTESIAN_POINT('Ctrl Pts',(52.6574320639669,27.2943668732086,8.46663623488187));
#62595=CARTESIAN_POINT('Ctrl Pts',(55.1554322223572,26.1064468689031,8.59333906524731));
#62596=CARTESIAN_POINT('Ctrl Pts',(57.5118027903804,27.5551278117337,8.72004189561275));
#62597=CARTESIAN_POINT('Ctrl Pts',(57.5794227061629,30.320373962602,8.84674472597822));
#62598=CARTESIAN_POINT('Ctrl Pts',(55.2966768114875,31.8824974878954,8.97344755634366));
#62599=CARTESIAN_POINT('Ctrl Pts',(52.743599484584,30.818093950329,9.10015038670912));
#62600=CARTESIAN_POINT('Ctrl Pts',(52.2465506688147,28.0970461369549,9.22685321707458));
#62601=CARTESIAN_POINT('Ctrl Pts',(54.258440443602,26.1987684275468,9.35355604744002));
#62602=CARTESIAN_POINT('Ctrl Pts',(56.9460380903923,26.8529684098888,9.48025887780547));
#62603=CARTESIAN_POINT('Ctrl Pts',(57.8604089672616,29.4635401149875,9.60696170817093));
#62604=CARTESIAN_POINT('Ctrl Pts',(56.1683798056569,31.6517348147818,9.73366453853637));
#62605=CARTESIAN_POINT('Ctrl Pts',(53.411724849185,31.4236730273486,9.86036736890182));
#62606=CARTESIAN_POINT('Ctrl Pts',(52.1023036489946,28.9871642856403,9.9870701992673));
#62607=CARTESIAN_POINT('Ctrl Pts',(53.4332586912184,26.5623514261588,10.1137730296327));
#62608=CARTESIAN_POINT('Ctrl Pts',(56.1918258875868,26.3587200163801,10.2404758599982));
#62609=CARTESIAN_POINT('Ctrl Pts',(57.864403257041,28.5618186685331,10.3671786903636));
#62610=CARTESIAN_POINT('Ctrl Pts',(56.9269409976151,31.1641874433383,10.4938815207291));
#62611=CARTESIAN_POINT('Ctrl Pts',(54.2336532084122,31.7945521095904,10.6205843510945));
#62612=CARTESIAN_POINT('Ctrl Pts',(52.238659379947,29.8785253998825,10.74728718146));
#62613=CARTESIAN_POINT('Ctrl Pts',(52.7597946717299,27.16198776245,10.8739900118254));
#62614=CARTESIAN_POINT('Ctrl Pts',(55.3222014462345,26.1202439120236,11.0006928421909));
#62615=CARTESIAN_POINT('Ctrl Pts',(57.5910187824897,27.7025291652685,11.1273956725564));
#62616=CARTESIAN_POINT('Ctrl Pts',(57.4989039822355,30.4670677509103,11.2540985029218));
#62617=CARTESIAN_POINT('Ctrl Pts',(55.1297919029255,31.8948165676132,11.3808013332873));
#62618=CARTESIAN_POINT('Ctrl Pts',(52.6424136509631,30.6848131958851,11.5075041636527));
#62619=CARTESIAN_POINT('Ctrl Pts',(52.3032642785649,27.9396107568781,11.6342069940182));
#62620=CARTESIAN_POINT('Ctrl Pts',(54.4213761469714,26.1606332862943,11.7609098243836));
#62621=CARTESIAN_POINT('Ctrl Pts',(57.0667291372093,26.9688821866757,11.887612654749));
#62622=CARTESIAN_POINT('Ctrl Pts',(57.8288818702845,29.62788236332,12.0143154851145));
#62623=CARTESIAN_POINT('Ctrl Pts',(56.013362004813,31.7147571429862,12.14101831548));
#62624=CARTESIAN_POINT('Ctrl Pts',(53.2744683146323,31.3279495915903,12.2677211458454));
#62625=CARTESIAN_POINT('Ctrl Pts',(52.1078763136874,28.8199181262256,12.3944239762109));
#62626=CARTESIAN_POINT('Ctrl Pts',(53.5765827520745,26.4759769738567,12.5211268065763));
#62627=CARTESIAN_POINT('Ctrl Pts',(56.3423046914688,26.4319215328472,12.6478296369418));
#62628=CARTESIAN_POINT('Ctrl Pts',(57.8849207605029,28.7278950500041,12.7745324673072));
#62629=CARTESIAN_POINT('Ctrl Pts',(56.7988016845878,31.27181015882,12.9012352976727));
#62630=CARTESIAN_POINT('Ctrl Pts',(54.0736174142975,31.7456555142808,13.0279381280381));
#62631=CARTESIAN_POINT('Ctrl Pts',(52.19255146228,29.7176639925804,13.1546409584036));
#62632=CARTESIAN_POINT('Ctrl Pts',(52.8696280907382,27.0357381980954,13.281343788769));
#62633=CARTESIAN_POINT('Ctrl Pts',(55.4878961676276,26.1436445900751,13.4080466191345));
#62634=CARTESIAN_POINT('Ctrl Pts',(57.6615940433218,27.8542574256199,13.5347494494999));
#62635=CARTESIAN_POINT('Ctrl Pts',(57.410051718641,30.6088690473959,13.6614522798654));
#62636=CARTESIAN_POINT('Ctrl Pts',(54.9624741542151,31.897481787534,13.7881551102308));
#62637=CARTESIAN_POINT('Ctrl Pts',(52.5490900799565,30.5459137951471,13.9148579405963));
#62638=CARTESIAN_POINT('Ctrl Pts',(52.3689711726764,27.7857116454543,14.0415607709617));
#62639=CARTESIAN_POINT('Ctrl Pts',(54.586241490241,26.1319670863473,14.1682636013272));
#62640=CARTESIAN_POINT('Ctrl Pts',(57.1805278946999,27.0915694933719,14.2949664316926));
#62641=CARTESIAN_POINT('Ctrl Pts',(57.7879207976748,29.790130700635,14.4216692620581));
#62642=CARTESIAN_POINT('Ctrl Pts',(55.8549647654138,31.7687260875887,14.5483720924235));
#62643=CARTESIAN_POINT('Ctrl Pts',(53.1429662175641,31.2244627281851,14.675074922789));
#62644=CARTESIAN_POINT('Ctrl Pts',(52.1230938577475,28.6532725178718,14.8017777531545));
#62645=CARTESIAN_POINT('Ctrl Pts',(53.7246537356544,26.3980198301654,14.9284805835199));
#62646=CARTESIAN_POINT('Ctrl Pts',(56.488307073099,26.5136872774414,15.0551834138854));
#62647=CARTESIAN_POINT('Ctrl Pts',(57.8958174054756,28.8948788682595,15.1818862442508));
#62648=CARTESIAN_POINT('Ctrl Pts',(56.6646635875745,31.3718566648084,15.3085890746163));
#62649=CARTESIAN_POINT('Ctrl Pts',(53.9166709929956,31.6876024930737,15.4352919049817));
#62650=CARTESIAN_POINT('Ctrl Pts',(52.1558060426984,29.5544092634894,15.5619947353472));
#62651=CARTESIAN_POINT('Ctrl Pts',(52.986566039947,26.9160392070151,15.6886975657126));
#62652=CARTESIAN_POINT('Ctrl Pts',(55.6519638148733,26.1765708646597,15.8154003960781));
#62653=CARTESIAN_POINT('Ctrl Pts',(57.7232932129982,28.0098065975625,15.9421032264435));
#62654=CARTESIAN_POINT('Ctrl Pts',(57.3131622268308,30.7453049620501,16.068806056809));
#62655=CARTESIAN_POINT('Ctrl Pts',(54.7952815496182,31.8904842594738,16.1955088871744));
#62656=CARTESIAN_POINT('Ctrl Pts',(52.463939994279,30.4018589606574,16.3222117175399));
#62657=CARTESIAN_POINT('Ctrl Pts',(52.4434522266802,27.6358620374293,16.4489145479053));
#62658=CARTESIAN_POINT('Ctrl Pts',(54.7524866676209,26.1128654259824,16.5756173782708));
#62659=CARTESIAN_POINT('Ctrl Pts',(57.2870548579027,27.2206211827898,16.7023202086362));
#62660=CARTESIAN_POINT('Ctrl Pts',(57.7376623496078,29.9497440485375,16.8290230390017));
#62661=CARTESIAN_POINT('Ctrl Pts',(55.6937163229126,31.8134616687487,16.9557258693671));
#62662=CARTESIAN_POINT('Ctrl Pts',(53.0176571014176,31.1135575531868,17.0824286997326));
#62663=CARTESIAN_POINT('Ctrl Pts',(52.1479055325239,28.4877832033359,17.209131530098));
#62664=CARTESIAN_POINT('Ctrl Pts',(53.8769778433068,26.3287399726403,17.3358343604635));
#62665=CARTESIAN_POINT('Ctrl Pts',(56.6293461323619,26.6037445713885,17.4625371908289));
#62666=CARTESIAN_POINT('Ctrl Pts',(57.8970568529781,29.062213252654,17.5892400211944));
#62667=CARTESIAN_POINT('Ctrl Pts',(56.5249740407513,31.4639933184218,17.7159428515598));
#62668=CARTESIAN_POINT('Ctrl Pts',(53.7633373416581,31.6205866457067,17.8426456819253));
#62669=CARTESIAN_POINT('Ctrl Pts',(52.1285456626905,29.3893056471977,17.9693485122907));
#62670=CARTESIAN_POINT('Ctrl Pts',(53.1102185455736,26.8032899707292,18.0960513426562));
#62671=CARTESIAN_POINT('Ctrl Pts',(55.8138572424009,26.2189129306717,18.2227541730216));
#62672=CARTESIAN_POINT('Ctrl Pts',(57.7759105323216,28.1686579436003,18.3494570033871));
#62673=CARTESIAN_POINT('Ctrl Pts',(57.2085586214295,30.8759204977563,18.4761598337526));
#62674=CARTESIAN_POINT('Ctrl Pts',(54.6287716560576,31.8738473193346,18.602862664118));
#62675=CARTESIAN_POINT('Ctrl Pts',(52.3872473590691,30.2531290976998,18.7295654944835));
#62676=CARTESIAN_POINT('Ctrl Pts',(52.5264590553553,27.490561662949,18.8562683248489));
#62677=CARTESIAN_POINT('Ctrl Pts',(54.9195572717431,26.1033920069047,18.9829711552144));
#62678=CARTESIAN_POINT('Ctrl Pts',(57.3859547724023,27.3556068833019,19.1096739855798));
#62679=CARTESIAN_POINT('Ctrl Pts',(57.6782741318717,30.1061901160017,19.2363768159453));
#62680=CARTESIAN_POINT('Ctrl Pts',(55.530154421177,31.8488146987648,19.3630796463107));
#62681=CARTESIAN_POINT('Ctrl Pts',(52.8989588567946,30.9956039218132,19.4897824766762));
#62682=CARTESIAN_POINT('Ctrl Pts',(52.1822285941116,28.3240020692746,19.6164853070416));
#62683=CARTESIAN_POINT('Ctrl Pts',(54.033047092729,26.2683684411494,19.7431881374071));
#62684=CARTESIAN_POINT('Ctrl Pts',(56.7649515212204,26.7017930846051,19.8698909677725));
#62685=CARTESIAN_POINT('Ctrl Pts',(57.8886349695947,29.2293401634538,19.996593798138));
#62686=CARTESIAN_POINT('Ctrl Pts',(56.3801988917198,31.5479128551569,20.1232966285034));
#62687=CARTESIAN_POINT('Ctrl Pts',(53.6141278092525,31.5448314618743,20.2499994588689));
#62688=CARTESIAN_POINT('Ctrl Pts',(52.1108612323695,29.222903744055,20.3767022892343));
#62689=CARTESIAN_POINT('Ctrl Pts',(53.2401732414635,26.6978664942751,20.5034051195998));
#62690=CARTESIAN_POINT('Ctrl Pts',(55.9730365556825,26.2705295822934,20.6301079499652));
#62691=CARTESIAN_POINT('Ctrl Pts',(57.8192705283958,28.3302817142776,20.7568107803307));
#62692=CARTESIAN_POINT('Ctrl Pts',(57.096589743788,31.0002800668915,20.8835136106961));
#62693=CARTESIAN_POINT('Ctrl Pts',(54.4634997615441,31.847626450769,21.0102164410616));
#62694=CARTESIAN_POINT('Ctrl Pts',(52.3192679391206,30.1002201992904,21.136919271427));
#62695=CARTESIAN_POINT('Ctrl Pts',(52.6177148327956,27.3502950867379,21.2636221017925));
#62696=CARTESIAN_POINT('Ctrl Pts',(55.0868961587425,26.1035784106085,21.3903249321579));
#62697=CARTESIAN_POINT('Ctrl Pts',(57.4768977873141,27.4960764560288,21.5170277625234));
#62698=CARTESIAN_POINT('Ctrl Pts',(57.609954259127,30.2589471314825,21.6437305928888));
#62699=CARTESIAN_POINT('Ctrl Pts',(55.3648243972843,31.8746673638808,21.7704334232543));
#62700=CARTESIAN_POINT('Ctrl Pts',(52.7872675667032,30.8709950298697,21.8971362536197));
#62701=CARTESIAN_POINT('Ctrl Pts',(52.2259481112485,28.1624756293933,22.0238390839852));
#62702=CARTESIAN_POINT('Ctrl Pts',(54.1923419291723,26.2171059332353,22.1505419143506));
#62703=CARTESIAN_POINT('Ctrl Pts',(56.894669215097,26.8075070798911,22.2772447447161));
#62704=CARTESIAN_POINT('Ctrl Pts',(57.8705833628646,29.395699817874,22.4039475750815));
#62705=CARTESIAN_POINT('Ctrl Pts',(56.2308140472889,31.6233401849381,22.530650405447));
#62706=CARTESIAN_POINT('Ctrl Pts',(53.4695535133207,31.4605802263176,22.6573532358124));
#62707=CARTESIAN_POINT('Ctrl Pts',(52.1027852305065,29.0557768047726,22.7840560661779));
#62708=CARTESIAN_POINT('Ctrl Pts',(53.3760486654888,26.6000844521299,22.9107588965434));
#62709=CARTESIAN_POINT('Ctrl Pts',(56.1288691699566,26.3313190323434,23.0374617269088));
#62710=CARTESIAN_POINT('Ctrl Pts',(57.8534279746937,28.4940010520624,23.1641645572743));
#62711=CARTESIAN_POINT('Ctrl Pts',(56.9772382162707,31.1182392339781,23.2908673876397));
#62712=CARTESIAN_POINT('Ctrl Pts',(54.3007838883385,31.8113778822148,23.4175702180052));
#62713=CARTESIAN_POINT('Ctrl Pts',(52.2587135542228,29.9447003610909,23.5442730483706));
#62714=CARTESIAN_POINT('Ctrl Pts',(52.7200168224909,27.2132689961283,23.6709758787361));
#62715=CARTESIAN_POINT('Ctrl Pts',(54.4042650983531,26.4844591653022,23.755444432313));
#62716=CARTESIAN_POINT('Ctrl Pts',(55.215028655103,26.5557857257648,23.7976787091015));
#62717=CARTESIAN_POINT('Ctrl Pts',(56.336854785976,27.1290313811225,4.75449970191464));
#62718=CARTESIAN_POINT('Ctrl Pts',(56.9577434568089,27.5726418515725,4.79675140782461));
#62719=CARTESIAN_POINT('Ctrl Pts',(57.7122609590011,29.1187488755531,4.88123739052305));
#62720=CARTESIAN_POINT('Ctrl Pts',(56.3745377635746,31.3440493270392,5.00795765001001));
#62721=CARTESIAN_POINT('Ctrl Pts',(53.7830010793689,31.4269778347293,5.13466048037544));
#62722=CARTESIAN_POINT('Ctrl Pts',(52.3011791350529,29.3014763218384,5.26136331074091));
#62723=CARTESIAN_POINT('Ctrl Pts',(53.2781156031241,26.899735803426,5.38806614110635));
#62724=CARTESIAN_POINT('Ctrl Pts',(55.8242360156779,26.4125345931323,5.51476897147182));
#62725=CARTESIAN_POINT('Ctrl Pts',(57.6192089378726,28.2826287272744,5.64147180183725));
#62726=CARTESIAN_POINT('Ctrl Pts',(57.0276164652357,30.8065940011404,5.76817463220272));
#62727=CARTESIAN_POINT('Ctrl Pts',(54.5884358028779,31.6842898360794,5.89487746256816));
#62728=CARTESIAN_POINT('Ctrl Pts',(52.5242857237017,30.1161181229829,6.02158029293361));
#62729=CARTESIAN_POINT('Ctrl Pts',(52.7159953816362,27.5309143173537,6.14828312329906));
#62730=CARTESIAN_POINT('Ctrl Pts',(54.9888899979691,26.2843528255842,6.27498595366452));
#62731=CARTESIAN_POINT('Ctrl Pts',(57.2719061761293,27.5122776130781,6.40168878402996));
#62732=CARTESIAN_POINT('Ctrl Pts',(57.4847660563198,30.0958162368193,6.52839161439542));
#62733=CARTESIAN_POINT('Ctrl Pts',(55.4335106298776,31.6808470373252,6.65509444476087));
#62734=CARTESIAN_POINT('Ctrl Pts',(52.9872412629635,30.8230952769617,6.78179727512633));
#62735=CARTESIAN_POINT('Ctrl Pts',(52.3749942858467,28.3041415620556,6.90850010549177));
#62736=CARTESIAN_POINT('Ctrl Pts',(54.1546483467435,26.4192531776336,7.03520293585723));
#62737=CARTESIAN_POINT('Ctrl Pts',(56.7045854381815,26.8859370117407,7.16190576622267));
#62738=CARTESIAN_POINT('Ctrl Pts',(57.7013070437574,29.2789516952854,7.28860859658814));
#62739=CARTESIAN_POINT('Ctrl Pts',(56.2366020184702,31.4177860114852,7.41531142695358));
#62740=CARTESIAN_POINT('Ctrl Pts',(53.6451072323636,31.353537629316,7.54201425731903));
#62741=CARTESIAN_POINT('Ctrl Pts',(52.2881885491009,29.1447495460208,7.66871708768449));
#62742=CARTESIAN_POINT('Ctrl Pts',(53.4022680881541,26.8040659141131,7.79541991804993));
#62743=CARTESIAN_POINT('Ctrl Pts',(55.9721983683126,26.4643138780574,7.92212274841539));
#62744=CARTESIAN_POINT('Ctrl Pts',(57.6562630632586,28.4350749485684,8.04882557878084));
#62745=CARTESIAN_POINT('Ctrl Pts',(56.9199451381163,30.9205948144127,8.17552840914629));
#62746=CARTESIAN_POINT('Ctrl Pts',(54.4341762991682,31.656071782673,8.30223123951175));
#62747=CARTESIAN_POINT('Ctrl Pts',(52.4639851039711,29.9713404254074,8.42893406987719));
#62748=CARTESIAN_POINT('Ctrl Pts',(52.8046065926559,27.4015252389023,8.55563690024265));
#62749=CARTESIAN_POINT('Ctrl Pts',(55.1456670139649,26.2882376770822,8.6823397306081));
#62750=CARTESIAN_POINT('Ctrl Pts',(57.3539958870469,27.645903571127,8.80904256097356));
#62751=CARTESIAN_POINT('Ctrl Pts',(57.4173675037376,30.2374199476299,8.93574539133899));
#62752=CARTESIAN_POINT('Ctrl Pts',(55.2780377491013,31.7014012632341,9.06244822170446));
#62753=CARTESIAN_POINT('Ctrl Pts',(52.8853604458274,30.7038701038671,9.18915105206991));
#62754=CARTESIAN_POINT('Ctrl Pts',(52.4195392943965,28.1537752533991,9.31585388243536));
#62755=CARTESIAN_POINT('Ctrl Pts',(54.3050297768413,26.3747590274706,9.44255671280081));
#62756=CARTESIAN_POINT('Ctrl Pts',(56.8237760059684,26.9878581424317,9.56925954316626));
#62757=CARTESIAN_POINT('Ctrl Pts',(57.68070047935,29.4344176733702,9.69596237353171));
#62758=CARTESIAN_POINT('Ctrl Pts',(56.0949749986577,31.4851365208452,9.82266520389716));
#62759=CARTESIAN_POINT('Ctrl Pts',(53.5115100648683,31.2714029778829,9.94936803426261));
#62760=CARTESIAN_POINT('Ctrl Pts',(52.2843547597365,28.9879707041789,10.0760708646281));
#62761=CARTESIAN_POINT('Ctrl Pts',(53.5316910184738,26.7154995054294,10.2027736949935));
#62762=CARTESIAN_POINT('Ctrl Pts',(56.1169480534857,26.5246614735075,10.329476525359));
#62763=CARTESIAN_POINT('Ctrl Pts',(57.6844438232736,28.5893479153682,10.4561793557244));
#62764=CARTESIAN_POINT('Ctrl Pts',(56.8058787100404,31.0282198745568,10.5828821860899));
#62765=CARTESIAN_POINT('Ctrl Pts',(54.2817998282517,31.6189811546143,10.7095850164553));
#62766=CARTESIAN_POINT('Ctrl Pts',(52.4121437848409,29.8233310297726,10.8362878468208));
#62767=CARTESIAN_POINT('Ctrl Pts',(52.9005381516877,27.277462998248,10.9629906771862));
#62768=CARTESIAN_POINT('Ctrl Pts',(55.3019587692717,26.3011679050775,11.0896935075517));
#62769=CARTESIAN_POINT('Ctrl Pts',(57.428235043213,27.7840442648531,11.2163963379172));
#62770=CARTESIAN_POINT('Ctrl Pts',(57.34190746138,30.3748975297296,11.3430991682826));
#62771=CARTESIAN_POINT('Ctrl Pts',(55.1216375771333,31.7129463825798,11.469801998648));
#62772=CARTESIAN_POINT('Ctrl Pts',(52.7905317287469,30.5789628663303,11.5965048290135));
#62773=CARTESIAN_POINT('Ctrl Pts',(52.4726898062928,28.0062309324054,11.723207659379));
#62774=CARTESIAN_POINT('Ctrl Pts',(54.4577288569815,26.3390197703904,11.8499104897444));
#62775=CARTESIAN_POINT('Ctrl Pts',(56.9368844987602,27.0964895026856,11.9766133201099));
#62776=CARTESIAN_POINT('Ctrl Pts',(57.6511541085528,29.5884349306662,12.1033161504753));
#62777=CARTESIAN_POINT('Ctrl Pts',(55.9496963696971,31.5441993986927,12.2300189808408));
#62778=CARTESIAN_POINT('Ctrl Pts',(53.3828768301873,31.1816934772279,12.3567218112062));
#62779=CARTESIAN_POINT('Ctrl Pts',(52.2895773153514,28.831231977359,12.4834246415716));
#62780=CARTESIAN_POINT('Ctrl Pts',(53.6660105801299,26.634551627577,12.6101274719371));
#62781=CARTESIAN_POINT('Ctrl Pts',(56.2579728531963,26.5932640203909,12.7368303023026));
#62782=CARTESIAN_POINT('Ctrl Pts',(57.7036722909489,28.7449903568908,12.863533132668));
#62783=CARTESIAN_POINT('Ctrl Pts',(56.6857898969414,31.1290810689813,12.9902359630335));
#62784=CARTESIAN_POINT('Ctrl Pts',(54.1318184672272,31.5731565442227,13.1169387933989));
#62785=CARTESIAN_POINT('Ctrl Pts',(52.3689326502071,29.6725759256601,13.2436416237644));
#62786=CARTESIAN_POINT('Ctrl Pts',(53.0034711596436,27.1591452081848,13.3703444541298));
#62787=CARTESIAN_POINT('Ctrl Pts',(55.4572435289504,26.3230984085781,13.4970472844953));
#62788=CARTESIAN_POINT('Ctrl Pts',(57.4943763319966,27.9262400224913,13.6237501148607));
#62789=CARTESIAN_POINT('Ctrl Pts',(57.2586374435837,30.5077899964403,13.7504529452262));
#62790=CARTESIAN_POINT('Ctrl Pts',(54.9648317586977,31.7154441569895,13.8771557755916));
#62791=CARTESIAN_POINT('Ctrl Pts',(52.7030713185765,30.4487899804244,14.0038586059571));
#62792=CARTESIAN_POINT('Ctrl Pts',(52.5342685891023,27.8620007099138,14.1305614363225));
#62793=CARTESIAN_POINT('Ctrl Pts',(54.6122363451726,26.3121545574719,14.257264266688));
#62794=CARTESIAN_POINT('Ctrl Pts',(57.0435337182411,27.2114688380306,14.3839670970534));
#62795=CARTESIAN_POINT('Ctrl Pts',(57.6127664625076,29.7404898293159,14.5106699274189));
#62796=CARTESIAN_POINT('Ctrl Pts',(55.8012506193009,31.5947776821905,14.6373727577843));
#62797=CARTESIAN_POINT('Ctrl Pts',(53.2596365038281,31.0847082952096,14.7640755881498));
#62798=CARTESIAN_POINT('Ctrl Pts',(52.3038387996787,28.675056071288,14.8907784185152));
#62799=CARTESIAN_POINT('Ctrl Pts',(53.804778833622,26.5614922312271,15.0174812488807));
#62800=CARTESIAN_POINT('Ctrl Pts',(56.3948024670389,26.6698927379054,15.1441840792461));
#62801=CARTESIAN_POINT('Ctrl Pts',(57.7138843416507,28.9014832244368,15.2708869096116));
#62802=CARTESIAN_POINT('Ctrl Pts',(56.5600791803697,31.2228420380001,15.3975897399771));
#62803=CARTESIAN_POINT('Ctrl Pts',(53.9847323856103,31.518750770937,15.5242925703425));
#62804=CARTESIAN_POINT('Ctrl Pts',(52.3344958039333,29.5195778629568,15.6509954007079));
#62805=CARTESIAN_POINT('Ctrl Pts',(53.1130623475071,27.0469664440852,15.7776982310734));
#62806=CARTESIAN_POINT('Ctrl Pts',(55.6110034372893,26.3539560520383,15.9044010614389));
#62807=CARTESIAN_POINT('Ctrl Pts',(57.5521991802746,28.0720166385492,16.0311038918043));
#62808=CARTESIAN_POINT('Ctrl Pts',(57.1678351456911,30.6356541676133,16.1578067221698));
#62809=CARTESIAN_POINT('Ctrl Pts',(54.8081432220527,31.7088862566892,16.2845095525352));
#62810=CARTESIAN_POINT('Ctrl Pts',(52.6232708851051,30.3137855568301,16.4112123829007));
#62811=CARTESIAN_POINT('Ctrl Pts',(52.604070285103,27.7215655761057,16.5379152132661));
#62812=CARTESIAN_POINT('Ctrl Pts',(54.7680369778069,26.2942529809203,16.6646180436316));
#62813=CARTESIAN_POINT('Ctrl Pts',(57.1433680022858,27.3324127064224,16.791320873997));
#62814=CARTESIAN_POINT('Ctrl Pts',(57.5656655593267,29.8900752847982,16.9180237043625));
#62815=CARTESIAN_POINT('Ctrl Pts',(55.6501327959216,31.6367026989388,17.0447265347279));
#62816=CARTESIAN_POINT('Ctrl Pts',(53.142200077231,30.9807708655682,17.1714293650934));
#62817=CARTESIAN_POINT('Ctrl Pts',(52.32709165241,28.519963813544,17.2981321954588));
#62818=CARTESIAN_POINT('Ctrl Pts',(53.9475330037683,26.4965649605458,17.4248350258243));
#62819=CARTESIAN_POINT('Ctrl Pts',(56.5269805849585,26.7542920786345,17.5515378561897));
#62820=CARTESIAN_POINT('Ctrl Pts',(57.7150459194364,29.0583046334003,17.6782406865552));
#62821=CARTESIAN_POINT('Ctrl Pts',(56.4291657902164,31.3091901002298,17.8049435169206));
#62822=CARTESIAN_POINT('Ctrl Pts',(53.8410320975238,31.4559452713678,17.9316463472861));
#62823=CARTESIAN_POINT('Ctrl Pts',(52.3089480886971,29.3648470715205,18.0583491776515));
#62824=CARTESIAN_POINT('Ctrl Pts',(53.2289462420482,26.9413008084306,18.185052008017));
#62825=CARTESIAN_POINT('Ctrl Pts',(55.7627257237678,26.3936379289848,18.3117548383824));
#62826=CARTESIAN_POINT('Ctrl Pts',(57.6015107559083,28.2208879658114,18.4384576687479));
#62827=CARTESIAN_POINT('Ctrl Pts',(57.0698033822789,30.7580636318493,18.5651604991133));
#62828=CARTESIAN_POINT('Ctrl Pts',(54.6520945043367,31.6932945514762,18.6918633294788));
#62829=CARTESIAN_POINT('Ctrl Pts',(52.5513965530351,30.1743998188159,18.8185661598443));
#62830=CARTESIAN_POINT('Ctrl Pts',(52.6818621141615,27.5853938650053,18.9452689902097));
#62831=CARTESIAN_POINT('Ctrl Pts',(54.9246111787976,26.2853747403073,19.0719718205751));
#62832=CARTESIAN_POINT('Ctrl Pts',(57.2360544157466,27.4589177748269,19.1986746509406));
#62833=CARTESIAN_POINT('Ctrl Pts',(57.5100084747716,30.0366924478834,19.325377481306));
#62834=CARTESIAN_POINT('Ctrl Pts',(55.4968468590487,31.6698346341256,19.4520803116715));
#62835=CARTESIAN_POINT('Ctrl Pts',(53.0309591865401,30.8702278069414,19.578783142037));
#62836=CARTESIAN_POINT('Ctrl Pts',(52.3592583281211,28.3664724178689,19.7054859724024));
#62837=CARTESIAN_POINT('Ctrl Pts',(54.093797022839,26.4399863400551,19.8321888027679));
#62838=CARTESIAN_POINT('Ctrl Pts',(56.6540664090754,26.8461805810787,19.9588916331333));
#62839=CARTESIAN_POINT('Ctrl Pts',(57.7071531505767,29.2149316035369,20.0855944634988));
#62840=CARTESIAN_POINT('Ctrl Pts',(56.2934863066709,31.3878372954132,20.2122972938642));
#62841=CARTESIAN_POINT('Ctrl Pts',(53.7011968258471,31.3849494942125,20.3390001242296));
#62842=CARTESIAN_POINT('Ctrl Pts',(52.2923747030794,29.2088995596001,20.4657029545951));
#62843=CARTESIAN_POINT('Ctrl Pts',(53.3507363844905,26.8425006833086,20.5924057849606));
#62844=CARTESIAN_POINT('Ctrl Pts',(55.9119044133541,26.4420117050176,20.719108615326));
#62845=CARTESIAN_POINT('Ctrl Pts',(57.6421466102883,28.3723575369419,20.8458114456915));
#62846=CARTESIAN_POINT('Ctrl Pts',(56.9648690783381,30.8746101678194,20.9725142760569));
#62847=CARTESIAN_POINT('Ctrl Pts',(54.4972060069519,31.6687210391787,21.0992171064224));
#62848=CARTESIAN_POINT('Ctrl Pts',(52.4876880184416,30.0310975980655,21.2259199367878));
#62849=CARTESIAN_POINT('Ctrl Pts',(52.7673846422782,27.453939698,21.3526227671533));
#62850=CARTESIAN_POINT('Ctrl Pts',(55.0814368074849,26.2855494329837,21.4793255975187));
#62851=CARTESIAN_POINT('Ctrl Pts',(57.3212838310008,27.5905621848581,21.6060284278842));
#62852=CARTESIAN_POINT('Ctrl Pts',(57.4459808767212,30.1798523279252,21.7327312582496));
#62853=CARTESIAN_POINT('Ctrl Pts',(55.3419038843298,31.6940630757792,21.8594340886151));
#62854=CARTESIAN_POINT('Ctrl Pts',(52.9262850303917,30.7534476121557,21.9861369189805));
#62855=CARTESIAN_POINT('Ctrl Pts',(52.4002311162387,28.215094062615,22.112839749346));
#62856=CARTESIAN_POINT('Ctrl Pts',(54.2430839777112,26.3919444582436,22.2395425797114));
#62857=CARTESIAN_POINT('Ctrl Pts',(56.7756344394286,26.9452529728523,22.3662454100769));
#62858=CARTESIAN_POINT('Ctrl Pts',(57.6902356568308,29.3708395210595,22.4929482404423));
#62859=CARTESIAN_POINT('Ctrl Pts',(56.1534867371489,31.4585258163257,22.6196510708078));
#62860=CARTESIAN_POINT('Ctrl Pts',(53.5657055765741,31.3059914395681,22.7463539011732));
#62861=CARTESIAN_POINT('Ctrl Pts',(52.2848060853352,29.0522725627704,22.8730567315387));
#62862=CARTESIAN_POINT('Ctrl Pts',(53.4780752785037,26.750861910584,22.9997595619041));
#62863=CARTESIAN_POINT('Ctrl Pts',(56.0579466641524,26.4989819878525,23.1264623922696));
#62864=CARTESIAN_POINT('Ctrl Pts',(57.6741580756808,28.5257910187628,23.253165222635));
#62865=CARTESIAN_POINT('Ctrl Pts',(56.8530159480028,30.9851584143716,23.3798680530005));
#62866=CARTESIAN_POINT('Ctrl Pts',(54.3447129458923,31.634749828694,23.5065708833659));
#62867=CARTESIAN_POINT('Ctrl Pts',(52.4309380325199,29.8853484728245,23.6332737137315));
#62868=CARTESIAN_POINT('Ctrl Pts',(52.8632593916422,27.3255224293559,23.7599765440968));
#62869=CARTESIAN_POINT('Ctrl Pts',(54.4416928297007,26.6425009155755,23.8444450976738));
#62870=CARTESIAN_POINT('Ctrl Pts',(55.2015192321819,26.7093463027249,23.8866793744623));
#62871=CARTESIAN_POINT('Ctrl Pts',(56.24723486984,27.2544571584588,4.84350036727542));
#62872=CARTESIAN_POINT('Ctrl Pts',(56.8265004779488,27.6683289216268,4.88575207318538));
#62873=CARTESIAN_POINT('Ctrl Pts',(57.5304367233141,29.1107882022024,4.97023805588383));
#62874=CARTESIAN_POINT('Ctrl Pts',(56.2823916603557,31.1869092200421,5.09695831537079));
#62875=CARTESIAN_POINT('Ctrl Pts',(53.8645861119009,31.264278376049,5.22366114573623));
#62876=CARTESIAN_POINT('Ctrl Pts',(52.4821023752731,29.2812659871308,5.35036397610169));
#62877=CARTESIAN_POINT('Ctrl Pts',(53.393547089672,27.0405330711135,5.47706680646714));
#62878=CARTESIAN_POINT('Ctrl Pts',(55.7689809772278,26.5859927990651,5.60376963683258));
#62879=CARTESIAN_POINT('Ctrl Pts',(57.4436227127888,28.3307197794772,5.73047246719804));
#62880=CARTESIAN_POINT('Ctrl Pts',(56.8916893477383,30.6854837619637,5.85717529756349));
#62881=CARTESIAN_POINT('Ctrl Pts',(54.6160261958042,31.5043407252877,5.98387812792894));
#62882=CARTESIAN_POINT('Ctrl Pts',(52.6902523703009,30.0412959256666,6.1105809582944));
#62883=CARTESIAN_POINT('Ctrl Pts',(52.8691102184153,27.6293987130087,6.23728378865985));
#62884=CARTESIAN_POINT('Ctrl Pts',(54.989634788997,26.4664040659876,6.3639866190253));
#62885=CARTESIAN_POINT('Ctrl Pts',(57.1196023933181,27.6120113739534,6.49068944939075));
#62886=CARTESIAN_POINT('Ctrl Pts',(57.3181925975411,30.0223550349936,6.6173922797562));
#62887=CARTESIAN_POINT('Ctrl Pts',(55.4044489945367,31.5011287244771,6.74409511012166));
#62888=CARTESIAN_POINT('Ctrl Pts',(53.1221723498006,30.7008788271698,6.8707979404871));
#62889=CARTESIAN_POINT('Ctrl Pts',(52.5509691145466,28.3507904393347,6.99750077085256));
#62890=CARTESIAN_POINT('Ctrl Pts',(54.2113189328573,26.5922609838778,7.124203601218));
#62891=CARTESIAN_POINT('Ctrl Pts',(56.5903136372207,27.0276593212251,7.25090643158346));
#62892=CARTESIAN_POINT('Ctrl Pts',(57.5202171353705,29.2602513638809,7.37760926194891));
#62893=CARTESIAN_POINT('Ctrl Pts',(56.1537028357381,31.2557027531859,7.50431209231437));
#62894=CARTESIAN_POINT('Ctrl Pts',(53.7359363766226,31.1957614466111,7.63101492267981));
#62895=CARTESIAN_POINT('Ctrl Pts',(52.4699826507158,29.1350458427381,7.75771775304527));
#62896=CARTESIAN_POINT('Ctrl Pts',(53.5093766548059,26.9512766887474,7.88442058341071));
#62897=CARTESIAN_POINT('Ctrl Pts',(55.9070242468225,26.6343009102913,8.01112341377616));
#62898=CARTESIAN_POINT('Ctrl Pts',(57.4781928080136,28.472946328664,8.13782624414162));
#62899=CARTESIAN_POINT('Ctrl Pts',(56.7912360785621,30.7918422019342,8.26452907450708));
#62900=CARTESIAN_POINT('Ctrl Pts',(54.4721079228182,31.4780143504736,8.39123190487252));
#62901=CARTESIAN_POINT('Ctrl Pts',(52.633994176524,29.9062238185945,8.51793473523798));
#62902=CARTESIAN_POINT('Ctrl Pts',(52.9517811213449,27.508683604596,8.64463756560342));
#62903=CARTESIAN_POINT('Ctrl Pts',(55.1359018055727,26.4700284852613,8.77134039596887));
#62904=CARTESIAN_POINT('Ctrl Pts',(57.1961889837133,27.7366793305203,8.89804322633434));
#62905=CARTESIAN_POINT('Ctrl Pts',(57.2553123013122,30.1544659326576,9.02474605669978));
#62906=CARTESIAN_POINT('Ctrl Pts',(55.2593986867151,31.5203050385728,9.15144888706523));
#62907=CARTESIAN_POINT('Ctrl Pts',(53.0271214070709,30.5896462574052,9.27815171743069));
#62908=CARTESIAN_POINT('Ctrl Pts',(52.5925279199782,28.2105043698432,9.40485454779613));
#62909=CARTESIAN_POINT('Ctrl Pts',(54.3516191100807,26.5507496273943,9.53155737816158));
#62910=CARTESIAN_POINT('Ctrl Pts',(56.7015139215443,27.1227478749746,9.65826020852703));
#62911=CARTESIAN_POINT('Ctrl Pts',(57.5009919914385,29.4052952317528,9.7849630388925));
#62912=CARTESIAN_POINT('Ctrl Pts',(56.0215701916583,31.3185382269086,9.91166586925794));
#62913=CARTESIAN_POINT('Ctrl Pts',(53.6112952805514,31.1191329284173,10.0383686996234));
#62914=CARTESIAN_POINT('Ctrl Pts',(52.4664058704783,28.9887771227173,10.1650715299889));
#62915=CARTESIAN_POINT('Ctrl Pts',(53.6301233457291,26.8686475847,10.2917743603543));
#62916=CARTESIAN_POINT('Ctrl Pts',(56.0420702193846,26.6906029306347,10.4184771907198));
#62917=CARTESIAN_POINT('Ctrl Pts',(57.5044843895061,28.6168771622033,10.5451800210852));
#62918=CARTESIAN_POINT('Ctrl Pts',(56.6848164224656,30.8922523057753,10.6718828514507));
#62919=CARTESIAN_POINT('Ctrl Pts',(54.3299464480911,31.4434101996381,10.7985856818161));
#62920=CARTESIAN_POINT('Ctrl Pts',(52.5856281897347,29.7681366596626,10.9252885121816));
#62921=CARTESIAN_POINT('Ctrl Pts',(53.0412816316454,27.3929382340459,11.051991342547));
#62922=CARTESIAN_POINT('Ctrl Pts',(55.2817160923089,26.4820918981314,11.1786941729125));
#62923=CARTESIAN_POINT('Ctrl Pts',(57.2654513039361,27.8655593644377,11.3053970032779));
#62924=CARTESIAN_POINT('Ctrl Pts',(57.1849109405247,30.2827273085489,11.4320998336434));
#62925=CARTESIAN_POINT('Ctrl Pts',(55.1134832513411,31.5310761975464,11.5588026640088));
#62926=CARTESIAN_POINT('Ctrl Pts',(52.9386498065307,30.4731125367757,11.6855054943743));
#62927=CARTESIAN_POINT('Ctrl Pts',(52.6421153340208,28.0728511079328,11.8122083247397));
#62928=CARTESIAN_POINT('Ctrl Pts',(54.4940815669917,26.5174062544863,11.9389111551052));
#62929=CARTESIAN_POINT('Ctrl Pts',(56.8070398603111,27.2240968186954,12.0656139854706));
#62930=CARTESIAN_POINT('Ctrl Pts',(57.4734263468209,29.5489874980123,12.1923168158361));
#62931=CARTESIAN_POINT('Ctrl Pts',(55.8860307345812,31.3736416543992,12.3190196462015));
#62932=CARTESIAN_POINT('Ctrl Pts',(53.4912853457422,31.0354373628656,12.445722476567));
#62933=CARTESIAN_POINT('Ctrl Pts',(52.4712783170154,28.8425458284923,12.5724253069325));
#62934=CARTESIAN_POINT('Ctrl Pts',(53.755438408185,26.7931262812974,12.6991281372979));
#62935=CARTESIAN_POINT('Ctrl Pts',(56.1736410149237,26.7546065079344,12.8258309676634));
#62936=CARTESIAN_POINT('Ctrl Pts',(57.522423821395,28.7620856637776,12.9525337980288));
#62937=CARTESIAN_POINT('Ctrl Pts',(56.572778109295,30.9863519791427,13.0792366283943));
#62938=CARTESIAN_POINT('Ctrl Pts',(54.1900195201569,31.4006575741647,13.2059394587597));
#62939=CARTESIAN_POINT('Ctrl Pts',(52.5453138381343,29.62748785874,13.3326422891252));
#62940=CARTESIAN_POINT('Ctrl Pts',(53.1373142285489,27.2825522182742,13.4593451194906));
#62941=CARTESIAN_POINT('Ctrl Pts',(55.4265908902734,26.5025522270812,13.5860479498561));
#62942=CARTESIAN_POINT('Ctrl Pts',(57.3271586206714,27.9982226193627,13.7127507802215));
#62943=CARTESIAN_POINT('Ctrl Pts',(57.1072231685262,30.406710945485,13.839453610587));
#62944=CARTESIAN_POINT('Ctrl Pts',(54.9671893631805,31.5334065264448,13.9661564409524));
#62945=CARTESIAN_POINT('Ctrl Pts',(52.8570525571963,30.3516661657017,14.0928592713179));
#62946=CARTESIAN_POINT('Ctrl Pts',(52.6995660055283,27.9382897743733,14.2195621016833));
#62947=CARTESIAN_POINT('Ctrl Pts',(54.6382312001043,26.4923420285965,14.3462649320488));
#62948=CARTESIAN_POINT('Ctrl Pts',(56.9065395417823,27.3313681826892,14.4729677624142));
#62949=CARTESIAN_POINT('Ctrl Pts',(57.4376121273402,29.6908489579968,14.5996705927797));
#62950=CARTESIAN_POINT('Ctrl Pts',(55.747536473188,31.4208292767924,14.7263734231451));
#62951=CARTESIAN_POINT('Ctrl Pts',(53.3763067900918,30.9449538622341,14.8530762535106));
#62952=CARTESIAN_POINT('Ctrl Pts',(52.4845837416101,28.6968396247043,14.979779083876));
#62953=CARTESIAN_POINT('Ctrl Pts',(53.8849039315895,26.7249646322888,15.1064819142415));
#62954=CARTESIAN_POINT('Ctrl Pts',(56.3012978609789,26.8260981983693,15.2331847446069));
#62955=CARTESIAN_POINT('Ctrl Pts',(57.5319512778258,28.9080875806142,15.3598875749724));
#62956=CARTESIAN_POINT('Ctrl Pts',(56.4554947731649,31.0738274111919,15.4865904053378));
#62957=CARTESIAN_POINT('Ctrl Pts',(54.052793778225,31.3498990488002,15.6132932357033));
#62958=CARTESIAN_POINT('Ctrl Pts',(52.513185565168,29.4847464624241,15.7399960660687));
#62959=CARTESIAN_POINT('Ctrl Pts',(53.2395586550675,27.1778936811554,15.8666988964342));
#62960=CARTESIAN_POINT('Ctrl Pts',(55.5700430597053,26.531341239417,15.9934017267996));
#62961=CARTESIAN_POINT('Ctrl Pts',(57.3811051475509,28.1342266795359,16.1201045571651));
#62962=CARTESIAN_POINT('Ctrl Pts',(57.0225080645516,30.5260033731763,16.2468073875305));
#62963=CARTESIAN_POINT('Ctrl Pts',(54.8210048944872,31.5272882539046,16.373510217896));
#62964=CARTESIAN_POINT('Ctrl Pts',(52.7826017759313,30.2257121530027,16.5002130482614));
#62965=CARTESIAN_POINT('Ctrl Pts',(52.764688343526,27.8072691147822,16.6269158786269));
#62966=CARTESIAN_POINT('Ctrl Pts',(54.7835872879929,26.475640535858,16.7536187089924));
#62967=CARTESIAN_POINT('Ctrl Pts',(56.9996811466689,27.444204230055,16.8803215393578));
#62968=CARTESIAN_POINT('Ctrl Pts',(57.3936687690455,29.8304065210588,17.0070243697233));
#62969=CARTESIAN_POINT('Ctrl Pts',(55.6065492689305,31.4599437291291,17.1337272000887));
#62970=CARTESIAN_POINT('Ctrl Pts',(53.2667430530446,30.8479841779496,17.2604300304542));
#62971=CARTESIAN_POINT('Ctrl Pts',(52.506277772296,28.5521444237522,17.3871328608196));
#62972=CARTESIAN_POINT('Ctrl Pts',(54.0180881642297,26.6643899484512,17.5138356911851));
#62973=CARTESIAN_POINT('Ctrl Pts',(56.4246150375551,26.9048395858806,17.6405385215505));
#62974=CARTESIAN_POINT('Ctrl Pts',(57.5330349858947,29.0543960141468,17.767241351916));
#62975=CARTESIAN_POINT('Ctrl Pts',(56.3333575396814,31.1543868820377,17.8939441822814));
#62976=CARTESIAN_POINT('Ctrl Pts',(53.9187268533894,31.291303897029,18.0206470126469));
#62977=CARTESIAN_POINT('Ctrl Pts',(52.4893505147037,29.3403884958433,18.1473498430123));
#62978=CARTESIAN_POINT('Ctrl Pts',(53.3476739385227,27.079311646132,18.2740526733778));
#62979=CARTESIAN_POINT('Ctrl Pts',(55.7115942051347,26.5683629272977,18.4007555037432));
#62980=CARTESIAN_POINT('Ctrl Pts',(57.427110979495,28.2731179880225,18.5274583341087));
#62981=CARTESIAN_POINT('Ctrl Pts',(56.9310481431283,30.6402067659422,18.6541611644741));
#62982=CARTESIAN_POINT('Ctrl Pts',(54.6754173526158,31.5127417836177,18.7808639948396));
#62983=CARTESIAN_POINT('Ctrl Pts',(52.7155457470008,30.0956705399321,18.9075668252051));
#62984=CARTESIAN_POINT('Ctrl Pts',(52.8372651729678,27.6802260670616,19.0342696555705));
#62985=CARTESIAN_POINT('Ctrl Pts',(54.9296650858523,26.46735747371,19.160972485936));
#62986=CARTESIAN_POINT('Ctrl Pts',(57.0861540590909,27.5622286663519,19.2876753163014));
#62987=CARTESIAN_POINT('Ctrl Pts',(57.3417428176716,29.9671947797651,19.4143781466669));
#62988=CARTESIAN_POINT('Ctrl Pts',(55.4635392969205,31.4908545694863,19.5410809770323));
#62989=CARTESIAN_POINT('Ctrl Pts',(53.1629595162855,30.7448516920698,19.6677838073978));
#62990=CARTESIAN_POINT('Ctrl Pts',(52.5362880621304,28.4089427664633,19.7944866377632));
#62991=CARTESIAN_POINT('Ctrl Pts',(54.1545469529491,26.6116042389608,19.9211894681287));
#62992=CARTESIAN_POINT('Ctrl Pts',(56.5431812969302,26.9905680775522,20.0478922984941));
#62993=CARTESIAN_POINT('Ctrl Pts',(57.5256713315587,29.20052304362,20.1745951288596));
#62994=CARTESIAN_POINT('Ctrl Pts',(56.2067737216222,31.2277617356693,20.301297959225));
#62995=CARTESIAN_POINT('Ctrl Pts',(53.7882658424417,31.2250675265509,20.4280007895905));
#62996=CARTESIAN_POINT('Ctrl Pts',(52.4738881737893,29.1948953751452,20.5547036199559));
#62997=CARTESIAN_POINT('Ctrl Pts',(53.4612995275174,26.9871348723422,20.6814064503214));
#62998=CARTESIAN_POINT('Ctrl Pts',(55.8507722710256,26.6134938277417,20.8081092806868));
#62999=CARTESIAN_POINT('Ctrl Pts',(57.4650226921806,28.4144333596062,20.9348121110523));
#63000=CARTESIAN_POINT('Ctrl Pts',(56.8331484128879,30.7489402687474,21.0615149414177));
#63001=CARTESIAN_POINT('Ctrl Pts',(54.5309122523596,31.4898156275883,21.1882177717832));
#63002=CARTESIAN_POINT('Ctrl Pts',(52.6561080977626,29.9619749968406,21.3149206021486));
#63003=CARTESIAN_POINT('Ctrl Pts',(52.9170544517607,27.5575843092621,21.441623432514));
#63004=CARTESIAN_POINT('Ctrl Pts',(55.0759774562272,26.4675204553589,21.5683262628795));
#63005=CARTESIAN_POINT('Ctrl Pts',(57.1656698746875,27.6850479136874,21.695029093245));
#63006=CARTESIAN_POINT('Ctrl Pts',(57.2820074943153,30.1007575243678,21.8217319236104));
#63007=CARTESIAN_POINT('Ctrl Pts',(55.3189833713753,31.5134587876777,21.9484347539759));
#63008=CARTESIAN_POINT('Ctrl Pts',(53.0653024940802,30.6359001944415,22.0751375843413));
#63009=CARTESIAN_POINT('Ctrl Pts',(52.5745141212291,28.2677124958368,22.2018404147068));
#63010=CARTESIAN_POINT('Ctrl Pts',(54.2938260262502,26.5667829832518,22.3285432450722));
#63011=CARTESIAN_POINT('Ctrl Pts',(56.6565996637603,27.0829988658134,22.4552460754377));
#63012=CARTESIAN_POINT('Ctrl Pts',(57.5098879507969,29.345979224245,22.5819489058031));
#63013=CARTESIAN_POINT('Ctrl Pts',(56.076159427009,31.2937114477132,22.7086517361686));
#63014=CARTESIAN_POINT('Ctrl Pts',(53.6618576398276,31.1514026528185,22.835354566534));
#63015=CARTESIAN_POINT('Ctrl Pts',(52.4668269401638,29.0487683207684,22.9620573968995));
#63016=CARTESIAN_POINT('Ctrl Pts',(53.5801018915184,26.9016393690381,23.0887602272649));
#63017=CARTESIAN_POINT('Ctrl Pts',(55.9870241583484,26.6666449433616,23.2154630576304));
#63018=CARTESIAN_POINT('Ctrl Pts',(57.4948881766679,28.5575809854631,23.3421658879959));
#63019=CARTESIAN_POINT('Ctrl Pts',(56.728793679735,30.8520775947651,23.4688687183613));
#63020=CARTESIAN_POINT('Ctrl Pts',(54.388642003446,31.4581217751733,23.5955715487267));
#63021=CARTESIAN_POINT('Ctrl Pts',(52.6031625108171,29.8259965845581,23.7222743790922));
#63022=CARTESIAN_POINT('Ctrl Pts',(53.0065019607934,27.4377758625836,23.8489772094577));
#63023=CARTESIAN_POINT('Ctrl Pts',(54.4791205610484,26.8005426658487,23.9334457630346));
#63024=CARTESIAN_POINT('Ctrl Pts',(55.1880098092608,26.8629068796849,23.9756800398231));
#63025=CARTESIAN_POINT('Ctrl Pts',(56.1576149537041,27.3798829357952,4.9325010326362));
#63026=CARTESIAN_POINT('Ctrl Pts',(56.6952574990887,27.764015991681,4.97475273854616));
#63027=CARTESIAN_POINT('Ctrl Pts',(57.3486124876272,29.1028275288519,5.05923872124462));
#63028=CARTESIAN_POINT('Ctrl Pts',(56.1902455571367,31.029769113045,5.18595898073157));
#63029=CARTESIAN_POINT('Ctrl Pts',(53.9461711444331,31.1015789173689,5.312661811097));
#63030=CARTESIAN_POINT('Ctrl Pts',(52.6630256154931,29.261055652423,5.43936464146247));
#63031=CARTESIAN_POINT('Ctrl Pts',(53.5089785762199,27.181330338801,5.56606747182791));
#63032=CARTESIAN_POINT('Ctrl Pts',(55.7137259387776,26.7594510049981,5.69277030219337));
#63033=CARTESIAN_POINT('Ctrl Pts',(57.268036487705,28.3788108316801,5.81947313255882));
#63034=CARTESIAN_POINT('Ctrl Pts',(56.7557622302409,30.5643735227871,5.94617596292426));
#63035=CARTESIAN_POINT('Ctrl Pts',(54.6436165887307,31.3243916144959,6.07287879328973));
#63036=CARTESIAN_POINT('Ctrl Pts',(52.8562190169,29.9664737283503,6.19958162365515));
#63037=CARTESIAN_POINT('Ctrl Pts',(53.0222250551942,27.7278831086637,6.32628445402062));
#63038=CARTESIAN_POINT('Ctrl Pts',(54.9903795800251,26.6484553063909,6.45298728438607));
#63039=CARTESIAN_POINT('Ctrl Pts',(56.9672986105068,27.7117451348286,6.57969011475152));
#63040=CARTESIAN_POINT('Ctrl Pts',(57.1516191387623,29.948893833168,6.70639294511698));
#63041=CARTESIAN_POINT('Ctrl Pts',(55.3753873591959,31.3214104116291,6.83309577548243));
#63042=CARTESIAN_POINT('Ctrl Pts',(53.2571034366377,30.578662377378,6.95979860584789));
#63043=CARTESIAN_POINT('Ctrl Pts',(52.7269439432466,28.397439316614,7.08650143621333));
#63044=CARTESIAN_POINT('Ctrl Pts',(54.267989518971,26.7652687901219,7.21320426657878));
#63045=CARTESIAN_POINT('Ctrl Pts',(56.4760418362601,27.1693816307097,7.33990709694424));
#63046=CARTESIAN_POINT('Ctrl Pts',(57.3391272269835,29.2415510324764,7.46660992730969));
#63047=CARTESIAN_POINT('Ctrl Pts',(56.070803653006,31.0936194948866,7.59331275767514));
#63048=CARTESIAN_POINT('Ctrl Pts',(53.8267655208816,31.0379852639061,7.72001558804059));
#63049=CARTESIAN_POINT('Ctrl Pts',(52.6517767523307,29.1253421394554,7.84671841840603));
#63050=CARTESIAN_POINT('Ctrl Pts',(53.6164852214576,27.098487463382,7.9734212487715));
#63051=CARTESIAN_POINT('Ctrl Pts',(55.8418501253325,26.8042879425251,8.10012407913695));
#63052=CARTESIAN_POINT('Ctrl Pts',(57.3001225527685,28.5108177087598,8.2268269095024));
#63053=CARTESIAN_POINT('Ctrl Pts',(56.6625270190076,30.6630895894556,8.35352973986785));
#63054=CARTESIAN_POINT('Ctrl Pts',(54.5100395464682,31.2999569182742,8.4802325702333));
#63055=CARTESIAN_POINT('Ctrl Pts',(52.8040032490768,29.8411072117814,8.60693540059876));
#63056=CARTESIAN_POINT('Ctrl Pts',(53.0989556500339,27.6158419702898,8.7336382309642));
#63057=CARTESIAN_POINT('Ctrl Pts',(55.1261365971803,26.6518192934402,8.86034106132966));
#63058=CARTESIAN_POINT('Ctrl Pts',(57.0383820803796,27.8274550899138,8.98704389169509));
#63059=CARTESIAN_POINT('Ctrl Pts',(57.0932570988867,30.0715119176853,9.11374672206057));
#63060=CARTESIAN_POINT('Ctrl Pts',(55.2407596243288,31.3392088139115,9.24044955242599));
#63061=CARTESIAN_POINT('Ctrl Pts',(53.1688823683142,30.4754224109433,9.36715238279147));
#63062=CARTESIAN_POINT('Ctrl Pts',(52.76551654556,28.2672334862874,9.49385521315691));
#63063=CARTESIAN_POINT('Ctrl Pts',(54.3982084433201,26.726740227318,9.62055804352238));
#63064=CARTESIAN_POINT('Ctrl Pts',(56.5792518371202,27.2576376075175,9.74726087388781));
#63065=CARTESIAN_POINT('Ctrl Pts',(57.321283503527,29.3761727901356,9.87396370425327));
#63066=CARTESIAN_POINT('Ctrl Pts',(55.948165384659,31.151939932972,10.0006665346187));
#63067=CARTESIAN_POINT('Ctrl Pts',(53.7110804962346,30.9668628789518,10.1273693649842));
#63068=CARTESIAN_POINT('Ctrl Pts',(52.6484569812201,28.9895835412558,10.2540721953497));
#63069=CARTESIAN_POINT('Ctrl Pts',(53.7285556729845,27.0217956639708,10.3807750257151));
#63070=CARTESIAN_POINT('Ctrl Pts',(55.9671923852834,26.856544387762,10.5074778560806));
#63071=CARTESIAN_POINT('Ctrl Pts',(57.3245249557388,28.6444064090384,10.634180686446));
#63072=CARTESIAN_POINT('Ctrl Pts',(56.5637541348908,30.7562847369938,10.7608835168115));
#63073=CARTESIAN_POINT('Ctrl Pts',(54.3780930679306,31.267839244662,10.8875863471769));
#63074=CARTESIAN_POINT('Ctrl Pts',(52.7591125946285,29.7129422895528,11.0142891775424));
#63075=CARTESIAN_POINT('Ctrl Pts',(53.1820251116031,27.5084134698438,11.1409920079078));
#63076=CARTESIAN_POINT('Ctrl Pts',(55.2614734153462,26.6630158911854,11.2676948382733));
#63077=CARTESIAN_POINT('Ctrl Pts',(57.1026675646594,27.9470744640223,11.3943976686387));
#63078=CARTESIAN_POINT('Ctrl Pts',(57.0279144196693,30.1905570873682,11.5211004990042));
#63079=CARTESIAN_POINT('Ctrl Pts',(55.1053289255489,31.3492060125132,11.6478033293696));
#63080=CARTESIAN_POINT('Ctrl Pts',(53.0867678843146,30.367262207221,11.7745061597351));
#63081=CARTESIAN_POINT('Ctrl Pts',(52.8115408617487,28.1394712834602,11.9012089901005));
#63082=CARTESIAN_POINT('Ctrl Pts',(54.5304342770019,26.6957927385822,12.027911820466));
#63083=CARTESIAN_POINT('Ctrl Pts',(56.677195221862,27.3517041347052,12.1546146508314));
#63084=CARTESIAN_POINT('Ctrl Pts',(57.295698585089,29.5095400653584,12.2813174811969));
#63085=CARTESIAN_POINT('Ctrl Pts',(55.8223650994653,31.2030839101057,12.4080203115623));
#63086=CARTESIAN_POINT('Ctrl Pts',(53.5996938612971,30.8891812485032,12.5347231419278));
#63087=CARTESIAN_POINT('Ctrl Pts',(52.6529793186795,28.8538596796258,12.6614259722933));
#63088=CARTESIAN_POINT('Ctrl Pts',(53.8448662362403,26.9517009350177,12.7881288026587));
#63089=CARTESIAN_POINT('Ctrl Pts',(56.0893091766512,26.9159489954782,12.9148316330242));
#63090=CARTESIAN_POINT('Ctrl Pts',(57.341175351841,28.7791809706643,13.0415344633896));
#63091=CARTESIAN_POINT('Ctrl Pts',(56.4597663216486,30.843622889304,13.1682372937551));
#63092=CARTESIAN_POINT('Ctrl Pts',(54.2482205730866,31.2281586041067,13.2949401241205));
#63093=CARTESIAN_POINT('Ctrl Pts',(52.7216950260614,29.5823997918197,13.421642954486));
#63094=CARTESIAN_POINT('Ctrl Pts',(53.2711572974542,27.4059592283635,13.5483457848514));
#63095=CARTESIAN_POINT('Ctrl Pts',(55.3959382515963,26.6820060455842,13.6750486152169));
#63096=CARTESIAN_POINT('Ctrl Pts',(57.1599409093461,28.0702052162341,13.8017514455823));
#63097=CARTESIAN_POINT('Ctrl Pts',(56.9558088934689,30.3056318945295,13.9284542759478));
#63098=CARTESIAN_POINT('Ctrl Pts',(54.9695469676632,31.3513688959002,14.0551571063132));
#63099=CARTESIAN_POINT('Ctrl Pts',(53.0110337958162,30.254542350979,14.1818599366787));
#63100=CARTESIAN_POINT('Ctrl Pts',(52.8648634219542,28.0145788388328,14.3085627670441));
#63101=CARTESIAN_POINT('Ctrl Pts',(54.6642260550361,26.6725294997212,14.4352655974096));
#63102=CARTESIAN_POINT('Ctrl Pts',(56.7695453653235,27.4512675273478,14.561968427775));
#63103=CARTESIAN_POINT('Ctrl Pts',(57.262457792173,29.641208086678,14.6886712581405));
#63104=CARTESIAN_POINT('Ctrl Pts',(55.693822327075,31.2468808713942,14.8153740885059));
#63105=CARTESIAN_POINT('Ctrl Pts',(53.4929770763557,30.8051994292586,14.9420769188714));
#63106=CARTESIAN_POINT('Ctrl Pts',(52.6653286835415,28.7186231781205,15.0687797492368));
#63107=CARTESIAN_POINT('Ctrl Pts',(53.9650290295572,26.8884370333506,15.1954825796023));
#63108=CARTESIAN_POINT('Ctrl Pts',(56.2077932549187,26.9823036588331,15.3221854099677));
#63109=CARTESIAN_POINT('Ctrl Pts',(57.3500182140011,28.9146919367915,15.4488882403332));
#63110=CARTESIAN_POINT('Ctrl Pts',(56.3509103659602,30.9248127843835,15.5755910706986));
#63111=CARTESIAN_POINT('Ctrl Pts',(54.1208551708396,31.1810473266634,15.7022939010641));
#63112=CARTESIAN_POINT('Ctrl Pts',(52.6918753264028,29.4499150618915,15.8289967314296));
#63113=CARTESIAN_POINT('Ctrl Pts',(53.3660549626277,27.3088209182255,15.955699561795));
#63114=CARTESIAN_POINT('Ctrl Pts',(55.5290826821211,26.7087264267957,16.0824023921605));
#63115=CARTESIAN_POINT('Ctrl Pts',(57.2100111148274,28.1964367205226,16.2091052225259));
#63116=CARTESIAN_POINT('Ctrl Pts',(56.8771809834118,30.4163525787395,16.3358080528913));
#63117=CARTESIAN_POINT('Ctrl Pts',(54.8338665669218,31.3456902511198,16.4625108832568));
#63118=CARTESIAN_POINT('Ctrl Pts',(52.9419326667575,30.1376387491754,16.5892137136222));
#63119=CARTESIAN_POINT('Ctrl Pts',(52.9253064019489,27.8929726534587,16.7159165439877));
#63120=CARTESIAN_POINT('Ctrl Pts',(54.7991375981788,26.6570280907958,16.8426193743531));
#63121=CARTESIAN_POINT('Ctrl Pts',(56.855994291052,27.5559957536877,16.9693222047186));
#63122=CARTESIAN_POINT('Ctrl Pts',(57.2216719787645,29.7707377573194,17.096025035084));
#63123=CARTESIAN_POINT('Ctrl Pts',(55.5629657419395,31.2831847593193,17.2227278654495));
#63124=CARTESIAN_POINT('Ctrl Pts',(53.391286028858,30.7151974903311,17.3494306958149));
#63125=CARTESIAN_POINT('Ctrl Pts',(52.6854638921822,28.5843250339603,17.4761335261804));
#63126=CARTESIAN_POINT('Ctrl Pts',(54.088643324691,26.8322149363567,17.6028363565458));
#63127=CARTESIAN_POINT('Ctrl Pts',(56.3222494901519,27.0553870931267,17.7295391869113));
#63128=CARTESIAN_POINT('Ctrl Pts',(57.3510240523529,29.0504873948933,17.8562420172768));
#63129=CARTESIAN_POINT('Ctrl Pts',(56.2375492891465,30.9995836638454,17.9829448476422));
#63130=CARTESIAN_POINT('Ctrl Pts',(53.996421609255,31.1266625226902,18.1096476780077));
#63131=CARTESIAN_POINT('Ctrl Pts',(52.6697529407101,29.3159299201662,18.2363505083731));
#63132=CARTESIAN_POINT('Ctrl Pts',(53.4664016349973,27.2173224838335,18.3630533387386));
#63133=CARTESIAN_POINT('Ctrl Pts',(55.6604626865017,26.7430879256107,18.489756169104));
#63134=CARTESIAN_POINT('Ctrl Pts',(57.2527112030815,28.3253480102336,18.6164589994695));
#63135=CARTESIAN_POINT('Ctrl Pts',(56.7922929039775,30.522349900035,18.7431618298349));
#63136=CARTESIAN_POINT('Ctrl Pts',(54.698740200895,31.3321890157593,18.8698646602004));
#63137=CARTESIAN_POINT('Ctrl Pts',(52.8796949409666,30.0169412610481,18.9965674905659));
#63138=CARTESIAN_POINT('Ctrl Pts',(52.992668231774,27.7750582691179,19.1232703209312));
#63139=CARTESIAN_POINT('Ctrl Pts',(54.9347189929068,26.6493402071125,19.2499731512967));
#63140=CARTESIAN_POINT('Ctrl Pts',(56.9362537024352,27.6655395578769,19.3766759816622));
#63141=CARTESIAN_POINT('Ctrl Pts',(57.1734771605715,29.8976971116468,19.5033788120276));
#63142=CARTESIAN_POINT('Ctrl Pts',(55.4302317347922,31.3118745048471,19.6300816423931));
#63143=CARTESIAN_POINT('Ctrl Pts',(53.2949598460309,30.6194755771981,19.7567844727585));
#63144=CARTESIAN_POINT('Ctrl Pts',(52.71331779614,28.4514131150576,19.883487303124));
#63145=CARTESIAN_POINT('Ctrl Pts',(54.2152968830592,26.7832221378665,20.0101901334894));
#63146=CARTESIAN_POINT('Ctrl Pts',(56.4322961847852,27.1349555740258,20.1368929638549));
#63147=CARTESIAN_POINT('Ctrl Pts',(57.3441895125406,29.1861144837031,20.2635957942203));
#63148=CARTESIAN_POINT('Ctrl Pts',(56.1200611365734,31.0676861759256,20.3902986245858));
#63149=CARTESIAN_POINT('Ctrl Pts',(53.8753348590363,31.0651855588891,20.5170014549512));
#63150=CARTESIAN_POINT('Ctrl Pts',(52.6554016444992,29.1808911906904,20.6437042853167));
#63151=CARTESIAN_POINT('Ctrl Pts',(53.5718626705443,27.1317690613758,20.7704071156822));
#63152=CARTESIAN_POINT('Ctrl Pts',(55.7896401286971,26.7849759504659,20.8971099460476));
#63153=CARTESIAN_POINT('Ctrl Pts',(57.2878987740729,28.4565091822705,21.0238127764131));
#63154=CARTESIAN_POINT('Ctrl Pts',(56.7014277474381,30.6232703696753,21.1505156067785));
#63155=CARTESIAN_POINT('Ctrl Pts',(54.5646184977673,31.310910215998,21.277218437144));
#63156=CARTESIAN_POINT('Ctrl Pts',(52.8245281770835,29.8928523956156,21.4039212675094));
#63157=CARTESIAN_POINT('Ctrl Pts',(53.0667242612434,27.6612289205243,21.5306240978748));
#63158=CARTESIAN_POINT('Ctrl Pts',(55.0705181049695,26.6494914777341,21.6573269282403));
#63159=CARTESIAN_POINT('Ctrl Pts',(57.0100559183742,27.7795336425169,21.7840297586058));
#63160=CARTESIAN_POINT('Ctrl Pts',(57.1180341119095,30.0216627208105,21.9107325889712));
#63161=CARTESIAN_POINT('Ctrl Pts',(55.2960628584209,31.3328544995762,22.0374354193367));
#63162=CARTESIAN_POINT('Ctrl Pts',(53.2043199577687,30.5183527767275,22.1641382497021));
#63163=CARTESIAN_POINT('Ctrl Pts',(52.7487971262193,28.3203309290585,22.2908410800676));
#63164=CARTESIAN_POINT('Ctrl Pts',(54.3445680747892,26.7416215082599,22.417543910433));
#63165=CARTESIAN_POINT('Ctrl Pts',(56.5375648880919,27.2207447587746,22.5442467407985));
#63166=CARTESIAN_POINT('Ctrl Pts',(57.3295402447631,29.3211189274305,22.6709495711639));
#63167=CARTESIAN_POINT('Ctrl Pts',(55.998832116869,31.1288970791007,22.7976524015294));
#63168=CARTESIAN_POINT('Ctrl Pts',(53.7580097030809,30.996813866069,22.9243552318949));
#63169=CARTESIAN_POINT('Ctrl Pts',(52.6488477949925,29.0452640787664,23.0510580622602));
#63170=CARTESIAN_POINT('Ctrl Pts',(53.6821285045334,27.0524168274922,23.1777608926258));
#63171=CARTESIAN_POINT('Ctrl Pts',(55.9161016525442,26.8343078988708,23.3044637229911));
#63172=CARTESIAN_POINT('Ctrl Pts',(57.315618277655,28.5893709521635,23.4311665533567));
#63173=CARTESIAN_POINT('Ctrl Pts',(56.6045714114671,30.7189967751585,23.5578693837221));
#63174=CARTESIAN_POINT('Ctrl Pts',(54.4325710609997,31.2814937216525,23.6845722140876));
#63175=CARTESIAN_POINT('Ctrl Pts',(52.7753869891141,29.7666446962917,23.811275044453));
#63176=CARTESIAN_POINT('Ctrl Pts',(53.1497445299447,27.5500292958113,23.9379778748185));
#63177=CARTESIAN_POINT('Ctrl Pts',(54.516548292396,26.9585844161219,24.0224464283954));
#63178=CARTESIAN_POINT('Ctrl Pts',(55.1745003863396,27.016467456645,24.0646807051839));
#63179=CARTESIAN_POINT('Ctrl Pts',(56.1167974000718,31.181218424916,4.9305));
#63180=CARTESIAN_POINT('Ctrl Pts',(56.1036115526316,31.1892689822654,4.9305));
#63181=CARTESIAN_POINT('Ctrl Pts',(56.0904257051915,31.1973195396149,4.9305));
#63182=CARTESIAN_POINT('Ctrl Pts',(56.0772398577513,31.2053700969644,4.9305));
#63183=CARTESIAN_POINT('Origin',(55.,29.,4.6));
#63184=CARTESIAN_POINT('',(53.6096550852048,28.9081480324703,4.7));
#63185=CARTESIAN_POINT('',(53.5566243270259,29.,4.65));
#63186=CARTESIAN_POINT('Ctrl Pts',(53.6096550852048,28.9081480324703,4.7));
#63187=CARTESIAN_POINT('Ctrl Pts',(53.5836070607731,28.9532645342227,4.67698273374721));
#63188=CARTESIAN_POINT('Ctrl Pts',(53.5566243270259,29.,4.65));
#63189=CARTESIAN_POINT('',(54.2252814053341,27.8418519675297,4.7));
#63190=CARTESIAN_POINT('Origin',(55.,29.,4.7));
#63191=CARTESIAN_POINT('',(54.278312163513,27.75,4.64999999999999));
#63192=CARTESIAN_POINT('Ctrl Pts',(54.278312163513,27.75,4.64999999999999));
#63193=CARTESIAN_POINT('Ctrl Pts',(54.2513294297658,27.7967354657773,4.6769827337472));
#63194=CARTESIAN_POINT('Ctrl Pts',(54.2252814053341,27.8418519675297,4.7));
#63195=CARTESIAN_POINT('',(54.3843736798707,27.75,4.7));
#63196=CARTESIAN_POINT('Ctrl Pts',(54.3843736798707,27.75,4.7));
#63197=CARTESIAN_POINT('Ctrl Pts',(54.3322776310074,27.75,4.6769827337472));
#63198=CARTESIAN_POINT('Ctrl Pts',(54.278312163513,27.75,4.64999999999999));
#63199=CARTESIAN_POINT('',(55.6156263201293,27.75,4.7));
#63200=CARTESIAN_POINT('Origin',(55.,29.,4.7));
#63201=CARTESIAN_POINT('',(55.721687836487,27.75,4.64999999999999));
#63202=CARTESIAN_POINT('Ctrl Pts',(55.721687836487,27.75,4.64999999999999));
#63203=CARTESIAN_POINT('Ctrl Pts',(55.6677223689926,27.75,4.6769827337472));
#63204=CARTESIAN_POINT('Ctrl Pts',(55.6156263201293,27.75,4.7));
#63205=CARTESIAN_POINT('',(55.7747185946659,27.8418519675297,4.7));
#63206=CARTESIAN_POINT('Ctrl Pts',(55.7747185946659,27.8418519675297,4.7));
#63207=CARTESIAN_POINT('Ctrl Pts',(55.7486705702342,27.7967354657773,4.6769827337472));
#63208=CARTESIAN_POINT('Ctrl Pts',(55.721687836487,27.75,4.64999999999999));
#63209=CARTESIAN_POINT('',(56.3903449147952,28.9081480324703,4.7));
#63210=CARTESIAN_POINT('Origin',(55.,29.,4.7));
#63211=CARTESIAN_POINT('',(56.4433756729741,29.,4.65));
#63212=CARTESIAN_POINT('Ctrl Pts',(56.4433756729741,29.,4.65));
#63213=CARTESIAN_POINT('Ctrl Pts',(56.4163929392269,28.9532645342227,4.67698273374721));
#63214=CARTESIAN_POINT('Ctrl Pts',(56.3903449147952,28.9081480324703,4.7));
#63215=CARTESIAN_POINT('',(56.3903449147952,29.0918519675297,4.7));
#63216=CARTESIAN_POINT('Ctrl Pts',(56.3903449147952,29.0918519675297,4.7));
#63217=CARTESIAN_POINT('Ctrl Pts',(56.4163929392268,29.0467354657773,4.67698273374722));
#63218=CARTESIAN_POINT('Ctrl Pts',(56.4433756729741,29.,4.65));
#63219=CARTESIAN_POINT('',(55.7747185946659,30.1581480324703,4.7));
#63220=CARTESIAN_POINT('Origin',(55.,29.,4.7));
#63221=CARTESIAN_POINT('',(55.721687836487,30.25,4.65000000000001));
#63222=CARTESIAN_POINT('Ctrl Pts',(55.721687836487,30.25,4.65000000000001));
#63223=CARTESIAN_POINT('Ctrl Pts',(55.7486705702342,30.2032645342227,4.67698273374721));
#63224=CARTESIAN_POINT('Ctrl Pts',(55.7747185946659,30.1581480324703,4.7));
#63225=CARTESIAN_POINT('',(55.6156263201293,30.25,4.7));
#63226=CARTESIAN_POINT('Ctrl Pts',(55.6156263201293,30.25,4.7));
#63227=CARTESIAN_POINT('Ctrl Pts',(55.6677223689926,30.25,4.67698273374721));
#63228=CARTESIAN_POINT('Ctrl Pts',(55.721687836487,30.25,4.65000000000001));
#63229=CARTESIAN_POINT('',(54.3843736798707,30.25,4.7));
#63230=CARTESIAN_POINT('Origin',(55.,29.,4.7));
#63231=CARTESIAN_POINT('',(54.278312163513,30.25,4.65000000000001));
#63232=CARTESIAN_POINT('Ctrl Pts',(54.278312163513,30.25,4.65000000000001));
#63233=CARTESIAN_POINT('Ctrl Pts',(54.3322776310074,30.25,4.67698273374721));
#63234=CARTESIAN_POINT('Ctrl Pts',(54.3843736798707,30.25,4.7));
#63235=CARTESIAN_POINT('',(54.2252814053341,30.1581480324703,4.7));
#63236=CARTESIAN_POINT('Ctrl Pts',(54.2252814053341,30.1581480324703,4.7));
#63237=CARTESIAN_POINT('Ctrl Pts',(54.2513294297658,30.2032645342228,4.67698273374719));
#63238=CARTESIAN_POINT('Ctrl Pts',(54.278312163513,30.25,4.65000000000001));
#63239=CARTESIAN_POINT('',(53.6096550852048,29.0918519675297,4.7));
#63240=CARTESIAN_POINT('Origin',(55.,29.,4.7));
#63241=CARTESIAN_POINT('Ctrl Pts',(53.5566243270259,29.,4.65));
#63242=CARTESIAN_POINT('Ctrl Pts',(53.5836070607731,29.0467354657773,4.67698273374721));
#63243=CARTESIAN_POINT('Ctrl Pts',(53.6096550852048,29.0918519675297,4.7));
#63244=CARTESIAN_POINT('',(53.4066243270259,29.,4.5));
#63245=CARTESIAN_POINT('',(53.5066243270259,29.,4.6));
#63246=CARTESIAN_POINT('Origin',(55.,29.,4.5));
#63247=CARTESIAN_POINT('Origin',(55.,29.,4.6));
#63248=CARTESIAN_POINT('',(56.3903449147952,28.9081480324703,4.5));
#63249=CARTESIAN_POINT('',(56.3903449147952,28.9081480324703,4.6));
#63250=CARTESIAN_POINT('',(55.7747185946659,27.8418519675297,4.5));
#63251=CARTESIAN_POINT('',(55.7747185946659,27.8418519675297,4.6));
#63252=CARTESIAN_POINT('Origin',(55.,29.,4.5));
#63253=CARTESIAN_POINT('Origin',(55.,29.,4.6));
#63254=CARTESIAN_POINT('',(55.7747185946659,30.1581480324703,4.5));
#63255=CARTESIAN_POINT('',(55.7747185946659,30.1581480324703,4.6));
#63256=CARTESIAN_POINT('',(56.3903449147952,29.0918519675297,4.5));
#63257=CARTESIAN_POINT('',(56.3903449147952,29.0918519675297,4.6));
#63258=CARTESIAN_POINT('Origin',(55.,29.,4.5));
#63259=CARTESIAN_POINT('Origin',(55.,29.,4.6));
#63260=CARTESIAN_POINT('',(54.3843736798707,27.75,4.5));
#63261=CARTESIAN_POINT('',(54.3843736798707,27.75,4.6));
#63262=CARTESIAN_POINT('',(55.6156263201293,27.75,4.5));
#63263=CARTESIAN_POINT('Origin',(55.,29.,4.5));
#63264=CARTESIAN_POINT('',(55.6156263201293,27.75,4.6));
#63265=CARTESIAN_POINT('Origin',(55.,29.,4.6));
#63266=CARTESIAN_POINT('',(54.3843736798707,30.25,4.5));
#63267=CARTESIAN_POINT('',(54.3843736798707,30.25,4.6));
#63268=CARTESIAN_POINT('',(55.6156263201293,30.25,4.5));
#63269=CARTESIAN_POINT('',(55.6156263201293,30.25,4.6));
#63270=CARTESIAN_POINT('Origin',(55.,29.,4.5));
#63271=CARTESIAN_POINT('Origin',(55.,29.,4.6));
#63272=CARTESIAN_POINT('',(53.6096550852048,28.9081480324703,4.5));
#63273=CARTESIAN_POINT('',(53.6096550852048,28.9081480324703,4.6));
#63274=CARTESIAN_POINT('',(54.2252814053341,27.8418519675297,4.5));
#63275=CARTESIAN_POINT('Origin',(55.,29.,4.5));
#63276=CARTESIAN_POINT('',(54.2252814053341,27.8418519675297,4.6));
#63277=CARTESIAN_POINT('Origin',(55.,29.,4.6));
#63278=CARTESIAN_POINT('',(54.2252814053341,30.1581480324703,4.5));
#63279=CARTESIAN_POINT('',(54.2252814053341,30.1581480324703,4.6));
#63280=CARTESIAN_POINT('',(53.6096550852048,29.0918519675297,4.5));
#63281=CARTESIAN_POINT('Origin',(55.,29.,4.5));
#63282=CARTESIAN_POINT('',(53.6096550852048,29.0918519675297,4.6));
#63283=CARTESIAN_POINT('Origin',(55.721687836487,30.25,4.5));
#63284=CARTESIAN_POINT('',(56.3708439182435,30.25,4.5));
#63285=CARTESIAN_POINT('',(55.721687836487,30.25,7.));
#63286=CARTESIAN_POINT('',(55.721687836487,30.25,4.5));
#63287=CARTESIAN_POINT('',(54.278312163513,30.25,7.));
#63288=CARTESIAN_POINT('',(55.721687836487,30.25,7.));
#63289=CARTESIAN_POINT('',(54.278312163513,30.25,4.5));
#63290=CARTESIAN_POINT('Origin',(56.4433756729741,29.,4.5));
#63291=CARTESIAN_POINT('',(56.5154537138523,28.8751571710889,4.5));
#63292=CARTESIAN_POINT('',(56.4433756729741,29.,7.));
#63293=CARTESIAN_POINT('',(56.4433756729741,29.,4.5));
#63294=CARTESIAN_POINT('',(56.4433756729741,29.,7.));
#63295=CARTESIAN_POINT('Origin',(55.721687836487,27.75,4.5));
#63296=CARTESIAN_POINT('',(56.1546097956088,28.4998428289111,4.5));
#63297=CARTESIAN_POINT('',(55.721687836487,27.75,7.));
#63298=CARTESIAN_POINT('',(55.721687836487,27.75,4.5));
#63299=CARTESIAN_POINT('',(55.721687836487,27.75,7.));
#63300=CARTESIAN_POINT('Origin',(57.02,29.,4.5));
#63301=CARTESIAN_POINT('Origin',(57.02,29.,4.5));
#63302=CARTESIAN_POINT('Origin',(57.02,29.,4.5));
#63303=CARTESIAN_POINT('',(55.6491560817565,27.75,4.5));
#63304=CARTESIAN_POINT('Origin',(57.02,29.,4.5));
#63305=CARTESIAN_POINT('Origin',(57.02,29.,4.5));
#63306=CARTESIAN_POINT('',(53.9895462861477,28.2501571710889,4.5));
#63307=CARTESIAN_POINT('Origin',(57.02,29.,4.5));
#63308=CARTESIAN_POINT('',(54.3503902043912,30.3748428289111,4.5));
#63309=CARTESIAN_POINT('Origin',(56.4433756729741,29.,7.));
#63310=CARTESIAN_POINT('',(54.278312163513,27.75,7.));
#63311=CARTESIAN_POINT('',(54.278312163513,27.75,7.));
#63312=CARTESIAN_POINT('Origin',(55.,29.,7.));
#63313=CARTESIAN_POINT('Origin',(56.4433756729741,29.,7.));
#63314=CARTESIAN_POINT('Origin',(55.,29.,7.));
#63315=CARTESIAN_POINT('Origin',(56.4433756729741,29.,7.));
#63316=CARTESIAN_POINT('Origin',(55.,29.,7.));
#63317=CARTESIAN_POINT('Origin',(56.4433756729741,29.,7.));
#63318=CARTESIAN_POINT('Origin',(55.,29.,7.));
#63319=CARTESIAN_POINT('Origin',(56.4433756729741,29.,7.));
#63320=CARTESIAN_POINT('',(53.5566243270259,29.,7.));
#63321=CARTESIAN_POINT('',(54.278312163513,30.25,7.));
#63322=CARTESIAN_POINT('Origin',(55.,29.,7.));
#63323=CARTESIAN_POINT('Origin',(56.4433756729741,29.,7.));
#63324=CARTESIAN_POINT('',(53.5566243270259,29.,7.));
#63325=CARTESIAN_POINT('Origin',(55.,29.,7.));
#63326=CARTESIAN_POINT('Origin',(55.,29.,7.));
#63327=CARTESIAN_POINT('',(55.,29.,7.86726760035252));
#63328=CARTESIAN_POINT('',(53.5566243270259,29.,7.));
#63329=CARTESIAN_POINT('Origin',(54.278312163513,27.75,4.5));
#63330=CARTESIAN_POINT('',(54.278312163513,27.75,4.5));
#63331=CARTESIAN_POINT('Origin',(53.5566243270259,29.,4.5));
#63332=CARTESIAN_POINT('',(53.5566243270259,29.,4.5));
#63333=CARTESIAN_POINT('Origin',(54.278312163513,30.25,4.5));
#63334=CARTESIAN_POINT('Origin',(57.02,29.,4.5));
#63335=CARTESIAN_POINT('',(52.98,29.,4.5));
#63336=CARTESIAN_POINT('Origin',(55.,29.,4.5));
#63337=CARTESIAN_POINT('Origin',(55.,29.,4.74));
#63338=CARTESIAN_POINT('',(52.74,29.,4.74));
#63339=CARTESIAN_POINT('Origin',(55.,29.,24.125));
#63340=CARTESIAN_POINT('',(53.25,29.,24.5));
#63341=CARTESIAN_POINT('',(52.875,29.,24.125));
#63342=CARTESIAN_POINT('Origin',(55.,29.,24.5));
#63343=CARTESIAN_POINT('Origin',(55.,29.,24.5));
#63344=CARTESIAN_POINT('',(0.,0.,0.));
#63345=CARTESIAN_POINT('Origin',(30.,21.,34.5704548813952));
#63346=CARTESIAN_POINT('',(29.0285070491141,22.7421908646526,36.5933647280801));
#63347=CARTESIAN_POINT('',(29.0285070491141,22.7421908646526,36.5));
#63348=CARTESIAN_POINT('',(29.0285070491141,22.7421908646526,34.5704548813952));
#63349=CARTESIAN_POINT('',(30.4423314238756,22.9450888087571,36.5));
#63350=CARTESIAN_POINT('Ctrl Pts',(30.4423314238756,22.9450888087571,36.5));
#63351=CARTESIAN_POINT('Ctrl Pts',(30.3662355841702,22.9623937158526,36.5049600370302));
#63352=CARTESIAN_POINT('Ctrl Pts',(30.2892837013555,22.975192508028,36.5099200740605));
#63353=CARTESIAN_POINT('Ctrl Pts',(30.2119875644214,22.9834537642785,36.5148801110907));
#63354=CARTESIAN_POINT('Ctrl Pts',(30.1343618519812,22.9917502448989,36.5198612967421));
#63355=CARTESIAN_POINT('Ctrl Pts',(30.0563892228182,22.9954704906302,36.5248424823934));
#63356=CARTESIAN_POINT('Ctrl Pts',(29.9785820065602,22.9946350122408,36.5298236680448));
#63357=CARTESIAN_POINT('Ctrl Pts',(29.9003694249949,22.9937951811196,36.5348308050147));
#63358=CARTESIAN_POINT('Ctrl Pts',(29.8223242552552,22.9883521111826,36.5398379419846));
#63359=CARTESIAN_POINT('Ctrl Pts',(29.7449566415887,22.9783782367966,36.5448450789545));
#63360=CARTESIAN_POINT('Ctrl Pts',(29.7246537813463,22.9757608860973,36.5461590551429));
#63361=CARTESIAN_POINT('Ctrl Pts',(29.7043975141738,22.9728317941917,36.5474730313313));
#63362=CARTESIAN_POINT('Ctrl Pts',(29.6841969077652,22.9695928435682,36.5487870075198));
#63363=CARTESIAN_POINT('Ctrl Pts',(29.6157197224541,22.9586132611944,36.5532412000885));
#63364=CARTESIAN_POINT('Ctrl Pts',(29.5476810636523,22.9440366831893,36.5576953926573));
#63365=CARTESIAN_POINT('Ctrl Pts',(29.4804876480764,22.9259113371853,36.5621495852261));
#63366=CARTESIAN_POINT('Ctrl Pts',(29.4133823824009,22.9078097695147,36.5665979344153));
#63367=CARTESIAN_POINT('Ctrl Pts',(29.3471206295807,22.8861687907933,36.5710462836045));
#63368=CARTESIAN_POINT('Ctrl Pts',(29.2821008695718,22.8610879616586,36.5754946327937));
#63369=CARTESIAN_POINT('Ctrl Pts',(29.2171555459823,22.8360358457507,36.5799378893897));
#63370=CARTESIAN_POINT('Ctrl Pts',(29.1534498458602,22.8075518748946,36.5843811459858));
#63371=CARTESIAN_POINT('Ctrl Pts',(29.091367063864,22.7757853895865,36.5888244025818));
#63372=CARTESIAN_POINT('Ctrl Pts',(29.0702207093069,22.7649652339852,36.5903378444146));
#63373=CARTESIAN_POINT('Ctrl Pts',(29.0492624937621,22.7537646643879,36.5918512862474));
#63374=CARTESIAN_POINT('Ctrl Pts',(29.0285070491141,22.7421908646526,36.5933647280801));
#63375=CARTESIAN_POINT('Origin',(30.,21.,36.5));
#63376=CARTESIAN_POINT('Origin',(30.,21.,34.5704548813952));
#63377=CARTESIAN_POINT('',(29.0285070711969,22.7421908769666,37.3944594262182));
#63378=CARTESIAN_POINT('',(29.0285070491141,22.7421908646526,37.2352940441794));
#63379=CARTESIAN_POINT('',(29.0285070491141,22.7421908646526,34.5704548813952));
#63380=CARTESIAN_POINT('',(28.0052502061177,21.0009068111524,36.728545118564));
#63381=CARTESIAN_POINT('Ctrl Pts',(29.0285070711969,22.7421908769666,37.3944594262182));
#63382=CARTESIAN_POINT('Ctrl Pts',(29.0505519466918,22.7544836980017,37.3929589895291));
#63383=CARTESIAN_POINT('Ctrl Pts',(29.0728387999716,22.766362930873,37.3914477881055));
#63384=CARTESIAN_POINT('Ctrl Pts',(29.1324581808279,22.7967002305002,37.3874118803961));
#63385=CARTESIAN_POINT('Ctrl Pts',(29.1701396501316,22.8144122904256,37.3848676333455));
#63386=CARTESIAN_POINT('Ctrl Pts',(29.2275108683841,22.8392183322913,37.3809871994448));
#63387=CARTESIAN_POINT('Ctrl Pts',(29.246804328479,22.8472032266414,37.3796811885625));
#63388=CARTESIAN_POINT('Ctrl Pts',(29.2821472466523,22.861184676385,37.3772850067571));
#63389=CARTESIAN_POINT('Ctrl Pts',(29.2981555580911,22.8672801944376,37.3761982996956));
#63390=CARTESIAN_POINT('Ctrl Pts',(29.333266665734,22.8801342392277,37.373810887938));
#63391=CARTESIAN_POINT('Ctrl Pts',(29.3523977597723,22.8868093132904,37.3725075377884));
#63392=CARTESIAN_POINT('Ctrl Pts',(29.407980165528,22.9052577907491,37.3687121581381));
#63393=CARTESIAN_POINT('Ctrl Pts',(29.4446714541357,22.9162736252472,37.3661958590089));
#63394=CARTESIAN_POINT('Ctrl Pts',(29.635229488006,22.9675525454124,37.3530655267716));
#63395=CARTESIAN_POINT('Ctrl Pts',(29.793176987161,22.9903591309445,37.3419125284843));
#63396=CARTESIAN_POINT('Ctrl Pts',(30.029961120004,22.9960442174414,37.3254471308986));
#63397=CARTESIAN_POINT('Ctrl Pts',(30.1078522927262,22.9933540726519,37.3200846017565));
#63398=CARTESIAN_POINT('Ctrl Pts',(30.2028333987317,22.9844880897592,37.3137505736092));
#63399=CARTESIAN_POINT('Ctrl Pts',(30.2202519211021,22.9826304516262,37.3125976114903));
#63400=CARTESIAN_POINT('Ctrl Pts',(30.2480971807814,22.9792893130701,37.3107706968631));
#63401=CARTESIAN_POINT('Ctrl Pts',(30.2585401479286,22.9779523250387,37.3100892024933));
#63402=CARTESIAN_POINT('Ctrl Pts',(30.2790498946707,22.9751612989511,37.3087586224246));
#63403=CARTESIAN_POINT('Ctrl Pts',(30.2891169863597,22.97371284027,37.3081092880351));
#63404=CARTESIAN_POINT('Ctrl Pts',(30.3148167709357,22.9698142883536,37.3064602947617));
#63405=CARTESIAN_POINT('Ctrl Pts',(30.3304325917298,22.9672550087523,37.3054665301816));
#63406=CARTESIAN_POINT('Ctrl Pts',(30.3996070685703,22.9550710363641,37.3010942466117));
#63407=CARTESIAN_POINT('Ctrl Pts',(30.452793525566,22.9434422161982,37.2978119933293));
#63408=CARTESIAN_POINT('Ctrl Pts',(30.6311337769079,22.8967287651445,37.2868768608316));
#63409=CARTESIAN_POINT('Ctrl Pts',(30.7533113326398,22.8516032905373,37.2794866753651));
#63410=CARTESIAN_POINT('Ctrl Pts',(30.9406893224414,22.7607559590314,37.2672543835919));
#63411=CARTESIAN_POINT('Ctrl Pts',(31.0090633444993,22.7224828646665,37.2625825347371));
#63412=CARTESIAN_POINT('Ctrl Pts',(31.0971119316904,22.6661517324684,37.2561570018365));
#63413=CARTESIAN_POINT('Ctrl Pts',(31.1189347184272,22.6515753637005,37.2545291011719));
#63414=CARTESIAN_POINT('Ctrl Pts',(31.1536583496348,22.6273778453901,37.2518774502933));
#63415=CARTESIAN_POINT('Ctrl Pts',(31.1667418288865,22.6180233989853,37.2508638535942));
#63416=CARTESIAN_POINT('Ctrl Pts',(31.1939282878908,22.5980843805586,37.2487262022977));
#63417=CARTESIAN_POINT('Ctrl Pts',(31.2080068435841,22.5874690160563,37.2476010075383));
#63418=CARTESIAN_POINT('Ctrl Pts',(31.2416639771832,22.5613842202759,37.2448656346279));
#63419=CARTESIAN_POINT('Ctrl Pts',(31.2610961916772,22.5457316769473,37.2432482838986));
#63420=CARTESIAN_POINT('Ctrl Pts',(31.3340048303601,22.4847141091252,37.2370301152855));
#63421=CARTESIAN_POINT('Ctrl Pts',(31.3853642558693,22.4369094783557,37.2323317138618));
#63422=CARTESIAN_POINT('Ctrl Pts',(31.5317835643389,22.2854643951884,37.2179546765141));
#63423=CARTESIAN_POINT('Ctrl Pts',(31.6185167005224,22.1743842133166,37.2080245036292));
#63424=CARTESIAN_POINT('Ctrl Pts',(31.7214981722948,22.0091607820043,37.1946117744597));
#63425=CARTESIAN_POINT('Ctrl Pts',(31.7482674785112,21.9620412104783,37.1909272696723));
#63426=CARTESIAN_POINT('Ctrl Pts',(31.7805148931126,21.8994760183349,37.1862656040438));
#63427=CARTESIAN_POINT('Ctrl Pts',(31.7877667007291,21.8849749468603,37.1852007429291));
#63428=CARTESIAN_POINT('Ctrl Pts',(31.7988719160402,21.8620746638501,37.1835452895328));
#63429=CARTESIAN_POINT('Ctrl Pts',(31.8028449648706,21.8537346996225,37.1829477806362));
#63430=CARTESIAN_POINT('Ctrl Pts',(31.8110648534309,21.8361667534254,37.1817008774943));
#63431=CARTESIAN_POINT('Ctrl Pts',(31.8152994023827,21.8269333886907,37.1810523074144));
#63432=CARTESIAN_POINT('Ctrl Pts',(31.8259253998944,21.8032885663352,37.1794076986467));
#63433=CARTESIAN_POINT('Ctrl Pts',(31.8322170402126,21.788832581248,37.1784174934755));
#63434=CARTESIAN_POINT('Ctrl Pts',(31.8592010672664,21.7247675677668,37.1740896785286));
#63435=CARTESIAN_POINT('Ctrl Pts',(31.8780564899883,21.6744045382354,37.1708459485977));
#63436=CARTESIAN_POINT('Ctrl Pts',(31.9342600914459,21.5035536178957,37.1601724553701));
#63437=CARTESIAN_POINT('Ctrl Pts',(31.9622189134631,21.3802999894884,37.1529920685108));
#63438=CARTESIAN_POINT('Ctrl Pts',(31.9887832957447,21.174390176544,37.1408187830289));
#63439=CARTESIAN_POINT('Ctrl Pts',(31.9942467866017,21.0929979291003,37.1359662941121));
#63440=CARTESIAN_POINT('Ctrl Pts',(31.9948719384502,20.98461136241,37.1293100692708));
#63441=CARTESIAN_POINT('Ctrl Pts',(31.994483143454,20.9577182779882,37.1276430535329));
#63442=CARTESIAN_POINT('Ctrl Pts',(31.9929893253837,20.9146572834782,37.1249451018273));
#63443=CARTESIAN_POINT('Ctrl Pts',(31.9922307922341,20.8984801697109,37.1239250418011));
#63444=CARTESIAN_POINT('Ctrl Pts',(31.990240848714,20.8648097157594,37.1217875138603));
#63445=CARTESIAN_POINT('Ctrl Pts',(31.9889755627939,20.8473198536811,37.1206690704946));
#63446=CARTESIAN_POINT('Ctrl Pts',(31.9853988037762,20.8055407685583,37.1179769552282));
#63447=CARTESIAN_POINT('Ctrl Pts',(31.9828719958702,20.781273314384,37.116396664224));
#63448=CARTESIAN_POINT('Ctrl Pts',(31.97195288093,20.692285535213,37.1105382221356));
#63449=CARTESIAN_POINT('Ctrl Pts',(31.9608319140613,20.6279475723352,37.1061767578868));
#63450=CARTESIAN_POINT('Ctrl Pts',(31.9205636100355,20.4480506722101,37.0936333132178));
#63451=CARTESIAN_POINT('Ctrl Pts',(31.8841920908289,20.3343961034967,37.0852793466902));
#63452=CARTESIAN_POINT('Ctrl Pts',(31.8071560880185,20.1517821235621,37.0714968516894));
#63453=CARTESIAN_POINT('Ctrl Pts',(31.7720930043362,20.0807744846037,37.0660448691127));
#63454=CARTESIAN_POINT('Ctrl Pts',(31.7242059054002,19.9967803011711,37.0596245336309));
#63455=CARTESIAN_POINT('Ctrl Pts',(31.715309472373,19.981643857447,37.0584688617362));
#63456=CARTESIAN_POINT('Ctrl Pts',(31.7007560212544,19.9576145053395,37.0566387384929));
#63457=CARTESIAN_POINT('Ctrl Pts',(31.695226577374,19.9486459079006,37.0559566996931));
#63458=CARTESIAN_POINT('Ctrl Pts',(31.6842242702422,19.9311129836435,37.0546260433189));
#63459=CARTESIAN_POINT('Ctrl Pts',(31.6787565686178,19.9225459469477,37.0539771650629));
#63460=CARTESIAN_POINT('Ctrl Pts',(31.6646282428951,19.900777712684,37.0523307958152));
#63461=CARTESIAN_POINT('Ctrl Pts',(31.6558757092233,19.8876365267462,37.0513391626404));
#63462=CARTESIAN_POINT('Ctrl Pts',(31.6164950702593,19.8300048831308,37.0469937855974));
#63463=CARTESIAN_POINT('Ctrl Pts',(31.5842208842064,19.786661583213,37.0437348576022));
#63464=CARTESIAN_POINT('Ctrl Pts',(31.46993776086,19.645530844033,37.0329600549671));
#63465=CARTESIAN_POINT('Ctrl Pts',(31.3803225844935,19.5543112020049,37.025698680878));
#63466=CARTESIAN_POINT('Ctrl Pts',(31.2213033017395,19.4208063667873,37.013516124595));
#63467=CARTESIAN_POINT('Ctrl Pts',(31.1569650209088,19.3730813660352,37.0087469674915));
#63468=CARTESIAN_POINT('Ctrl Pts',(31.0675314425625,19.3147344556502,37.002187845244));
#63469=CARTESIAN_POINT('Ctrl Pts',(31.0448334806621,19.3005688517418,37.0005292251542));
#63470=CARTESIAN_POINT('Ctrl Pts',(31.0079697451104,19.2785802147049,36.997841158744));
#63471=CARTESIAN_POINT('Ctrl Pts',(30.9939813000039,19.2704653126584,36.996822430059));
#63472=CARTESIAN_POINT('Ctrl Pts',(30.9646036750718,19.2538970384935,36.9946847698269));
#63473=CARTESIAN_POINT('Ctrl Pts',(30.9491985141791,19.2454750072078,36.993564827598));
#63474=CARTESIAN_POINT('Ctrl Pts',(30.9120204002801,19.2257826048474,36.9908634274208));
#63475=CARTESIAN_POINT('Ctrl Pts',(30.8901473580621,19.2147083801958,36.9892752349388));
#63476=CARTESIAN_POINT('Ctrl Pts',(30.8084305949921,19.1752106044216,36.983343311587));
#63477=CARTESIAN_POINT('Ctrl Pts',(30.7473916484745,19.1493729524247,36.9789134720229));
#63478=CARTESIAN_POINT('Ctrl Pts',(30.5696717075202,19.084372100307,36.9660294515073));
#63479=CARTESIAN_POINT('Ctrl Pts',(30.4505033572301,19.05290000393,36.9573901538706));
#63480=CARTESIAN_POINT('Ctrl Pts',(30.2559420711087,19.020343548509,36.9436898968894));
#63481=CARTESIAN_POINT('Ctrl Pts',(30.1820392630783,19.0121846476817,36.9385825419192));
#63482=CARTESIAN_POINT('Ctrl Pts',(30.0904986835374,19.0072282110943,36.9324971381318));
#63483=CARTESIAN_POINT('Ctrl Pts',(30.0731379592029,19.0065155374074,36.9313537796742));
#63484=CARTESIAN_POINT('Ctrl Pts',(30.0452754435835,19.0057362493949,36.9295383293677));
#63485=CARTESIAN_POINT('Ctrl Pts',(30.0347789939,19.0055255813799,36.9288588541997));
#63486=CARTESIAN_POINT('Ctrl Pts',(30.0140837766536,19.005273650292,36.9275285836808));
#63487=CARTESIAN_POINT('Ctrl Pts',(30.0038854874693,19.0052277138254,36.9268775826602));
#63488=CARTESIAN_POINT('Ctrl Pts',(29.9777397174193,19.0053104592963,36.9252192026252));
#63489=CARTESIAN_POINT('Ctrl Pts',(29.9617929176046,19.0055521714252,36.9242178474603));
#63490=CARTESIAN_POINT('Ctrl Pts',(29.8899994323436,19.0075018093649,36.9197483962374));
#63491=CARTESIAN_POINT('Ctrl Pts',(29.8342318638349,19.0113644823723,36.916381884886));
#63492=CARTESIAN_POINT('Ctrl Pts',(29.6405289045097,19.0329880599958,36.9048330082955));
#63493=CARTESIAN_POINT('Ctrl Pts',(29.5043510713071,19.0628137583321,36.8969455773903));
#63494=CARTESIAN_POINT('Ctrl Pts',(29.306573983947,19.1283713713343,36.8846476268788));
#63495=CARTESIAN_POINT('Ctrl Pts',(29.2419584534486,19.1535967474226,36.8804906917809));
#63496=CARTESIAN_POINT('Ctrl Pts',(29.1556456019692,19.1925879697277,36.8746606160187));
#63497=CARTESIAN_POINT('Ctrl Pts',(29.1327028425009,19.2034844431534,36.8730833353602));
#63498=CARTESIAN_POINT('Ctrl Pts',(29.094279685868,19.2226407633797,36.8703913119002));
#63499=CARTESIAN_POINT('Ctrl Pts',(29.0786885194952,19.2306723685026,36.8692845890791));
#63500=CARTESIAN_POINT('Ctrl Pts',(29.0472320849437,19.2474052902033,36.867021256783));
#63501=CARTESIAN_POINT('Ctrl Pts',(29.0313752935115,19.2561189664718,36.8658642851627));
#63502=CARTESIAN_POINT('Ctrl Pts',(28.9918131296237,19.2785653517224,36.8629359513471));
#63503=CARTESIAN_POINT('Ctrl Pts',(28.9682686622855,19.2925725968994,36.8611548424468));
#63504=CARTESIAN_POINT('Ctrl Pts',(28.8590692792431,19.3606216889673,36.8527076378899));
#63505=CARTESIAN_POINT('Ctrl Pts',(28.7773337549541,19.4206437661393,36.845824652764));
#63506=CARTESIAN_POINT('Ctrl Pts',(28.5919030991364,19.5798642614653,36.8289010611239));
#63507=CARTESIAN_POINT('Ctrl Pts',(28.4936435258082,19.684547782622,36.8187645711298));
#63508=CARTESIAN_POINT('Ctrl Pts',(28.3924323754014,19.8187402428948,36.8074754861495));
#63509=CARTESIAN_POINT('Ctrl Pts',(28.3778032665314,19.8389116428921,36.8058198795782));
#63510=CARTESIAN_POINT('Ctrl Pts',(28.3566819727408,19.8692135930201,36.8033994341084));
#63511=CARTESIAN_POINT('Ctrl Pts',(28.3498978380449,19.8791365338724,36.8026171413259));
#63512=CARTESIAN_POINT('Ctrl Pts',(28.3377998356182,19.8971798289228,36.8012140966905));
#63513=CARTESIAN_POINT('Ctrl Pts',(28.3324550802124,19.9052782706601,36.800591408918));
#63514=CARTESIAN_POINT('Ctrl Pts',(28.3202544760473,19.9240614891959,36.7991631418085));
#63515=CARTESIAN_POINT('Ctrl Pts',(28.3134412459352,19.9347731257423,36.7983603058982));
#63516=CARTESIAN_POINT('Ctrl Pts',(28.2915224937793,19.9699709380131,36.7957576078963));
#63517=CARTESIAN_POINT('Ctrl Pts',(28.2768436795831,19.9947200654301,36.7939828145033));
#63518=CARTESIAN_POINT('Ctrl Pts',(28.2417000832152,20.0570068758419,36.7896295976838));
#63519=CARTESIAN_POINT('Ctrl Pts',(28.2218963417669,20.0949019781294,36.7870805022924));
#63520=CARTESIAN_POINT('Ctrl Pts',(28.1552996583477,20.2329743084075,36.7780417660263));
#63521=CARTESIAN_POINT('Ctrl Pts',(28.1156336597192,20.3363640582666,36.7717205270939));
#63522=CARTESIAN_POINT('Ctrl Pts',(28.0605293921342,20.5256754378019,36.7601816624638));
#63523=CARTESIAN_POINT('Ctrl Pts',(28.0417667170985,20.610320602388,36.7550359031402));
#63524=CARTESIAN_POINT('Ctrl Pts',(28.0244772296112,20.7224099562335,36.7480704341553));
#63525=CARTESIAN_POINT('Ctrl Pts',(28.0209247192546,20.7489873005574,36.7464084049198));
#63526=CARTESIAN_POINT('Ctrl Pts',(28.0160898839718,20.7916978437649,36.7437168309782));
#63527=CARTESIAN_POINT('Ctrl Pts',(28.0144662497862,20.8077895977779,36.7426980830205));
#63528=CARTESIAN_POINT('Ctrl Pts',(28.0115968167425,20.8401656270264,36.740638199966));
#63529=CARTESIAN_POINT('Ctrl Pts',(28.0103549747104,20.8564489876068,36.7395970233493));
#63530=CARTESIAN_POINT('Ctrl Pts',(28.0080226188934,20.8929348103733,36.7372517647791));
#63531=CARTESIAN_POINT('Ctrl Pts',(28.0070392649365,20.9131420696515,36.7359444286128));
#63532=CARTESIAN_POINT('Ctrl Pts',(28.0056098626701,20.9559049249684,36.7331590673407));
#63533=CARTESIAN_POINT('Ctrl Pts',(28.0052387767564,20.9784598849025,36.7316789202021));
#63534=CARTESIAN_POINT('Ctrl Pts',(28.0052502584425,21.0010154093453,36.7301874407357));
#63535=CARTESIAN_POINT('Ctrl Pts',(29.0285070491141,22.7421908646526,36.5933647280801));
#63536=CARTESIAN_POINT('Ctrl Pts',(28.9676176456079,22.7082372792619,36.5978046508089));
#63537=CARTESIAN_POINT('Ctrl Pts',(28.9084752835363,22.6710682151059,36.6022445735377));
#63538=CARTESIAN_POINT('Ctrl Pts',(28.8514330820545,22.6308959493178,36.6066844962665));
#63539=CARTESIAN_POINT('Ctrl Pts',(28.7944006664215,22.5907305752643,36.6111236573064));
#63540=CARTESIAN_POINT('Ctrl Pts',(28.7394680955456,22.5475633047902,36.6155628183463));
#63541=CARTESIAN_POINT('Ctrl Pts',(28.6869589491316,22.501649346963,36.6200019793861));
#63542=CARTESIAN_POINT('Ctrl Pts',(28.6319025478678,22.4535080714257,36.6246564871848));
#63543=CARTESIAN_POINT('Ctrl Pts',(28.5795111414156,22.4023472009318,36.6293109949835));
#63544=CARTESIAN_POINT('Ctrl Pts',(28.5301161934672,22.3485062690965,36.6339655027822));
#63545=CARTESIAN_POINT('Ctrl Pts',(28.4829441605491,22.2970883343813,36.6384105443141));
#63546=CARTESIAN_POINT('Ctrl Pts',(28.4385049568665,22.2432268115348,36.642855585846));
#63547=CARTESIAN_POINT('Ctrl Pts',(28.3970458829366,22.1872513049432,36.6473006273779));
#63548=CARTESIAN_POINT('Ctrl Pts',(28.355557612108,22.1312363784844,36.6517487992602));
#63549=CARTESIAN_POINT('Ctrl Pts',(28.3170539153061,22.0731049144069,36.6561969711424));
#63550=CARTESIAN_POINT('Ctrl Pts',(28.2817379201812,22.0132141864171,36.6606451430247));
#63551=CARTESIAN_POINT('Ctrl Pts',(28.2463644782723,21.9532260371397,36.6651005505284));
#63552=CARTESIAN_POINT('Ctrl Pts',(28.2141893024353,21.8914733502745,36.669555958032));
#63553=CARTESIAN_POINT('Ctrl Pts',(28.1853684355378,21.8283355888512,36.6740113655357));
#63554=CARTESIAN_POINT('Ctrl Pts',(28.1813907920867,21.8196217807573,36.6746262680139));
#63555=CARTESIAN_POINT('Ctrl Pts',(28.1774769626901,21.8108816159094,36.6752411704921));
#63556=CARTESIAN_POINT('Ctrl Pts',(28.1736272830851,21.8021161146672,36.6758560729703));
#63557=CARTESIAN_POINT('Ctrl Pts',(28.1429611739475,21.7322911304302,36.6807543160555));
#63558=CARTESIAN_POINT('Ctrl Pts',(28.116265697656,21.6606202638874,36.6856525591407));
#63559=CARTESIAN_POINT('Ctrl Pts',(28.0937438469357,21.5875500331072,36.6905508022258));
#63560=CARTESIAN_POINT('Ctrl Pts',(28.0712891522905,21.514697684506,36.6954344396383));
#63561=CARTESIAN_POINT('Ctrl Pts',(28.0529833994963,21.4404545853452,36.7003180770508));
#63562=CARTESIAN_POINT('Ctrl Pts',(28.0389815215822,21.365286312095,36.7052017144632));
#63563=CARTESIAN_POINT('Ctrl Pts',(28.0250482095369,21.2904861307532,36.7100614371662));
#63564=CARTESIAN_POINT('Ctrl Pts',(28.0153768565579,21.2147701145771,36.7149211598692));
#63565=CARTESIAN_POINT('Ctrl Pts',(28.0100720374931,21.1386155349627,36.7197808825722));
#63566=CARTESIAN_POINT('Ctrl Pts',(28.0068830567618,21.0928353709229,36.7227022945695));
#63567=CARTESIAN_POINT('Ctrl Pts',(28.0052711132345,21.0468970559952,36.7256237065667));
#63568=CARTESIAN_POINT('Ctrl Pts',(28.0052502061177,21.0009068111524,36.728545118564));
#63569=CARTESIAN_POINT('',(28.29025763663,22.0275229169844,36.501576848773));
#63570=CARTESIAN_POINT('Origin',(30.,21.,36.5));
#63571=CARTESIAN_POINT('',(28.0052500270373,21.000328428416,36.5704549034975));
#63572=CARTESIAN_POINT('Ctrl Pts',(28.2902566323839,22.0275238096476,36.5015864635853));
#63573=CARTESIAN_POINT('Ctrl Pts',(28.2530535621634,21.9656199374772,36.5061693646417));
#63574=CARTESIAN_POINT('Ctrl Pts',(28.2192474515991,21.9017453975362,36.510752265698));
#63575=CARTESIAN_POINT('Ctrl Pts',(28.1890241385836,21.8362977889886,36.5153351667544));
#63576=CARTESIAN_POINT('Ctrl Pts',(28.1587307817518,21.7706985028179,36.5199286888793));
#63577=CARTESIAN_POINT('Ctrl Pts',(28.1320369926429,21.7035192682946,36.5245222110042));
#63578=CARTESIAN_POINT('Ctrl Pts',(28.1090803750041,21.6351775612419,36.5291157331292));
#63579=CARTESIAN_POINT('Ctrl Pts',(28.0860958385404,21.5667527400224,36.5337148416929));
#63580=CARTESIAN_POINT('Ctrl Pts',(28.066857645781,21.497163054947,36.5383139502567));
#63581=CARTESIAN_POINT('Ctrl Pts',(28.0514526602536,21.4268381745663,36.5429130588204));
#63582=CARTESIAN_POINT('Ctrl Pts',(28.0360074155949,21.3563295083206,36.5475241866175));
#63583=CARTESIAN_POINT('Ctrl Pts',(28.0244154684101,21.2850822436007,36.5521353144146));
#63584=CARTESIAN_POINT('Ctrl Pts',(28.0167120719566,21.2135335031729,36.5567464422117));
#63585=CARTESIAN_POINT('Ctrl Pts',(28.0112867761488,21.1631436415273,36.5599939360227));
#63586=CARTESIAN_POINT('Ctrl Pts',(28.0077891046199,21.1126043416051,36.5632414298337));
#63587=CARTESIAN_POINT('Ctrl Pts',(28.0062158685675,21.0620677029381,36.5664889236447));
#63588=CARTESIAN_POINT('Ctrl Pts',(28.0055754375071,21.0414953081962,36.5678109095616));
#63589=CARTESIAN_POINT('Ctrl Pts',(28.0052534198484,21.0209135090081,36.5691328954784));
#63590=CARTESIAN_POINT('Ctrl Pts',(28.005250027094,21.0003287725725,36.5704548813952));
#63591=CARTESIAN_POINT('Ctrl Pts',(28.0052500269806,21.0003280842595,36.5704549255998));
#63592=CARTESIAN_POINT('Ctrl Pts',(28.0052386714972,20.9312868256578,36.574888869682));
#63593=CARTESIAN_POINT('Ctrl Pts',(28.0088160317775,20.8621028756339,36.5793228137642));
#63594=CARTESIAN_POINT('Ctrl Pts',(28.0160004941859,20.7931823909103,36.5837567578465));
#63595=CARTESIAN_POINT('Ctrl Pts',(28.0234042602584,20.7221581280657,36.588326046806));
#63596=CARTESIAN_POINT('Ctrl Pts',(28.0346390301168,20.651414201514,36.5928953357655));
#63597=CARTESIAN_POINT('Ctrl Pts',(28.0496669166672,20.5813970538116,36.5974646247251));
#63598=CARTESIAN_POINT('Ctrl Pts',(28.0642105588504,20.5136360722889,36.6018866772496));
#63599=CARTESIAN_POINT('Ctrl Pts',(28.0823064725704,20.4465562705405,36.6063087297742));
#63600=CARTESIAN_POINT('Ctrl Pts',(28.1038678101182,20.3805564747339,36.6107307822988));
#63601=CARTESIAN_POINT('Ctrl Pts',(28.1254162281456,20.3145962259038,36.6151501851362));
#63602=CARTESIAN_POINT('Ctrl Pts',(28.1504257983438,20.249715168508,36.6195695879737));
#63603=CARTESIAN_POINT('Ctrl Pts',(28.1787594529453,20.1862983149435,36.6239889908111));
#63604=CARTESIAN_POINT('Ctrl Pts',(28.2070859824803,20.1228974088203,36.628407282301));
#63605=CARTESIAN_POINT('Ctrl Pts',(28.2387347352602,20.0609604267976,36.6328255737909));
#63606=CARTESIAN_POINT('Ctrl Pts',(28.2735207007135,20.0008519671064,36.6372438652808));
#63607=CARTESIAN_POINT('Ctrl Pts',(28.3083100144199,19.9407377217963,36.6416625820444));
#63608=CARTESIAN_POINT('Ctrl Pts',(28.3462368897675,19.8824527744823,36.6460812988081));
#63609=CARTESIAN_POINT('Ctrl Pts',(28.3870715365556,19.8263350843146,36.6505000155717));
#63610=CARTESIAN_POINT('Ctrl Pts',(28.4279494873314,19.770157882924,36.6549234182595));
#63611=CARTESIAN_POINT('Ctrl Pts',(28.4717410687165,19.7161529232429,36.6593468209473));
#63612=CARTESIAN_POINT('Ctrl Pts',(28.5181751866023,19.6646263500807,36.6637702236351));
#63613=CARTESIAN_POINT('Ctrl Pts',(28.5646391040617,19.6130667092093,36.6681964650871));
#63614=CARTESIAN_POINT('Ctrl Pts',(28.6137485814085,19.5639889673164,36.6726227065391));
#63615=CARTESIAN_POINT('Ctrl Pts',(28.6651965229941,19.5176615635177,36.6770489479911));
#63616=CARTESIAN_POINT('Ctrl Pts',(28.7167278672448,19.4712590579981,36.6814823648582));
#63617=CARTESIAN_POINT('Ctrl Pts',(28.7706048521435,19.4276160918823,36.6859157817252));
#63618=CARTESIAN_POINT('Ctrl Pts',(28.8264891705401,19.3869594252964,36.6903491985923));
#63619=CARTESIAN_POINT('Ctrl Pts',(28.8393906176858,19.3775734320494,36.6913726966867));
#63620=CARTESIAN_POINT('Ctrl Pts',(28.8523989386336,19.3683464074629,36.6923961947811));
#63621=CARTESIAN_POINT('Ctrl Pts',(28.8655097834363,19.3592807945839,36.6934196928754));
#63622=CARTESIAN_POINT('Ctrl Pts',(28.9226695512531,19.3197571532715,36.6978818701277));
#63623=CARTESIAN_POINT('Ctrl Pts',(28.9820056711569,19.2831490561882,36.70234404738));
#63624=CARTESIAN_POINT('Ctrl Pts',(29.0431890178685,19.2497027946739,36.7068062246323));
#63625=CARTESIAN_POINT('Ctrl Pts',(29.1042829228631,19.2163054270369,36.7112618787894));
#63626=CARTESIAN_POINT('Ctrl Pts',(29.1672182698099,19.1860609517794,36.7157175329465));
#63627=CARTESIAN_POINT('Ctrl Pts',(29.2316367156414,19.159172624674,36.7201731871036));
#63628=CARTESIAN_POINT('Ctrl Pts',(29.2959823945075,19.1323146705766,36.7246238081614));
#63629=CARTESIAN_POINT('Ctrl Pts',(29.3618073968103,19.1088055213526,36.7290744292193));
#63630=CARTESIAN_POINT('Ctrl Pts',(29.4287300887424,19.0888018807586,36.7335250502771));
#63631=CARTESIAN_POINT('Ctrl Pts',(29.4956125476592,19.0688102660823,36.7379729956819));
#63632=CARTESIAN_POINT('Ctrl Pts',(29.5635909208368,19.0523201179599,36.7424209410867));
#63633=CARTESIAN_POINT('Ctrl Pts',(29.6322663951171,19.0394389684736,36.7468688864915));
#63634=CARTESIAN_POINT('Ctrl Pts',(29.7009236688492,19.0265612327822,36.7513156530905));
#63635=CARTESIAN_POINT('Ctrl Pts',(29.7702771979811,19.0172906864354,36.7557624196896));
#63636=CARTESIAN_POINT('Ctrl Pts',(29.8399176209918,19.0116838293594,36.7602091862886));
#63637=CARTESIAN_POINT('Ctrl Pts',(29.9095629973759,19.0060765734797,36.7646562691765));
#63638=CARTESIAN_POINT('Ctrl Pts',(29.9794948221041,19.0041335609959,36.7691033520645));
#63639=CARTESIAN_POINT('Ctrl Pts',(30.0493000077049,19.0058593149579,36.7735504349525));
#63640=CARTESIAN_POINT('Ctrl Pts',(30.1191800615645,19.0075869198453,36.7780022874768));
#63641=CARTESIAN_POINT('Ctrl Pts',(30.1889327169807,19.0129911325344,36.7824541400012));
#63642=CARTESIAN_POINT('Ctrl Pts',(30.2581472309743,19.0220243758731,36.7869059925255));
#63643=CARTESIAN_POINT('Ctrl Pts',(30.3274030821619,19.031063014163,36.7913605038432));
#63644=CARTESIAN_POINT('Ctrl Pts',(30.3961196727158,19.0437349089237,36.795815015161));
#63645=CARTESIAN_POINT('Ctrl Pts',(30.4638964470654,19.0599413284903,36.8002695264787));
#63646=CARTESIAN_POINT('Ctrl Pts',(30.5317904704488,19.0761757840184,36.8047317437864));
#63647=CARTESIAN_POINT('Ctrl Pts',(30.5987409649366,19.0959568315954,36.8091939610942));
#63648=CARTESIAN_POINT('Ctrl Pts',(30.6643632856274,19.1191361061442,36.813656178402));
#63649=CARTESIAN_POINT('Ctrl Pts',(30.6971791408953,19.1307274017705,36.8158876063034));
#63650=CARTESIAN_POINT('Ctrl Pts',(30.7296631820897,19.1431677458785,36.8181190342048));
#63651=CARTESIAN_POINT('Ctrl Pts',(30.761769523972,19.1564342282285,36.8203504621062));
#63652=CARTESIAN_POINT('Ctrl Pts',(30.8258050956774,19.1828940094428,36.824801008416));
#63653=CARTESIAN_POINT('Ctrl Pts',(30.8885889960873,19.2127472807336,36.8292515547259));
#63654=CARTESIAN_POINT('Ctrl Pts',(30.9497368226418,19.2458541878686,36.8337021010357));
#63655=CARTESIAN_POINT('Ctrl Pts',(31.0107920689531,19.2789109698283,36.8381459090413));
#63656=CARTESIAN_POINT('Ctrl Pts',(31.0702157298272,19.3152113794572,36.8425897170468));
#63657=CARTESIAN_POINT('Ctrl Pts',(31.1276433749924,19.3545675397222,36.8470335250524));
#63658=CARTESIAN_POINT('Ctrl Pts',(31.1850026111637,19.3938768181184,36.8514720395023));
#63659=CARTESIAN_POINT('Ctrl Pts',(31.2403701512933,19.436234341885,36.8559105539523));
#63660=CARTESIAN_POINT('Ctrl Pts',(31.2934077780998,19.4814072691959,36.8603490684022));
#63661=CARTESIAN_POINT('Ctrl Pts',(31.3464115884187,19.5265513945067,36.8647847528807));
#63662=CARTESIAN_POINT('Ctrl Pts',(31.3970880597347,19.5745070452748,36.8692204373592));
#63663=CARTESIAN_POINT('Ctrl Pts',(31.4451307387815,19.625000105335,36.8736561218377));
#63664=CARTESIAN_POINT('Ctrl Pts',(31.4931591819423,19.6754782034183,36.8780904919453));
#63665=CARTESIAN_POINT('Ctrl Pts',(31.5385550441581,19.728491863154,36.8825248620529));
#63666=CARTESIAN_POINT('Ctrl Pts',(31.5810488507624,19.7837302544242,36.8869592321605));
#63667=CARTESIAN_POINT('Ctrl Pts',(31.6235445674886,19.838971128693,36.8913938015957));
#63668=CARTESIAN_POINT('Ctrl Pts',(31.6631376725093,19.8964365428245,36.8958283710309));
#63669=CARTESIAN_POINT('Ctrl Pts',(31.6996002142036,19.9557841820873,36.9002629404661));
#63670=CARTESIAN_POINT('Ctrl Pts',(31.7361012208808,20.015194428229,36.9047021880074));
#63671=CARTESIAN_POINT('Ctrl Pts',(31.7694648155461,20.0764904438482,36.9091414355486));
#63672=CARTESIAN_POINT('Ctrl Pts',(31.7995080072554,20.1393034830303,36.9135806830899));
#63673=CARTESIAN_POINT('Ctrl Pts',(31.8295687154451,20.2021531449316,36.9180225189045));
#63674=CARTESIAN_POINT('Ctrl Pts',(31.8563049794955,20.2665211377134,36.9224643547192));
#63675=CARTESIAN_POINT('Ctrl Pts',(31.8795822660123,20.3320194106172,36.9269061905338));
#63676=CARTESIAN_POINT('Ctrl Pts',(31.9029000655277,20.3976316801177,36.9313557571502));
#63677=CARTESIAN_POINT('Ctrl Pts',(31.9227467310129,20.4643776864229,36.9358053237667));
#63678=CARTESIAN_POINT('Ctrl Pts',(31.9390380341855,20.531855722579,36.9402548903831));
#63679=CARTESIAN_POINT('Ctrl Pts',(31.9476132701235,20.567374064761,36.9425970040344));
#63680=CARTESIAN_POINT('Ctrl Pts',(31.9552043041219,20.6030950764752,36.9449391176857));
#63681=CARTESIAN_POINT('Ctrl Pts',(31.9618046223388,20.6389595780662,36.947281231337));
#63682=CARTESIAN_POINT('Ctrl Pts',(31.9743612682226,20.7071892954034,36.9517369394972));
#63683=CARTESIAN_POINT('Ctrl Pts',(31.983378916413,20.7762090129602,36.9561926476574));
#63684=CARTESIAN_POINT('Ctrl Pts',(31.9887669676629,20.8456189427659,36.9606483558175));
#63685=CARTESIAN_POINT('Ctrl Pts',(31.9941469496941,20.9149249233175,36.9650973910486));
#63686=CARTESIAN_POINT('Ctrl Pts',(31.995908086141,20.9846194724866,36.9695464262797));
#63687=CARTESIAN_POINT('Ctrl Pts',(31.9940109741103,21.0542936241897,36.9739954615108));
#63688=CARTESIAN_POINT('Ctrl Pts',(31.9921160888979,21.1238859928087,36.9784392744922));
#63689=CARTESIAN_POINT('Ctrl Pts',(31.9865714971795,21.1934575249014,36.9828830874735));
#63690=CARTESIAN_POINT('Ctrl Pts',(31.9773897947127,21.2625969578388,36.9873269004548));
#63691=CARTESIAN_POINT('Ctrl Pts',(31.9682138543114,21.3316930016611,36.9917679246786));
#63692=CARTESIAN_POINT('Ctrl Pts',(31.9554053955368,21.4003570005243,36.9962089489025));
#63693=CARTESIAN_POINT('Ctrl Pts',(31.9390289146708,21.4681820485352,37.0006499731263));
#63694=CARTESIAN_POINT('Ctrl Pts',(31.9226571582324,21.5359875297947,37.0050897161654));
#63695=CARTESIAN_POINT('Ctrl Pts',(31.902719537934,21.6029540654654,37.0095294592044));
#63696=CARTESIAN_POINT('Ctrl Pts',(31.879331443147,21.6686859422024,37.0139692022435));
#63697=CARTESIAN_POINT('Ctrl Pts',(31.8559421655853,21.734421143109,37.0184091698077));
#63698=CARTESIAN_POINT('Ctrl Pts',(31.8291022333342,21.7989211011065,37.0228491373719));
#63699=CARTESIAN_POINT('Ctrl Pts',(31.7989760009868,21.8618079312547,37.0272891049362));
#63700=CARTESIAN_POINT('Ctrl Pts',(31.7688180178141,21.9247610394802,37.0317337518985));
#63701=CARTESIAN_POINT('Ctrl Pts',(31.7353670334275,21.9860971845992,37.0361783988608));
#63702=CARTESIAN_POINT('Ctrl Pts',(31.6988339900007,22.0454619251405,37.0406230458231));
#63703=CARTESIAN_POINT('Ctrl Pts',(31.6622795997693,22.1048613533888,37.0450702898592));
#63704=CARTESIAN_POINT('Ctrl Pts',(31.6226398438709,22.162286681586,37.0495175338953));
#63705=CARTESIAN_POINT('Ctrl Pts',(31.5801681727807,22.2174136964199,37.0539647779315));
#63706=CARTESIAN_POINT('Ctrl Pts',(31.5376230902326,22.2726359972274,37.0584197089424));
#63707=CARTESIAN_POINT('Ctrl Pts',(31.4922366400443,22.3255516837158,37.0628746399534));
#63708=CARTESIAN_POINT('Ctrl Pts',(31.444301042517,22.3758713824644,37.0673295709644));
#63709=CARTESIAN_POINT('Ctrl Pts',(31.4196157836681,22.4017843751646,37.0696237141655));
#63710=CARTESIAN_POINT('Ctrl Pts',(31.3942550895449,22.4270095608114,37.0719178573667));
#63711=CARTESIAN_POINT('Ctrl Pts',(31.3682622464784,22.4515116215043,37.0742120005678));
#63712=CARTESIAN_POINT('Ctrl Pts',(31.3177777071752,22.4991006921917,37.078667794892));
#63713=CARTESIAN_POINT('Ctrl Pts',(31.2647084104482,22.5441461487519,37.0831235892161));
#63714=CARTESIAN_POINT('Ctrl Pts',(31.2093410011878,22.5863549115334,37.0875793835403));
#63715=CARTESIAN_POINT('Ctrl Pts',(31.1540562981378,22.6285006241042,37.0920285219298));
#63716=CARTESIAN_POINT('Ctrl Pts',(31.0964806819931,22.6678177591639,37.0964776603192));
#63717=CARTESIAN_POINT('Ctrl Pts',(31.0369362891096,22.7040512594484,37.1009267987086));
#63718=CARTESIAN_POINT('Ctrl Pts',(30.9774614551959,22.7402424322385,37.1053707396736));
#63719=CARTESIAN_POINT('Ctrl Pts',(30.9160228283773,22.773356871914,37.1098146806386));
#63720=CARTESIAN_POINT('Ctrl Pts',(30.8529726938128,22.8031819503616,37.1142586216036));
#63721=CARTESIAN_POINT('Ctrl Pts',(30.789961908263,22.8329884152493,37.1186997891455));
#63722=CARTESIAN_POINT('Ctrl Pts',(30.7253420513037,22.8595093828041,37.1231409566874));
#63723=CARTESIAN_POINT('Ctrl Pts',(30.6594899134094,22.8825781833993,37.1275821242293));
#63724=CARTESIAN_POINT('Ctrl Pts',(30.5936565478156,22.9056404078306,37.132022025739));
#63725=CARTESIAN_POINT('Ctrl Pts',(30.5265920600452,22.9252522573811,37.1364619272486));
#63726=CARTESIAN_POINT('Ctrl Pts',(30.4586914576963,22.9412958839745,37.1409018287583));
#63727=CARTESIAN_POINT('Ctrl Pts',(30.3907871924322,22.9573403760455,37.1453419697795));
#63728=CARTESIAN_POINT('Ctrl Pts',(30.3220471995847,22.9698161528819,37.1497821108008));
#63729=CARTESIAN_POINT('Ctrl Pts',(30.2528780842132,22.9786561694809,37.154222251822));
#63730=CARTESIAN_POINT('Ctrl Pts',(30.183635734459,22.9875055456496,37.1586670939441));
#63731=CARTESIAN_POINT('Ctrl Pts',(30.1139638414636,22.9927114163849,37.1631119360662));
#63732=CARTESIAN_POINT('Ctrl Pts',(30.0442746033641,22.9942585895508,37.1675567781883));
#63733=CARTESIAN_POINT('Ctrl Pts',(29.9745444485121,22.9958066711109,37.1720042300176));
#63734=CARTESIAN_POINT('Ctrl Pts',(29.9047974172846,22.9936917942619,37.1764516818469));
#63735=CARTESIAN_POINT('Ctrl Pts',(29.8354433862942,22.9879508754961,37.1808991336762));
#63736=CARTESIAN_POINT('Ctrl Pts',(29.7659692095172,22.9822000114223,37.1853542900699));
#63737=CARTESIAN_POINT('Ctrl Pts',(29.6968898764961,22.9728106325431,37.1898094464635));
#63738=CARTESIAN_POINT('Ctrl Pts',(29.6286070416676,22.9598711266308,37.1942646028572));
#63739=CARTESIAN_POINT('Ctrl Pts',(29.5934671800723,22.9532121698372,37.196557325171));
#63740=CARTESIAN_POINT('Ctrl Pts',(29.5585380467932,22.9456138345229,37.1988500474848));
#63741=CARTESIAN_POINT('Ctrl Pts',(29.5238726929801,22.9370932734409,37.2011427697985));
#63742=CARTESIAN_POINT('Ctrl Pts',(29.4565256301231,22.9205397206959,37.2055970186896));
#63743=CARTESIAN_POINT('Ctrl Pts',(29.3899099067316,22.9004371101155,37.2100512675806));
#63744=CARTESIAN_POINT('Ctrl Pts',(29.3244270369207,22.8768667331636,37.2145055164717));
#63745=CARTESIAN_POINT('Ctrl Pts',(29.2590489305348,22.8533340655153,37.218952639188));
#63746=CARTESIAN_POINT('Ctrl Pts',(29.1948005354634,22.8263448123012,37.2233997619044));
#63747=CARTESIAN_POINT('Ctrl Pts',(29.1320706273667,22.7960306697327,37.2278468846207));
#63748=CARTESIAN_POINT('Ctrl Pts',(29.0970547557198,22.7791092974962,37.2303292711403));
#63749=CARTESIAN_POINT('Ctrl Pts',(29.06251179142,22.7611528326649,37.2328116576599));
#63750=CARTESIAN_POINT('Ctrl Pts',(29.0285070491141,22.7421908646526,37.2352940441794));
#63751=CARTESIAN_POINT('Origin',(30.,21.,34.5704548813952));
#63752=CARTESIAN_POINT('',(29.0285070492154,22.7421908647091,38.1915268296408));
#63753=CARTESIAN_POINT('',(29.0285070491141,22.7421908646526,38.0351948256389));
#63754=CARTESIAN_POINT('',(29.0285070491141,22.7421908646526,34.5704548813952));
#63755=CARTESIAN_POINT('Ctrl Pts',(29.0285070492154,22.7421908647091,38.1915268296408));
#63756=CARTESIAN_POINT('Ctrl Pts',(29.0365800098479,22.7466925668505,38.1909595153784));
#63757=CARTESIAN_POINT('Ctrl Pts',(29.04468452496,22.7511383037825,38.1903948448985));
#63758=CARTESIAN_POINT('Ctrl Pts',(29.17424040473,22.8210390713102,38.1814406805563));
#63759=CARTESIAN_POINT('Ctrl Pts',(29.3021415357132,22.8737832221873,38.1735891043926));
#63760=CARTESIAN_POINT('Ctrl Pts',(29.5114982215156,22.9356768422155,38.1608674012811));
#63761=CARTESIAN_POINT('Ctrl Pts',(29.5898222654284,22.9537736424879,38.1561393308334));
#63762=CARTESIAN_POINT('Ctrl Pts',(29.706476237995,22.9734016687763,38.148975413452));
#63763=CARTESIAN_POINT('Ctrl Pts',(29.7441040460161,22.9786326899555,38.1466469977521));
#63764=CARTESIAN_POINT('Ctrl Pts',(29.8019359873461,22.9849952835544,38.1430291420011));
#63765=CARTESIAN_POINT('Ctrl Pts',(29.8220472691853,22.986899193958,38.1417638477182));
#63766=CARTESIAN_POINT('Ctrl Pts',(29.8592611977757,22.9898526677302,38.1394076556626));
#63767=CARTESIAN_POINT('Ctrl Pts',(29.8763552645962,22.9909879455026,38.1383195636265));
#63768=CARTESIAN_POINT('Ctrl Pts',(29.9143811365715,22.9930217910881,38.1358853082497));
#63769=CARTESIAN_POINT('Ctrl Pts',(29.9353165000315,22.9938110338678,38.1345358384149));
#63770=CARTESIAN_POINT('Ctrl Pts',(29.9968882439604,22.9951614838551,38.1305381587301));
#63771=CARTESIAN_POINT('Ctrl Pts',(30.0375318190381,22.9948107671914,38.1278621632728));
#63772=CARTESIAN_POINT('Ctrl Pts',(30.2258584634346,22.9874283790031,38.1152852304615));
#63773=CARTESIAN_POINT('Ctrl Pts',(30.3724640935126,22.9652333253242,38.1049404294473));
#63774=CARTESIAN_POINT('Ctrl Pts',(30.570741395996,22.9122190722138,38.0906530865214));
#63775=CARTESIAN_POINT('Ctrl Pts',(30.6255735345576,22.894989709113,38.0866755334977));
#63776=CARTESIAN_POINT('Ctrl Pts',(30.7125786403059,22.86346197472,38.0803899137055));
#63777=CARTESIAN_POINT('Ctrl Pts',(30.7452503010156,22.8506380458435,38.0780358611323));
#63778=CARTESIAN_POINT('Ctrl Pts',(30.7901627955289,22.831626967783,38.0748245414112));
#63779=CARTESIAN_POINT('Ctrl Pts',(30.8027021492279,22.8261664429801,38.0739306968194));
#63780=CARTESIAN_POINT('Ctrl Pts',(30.824126600144,22.8165733941425,38.0724094441732));
#63781=CARTESIAN_POINT('Ctrl Pts',(30.8330390066345,22.8125036769592,38.071778439769));
#63782=CARTESIAN_POINT('Ctrl Pts',(30.8522186885074,22.8035741962733,38.0704247585852));
#63783=CARTESIAN_POINT('Ctrl Pts',(30.8624749173958,22.7986921933208,38.0697034188892));
#63784=CARTESIAN_POINT('Ctrl Pts',(30.8914706320288,22.7845850817138,38.0676697497463));
#63785=CARTESIAN_POINT('Ctrl Pts',(30.9101082760709,22.7751526152732,38.0663693225785));
#63786=CARTESIAN_POINT('Ctrl Pts',(31.0575902165645,22.697578813938,38.0561059090748));
#63787=CARTESIAN_POINT('Ctrl Pts',(31.1787770002033,22.6157867233193,38.0478142623707));
#63788=CARTESIAN_POINT('Ctrl Pts',(31.3696085324446,22.4539941518065,38.0332522327653));
#63789=CARTESIAN_POINT('Ctrl Pts',(31.4438070964583,22.3803419914948,38.0271035197814));
#63790=CARTESIAN_POINT('Ctrl Pts',(31.5298650756104,22.2803511528691,38.0190096932702));
#63791=CARTESIAN_POINT('Ctrl Pts',(31.5473975758435,22.2591055760042,38.0173037397508));
#63792=CARTESIAN_POINT('Ctrl Pts',(31.5757246577007,22.2232937776063,38.0144461502316));
#63793=CARTESIAN_POINT('Ctrl Pts',(31.586770925177,22.2089308745206,38.0133047009676));
#63794=CARTESIAN_POINT('Ctrl Pts',(31.6081048038498,22.1803953265292,38.0110447796811));
#63795=CARTESIAN_POINT('Ctrl Pts',(31.6184044794508,22.1662337225799,38.0099269219977));
#63796=CARTESIAN_POINT('Ctrl Pts',(31.6431048365196,22.1313143914951,38.0071784874097));
#63797=CARTESIAN_POINT('Ctrl Pts',(31.6572998571073,22.1104156170168,38.0055402726073));
#63798=CARTESIAN_POINT('Ctrl Pts',(31.7081404802935,22.032417769243,37.9994477387248));
#63799=CARTESIAN_POINT('Ctrl Pts',(31.742259746902,21.9737348714386,37.9949035570723));
#63800=CARTESIAN_POINT('Ctrl Pts',(31.8377247831637,21.7884010041351,37.9806857591672));
#63801=CARTESIAN_POINT('Ctrl Pts',(31.8887223093803,21.6569104137249,37.9707508615294));
#63802=CARTESIAN_POINT('Ctrl Pts',(31.9401255390151,21.4670006653344,37.9571877036123));
#63803=CARTESIAN_POINT('Ctrl Pts',(31.9524963592611,21.4122327344734,37.9533682340408));
#63804=CARTESIAN_POINT('Ctrl Pts',(31.965399007328,21.3413050821042,37.9485960998558));
#63805=CARTESIAN_POINT('Ctrl Pts',(31.9680676605472,21.3255643400712,37.9475479711228));
#63806=CARTESIAN_POINT('Ctrl Pts',(31.9721310483743,21.2997177073479,37.9458466540851));
#63807=CARTESIAN_POINT('Ctrl Pts',(31.9736377132647,21.2896303982261,37.9451875779669));
#63808=CARTESIAN_POINT('Ctrl Pts',(31.9763562190106,21.2704224420834,37.9439424680055));
#63809=CARTESIAN_POINT('Ctrl Pts',(31.9775824391884,21.2613042403052,37.9433555991971));
#63810=CARTESIAN_POINT('Ctrl Pts',(31.9807697285647,21.2362947503285,37.9417566159598));
#63811=CARTESIAN_POINT('Ctrl Pts',(31.9826026679967,21.2203874452233,37.9407513806375));
#63812=CARTESIAN_POINT('Ctrl Pts',(31.9895929916324,21.1525474699744,37.9365079480485));
#63813=CARTESIAN_POINT('Ctrl Pts',(31.9929032866454,21.1004411941988,37.9333570623933));
#63814=CARTESIAN_POINT('Ctrl Pts',(31.9976126614615,20.9058471974677,37.9217976483913));
#63815=CARTESIAN_POINT('Ctrl Pts',(31.9857942187847,20.7634708645238,37.9137262535013));
#63816=CARTESIAN_POINT('Ctrl Pts',(31.9456057440939,20.5543376691775,37.9011586157495));
#63817=CARTESIAN_POINT('Ctrl Pts',(31.9286441451956,20.485872675882,37.8969312416665));
#63818=CARTESIAN_POINT('Ctrl Pts',(31.9008105876728,20.3945487784849,37.8910505617771));
#63819=CARTESIAN_POINT('Ctrl Pts',(31.8930766839286,20.370784096324,37.8894977499826));
#63820=CARTESIAN_POINT('Ctrl Pts',(31.8791261173115,20.330504888115,37.8868239520947));
#63821=CARTESIAN_POINT('Ctrl Pts',(31.8731329471791,20.3139157490065,37.8857104300889));
#63822=CARTESIAN_POINT('Ctrl Pts',(31.8605004142059,20.2803486706604,37.8834310845565));
#63823=CARTESIAN_POINT('Ctrl Pts',(31.8538467421039,20.2633779480695,37.8822648680552));
#63824=CARTESIAN_POINT('Ctrl Pts',(31.8363490719971,20.2204879966235,37.8792810703293));
#63825=CARTESIAN_POINT('Ctrl Pts',(31.8251886274952,20.1947030248264,37.8774529567593));
#63826=CARTESIAN_POINT('Ctrl Pts',(31.7678171306725,20.069476825239,37.8684007133234));
#63827=CARTESIAN_POINT('Ctrl Pts',(31.7140116982449,19.9737407123065,37.86091967338));
#63828=CARTESIAN_POINT('Ctrl Pts',(31.6060319032221,19.8139937248266,37.8475324685565));
#63829=CARTESIAN_POINT('Ctrl Pts',(31.5551744072725,19.7480487691076,37.8416984592184));
#63830=CARTESIAN_POINT('Ctrl Pts',(31.4715834960407,19.6526415371946,37.8329204961276));
#63831=CARTESIAN_POINT('Ctrl Pts',(31.441747419404,19.6207619422863,37.8299241654506));
#63832=CARTESIAN_POINT('Ctrl Pts',(31.3902499151999,19.569236201777,37.8250059006833));
#63833=CARTESIAN_POINT('Ctrl Pts',(31.3691599303784,19.5490412948252,37.8230574527094));
#63834=CARTESIAN_POINT('Ctrl Pts',(31.3382173537081,19.5206876698258,37.8203008498271));
#63835=CARTESIAN_POINT('Ctrl Pts',(31.3287187815302,19.5121501834922,37.8194679631413));
#63836=CARTESIAN_POINT('Ctrl Pts',(31.312550186523,19.4978959044242,37.8180734829072));
#63837=CARTESIAN_POINT('Ctrl Pts',(31.3059234640638,19.4921310990031,37.8175084567572));
#63838=CARTESIAN_POINT('Ctrl Pts',(31.2905219130485,19.4789104814704,37.8162103216059));
#63839=CARTESIAN_POINT('Ctrl Pts',(31.2817203256556,19.471486619702,37.8154795030613));
#63840=CARTESIAN_POINT('Ctrl Pts',(31.2562075988905,19.450342780771,37.8133909764482));
#63841=CARTESIAN_POINT('Ctrl Pts',(31.2393365079515,19.4368173053894,37.8120461920918));
#63842=CARTESIAN_POINT('Ctrl Pts',(31.1419843348333,19.3613376659719,37.804468890111));
#63843=CARTESIAN_POINT('Ctrl Pts',(31.0570757537695,19.3053207085734,37.7985533536824));
#63844=CARTESIAN_POINT('Ctrl Pts',(30.8830409175739,19.2086967250122,37.7869975478721));
#63845=CARTESIAN_POINT('Ctrl Pts',(30.7944694110043,19.1676938316014,37.781369560801));
#63846=CARTESIAN_POINT('Ctrl Pts',(30.648207810546,19.1125903719245,37.7720758147644));
#63847=CARTESIAN_POINT('Ctrl Pts',(30.5922694474847,19.0942968647123,37.7685231180385));
#63848=CARTESIAN_POINT('Ctrl Pts',(30.5128886839025,19.0721698642366,37.7634348190275));
#63849=CARTESIAN_POINT('Ctrl Pts',(30.4900596550042,19.0662406315522,37.7619663525104));
#63850=CARTESIAN_POINT('Ctrl Pts',(30.4502088604187,19.0566414278505,37.7593913723901));
#63851=CARTESIAN_POINT('Ctrl Pts',(30.4332339450496,19.0527868951685,37.7582909185817));
#63852=CARTESIAN_POINT('Ctrl Pts',(30.3979441854316,19.045257853421,37.7559946722969));
#63853=CARTESIAN_POINT('Ctrl Pts',(30.379623884991,19.0416174783825,37.7547979053101));
#63854=CARTESIAN_POINT('Ctrl Pts',(30.3314293848595,19.032742543633,37.7516361646813));
#63855=CARTESIAN_POINT('Ctrl Pts',(30.301483171276,19.0279312722926,37.7496580376465));
#63856=CARTESIAN_POINT('Ctrl Pts',(30.1169987027008,19.0025914150675,37.7373828549941));
#63857=CARTESIAN_POINT('Ctrl Pts',(29.9606269134045,18.9995593215533,37.7265351049973));
#63858=CARTESIAN_POINT('Ctrl Pts',(29.74128703512,19.0210452139412,37.7111708313249));
#63859=CARTESIAN_POINT('Ctrl Pts',(29.6773830620616,19.0304534499627,37.706685640414));
#63860=CARTESIAN_POINT('Ctrl Pts',(29.588542986694,19.0479737875423,37.7005203398869));
#63861=CARTESIAN_POINT('Ctrl Pts',(29.5631405151695,19.0535013166384,37.6987658340742));
#63862=CARTESIAN_POINT('Ctrl Pts',(29.518357555042,19.0641669194333,37.695695684531));
#63863=CARTESIAN_POINT('Ctrl Pts',(29.498933064531,19.0691035346013,37.6943717547184));
#63864=CARTESIAN_POINT('Ctrl Pts',(29.4689080016486,19.0772178528433,37.6923407920378));
#63865=CARTESIAN_POINT('Ctrl Pts',(29.4582544697299,19.0801922776979,37.6916232146978));
#63866=CARTESIAN_POINT('Ctrl Pts',(29.4381271741554,19.085992630716,37.6902740386753));
#63867=CARTESIAN_POINT('Ctrl Pts',(29.428648939645,19.0888005725898,37.6896415316996));
#63868=CARTESIAN_POINT('Ctrl Pts',(29.4055321029332,19.095836311611,37.688105141187));
#63869=CARTESIAN_POINT('Ctrl Pts',(29.391917000842,19.1001403928171,37.6872055559768));
#63870=CARTESIAN_POINT('Ctrl Pts',(29.3434392927858,19.1160399772163,37.6840175931844));
#63871=CARTESIAN_POINT('Ctrl Pts',(29.3088502934627,19.1284525695894,37.6817709824414));
#63872=CARTESIAN_POINT('Ctrl Pts',(29.166743197239,19.183926797322,37.6725816596675));
#63873=CARTESIAN_POINT('Ctrl Pts',(29.0627287566824,19.2353568115754,37.6659437315219));
#63874=CARTESIAN_POINT('Ctrl Pts',(28.8874295612915,19.3419306086835,37.654017817658));
#63875=CARTESIAN_POINT('Ctrl Pts',(28.8143087223068,19.3934069218964,37.6487837602794));
#63876=CARTESIAN_POINT('Ctrl Pts',(28.7143644434042,19.474316197793,37.6410069708955));
#63877=CARTESIAN_POINT('Ctrl Pts',(28.6845788958735,19.4999210501602,37.6386021999299));
#63878=CARTESIAN_POINT('Ctrl Pts',(28.6404663197341,19.5401665418745,37.6348912988511));
#63879=CARTESIAN_POINT('Ctrl Pts',(28.6255759991514,19.5541769921639,37.6336113748825));
#63880=CARTESIAN_POINT('Ctrl Pts',(28.5986136220483,19.580339104199,37.6312411722315));
#63881=CARTESIAN_POINT('Ctrl Pts',(28.5864775765877,19.592422233784,37.6301539377632));
#63882=CARTESIAN_POINT('Ctrl Pts',(28.5600325858841,19.6194388449124,37.6277383000814));
#63883=CARTESIAN_POINT('Ctrl Pts',(28.5457974412304,19.6344414617993,37.6264068469774));
#63884=CARTESIAN_POINT('Ctrl Pts',(28.5052203826974,19.6785602722322,37.6225183392841));
#63885=CARTESIAN_POINT('Ctrl Pts',(28.4795028524336,19.708234880024,37.6199357443588));
#63886=CARTESIAN_POINT('Ctrl Pts',(28.3430094690274,19.8754570141499,37.6055517139773));
#63887=CARTESIAN_POINT('Ctrl Pts',(28.2500137321363,20.0264789741271,37.5930720741977));
#63888=CARTESIAN_POINT('Ctrl Pts',(28.1535242688254,20.2428973867132,37.5767024843919));
#63889=CARTESIAN_POINT('Ctrl Pts',(28.1314413967557,20.2991668585337,37.5725806125634));
#63890=CARTESIAN_POINT('Ctrl Pts',(28.1066877680849,20.3717788313914,37.5674989615502));
#63891=CARTESIAN_POINT('Ctrl Pts',(28.1016192791251,20.3872653722515,37.5664285907207));
#63892=CARTESIAN_POINT('Ctrl Pts',(28.0936671755941,20.4126090415539,37.5647006959001));
#63893=CARTESIAN_POINT('Ctrl Pts',(28.0906690032086,20.4224291095546,37.5640369438432));
#63894=CARTESIAN_POINT('Ctrl Pts',(28.085144516901,20.4410370008445,37.5627906628838));
#63895=CARTESIAN_POINT('Ctrl Pts',(28.0826025680451,20.4498198008244,37.5622072057508));
#63896=CARTESIAN_POINT('Ctrl Pts',(28.075859475613,20.4737326177067,37.560630812762));
#63897=CARTESIAN_POINT('Ctrl Pts',(28.0717763477665,20.488895608791,37.5596444211528));
#63898=CARTESIAN_POINT('Ctrl Pts',(28.0557786940539,20.5512264552559,37.5556375483807));
#63899=CARTESIAN_POINT('Ctrl Pts',(28.0454116318397,20.5987777744408,37.5526924761184));
#63900=CARTESIAN_POINT('Ctrl Pts',(28.015908250974,20.7627047278765,37.542773362769));
#63901=CARTESIAN_POINT('Ctrl Pts',(28.0053517652046,20.8803735445233,37.53603925341));
#63902=CARTESIAN_POINT('Ctrl Pts',(28.0051704120784,21.0920338424653,37.5236848978873));
#63903=CARTESIAN_POINT('Ctrl Pts',(28.0116981263056,21.1856559230649,37.5181369904141));
#63904=CARTESIAN_POINT('Ctrl Pts',(28.0286140522835,21.3056441447409,37.5107016416399));
#63905=CARTESIAN_POINT('Ctrl Pts',(28.0330060091454,21.3327392735753,37.509001492195));
#63906=CARTESIAN_POINT('Ctrl Pts',(28.0412195766724,21.3775373118615,37.5061509399333));
#63907=CARTESIAN_POINT('Ctrl Pts',(28.0447257906238,21.395294700256,37.5050106163347));
#63908=CARTESIAN_POINT('Ctrl Pts',(28.0521438325434,21.4303466553135,37.5027378938312));
#63909=CARTESIAN_POINT('Ctrl Pts',(28.0560455760191,21.4476416611827,37.5016059131602));
#63910=CARTESIAN_POINT('Ctrl Pts',(28.0661199464601,21.4896792036977,37.4988275782407));
#63911=CARTESIAN_POINT('Ctrl Pts',(28.0725373569274,21.5143592553,37.4971734902399));
#63912=CARTESIAN_POINT('Ctrl Pts',(28.0998188235944,21.6115855383253,37.4905629932941));
#63913=CARTESIAN_POINT('Ctrl Pts',(28.1243182002619,21.6830379331354,37.4854919333402));
#63914=CARTESIAN_POINT('Ctrl Pts',(28.2194466528817,21.9164226484134,37.4682375698175));
#63915=CARTESIAN_POINT('Ctrl Pts',(28.3074946182132,22.0703372899519,37.4556272724443));
#63916=CARTESIAN_POINT('Ctrl Pts',(28.4284591182776,22.2287412040328,37.4422800204101));
#63917=CARTESIAN_POINT('Ctrl Pts',(28.4425833904532,22.2465950818086,37.440771077684));
#63918=CARTESIAN_POINT('Ctrl Pts',(28.4643684060945,22.2731841754553,37.4385217344837));
#63919=CARTESIAN_POINT('Ctrl Pts',(28.4718044159157,22.2821000778645,37.4377671109173));
#63920=CARTESIAN_POINT('Ctrl Pts',(28.4855675982577,22.2983124870437,37.4363950492201));
#63921=CARTESIAN_POINT('Ctrl Pts',(28.4918702711509,22.3056284079557,37.4357760355773));
#63922=CARTESIAN_POINT('Ctrl Pts',(28.5069121987213,22.322834283231,37.4343201382086));
#63923=CARTESIAN_POINT('Ctrl Pts',(28.5156968254845,22.3326836953688,37.4334865666578));
#63924=CARTESIAN_POINT('Ctrl Pts',(28.5460175038624,22.3660077819022,37.4306628171376));
#63925=CARTESIAN_POINT('Ctrl Pts',(28.5680188889317,22.3890546108835,37.4287039139942));
#63926=CARTESIAN_POINT('Ctrl Pts',(28.6256625093559,22.4466112426413,37.4237651933596));
#63927=CARTESIAN_POINT('Ctrl Pts',(28.6620578499049,22.4803374672231,37.4208258430704));
#63928=CARTESIAN_POINT('Ctrl Pts',(28.8013481942874,22.6000743104362,37.4100541646177));
#63929=CARTESIAN_POINT('Ctrl Pts',(28.9115212273816,22.6769563946035,37.4024218142213));
#63930=CARTESIAN_POINT('Ctrl Pts',(29.0285070711969,22.7421908769666,37.3944594262182));
#63931=CARTESIAN_POINT('',(28.0052505873043,21.0015307025596,37.3704548813502));
#63932=CARTESIAN_POINT('Ctrl Pts',(29.0285070491141,22.7421908646526,37.2352940441794));
#63933=CARTESIAN_POINT('Ctrl Pts',(28.9676750007528,22.7082692620487,37.2397348558595));
#63934=CARTESIAN_POINT('Ctrl Pts',(28.9085669082878,22.6711271905714,37.2441756675396));
#63935=CARTESIAN_POINT('Ctrl Pts',(28.8515391222872,22.6309706235439,37.2486164792197));
#63936=CARTESIAN_POINT('Ctrl Pts',(28.7945363606911,22.5908316776489,37.2530553422239));
#63937=CARTESIAN_POINT('Ctrl Pts',(28.7396124938189,22.5476811426052,37.2574942052282));
#63938=CARTESIAN_POINT('Ctrl Pts',(28.6870952912065,22.5017685534489,37.2619330682325));
#63939=CARTESIAN_POINT('Ctrl Pts',(28.6345832990225,22.4558605194525,37.2663714908405));
#63940=CARTESIAN_POINT('Ctrl Pts',(28.5844778645941,22.4071912985624,37.2708099134485));
#63941=CARTESIAN_POINT('Ctrl Pts',(28.5370726524019,22.3560498287856,37.2752483360566));
#63942=CARTESIAN_POINT('Ctrl Pts',(28.4896219666951,22.304859301484,37.2796910162275));
#63943=CARTESIAN_POINT('Ctrl Pts',(28.4448770119837,22.2511921468912,37.2841336963985));
#63944=CARTESIAN_POINT('Ctrl Pts',(28.4030929756531,22.1953725436413,37.2885763765695));
#63945=CARTESIAN_POINT('Ctrl Pts',(28.3612901010681,22.139527774228,37.2930210597145));
#63946=CARTESIAN_POINT('Ctrl Pts',(28.3224510779613,22.0815290297261,37.2974657428595));
#63947=CARTESIAN_POINT('Ctrl Pts',(28.2867876795183,22.0217294688173,37.3019104260045));
#63948=CARTESIAN_POINT('Ctrl Pts',(28.251057438419,21.9618178276898,37.3063634396632));
#63949=CARTESIAN_POINT('Ctrl Pts',(28.2185149452665,21.9000990595722,37.3108164533218));
#63950=CARTESIAN_POINT('Ctrl Pts',(28.189325692928,21.8369504861156,37.3152694669805));
#63951=CARTESIAN_POINT('Ctrl Pts',(28.1613490372183,21.7764252668444,37.3195374909968));
#63952=CARTESIAN_POINT('Ctrl Pts',(28.1364526001043,21.7145870758048,37.3238055150131));
#63953=CARTESIAN_POINT('Ctrl Pts',(28.1147390994969,21.6517813280038,37.3280735390294));
#63954=CARTESIAN_POINT('Ctrl Pts',(28.0881391268734,21.5748415842784,37.3333020521118));
#63955=CARTESIAN_POINT('Ctrl Pts',(28.0662290812613,21.4962022913531,37.3385305651942));
#63956=CARTESIAN_POINT('Ctrl Pts',(28.0491946728556,21.4163966115195,37.3437590782766));
#63957=CARTESIAN_POINT('Ctrl Pts',(28.0323305966141,21.3373889326406,37.3489353098868));
#63958=CARTESIAN_POINT('Ctrl Pts',(28.0202452166158,21.2572382007314,37.354111541497));
#63959=CARTESIAN_POINT('Ctrl Pts',(28.0130723499623,21.1764825090925,37.3592877731071));
#63960=CARTESIAN_POINT('Ctrl Pts',(28.0079141457985,21.1184088873482,37.3630101425215));
#63961=CARTESIAN_POINT('Ctrl Pts',(28.0052954721807,21.0600228505839,37.3667325119358));
#63962=CARTESIAN_POINT('Ctrl Pts',(28.0052505873043,21.0015307025596,37.3704548813502));
#63963=CARTESIAN_POINT('Ctrl Pts',(28.0052505873038,21.0015307018519,37.3704548813952));
#63964=CARTESIAN_POINT('Ctrl Pts',(28.0051970875676,20.9318119861274,37.3748916959726));
#63965=CARTESIAN_POINT('Ctrl Pts',(28.0088030231443,20.8620506010969,37.37932851055));
#63966=CARTESIAN_POINT('Ctrl Pts',(28.0160551888972,20.7926583761076,37.3837653251274));
#63967=CARTESIAN_POINT('Ctrl Pts',(28.0233061729072,20.7232774586061,37.3882014167242));
#63968=CARTESIAN_POINT('Ctrl Pts',(28.0342021560973,20.6542660682087,37.3926375083211));
#63969=CARTESIAN_POINT('Ctrl Pts',(28.0486780446787,20.5860311736604,37.397073599918));
#63970=CARTESIAN_POINT('Ctrl Pts',(28.0631564854405,20.5177842489169,37.4015104736227));
#63971=CARTESIAN_POINT('Ctrl Pts',(28.0812159804205,20.4503145698138,37.4059473473275));
#63972=CARTESIAN_POINT('Ctrl Pts',(28.1027406541306,20.3840174215034,37.4103842210322));
#63973=CARTESIAN_POINT('Ctrl Pts',(28.1242909534436,20.3176413449629,37.4148263769338));
#63974=CARTESIAN_POINT('Ctrl Pts',(28.149314510197,20.2524410501686,37.4192685328354));
#63975=CARTESIAN_POINT('Ctrl Pts',(28.1776463422157,20.1887942872118,37.423710688737));
#63976=CARTESIAN_POINT('Ctrl Pts',(28.2059978569738,20.1251033074656,37.4281559307008));
#63977=CARTESIAN_POINT('Ctrl Pts',(28.2376619969177,20.062968442017,37.4326011726647));
#63978=CARTESIAN_POINT('Ctrl Pts',(28.2724279088081,20.0027426449331,37.4370464146285));
#63979=CARTESIAN_POINT('Ctrl Pts',(28.3072551088155,19.9424106770199,37.4414994930187));
#63980=CARTESIAN_POINT('Ctrl Pts',(28.3451947235225,19.88399490096,37.445952571409));
#63981=CARTESIAN_POINT('Ctrl Pts',(28.3859932468674,19.8278183744222,37.4504056497992));
#63982=CARTESIAN_POINT('Ctrl Pts',(28.4000373498548,19.8084806911069,37.4519385359528));
#63983=CARTESIAN_POINT('Ctrl Pts',(28.4144198789395,19.7894080447954,37.4534714221064));
#63984=CARTESIAN_POINT('Ctrl Pts',(28.4291294646721,19.7706126225886,37.4550043082601));
#63985=CARTESIAN_POINT('Ctrl Pts',(28.4718807834891,19.7159864011795,37.4594594238463));
#63986=CARTESIAN_POINT('Ctrl Pts',(28.5175690562093,19.6634852813327,37.4639145394325));
#63987=CARTESIAN_POINT('Ctrl Pts',(28.565955127025,19.6134420802599,37.4683696550187));
#63988=CARTESIAN_POINT('Ctrl Pts',(28.6142687478787,19.5634738104215,37.4728180998224));
#63989=CARTESIAN_POINT('Ctrl Pts',(28.6652718119006,19.5159565035892,37.4772665446261));
#63990=CARTESIAN_POINT('Ctrl Pts',(28.7186843478964,19.4711907371506,37.4817149894298));
#63991=CARTESIAN_POINT('Ctrl Pts',(28.7720342547224,19.4264774610633,37.4861582181845));
#63992=CARTESIAN_POINT('Ctrl Pts',(28.8277876489463,19.3845096301406,37.4906014469392));
#63993=CARTESIAN_POINT('Ctrl Pts',(28.8856283642533,19.3455504178298,37.4950446756939));
#63994=CARTESIAN_POINT('Ctrl Pts',(28.943432830965,19.3066156211354,37.4994851198911));
#63995=CARTESIAN_POINT('Ctrl Pts',(29.0033216188074,19.2706859752787,37.5039255640882));
#63996=CARTESIAN_POINT('Ctrl Pts',(29.0649474143262,19.2379829102631,37.5083660082854));
#63997=CARTESIAN_POINT('Ctrl Pts',(29.1265555001082,19.2052892433036,37.5128051764082));
#63998=CARTESIAN_POINT('Ctrl Pts',(29.1898991706166,19.1758205456311,37.5172443445309));
#63999=CARTESIAN_POINT('Ctrl Pts',(29.2546057525191,19.1497527250872,37.5216835126537));
#64000=CARTESIAN_POINT('Ctrl Pts',(29.319315694997,19.1236835506953,37.5261229113274));
#64001=CARTESIAN_POINT('Ctrl Pts',(29.3853882346695,19.1010157846872,37.5305623100011));
#64002=CARTESIAN_POINT('Ctrl Pts',(29.4524315863539,19.081876856175,37.5350017086747));
#64003=CARTESIAN_POINT('Ctrl Pts',(29.5195458045972,19.0627176973197,37.5394457999077));
#64004=CARTESIAN_POINT('Ctrl Pts',(29.587632411586,19.0470949553679,37.5438898911408));
#64005=CARTESIAN_POINT('Ctrl Pts',(29.6562862907838,19.0350856383555,37.5483339823738));
#64006=CARTESIAN_POINT('Ctrl Pts',(29.7249803935313,19.0230692852169,37.5527806773508));
#64007=CARTESIAN_POINT('Ctrl Pts',(29.7942419441702,19.0146706297299,37.5572273723278));
#64008=CARTESIAN_POINT('Ctrl Pts',(29.8636602826768,19.0099148148935,37.5616740673048));
#64009=CARTESIAN_POINT('Ctrl Pts',(29.9331988788893,19.0051507612633,37.5661284655681));
#64010=CARTESIAN_POINT('Ctrl Pts',(30.0028943160324,19.0040421529423,37.5705828638314));
#64011=CARTESIAN_POINT('Ctrl Pts',(30.0723363214446,19.0065620102196,37.5750372620947));
#64012=CARTESIAN_POINT('Ctrl Pts',(30.1081809036425,19.0078627104336,37.5773365338934));
#64013=CARTESIAN_POINT('Ctrl Pts',(30.1439580479989,19.010129337037,37.5796358056922));
#64014=CARTESIAN_POINT('Ctrl Pts',(30.1796122418824,19.0133528232054,37.5819350774909));
#64015=CARTESIAN_POINT('Ctrl Pts',(30.2486942549679,19.0195985096005,37.5863900463791));
#64016=CARTESIAN_POINT('Ctrl Pts',(30.3175862033279,19.02946409394,37.5908450152674));
#64017=CARTESIAN_POINT('Ctrl Pts',(30.3858787744911,19.0429294509657,37.5952999841557));
#64018=CARTESIAN_POINT('Ctrl Pts',(30.4540690398109,19.0563746361824,37.5997482792675));
#64019=CARTESIAN_POINT('Ctrl Pts',(30.5216612338784,19.073408796921,37.6041965743794));
#64020=CARTESIAN_POINT('Ctrl Pts',(30.5882509561794,19.0939600279495,37.6086448694913));
#64021=CARTESIAN_POINT('Ctrl Pts',(30.6547625402009,19.1144871435775,37.6130879448468));
#64022=CARTESIAN_POINT('Ctrl Pts',(30.7202735235098,19.1385229889579,37.6175310202023));
#64023=CARTESIAN_POINT('Ctrl Pts',(30.7843912635446,19.1659449549768,37.6219740955578));
#64024=CARTESIAN_POINT('Ctrl Pts',(30.8484687879124,19.1933497215023,37.6264143841457));
#64025=CARTESIAN_POINT('Ctrl Pts',(30.9111543537307,19.2241362034049,37.6308546727336));
#64026=CARTESIAN_POINT('Ctrl Pts',(30.9720734615318,19.2581329706646,37.6352949613216));
#64027=CARTESIAN_POINT('Ctrl Pts',(31.0329750349667,19.292119952624,37.6397339718598));
#64028=CARTESIAN_POINT('Ctrl Pts',(31.0921107326892,19.3293151472234,37.6441729823981));
#64029=CARTESIAN_POINT('Ctrl Pts',(31.1491305142306,19.3695011120015,37.6486119929363));
#64030=CARTESIAN_POINT('Ctrl Pts',(31.2061532348479,19.4096891481592,37.6530512322827));
#64031=CARTESIAN_POINT('Ctrl Pts',(31.2610594241858,19.4528679767003,37.6574904716291));
#64032=CARTESIAN_POINT('Ctrl Pts',(31.3135293763748,19.4987777846367,37.6619297109755));
#64033=CARTESIAN_POINT('Ctrl Pts',(31.3660547742256,19.5447361060475,37.6663736413222));
#64034=CARTESIAN_POINT('Ctrl Pts',(31.4161384277138,19.5934308438923,37.670817571669));
#64035=CARTESIAN_POINT('Ctrl Pts',(31.4634957355631,19.6445636147393,37.6752615020157));
#64036=CARTESIAN_POINT('Ctrl Pts',(31.5108807785624,19.6957263318635,37.6797080349824));
#64037=CARTESIAN_POINT('Ctrl Pts',(31.5555359845813,19.7493295479291,37.6841545679491));
#64038=CARTESIAN_POINT('Ctrl Pts',(31.597217298084,19.8050420655098,37.6886011009158));
#64039=CARTESIAN_POINT('Ctrl Pts',(31.6389708210197,19.8608511004255,37.6930553371335));
#64040=CARTESIAN_POINT('Ctrl Pts',(31.6777398953439,19.9187763244634,37.6975095733513));
#64041=CARTESIAN_POINT('Ctrl Pts',(31.7133244478229,19.9784585671681,37.7019638095691));
#64042=CARTESIAN_POINT('Ctrl Pts',(31.7317043968018,20.0092853304526,37.70426448862));
#64043=CARTESIAN_POINT('Ctrl Pts',(31.7492355156924,20.0405804562712,37.7065651676708));
#64044=CARTESIAN_POINT('Ctrl Pts',(31.7658952391199,20.0722923052202,37.7088658467217));
#64045=CARTESIAN_POINT('Ctrl Pts',(31.7981553081255,20.1336994732228,37.7133209065709));
#64046=CARTESIAN_POINT('Ctrl Pts',(31.8272720354534,20.1969122905168,37.71777596642));
#64047=CARTESIAN_POINT('Ctrl Pts',(31.8530401133341,20.2615760696764,37.7222310262692));
#64048=CARTESIAN_POINT('Ctrl Pts',(31.8787695978004,20.326143000478,37.7266794136777));
#64049=CARTESIAN_POINT('Ctrl Pts',(31.9011602075757,20.3921561290545,37.7311278010862));
#64050=CARTESIAN_POINT('Ctrl Pts',(31.9200527874283,20.4592367838055,37.7355761884947));
#64051=CARTESIAN_POINT('Ctrl Pts',(31.9389232051245,20.5262387488294,37.7400193576716));
#64052=CARTESIAN_POINT('Ctrl Pts',(31.9543036108986,20.5943052840939,37.7444625268485));
#64053=CARTESIAN_POINT('Ctrl Pts',(31.9660838146113,20.6630400670353,37.7489056960254));
#64054=CARTESIAN_POINT('Ctrl Pts',(31.9778566321101,20.7317317531155,37.7533460793254));
#64055=CARTESIAN_POINT('Ctrl Pts',(31.9860336432338,20.8010903745115,37.7577864626254));
#64056=CARTESIAN_POINT('Ctrl Pts',(31.9905555078152,20.8707083420851,37.7622268459254));
#64057=CARTESIAN_POINT('Ctrl Pts',(31.9950760716551,20.9403062836303,37.7666659519224));
#64058=CARTESIAN_POINT('Ctrl Pts',(31.9959435445788,21.0101629352344,37.7711050579193));
#64059=CARTESIAN_POINT('Ctrl Pts',(31.9931505064754,21.0798662697074,37.7755441639163));
#64060=CARTESIAN_POINT('Ctrl Pts',(31.9903573240286,21.1495732064262,37.7799834993248));
#64061=CARTESIAN_POINT('Ctrl Pts',(31.9839032769814,21.2191263214869,37.7844228347333));
#64062=CARTESIAN_POINT('Ctrl Pts',(31.9738329964775,21.2881160608448,37.7888621701419));
#64063=CARTESIAN_POINT('Ctrl Pts',(31.9637520742299,21.3571787049365,37.7933061968069));
#64064=CARTESIAN_POINT('Ctrl Pts',(31.9500473621252,21.4256762999692,37.797750223472));
#64065=CARTESIAN_POINT('Ctrl Pts',(31.9328149407851,21.4932078336542,37.802194250137));
#64066=CARTESIAN_POINT('Ctrl Pts',(31.9155724262556,21.5607789211862,37.8066408797098));
#64067=CARTESIAN_POINT('Ctrl Pts',(31.8947982356396,21.6273823539259,37.8110875092826));
#64068=CARTESIAN_POINT('Ctrl Pts',(31.8706380187518,21.6926333556077,37.8155341388554));
#64069=CARTESIAN_POINT('Ctrl Pts',(31.8464359503377,21.7579973883117,37.8199884711005));
#64070=CARTESIAN_POINT('Ctrl Pts',(31.818836341289,21.8220038643766,37.8244428033456));
#64071=CARTESIAN_POINT('Ctrl Pts',(31.7880322108752,21.8842897575867,37.8288971355908));
#64072=CARTESIAN_POINT('Ctrl Pts',(31.7721276576484,21.916448734014,37.831196962378));
#64073=CARTESIAN_POINT('Ctrl Pts',(31.755369586707,21.9481494680602,37.8334967891652));
#64074=CARTESIAN_POINT('Ctrl Pts',(31.737789077975,21.9793450275418,37.8357966159524));
#64075=CARTESIAN_POINT('Ctrl Pts',(31.7037334727485,22.0397746587157,37.8402516629791));
#64076=CARTESIAN_POINT('Ctrl Pts',(31.6664549874929,22.0985448139774,37.8447067100058));
#64077=CARTESIAN_POINT('Ctrl Pts',(31.6261400249968,22.1552905182695,37.8491617570326));
#64078=CARTESIAN_POINT('Ctrl Pts',(31.5858854431001,22.2119512332815,37.8536101316381));
#64079=CARTESIAN_POINT('Ctrl Pts',(31.5426036914941,22.2665931196839,37.8580585062436));
#64080=CARTESIAN_POINT('Ctrl Pts',(31.4965263710486,22.3188769401488,37.8625068808491));
#64081=CARTESIAN_POINT('Ctrl Pts',(31.4505031013113,22.37109942941,37.8669500373171));
#64082=CARTESIAN_POINT('Ctrl Pts',(31.4016910979545,22.4209689813424,37.871393193785));
#64083=CARTESIAN_POINT('Ctrl Pts',(31.3503633682412,22.4681778966502,37.8758363502529));
#64084=CARTESIAN_POINT('Ctrl Pts',(31.2990678204587,22.5153572124793,37.8802767209098));
#64085=CARTESIAN_POINT('Ctrl Pts',(31.2452600347722,22.5598788706026,37.8847170915668));
#64086=CARTESIAN_POINT('Ctrl Pts',(31.1892500865086,22.6014717588017,37.8891574622237));
#64087=CARTESIAN_POINT('Ctrl Pts',(31.1332562488101,22.6430526833237,37.8935965556632));
#64088=CARTESIAN_POINT('Ctrl Pts',(31.0750618986584,22.6817062187649,37.8980356491027));
#64089=CARTESIAN_POINT('Ctrl Pts',(31.0150090257792,22.7172024458656,37.9024747425423));
#64090=CARTESIAN_POINT('Ctrl Pts',(30.954953047952,22.752700508248,37.9069140654988));
#64091=CARTESIAN_POINT('Ctrl Pts',(30.8930387790592,22.7850406913028,37.9113533884553));
#64092=CARTESIAN_POINT('Ctrl Pts',(30.8296343904043,22.8140381310101,37.9157927114118));
#64093=CARTESIAN_POINT('Ctrl Pts',(30.7661629955968,22.8430662153921,37.9202367258724));
#64094=CARTESIAN_POINT('Ctrl Pts',(30.7011987837915,22.8687443017592,37.9246807403331));
#64095=CARTESIAN_POINT('Ctrl Pts',(30.6351306847448,22.8909353706025,37.9291247547937));
#64096=CARTESIAN_POINT('Ctrl Pts',(30.5690238870659,22.9131394376102,37.9335713722849));
#64097=CARTESIAN_POINT('Ctrl Pts',(30.5018123866641,22.931852290481,37.9380179897762));
#64098=CARTESIAN_POINT('Ctrl Pts',(30.4338983892305,22.9469873523788,37.9424646072674));
#64099=CARTESIAN_POINT('Ctrl Pts',(30.3658667425723,22.9621486331471,37.9469189277524));
#64100=CARTESIAN_POINT('Ctrl Pts',(30.2971306521092,22.9737196700521,37.9513732482374));
#64101=CARTESIAN_POINT('Ctrl Pts',(30.2280997745616,22.9816654751357,37.9558275687223));
#64102=CARTESIAN_POINT('Ctrl Pts',(30.1924564490298,22.9857682031796,37.9581275075426));
#64103=CARTESIAN_POINT('Ctrl Pts',(30.1567345731691,22.9889052759571,37.9604274463629));
#64104=CARTESIAN_POINT('Ctrl Pts',(30.1209904421614,22.9910773152757,37.9627273851832));
#64105=CARTESIAN_POINT('Ctrl Pts',(30.0517594247995,22.9952842294611,37.9671820215084));
#64106=CARTESIAN_POINT('Ctrl Pts',(29.9821723908552,22.99588431811,37.9716366578335));
#64107=CARTESIAN_POINT('Ctrl Pts',(29.9126369316935,22.9928359834156,37.9760912941587));
#64108=CARTESIAN_POINT('Ctrl Pts',(29.8432006204944,22.9897919952256,37.9805395787876));
#64109=CARTESIAN_POINT('Ctrl Pts',(29.7738162228982,22.9831099262811,37.9849878634165));
#64110=CARTESIAN_POINT('Ctrl Pts',(29.7048943424097,22.9728000946265,37.9894361480454));
#64111=CARTESIAN_POINT('Ctrl Pts',(29.6360532006688,22.9625023404556,37.9938792217177));
#64112=CARTESIAN_POINT('Ctrl Pts',(29.5676739814763,22.9485853362069,37.99832229539));
#64113=CARTESIAN_POINT('Ctrl Pts',(29.5001632856801,22.9311112918519,38.0027653690623));
#64114=CARTESIAN_POINT('Ctrl Pts',(29.4326984427486,22.9136491157643,38.0072054250252));
#64115=CARTESIAN_POINT('Ctrl Pts',(29.3661014246855,22.8926348178249,38.0116454809882));
#64116=CARTESIAN_POINT('Ctrl Pts',(29.30076817101,22.868181578923,38.0160855369512));
#64117=CARTESIAN_POINT('Ctrl Pts',(29.2354480376213,22.8437332507441,38.0205247012578));
#64118=CARTESIAN_POINT('Ctrl Pts',(29.1713916246071,22.8158475190688,38.0249638655645));
#64119=CARTESIAN_POINT('Ctrl Pts',(29.1089777080109,22.7846867617816,38.0294030298711));
#64120=CARTESIAN_POINT('Ctrl Pts',(29.08183381087,22.7711349060936,38.0313336284604));
#64121=CARTESIAN_POINT('Ctrl Pts',(29.0550003164454,22.7569642301779,38.0332642270497));
#64122=CARTESIAN_POINT('Ctrl Pts',(29.0285070491141,22.7421908646526,38.0351948256389));
#64123=CARTESIAN_POINT('Origin',(30.,21.,34.5704548813952));
#64124=CARTESIAN_POINT('',(29.0285070786203,22.742190881106,38.9934724864331));
#64125=CARTESIAN_POINT('',(29.0285070491141,22.7421908646526,38.8351573073316));
#64126=CARTESIAN_POINT('',(29.0285070491141,22.7421908646526,34.5704548813952));
#64127=CARTESIAN_POINT('',(28.0052500005311,20.9999539693013,38.3266423355102));
#64128=CARTESIAN_POINT('Ctrl Pts',(29.0285070786203,22.742190881106,38.9934724864331));
#64129=CARTESIAN_POINT('Ctrl Pts',(29.1261719400268,22.7966514586196,38.9856837164118));
#64130=CARTESIAN_POINT('Ctrl Pts',(29.2282644481304,22.8428150981434,38.9778312441651));
#64131=CARTESIAN_POINT('Ctrl Pts',(29.3602290880631,22.8895798912096,38.9683904123005));
#64132=CARTESIAN_POINT('Ctrl Pts',(29.3869429891265,22.8984152003077,38.9665147657409));
#64133=CARTESIAN_POINT('Ctrl Pts',(29.4257458574274,22.9103442054419,38.963849789298));
#64134=CARTESIAN_POINT('Ctrl Pts',(29.4376897690429,22.9138939435479,38.9630375166519));
#64135=CARTESIAN_POINT('Ctrl Pts',(29.4589957458048,22.9200094177528,38.9616037720753));
#64136=CARTESIAN_POINT('Ctrl Pts',(29.4683443248162,22.9226190528019,38.9609799194553));
#64137=CARTESIAN_POINT('Ctrl Pts',(29.4893403217739,22.9283151765138,38.9595905535825));
#64138=CARTESIAN_POINT('Ctrl Pts',(29.5009971120419,22.9313645078824,38.9588271207487));
#64139=CARTESIAN_POINT('Ctrl Pts',(29.5369928297828,22.9404330688693,38.9564920138923));
#64140=CARTESIAN_POINT('Ctrl Pts',(29.5614191016366,22.9460994483439,38.9549387609837));
#64141=CARTESIAN_POINT('Ctrl Pts',(29.6203867865655,22.9586119770588,38.9512497979312));
#64142=CARTESIAN_POINT('Ctrl Pts',(29.6550159104204,22.9650072034573,38.9491330140999));
#64143=CARTESIAN_POINT('Ctrl Pts',(29.8039952556494,22.9884601893047,38.9401692216269));
#64144=CARTESIAN_POINT('Ctrl Pts',(29.9195438375984,22.9964771930964,38.9335633735301));
#64145=CARTESIAN_POINT('Ctrl Pts',(30.1283304682209,22.9927984988894,38.9213727239291));
#64146=CARTESIAN_POINT('Ctrl Pts',(30.221280588503,22.9846275855641,38.9158552584771));
#64147=CARTESIAN_POINT('Ctrl Pts',(30.3403974775534,22.9656828965603,38.9084540736092));
#64148=CARTESIAN_POINT('Ctrl Pts',(30.3673892531734,22.9608173590714,38.9067552395224));
#64149=CARTESIAN_POINT('Ctrl Pts',(30.4120098705479,22.9518204024578,38.9039062719728));
#64150=CARTESIAN_POINT('Ctrl Pts',(30.4296985932853,22.9480025926766,38.902766193145));
#64151=CARTESIAN_POINT('Ctrl Pts',(30.4646137380158,22.939968065006,38.9004934764392));
#64152=CARTESIAN_POINT('Ctrl Pts',(30.4818407297721,22.935761218852,38.899361250248));
#64153=CARTESIAN_POINT('Ctrl Pts',(30.5237157697067,22.9249416967329,38.8965814295517));
#64154=CARTESIAN_POINT('Ctrl Pts',(30.5482968634414,22.9180847719852,38.8949260820902));
#64155=CARTESIAN_POINT('Ctrl Pts',(30.645229076629,22.8890299042917,38.8883015259722));
#64156=CARTESIAN_POINT('Ctrl Pts',(30.7164157546297,22.8631963526262,38.8832170273903));
#64157=CARTESIAN_POINT('Ctrl Pts',(30.9430063740048,22.7660588994322,38.8663369730759));
#64158=CARTESIAN_POINT('Ctrl Pts',(31.0907425043475,22.6788393435921,38.854152321631));
#64159=CARTESIAN_POINT('Ctrl Pts',(31.2462669994359,22.5577340755355,38.8408904933856));
#64160=CARTESIAN_POINT('Ctrl Pts',(31.2666629325392,22.5411950083032,38.8391433092643));
#64161=CARTESIAN_POINT('Ctrl Pts',(31.2960986777053,22.5163463262876,38.8366169998726));
#64162=CARTESIAN_POINT('Ctrl Pts',(31.3053970191235,22.508348966498,38.8358182611524));
#64163=CARTESIAN_POINT('Ctrl Pts',(31.3219161645369,22.4938739209478,38.8343988858292));
#64164=CARTESIAN_POINT('Ctrl Pts',(31.3291641727891,22.4874287374167,38.8337760659393));
#64165=CARTESIAN_POINT('Ctrl Pts',(31.3455957223273,22.4726011988472,38.8323638651608));
#64166=CARTESIAN_POINT('Ctrl Pts',(31.3547482732204,22.4641855326901,38.8315769593707));
#64167=CARTESIAN_POINT('Ctrl Pts',(31.3836785814484,22.4370809070461,38.829086368869));
#64168=CARTESIAN_POINT('Ctrl Pts',(31.4031537338011,22.4180718302162,38.827404820595));
#64169=CARTESIAN_POINT('Ctrl Pts',(31.4499145161824,22.3705231906095,38.8233364773896));
#64170=CARTESIAN_POINT('Ctrl Pts',(31.4767541071958,22.3415601268839,38.8209742265413));
#64171=CARTESIAN_POINT('Ctrl Pts',(31.6050803646051,22.1945594420947,38.8094310299026));
#64172=CARTESIAN_POINT('Ctrl Pts',(31.6933668120287,22.0657237407482,38.8006371880744));
#64173=CARTESIAN_POINT('Ctrl Pts',(31.7911444298746,21.8796604628152,38.7881094478695));
#64174=CARTESIAN_POINT('Ctrl Pts',(31.8145185199592,21.8303750261141,38.784810838852));
#64175=CARTESIAN_POINT('Ctrl Pts',(31.8441510696838,21.7606481263319,38.7801328320607));
#64176=CARTESIAN_POINT('Ctrl Pts',(31.8521458990659,21.7409684572614,38.7788114243597));
#64177=CARTESIAN_POINT('Ctrl Pts',(31.8661548937171,21.704840444289,38.7763814842166));
#64178=CARTESIAN_POINT('Ctrl Pts',(31.8722696853947,21.6884332449827,38.7752764385417));
#64179=CARTESIAN_POINT('Ctrl Pts',(31.8842717352779,21.6548862181166,38.7730128999078));
#64180=CARTESIAN_POINT('Ctrl Pts',(31.8901429752788,21.6377424466212,38.7718539970609));
#64181=CARTESIAN_POINT('Ctrl Pts',(31.9043509182818,21.5943352017041,38.7689132355796));
#64182=CARTESIAN_POINT('Ctrl Pts',(31.9123782926977,21.5679752561361,38.767121449598));
#64183=CARTESIAN_POINT('Ctrl Pts',(31.9482511970124,21.4407802223936,38.7584430581908));
#64184=CARTESIAN_POINT('Ctrl Pts',(31.9686781336224,21.3380392717237,38.7513237551309));
#64185=CARTESIAN_POINT('Ctrl Pts',(31.9980312035058,21.0897428861422,38.7339927097622));
#64186=CARTESIAN_POINT('Ctrl Pts',(31.9992584473795,20.9438644916594,38.7236945439104));
#64187=CARTESIAN_POINT('Ctrl Pts',(31.98250342374,20.7783103372444,38.7125770837495));
#64188=CARTESIAN_POINT('Ctrl Pts',(31.9800666540482,20.7575082274679,38.7111913246484));
#64189=CARTESIAN_POINT('Ctrl Pts',(31.9758020570041,20.7254766387862,38.7090786282242));
#64190=CARTESIAN_POINT('Ctrl Pts',(31.9742051154172,20.7142185770148,38.708340130257));
#64191=CARTESIAN_POINT('Ctrl Pts',(31.9710534470934,20.6932887154148,38.7069754998225));
#64192=CARTESIAN_POINT('Ctrl Pts',(31.9695236892128,20.683614246275,38.7063481313656));
#64193=CARTESIAN_POINT('Ctrl Pts',(31.9656907574216,20.6604799650858,38.7048555578994));
#64194=CARTESIAN_POINT('Ctrl Pts',(31.9633205472482,20.647031925721,38.7039940500255));
#64195=CARTESIAN_POINT('Ctrl Pts',(31.9543948070726,20.5992641201194,38.7009523909232));
#64196=CARTESIAN_POINT('Ctrl Pts',(31.9470755800144,20.5650915952059,38.6988103836295));
#64197=CARTESIAN_POINT('Ctrl Pts',(31.925449041231,20.4756625738358,38.6932527917642));
#64198=CARTESIAN_POINT('Ctrl Pts',(31.9096615288459,20.4207958986623,38.6898916058998));
#64199=CARTESIAN_POINT('Ctrl Pts',(31.8450906662349,20.227941958694,38.6780186853723));
#64200=CARTESIAN_POINT('Ctrl Pts',(31.7835203951718,20.0947450518531,38.6696736552688));
#64201=CARTESIAN_POINT('Ctrl Pts',(31.6859945508057,19.9331100106157,38.658293652308));
#64202=CARTESIAN_POINT('Ctrl Pts',(31.662895341532,19.8974526900899,38.6556992826264));
#64203=CARTESIAN_POINT('Ctrl Pts',(31.6266835933433,19.8452834013188,38.6517580681359));
#64204=CARTESIAN_POINT('Ctrl Pts',(31.6144182797286,19.8281964751232,38.6504428912696));
#64205=CARTESIAN_POINT('Ctrl Pts',(31.5916747503448,19.7975472375871,38.6480373200431));
#64206=CARTESIAN_POINT('Ctrl Pts',(31.5812874656464,19.7839197897455,38.646950535793));
#64207=CARTESIAN_POINT('Ctrl Pts',(31.5583179049367,19.7545771439819,38.6445717443706));
#64208=CARTESIAN_POINT('Ctrl Pts',(31.5456708000475,19.7389153431565,38.6432772203316));
#64209=CARTESIAN_POINT('Ctrl Pts',(31.5087166554658,19.6945435369297,38.6395361472075));
#64210=CARTESIAN_POINT('Ctrl Pts',(31.4838327720682,19.6663274343909,38.6370663980428));
#64211=CARTESIAN_POINT('Ctrl Pts',(31.3841324134644,19.5595221473438,38.6273518474158));
#64212=CARTESIAN_POINT('Ctrl Pts',(31.3037597022464,19.4863937264061,38.6198826459773));
#64213=CARTESIAN_POINT('Ctrl Pts',(31.1196987106189,19.344505669233,38.6036959190505));
#64214=CARTESIAN_POINT('Ctrl Pts',(31.0147014430383,19.2781487132412,38.5949847780099));
#64215=CARTESIAN_POINT('Ctrl Pts',(30.8860615123536,19.2127290350888,38.5853512654273));
#64216=CARTESIAN_POINT('Ctrl Pts',(30.8677631763936,19.2037734965193,38.5840043557759));
#64217=CARTESIAN_POINT('Ctrl Pts',(30.8391528571472,19.1903103704863,38.5819380436388));
#64218=CARTESIAN_POINT('Ctrl Pts',(30.8289350472629,19.1856073261418,38.5812078177547));
#64219=CARTESIAN_POINT('Ctrl Pts',(30.8097174925182,19.1769581208796,38.5798495960728));
#64220=CARTESIAN_POINT('Ctrl Pts',(30.8007279774588,19.1729918389495,38.5792205009467));
#64221=CARTESIAN_POINT('Ctrl Pts',(30.7789652853323,19.1635813618888,38.5777119564451));
#64222=CARTESIAN_POINT('Ctrl Pts',(30.7661639816944,19.1582038361249,38.5768364330705));
#64223=CARTESIAN_POINT('Ctrl Pts',(30.7194291868712,19.1391432530707,38.5736792579904));
#64224=CARTESIAN_POINT('Ctrl Pts',(30.6851751105106,19.1262599897052,38.5714396845317));
#64225=CARTESIAN_POINT('Ctrl Pts',(30.5926001924708,19.0943203652585,38.5655353622074));
#64226=CARTESIAN_POINT('Ctrl Pts',(30.5337210479095,19.0769990560148,38.5619337703739));
#64227=CARTESIAN_POINT('Ctrl Pts',(30.3162492490716,19.0237828458139,38.5488891576929));
#64228=CARTESIAN_POINT('Ctrl Pts',(30.1542500927719,19.004592607178,38.539605629667));
#64229=CARTESIAN_POINT('Ctrl Pts',(29.9623522782642,19.0053890748723,38.5278626789189));
#64230=CARTESIAN_POINT('Ctrl Pts',(29.9329911836527,19.0061595414374,38.5260474684379));
#64231=CARTESIAN_POINT('Ctrl Pts',(29.8851966015945,19.0084705885994,38.5230570271447));
#64232=CARTESIAN_POINT('Ctrl Pts',(29.8667481005039,19.0096198576252,38.5218940835576));
#64233=CARTESIAN_POINT('Ctrl Pts',(29.8308768702242,19.0123554349897,38.5196147760501));
#64234=CARTESIAN_POINT('Ctrl Pts',(29.8134537489871,19.013914902641,38.5184993582715));
#64235=CARTESIAN_POINT('Ctrl Pts',(29.7720490545758,19.0181704801742,38.5158278346409));
#64236=CARTESIAN_POINT('Ctrl Pts',(29.7480919427068,19.0210729864507,38.5142653752762));
#64237=CARTESIAN_POINT('Ctrl Pts',(29.6617427421401,19.0331279166417,38.5085708438117));
#64238=CARTESIAN_POINT('Ctrl Pts',(29.5997459870369,19.04480203505,38.5043615625894));
#64239=CARTESIAN_POINT('Ctrl Pts',(29.4375777013574,19.0833750114181,38.4930361402285));
#64240=CARTESIAN_POINT('Ctrl Pts',(29.3387740896111,19.1151797928065,38.4858030141114));
#64241=CARTESIAN_POINT('Ctrl Pts',(29.1601980044313,19.1884397718601,38.4723440741033));
#64242=CARTESIAN_POINT('Ctrl Pts',(29.0798650600122,19.2278904505962,38.4661343892974));
#64243=CARTESIAN_POINT('Ctrl Pts',(28.9834993954173,19.2835406586168,38.4586889918098));
#64244=CARTESIAN_POINT('Ctrl Pts',(28.9647351365839,19.2947924157477,38.4572396834865));
#64245=CARTESIAN_POINT('Ctrl Pts',(28.9363375327525,19.3124622896474,38.4550513795919));
#64246=CARTESIAN_POINT('Ctrl Pts',(28.9265692127435,19.3186589492467,38.4542995755035));
#64247=CARTESIAN_POINT('Ctrl Pts',(28.9087403618766,19.3301876313821,38.4529299332469));
#64248=CARTESIAN_POINT('Ctrl Pts',(28.9006642053438,19.3354935386767,38.4523105647302));
#64249=CARTESIAN_POINT('Ctrl Pts',(28.8815962470865,19.3482202112982,38.4508503212496));
#64250=CARTESIAN_POINT('Ctrl Pts',(28.8706394246571,19.3556922007663,38.4500128220699));
#64251=CARTESIAN_POINT('Ctrl Pts',(28.8332761447241,19.3817217099671,38.4471593712306));
#64252=CARTESIAN_POINT('Ctrl Pts',(28.8072446373423,19.4008114283597,38.445175588265));
#64253=CARTESIAN_POINT('Ctrl Pts',(28.7416412343071,19.451414039404,38.4401550235173));
#64254=CARTESIAN_POINT('Ctrl Pts',(28.7027828720629,19.4838161068116,38.4371604259035));
#64255=CARTESIAN_POINT('Ctrl Pts',(28.5413125590712,19.6292156101698,38.4244265430131));
#64256=CARTESIAN_POINT('Ctrl Pts',(28.4319085545446,19.7558508007852,38.4149780941566));
#64257=CARTESIAN_POINT('Ctrl Pts',(28.3197215603009,19.924374741007,38.4026931886661));
#64258=CARTESIAN_POINT('Ctrl Pts',(28.3007175542428,19.9546559116108,38.400498821796));
#64259=CARTESIAN_POINT('Ctrl Pts',(28.2723805329349,20.0026247553496,38.397032382148));
#64260=CARTESIAN_POINT('Ctrl Pts',(28.2624820060267,20.0199706247866,38.3957808402538));
#64261=CARTESIAN_POINT('Ctrl Pts',(28.2445732468259,20.0524777602532,38.3934373655492));
#64262=CARTESIAN_POINT('Ctrl Pts',(28.2364947828984,20.0675994424353,38.3923480111075));
#64263=CARTESIAN_POINT('Ctrl Pts',(28.2188511441517,20.101675441006,38.3898940026575));
#64264=CARTESIAN_POINT('Ctrl Pts',(28.2093917662706,20.1206818804129,38.3885257764755));
#64265=CARTESIAN_POINT('Ctrl Pts',(28.181442113687,20.1791622093136,38.3843158605028));
#64266=CARTESIAN_POINT('Ctrl Pts',(28.163941773927,20.2190920865512,38.3814409680758));
#64267=CARTESIAN_POINT('Ctrl Pts',(28.1252843302413,20.3157950757867,38.3744747904176));
#64268=CARTESIAN_POINT('Ctrl Pts',(28.1053787260614,20.3730196231009,38.3703488499643));
#64269=CARTESIAN_POINT('Ctrl Pts',(28.0506865276456,20.5568087832779,38.3571254767949));
#64270=CARTESIAN_POINT('Ctrl Pts',(28.0257640951714,20.6859410108696,38.3478535727279));
#64271=CARTESIAN_POINT('Ctrl Pts',(28.0100420914412,20.8562012952192,38.336166849105));
#64272=CARTESIAN_POINT('Ctrl Pts',(28.0075695812252,20.8959229884023,38.333480220987));
#64273=CARTESIAN_POINT('Ctrl Pts',(28.0058509138303,20.9492083396158,38.3299513932691));
#64274=CARTESIAN_POINT('Ctrl Pts',(28.0055524375389,20.9627264884663,38.3290626395997));
#64275=CARTESIAN_POINT('Ctrl Pts',(28.0052973275745,20.9841488621085,38.3276655801364));
#64276=CARTESIAN_POINT('Ctrl Pts',(28.0052501828923,20.9920513079393,38.3271526709971));
#64277=CARTESIAN_POINT('Ctrl Pts',(28.0052500005311,20.9999539693013,38.3266423355102));
#64278=CARTESIAN_POINT('Ctrl Pts',(28.0052500005237,20.9999542895831,38.3266423148271));
#64279=CARTESIAN_POINT('Ctrl Pts',(28.0052499353216,21.0027996336104,38.3264585691541));
#64280=CARTESIAN_POINT('Ctrl Pts',(28.0052559580871,21.0056449990733,38.3262751575534));
#64281=CARTESIAN_POINT('Ctrl Pts',(28.0052915554529,21.014008266251,38.3257370685318));
#64282=CARTESIAN_POINT('Ctrl Pts',(28.0053379360369,21.0195259182242,38.3253833666345));
#64283=CARTESIAN_POINT('Ctrl Pts',(28.0055430235024,21.0358601424736,38.3243399943713));
#64284=CARTESIAN_POINT('Ctrl Pts',(28.0057668233762,21.0466758070004,38.3236539289844));
#64285=CARTESIAN_POINT('Ctrl Pts',(28.0067037247021,21.0791706198002,38.3216056947997));
#64286=CARTESIAN_POINT('Ctrl Pts',(28.0076824637508,21.1008412192493,38.3202571251304));
#64287=CARTESIAN_POINT('Ctrl Pts',(28.0146518748454,21.2141215530399,38.3132786163443));
#64288=CARTESIAN_POINT('Ctrl Pts',(28.0266085742015,21.3052622726676,38.307904085915));
#64289=CARTESIAN_POINT('Ctrl Pts',(28.0625866105701,21.4832301201308,38.2973486523115));
#64290=CARTESIAN_POINT('Ctrl Pts',(28.0862862554856,21.5698957836393,38.2921768223953));
#64291=CARTESIAN_POINT('Ctrl Pts',(28.1394109870688,21.7227988264733,38.2826331726122));
#64292=CARTESIAN_POINT('Ctrl Pts',(28.1667576821797,21.789588915637,38.2783118530124));
#64293=CARTESIAN_POINT('Ctrl Pts',(28.2084407559848,21.877482875285,38.2723216468109));
#64294=CARTESIAN_POINT('Ctrl Pts',(28.2196517372263,21.9000114974699,38.2707584839981));
#64295=CARTESIAN_POINT('Ctrl Pts',(28.2394550801156,21.9379879177497,38.2680724063024));
#64296=CARTESIAN_POINT('Ctrl Pts',(28.2478322496926,21.953544907737,38.2669571320671));
#64297=CARTESIAN_POINT('Ctrl Pts',(28.2652475144405,21.9848817181851,38.2646790454114));
#64298=CARTESIAN_POINT('Ctrl Pts',(28.2742969192428,22.0006532995147,38.2635159040854));
#64299=CARTESIAN_POINT('Ctrl Pts',(28.2977586079486,22.0402780447871,38.2605501691011));
#64300=CARTESIAN_POINT('Ctrl Pts',(28.3124571079463,22.0639563075914,38.2587372983413));
#64301=CARTESIAN_POINT('Ctrl Pts',(28.3862524131256,22.1774574780032,38.2498430952989));
#64302=CARTESIAN_POINT('Ctrl Pts',(28.452041508447,22.2626977740906,38.242515249841));
#64303=CARTESIAN_POINT('Ctrl Pts',(28.5940153617141,22.4187842910637,38.2278755020148));
#64304=CARTESIAN_POINT('Ctrl Pts',(28.6695177488835,22.4898184268421,38.2205970864918));
#64305=CARTESIAN_POINT('Ctrl Pts',(28.7762789410399,22.5756442072145,38.2111915221725));
#64306=CARTESIAN_POINT('Ctrl Pts',(28.8028910913515,22.5959568895346,38.2089135559009));
#64307=CARTESIAN_POINT('Ctrl Pts',(28.8495779822753,22.6297671227649,38.205045765066));
#64308=CARTESIAN_POINT('Ctrl Pts',(28.8694098895584,22.643586875849,38.2034410056227));
#64309=CARTESIAN_POINT('Ctrl Pts',(28.8993576194421,22.6636571284915,38.2010796882376));
#64310=CARTESIAN_POINT('Ctrl Pts',(28.909285345264,22.6701826996185,38.2003068273198));
#64311=CARTESIAN_POINT('Ctrl Pts',(28.9274388052809,22.6818842041793,38.1989123887478));
#64312=CARTESIAN_POINT('Ctrl Pts',(28.9356446367017,22.6870891085592,38.1982890263585));
#64313=CARTESIAN_POINT('Ctrl Pts',(28.9546287244898,22.6989369420292,38.1968625524669));
#64314=CARTESIAN_POINT('Ctrl Pts',(28.9654326137859,22.7055375047443,38.1960621349731));
#64315=CARTESIAN_POINT('Ctrl Pts',(28.9935484837526,22.7223492207744,38.1940064685457));
#64316=CARTESIAN_POINT('Ctrl Pts',(29.010953171196,22.7324023454945,38.1927604000512));
#64317=CARTESIAN_POINT('Ctrl Pts',(29.0285070492154,22.7421908647091,38.1915268296408));
#64318=CARTESIAN_POINT('',(28.0052504446904,20.9986680494153,38.1704548814437));
#64319=CARTESIAN_POINT('Ctrl Pts',(29.0285070491141,22.7421908646526,38.0351948256389));
#64320=CARTESIAN_POINT('Ctrl Pts',(28.9662244865535,22.7074604159295,38.0397334363702));
#64321=CARTESIAN_POINT('Ctrl Pts',(28.9058244632904,22.6693959224897,38.0442720471014));
#64322=CARTESIAN_POINT('Ctrl Pts',(28.8476729941294,22.62824139305,38.0488106578327));
#64323=CARTESIAN_POINT('Ctrl Pts',(28.7907206949419,22.5879355313514,38.0532556756455));
#64324=CARTESIAN_POINT('Ctrl Pts',(28.7359254420456,22.544666231565,38.0577006934583));
#64325=CARTESIAN_POINT('Ctrl Pts',(28.6835980319698,22.4987039137422,38.0621457112711));
#64326=CARTESIAN_POINT('Ctrl Pts',(28.6296179372828,22.451289943425,38.0667311184616));
#64327=CARTESIAN_POINT('Ctrl Pts',(28.5782646094843,22.4010103669668,38.0713165256521));
#64328=CARTESIAN_POINT('Ctrl Pts',(28.5298368250253,22.3482016916799,38.0759019328425));
#64329=CARTESIAN_POINT('Ctrl Pts',(28.4814090405664,22.295393016393,38.080487340033));
#64330=CARTESIAN_POINT('Ctrl Pts',(28.4359071028786,22.2400557227533,38.0850727472235));
#64331=CARTESIAN_POINT('Ctrl Pts',(28.3935816618508,22.1825598020219,38.0896581544139));
#64332=CARTESIAN_POINT('Ctrl Pts',(28.3522336481963,22.1263916426889,38.0941376701501));
#64333=CARTESIAN_POINT('Ctrl Pts',(28.3137534845701,22.0679416529915,38.0986171858863));
#64334=CARTESIAN_POINT('Ctrl Pts',(28.2784002030468,22.0075324816753,38.1030967016224));
#64335=CARTESIAN_POINT('Ctrl Pts',(28.2431007530867,21.947215293903,38.1075693965113));
#64336=CARTESIAN_POINT('Ctrl Pts',(28.2109189775721,21.8849452570051,38.1120420914001));
#64337=CARTESIAN_POINT('Ctrl Pts',(28.182072043412,21.8210758230248,38.116514786289));
#64338=CARTESIAN_POINT('Ctrl Pts',(28.1530811998829,21.7568877621189,38.1210097942145));
#64339=CARTESIAN_POINT('Ctrl Pts',(28.1274588572479,21.6910846990376,38.12550480214));
#64340=CARTESIAN_POINT('Ctrl Pts',(28.105379654119,21.6240523275126,38.1299998100656));
#64341=CARTESIAN_POINT('Ctrl Pts',(28.0834561672684,21.5574927099795,38.1344631163984));
#64342=CARTESIAN_POINT('Ctrl Pts',(28.065026159838,21.4897215305499,38.1389264227312));
#64343=CARTESIAN_POINT('Ctrl Pts',(28.0502123832888,21.4211363344806,38.143389729064));
#64344=CARTESIAN_POINT('Ctrl Pts',(28.0352407796909,21.3518204267628,38.1479005877858));
#64345=CARTESIAN_POINT('Ctrl Pts',(28.0239630968909,21.2816735241105,38.1524114465077));
#64346=CARTESIAN_POINT('Ctrl Pts',(28.0164536567916,21.2111195558078,38.1569223052296));
#64347=CARTESIAN_POINT('Ctrl Pts',(28.0089442166923,21.140565587505,38.1614331639515));
#64348=CARTESIAN_POINT('Ctrl Pts',(28.0052030780735,21.0696050596119,38.1659440226733));
#64349=CARTESIAN_POINT('Ctrl Pts',(28.0052504446899,20.9986680501775,38.1704548813952));
#64350=CARTESIAN_POINT('Ctrl Pts',(28.0052504446904,20.9986680494153,38.1704548814437));
#64351=CARTESIAN_POINT('Ctrl Pts',(28.0053033577008,20.9194247162574,38.1754939362809));
#64352=CARTESIAN_POINT('Ctrl Pts',(28.0100823501052,20.8403644159677,38.1805329911182));
#64353=CARTESIAN_POINT('Ctrl Pts',(28.0194980695967,20.7620091048615,38.1855720459555));
#64354=CARTESIAN_POINT('Ctrl Pts',(28.0291574941401,20.681625740012,38.1907415255704));
#64355=CARTESIAN_POINT('Ctrl Pts',(28.0436968045175,20.6019846203246,38.1959110051852));
#64356=CARTESIAN_POINT('Ctrl Pts',(28.0629665565717,20.5236293443753,38.2010804848001));
#64357=CARTESIAN_POINT('Ctrl Pts',(28.0822363086259,20.445274068426,38.206249964415));
#64358=CARTESIAN_POINT('Ctrl Pts',(28.1062363183479,20.3682048301099,38.2114194440298));
#64359=CARTESIAN_POINT('Ctrl Pts',(28.134766354791,20.2929420028879,38.2165889236447));
#64360=CARTESIAN_POINT('Ctrl Pts',(28.159353446891,20.2280807445326,38.2210439642702));
#64361=CARTESIAN_POINT('Ctrl Pts',(28.1873762006749,20.1643757540817,38.2254990048957));
#64362=CARTESIAN_POINT('Ctrl Pts',(28.2187051826263,20.1022158744456,38.2299540455211));
#64363=CARTESIAN_POINT('Ctrl Pts',(28.2499872411846,20.0401490955835,38.2344024135512));
#64364=CARTESIAN_POINT('Ctrl Pts',(28.2845654808836,19.979623267721,38.2388507815812));
#64365=CARTESIAN_POINT('Ctrl Pts',(28.3222619153755,19.9210085811738,38.2432991496112));
#64366=CARTESIAN_POINT('Ctrl Pts',(28.3599141283183,19.8624626553006,38.247742299277));
#64367=CARTESIAN_POINT('Ctrl Pts',(28.4006770073976,19.8058238274401,38.2521854489428));
#64368=CARTESIAN_POINT('Ctrl Pts',(28.4443268903497,19.7514373310038,38.2566285986086));
#64369=CARTESIAN_POINT('Ctrl Pts',(28.4879494039135,19.6970849360366,38.2610689623267));
#64370=CARTESIAN_POINT('Ctrl Pts',(28.5344550246538,19.6449824515438,38.2655093260449));
#64371=CARTESIAN_POINT('Ctrl Pts',(28.5835779446301,19.5954445103302,38.2699496897631));
#64372=CARTESIAN_POINT('Ctrl Pts',(28.6326867335903,19.5459208195203,38.2743887761376));
#64373=CARTESIAN_POINT('Ctrl Pts',(28.6844109827346,19.498960554679,38.2788278625121));
#64374=CARTESIAN_POINT('Ctrl Pts',(28.7384471413776,19.4548424198802,38.2832669488865));
#64375=CARTESIAN_POINT('Ctrl Pts',(28.7924860924751,19.4107220051658,38.287706264662));
#64376=CARTESIAN_POINT('Ctrl Pts',(28.8488368097305,19.3694443196648,38.2921455804375));
#64377=CARTESIAN_POINT('Ctrl Pts',(28.907163086983,19.3312474587143,38.2965848962129));
#64378=CARTESIAN_POINT('Ctrl Pts',(28.9655510022316,19.2930102321159,38.3010289033649));
#64379=CARTESIAN_POINT('Ctrl Pts',(29.0259182342395,19.2578605967989,38.3054729105169));
#64380=CARTESIAN_POINT('Ctrl Pts',(29.0879008637305,19.225992466725,38.3099169176689));
#64381=CARTESIAN_POINT('Ctrl Pts',(29.149919797734,19.194105670826,38.3143635277681));
#64382=CARTESIAN_POINT('Ctrl Pts',(29.2135555660711,19.1655044064381,38.3188101378674));
#64383=CARTESIAN_POINT('Ctrl Pts',(29.2784235434252,19.1403347129613,38.3232567479666));
#64384=CARTESIAN_POINT('Ctrl Pts',(29.3434038927321,19.115121417576,38.3277110610077));
#64385=CARTESIAN_POINT('Ctrl Pts',(29.4096202471859,19.0933517118923,38.3321653740488));
#64386=CARTESIAN_POINT('Ctrl Pts',(29.4766728619332,19.0751217521457,38.3366196870899));
#64387=CARTESIAN_POINT('Ctrl Pts',(29.511295741333,19.0657086412603,38.3389196890184));
#64388=CARTESIAN_POINT('Ctrl Pts',(29.5461414162752,19.0572384654601,38.341219690947));
#64389=CARTESIAN_POINT('Ctrl Pts',(29.581154132761,19.0497190710062,38.3435196928755));
#64390=CARTESIAN_POINT('Ctrl Pts',(29.6489727799341,19.0351542154165,38.3479747319283));
#64391=CARTESIAN_POINT('Ctrl Pts',(29.717685610293,19.0241023559207,38.3524297709811));
#64392=CARTESIAN_POINT('Ctrl Pts',(29.7868958052815,19.0166658968562,38.3568848100339));
#64393=CARTESIAN_POINT('Ctrl Pts',(29.8560023391715,19.0092405759125,38.3613331764535));
#64394=CARTESIAN_POINT('Ctrl Pts',(29.9256042765727,19.0054199595103,38.3657815428732));
#64395=CARTESIAN_POINT('Ctrl Pts',(29.9952941040524,19.0052555509431,38.3702299092928));
#64396=CARTESIAN_POINT('Ctrl Pts',(30.0649021778678,19.0050913352449,38.3746730573001));
#64397=CARTESIAN_POINT('Ctrl Pts',(30.1345974500217,19.0085748096506,38.3791162053074));
#64398=CARTESIAN_POINT('Ctrl Pts',(30.2039685684346,19.0157055698333,38.3835593533148));
#64399=CARTESIAN_POINT('Ctrl Pts',(30.2732961892405,19.0228318588324,38.3879997153456));
#64400=CARTESIAN_POINT('Ctrl Pts',(30.3422995739079,19.0336008467942,38.3924400773764));
#64401=CARTESIAN_POINT('Ctrl Pts',(30.4105701878447,19.0479601224992,38.3968804394072));
#64402=CARTESIAN_POINT('Ctrl Pts',(30.4788211622039,19.0623152674357,38.401319524068));
#64403=CARTESIAN_POINT('Ctrl Pts',(30.5463393057376,19.0802585490548,38.4057586087288));
#64404=CARTESIAN_POINT('Ctrl Pts',(30.6127257662419,19.1016863541861,38.4101976933896));
#64405=CARTESIAN_POINT('Ctrl Pts',(30.6791156570786,19.1231152665386,38.4146370074275));
#64406=CARTESIAN_POINT('Ctrl Pts',(30.7443732838954,19.1480289072775,38.4190763214655));
#64407=CARTESIAN_POINT('Ctrl Pts',(30.8081161690147,19.1762741927919,38.4235156355034));
#64408=CARTESIAN_POINT('Ctrl Pts',(30.8719264159649,19.2045493271928,38.4279596408935));
#64409=CARTESIAN_POINT('Ctrl Pts',(30.934218278086,19.2361629349013,38.4324036462836));
#64410=CARTESIAN_POINT('Ctrl Pts',(30.9946313357288,19.2709146728729,38.4368476516737));
#64411=CARTESIAN_POINT('Ctrl Pts',(31.0550797783436,19.3056867655379,38.4412942599945));
#64412=CARTESIAN_POINT('Ctrl Pts',(31.1136468153052,19.3436003809612,38.4457408683154));
#64413=CARTESIAN_POINT('Ctrl Pts',(31.1700009906591,19.3844117961694,38.4501874766363));
#64414=CARTESIAN_POINT('Ctrl Pts',(31.2264527893072,19.4252939096845,38.4546417878921));
#64415=CARTESIAN_POINT('Ctrl Pts',(31.2806836939092,19.4690835359395,38.459096099148));
#64416=CARTESIAN_POINT('Ctrl Pts',(31.3323959319347,19.5154971731034,38.4635504104039));
#64417=CARTESIAN_POINT('Ctrl Pts',(31.3590979363168,19.5394632049415,38.465850427638));
#64418=CARTESIAN_POINT('Ctrl Pts',(31.3851290117348,19.5641282675209,38.4681504448722));
#64419=CARTESIAN_POINT('Ctrl Pts',(31.4104522994071,19.5894497975623,38.4704504621063));
#64420=CARTESIAN_POINT('Ctrl Pts',(31.4595024849717,19.6384965786668,38.4749055026048));
#64421=CARTESIAN_POINT('Ctrl Pts',(31.5060879097224,19.6902014941159,38.4793605431033));
#64422=CARTESIAN_POINT('Ctrl Pts',(31.5499071425516,19.7442868910585,38.4838155836019));
#64423=CARTESIAN_POINT('Ctrl Pts',(31.593660744409,19.7982912807142,38.4882639514907));
#64424=CARTESIAN_POINT('Ctrl Pts',(31.6346560720253,19.8546686981639,38.4927123193795));
#64425=CARTESIAN_POINT('Ctrl Pts',(31.6726286347102,19.9131048749545,38.4971606872683));
#64426=CARTESIAN_POINT('Ctrl Pts',(31.7105566517444,19.9714725002086,38.5016038367724));
#64427=CARTESIAN_POINT('Ctrl Pts',(31.745468681447,20.031893679646,38.5060469862765));
#64428=CARTESIAN_POINT('Ctrl Pts',(31.7771417410935,20.0940227405927,38.5104901357806));
#64429=CARTESIAN_POINT('Ctrl Pts',(31.8087949409794,20.1561128451425,38.5149304993244));
#64430=CARTESIAN_POINT('Ctrl Pts',(31.8372129780541,20.2199082718438,38.5193708628682));
#64431=CARTESIAN_POINT('Ctrl Pts',(31.8622180745264,20.2850374797186,38.523811226412));
#64432=CARTESIAN_POINT('Ctrl Pts',(31.8872159778013,20.3501479519226,38.5282503125997));
#64433=CARTESIAN_POINT('Ctrl Pts',(31.9088027142856,20.4165909870344,38.5326893987874));
#64434=CARTESIAN_POINT('Ctrl Pts',(31.9268487620699,20.4839753779035,38.5371284849752));
#64435=CARTESIAN_POINT('Ctrl Pts',(31.9448957423796,20.5513632508458,38.5415678005517));
#64436=CARTESIAN_POINT('Ctrl Pts',(31.9594015464992,20.6196921028616,38.5460071161282));
#64437=CARTESIAN_POINT('Ctrl Pts',(31.9702870874265,20.6885576207058,38.5504464317047));
#64438=CARTESIAN_POINT('Ctrl Pts',(31.9811841319252,20.7574959139321,38.5548904386405));
#64439=CARTESIAN_POINT('Ctrl Pts',(31.9884532007772,20.826971520689,38.5593344455763));
#64440=CARTESIAN_POINT('Ctrl Pts',(31.9920668706479,20.8965729949813,38.5637784525121));
#64441=CARTESIAN_POINT('Ctrl Pts',(31.9956826571119,20.966215236145,38.568225062385));
#64442=CARTESIAN_POINT('Ctrl Pts',(31.9956387833975,21.0359830021607,38.5726716722579));
#64443=CARTESIAN_POINT('Ctrl Pts',(31.9919599809071,21.1054656198218,38.5771182821308));
#64444=CARTESIAN_POINT('Ctrl Pts',(31.9882748055725,21.175068603255,38.5815725949321));
#64445=CARTESIAN_POINT('Ctrl Pts',(31.9809421837478,21.2443849658485,38.5860269077334));
#64446=CARTESIAN_POINT('Ctrl Pts',(31.9700385397303,21.3130107258186,38.5904812205348));
#64447=CARTESIAN_POINT('Ctrl Pts',(31.9644083961772,21.3484459325667,38.5927812241355));
#64448=CARTESIAN_POINT('Ctrl Pts',(31.9578269728795,21.3836971987488,38.5950812277363));
#64449=CARTESIAN_POINT('Ctrl Pts',(31.9503100035496,21.41871046387,38.597381231337));
#64450=CARTESIAN_POINT('Ctrl Pts',(31.9357498524979,21.4865301404717,38.6018362714438));
#64451=CARTESIAN_POINT('Ctrl Pts',(31.9176192905568,21.5537230114834,38.6062913115506));
#64452=CARTESIAN_POINT('Ctrl Pts',(31.8959878436836,21.6198851983264,38.6107463516575));
#64453=CARTESIAN_POINT('Ctrl Pts',(31.8743887956824,21.6859482896147,38.6151947191512));
#64454=CARTESIAN_POINT('Ctrl Pts',(31.849299420854,21.7509832993906,38.619643086645));
#64455=CARTESIAN_POINT('Ctrl Pts',(31.8208400497719,21.8145974930276,38.6240914541388));
#64456=CARTESIAN_POINT('Ctrl Pts',(31.7924140644281,21.878137060742,38.6285346032448));
#64457=CARTESIAN_POINT('Ctrl Pts',(31.7606261336652,21.9402586782658,38.6329777523509));
#64458=CARTESIAN_POINT('Ctrl Pts',(31.725645495878,22.0005874199968,38.6374209014569));
#64459=CARTESIAN_POINT('Ctrl Pts',(31.6906867917963,22.0608783341486,38.641861264601));
#64460=CARTESIAN_POINT('Ctrl Pts',(31.6525395969839,22.1193781803559,38.6463016277452));
#64461=CARTESIAN_POINT('Ctrl Pts',(31.6114194156794,22.1757359521897,38.6507419908893));
#64462=CARTESIAN_POINT('Ctrl Pts',(31.5703110633973,22.2320775116109,38.6551810766764));
#64463=CARTESIAN_POINT('Ctrl Pts',(31.5262317107216,22.2862778249092,38.6596201624635));
#64464=CARTESIAN_POINT('Ctrl Pts',(31.4794395755487,22.3380157341378,38.6640592482505));
#64465=CARTESIAN_POINT('Ctrl Pts',(31.4326450224067,22.3897563169068,38.668498563426));
#64466=CARTESIAN_POINT('Ctrl Pts',(31.383137738449,22.439033881712,38.6729378786014));
#64467=CARTESIAN_POINT('Ctrl Pts',(31.3312143290751,22.4855625104872,38.6773771937769));
#64468=CARTESIAN_POINT('Ctrl Pts',(31.2792360482914,22.532140309598,38.6818212003138));
#64469=CARTESIAN_POINT('Ctrl Pts',(31.2248369110719,22.5759630474057,38.6862652068507));
#64470=CARTESIAN_POINT('Ctrl Pts',(31.168347561005,22.6167843205554,38.6907092133877));
#64471=CARTESIAN_POINT('Ctrl Pts',(31.1118251240692,22.6576295034882,38.6951558228623));
#64472=CARTESIAN_POINT('Ctrl Pts',(31.0532104486739,22.6954694571733,38.699602432337));
#64473=CARTESIAN_POINT('Ctrl Pts',(30.992861844136,22.7301019972704,38.7040490418117));
#64474=CARTESIAN_POINT('Ctrl Pts',(30.9324086967318,22.7647945318783,38.7085033542201));
#64475=CARTESIAN_POINT('Ctrl Pts',(30.8702160609267,22.7962683411249,38.7129576666284));
#64476=CARTESIAN_POINT('Ctrl Pts',(30.8066646905723,22.8243682850466,38.7174119790368));
#64477=CARTESIAN_POINT('Ctrl Pts',(30.7738496128403,22.8388778359644,38.7197119862138));
#64478=CARTESIAN_POINT('Ctrl Pts',(30.7406725588488,22.8524886398037,38.7220119933908));
#64479=CARTESIAN_POINT('Ctrl Pts',(30.7071874705828,22.8651845602917,38.7243120005678));
#64480=CARTESIAN_POINT('Ctrl Pts',(30.6399473745884,22.8906787416293,38.7289305550163));
#64481=CARTESIAN_POINT('Ctrl Pts',(30.5711895972421,22.9125843100179,38.7335491094648));
#64482=CARTESIAN_POINT('Ctrl Pts',(30.5013345674729,22.9307229770106,38.7381676639133));
#64483=CARTESIAN_POINT('Ctrl Pts',(30.434069343021,22.9481891710779,38.7426149900778));
#64484=CARTESIAN_POINT('Ctrl Pts',(30.3657873143873,22.9621626908888,38.7470623162424));
#64485=CARTESIAN_POINT('Ctrl Pts',(30.2968839503906,22.9725332652456,38.751509642407));
#64486=CARTESIAN_POINT('Ctrl Pts',(30.2280487577815,22.9828935791971,38.7559525684904));
#64487=CARTESIAN_POINT('Ctrl Pts',(30.1585939306255,22.9896579468043,38.7603954945738));
#64488=CARTESIAN_POINT('Ctrl Pts',(30.0889264887833,22.9927668308391,38.7648384206572));
#64489=CARTESIAN_POINT('Ctrl Pts',(30.0193043302163,22.9958736941244,38.7692784588745));
#64490=CARTESIAN_POINT('Ctrl Pts',(29.9494703188918,22.9953297680141,38.7737184970918));
#64491=CARTESIAN_POINT('Ctrl Pts',(29.8798362094755,22.9911273756209,38.7781585353091));
#64492=CARTESIAN_POINT('Ctrl Pts',(29.8102237308516,22.9869262886378,38.7825971942951));
#64493=CARTESIAN_POINT('Ctrl Pts',(29.7408115187254,22.9790690231803,38.787035853281));
#64494=CARTESIAN_POINT('Ctrl Pts',(29.6720091552,22.9675999512674,38.791474512267));
#64495=CARTESIAN_POINT('Ctrl Pts',(29.6031755485967,22.9561256712615,38.7959151868432));
#64496=CARTESIAN_POINT('Ctrl Pts',(29.5349528272508,22.9410363868837,38.8003558614193));
#64497=CARTESIAN_POINT('Ctrl Pts',(29.4677420410995,22.9224278992168,38.8047965359955));
#64498=CARTESIAN_POINT('Ctrl Pts',(29.4005125436344,22.9038142309938,38.8092384468443));
#64499=CARTESIAN_POINT('Ctrl Pts',(29.334296008895,22.8816795567646,38.8136803576931));
#64500=CARTESIAN_POINT('Ctrl Pts',(29.2694776142112,22.8561693366612,38.8181222685418));
#64501=CARTESIAN_POINT('Ctrl Pts',(29.2045867169759,22.8306305821263,38.8225691478856));
#64502=CARTESIAN_POINT('Ctrl Pts',(29.1410975277273,22.8017089455978,38.8270160272294));
#64503=CARTESIAN_POINT('Ctrl Pts',(29.0793734864984,22.7695972381132,38.8314629065732));
#64504=CARTESIAN_POINT('Ctrl Pts',(29.0622803501589,22.7607045962317,38.8326943734927));
#64505=CARTESIAN_POINT('Ctrl Pts',(29.0453224246989,22.7515675748504,38.8339258404121));
#64506=CARTESIAN_POINT('Ctrl Pts',(29.0285070491141,22.7421908646526,38.8351573073316));
#64507=CARTESIAN_POINT('Origin',(30.,21.,34.5704548813952));
#64508=CARTESIAN_POINT('',(29.0285070493988,22.7421908648114,39.7951262847314));
#64509=CARTESIAN_POINT('',(29.0285070491141,22.7421908646526,39.6352957892028));
#64510=CARTESIAN_POINT('',(29.0285070491141,22.7421908646526,34.5704548813952));
#64511=CARTESIAN_POINT('Ctrl Pts',(29.0285070493988,22.7421908648114,39.7951262847314));
#64512=CARTESIAN_POINT('Ctrl Pts',(29.036539361456,22.7466699002019,39.7945520334221));
#64513=CARTESIAN_POINT('Ctrl Pts',(29.0446025931056,22.7510933553019,39.7939758446525));
#64514=CARTESIAN_POINT('Ctrl Pts',(29.0679332045984,22.7636833123941,39.7923092073879));
#64515=CARTESIAN_POINT('Ctrl Pts',(29.0832762380762,22.7717067621654,39.7912138221446));
#64516=CARTESIAN_POINT('Ctrl Pts',(29.1156263497491,22.7880911309112,39.788904618725));
#64517=CARTESIAN_POINT('Ctrl Pts',(29.132651951512,22.796411413743,39.7876895104054));
#64518=CARTESIAN_POINT('Ctrl Pts',(29.1784375838042,22.8179838881956,39.7844211433771));
#64519=CARTESIAN_POINT('Ctrl Pts',(29.2073979806479,22.8307954746988,39.7823530619238));
#64520=CARTESIAN_POINT('Ctrl Pts',(29.3707593117285,22.8984611764182,39.7706772357746));
#64521=CARTESIAN_POINT('Ctrl Pts',(29.510511170617,22.9391972368264,39.7606050976751));
#64522=CARTESIAN_POINT('Ctrl Pts',(29.7225137441991,22.9766011141778,39.7455891852928));
#64523=CARTESIAN_POINT('Ctrl Pts',(29.7922092847968,22.9851384194155,39.7407023088821));
#64524=CARTESIAN_POINT('Ctrl Pts',(29.9018599149984,22.9927306714876,39.7332063243256));
#64525=CARTESIAN_POINT('Ctrl Pts',(29.9415834412332,22.9942905959305,39.7305304517894));
#64526=CARTESIAN_POINT('Ctrl Pts',(29.9956257829792,22.9947964360434,39.7269663075634));
#64527=CARTESIAN_POINT('Ctrl Pts',(30.0099232799932,22.9947765569524,39.7260306439618));
#64528=CARTESIAN_POINT('Ctrl Pts',(30.0341069483306,22.9944829024896,39.7244616798304));
#64529=CARTESIAN_POINT('Ctrl Pts',(30.0439933645323,22.9942893304325,39.7238241691572));
#64530=CARTESIAN_POINT('Ctrl Pts',(30.0649267946733,22.9937237090246,39.7224829691445));
#64531=CARTESIAN_POINT('Ctrl Pts',(30.0759727385705,22.9933333573353,39.7217802620254));
#64532=CARTESIAN_POINT('Ctrl Pts',(30.1069969335266,22.9919787274037,39.7198192366003));
#64533=CARTESIAN_POINT('Ctrl Pts',(30.126965330382,22.9908057339666,39.7185717700403));
#64534=CARTESIAN_POINT('Ctrl Pts',(30.2763099853637,22.9797765281081,39.7093297276297));
#64535=CARTESIAN_POINT('Ctrl Pts',(30.4044824469687,22.9576171520778,39.7018778467403));
#64536=CARTESIAN_POINT('Ctrl Pts',(30.6463707309361,22.8910050748657,39.6873159889492));
#64537=CARTESIAN_POINT('Ctrl Pts',(30.759950135686,22.8482874585378,39.680242682745));
#64538=CARTESIAN_POINT('Ctrl Pts',(30.8942645725224,22.7832861358474,39.6710957038127));
#64539=CARTESIAN_POINT('Ctrl Pts',(30.9193176298218,22.7705009295334,39.6693549498248));
#64540=CARTESIAN_POINT('Ctrl Pts',(30.9601536807495,22.7485608240514,39.6664551459016));
#64541=CARTESIAN_POINT('Ctrl Pts',(30.9760967366155,22.7397112321717,39.6653069367518));
#64542=CARTESIAN_POINT('Ctrl Pts',(31.007041123299,22.721975512469,39.6630454764577));
#64543=CARTESIAN_POINT('Ctrl Pts',(31.0220517174939,22.7131087952896,39.6619330018443));
#64544=CARTESIAN_POINT('Ctrl Pts',(31.0548174625421,22.6931702362864,39.6594694504006));
#64545=CARTESIAN_POINT('Ctrl Pts',(31.0725183190534,22.6820135933654,39.6581153463001));
#64546=CARTESIAN_POINT('Ctrl Pts',(31.133431399875,22.6422683254831,39.6533723970482));
#64547=CARTESIAN_POINT('Ctrl Pts',(31.1756998199195,22.612278241014,39.6499323550293));
#64548=CARTESIAN_POINT('Ctrl Pts',(31.3379604917383,22.4873757941637,39.6361224559463));
#64549=CARTESIAN_POINT('Ctrl Pts',(31.4480280930436,22.380445386564,39.6253320913515));
#64550=CARTESIAN_POINT('Ctrl Pts',(31.5721117980322,22.2285594000522,39.6117634676041));
#64551=CARTESIAN_POINT('Ctrl Pts',(31.5983499650048,22.1942242306438,39.608799037308));
#64552=CARTESIAN_POINT('Ctrl Pts',(31.6402957240669,22.135472427847,39.6039264574108));
#64553=CARTESIAN_POINT('Ctrl Pts',(31.6566225584666,22.111516800433,39.601992361586));
#64554=CARTESIAN_POINT('Ctrl Pts',(31.6793639839113,22.0765344294473,39.5992520729199));
#64555=CARTESIAN_POINT('Ctrl Pts',(31.6862033755062,22.0657898317303,39.59842153022));
#64556=CARTESIAN_POINT('Ctrl Pts',(31.6975828484574,22.0475290513263,39.5970296428039));
#64557=CARTESIAN_POINT('Ctrl Pts',(31.7021768848335,22.0400473565419,39.5964648985972));
#64558=CARTESIAN_POINT('Ctrl Pts',(31.7126941853753,22.0226628587045,39.5951655284143));
#64559=CARTESIAN_POINT('Ctrl Pts',(31.7185811263426,22.0127386745704,39.5944332187545));
#64560=CARTESIAN_POINT('Ctrl Pts',(31.7353092515664,21.9839725004442,39.5923360055154));
#64561=CARTESIAN_POINT('Ctrl Pts',(31.7459293389183,21.9650030637591,39.5909841909232));
#64562=CARTESIAN_POINT('Ctrl Pts',(31.8022849931748,21.8603643031657,39.5836750507146));
#64563=CARTESIAN_POINT('Ctrl Pts',(31.8420325602963,21.7716074610855,39.578005650729));
#64564=CARTESIAN_POINT('Ctrl Pts',(31.9214090425261,21.5528163594701,39.5644868324749));
#64565=CARTESIAN_POINT('Ctrl Pts',(31.9545350176356,21.4209607285378,39.556679494198));
#64566=CARTESIAN_POINT('Ctrl Pts',(31.9792139773808,21.2510782517781,39.5462613715487));
#64567=CARTESIAN_POINT('Ctrl Pts',(31.983429621771,21.2152555373467,39.5440468889905));
#64568=CARTESIAN_POINT('Ctrl Pts',(31.9884545489312,21.1595909366878,39.5405681285468));
#64569=CARTESIAN_POINT('Ctrl Pts',(31.98994268374,21.1398171328206,39.5393250675867));
#64570=CARTESIAN_POINT('Ctrl Pts',(31.9921680020967,21.102900559982,39.5369891882851));
#64571=CARTESIAN_POINT('Ctrl Pts',(31.9929792726879,21.0857639918764,39.535898806203));
#64572=CARTESIAN_POINT('Ctrl Pts',(31.9943061497982,21.0472148792541,39.5334313789949));
#64573=CARTESIAN_POINT('Ctrl Pts',(31.9946981073203,21.0258004883987,39.5320505841083));
#64574=CARTESIAN_POINT('Ctrl Pts',(31.9948207884896,20.9699876220486,39.5284239734044));
#64575=CARTESIAN_POINT('Ctrl Pts',(31.9940066814086,20.9355963121984,39.5261616705115));
#64576=CARTESIAN_POINT('Ctrl Pts',(31.9848113712231,20.7500883739725,39.5138053010006));
#64577=CARTESIAN_POINT('Ctrl Pts',(31.960141334953,20.6002945780966,39.5032235081476));
#64578=CARTESIAN_POINT('Ctrl Pts',(31.9028457745142,20.3986628464908,39.4886284538996));
#64579=CARTESIAN_POINT('Ctrl Pts',(31.8844523582095,20.3432896644977,39.4845887054885));
#64580=CARTESIAN_POINT('Ctrl Pts',(31.8549341227635,20.2659389187308,39.4789635159574));
#64581=CARTESIAN_POINT('Ctrl Pts',(31.8457899192858,20.2432398314864,39.4773151633225));
#64582=CARTESIAN_POINT('Ctrl Pts',(31.8287498502307,20.2030883645434,39.4744105693014));
#64583=CARTESIAN_POINT('Ctrl Pts',(31.8210160062335,20.1855707893965,39.4731471829315));
#64584=CARTESIAN_POINT('Ctrl Pts',(31.8084962199335,20.1582831661363,39.4711882686405));
#64585=CARTESIAN_POINT('Ctrl Pts',(31.8038807772557,20.1484367546845,39.4704833029243));
#64586=CARTESIAN_POINT('Ctrl Pts',(31.7949325171252,20.1297461305102,39.4691494220737));
#64587=CARTESIAN_POINT('Ctrl Pts',(31.7906143990114,20.120895560238,39.4685197199439));
#64588=CARTESIAN_POINT('Ctrl Pts',(31.7797141684215,20.0989676093408,39.4669636269963));
#64589=CARTESIAN_POINT('Ctrl Pts',(31.77305314167,20.0859297197853,39.4660419790785));
#64590=CARTESIAN_POINT('Ctrl Pts',(31.7479574947235,20.0381157723963,39.4626708981153));
#64591=CARTESIAN_POINT('Ctrl Pts',(31.7286372558179,20.0038120885293,39.4602698051089));
#64592=CARTESIAN_POINT('Ctrl Pts',(31.6280555694553,19.8369754385789,39.448567706297));
#64593=CARTESIAN_POINT('Ctrl Pts',(31.5325081399703,19.7136807639498,39.4398026153954));
#64594=CARTESIAN_POINT('Ctrl Pts',(31.3726604466452,19.5508207917746,39.4263527703968));
#64595=CARTESIAN_POINT('Ctrl Pts',(31.3189196381397,19.5017455263475,39.421996765647));
#64596=CARTESIAN_POINT('Ctrl Pts',(31.2430947229039,19.4397502216716,39.4159661665922));
#64597=CARTESIAN_POINT('Ctrl Pts',(31.2232658464881,19.4241559594372,39.4143992642414));
#64598=CARTESIAN_POINT('Ctrl Pts',(31.1890453615028,19.3982786539014,39.4117087437697));
#64599=CARTESIAN_POINT('Ctrl Pts',(31.1748026870798,19.3878031273614,39.4105928303341));
#64600=CARTESIAN_POINT('Ctrl Pts',(31.1456462635157,19.366950016697,39.4083151626601));
#64601=CARTESIAN_POINT('Ctrl Pts',(31.1307262466197,19.3565841280522,39.4071531023408));
#64602=CARTESIAN_POINT('Ctrl Pts',(31.0926321783687,19.3308820779916,39.4041937274019));
#64603=CARTESIAN_POINT('Ctrl Pts',(31.0692760186317,19.3158241239205,39.4023862250952));
#64604=CARTESIAN_POINT('Ctrl Pts',(30.9556059664718,19.2458575875083,39.39361815547));
#64605=CARTESIAN_POINT('Ctrl Pts',(30.8613506353367,19.1977049332483,39.38642006757));
#64606=CARTESIAN_POINT('Ctrl Pts',(30.6666764102505,19.1170211348587,39.3718063969198));
#64607=CARTESIAN_POINT('Ctrl Pts',(30.5665886628764,19.0845250397915,39.3644161747849));
#64608=CARTESIAN_POINT('Ctrl Pts',(30.4316247101106,19.0522156343634,39.3548851780221));
#64609=CARTESIAN_POINT('Ctrl Pts',(30.3986470411496,19.0451996008548,39.3525905483028));
#64610=CARTESIAN_POINT('Ctrl Pts',(30.3416237862887,19.0345710608401,39.3486978429287));
#64611=CARTESIAN_POINT('Ctrl Pts',(30.3176611870913,19.0305561137239,39.3470845943403));
#64612=CARTESIAN_POINT('Ctrl Pts',(30.2818564198595,19.0252275552892,39.3447133944285));
#64613=CARTESIAN_POINT('Ctrl Pts',(30.2700670315828,19.0235807465391,39.3439389501191));
#64614=CARTESIAN_POINT('Ctrl Pts',(30.248629463671,19.0207816329349,39.3425430375795));
#64615=CARTESIAN_POINT('Ctrl Pts',(30.2389869108534,19.0195941783973,39.3419197599276));
#64616=CARTESIAN_POINT('Ctrl Pts',(30.2167882993152,19.017024978859,39.3404951749532));
#64617=CARTESIAN_POINT('Ctrl Pts',(30.2042272897888,19.0156919757201,39.3396965330382));
#64618=CARTESIAN_POINT('Ctrl Pts',(30.1626258394908,19.0116763622526,39.3370735980436));
#64619=CARTESIAN_POINT('Ctrl Pts',(30.1335379129146,19.0095111458063,39.3352752317517));
#64620=CARTESIAN_POINT('Ctrl Pts',(29.9366289899129,18.9991901838455,39.3232788075919));
#64621=CARTESIAN_POINT('Ctrl Pts',(29.7683928234852,19.0116272344936,39.3138485730711));
#64622=CARTESIAN_POINT('Ctrl Pts',(29.5306879467169,19.0598137747538,39.2995672354121));
#64623=CARTESIAN_POINT('Ctrl Pts',(29.4585754864453,19.0786894598511,39.2951101529228));
#64624=CARTESIAN_POINT('Ctrl Pts',(29.3635160308809,19.1093490534305,39.2889619759911));
#64625=CARTESIAN_POINT('Ctrl Pts',(29.3394920508996,19.1176073729015,39.2873844247795));
#64626=CARTESIAN_POINT('Ctrl Pts',(29.298996294201,19.1323985764078,39.2846812348498));
#64627=CARTESIAN_POINT('Ctrl Pts',(29.2824415720761,19.1386963861972,39.2835634839099));
#64628=CARTESIAN_POINT('Ctrl Pts',(29.2491216366345,19.1518826603319,39.2812869086713));
#64629=CARTESIAN_POINT('Ctrl Pts',(29.2323620929147,19.1587808317543,39.2801278423885));
#64630=CARTESIAN_POINT('Ctrl Pts',(29.1903538877437,19.1767445065439,39.2771861159289));
#64631=CARTESIAN_POINT('Ctrl Pts',(29.1652369650154,19.1881065233334,39.2753935149562));
#64632=CARTESIAN_POINT('Ctrl Pts',(29.0527584166285,19.2418230435803,39.2672081296334));
#64633=CARTESIAN_POINT('Ctrl Pts',(28.9683357554302,19.28999502394,39.2606182858524));
#64634=CARTESIAN_POINT('Ctrl Pts',(28.7945763681421,19.4067067635837,39.2461416331602));
#64635=CARTESIAN_POINT('Ctrl Pts',(28.706840534923,19.4770529692606,39.2382359896392));
#64636=CARTESIAN_POINT('Ctrl Pts',(28.5884725136578,19.5896005445797,39.2270077220312));
#64637=CARTESIAN_POINT('Ctrl Pts',(28.5528188533942,19.6262081330973,39.2235419411672));
#64638=CARTESIAN_POINT('Ctrl Pts',(28.5082100646531,19.6756770067108,39.2191366704599));
#64639=CARTESIAN_POINT('Ctrl Pts',(28.4979474901013,19.6873283368284,39.218118149193));
#64640=CARTESIAN_POINT('Ctrl Pts',(28.481228013859,19.7067631940213,39.2164520575789));
#64641=CARTESIAN_POINT('Ctrl Pts',(28.4746925250606,19.7144779638994,39.2157990472697));
#64642=CARTESIAN_POINT('Ctrl Pts',(28.4614188950304,19.7303904799072,39.2144697261078));
#64643=CARTESIAN_POINT('Ctrl Pts',(28.4546870172411,19.7385928699133,39.2137938349335));
#64644=CARTESIAN_POINT('Ctrl Pts',(28.4367724369021,19.7607793847186,39.2119893304385));
#64645=CARTESIAN_POINT('Ctrl Pts',(28.4257117558051,19.7748613449683,39.2108689452228));
#64646=CARTESIAN_POINT('Ctrl Pts',(28.3550264195727,19.8673930174197,39.203653438866));
#64647=CARTESIAN_POINT('Ctrl Pts',(28.3010875597762,19.9500295849003,39.1978806799631));
#64648=CARTESIAN_POINT('Ctrl Pts',(28.2139735807999,20.1079113217731,39.1873965940486));
#64649=CARTESIAN_POINT('Ctrl Pts',(28.1789129008328,20.1818593835315,39.1826820133975));
#64650=CARTESIAN_POINT('Ctrl Pts',(28.1190415846686,20.3312054717283,39.1732303802816));
#64651=CARTESIAN_POINT('Ctrl Pts',(28.0939937861229,20.406342665544,39.1685072648476));
#64652=CARTESIAN_POINT('Ctrl Pts',(28.0667756506715,20.5077206859994,39.1620505163735));
#64653=CARTESIAN_POINT('Ctrl Pts',(28.0605610103498,20.5328045191102,39.1604466639663));
#64654=CARTESIAN_POINT('Ctrl Pts',(28.0508931693392,20.5753510986682,39.1577120750776));
#64655=CARTESIAN_POINT('Ctrl Pts',(28.0471831570209,20.5927525673691,39.1565896833262));
#64656=CARTESIAN_POINT('Ctrl Pts',(28.0401846661912,20.6278760496174,39.1543152043465));
#64657=CARTESIAN_POINT('Ctrl Pts',(28.0369026261939,20.6455976258528,39.1531630280942));
#64658=CARTESIAN_POINT('Ctrl Pts',(28.0292960540955,20.6900237501206,39.150262142754));
#64659=CARTESIAN_POINT('Ctrl Pts',(28.0252738967388,20.716775679519,39.1485040575199));
#64660=CARTESIAN_POINT('Ctrl Pts',(28.0107008279263,20.8292113074831,39.1410644376238));
#64661=CARTESIAN_POINT('Ctrl Pts',(28.0051750809864,20.9154415709448,39.1352306109172));
#64662=CARTESIAN_POINT('Ctrl Pts',(28.0053176225983,21.0779873850309,39.124035666902));
#64663=CARTESIAN_POINT('Ctrl Pts',(28.0097550986224,21.1541564993808,39.1187090408974));
#64664=CARTESIAN_POINT('Ctrl Pts',(28.0285782558279,21.3164024973286,39.1073225283172));
#64665=CARTESIAN_POINT('Ctrl Pts',(28.0442732178099,21.4021810359098,39.1012776071046));
#64666=CARTESIAN_POINT('Ctrl Pts',(28.0708295633449,21.5077413895338,39.0939963969326));
#64667=CARTESIAN_POINT('Ctrl Pts',(28.0764762180912,21.5287307860752,39.0925568501137));
#64668=CARTESIAN_POINT('Ctrl Pts',(28.0856440218507,21.560715492244,39.0903801380092));
#64669=CARTESIAN_POINT('Ctrl Pts',(28.0889192463241,21.5717788410034,39.0896303592631));
#64670=CARTESIAN_POINT('Ctrl Pts',(28.0948555962653,21.5912101555911,39.0883197671906));
#64671=CARTESIAN_POINT('Ctrl Pts',(28.0974761396397,21.5995895364476,39.0877567408961));
#64672=CARTESIAN_POINT('Ctrl Pts',(28.104034099362,21.620083143173,39.0863847132165));
#64673=CARTESIAN_POINT('Ctrl Pts',(28.1080323446956,21.6321773584763,39.0855792172441));
#64674=CARTESIAN_POINT('Ctrl Pts',(28.1215099090744,21.6716718843333,39.0829600643823));
#64675=CARTESIAN_POINT('Ctrl Pts',(28.1314711933364,21.6989051710781,39.0811718777035));
#64676=CARTESIAN_POINT('Ctrl Pts',(28.1577497566417,21.7661652275158,39.0767775167423));
#64677=CARTESIAN_POINT('Ctrl Pts',(28.174781118424,21.8058979952606,39.0742013516575));
#64678=CARTESIAN_POINT('Ctrl Pts',(28.2574821614429,21.9827320241816,39.0626946049925));
#64679=CARTESIAN_POINT('Ctrl Pts',(28.3373975873175,22.1126030987577,39.0540887564798));
#64680=CARTESIAN_POINT('Ctrl Pts',(28.4636887270526,22.2733917758775,39.0418842982781));
#64681=CARTESIAN_POINT('Ctrl Pts',(28.4977010645186,22.3133454116577,39.0387072556169));
#64682=CARTESIAN_POINT('Ctrl Pts',(28.5474923447362,22.3673664180795,39.0341689392116));
#64683=CARTESIAN_POINT('Ctrl Pts',(28.5619814072631,22.3825960670351,39.0328607715581));
#64684=CARTESIAN_POINT('Ctrl Pts',(28.5889386140916,22.4100489545731,39.0304472782084));
#64685=CARTESIAN_POINT('Ctrl Pts',(28.6013318543462,22.4223430233554,39.0293452646484));
#64686=CARTESIAN_POINT('Ctrl Pts',(28.6269713288994,22.4471181730405,39.0270795917211));
#64687=CARTESIAN_POINT('Ctrl Pts',(28.6402301824945,22.459583757621,39.0259154128056));
#64688=CARTESIAN_POINT('Ctrl Pts',(28.6742766464513,22.4907266809058,39.0229435798523));
#64689=CARTESIAN_POINT('Ctrl Pts',(28.6952890445337,22.5091512974628,39.0211255627704));
#64690=CARTESIAN_POINT('Ctrl Pts',(28.8043883830207,22.6008327514987,39.0117622549586));
#64691=CARTESIAN_POINT('Ctrl Pts',(28.8982689392763,22.6668334911248,39.0039334509847));
#64692=CARTESIAN_POINT('Ctrl Pts',(29.0076366686528,22.730429466154,38.9951403796879));
#64693=CARTESIAN_POINT('Ctrl Pts',(29.0180464715703,22.736357762696,38.9943067195587));
#64694=CARTESIAN_POINT('Ctrl Pts',(29.0285070786203,22.742190881106,38.9934724864331));
#64695=CARTESIAN_POINT('',(28.0052501307333,20.9992778085393,38.970454881338));
#64696=CARTESIAN_POINT('Ctrl Pts',(29.0285070491141,22.7421908646526,38.8351573073316));
#64697=CARTESIAN_POINT('Ctrl Pts',(28.9676751363981,22.7082693376882,38.8396123067325));
#64698=CARTESIAN_POINT('Ctrl Pts',(28.9087114018273,22.6712078571221,38.8440673061334));
#64699=CARTESIAN_POINT('Ctrl Pts',(28.8519426650187,22.6312547066892,38.8485223055344));
#64700=CARTESIAN_POINT('Ctrl Pts',(28.8403873084475,22.6231221864791,38.8494291269558));
#64701=CARTESIAN_POINT('Ctrl Pts',(28.8289227839801,22.614869985163,38.8503359483772));
#64702=CARTESIAN_POINT('Ctrl Pts',(28.8175516689289,22.6065003911756,38.8512427697985));
#64703=CARTESIAN_POINT('Ctrl Pts',(28.7621838466573,22.5657474667445,38.8556582318764));
#64704=CARTESIAN_POINT('Ctrl Pts',(28.7088067554031,22.5220413849772,38.8600736939542));
#64705=CARTESIAN_POINT('Ctrl Pts',(28.6577568306917,22.4756052442795,38.864489156032));
#64706=CARTESIAN_POINT('Ctrl Pts',(28.6067094902745,22.429171454313,38.8689043945864));
#64707=CARTESIAN_POINT('Ctrl Pts',(28.5579895074002,22.3800081452107,38.8733196331408));
#64708=CARTESIAN_POINT('Ctrl Pts',(28.5119039421239,22.3283816036943,38.8777348716952));
#64709=CARTESIAN_POINT('Ctrl Pts',(28.4659385855046,22.2768897238054,38.8821385936306));
#64710=CARTESIAN_POINT('Ctrl Pts',(28.422594285554,22.2229477866579,38.8865423155661));
#64711=CARTESIAN_POINT('Ctrl Pts',(28.3821406240037,22.1668584327162,38.8909460375015));
#64712=CARTESIAN_POINT('Ctrl Pts',(28.3417112466882,22.1108027490774,38.8953471158933));
#64713=CARTESIAN_POINT('Ctrl Pts',(28.3041693581068,22.0526026086582,38.8997481942851));
#64714=CARTESIAN_POINT('Ctrl Pts',(28.2697438215374,21.9925931288257,38.9041492726769));
#64715=CARTESIAN_POINT('Ctrl Pts',(28.2353267479062,21.9325984013129,38.9085492691378));
#64716=CARTESIAN_POINT('Ctrl Pts',(28.2040247535269,21.8707956500677,38.9129492655986));
#64717=CARTESIAN_POINT('Ctrl Pts',(28.1760219557701,21.8075466900851,38.9173492620595));
#64718=CARTESIAN_POINT('Ctrl Pts',(28.1478570483352,21.7439315785259,38.9217747303327));
#64719=CARTESIAN_POINT('Ctrl Pts',(28.1230298891774,21.6788539153757,38.9262001986059));
#64720=CARTESIAN_POINT('Ctrl Pts',(28.1016788534891,21.6127025275038,38.9306256668791));
#64721=CARTESIAN_POINT('Ctrl Pts',(28.0804264062742,21.5468565938703,38.9350307005389));
#64722=CARTESIAN_POINT('Ctrl Pts',(28.0626181345658,21.4799473286767,38.9394357341986));
#64723=CARTESIAN_POINT('Ctrl Pts',(28.0483398485905,21.412371453789,38.9438407678584));
#64724=CARTESIAN_POINT('Ctrl Pts',(28.033962208804,21.3443253599466,38.9482764534383));
#64725=CARTESIAN_POINT('Ctrl Pts',(28.0231639545741,21.2756038496504,38.9527121390182));
#64726=CARTESIAN_POINT('Ctrl Pts',(28.0159796898694,21.2066179360303,38.9571478245982));
#64727=CARTESIAN_POINT('Ctrl Pts',(28.0087954251648,21.1376320224102,38.9615835101781));
#64728=CARTESIAN_POINT('Ctrl Pts',(28.0052251117498,21.0683822176057,38.966019195758));
#64729=CARTESIAN_POINT('Ctrl Pts',(28.0052501307333,20.9992778085393,38.970454881338));
#64730=CARTESIAN_POINT('Ctrl Pts',(28.0052501307336,20.9992778076475,38.9704548813952));
#64731=CARTESIAN_POINT('Ctrl Pts',(28.0052646428238,20.9591943177361,38.9730277672733));
#64732=CARTESIAN_POINT('Ctrl Pts',(28.0064872516091,20.9191342037145,38.9756006531513));
#64733=CARTESIAN_POINT('Ctrl Pts',(28.0089142811437,20.8791479306482,38.9781735390294));
#64734=CARTESIAN_POINT('Ctrl Pts',(28.013116765964,20.8099103283949,38.982628579107));
#64735=CARTESIAN_POINT('Ctrl Pts',(28.0209433109417,20.7407558325127,38.9870836191846));
#64736=CARTESIAN_POINT('Ctrl Pts',(28.0323858767816,20.6720941833217,38.9915386592623));
#64737=CARTESIAN_POINT('Ctrl Pts',(28.0438113043172,20.603535373324,38.9959870267253));
#64738=CARTESIAN_POINT('Ctrl Pts',(28.0588419233784,20.5354684236485,39.0004353941882));
#64739=CARTESIAN_POINT('Ctrl Pts',(28.0774177922863,20.4682996924181,39.0048837616512));
#64740=CARTESIAN_POINT('Ctrl Pts',(28.0959718697999,20.4012097569798,39.0093269107241));
#64741=CARTESIAN_POINT('Ctrl Pts',(28.118062807048,20.3350164165094,39.0137700597971));
#64742=CARTESIAN_POINT('Ctrl Pts',(28.1435796335573,20.2701157724975,39.01821320887));
#64743=CARTESIAN_POINT('Ctrl Pts',(28.1690804603916,20.205255822779,39.0226535719796));
#64744=CARTESIAN_POINT('Ctrl Pts',(28.1980027363842,20.1416874158493,39.0270939350893));
#64745=CARTESIAN_POINT('Ctrl Pts',(28.2301861559739,20.0797899587629,39.0315342981989));
#64746=CARTESIAN_POINT('Ctrl Pts',(28.2623603173653,20.0179103077064,39.0359733839502));
#64747=CARTESIAN_POINT('Ctrl Pts',(28.2977935343363,19.9577010861296,39.0404124697014));
#64748=CARTESIAN_POINT('Ctrl Pts',(28.3362787869917,19.8995186108406,39.0448515554526));
#64749=CARTESIAN_POINT('Ctrl Pts',(28.3747660283493,19.8413331290073,39.0492908705909));
#64750=CARTESIAN_POINT('Ctrl Pts',(28.4163053465543,19.7851750081495,39.0537301857292));
#64751=CARTESIAN_POINT('Ctrl Pts',(28.4606464741506,19.7313714945047,39.0581695008675));
#64752=CARTESIAN_POINT('Ctrl Pts',(28.505034460367,19.6775111226217,39.0626135073655));
#64753=CARTESIAN_POINT('Ctrl Pts',(28.5522298537989,19.6260107026534,39.0670575138636));
#64754=CARTESIAN_POINT('Ctrl Pts',(28.6019427969031,19.5771635303491,39.0715015203616));
#64755=CARTESIAN_POINT('Ctrl Pts',(28.6516848577964,19.5282877473535,39.0759481297963));
#64756=CARTESIAN_POINT('Ctrl Pts',(28.7039470367298,19.4820686294349,39.0803947392311));
#64757=CARTESIAN_POINT('Ctrl Pts',(28.7584054791707,19.4387599132912,39.0848413486658));
#64758=CARTESIAN_POINT('Ctrl Pts',(28.8129582608405,19.3953761727673,39.0892956610331));
#64759=CARTESIAN_POINT('Ctrl Pts',(28.86971450213,19.3549131818436,39.0937499734003));
#64760=CARTESIAN_POINT('Ctrl Pts',(28.9283210888019,19.3175815402245,39.0982042857675));
#64761=CARTESIAN_POINT('Ctrl Pts',(28.9585829064826,19.2983051517407,39.1005042932651));
#64762=CARTESIAN_POINT('Ctrl Pts',(28.9893376579779,19.2798629034819,39.1028043007626));
#64763=CARTESIAN_POINT('Ctrl Pts',(29.0205344389625,19.262278855155,39.1051043082601));
#64764=CARTESIAN_POINT('Ctrl Pts',(29.0809615938137,19.2282191227843,39.109559348326));
#64765=CARTESIAN_POINT('Ctrl Pts',(29.1432864519631,19.1972479889171,39.1140143883918));
#64766=CARTESIAN_POINT('Ctrl Pts',(29.2071605495953,19.1695811494683,39.1184694284577));
#64767=CARTESIAN_POINT('Ctrl Pts',(29.2709389786676,19.1419557485177,39.1229177959085));
#64768=CARTESIAN_POINT('Ctrl Pts',(29.3362615963458,19.1176250120267,39.1273661633593));
#64769=CARTESIAN_POINT('Ctrl Pts',(29.4027546014648,19.0967592121782,39.13181453081));
#64770=CARTESIAN_POINT('Ctrl Pts',(29.4691696034795,19.0759178900498,39.1362576798703));
#64771=CARTESIAN_POINT('Ctrl Pts',(29.5367518013512,19.0585335771767,39.1407008289305));
#64772=CARTESIAN_POINT('Ctrl Pts',(29.6051083039763,19.0447281235308,39.1451439779907));
#64773=CARTESIAN_POINT('Ctrl Pts',(29.6734219453948,19.0309313262434,39.1495843410873));
#64774=CARTESIAN_POINT('Ctrl Pts',(29.7425084498925,19.0207090330657,39.1540247041839));
#64775=CARTESIAN_POINT('Ctrl Pts',(29.8119621623945,19.0141325990569,39.1584650672805));
#64776=CARTESIAN_POINT('Ctrl Pts',(29.881395895155,19.0075580568901,39.1629041530183));
#64777=CARTESIAN_POINT('Ctrl Pts',(29.9511961393392,19.0046273378733,39.1673432387562));
#64778=CARTESIAN_POINT('Ctrl Pts',(30.0209512698956,19.0053600307851,39.171782324494));
#64779=CARTESIAN_POINT('Ctrl Pts',(30.0907100050019,19.0060927615582,39.1762216396187));
#64780=CARTESIAN_POINT('Ctrl Pts',(30.1604231326141,19.0104892725408,39.1806609547433));
#64781=CARTESIAN_POINT('Ctrl Pts',(30.2296799620765,19.0185170509135,39.185100269868));
#64782=CARTESIAN_POINT('Ctrl Pts',(30.2990099804584,19.0265533128455,39.1895442763521));
#64783=CARTESIAN_POINT('Ctrl Pts',(30.3678822512674,19.0382284448406,39.1939882828361));
#64784=CARTESIAN_POINT('Ctrl Pts',(30.4358931020272,19.0534582547232,39.1984322893201));
#64785=CARTESIAN_POINT('Ctrl Pts',(30.5039437879954,19.0686969849862,39.2028788987407));
#64786=CARTESIAN_POINT('Ctrl Pts',(30.5711315783388,19.0874944053553,39.2073255081612));
#64787=CARTESIAN_POINT('Ctrl Pts',(30.6370675653063,19.1097162964955,39.2117721175817));
#64788=CARTESIAN_POINT('Ctrl Pts',(30.7031177742337,19.1319766829715,39.2162264299346));
#64789=CARTESIAN_POINT('Ctrl Pts',(30.7679113964543,19.1576732013188,39.2206807422874));
#64790=CARTESIAN_POINT('Ctrl Pts',(30.8310798655559,19.1866236409483,39.2251350546402));
#64791=CARTESIAN_POINT('Ctrl Pts',(30.8636972368969,19.2015723527552,39.2274350622571));
#64792=CARTESIAN_POINT('Ctrl Pts',(30.8958817114017,19.2173878829902,39.229735069874));
#64793=CARTESIAN_POINT('Ctrl Pts',(30.9275854478883,19.2340405442463,39.2320350774909));
#64794=CARTESIAN_POINT('Ctrl Pts',(30.9889945562375,19.2662962084899,39.2364901175777));
#64795=CARTESIAN_POINT('Ctrl Pts',(31.0488401240088,19.3018223558264,39.2409451576645));
#64796=CARTESIAN_POINT('Ctrl Pts',(31.1067518297036,19.3404434478006,39.2454001977513));
#64797=CARTESIAN_POINT('Ctrl Pts',(31.1645767971218,19.3790066943546,39.2498485652234));
#64798=CARTESIAN_POINT('Ctrl Pts',(31.2204732475762,19.4206554157403,39.2542969326955));
#64799=CARTESIAN_POINT('Ctrl Pts',(31.2740952507473,19.4651681347707,39.2587453001676));
#64800=CARTESIAN_POINT('Ctrl Pts',(31.3276543498231,19.509628635828,39.2631884492496));
#64801=CARTESIAN_POINT('Ctrl Pts',(31.3789439263179,19.5569461504788,39.2676315983316));
#64802=CARTESIAN_POINT('Ctrl Pts',(31.427648350918,19.606856881501,39.2720747474136));
#64803=CARTESIAN_POINT('Ctrl Pts',(31.4763222366504,19.6567363172717,39.2765151105322));
#64804=CARTESIAN_POINT('Ctrl Pts',(31.5224138452266,19.7092053943128,39.2809554736508));
#64805=CARTESIAN_POINT('Ctrl Pts',(31.5656430233468,19.7639621826394,39.2853958367694));
#64806=CARTESIAN_POINT('Ctrl Pts',(31.6088597657366,19.81870321909,39.2898349225296));
#64807=CARTESIAN_POINT('Ctrl Pts',(31.6492154093433,19.8757302764879,39.2942740082897));
#64808=CARTESIAN_POINT('Ctrl Pts',(31.6864700330219,19.9347083074485,39.2987130940498));
#64809=CARTESIAN_POINT('Ctrl Pts',(31.7237265818099,19.9936893860621,39.3031524091969));
#64810=CARTESIAN_POINT('Ctrl Pts',(31.7578815332684,20.0546212234293,39.307591724344));
#64811=CARTESIAN_POINT('Ctrl Pts',(31.7887392283771,20.1171412710037,39.3120310394912));
#64812=CARTESIAN_POINT('Ctrl Pts',(31.8196295331424,20.1797273882334,39.3164750459978));
#64813=CARTESIAN_POINT('Ctrl Pts',(31.8472154099551,20.2439046259247,39.3209190525045));
#64814=CARTESIAN_POINT('Ctrl Pts',(31.8713484101972,20.309288272756,39.3253630590111));
#64815=CARTESIAN_POINT('Ctrl Pts',(31.8954955455828,20.3747102159956,39.3298096684544));
#64816=CARTESIAN_POINT('Ctrl Pts',(31.9161856338551,20.4413395074155,39.3342562778977));
#64817=CARTESIAN_POINT('Ctrl Pts',(31.9333202548722,20.5087766754307,39.3387028873409));
#64818=CARTESIAN_POINT('Ctrl Pts',(31.9504845584657,20.5763306659243,39.3431571997164));
#64819=CARTESIAN_POINT('Ctrl Pts',(31.964081004968,20.6446948467698,39.3476115120919));
#64820=CARTESIAN_POINT('Ctrl Pts',(31.9740625204969,20.7134607746408,39.3520658244674));
#64821=CARTESIAN_POINT('Ctrl Pts',(31.9792165280798,20.7489684200146,39.3543658318855));
#64822=CARTESIAN_POINT('Ctrl Pts',(31.9834075640945,20.7845831134649,39.3566658393035));
#64823=CARTESIAN_POINT('Ctrl Pts',(31.986634587087,20.820248560813,39.3589658467216));
#64824=CARTESIAN_POINT('Ctrl Pts',(31.9928852263902,20.8893313803301,39.3634208868));
#64825=CARTESIAN_POINT('Ctrl Pts',(31.9955404755269,20.9588766803797,39.3678759268784));
#64826=CARTESIAN_POINT('Ctrl Pts',(31.9945467045323,21.028478166011,39.3723309669568));
#64827=CARTESIAN_POINT('Ctrl Pts',(31.9935544219757,21.0979754047903,39.3767793344204));
#64828=CARTESIAN_POINT('Ctrl Pts',(31.9889239738688,21.1675281768276,39.381227701884));
#64829=CARTESIAN_POINT('Ctrl Pts',(31.9806535514527,21.2367257307899,39.3856760693476));
#64830=CARTESIAN_POINT('Ctrl Pts',(31.9723928310883,21.3058421089405,39.390119218421));
#64831=CARTESIAN_POINT('Ctrl Pts',(31.9605006752226,21.3746036131444,39.3945623674944));
#64832=CARTESIAN_POINT('Ctrl Pts',(31.9450272657607,21.4426019633345,39.3990055165678));
#64833=CARTESIAN_POINT('Ctrl Pts',(31.9295635585059,21.5105576768917,39.4034458796777));
#64834=CARTESIAN_POINT('Ctrl Pts',(31.91052316071,21.5777507097199,39.4078862427877));
#64835=CARTESIAN_POINT('Ctrl Pts',(31.88800753798,21.6437818722445,39.4123266058976));
#64836=CARTESIAN_POINT('Ctrl Pts',(31.8654983923157,21.7097940395949,39.416765691649));
#64837=CARTESIAN_POINT('Ctrl Pts',(31.8395161642236,21.7746445372969,39.4212047774004));
#64838=CARTESIAN_POINT('Ctrl Pts',(31.8102119732197,21.8379499832998,39.4256438631518));
#64839=CARTESIAN_POINT('Ctrl Pts',(31.7809062679401,21.9012587005718,39.4300831782902));
#64840=CARTESIAN_POINT('Ctrl Pts',(31.7482784666747,21.9630217646245,39.4345224934285));
#64841=CARTESIAN_POINT('Ctrl Pts',(31.7125268142031,22.0228780343401,39.4389618085669));
#64842=CARTESIAN_POINT('Ctrl Pts',(31.6767373802605,22.082797558696,39.4434058150648));
#64843=CARTESIAN_POINT('Ctrl Pts',(31.6378177576339,22.1408058459857,39.4478498215627));
#64844=CARTESIAN_POINT('Ctrl Pts',(31.5960104338124,22.1965693701837,39.4522938280606));
#64845=CARTESIAN_POINT('Ctrl Pts',(31.5541786226701,22.2523655561066,39.4567404374951));
#64846=CARTESIAN_POINT('Ctrl Pts',(31.509456057548,22.3059139863257,39.4611870469296));
#64847=CARTESIAN_POINT('Ctrl Pts',(31.4621247819541,22.3569151353329,39.4656336563641));
#64848=CARTESIAN_POINT('Ctrl Pts',(31.414711513638,22.4080046344426,39.470087968731));
#64849=CARTESIAN_POINT('Ctrl Pts',(31.3646808653404,22.4565377035091,39.4745422810978));
#64850=CARTESIAN_POINT('Ctrl Pts',(31.3123502908188,22.5022530667927,39.4789965934646));
#64851=CARTESIAN_POINT('Ctrl Pts',(31.2853291248666,22.5258584338107,39.4812966009605));
#64852=CARTESIAN_POINT('Ctrl Pts',(31.2576952644839,22.5487132149282,39.4835966084565));
#64853=CARTESIAN_POINT('Ctrl Pts',(31.2294954200378,22.5707859735196,39.4858966159524));
#64854=CARTESIAN_POINT('Ctrl Pts',(31.1748732340598,22.6135401925059,39.4903516560302));
#64855=CARTESIAN_POINT('Ctrl Pts',(31.1179107266147,22.6535260881525,39.4948066961079));
#64856=CARTESIAN_POINT('Ctrl Pts',(31.0589199879724,22.6904780452797,39.4992617361857));
#64857=CARTESIAN_POINT('Ctrl Pts',(31.0000176037491,22.7273746569614,39.5037101036486));
#64858=CARTESIAN_POINT('Ctrl Pts',(30.9390934290822,22.7612460916392,39.5081584711115));
#64859=CARTESIAN_POINT('Ctrl Pts',(30.8764914303458,22.7918678341413,39.5126068385744));
#64860=CARTESIAN_POINT('Ctrl Pts',(30.8139628701606,22.8224536542057,39.5170499876471));
#64861=CARTESIAN_POINT('Ctrl Pts',(30.7497608326115,22.8497971397991,39.5214931367197));
#64862=CARTESIAN_POINT('Ctrl Pts',(30.6842554343482,22.8737187790768,39.5259362857923));
#64863=CARTESIAN_POINT('Ctrl Pts',(30.6187911095762,22.8976254188999,39.5303766489015));
#64864=CARTESIAN_POINT('Ctrl Pts',(30.5520255039005,22.9181143013995,39.5348170120107));
#64865=CARTESIAN_POINT('Ctrl Pts',(30.4843489416209,22.9350539179182,39.5392573751199));
#64866=CARTESIAN_POINT('Ctrl Pts',(30.4166918478479,22.95198866142,39.5436964608705));
#64867=CARTESIAN_POINT('Ctrl Pts',(30.3481247921238,22.9653760471501,39.5481355466211));
#64868=CARTESIAN_POINT('Ctrl Pts',(30.2790517806338,22.9751348476054,39.5525746323717));
#64869=CARTESIAN_POINT('Ctrl Pts',(30.2099751998398,22.9848941523405,39.5570139475092));
#64870=CARTESIAN_POINT('Ctrl Pts',(30.14039309619,22.9910244334813,39.5614532626468));
#64871=CARTESIAN_POINT('Ctrl Pts',(30.0707163821908,22.9934961138136,39.5658925777843));
#64872=CARTESIAN_POINT('Ctrl Pts',(30.0009660355468,22.9959704061571,39.5703365842813));
#64873=CARTESIAN_POINT('Ctrl Pts',(29.931121368945,22.9947783635379,39.5747805907784));
#64874=CARTESIAN_POINT('Ctrl Pts',(29.8615941230685,22.9899425558872,39.5792245972754));
#64875=CARTESIAN_POINT('Ctrl Pts',(29.7920261538018,22.9851039158148,39.583671206709));
#64876=CARTESIAN_POINT('Ctrl Pts',(29.7227764611,22.9766173223029,39.5881178161426));
#64877=CARTESIAN_POINT('Ctrl Pts',(29.6542497069565,22.9645570231888,39.5925644255762));
#64878=CARTESIAN_POINT('Ctrl Pts',(29.5856042428263,22.9524758318266,39.5970187379421));
#64879=CARTESIAN_POINT('Ctrl Pts',(29.5176846937674,22.9368086873366,39.601473050308));
#64880=CARTESIAN_POINT('Ctrl Pts',(29.4508828238384,22.9176803407618,39.6059273626739));
#64881=CARTESIAN_POINT('Ctrl Pts',(29.4163893286731,22.907803318894,39.608227370177));
#64882=CARTESIAN_POINT('Ctrl Pts',(29.3821935436789,22.8970042653971,39.6105273776801));
#64883=CARTESIAN_POINT('Ctrl Pts',(29.3483472282633,22.8853053406777,39.6128273851832));
#64884=CARTESIAN_POINT('Ctrl Pts',(29.2828030888582,22.8626501138596,39.6172814006518));
#64885=CARTESIAN_POINT('Ctrl Pts',(29.2183127414046,22.8365281678362,39.6217354161204));
#64886=CARTESIAN_POINT('Ctrl Pts',(29.1552684130968,22.8070573063929,39.626189431589));
#64887=CARTESIAN_POINT('Ctrl Pts',(29.112303123076,22.7869726430606,39.6292248841269));
#64888=CARTESIAN_POINT('Ctrl Pts',(29.0700092676253,22.7653336290579,39.6322603366649));
#64889=CARTESIAN_POINT('Ctrl Pts',(29.0285070491141,22.7421908646526,39.6352957892028));
#64890=CARTESIAN_POINT('Origin',(30.,21.,34.5704548813952));
#64891=CARTESIAN_POINT('',(29.0285071367644,22.7421909135288,40.592474930186));
#64892=CARTESIAN_POINT('',(29.0285070491141,22.7421908646526,40.4352302045579));
#64893=CARTESIAN_POINT('',(29.0285070491141,22.7421908646526,34.5704548813952));
#64894=CARTESIAN_POINT('',(28.0052502116719,20.9990810521211,39.9301166301426));
#64895=CARTESIAN_POINT('Ctrl Pts',(29.0285071367644,22.7421909135288,40.592474930186));
#64896=CARTESIAN_POINT('Ctrl Pts',(29.0960687329284,22.7798650903325,40.5879600119655));
#64897=CARTESIAN_POINT('Ctrl Pts',(29.1657938625114,22.8135936960508,40.5835015453423));
#64898=CARTESIAN_POINT('Ctrl Pts',(29.3247841510807,22.879379618777,40.5734612728819));
#64899=CARTESIAN_POINT('Ctrl Pts',(29.4146880486724,22.9092907596867,40.5678627366657));
#64900=CARTESIAN_POINT('Ctrl Pts',(29.5329960975536,22.9395077127843,40.5603706304539));
#64901=CARTESIAN_POINT('Ctrl Pts',(29.5597597683602,22.9457572400108,40.5586683913905));
#64902=CARTESIAN_POINT('Ctrl Pts',(29.6043568641948,22.9552038078342,40.5558153011756));
#64903=CARTESIAN_POINT('Ctrl Pts',(29.6221204769607,22.958714489749,40.5546745677748));
#64904=CARTESIAN_POINT('Ctrl Pts',(29.6573621342639,22.9651821816829,40.5524017752951));
#64905=CARTESIAN_POINT('Ctrl Pts',(29.6748366922898,22.9681490045451,40.5512701446101));
#64906=CARTESIAN_POINT('Ctrl Pts',(29.7175143111167,22.974810920883,40.5484940314886));
#64907=CARTESIAN_POINT('Ctrl Pts',(29.7427525223607,22.9782568016268,40.5468418447261));
#64908=CARTESIAN_POINT('Ctrl Pts',(29.8427293246642,22.9899615858731,40.5402527064019));
#64909=CARTESIAN_POINT('Ctrl Pts',(29.9178357607172,22.9944743417707,40.5352020751141));
#64910=CARTESIAN_POINT('Ctrl Pts',(30.1669081109147,22.9953470928876,40.5181527011763));
#64911=CARTESIAN_POINT('Ctrl Pts',(30.3401244480812,22.9732154522397,40.5057420662623));
#64912=CARTESIAN_POINT('Ctrl Pts',(30.5321243766572,22.9226231325099,40.4924105970826));
#64913=CARTESIAN_POINT('Ctrl Pts',(30.5558605981998,22.9158954009407,40.4907718030728));
#64914=CARTESIAN_POINT('Ctrl Pts',(30.590924269536,22.9052504912435,40.4883709020529));
#64915=CARTESIAN_POINT('Ctrl Pts',(30.6023502095324,22.9016690483001,40.4875917246693));
#64916=CARTESIAN_POINT('Ctrl Pts',(30.6220567253492,22.8952966333065,40.4862542248366));
#64917=CARTESIAN_POINT('Ctrl Pts',(30.6303519883818,22.8925539028408,40.4856932388778));
#64918=CARTESIAN_POINT('Ctrl Pts',(30.6501852574323,22.8858513939182,40.4843567110806));
#64919=CARTESIAN_POINT('Ctrl Pts',(30.6617053213933,22.8818401724716,40.4835841585812));
#64920=CARTESIAN_POINT('Ctrl Pts',(30.6975577794693,22.868986600885,40.4811894916869));
#64921=CARTESIAN_POINT('Ctrl Pts',(30.7217562832923,22.8597757344726,40.4795871810929));
#64922=CARTESIAN_POINT('Ctrl Pts',(30.7799113448541,22.8363335475747,40.4757547316584));
#64923=CARTESIAN_POINT('Ctrl Pts',(30.8136672007711,22.8216280035967,40.4735455508008));
#64924=CARTESIAN_POINT('Ctrl Pts',(30.9633523573462,22.7514267949069,40.4637372845584));
#64925=CARTESIAN_POINT('Ctrl Pts',(31.0741638298145,22.6857397442724,40.4564246481082));
#64926=CARTESIAN_POINT('Ctrl Pts',(31.2417254070379,22.5631385717563,40.4442369430036));
#64927=CARTESIAN_POINT('Ctrl Pts',(31.3027207039125,22.5126800779375,40.4395215207509));
#64928=CARTESIAN_POINT('Ctrl Pts',(31.3800497389339,22.4405557518614,40.4330253376262));
#64929=CARTESIAN_POINT('Ctrl Pts',(31.3991764833804,22.421985660879,40.4313725361311));
#64930=CARTESIAN_POINT('Ctrl Pts',(31.4292871360043,22.3915555359962,40.4286914046391));
#64931=CARTESIAN_POINT('Ctrl Pts',(31.440509390113,22.3799352155775,40.4276736852452));
#64932=CARTESIAN_POINT('Ctrl Pts',(31.463639712474,22.3553947909158,40.4255361669615));
#64933=CARTESIAN_POINT('Ctrl Pts',(31.4755206409163,22.3424511361077,40.4244153336846));
#64934=CARTESIAN_POINT('Ctrl Pts',(31.5036181893569,22.311016674992,40.421707932134));
#64935=CARTESIAN_POINT('Ctrl Pts',(31.5196665051278,22.2923799769558,40.4201145510715));
#64936=CARTESIAN_POINT('Ctrl Pts',(31.5780877378331,22.2219431253007,40.4141328358146));
#64937=CARTESIAN_POINT('Ctrl Pts',(31.6181863326005,22.1683224023332,40.4096564473149));
#64938=CARTESIAN_POINT('Ctrl Pts',(31.725666617251,22.0084230824251,40.3965331214788));
#64939=CARTESIAN_POINT('Ctrl Pts',(31.7857908214355,21.8976574936066,40.3876913783191));
#64940=CARTESIAN_POINT('Ctrl Pts',(31.8629083714837,21.7166854304469,40.3740427701163));
#64941=CARTESIAN_POINT('Ctrl Pts',(31.8872314312267,21.6499423692024,40.3691707287951));
#64942=CARTESIAN_POINT('Ctrl Pts',(31.9129709497089,21.5655672104859,40.3633167114285));
#64943=CARTESIAN_POINT('Ctrl Pts',(31.9177824672936,21.5490305822521,40.362183684447));
#64944=CARTESIAN_POINT('Ctrl Pts',(31.925172600491,21.5223480921013,40.3603806678989));
#64945=CARTESIAN_POINT('Ctrl Pts',(31.9278864647504,21.5122410195493,40.359703461862));
#64946=CARTESIAN_POINT('Ctrl Pts',(31.933093199993,21.4922221896989,40.3583741372569));
#64947=CARTESIAN_POINT('Ctrl Pts',(31.9355896658313,21.4823117847147,40.3577218557724));
#64948=CARTESIAN_POINT('Ctrl Pts',(31.9418143625754,21.4567741626826,40.3560549040052));
#64949=CARTESIAN_POINT('Ctrl Pts',(31.9454302644967,21.4411199148273,40.3550463887352));
#64950=CARTESIAN_POINT('Ctrl Pts',(31.961094679351,21.3693614687676,40.3504769146551));
#64951=CARTESIAN_POINT('Ctrl Pts',(31.9709090000554,21.3127925244291,40.3470233104871));
#64952=CARTESIAN_POINT('Ctrl Pts',(31.9974623778437,21.1074972505957,40.3347712016247));
#64953=CARTESIAN_POINT('Ctrl Pts',(31.9999006372939,20.9574316356273,40.3263066742011));
#64954=CARTESIAN_POINT('Ctrl Pts',(31.9798064399963,20.7490886013524,40.3138780160435));
#64955=CARTESIAN_POINT('Ctrl Pts',(31.9714132188086,20.6899693042299,40.3102790028381));
#64956=CARTESIAN_POINT('Ctrl Pts',(31.9558918794299,20.6074379231036,40.3051002091521));
#64957=CARTESIAN_POINT('Ctrl Pts',(31.9509648783114,20.5836419913619,40.3035888610824));
#64958=CARTESIAN_POINT('Ctrl Pts',(31.9417395168266,20.542854328133,40.3009639463476));
#64959=CARTESIAN_POINT('Ctrl Pts',(31.9376495846089,20.525817996923,40.2998571460824));
#64960=CARTESIAN_POINT('Ctrl Pts',(31.9287980722794,20.4909762286221,40.2975711058046));
#64961=CARTESIAN_POINT('Ctrl Pts',(31.9240130756965,20.4731785404145,40.2963912014753));
#64962=CARTESIAN_POINT('Ctrl Pts',(31.9110386121741,20.4274567988189,40.2933274612075));
#64963=CARTESIAN_POINT('Ctrl Pts',(31.9024837135227,20.3996418851171,40.2914319399806));
#64964=CARTESIAN_POINT('Ctrl Pts',(31.8549392864333,20.2562969623157,40.2814929830942));
#64965=CARTESIAN_POINT('Ctrl Pts',(31.8060310704993,20.1443499242521,40.2731275645003));
#64966=CARTESIAN_POINT('Ctrl Pts',(31.6862794250549,19.9269465798762,40.2558454622255));
#64967=CARTESIAN_POINT('Ctrl Pts',(31.6149634027058,19.8223415627265,40.2469606497743));
#64968=CARTESIAN_POINT('Ctrl Pts',(31.5213539423238,19.7096839120542,40.2371868425998));
#64969=CARTESIAN_POINT('Ctrl Pts',(31.5082442616112,19.6943841506517,40.2358551510203));
#64970=CARTESIAN_POINT('Ctrl Pts',(31.4874894521765,19.6708919847042,40.2338070412667));
#64971=CARTESIAN_POINT('Ctrl Pts',(31.4800036834338,19.662561366562,40.2330800831842));
#64972=CARTESIAN_POINT('Ctrl Pts',(31.4658097940107,19.6470306613671,40.2317242908243));
#64973=CARTESIAN_POINT('Ctrl Pts',(31.4591182800737,19.6398168388623,40.2310944118102));
#64974=CARTESIAN_POINT('Ctrl Pts',(31.4427899530334,19.6224731689399,40.2295790970551));
#64975=CARTESIAN_POINT('Ctrl Pts',(31.4330995722738,19.61239463057,40.2286976836892));
#64976=CARTESIAN_POINT('Ctrl Pts',(31.3971688175285,19.5758025783677,40.2254906065939));
#64977=CARTESIAN_POINT('Ctrl Pts',(31.3702906264709,19.5499231089544,40.2232087841669));
#64978=CARTESIAN_POINT('Ctrl Pts',(31.2959178956472,19.4822298783655,40.2171502537228));
#64979=CARTESIAN_POINT('Ctrl Pts',(31.2471330798358,19.4418955730976,40.2134408174098));
#64980=CARTESIAN_POINT('Ctrl Pts',(31.0696822991831,19.3088663539484,40.2005288783621));
#64981=CARTESIAN_POINT('Ctrl Pts',(30.9319860950049,19.2292513045153,40.1914610929956));
#64982=CARTESIAN_POINT('Ctrl Pts',(30.7587912730339,19.1549631985256,40.1799381376238));
#64983=CARTESIAN_POINT('Ctrl Pts',(30.7309985141636,19.1437764086102,40.1780877469968));
#64984=CARTESIAN_POINT('Ctrl Pts',(30.6855559610989,19.1266642968388,40.1750543717657));
#64985=CARTESIAN_POINT('Ctrl Pts',(30.6680560836306,19.1203525160011,40.1738843807477));
#64986=CARTESIAN_POINT('Ctrl Pts',(30.6339863597613,19.1086002712322,40.1716017591842));
#64987=CARTESIAN_POINT('Ctrl Pts',(30.6174283629187,19.103130520251,40.1704902239753));
#64988=CARTESIAN_POINT('Ctrl Pts',(30.5781183392696,19.0907141146697,40.1678452584596));
#64989=CARTESIAN_POINT('Ctrl Pts',(30.5553099898122,19.0839561226298,40.1663058125653));
#64990=CARTESIAN_POINT('Ctrl Pts',(30.4742205382256,19.0614992202077,40.1608134534591));
#64991=CARTESIAN_POINT('Ctrl Pts',(30.4153584522196,19.0480403421593,40.1567904937402));
#64992=CARTESIAN_POINT('Ctrl Pts',(30.2554872697765,19.0190443869337,40.1457719792754));
#64993=CARTESIAN_POINT('Ctrl Pts',(30.1537492991613,19.0085641626037,40.1386556363141));
#64994=CARTESIAN_POINT('Ctrl Pts',(29.9570826895674,19.0034685850981,40.1249336148917));
#64995=CARTESIAN_POINT('Ctrl Pts',(29.8624366157282,19.0077502916956,40.1183482940853));
#64996=CARTESIAN_POINT('Ctrl Pts',(29.7468143079319,19.0212633166416,40.1105608703395));
#64997=CARTESIAN_POINT('Ctrl Pts',(29.7252250232875,19.0241455871365,40.1091182523118));
#64998=CARTESIAN_POINT('Ctrl Pts',(29.6922675017215,19.0290962473652,40.1069378922821));
#64999=CARTESIAN_POINT('Ctrl Pts',(29.6808635097747,19.0309106650382,40.1061874755816));
#65000=CARTESIAN_POINT('Ctrl Pts',(29.660818549599,19.0342786143093,40.1048763293535));
#65001=CARTESIAN_POINT('Ctrl Pts',(29.6521714935312,19.0357902462071,40.1043133769416));
#65002=CARTESIAN_POINT('Ctrl Pts',(29.6310150410694,19.0396327993481,40.1029422502506));
#65003=CARTESIAN_POINT('Ctrl Pts',(29.6185175567197,19.0420263977322,40.1021375686636));
#65004=CARTESIAN_POINT('Ctrl Pts',(29.5777000507225,19.0502496904801,40.0995241565624));
#65005=CARTESIAN_POINT('Ctrl Pts',(29.5494824784796,19.0565757860059,40.0977407422773));
#65006=CARTESIAN_POINT('Ctrl Pts',(29.4796241136988,19.0738407955747,40.0933611912371));
#65007=CARTESIAN_POINT('Ctrl Pts',(29.4381801580459,19.0855185468424,40.0907948025244));
#65008=CARTESIAN_POINT('Ctrl Pts',(29.2422551456768,19.1476359782371,40.0786779397923));
#65009=CARTESIAN_POINT('Ctrl Pts',(29.0939500578891,19.2154818238749,40.0694995621531));
#65010=CARTESIAN_POINT('Ctrl Pts',(28.9158107052753,19.3249677977458,40.0569433889924));
#65011=CARTESIAN_POINT('Ctrl Pts',(28.87697787,19.3507516555636,40.0541058904729));
#65012=CARTESIAN_POINT('Ctrl Pts',(28.8214012657796,19.390526329014,40.049870962468));
#65013=CARTESIAN_POINT('Ctrl Pts',(28.8039257224924,19.4034704080505,40.0485129378575));
#65014=CARTESIAN_POINT('Ctrl Pts',(28.773028841815,19.4271476489753,40.0460620374657));
#65015=CARTESIAN_POINT('Ctrl Pts',(28.7595278143415,19.4377735543045,40.0449734517593));
#65016=CARTESIAN_POINT('Ctrl Pts',(28.7309210098843,19.460893021243,40.0426278421931));
#65017=CARTESIAN_POINT('Ctrl Pts',(28.7158588605419,19.4734374353878,40.0413688306624));
#65018=CARTESIAN_POINT('Ctrl Pts',(28.6744922139242,19.5089348375416,40.0378422189949));
#65019=CARTESIAN_POINT('Ctrl Pts',(28.6486027938534,19.5323585085854,40.0355554233331));
#65020=CARTESIAN_POINT('Ctrl Pts',(28.5912097710309,19.5870919327397,40.0302981622785));
#65021=CARTESIAN_POINT('Ctrl Pts',(28.5601111979405,19.6187980287938,40.0273122730739));
#65022=CARTESIAN_POINT('Ctrl Pts',(28.4492410694052,19.7396507084203,40.0161521445457));
#65023=CARTESIAN_POINT('Ctrl Pts',(28.3764799802037,19.8348768043067,40.0077611379531));
#65024=CARTESIAN_POINT('Ctrl Pts',(28.2708359236142,20.0024142243903,39.9939901212667));
#65025=CARTESIAN_POINT('Ctrl Pts',(28.2329283045117,20.0712127072359,39.988583916848));
#65026=CARTESIAN_POINT('Ctrl Pts',(28.191628135908,20.1579036356095,39.9822076652887));
#65027=CARTESIAN_POINT('Ctrl Pts',(28.1842946609797,20.1738346060227,39.9810533137794));
#65028=CARTESIAN_POINT('Ctrl Pts',(28.1728944992523,20.1994851808,39.9792247396629));
#65029=CARTESIAN_POINT('Ctrl Pts',(28.1686932279146,20.209143498844,39.9785429521871));
#65030=CARTESIAN_POINT('Ctrl Pts',(28.1605872142881,20.2281894502355,39.9772123215074));
#65031=CARTESIAN_POINT('Ctrl Pts',(28.1566774032896,20.2375744414096,39.9765632234225));
#65032=CARTESIAN_POINT('Ctrl Pts',(28.1468729834634,20.261625005888,39.9749155620193));
#65033=CARTESIAN_POINT('Ctrl Pts',(28.1410804630544,20.2763318691068,39.9739228747092));
#65034=CARTESIAN_POINT('Ctrl Pts',(28.1161968059784,20.3417810518088,39.9695640755936));
#65035=CARTESIAN_POINT('Ctrl Pts',(28.0990025554086,20.3932245710578,39.966293504175));
#65036=CARTESIAN_POINT('Ctrl Pts',(28.0318197074381,20.62529508557,39.9519609221912));
#65037=CARTESIAN_POINT('Ctrl Pts',(28.0053365300759,20.8117106669367,39.9414689951905));
#65038=CARTESIAN_POINT('Ctrl Pts',(28.0052502116719,20.9990810521211,39.9301166301426));
#65039=CARTESIAN_POINT('Ctrl Pts',(28.005250210651,20.9990832709263,39.9301164957099));
#65040=CARTESIAN_POINT('Ctrl Pts',(28.0052354568568,21.0311866794835,39.9281714189102));
#65041=CARTESIAN_POINT('Ctrl Pts',(28.0059957083417,21.0632847101422,39.9262061723218));
#65042=CARTESIAN_POINT('Ctrl Pts',(28.0083647951165,21.1127902920397,39.9231358281105));
#65043=CARTESIAN_POINT('Ctrl Pts',(28.0094283613751,21.1302188951357,39.9220473890065));
#65044=CARTESIAN_POINT('Ctrl Pts',(28.0119188963853,21.1637780693675,39.9199358763793));
#65045=CARTESIAN_POINT('Ctrl Pts',(28.0133137609071,21.1799096799813,39.918913879985));
#65046=CARTESIAN_POINT('Ctrl Pts',(28.0166746677519,21.2139452218374,39.9167419279425));
#65047=CARTESIAN_POINT('Ctrl Pts',(28.0186871221377,21.2318429993355,39.9155905989823));
#65048=CARTESIAN_POINT('Ctrl Pts',(28.0243199698841,21.2764856162233,39.9126947615763));
#65049=CARTESIAN_POINT('Ctrl Pts',(28.0282412168507,21.303188159405,39.9109409461418));
#65050=CARTESIAN_POINT('Ctrl Pts',(28.0474792090956,21.4179444701417,39.9033064013374));
#65051=CARTESIAN_POINT('Ctrl Pts',(28.0681605298537,21.5049827132208,39.8972608557067));
#65052=CARTESIAN_POINT('Ctrl Pts',(28.1180316848069,21.6659503350148,39.8856420114441));
#65053=CARTESIAN_POINT('Ctrl Pts',(28.1459400045123,21.7401049364899,39.880104935248));
#65054=CARTESIAN_POINT('Ctrl Pts',(28.2028256377524,21.8676716318516,39.8703745597673));
#65055=CARTESIAN_POINT('Ctrl Pts',(28.2299757372047,21.9217942520003,39.8661777875862));
#65056=CARTESIAN_POINT('Ctrl Pts',(28.2772701141578,22.0062530950429,39.8595958008263));
#65057=CARTESIAN_POINT('Ctrl Pts',(28.2958556505021,22.0374179274833,39.857159792246));
#65058=CARTESIAN_POINT('Ctrl Pts',(28.322693410728,22.0797507846873,39.8538579929893));
#65059=CARTESIAN_POINT('Ctrl Pts',(28.3302264135108,22.0913639848687,39.8529529880005));
#65060=CARTESIAN_POINT('Ctrl Pts',(28.3433091531497,22.1110802955399,39.8514191214463));
#65061=CARTESIAN_POINT('Ctrl Pts',(28.3487988375268,22.1192223741704,39.850786499799));
#65062=CARTESIAN_POINT('Ctrl Pts',(28.3607177100019,22.1366213702486,39.8494367108435));
#65063=CARTESIAN_POINT('Ctrl Pts',(28.3671655130134,22.1458647906036,39.8487207798172));
#65064=CARTESIAN_POINT('Ctrl Pts',(28.3855456419138,22.1717439072819,39.8467181298957));
#65065=CARTESIAN_POINT('Ctrl Pts',(28.3976565663506,22.1882517641354,39.8454427528857));
#65066=CARTESIAN_POINT('Ctrl Pts',(28.4840721076974,22.3023164252069,39.8366224074094));
#65067=CARTESIAN_POINT('Ctrl Pts',(28.5669893915256,22.3930374980453,39.8295553376561));
#65068=CARTESIAN_POINT('Ctrl Pts',(28.7203560479146,22.532549413148,39.8175268258092));
#65069=CARTESIAN_POINT('Ctrl Pts',(28.7865492704861,22.5854754778512,39.8126056876589));
#65070=CARTESIAN_POINT('Ctrl Pts',(28.9003002051002,22.665120285285,39.8043199837267));
#65071=CARTESIAN_POINT('Ctrl Pts',(28.945944363292,22.6943822378488,39.801037111244));
#65072=CARTESIAN_POINT('Ctrl Pts',(29.0045791278445,22.7286855139769,39.7968375625133));
#65073=CARTESIAN_POINT('Ctrl Pts',(29.0165085923217,22.7355001992225,39.7959840862754));
#65074=CARTESIAN_POINT('Ctrl Pts',(29.0285070493988,22.7421908648114,39.7951262847314));
#65075=CARTESIAN_POINT('',(28.0052508284892,21.0018180365441,39.7704548813608));
#65076=CARTESIAN_POINT('Ctrl Pts',(29.0285070491141,22.7421908646526,39.6352957892028));
#65077=CARTESIAN_POINT('Ctrl Pts',(28.96774165785,22.7083064318567,39.6397401410411));
#65078=CARTESIAN_POINT('Ctrl Pts',(28.9086745168633,22.6711963538654,39.6441844928793));
#65079=CARTESIAN_POINT('Ctrl Pts',(28.8516654162016,22.6310595470897,39.6486288447176));
#65080=CARTESIAN_POINT('Ctrl Pts',(28.7946982147363,22.5909522391122,39.6530699301515));
#65081=CARTESIAN_POINT('Ctrl Pts',(28.7397864521312,22.5478228956387,39.6575110155855));
#65082=CARTESIAN_POINT('Ctrl Pts',(28.6872624264623,22.5019146532085,39.6619521010195));
#65083=CARTESIAN_POINT('Ctrl Pts',(28.6347591791897,22.4560245719843,39.6663914295692));
#65084=CARTESIAN_POINT('Ctrl Pts',(28.584642162309,22.4073580952149,39.6708307581189));
#65085=CARTESIAN_POINT('Ctrl Pts',(28.5372105475533,22.3561985770199,39.6752700866686));
#65086=CARTESIAN_POINT('Ctrl Pts',(28.4897816008461,22.3050419365695,39.6797091655042));
#65087=CARTESIAN_POINT('Ctrl Pts',(28.4450380877795,22.2513928930657,39.6841482443398));
#65088=CARTESIAN_POINT('Ctrl Pts',(28.4032410154082,22.195570285523,39.6885873231754));
#65089=CARTESIAN_POINT('Ctrl Pts',(28.3614026648769,22.1396925484126,39.6930307859785));
#65090=CARTESIAN_POINT('Ctrl Pts',(28.3225168610619,22.0816373523696,39.6974742487816));
#65091=CARTESIAN_POINT('Ctrl Pts',(28.2868025451921,22.0217543948229,39.7019177115847));
#65092=CARTESIAN_POINT('Ctrl Pts',(28.2510707672903,21.9618421583134,39.7063633469589));
#65093=CARTESIAN_POINT('Ctrl Pts',(28.2185137948009,21.9001008135688,39.7108089823331));
#65094=CARTESIAN_POINT('Ctrl Pts',(28.1893042843611,21.8369041688671,39.7152546177073));
#65095=CARTESIAN_POINT('Ctrl Pts',(28.1600412481287,21.7735917176884,39.7197083996116));
#65096=CARTESIAN_POINT('Ctrl Pts',(28.1341381106743,21.7088190942514,39.7241621815159));
#65097=CARTESIAN_POINT('Ctrl Pts',(28.1117188940398,21.6429790256094,39.7286159634202));
#65098=CARTESIAN_POINT('Ctrl Pts',(28.0930232327615,21.5880741802737,39.7323300270848));
#65099=CARTESIAN_POINT('Ctrl Pts',(28.0767494597394,21.5324274606828,39.7360440907494));
#65100=CARTESIAN_POINT('Ctrl Pts',(28.0629422857144,21.4762719538526,39.7397581544139));
#65101=CARTESIAN_POINT('Ctrl Pts',(28.0412145886808,21.3879026874869,39.7456028008217));
#65102=CARTESIAN_POINT('Ctrl Pts',(28.0255254144271,21.2979944490804,39.7514474472295));
#65103=CARTESIAN_POINT('Ctrl Pts',(28.016046414538,21.2072576493942,39.7572920936373));
#65104=CARTESIAN_POINT('Ctrl Pts',(28.0089304971288,21.1391412257108,39.7616796895451));
#65105=CARTESIAN_POINT('Ctrl Pts',(28.0053134790015,21.070558160593,39.7660672854529));
#65106=CARTESIAN_POINT('Ctrl Pts',(28.0052508284892,21.0018180365441,39.7704548813608));
#65107=CARTESIAN_POINT('Ctrl Pts',(28.0052508284887,21.0018180360048,39.7704548813952));
#65108=CARTESIAN_POINT('Ctrl Pts',(28.005188142268,20.9330387123611,39.774844979364));
#65109=CARTESIAN_POINT('Ctrl Pts',(28.0086869930047,20.8641639778316,39.7792350773327));
#65110=CARTESIAN_POINT('Ctrl Pts',(28.0157502989284,20.7955967556587,39.7836251753015));
#65111=CARTESIAN_POINT('Ctrl Pts',(28.0228088252637,20.727075931462,39.7880123025846));
#65112=CARTESIAN_POINT('Ctrl Pts',(28.0334269744883,20.6588627054711,39.7923994298677));
#65113=CARTESIAN_POINT('Ctrl Pts',(28.0475556429306,20.5913576196137,39.7967865571509));
#65114=CARTESIAN_POINT('Ctrl Pts',(28.0616798259449,20.5238739645937,39.8011722916529));
#65115=CARTESIAN_POINT('Ctrl Pts',(28.079312214332,20.4570984951133,39.8055580261549));
#65116=CARTESIAN_POINT('Ctrl Pts',(28.1003524606402,20.3914223231958,39.8099437606568));
#65117=CARTESIAN_POINT('Ctrl Pts',(28.1213935848097,20.3257434110742,39.8143296781446));
#65118=CARTESIAN_POINT('Ctrl Pts',(28.145842692668,20.2611643649232,39.8187155956324));
#65119=CARTESIAN_POINT('Ctrl Pts',(28.173549948333,20.1980599952207,39.8231015131202));
#65120=CARTESIAN_POINT('Ctrl Pts',(28.2012858294595,20.1348904298983,39.8274919618728));
#65121=CARTESIAN_POINT('Ctrl Pts',(28.2322863701428,20.0731990405785,39.8318824106254));
#65122=CARTESIAN_POINT('Ctrl Pts',(28.2663545563422,20.0133384378702,39.836272859378));
#65123=CARTESIAN_POINT('Ctrl Pts',(28.3004436157103,19.953441159289,39.8406659981058));
#65124=CARTESIAN_POINT('Ctrl Pts',(28.3376037860427,19.8953773196889,39.8450591368337));
#65125=CARTESIAN_POINT('Ctrl Pts',(28.37759484984,19.8394703402178,39.8494522755615));
#65126=CARTESIAN_POINT('Ctrl Pts',(28.4176522429257,19.7834706332766,39.8538527007613));
#65127=CARTESIAN_POINT('Ctrl Pts',(28.460549579183,19.7296353109768,39.8582531259612));
#65128=CARTESIAN_POINT('Ctrl Pts',(28.5060073039398,19.678253660259,39.862653551161));
#65129=CARTESIAN_POINT('Ctrl Pts',(28.519902843827,19.662547291741,39.8639986753222));
#65130=CARTESIAN_POINT('Ctrl Pts',(28.5340373797176,19.6470699231913,39.8653437994835));
#65131=CARTESIAN_POINT('Ctrl Pts',(28.5484022985648,19.6318290765815,39.8666889236447));
#65132=CARTESIAN_POINT('Ctrl Pts',(28.5959787907883,19.5813515188641,39.8711439637238));
#65133=CARTESIAN_POINT('Ctrl Pts',(28.6462850630246,19.5332591277618,39.8755990038028));
#65134=CARTESIAN_POINT('Ctrl Pts',(28.6990524875787,19.4878614043598,39.8800540438819));
#65135=CARTESIAN_POINT('Ctrl Pts',(28.7517408787924,19.4425316761982,39.8845024113461));
#65136=CARTESIAN_POINT('Ctrl Pts',(28.8068827379929,19.3998889216797,39.8889507788104));
#65137=CARTESIAN_POINT('Ctrl Pts',(28.8641717466803,19.3602067991784,39.8933991462746));
#65138=CARTESIAN_POINT('Ctrl Pts',(28.9213935494979,19.3205712278676,39.8978422953486));
#65139=CARTESIAN_POINT('Ctrl Pts',(28.9807570987089,19.2838896676793,39.9022854444226));
#65140=CARTESIAN_POINT('Ctrl Pts',(29.0419234591962,19.250395214781,39.9067285934966));
#65141=CARTESIAN_POINT('Ctrl Pts',(29.1030514668754,19.216921763726,39.9111689566072));
#65142=CARTESIAN_POINT('Ctrl Pts',(29.1659796151259,19.1866316899739,39.9156093197177));
#65143=CARTESIAN_POINT('Ctrl Pts',(29.2303417765112,19.1597136686059,39.9200496828283));
#65144=CARTESIAN_POINT('Ctrl Pts',(29.2946854228434,19.132803390741,39.9244887685803));
#65145=CARTESIAN_POINT('Ctrl Pts',(29.3604618121782,19.1092634282051,39.9289278543323));
#65146=CARTESIAN_POINT('Ctrl Pts',(29.4272837340643,19.0892348021715,39.9333669400843));
#65147=CARTESIAN_POINT('Ctrl Pts',(29.4941091089309,19.0692051411713,39.9378062552232));
#65148=CARTESIAN_POINT('Ctrl Pts',(29.5619796542283,19.0526873150749,39.9422455703622));
#65149=CARTESIAN_POINT('Ctrl Pts',(29.6304935693411,19.0397723192951,39.9466848855011));
#65150=CARTESIAN_POINT('Ctrl Pts',(29.6990798882816,19.026843675264,39.9511288919996));
#65151=CARTESIAN_POINT('Ctrl Pts',(29.7683104522737,19.0175255515059,39.955572898498));
#65152=CARTESIAN_POINT('Ctrl Pts',(29.8377748049809,19.0118575130034,39.9600169049965));
#65153=CARTESIAN_POINT('Ctrl Pts',(29.9072798442408,19.0061861546262,39.9644635144316));
#65154=CARTESIAN_POINT('Ctrl Pts',(29.9770184555524,19.0041691509635,39.9689101238666));
#65155=CARTESIAN_POINT('Ctrl Pts',(30.0465794144433,19.0057939121921,39.9733567333016));
#65156=CARTESIAN_POINT('Ctrl Pts',(30.1162608748904,19.0074214880204,39.977811045669));
#65157=CARTESIAN_POINT('Ctrl Pts',(30.1857635808322,19.0127033844924,39.9822653580363));
#65158=CARTESIAN_POINT('Ctrl Pts',(30.2546814693548,19.0215751437906,39.9867196704037));
#65159=CARTESIAN_POINT('Ctrl Pts',(30.2902675815907,19.0261561231108,39.9890196778942));
#65160=CARTESIAN_POINT('Ctrl Pts',(30.3256979326675,19.0316934036972,39.9913196853848));
#65161=CARTESIAN_POINT('Ctrl Pts',(30.3609180206438,19.0381728555057,39.9936196928754));
#65162=CARTESIAN_POINT('Ctrl Pts',(30.4291381913059,19.0507233439789,39.9980747329548));
#65163=CARTESIAN_POINT('Ctrl Pts',(30.4968372954426,19.0668612003423,40.0025297730341));
#65164=CARTESIAN_POINT('Ctrl Pts',(30.563609577007,19.0865288590611,40.0069848131134));
#65165=CARTESIAN_POINT('Ctrl Pts',(30.6302818492097,19.1061670601974,40.011433180578));
#65166=CARTESIAN_POINT('Ctrl Pts',(30.6960295884878,19.1293244333095,40.0158815480425));
#65167=CARTESIAN_POINT('Ctrl Pts',(30.7604566771772,19.1558923012371,40.020329915507));
#65168=CARTESIAN_POINT('Ctrl Pts',(30.8248081862986,19.1824290023368,40.0247730645813));
#65169=CARTESIAN_POINT('Ctrl Pts',(30.8878416717185,19.2123680662701,40.0292162136556));
#65170=CARTESIAN_POINT('Ctrl Pts',(30.9491773723481,19.24555140334,40.0336593627299));
#65171=CARTESIAN_POINT('Ctrl Pts',(31.0104746139893,19.2787139336437,40.0380997258407));
#65172=CARTESIAN_POINT('Ctrl Pts',(31.0700757533565,19.3151164692266,40.0425400889516));
#65173=CARTESIAN_POINT('Ctrl Pts',(31.1276235714594,19.3545539681931,40.0469804520625));
#65174=CARTESIAN_POINT('Ctrl Pts',(31.1851548347903,19.3939801221803,40.0514195378148));
#65175=CARTESIAN_POINT('Ctrl Pts',(31.2406335460804,19.436439229852,40.055858623567));
#65176=CARTESIAN_POINT('Ctrl Pts',(31.2937310600872,19.4816826726057,40.0602977093193));
#65177=CARTESIAN_POINT('Ctrl Pts',(31.3468313178745,19.5269284532858,40.0647370244586));
#65178=CARTESIAN_POINT('Ctrl Pts',(31.397549763227,19.5749585355209,40.0691763395978));
#65179=CARTESIAN_POINT('Ctrl Pts',(31.4455918414855,19.6254848890134,40.0736156547371));
#65180=CARTESIAN_POINT('Ctrl Pts',(31.4936846894358,19.6760646375189,40.0780596612358));
#65181=CARTESIAN_POINT('Ctrl Pts',(31.5390951874425,19.7291455671678,40.0825036677346));
#65182=CARTESIAN_POINT('Ctrl Pts',(31.5815672728679,19.7844044571104,40.0869476742334));
#65183=CARTESIAN_POINT('Ctrl Pts',(31.6240642349772,19.8396957132041,40.0913942836687));
#65184=CARTESIAN_POINT('Ctrl Pts',(31.6636190813938,19.8971670655199,40.0958408931041));
#65185=CARTESIAN_POINT('Ctrl Pts',(31.7000191319871,19.956466333376,40.1002875025394));
#65186=CARTESIAN_POINT('Ctrl Pts',(31.7364822389673,20.0158683262974,40.1047418149071));
#65187=CARTESIAN_POINT('Ctrl Pts',(31.7697794075027,20.0771041257262,40.1091961272747));
#65188=CARTESIAN_POINT('Ctrl Pts',(31.7997443183266,20.1397977266066,40.1136504396423));
#65189=CARTESIAN_POINT('Ctrl Pts',(31.815216856753,20.1721698953213,40.1159504471303));
#65190=CARTESIAN_POINT('Ctrl Pts',(31.8298017323675,20.2049304303304,40.1182504546183));
#65191=CARTESIAN_POINT('Ctrl Pts',(31.8434812225516,20.2380258898101,40.1205504621063));
#65192=CARTESIAN_POINT('Ctrl Pts',(31.8699779523889,20.3021307238994,40.1250055021854));
#65193=CARTESIAN_POINT('Ctrl Pts',(31.8931791300075,20.367745542848,40.1294605422646));
#65194=CARTESIAN_POINT('Ctrl Pts',(31.9129128146097,20.4344983411148,40.1339155823438));
#65195=CARTESIAN_POINT('Ctrl Pts',(31.932616942738,20.5011511592013,40.1383639498082));
#65196=CARTESIAN_POINT('Ctrl Pts',(31.9488637482724,20.5689381082344,40.1428123172725));
#65197=CARTESIAN_POINT('Ctrl Pts',(31.9615294465421,20.6374675285603,40.1472606847369));
#65198=CARTESIAN_POINT('Ctrl Pts',(31.9741802866517,20.7059165568633,40.151703833811));
#65199=CARTESIAN_POINT('Ctrl Pts',(31.9832582748551,20.7751058476765,40.1561469828851));
#65200=CARTESIAN_POINT('Ctrl Pts',(31.988690003011,20.8446306515937,40.1605901319593));
#65201=CARTESIAN_POINT('Ctrl Pts',(31.9941183253401,20.9141118617539,40.16503049507));
#65202=CARTESIAN_POINT('Ctrl Pts',(31.9959048851972,20.9839276809806,40.1694708581806));
#65203=CARTESIAN_POINT('Ctrl Pts',(31.9940279428916,21.0536668004215,40.1739112212913));
#65204=CARTESIAN_POINT('Ctrl Pts',(31.9921515405257,21.1233858580206,40.1783503070435));
#65205=CARTESIAN_POINT('Ctrl Pts',(31.9866137413496,21.1930277707646,40.1827893927956));
#65206=CARTESIAN_POINT('Ctrl Pts',(31.9774449139628,21.2621815682738,40.1872284785477));
#65207=CARTESIAN_POINT('Ctrl Pts',(31.9682756127827,21.3313389392618,40.1916677936868));
#65208=CARTESIAN_POINT('Ctrl Pts',(31.9554749775831,21.40000766021,40.1961071088259));
#65209=CARTESIAN_POINT('Ctrl Pts',(31.9391249825634,21.4677839934184,40.200546423965));
#65210=CARTESIAN_POINT('Ctrl Pts',(31.9227577092693,21.535631950996,40.2049904304636));
#65211=CARTESIAN_POINT('Ctrl Pts',(31.9028337047619,21.6025851620144,40.2094344369622));
#65212=CARTESIAN_POINT('Ctrl Pts',(31.8794853934634,21.6682531094261,40.2138784434608));
#65213=CARTESIAN_POINT('Ctrl Pts',(31.8561234066284,21.7339595197657,40.2183250528959));
#65214=CARTESIAN_POINT('Ctrl Pts',(31.8293333088405,21.798378716223,40.2227716623311));
#65215=CARTESIAN_POINT('Ctrl Pts',(31.7992953972322,21.8611408920722,40.2272182717663));
#65216=CARTESIAN_POINT('Ctrl Pts',(31.7692054504717,21.9240117918375,40.2316725841338));
#65217=CARTESIAN_POINT('Ctrl Pts',(31.7358566933557,21.9852195116337,40.2361268965012));
#65218=CARTESIAN_POINT('Ctrl Pts',(31.6994745999223,22.0444202443074,40.2405812088687));
#65219=CARTESIAN_POINT('Ctrl Pts',(31.6806885156796,22.0749888522756,40.2428812163581));
#65220=CARTESIAN_POINT('Ctrl Pts',(31.6610943714265,22.1050228457397,40.2451812238476));
#65221=CARTESIAN_POINT('Ctrl Pts',(31.6407274259471,22.1344783277988,40.247481231337));
#65222=CARTESIAN_POINT('Ctrl Pts',(31.6012773116242,22.191532643373,40.2519362714162));
#65223=CARTESIAN_POINT('Ctrl Pts',(31.5587699647844,22.2466391273221,40.2563913114954));
#65224=CARTESIAN_POINT('Ctrl Pts',(31.5134244487598,22.2994514228689,40.2608463515746));
#65225=CARTESIAN_POINT('Ctrl Pts',(31.4681468497813,22.3521846178689,40.265294719039));
#65226=CARTESIAN_POINT('Ctrl Pts',(31.4200398349791,22.4026300762978,40.2697430865033));
#65227=CARTESIAN_POINT('Ctrl Pts',(31.3693651170561,22.4504712126375,40.2741914539677));
#65228=CARTESIAN_POINT('Ctrl Pts',(31.3187498457626,22.4982562264287,40.2786346030418));
#65229=CARTESIAN_POINT('Ctrl Pts',(31.2655732081003,22.5434426518239,40.283077752116));
#65230=CARTESIAN_POINT('Ctrl Pts',(31.2101352588555,22.5857491030345,40.2875209011901));
#65231=CARTESIAN_POINT('Ctrl Pts',(31.1547320705643,22.6280290270627,40.2919612643008));
#65232=CARTESIAN_POINT('Ctrl Pts',(31.097070771626,22.667432263163,40.2964016274115));
#65233=CARTESIAN_POINT('Ctrl Pts',(31.037484976151,22.7037172555213,40.3008419905222));
#65234=CARTESIAN_POINT('Ctrl Pts',(30.9779163217127,22.7399918097814,40.3052810762743));
#65235=CARTESIAN_POINT('Ctrl Pts',(30.9164246874985,22.7731496467442,40.3097201620265));
#65236=CARTESIAN_POINT('Ctrl Pts',(30.8533716928697,22.8029931548147,40.3141592477786));
#65237=CARTESIAN_POINT('Ctrl Pts',(30.7903154400174,22.8328382050296,40.3185985629177));
#65238=CARTESIAN_POINT('Ctrl Pts',(30.7256981098559,22.8593683791901,40.3230378780568));
#65239=CARTESIAN_POINT('Ctrl Pts',(30.6599032643427,22.8824333306149,40.3274771931959));
#65240=CARTESIAN_POINT('Ctrl Pts',(30.594038888448,22.9055226565155,40.3319211996945));
#65241=CARTESIAN_POINT('Ctrl Pts',(30.526994976218,22.9251392885967,40.3363652061931));
#65242=CARTESIAN_POINT('Ctrl Pts',(30.4591713762641,22.9411824256673,40.3408092126917));
#65243=CARTESIAN_POINT('Ctrl Pts',(30.3913080507767,22.9572349594992,40.3452558221269));
#65244=CARTESIAN_POINT('Ctrl Pts',(30.322664610131,22.9697097447899,40.3497024315621));
#65245=CARTESIAN_POINT('Ctrl Pts',(30.2536495004518,22.9785574273749,40.3541490409973));
#65246=CARTESIAN_POINT('Ctrl Pts',(30.1845148347999,22.9874204369413,40.3586033533648));
#65247=CARTESIAN_POINT('Ctrl Pts',(30.1150077027371,22.9926437650225,40.3630576657322));
#65248=CARTESIAN_POINT('Ctrl Pts',(30.0455392424493,22.9942301120726,40.3675119780997));
#65249=CARTESIAN_POINT('Ctrl Pts',(30.0096688396229,22.9950492306694,40.3698119855891));
#65250=CARTESIAN_POINT('Ctrl Pts',(29.9738087108839,22.9948995004175,40.3721119930784));
#65251=CARTESIAN_POINT('Ctrl Pts',(29.9380148627151,22.9937867000398,40.3744120005678));
#65252=CARTESIAN_POINT('Ctrl Pts',(29.8686813887232,22.9916311811452,40.3788671658435));
#65253=CARTESIAN_POINT('Ctrl Pts',(29.7993239332432,22.9858505246595,40.3833223311191));
#65254=CARTESIAN_POINT('Ctrl Pts',(29.7303523298611,22.9764406635385,40.3877774963948));
#65255=CARTESIAN_POINT('Ctrl Pts',(29.6614987482632,22.9670469042413,40.3922250381482));
#65256=CARTESIAN_POINT('Ctrl Pts',(29.5930301878976,22.9540363429594,40.3966725799016));
#65257=CARTESIAN_POINT('Ctrl Pts',(29.5253543733448,22.9374568618674,40.401120121655));
#65258=CARTESIAN_POINT('Ctrl Pts',(29.4577458049611,22.9208938550004,40.4055632441022));
#65259=CARTESIAN_POINT('Ctrl Pts',(29.3909288925793,22.9007690785748,40.4100063665495));
#65260=CARTESIAN_POINT('Ctrl Pts',(29.3253028373582,22.877181744324,40.4144494889967));
#65261=CARTESIAN_POINT('Ctrl Pts',(29.2597185852575,22.8536094349617,40.4188897812207));
#65262=CARTESIAN_POINT('Ctrl Pts',(29.1953241446342,22.82657910902,40.4233300734448));
#65263=CARTESIAN_POINT('Ctrl Pts',(29.1325034769165,22.7962397793552,40.4277703656688));
#65264=CARTESIAN_POINT('Ctrl Pts',(29.0973232052565,22.7792494177693,40.4302569786319));
#65265=CARTESIAN_POINT('Ctrl Pts',(29.0626361878621,22.7612221995001,40.4327435915949));
#65266=CARTESIAN_POINT('Ctrl Pts',(29.0285070491141,22.7421908646526,40.4352302045579));
#65267=CARTESIAN_POINT('Origin',(30.,21.,34.5704548813952));
#65268=CARTESIAN_POINT('',(29.0285070491341,22.7421908646638,41.392186712139));
#65269=CARTESIAN_POINT('',(29.0285070491141,22.7421908646526,41.2351467212172));
#65270=CARTESIAN_POINT('',(29.0285070491141,22.7421908646526,34.5704548813952));
#65271=CARTESIAN_POINT('Ctrl Pts',(29.0285070491341,22.7421908646638,41.392186712139));
#65272=CARTESIAN_POINT('Ctrl Pts',(29.0783988147974,22.7700118684534,41.3882464250647));
#65273=CARTESIAN_POINT('Ctrl Pts',(29.1294676353672,22.7956796508801,41.3843557908295));
#65274=CARTESIAN_POINT('Ctrl Pts',(29.1962551987017,22.825727547167,41.3795065614409));
#65275=CARTESIAN_POINT('Ctrl Pts',(29.2110179528093,22.8321556023395,41.3784492427945));
#65276=CARTESIAN_POINT('Ctrl Pts',(29.2352826800822,22.8423733524512,41.3767369552561));
#65277=CARTESIAN_POINT('Ctrl Pts',(29.2447385844778,22.8462698496204,41.3760759583762));
#65278=CARTESIAN_POINT('Ctrl Pts',(29.2639220336912,22.8540027282305,41.3747482377556));
#65279=CARTESIAN_POINT('Ctrl Pts',(29.273650556896,22.8578356728283,41.3740817146443));
#65280=CARTESIAN_POINT('Ctrl Pts',(29.299442411749,22.8677638470503,41.3723314490789));
#65281=CARTESIAN_POINT('Ctrl Pts',(29.3155554921175,22.8737284982767,41.3712550948816));
#65282=CARTESIAN_POINT('Ctrl Pts',(29.3976470125942,22.902916358766,41.3658479894058));
#65283=CARTESIAN_POINT('Ctrl Pts',(29.4647436332688,22.9228682767636,41.3616769625914));
#65284=CARTESIAN_POINT('Ctrl Pts',(29.6558376539838,22.9689104467555,41.350134650315));
#65285=CARTESIAN_POINT('Ctrl Pts',(29.7814617199492,22.9867807798648,41.3429173419661));
#65286=CARTESIAN_POINT('Ctrl Pts',(29.9749843992764,22.9957222222231,41.3314614568032));
#65287=CARTESIAN_POINT('Ctrl Pts',(30.0421430316378,22.9954336933537,41.3274282679224));
#65288=CARTESIAN_POINT('Ctrl Pts',(30.1337345118057,22.9904141798851,41.3217745626348));
#65289=CARTESIAN_POINT('Ctrl Pts',(30.1582860397527,22.9886123235188,41.3202441914261));
#65290=CARTESIAN_POINT('Ctrl Pts',(30.2002965755275,22.9847462479271,41.3175969133747));
#65291=CARTESIAN_POINT('Ctrl Pts',(30.217773512646,22.9829047006894,41.3164870911432));
#65292=CARTESIAN_POINT('Ctrl Pts',(30.2512602343165,22.9789281603819,41.3143432623251));
#65293=CARTESIAN_POINT('Ctrl Pts',(30.267272949745,22.9768291565714,41.3133104767029));
#65294=CARTESIAN_POINT('Ctrl Pts',(30.3096169904497,22.9707546713981,41.3105582895207));
#65295=CARTESIAN_POINT('Ctrl Pts',(30.3358964648287,22.966446059951,41.3088285131224));
#65296=CARTESIAN_POINT('Ctrl Pts',(30.4396008200475,22.9473039770417,41.3019129629953));
#65297=CARTESIAN_POINT('Ctrl Pts',(30.5161952487708,22.9284142448369,41.296602652232));
#65298=CARTESIAN_POINT('Ctrl Pts',(30.7144745279476,22.8668540138849,41.2823521968396));
#65299=CARTESIAN_POINT('Ctrl Pts',(30.8334886344292,22.8168411497006,41.2732627458577));
#65300=CARTESIAN_POINT('Ctrl Pts',(30.9945703783259,22.7299702955147,41.2606589141987));
#65301=CARTESIAN_POINT('Ctrl Pts',(31.0412288178922,22.7022958172686,41.2569727124745));
#65302=CARTESIAN_POINT('Ctrl Pts',(31.0999597343551,22.6641412120747,41.2523381714851));
#65303=CARTESIAN_POINT('Ctrl Pts',(31.1131119502518,22.6553728326301,41.251300720779));
#65304=CARTESIAN_POINT('Ctrl Pts',(31.1345503416056,22.6407091277087,41.2496121302984));
#65305=CARTESIAN_POINT('Ctrl Pts',(31.1428979450318,22.6349052639044,41.2489552648657));
#65306=CARTESIAN_POINT('Ctrl Pts',(31.1598021219504,22.6229594945695,41.24762697227));
#65307=CARTESIAN_POINT('Ctrl Pts',(31.1683550821845,22.6168131918126,41.2469558550686));
#65308=CARTESIAN_POINT('Ctrl Pts',(31.1910177415001,22.6002536667147,41.245178991534));
#65309=CARTESIAN_POINT('Ctrl Pts',(31.2050398254683,22.5897213991733,41.244081041016));
#65310=CARTESIAN_POINT('Ctrl Pts',(31.2810095779918,22.5310761296009,41.2381293927626));
#65311=CARTESIAN_POINT('Ctrl Pts',(31.3402234880531,22.4795213149424,41.233477641371));
#65312=CARTESIAN_POINT('Ctrl Pts',(31.5094624950596,22.3136508167594,41.2196167053532));
#65313=CARTESIAN_POINT('Ctrl Pts',(31.6090365643494,22.189603034915,41.2106063583353));
#65314=CARTESIAN_POINT('Ctrl Pts',(31.7131036889562,22.0226267398648,41.1986942672323));
#65315=CARTESIAN_POINT('Ctrl Pts',(31.732390381713,21.9896024323267,41.1963507917934));
#65316=CARTESIAN_POINT('Ctrl Pts',(31.7604202776747,21.9382739659812,41.1927145730851));
#65317=CARTESIAN_POINT('Ctrl Pts',(31.7698538283404,21.9203558919153,41.1914463757514));
#65318=CARTESIAN_POINT('Ctrl Pts',(31.7867610830616,21.887020755466,41.1890874412639));
#65319=CARTESIAN_POINT('Ctrl Pts',(31.7943121486991,21.8716449229019,41.187999557427));
#65320=CARTESIAN_POINT('Ctrl Pts',(31.8106320704697,21.8373025904847,41.1855691831093));
#65321=CARTESIAN_POINT('Ctrl Pts',(31.8193027170477,21.8182919352196,41.1842234390547));
#65322=CARTESIAN_POINT('Ctrl Pts',(31.8438387173611,21.7621775276537,41.1802484839769));
#65323=CARTESIAN_POINT('Ctrl Pts',(31.8588779554427,21.7247262647507,41.1775919622537));
#65324=CARTESIAN_POINT('Ctrl Pts',(31.9237899582611,21.5477358974643,41.1650155444085));
#65325=CARTESIAN_POINT('Ctrl Pts',(31.9591444679488,21.4033895812671,41.1546481264045));
#65326=CARTESIAN_POINT('Ctrl Pts',(31.9855885476766,21.1994373616712,41.1403314195655));
#65327=CARTESIAN_POINT('Ctrl Pts',(31.9905146236455,21.1420894092123,41.1363478960723));
#65328=CARTESIAN_POINT('Ctrl Pts',(31.9939842612521,21.0603595494968,41.1307914416761));
#65329=CARTESIAN_POINT('Ctrl Pts',(31.9945710681169,21.0360952805971,41.1291570180706));
#65330=CARTESIAN_POINT('Ctrl Pts',(31.9948277521411,20.9927973209204,41.1262742496738));
#65331=CARTESIAN_POINT('Ctrl Pts',(31.9946682875041,20.9737678514942,41.125018904176));
#65332=CARTESIAN_POINT('Ctrl Pts',(31.9939903879076,20.9438965575214,41.1230695779838));
#65333=CARTESIAN_POINT('Ctrl Pts',(31.9936557557704,20.9330522283619,41.1223663028804));
#65334=CARTESIAN_POINT('Ctrl Pts',(31.9928481862978,20.9123594430176,41.1210334230297));
#65335=CARTESIAN_POINT('Ctrl Pts',(31.9923906888463,20.9025109877388,41.120403060864));
#65336=CARTESIAN_POINT('Ctrl Pts',(31.9910689099022,20.8779819210449,41.1188422391293));
#65337=CARTESIAN_POINT('Ctrl Pts',(31.990115246675,20.8633063609461,41.1179165893663));
#65338=CARTESIAN_POINT('Ctrl Pts',(31.9859753857473,20.8089042788245,41.1145111368561));
#65339=CARTESIAN_POINT('Ctrl Pts',(31.9817610088244,20.7692629788546,41.1120809646955));
#65340=CARTESIAN_POINT('Ctrl Pts',(31.9592578261142,20.6046819809806,41.1021078289706));
#65341=CARTESIAN_POINT('Ctrl Pts',(31.9303159879416,20.4814902520085,41.094908319882));
#65342=CARTESIAN_POINT('Ctrl Pts',(31.8589011775357,20.269989544181,41.0818882115268));
#65343=CARTESIAN_POINT('Ctrl Pts',(31.8212292749245,20.1805186462145,41.076155824671));
#65344=CARTESIAN_POINT('Ctrl Pts',(31.7648746092339,20.0699556814467,41.0685378423553));
#65345=CARTESIAN_POINT('Ctrl Pts',(31.7520519963007,20.0460196476569,41.0668553369791));
#65346=CARTESIAN_POINT('Ctrl Pts',(31.7299025405598,20.0066268121713,41.0640261216806));
#65347=CARTESIAN_POINT('Ctrl Pts',(31.7208470716229,19.9910211043967,41.0628891655105));
#65348=CARTESIAN_POINT('Ctrl Pts',(31.702558528249,19.9604661247648,41.0606298275783));
#65349=CARTESIAN_POINT('Ctrl Pts',(31.693337150051,19.9455117432933,41.0595079468783));
#65350=CARTESIAN_POINT('Ctrl Pts',(31.6702032711251,19.9090814429663,41.0567340749481));
#65351=CARTESIAN_POINT('Ctrl Pts',(31.6560730842049,19.8877481833498,41.0550741107011));
#65352=CARTESIAN_POINT('Ctrl Pts',(31.6014702546122,19.8086587598874,41.0487818048469));
#65353=CARTESIAN_POINT('Ctrl Pts',(31.558358490369,19.75279599977,41.044051623411));
#65354=CARTESIAN_POINT('Ctrl Pts',(31.4225767115047,19.5949116704993,41.0298264469451));
#65355=CARTESIAN_POINT('Ctrl Pts',(31.3221965749725,19.5000702089894,41.0200991070525));
#65356=CARTESIAN_POINT('Ctrl Pts',(31.1686596491569,19.3824827594207,41.0067700897673));
#65357=CARTESIAN_POINT('Ctrl Pts',(31.1230553297336,19.3504924263493,41.0029816437539));
#65358=CARTESIAN_POINT('Ctrl Pts',(31.0627572081478,19.3118565278575,40.9982414732662));
#65359=CARTESIAN_POINT('Ctrl Pts',(31.0492430418437,19.3034239351426,40.9971957807613));
#65360=CARTESIAN_POINT('Ctrl Pts',(31.0269186395826,19.2898627151663,40.9954973694422));
#65361=CARTESIAN_POINT('Ctrl Pts',(31.0181677414245,19.2846382624943,40.9948387998748));
#65362=CARTESIAN_POINT('Ctrl Pts',(31.0014359384849,19.2748222162752,40.9935937862481));
#65363=CARTESIAN_POINT('Ctrl Pts',(30.9934626614644,19.2702184320494,40.99300651775));
#65364=CARTESIAN_POINT('Ctrl Pts',(30.9715054965582,19.2577422285986,40.9914049204877));
#65365=CARTESIAN_POINT('Ctrl Pts',(30.9574577081136,19.2499829007143,40.9903975098373));
#65366=CARTESIAN_POINT('Ctrl Pts',(30.8969647553191,19.2175159900352,40.9861260697649));
#65367=CARTESIAN_POINT('Ctrl Pts',(30.8496420807292,19.1944794897122,40.982950817927));
#65368=CARTESIAN_POINT('Ctrl Pts',(30.6713740279114,19.1162631454633,40.9713938503068));
#65369=CARTESIAN_POINT('Ctrl Pts',(30.535560558107,19.0732446873642,40.963343843533));
#65370=CARTESIAN_POINT('Ctrl Pts',(30.3496517391777,19.035556302364,40.9521489172287));
#65371=CARTESIAN_POINT('Ctrl Pts',(30.3026581794283,19.0277695428048,40.9493078450722));
#65372=CARTESIAN_POINT('Ctrl Pts',(30.2189882499579,19.0169664453593,40.9441917969594));
#65373=CARTESIAN_POINT('Ctrl Pts',(30.1824222360765,19.0132690667533,40.941936781028));
#65374=CARTESIAN_POINT('Ctrl Pts',(30.1258677157363,19.0091249728261,40.9384085026455));
#65375=CARTESIAN_POINT('Ctrl Pts',(30.1059386227073,19.0079651062285,40.9371574792123));
#65376=CARTESIAN_POINT('Ctrl Pts',(30.068867323712,19.0063654313446,40.9348144746451));
#65377=CARTESIAN_POINT('Ctrl Pts',(30.0517302495366,19.0058471841884,40.9337250632387));
#65378=CARTESIAN_POINT('Ctrl Pts',(30.0133514864003,19.0051815946914,40.9312702634482));
#65379=CARTESIAN_POINT('Ctrl Pts',(29.9921101078738,19.0051525311417,40.9299012923569));
#65380=CARTESIAN_POINT('Ctrl Pts',(29.937115896891,19.0059556335037,40.9263288598602));
#65381=CARTESIAN_POINT('Ctrl Pts',(29.9033785831263,19.0073054875259,40.9241097203117));
#65382=CARTESIAN_POINT('Ctrl Pts',(29.6900619657174,19.0212701780155,40.9098988032085));
#65383=CARTESIAN_POINT('Ctrl Pts',(29.5128666115394,19.0572923524432,40.8971793153853));
#65384=CARTESIAN_POINT('Ctrl Pts',(29.285618296824,19.1365693946878,40.8805499618143));
#65385=CARTESIAN_POINT('Ctrl Pts',(29.2292216323176,19.1591803683033,40.8764060424333));
#65386=CARTESIAN_POINT('Ctrl Pts',(29.159088626545,19.1910882169286,40.8713019679127));
#65387=CARTESIAN_POINT('Ctrl Pts',(29.1443202204914,19.1980272107316,40.8702300796092));
#65388=CARTESIAN_POINT('Ctrl Pts',(29.1203956233064,19.2096287500604,40.8685003693419));
#65389=CARTESIAN_POINT('Ctrl Pts',(29.111187653951,19.214182064474,40.8678362959442));
#65390=CARTESIAN_POINT('Ctrl Pts',(29.0938540759062,19.2229207517305,40.8665899123099));
#65391=CARTESIAN_POINT('Ctrl Pts',(29.0857213456674,19.2270911922328,40.8660066677032));
#65392=CARTESIAN_POINT('Ctrl Pts',(29.0637125555656,19.2385689591375,40.8644317213948));
#65393=CARTESIAN_POINT('Ctrl Pts',(29.0498932211605,19.2459844255293,40.8634465424598));
#65394=CARTESIAN_POINT('Ctrl Pts',(28.9937573030636,19.2769651572645,40.8594540272724));
#65395=CARTESIAN_POINT('Ctrl Pts',(28.9522151689417,19.3019066116733,40.8565214078539));
#65396=CARTESIAN_POINT('Ctrl Pts',(28.7892147114622,19.4080324652554,40.8449361372304));
#65397=CARTESIAN_POINT('Ctrl Pts',(28.6759297202561,19.5009322748394,40.8366715659025));
#65398=CARTESIAN_POINT('Ctrl Pts',(28.5240501537722,19.6562503766664,40.8238565377191));
#65399=CARTESIAN_POINT('Ctrl Pts',(28.4770626782782,19.7097475450698,40.8195908341328));
#65400=CARTESIAN_POINT('Ctrl Pts',(28.4175283521975,19.7853234542852,40.8136654456841));
#65401=CARTESIAN_POINT('Ctrl Pts',(28.4023932791891,19.8052999102075,40.8121083707291));
#65402=CARTESIAN_POINT('Ctrl Pts',(28.3772468686914,19.8398226914187,40.8094295180314));
#65403=CARTESIAN_POINT('Ctrl Pts',(28.3670447647968,19.8542267763879,40.8083152769599));
#65404=CARTESIAN_POINT('Ctrl Pts',(28.3467087718258,19.883762006806,40.8060364663726));
#65405=CARTESIAN_POINT('Ctrl Pts',(28.3365882792009,19.8989002981793,40.8048715304247));
#65406=CARTESIAN_POINT('Ctrl Pts',(28.3114350366837,19.9376629821515,40.8018952514135));
#65407=CARTESIAN_POINT('Ctrl Pts',(28.2966902808344,19.9614686122781,40.800073482506));
#65408=CARTESIAN_POINT('Ctrl Pts',(28.2270105001256,20.0794452495436,40.7910701279346));
#65409=CARTESIAN_POINT('Ctrl Pts',(28.1793658537273,20.1776876147103,40.7836346604546));
#65410=CARTESIAN_POINT('Ctrl Pts',(28.1101139219429,20.3564196104473,40.7703292160787));
#65411=CARTESIAN_POINT('Ctrl Pts',(28.0850625034879,20.4353059110091,40.7645312166492));
#65412=CARTESIAN_POINT('Ctrl Pts',(28.0490635393503,20.5790860263211,40.7542694057252));
#65413=CARTESIAN_POINT('Ctrl Pts',(28.0362883544957,20.6434051887234,40.7497856647631));
#65414=CARTESIAN_POINT('Ctrl Pts',(28.0242684515574,20.7247015329028,40.7443382437101));
#65415=CARTESIAN_POINT('Ctrl Pts',(28.0220408090699,20.7411914216751,40.7432445880336));
#65416=CARTESIAN_POINT('Ctrl Pts',(28.0187637128904,20.7679714350686,40.7414887896749));
#65417=CARTESIAN_POINT('Ctrl Pts',(28.0175875414003,20.7782448738286,40.7408200586066));
#65418=CARTESIAN_POINT('Ctrl Pts',(28.0155275886762,20.7975662029829,40.7395720353089));
#65419=CARTESIAN_POINT('Ctrl Pts',(28.014625673241,20.8066118308211,40.7389917226292));
#65420=CARTESIAN_POINT('Ctrl Pts',(28.0123617647267,20.8310053080897,40.7374367188637));
#65421=CARTESIAN_POINT('Ctrl Pts',(28.0111156738678,20.8463636367657,40.7364682579945));
#65422=CARTESIAN_POINT('Ctrl Pts',(28.0068800068863,20.9073248414323,40.7326606470627));
#65423=CARTESIAN_POINT('Ctrl Pts',(28.0052797412273,20.9530133742082,40.7298876570754));
#65424=CARTESIAN_POINT('Ctrl Pts',(28.0051910645533,21.0912006518033,40.7216374078533));
#65425=CARTESIAN_POINT('Ctrl Pts',(28.0115631701603,21.1835787849369,40.7163033240241));
#65426=CARTESIAN_POINT('Ctrl Pts',(28.0397940707045,21.3862606381217,40.704426295711));
#65427=CARTESIAN_POINT('Ctrl Pts',(28.0646029222984,21.4958217449137,40.6978818965525));
#65428=CARTESIAN_POINT('Ctrl Pts',(28.1084183083359,21.6340563167445,40.6890483566391));
#65429=CARTESIAN_POINT('Ctrl Pts',(28.1191262188896,21.6651483585229,40.6870234220573));
#65430=CARTESIAN_POINT('Ctrl Pts',(28.1372944175485,21.7139495376848,40.6837765497706));
#65431=CARTESIAN_POINT('Ctrl Pts',(28.144250768065,21.7318406769048,40.6825713361627));
#65432=CARTESIAN_POINT('Ctrl Pts',(28.1579470372654,21.7656148167054,40.6802663951532));
#65433=CARTESIAN_POINT('Ctrl Pts',(28.1646369719428,21.7815162759595,40.6791684437462));
#65434=CARTESIAN_POINT('Ctrl Pts',(28.1805000655374,21.817894198495,40.6766262248632));
#65435=CARTESIAN_POINT('Ctrl Pts',(28.1898140004864,21.8383063344212,40.6751772434949));
#65436=CARTESIAN_POINT('Ctrl Pts',(28.2213689507853,21.9044821142122,40.6704035863536));
#65437=CARTESIAN_POINT('Ctrl Pts',(28.2450152866754,21.9495494718544,40.6670312859722));
#65438=CARTESIAN_POINT('Ctrl Pts',(28.3084466381575,22.059963037024,40.6584584848829));
#65439=CARTESIAN_POINT('Ctrl Pts',(28.3503141689958,22.1240147803844,40.653196707343));
#65440=CARTESIAN_POINT('Ctrl Pts',(28.4692940301177,22.2850213052643,40.6392825395962));
#65441=CARTESIAN_POINT('Ctrl Pts',(28.551940481958,22.3774856062171,40.6305634210846));
#65442=CARTESIAN_POINT('Ctrl Pts',(28.6633192486533,22.4809151509201,40.6203127456696));
#65443=CARTESIAN_POINT('Ctrl Pts',(28.6844204863953,22.4996919173322,40.618429649468));
#65444=CARTESIAN_POINT('Ctrl Pts',(28.715410276333,22.5261102520652,40.6157561841209));
#65445=CARTESIAN_POINT('Ctrl Pts',(28.7249820444586,22.5341161925347,40.6149426794435));
#65446=CARTESIAN_POINT('Ctrl Pts',(28.7421323654658,22.5481895225061,40.6135076403695));
#65447=CARTESIAN_POINT('Ctrl Pts',(28.749680926477,22.554292125031,40.6128837071507));
#65448=CARTESIAN_POINT('Ctrl Pts',(28.7666862329129,22.5678359262381,40.6114952590458));
#65449=CARTESIAN_POINT('Ctrl Pts',(28.7761661251457,22.5752469660162,40.6107328078489));
#65450=CARTESIAN_POINT('Ctrl Pts',(28.8055346138781,22.5977810312133,40.6084040510527));
#65451=CARTESIAN_POINT('Ctrl Pts',(28.8256414914497,22.6126171297938,40.6068560220941));
#65452=CARTESIAN_POINT('Ctrl Pts',(28.8746023689811,22.6473419138684,40.6031822266392));
#65453=CARTESIAN_POINT('Ctrl Pts',(28.9037125419554,22.6668561061358,40.6010751782613));
#65454=CARTESIAN_POINT('Ctrl Pts',(28.9645334147829,22.7053447379297,40.596796341949));
#65455=CARTESIAN_POINT('Ctrl Pts',(28.9962740328145,22.7242168613144,40.5946289620116));
#65456=CARTESIAN_POINT('Ctrl Pts',(29.0285071367644,22.7421909135288,40.592474930186));
#65457=CARTESIAN_POINT('',(28.0052500576935,20.9995202415483,40.5704548814432));
#65458=CARTESIAN_POINT('Ctrl Pts',(29.0285070491141,22.7421908646526,40.4352302045579));
#65459=CARTESIAN_POINT('Ctrl Pts',(28.9675807103231,22.7082166831438,40.4396692331823));
#65460=CARTESIAN_POINT('Ctrl Pts',(28.9084339214687,22.6710400771609,40.4441082618066));
#65461=CARTESIAN_POINT('Ctrl Pts',(28.8514141220663,22.6308825964831,40.4485472904309));
#65462=CARTESIAN_POINT('Ctrl Pts',(28.7943395779221,22.5906865605851,40.4529905809692));
#65463=CARTESIAN_POINT('Ctrl Pts',(28.7393965044057,22.5475042143395,40.4574338715075));
#65464=CARTESIAN_POINT('Ctrl Pts',(28.6869020394544,22.5015995832814,40.4618771620457));
#65465=CARTESIAN_POINT('Ctrl Pts',(28.6343838567526,22.4556742118541,40.4663224601262));
#65466=CARTESIAN_POINT('Ctrl Pts',(28.584316838868,22.4070244461456,40.4707677582067));
#65467=CARTESIAN_POINT('Ctrl Pts',(28.5369816920423,22.3559516927533,40.4752130562872));
#65468=CARTESIAN_POINT('Ctrl Pts',(28.4895578967346,22.3047832911511,40.4796666794486));
#65469=CARTESIAN_POINT('Ctrl Pts',(28.4448765108707,22.2511832108462,40.48412030261));
#65470=CARTESIAN_POINT('Ctrl Pts',(28.4031780030416,22.1954861239386,40.4885739257714));
#65471=CARTESIAN_POINT('Ctrl Pts',(28.3633271727297,22.1422569971719,40.4928302071138));
#65472=CARTESIAN_POINT('Ctrl Pts',(28.3262006184482,22.0871131274035,40.4970864884562));
#65473=CARTESIAN_POINT('Ctrl Pts',(28.2919693293639,22.0303682791441,40.5013427697985));
#65474=CARTESIAN_POINT('Ctrl Pts',(28.2549707662894,21.9690361498658,40.5059431309863));
#65475=CARTESIAN_POINT('Ctrl Pts',(28.2212168354539,21.9056053030204,40.510543492174));
#65476=CARTESIAN_POINT('Ctrl Pts',(28.1909430004169,21.8404405599204,40.5151438533617));
#65477=CARTESIAN_POINT('Ctrl Pts',(28.1606106549391,21.7751498724915,40.5197531056978));
#65478=CARTESIAN_POINT('Ctrl Pts',(28.1337721552087,21.708118934563,40.5243623580339));
#65479=CARTESIAN_POINT('Ctrl Pts',(28.1106202090465,21.6397433610727,40.5289716103701));
#65480=CARTESIAN_POINT('Ctrl Pts',(28.087602011715,21.5717627933815,40.533554235048));
#65481=CARTESIAN_POINT('Ctrl Pts',(28.0682280672016,21.5024534966911,40.5381368597258));
#65482=CARTESIAN_POINT('Ctrl Pts',(28.0526408693613,21.4322267678177,40.5427194844037));
#65483=CARTESIAN_POINT('Ctrl Pts',(28.0369178157813,21.3613879530327,40.547342050569));
#65484=CARTESIAN_POINT('Ctrl Pts',(28.0250480438997,21.2896160515693,40.5519646167342));
#65485=CARTESIAN_POINT('Ctrl Pts',(28.0171267005988,21.2173500426085,40.5565871828995));
#65486=CARTESIAN_POINT('Ctrl Pts',(28.0092053572979,21.1450840336476,40.5612097490647));
#65487=CARTESIAN_POINT('Ctrl Pts',(28.005232547557,21.0723243759812,40.56583231523));
#65488=CARTESIAN_POINT('Ctrl Pts',(28.0052500576933,20.9995202423044,40.5704548813952));
#65489=CARTESIAN_POINT('Ctrl Pts',(28.0052500576935,20.9995202415483,40.5704548814432));
#65490=CARTESIAN_POINT('Ctrl Pts',(28.0052683089947,20.9236345912157,40.5752731029087));
#65491=CARTESIAN_POINT('Ctrl Pts',(28.0096214048906,20.8478643416663,40.5800913243742));
#65492=CARTESIAN_POINT('Ctrl Pts',(28.0182431153192,20.7726957710024,40.5849095458397));
#65493=CARTESIAN_POINT('Ctrl Pts',(28.0267660125351,20.6983887054913,40.5896725457867));
#65494=CARTESIAN_POINT('Ctrl Pts',(28.039459995078,20.624669945129,40.5944355457336));
#65495=CARTESIAN_POINT('Ctrl Pts',(28.0562100998338,20.5519951043663,40.5991985456806));
#65496=CARTESIAN_POINT('Ctrl Pts',(28.073251501954,20.4780563915336,40.6040443779053));
#65497=CARTESIAN_POINT('Ctrl Pts',(28.0944912867664,20.4051986394074,40.6088902101301));
#65498=CARTESIAN_POINT('Ctrl Pts',(28.1197571437131,20.3338811188068,40.6137360423549));
#65499=CARTESIAN_POINT('Ctrl Pts',(28.1450230006597,20.2625635982063,40.6185818745797));
#65500=CARTESIAN_POINT('Ctrl Pts',(28.1743146992191,20.1927866475378,40.6234277068045));
#65501=CARTESIAN_POINT('Ctrl Pts',(28.2074114249576,20.1249835640815,40.6282735390293));
#65502=CARTESIAN_POINT('Ctrl Pts',(28.237839065209,20.0626484603724,40.6327285791085));
#65503=CARTESIAN_POINT('Ctrl Pts',(28.2715819464657,20.0017796089535,40.6371836191876));
#65504=CARTESIAN_POINT('Ctrl Pts',(28.3084755457094,19.9427523549154,40.6416386592668));
#65505=CARTESIAN_POINT('Ctrl Pts',(28.3453138869145,19.8838135099876,40.6460870267312));
#65506=CARTESIAN_POINT('Ctrl Pts',(28.3852933225449,19.8267111993866,40.6505353941956));
#65507=CARTESIAN_POINT('Ctrl Pts',(28.4282026904114,19.7717977446405,40.6549837616599));
#65508=CARTESIAN_POINT('Ctrl Pts',(28.4710617211985,19.7169487089962,40.659426910734));
#65509=CARTESIAN_POINT('Ctrl Pts',(28.5168435577483,19.6642838129536,40.6638700598082));
#65510=CARTESIAN_POINT('Ctrl Pts',(28.5652938412495,19.6141263403386,40.6683132088823));
#65511=CARTESIAN_POINT('Ctrl Pts',(28.6137137452349,19.5640003176888,40.672753571993));
#65512=CARTESIAN_POINT('Ctrl Pts',(28.6647984377143,19.5163789505865,40.6771939351037));
#65513=CARTESIAN_POINT('Ctrl Pts',(28.7182543958363,19.4715511887188,40.6816342982144));
#65514=CARTESIAN_POINT('Ctrl Pts',(28.771694976291,19.4267363224464,40.6860733839665));
#65515=CARTESIAN_POINT('Ctrl Pts',(28.8275050934516,19.3847137802471,40.6905124697186));
#65516=CARTESIAN_POINT('Ctrl Pts',(28.8853569331097,19.345733275456,40.6949515554708));
#65517=CARTESIAN_POINT('Ctrl Pts',(28.9432117622251,19.306750756372,40.6993908706099));
#65518=CARTESIAN_POINT('Ctrl Pts',(29.0031081161784,19.2708108581908,40.7038301857489));
#65519=CARTESIAN_POINT('Ctrl Pts',(29.0646893841519,19.238119863787,40.708269500888));
#65520=CARTESIAN_POINT('Ctrl Pts',(29.1263357297013,19.205394322341,40.7127135073866));
#65521=CARTESIAN_POINT('Ctrl Pts',(29.1896701100956,19.1759247671806,40.7171575138852));
#65522=CARTESIAN_POINT('Ctrl Pts',(29.2543123668765,19.1498709460401,40.7216015203838));
#65523=CARTESIAN_POINT('Ctrl Pts',(29.3189924858195,19.123801864696,40.726048129819));
#65524=CARTESIAN_POINT('Ctrl Pts',(29.3849815429722,19.1011526583566,40.7304947392542));
#65525=CARTESIAN_POINT('Ctrl Pts',(29.4518831482747,19.0820335041105,40.7349413486894));
#65526=CARTESIAN_POINT('Ctrl Pts',(29.5189006482926,19.0628812294492,40.7393956610569));
#65527=CARTESIAN_POINT('Ctrl Pts',(29.5868333751877,19.0472713229655,40.7438499734244));
#65528=CARTESIAN_POINT('Ctrl Pts',(29.6552744543684,19.0352629029081,40.7483042857918));
#65529=CARTESIAN_POINT('Ctrl Pts',(29.6906143635875,19.0290622924009,40.7506042932812));
#65530=CARTESIAN_POINT('Ctrl Pts',(29.7260897191631,19.023821071248,40.7529043007707));
#65531=CARTESIAN_POINT('Ctrl Pts',(29.7616442822397,19.0195419433093,40.7552043082601));
#65532=CARTESIAN_POINT('Ctrl Pts',(29.8305123203823,19.0112534109636,40.7596593483394));
#65533=CARTESIAN_POINT('Ctrl Pts',(29.8999488406028,19.0065450387862,40.7641143884188));
#65534=CARTESIAN_POINT('Ctrl Pts',(29.9695493094053,19.0054824347872,40.7685694284981));
#65535=CARTESIAN_POINT('Ctrl Pts',(30.0390455328786,19.0044214223222,40.7730177959627));
#65536=CARTESIAN_POINT('Ctrl Pts',(30.1087047322639,19.0069953474599,40.7774661634272));
#65537=CARTESIAN_POINT('Ctrl Pts',(30.178116388894,19.0132181512538,40.7819145308917));
#65538=CARTESIAN_POINT('Ctrl Pts',(30.2474466185478,19.0194336550621,40.786357679966));
#65539=CARTESIAN_POINT('Ctrl Pts',(30.3165293971986,19.0292894922795,40.7908008290403));
#65540=CARTESIAN_POINT('Ctrl Pts',(30.3849551406269,19.042747562984,40.7952439781146));
#65541=CARTESIAN_POINT('Ctrl Pts',(30.4533379794362,19.0561971951482,40.7996843412254));
#65542=CARTESIAN_POINT('Ctrl Pts',(30.5210641213143,19.0732444857554,40.8041247043363));
#65543=CARTESIAN_POINT('Ctrl Pts',(30.5877315537106,19.093799805038,40.8085650674472));
#65544=CARTESIAN_POINT('Ctrl Pts',(30.6543798078969,19.1143492111752,40.8130041531995));
#65545=CARTESIAN_POINT('Ctrl Pts',(30.7199694898821,19.1384044984893,40.8174432389517));
#65546=CARTESIAN_POINT('Ctrl Pts',(30.7841129210272,19.1658259380369,40.821882324704));
#65547=CARTESIAN_POINT('Ctrl Pts',(30.8482596667434,19.19324879457,40.8263216398433));
#65548=CARTESIAN_POINT('Ctrl Pts',(30.9109595642926,19.2240379541205,40.8307609549825));
#65549=CARTESIAN_POINT('Ctrl Pts',(30.9718457742414,19.2580059260752,40.8352002701218));
#65550=CARTESIAN_POINT('Ctrl Pts',(31.0327963272459,19.2920097945508,40.8396442766205));
#65551=CARTESIAN_POINT('Ctrl Pts',(31.0919289390608,19.3291989413758,40.8440882831193));
#65552=CARTESIAN_POINT('Ctrl Pts',(31.1489030664204,19.3693408368179,40.848532289618));
#65553=CARTESIAN_POINT('Ctrl Pts',(31.2059105645774,19.4095062441086,40.8529788990534));
#65554=CARTESIAN_POINT('Ctrl Pts',(31.2607566771483,19.4526275398672,40.8574255084887));
#65555=CARTESIAN_POINT('Ctrl Pts',(31.3131336781127,19.4984316512705,40.8618721179241));
#65556=CARTESIAN_POINT('Ctrl Pts',(31.3656014125893,19.5443151098649,40.8663264302917));
#65557=CARTESIAN_POINT('Ctrl Pts',(31.415591146707,19.5928903200756,40.8707807426593));
#65558=CARTESIAN_POINT('Ctrl Pts',(31.4628323415477,19.6438476844314,40.875235055027));
#65559=CARTESIAN_POINT('Ctrl Pts',(31.4872255795846,19.6701597860337,40.8775350625149));
#65560=CARTESIAN_POINT('Ctrl Pts',(31.5108866574866,19.6971064860784,40.8798350700029));
#65561=CARTESIAN_POINT('Ctrl Pts',(31.53378277258,19.7246420231807,40.8821350774909));
#65562=CARTESIAN_POINT('Ctrl Pts',(31.5781318066283,19.7779774675345,40.8865901175699));
#65563=CARTESIAN_POINT('Ctrl Pts',(31.6197828555183,19.8337339849531,40.891045157649));
#65564=CARTESIAN_POINT('Ctrl Pts',(31.6584612012166,19.8916074672936,40.895500197728));
#65565=CARTESIAN_POINT('Ctrl Pts',(31.6970816157408,19.9493942686057,40.8999485651922));
#65566=CARTESIAN_POINT('Ctrl Pts',(31.7327378945137,20.0092913380924,40.9043969326564));
#65567=CARTESIAN_POINT('Ctrl Pts',(31.7651954599952,20.0709614913727,40.9088453001207));
#65568=CARTESIAN_POINT('Ctrl Pts',(31.7976149494309,20.1325592992524,40.9132884491947));
#65569=CARTESIAN_POINT('Ctrl Pts',(31.8268429516728,20.1959256287795,40.9177315982686));
#65570=CARTESIAN_POINT('Ctrl Pts',(31.8526891004231,20.2606958273665,40.9221747473426));
#65571=CARTESIAN_POINT('Ctrl Pts',(31.8785190430044,20.3254254134507,40.9266151104532));
#65572=CARTESIAN_POINT('Ctrl Pts',(31.900971157867,20.391556668908,40.9310554735637));
#65573=CARTESIAN_POINT('Ctrl Pts',(31.9199024640449,20.4587033243641,40.9354958366743));
#65574=CARTESIAN_POINT('Ctrl Pts',(31.9388283242568,20.5258306637523,40.9399349224263));
#65575=CARTESIAN_POINT('Ctrl Pts',(31.9542352537796,20.5939723525543,40.9443740081783));
#65576=CARTESIAN_POINT('Ctrl Pts',(31.9660301267147,20.6627269602383,40.9488130939303));
#65577=CARTESIAN_POINT('Ctrl Pts',(31.9778256091424,20.7314851207732,40.9532524090692));
#65578=CARTESIAN_POINT('Ctrl Pts',(31.9860085840666,20.8008557804161,40.9576917242082));
#65579=CARTESIAN_POINT('Ctrl Pts',(31.990537349335,20.8704290796422,40.9621310393471));
#65580=CARTESIAN_POINT('Ctrl Pts',(31.9950709004916,20.9400759022271,40.9665750458456));
#65581=CARTESIAN_POINT('Ctrl Pts',(31.9959425026353,21.0099253025877,40.9710190523441));
#65582=CARTESIAN_POINT('Ctrl Pts',(31.9931625535409,21.0795650530216,40.9754630588425));
#65583=CARTESIAN_POINT('Ctrl Pts',(31.990380976179,21.149245592742,40.9799096682776));
#65584=CARTESIAN_POINT('Ctrl Pts',(31.9839436357183,21.21871575079,40.9843562777126));
#65585=CARTESIAN_POINT('Ctrl Pts',(31.9739127943848,21.2875688485634,40.9888028871477));
#65586=CARTESIAN_POINT('Ctrl Pts',(31.9638645764652,21.3565412216538,40.993257199515));
#65587=CARTESIAN_POINT('Ctrl Pts',(31.9502105275691,21.424893921032,40.9977115118824));
#65588=CARTESIAN_POINT('Ctrl Pts',(31.9330637720797,21.4922316686004,41.0021658242497));
#65589=CARTESIAN_POINT('Ctrl Pts',(31.9242099551909,21.5270018667896,41.0044658317404));
#65590=CARTESIAN_POINT('Ctrl Pts',(31.9144257150367,21.5615017203884,41.006765839231));
#65591=CARTESIAN_POINT('Ctrl Pts',(31.9037316734446,21.5956788379855,41.0090658467216));
#65592=CARTESIAN_POINT('Ctrl Pts',(31.8830176609496,21.6618788087689,41.0135208868007));
#65593=CARTESIAN_POINT('Ctrl Pts',(31.8588057035532,21.7271274120279,41.0179759268797));
#65594=CARTESIAN_POINT('Ctrl Pts',(31.8312020468742,21.7910288401972,41.0224309669588));
#65595=CARTESIAN_POINT('Ctrl Pts',(31.8036397340587,21.8548345588758,41.026879334423));
#65596=CARTESIAN_POINT('Ctrl Pts',(31.7726959971272,21.9172966617358,41.0313277018872));
#65597=CARTESIAN_POINT('Ctrl Pts',(31.7385266512765,21.9780350941051,41.0357760693514));
#65598=CARTESIAN_POINT('Ctrl Pts',(31.7043973895652,22.0387022740778,41.0402192184254));
#65599=CARTESIAN_POINT('Ctrl Pts',(31.6670502732538,22.0976493752445,41.0446623674994));
#65600=CARTESIAN_POINT('Ctrl Pts',(31.6266881875033,22.1545185590267,41.0491055165734));
#65601=CARTESIAN_POINT('Ctrl Pts',(31.5863514097704,22.2113520844361,41.053545879684));
#65602=CARTESIAN_POINT('Ctrl Pts',(31.5430036954772,22.2661098790928,41.0579862427945));
#65603=CARTESIAN_POINT('Ctrl Pts',(31.4968918089427,22.3184621628323,41.0624266059051));
#65604=CARTESIAN_POINT('Ctrl Pts',(31.4507931874074,22.3707993863984,41.0668656916571));
#65605=CARTESIAN_POINT('Ctrl Pts',(31.4019322954712,22.4207321058244,41.071304777409));
#65606=CARTESIAN_POINT('Ctrl Pts',(31.3505956959991,22.4679641781899,41.075743863161));
#65607=CARTESIAN_POINT('Ctrl Pts',(31.2992564437407,22.5151986912429,41.0801831783));
#65608=CARTESIAN_POINT('Ctrl Pts',(31.2454415916704,22.5597319506625,41.0846224934389));
#65609=CARTESIAN_POINT('Ctrl Pts',(31.1894726991707,22.6013064230271,41.0890618085779));
#65610=CARTESIAN_POINT('Ctrl Pts',(31.1334446601159,22.6429248302758,41.0935058150763));
#65611=CARTESIAN_POINT('Ctrl Pts',(31.0752584308543,22.681577917414,41.0979498215748));
#65612=CARTESIAN_POINT('Ctrl Pts',(31.0152658445187,22.7170506187803,41.1023938280732));
#65613=CARTESIAN_POINT('Ctrl Pts',(30.9552381194187,22.7525440971621,41.1068404375083));
#65614=CARTESIAN_POINT('Ctrl Pts',(30.893402365152,22.7848532553943,41.1112870469433));
#65615=CARTESIAN_POINT('Ctrl Pts',(30.8301339118456,22.8138095960998,41.1157336563784));
#65616=CARTESIAN_POINT('Ctrl Pts',(30.7667558575907,22.8428160983352,41.1201879687457));
#65617=CARTESIAN_POINT('Ctrl Pts',(30.7019406050655,22.8684580094109,41.124642281113));
#65618=CARTESIAN_POINT('Ctrl Pts',(30.636081523246,22.8906157352262,41.1290965934804));
#65619=CARTESIAN_POINT('Ctrl Pts',(30.60207484185,22.9020569928546,41.131396600971));
#65620=CARTESIAN_POINT('Ctrl Pts',(30.5677900702718,22.9125701128308,41.1336966084617));
#65621=CARTESIAN_POINT('Ctrl Pts',(30.5332824022933,22.9221439701293,41.1359966159524));
#65622=CARTESIAN_POINT('Ctrl Pts',(30.4664614855868,22.9406828618764,41.140450368349));
#65623=CARTESIAN_POINT('Ctrl Pts',(30.3985411344477,22.9557696878217,41.1449041207455));
#65624=CARTESIAN_POINT('Ctrl Pts',(30.3299110872441,22.9672788915183,41.1493578731421));
#65625=CARTESIAN_POINT('Ctrl Pts',(30.2613748664854,22.9787723605956,41.153805536664));
#65626=CARTESIAN_POINT('Ctrl Pts',(30.1921313521205,22.9866978282039,41.1582532001859));
#65627=CARTESIAN_POINT('Ctrl Pts',(30.1225841092882,22.990979833813,41.1627008637079));
#65628=CARTESIAN_POINT('Ctrl Pts',(30.0531083380928,22.9952574389321,41.167143956498));
#65629=CARTESIAN_POINT('Ctrl Pts',(29.9833299435588,22.9958989814401,41.1715870492882));
#65630=CARTESIAN_POINT('Ctrl Pts',(29.9136595662431,22.9928805513624,41.1760301420784));
#65631=CARTESIAN_POINT('Ctrl Pts',(29.8440371407194,22.9898641987693,41.1804701768363));
#65632=CARTESIAN_POINT('Ctrl Pts',(29.77452307242,22.9831928958928,41.1849102115942));
#65633=CARTESIAN_POINT('Ctrl Pts',(29.7055281883306,22.9728948057695,41.1893502463521));
#65634=CARTESIAN_POINT('Ctrl Pts',(29.6365382419028,22.9625974526353,41.1937899633562));
#65635=CARTESIAN_POINT('Ctrl Pts',(29.5680678916448,22.9486738865793,41.1982296803603));
#65636=CARTESIAN_POINT('Ctrl Pts',(29.5005215894561,22.9312039974846,41.2026693973643));
#65637=CARTESIAN_POINT('Ctrl Pts',(29.4329784865895,22.913734935849,41.2071089040818));
#65638=CARTESIAN_POINT('Ctrl Pts',(29.3663598166088,22.8927200155239,41.2115484107992));
#65639=CARTESIAN_POINT('Ctrl Pts',(29.3010564866216,22.8682894656895,41.2159879175166));
#65640=CARTESIAN_POINT('Ctrl Pts',(29.2357051510874,22.8438409565579,41.2204306877882));
#65641=CARTESIAN_POINT('Ctrl Pts',(29.1716715406158,22.8159719870887,41.2248734580597));
#65642=CARTESIAN_POINT('Ctrl Pts',(29.109326978281,22.7848610956828,41.2293162283312));
#65643=CARTESIAN_POINT('Ctrl Pts',(29.082054240405,22.7712515818034,41.2312597259599));
#65644=CARTESIAN_POINT('Ctrl Pts',(29.0551044216415,22.7570222820631,41.2332032235885));
#65645=CARTESIAN_POINT('Ctrl Pts',(29.0285070491141,22.7421908646526,41.2351467212172));
#65646=CARTESIAN_POINT('Origin',(30.,21.,34.5704548813952));
#65647=CARTESIAN_POINT('',(29.0285070576893,22.7421908694344,42.1950453911705));
#65648=CARTESIAN_POINT('',(29.0271745210922,22.7445458878821,42.0352855536299));
#65649=CARTESIAN_POINT('',(29.0285070491141,22.7421908646526,34.5704548813952));
#65650=CARTESIAN_POINT('',(28.0052507199072,21.0016947180269,41.5280186851748));
#65651=CARTESIAN_POINT('Ctrl Pts',(29.0285070576893,22.7421908694344,42.1950453911705));
#65652=CARTESIAN_POINT('Ctrl Pts',(29.0854792583077,22.7739601157206,42.1907449642306));
#65653=CARTESIAN_POINT('Ctrl Pts',(29.1439752931866,22.8029155541729,42.1863498638858));
#65654=CARTESIAN_POINT('Ctrl Pts',(29.3655541149389,22.8993774258534,42.1698050565103));
#65655=CARTESIAN_POINT('Ctrl Pts',(29.5359371700845,22.9480240136795,42.1572042394495));
#65656=CARTESIAN_POINT('Ctrl Pts',(29.7330985378328,22.9769454511594,42.1438578658572));
#65657=CARTESIAN_POINT('Ctrl Pts',(29.7557635613907,22.9798733229191,42.1423429272947));
#65658=CARTESIAN_POINT('Ctrl Pts',(29.7900295861683,22.9837023878216,42.1400865505333));
#65659=CARTESIAN_POINT('Ctrl Pts',(29.8015955895226,22.9848925522928,42.1393307627143));
#65660=CARTESIAN_POINT('Ctrl Pts',(29.8228757329182,22.9868944507893,42.1379516997219));
#65661=CARTESIAN_POINT('Ctrl Pts',(29.8325859795035,22.9877361785976,42.1373269090836));
#65662=CARTESIAN_POINT('Ctrl Pts',(29.8554941476766,22.9895528973066,42.1358630758892));
#65663=CARTESIAN_POINT('Ctrl Pts',(29.8686961576703,22.9904677832751,42.1350273108511));
#65664=CARTESIAN_POINT('Ctrl Pts',(29.9139391467252,22.9931509670232,42.1321870180222));
#65665=CARTESIAN_POINT('Ctrl Pts',(29.9460148028531,22.994277590147,42.1302142611265));
#65666=CARTESIAN_POINT('Ctrl Pts',(30.0282429090343,22.9951801797665,42.1252300491227));
#65667=CARTESIAN_POINT('Ctrl Pts',(30.0783862285429,22.9938399668942,42.1222600106318));
#65668=CARTESIAN_POINT('Ctrl Pts',(30.2914814672339,22.9800916780811,42.1097421136857));
#65669=CARTESIAN_POINT('Ctrl Pts',(30.4526150172587,22.9495803530892,42.1004796416621));
#65670=CARTESIAN_POINT('Ctrl Pts',(30.6413450741328,22.8891568134121,42.0884860594092));
#65671=CARTESIAN_POINT('Ctrl Pts',(30.6741809894842,22.8776892041139,42.0863578583756));
#65672=CARTESIAN_POINT('Ctrl Pts',(30.7268250480488,22.8577448983522,42.0828678269669));
#65673=CARTESIAN_POINT('Ctrl Pts',(30.7468257299362,22.8497951319066,42.0815232840372));
#65674=CARTESIAN_POINT('Ctrl Pts',(30.782537780389,22.8349269055818,42.0790868726022));
#65675=CARTESIAN_POINT('Ctrl Pts',(30.7982960691763,22.8281262216976,42.0779990805245));
#65676=CARTESIAN_POINT('Ctrl Pts',(30.8319988833424,22.8130625040648,42.0756441557654));
#65677=CARTESIAN_POINT('Ctrl Pts',(30.8499122205849,22.8047345944107,42.0743748801514));
#65678=CARTESIAN_POINT('Ctrl Pts',(30.8998279938788,22.780620782443,42.0707869002768));
#65679=CARTESIAN_POINT('Ctrl Pts',(30.9315334855326,22.7642408804795,42.0684478899974));
#65680=CARTESIAN_POINT('Ctrl Pts',(31.0028444764471,22.7249414697906,42.0630456633661));
#65681=CARTESIAN_POINT('Ctrl Pts',(31.042133918142,22.7014924352787,42.059965722005));
#65682=CARTESIAN_POINT('Ctrl Pts',(31.1883196932924,22.6072811509133,42.0481153513728));
#65683=CARTESIAN_POINT('Ctrl Pts',(31.289110859743,22.5276272236387,42.03909605874));
#65684=CARTESIAN_POINT('Ctrl Pts',(31.4306298341418,22.3917452011373,42.0254970384011));
#65685=CARTESIAN_POINT('Ctrl Pts',(31.4772678700464,22.3421392765494,42.0208337418266));
#65686=CARTESIAN_POINT('Ctrl Pts',(31.532356790015,22.2771857078011,42.0151828808977));
#65687=CARTESIAN_POINT('Ctrl Pts',(31.5432623729052,22.2639865346639,42.0140566645001));
#65688=CARTESIAN_POINT('Ctrl Pts',(31.5605445987023,22.2425124450626,42.0122618131222));
#65689=CARTESIAN_POINT('Ctrl Pts',(31.5670282944917,22.2343253043438,42.0115860717325));
#65690=CARTESIAN_POINT('Ctrl Pts',(31.5797402770202,22.2180119175215,42.0102570952762));
#65691=CARTESIAN_POINT('Ctrl Pts',(31.5859708503648,22.2098879471206,42.0096037272472));
#65692=CARTESIAN_POINT('Ctrl Pts',(31.6018697178634,22.1888237367504,42.0079302731877));
#65693=CARTESIAN_POINT('Ctrl Pts',(31.6114441159566,22.1758130679173,42.0069164367508));
#65694=CARTESIAN_POINT('Ctrl Pts',(31.6549645062409,22.1151428728462,42.0022721767189));
#65695=CARTESIAN_POINT('Ctrl Pts',(31.6869641156262,22.0661165474519,41.9987534821668));
#65696=CARTESIAN_POINT('Ctrl Pts',(31.7975251181402,21.879252442424,41.9859126497666));
#65697=CARTESIAN_POINT('Ctrl Pts',(31.86171905515,21.7336120045203,41.9769581353581));
#65698=CARTESIAN_POINT('Ctrl Pts',(31.9231563421516,21.532166263567,41.9643819188724));
#65699=CARTESIAN_POINT('Ctrl Pts',(31.9363732131816,21.4818603148071,41.9612315449816));
#65700=CARTESIAN_POINT('Ctrl Pts',(31.9521370706143,21.4106426182462,41.9567250727164));
#65701=CARTESIAN_POINT('Ctrl Pts',(31.9563422126151,21.3901174153546,41.955421059717));
#65702=CARTESIAN_POINT('Ctrl Pts',(31.9634539678793,21.3523921606852,41.9530127090358));
#65703=CARTESIAN_POINT('Ctrl Pts',(31.9664597845024,21.3352127735774,41.9519116288995));
#65704=CARTESIAN_POINT('Ctrl Pts',(31.9721450412747,21.3000060011607,41.9496451909598));
#65705=CARTESIAN_POINT('Ctrl Pts',(31.9748034420974,21.281976937325,41.9484792783824));
#65706=CARTESIAN_POINT('Ctrl Pts',(31.9809284737358,21.2360889609737,41.9454972673732));
#65707=CARTESIAN_POINT('Ctrl Pts',(31.9840545994372,21.2081894061873,41.9436706619595));
#65708=CARTESIAN_POINT('Ctrl Pts',(31.997340471984,21.0617489607251,41.9340076080548));
#65709=CARTESIAN_POINT('Ctrl Pts',(31.9974669252414,20.942558243678,41.9258633389905));
#65710=CARTESIAN_POINT('Ctrl Pts',(31.9752852508737,20.692015054224,41.9083652407192));
#65711=CARTESIAN_POINT('Ctrl Pts',(31.9504539000925,20.5614335932811,41.8990215166364));
#65712=CARTESIAN_POINT('Ctrl Pts',(31.9072677427889,20.415410968998,41.8888722698805));
#65713=CARTESIAN_POINT('Ctrl Pts',(31.9014094089873,20.3966287155427,41.8875732460272));
#65714=CARTESIAN_POINT('Ctrl Pts',(31.8918485053776,20.3674990548923,41.8855718905294));
#65715=CARTESIAN_POINT('Ctrl Pts',(31.8883368633434,20.3570908950897,41.884859475448));
#65716=CARTESIAN_POINT('Ctrl Pts',(31.8814923219848,20.3373443577485,41.8835136903615));
#65717=CARTESIAN_POINT('Ctrl Pts',(31.8781755322226,20.3280010926377,41.8828795008129));
#65718=CARTESIAN_POINT('Ctrl Pts',(31.8698514839027,20.3050957048882,41.8813303799502));
#65719=CARTESIAN_POINT('Ctrl Pts',(31.8647660819367,20.2915622540395,41.8804199262898));
#65720=CARTESIAN_POINT('Ctrl Pts',(31.8446814841133,20.2398276596656,41.8769537661241));
#65721=CARTESIAN_POINT('Ctrl Pts',(31.8286509185866,20.2020350341443,41.8744516772497));
#65722=CARTESIAN_POINT('Ctrl Pts',(31.7804508717148,20.0974988447337,41.867543902965));
#65723=CARTESIAN_POINT('Ctrl Pts',(31.7457129571354,20.0320117476545,41.8632305525037));
#65724=CARTESIAN_POINT('Ctrl Pts',(31.6358457186826,19.8501332449017,41.8508947001353));
#65725=CARTESIAN_POINT('Ctrl Pts',(31.5521522836659,19.739443080927,41.8429121443202));
#65726=CARTESIAN_POINT('Ctrl Pts',(31.4356373353596,19.6147146035595,41.8325072146796));
#65727=CARTESIAN_POINT('Ctrl Pts',(31.4130265388364,19.591658419086,41.8305175287726));
#65728=CARTESIAN_POINT('Ctrl Pts',(31.3761837512508,19.5558705935481,41.8273138029325));
#65729=CARTESIAN_POINT('Ctrl Pts',(31.362310872503,19.5427764392133,41.8261157028677));
#65730=CARTESIAN_POINT('Ctrl Pts',(31.3355178742106,19.5182044170064,41.8238158920642));
#65731=CARTESIAN_POINT('Ctrl Pts',(31.3226321637883,19.5066915018879,41.8227158265741));
#65732=CARTESIAN_POINT('Ctrl Pts',(31.2924989673542,19.4804645789996,41.8201560691812));
#65733=CARTESIAN_POINT('Ctrl Pts',(31.2751472438717,19.465874544796,41.8186914407425));
#65734=CARTESIAN_POINT('Ctrl Pts',(31.2168708821208,19.4185452070709,41.8138009479045));
#65735=CARTESIAN_POINT('Ctrl Pts',(31.1749077579804,19.3871252566718,41.8103241287133));
#65736=CARTESIAN_POINT('Ctrl Pts',(31.0657587094978,19.3119212179909,41.80138928608));
#65737=CARTESIAN_POINT('Ctrl Pts',(30.997082897908,19.2704696470217,41.7958627127323));
#65738=CARTESIAN_POINT('Ctrl Pts',(30.8099243345128,19.1723629334995,41.781158929487));
#65739=CARTESIAN_POINT('Ctrl Pts',(30.6880124538335,19.1230668956076,41.7719184413867));
#65740=CARTESIAN_POINT('Ctrl Pts',(30.5431036339228,19.0805053964918,41.7618494411781));
#65741=CARTESIAN_POINT('Ctrl Pts',(30.5239868937176,19.0751989981917,41.7605392394785));
#65742=CARTESIAN_POINT('Ctrl Pts',(30.4941335506915,19.0673901060209,41.7585245907541));
#65743=CARTESIAN_POINT('Ctrl Pts',(30.483450542721,19.0646900623252,41.757809854374));
#65744=CARTESIAN_POINT('Ctrl Pts',(30.4631265598757,19.0597321370007,41.7564625700918));
#65745=CARTESIAN_POINT('Ctrl Pts',(30.453490405073,19.0574573243894,41.7558291625399));
#65746=CARTESIAN_POINT('Ctrl Pts',(30.4298229632205,19.0520558476672,41.7542858809167));
#65747=CARTESIAN_POINT('Ctrl Pts',(30.4157737603982,19.0490088649463,41.7533804023033));
#65748=CARTESIAN_POINT('Ctrl Pts',(30.3621474427258,19.0379840244455,41.7499602719406));
#65749=CARTESIAN_POINT('Ctrl Pts',(30.3223618334492,19.0310559202059,41.7474974240678));
#65750=CARTESIAN_POINT('Ctrl Pts',(30.2110785107331,19.0151416088073,41.7407469865064));
#65751=CARTESIAN_POINT('Ctrl Pts',(30.1392618316289,19.0088133214595,41.7365467832774));
#65752=CARTESIAN_POINT('Ctrl Pts',(29.9255007044258,19.0016019008581,41.7241253509934));
#65753=CARTESIAN_POINT('Ctrl Pts',(29.7836536934932,19.0119519527643,41.7159568533099));
#65754=CARTESIAN_POINT('Ctrl Pts',(29.6126232056761,19.0429638034668,41.7053569066981));
#65755=CARTESIAN_POINT('Ctrl Pts',(29.5812816623526,19.0494292544733,41.7033846051779));
#65756=CARTESIAN_POINT('Ctrl Pts',(29.5315833374115,19.0609344923361,41.7002021564832));
#65757=CARTESIAN_POINT('Ctrl Pts',(29.5131190317759,19.0654881505653,41.6990075682109));
#65758=CARTESIAN_POINT('Ctrl Pts',(29.4779922470621,19.0746858481063,41.6967101892921));
#65759=CARTESIAN_POINT('Ctrl Pts',(29.4613194771584,19.0792840030507,41.6956089782982));
#65760=CARTESIAN_POINT('Ctrl Pts',(29.4228185543607,19.0904428294336,41.6930400463941));
#65761=CARTESIAN_POINT('Ctrl Pts',(29.4010392206151,19.0971618770781,41.6915672727094));
#65762=CARTESIAN_POINT('Ctrl Pts',(29.3288036766819,19.1208099543033,41.686614839902));
#65763=CARTESIAN_POINT('Ctrl Pts',(29.278913983689,19.1393834829689,41.6830824118109));
#65764=CARTESIAN_POINT('Ctrl Pts',(29.1540327948212,19.1916530308638,41.6739508525793));
#65765=CARTESIAN_POINT('Ctrl Pts',(29.0802747338343,19.2280286292672,41.6682790097745));
#65766=CARTESIAN_POINT('Ctrl Pts',(28.89837950467,19.332157149726,41.6536871414908));
#65767=CARTESIAN_POINT('Ctrl Pts',(28.794098402385,19.4059256224598,41.6447204715145));
#65768=CARTESIAN_POINT('Ctrl Pts',(28.6824612400831,19.5021626417024,41.6348886727058));
#65769=CARTESIAN_POINT('Ctrl Pts',(28.6675542896391,19.5154079224363,41.6335710170597));
#65770=CARTESIAN_POINT('Ctrl Pts',(28.6446213914946,19.5364082493885,41.6315397116697));
#65771=CARTESIAN_POINT('Ctrl Pts',(28.6364580753141,19.5440105018075,41.6308157808403));
#65772=CARTESIAN_POINT('Ctrl Pts',(28.6212044328101,19.5584565777869,41.6294621830501));
#65773=CARTESIAN_POINT('Ctrl Pts',(28.6141007309128,19.5652847412564,41.6288315222547));
#65774=CARTESIAN_POINT('Ctrl Pts',(28.596973994507,19.5819930734273,41.6273096827627));
#65775=CARTESIAN_POINT('Ctrl Pts',(28.5870044308445,19.5919271452122,41.626422619032));
#65776=CARTESIAN_POINT('Ctrl Pts',(28.550507486961,19.629072187355,41.623166874149));
#65777=CARTESIAN_POINT('Ctrl Pts',(28.5246525484343,19.6569356231421,41.6208437908591));
#65778=CARTESIAN_POINT('Ctrl Pts',(28.4566557939539,19.7345495922136,41.6146321363021));
#65779=CARTESIAN_POINT('Ctrl Pts',(28.4161298953124,19.7856554791639,41.6108150558015));
#65780=CARTESIAN_POINT('Ctrl Pts',(28.2881610496036,19.9643647665012,41.5980267801062));
#65781=CARTESIAN_POINT('Ctrl Pts',(28.2130735011121,20.1000987145098,41.5891682031628));
#65782=CARTESIAN_POINT('Ctrl Pts',(28.1428416569309,20.2713569466394,41.5778585571733));
#65783=CARTESIAN_POINT('Ctrl Pts',(28.131918387685,20.2998366285736,41.5759757245373));
#65784=CARTESIAN_POINT('Ctrl Pts',(28.1153538122592,20.3461754910199,41.5729027143206));
#65785=CARTESIAN_POINT('Ctrl Pts',(28.1093033232988,20.3638838313413,41.5717261950309));
#65786=CARTESIAN_POINT('Ctrl Pts',(28.0981115402182,20.3982106908914,41.569440098028));
#65787=CARTESIAN_POINT('Ctrl Pts',(28.0929367157205,20.4148165379885,41.5683317491421));
#65788=CARTESIAN_POINT('Ctrl Pts',(28.0812836391893,20.4540081436009,41.5657092578049));
#65789=CARTESIAN_POINT('Ctrl Pts',(28.0749861025505,20.4766444834098,41.5641893847547));
#65790=CARTESIAN_POINT('Ctrl Pts',(28.0624938764999,20.5248280403254,41.560941896681));
#65791=CARTESIAN_POINT('Ctrl Pts',(28.0564014459874,20.5503969265444,41.5592113567689));
#65792=CARTESIAN_POINT('Ctrl Pts',(28.0204000915491,20.7159302500691,41.5479593609565));
#65793=CARTESIAN_POINT('Ctrl Pts',(28.005129170239,20.8586260132183,41.5379938008639));
#65794=CARTESIAN_POINT('Ctrl Pts',(28.0052507199072,21.0016947180269,41.5280186851748));
#65795=CARTESIAN_POINT('Ctrl Pts',(28.0052507211432,21.0016961722432,41.5280185837832));
#65796=CARTESIAN_POINT('Ctrl Pts',(28.0053114286813,21.0730900524378,41.5230408202257));
#65797=CARTESIAN_POINT('Ctrl Pts',(28.0092049813008,21.1444349284456,41.5180794287087));
#65798=CARTESIAN_POINT('Ctrl Pts',(28.0201568552617,21.2452530317649,41.5112009530846));
#65799=CARTESIAN_POINT('Ctrl Pts',(28.024070228267,21.2750084999931,41.5091877146635));
#65800=CARTESIAN_POINT('Ctrl Pts',(28.0304079739908,21.3160169869038,41.5064463739901));
#65801=CARTESIAN_POINT('Ctrl Pts',(28.032260291741,21.3273529287226,41.5056921296246));
#65802=CARTESIAN_POINT('Ctrl Pts',(28.0360428796999,21.34930856676,41.5042389909577));
#65803=CARTESIAN_POINT('Ctrl Pts',(28.0379616299795,21.3599298443959,41.5035395268314));
#65804=CARTESIAN_POINT('Ctrl Pts',(28.0418028948491,21.3802491155316,41.5022088113297));
#65805=CARTESIAN_POINT('Ctrl Pts',(28.0437114354257,21.3899491614671,41.5015768698837));
#65806=CARTESIAN_POINT('Ctrl Pts',(28.0486689221581,21.4141924365203,41.5000049579393));
#65807=CARTESIAN_POINT('Ctrl Pts',(28.0518084789715,21.4287168978923,41.4990699543093));
#65808=CARTESIAN_POINT('Ctrl Pts',(28.064228118828,21.4832172035529,41.4955823287349));
#65809=CARTESIAN_POINT('Ctrl Pts',(28.0745793336854,21.5229411041993,41.493082499017));
#65810=CARTESIAN_POINT('Ctrl Pts',(28.1213620122769,21.6821654399037,41.4831307490119));
#65811=CARTESIAN_POINT('Ctrl Pts',(28.1677557539872,21.7984458236206,41.4760057875152));
#65812=CARTESIAN_POINT('Ctrl Pts',(28.268801882108,21.9956522735064,41.4630809939904));
#65813=CARTESIAN_POINT('Ctrl Pts',(28.3190683852499,22.0783488361528,41.4573661155972));
#65814=CARTESIAN_POINT('Ctrl Pts',(28.3909093586371,22.1792350051902,41.4497638447516));
#65815=CARTESIAN_POINT('Ctrl Pts',(28.4071433317298,22.2010726093318,41.4480779562521));
#65816=CARTESIAN_POINT('Ctrl Pts',(28.4348831101777,22.2368357242988,41.4452446510711));
#65817=CARTESIAN_POINT('Ctrl Pts',(28.4461407761387,22.2509496255342,41.4441070502393));
#65818=CARTESIAN_POINT('Ctrl Pts',(28.4687232730475,22.278486409935,41.441847652925));
#65819=CARTESIAN_POINT('Ctrl Pts',(28.4800368777491,22.2919164018396,41.4407263740635));
#65820=CARTESIAN_POINT('Ctrl Pts',(28.5055595812257,22.3214141673056,41.4382192448285));
#65821=CARTESIAN_POINT('Ctrl Pts',(28.5198533369712,22.3374054595144,41.4368299550113));
#65822=CARTESIAN_POINT('Ctrl Pts',(28.5730084646564,22.3949772993208,41.4317148626857));
#65823=CARTESIAN_POINT('Ctrl Pts',(28.6133835493182,22.4351168174772,41.4279258127185));
#65824=CARTESIAN_POINT('Ctrl Pts',(28.768491774527,22.5766573031777,41.4137119258405));
#65825=CARTESIAN_POINT('Ctrl Pts',(28.8930648978236,22.6664772578702,41.4028930290831));
#65826=CARTESIAN_POINT('Ctrl Pts',(29.0272737978734,22.7415027409708,41.3922841321572));
#65827=CARTESIAN_POINT('Ctrl Pts',(29.0278903335763,22.7418469673163,41.3922354182994));
#65828=CARTESIAN_POINT('Ctrl Pts',(29.0285070491341,22.7421908646638,41.392186712139));
#65829=CARTESIAN_POINT('',(28.0044538746745,20.9984594462732,41.3704548663374));
#65830=CARTESIAN_POINT('Ctrl Pts',(29.0285070491141,22.7421908646526,41.2351467212172));
#65831=CARTESIAN_POINT('Ctrl Pts',(28.9651425374846,22.7068570917387,41.2397768318782));
#65832=CARTESIAN_POINT('Ctrl Pts',(28.9037810321329,22.6681026511783,41.2444069425392));
#65833=CARTESIAN_POINT('Ctrl Pts',(28.8447961328331,22.6262015827635,41.2490370532002));
#65834=CARTESIAN_POINT('Ctrl Pts',(28.7858112335333,22.5843005143488,41.2536671638612));
#65835=CARTESIAN_POINT('Ctrl Pts',(28.7292033575836,22.5392532443536,41.2582972745222));
#65836=CARTESIAN_POINT('Ctrl Pts',(28.6753044888271,22.4913783440758,41.2629273851832));
#65837=CARTESIAN_POINT('Ctrl Pts',(28.6231494286428,22.4450523568536,41.2674076962872));
#65838=CARTESIAN_POINT('Ctrl Pts',(28.5733076698616,22.3958804966255,41.2718880073913));
#65839=CARTESIAN_POINT('Ctrl Pts',(28.5261114495448,22.3441280085382,41.2763683184953));
#65840=CARTESIAN_POINT('Ctrl Pts',(28.4799540166452,22.2935145911874,41.2807500180841));
#65841=CARTESIAN_POINT('Ctrl Pts',(28.436327239288,22.2404333591896,41.2851317176728));
#65842=CARTESIAN_POINT('Ctrl Pts',(28.3955086691601,22.1851730387414,41.2895134172616));
#65843=CARTESIAN_POINT('Ctrl Pts',(28.3547289586535,22.129965326582,41.2938909454356));
#65844=CARTESIAN_POINT('Ctrl Pts',(28.3167524558851,22.0725830411258,41.2982684736096));
#65845=CARTESIAN_POINT('Ctrl Pts',(28.2818174815142,22.0133490986179,41.3026460017836));
#65846=CARTESIAN_POINT('Ctrl Pts',(28.246903085809,21.9541500482354,41.3070209513471));
#65847=CARTESIAN_POINT('Ctrl Pts',(28.2150269218007,21.8931019378278,41.3113959009107));
#65848=CARTESIAN_POINT('Ctrl Pts',(28.1863837422199,21.830556218456,41.3157708504743));
#65849=CARTESIAN_POINT('Ctrl Pts',(28.1565486617622,21.7654078446699,41.3203278505747));
#65850=CARTESIAN_POINT('Ctrl Pts',(28.1302218414353,21.69863498356,41.3248848506752));
#65851=CARTESIAN_POINT('Ctrl Pts',(28.1075691378912,21.6306607603444,41.3294418507757));
#65852=CARTESIAN_POINT('Ctrl Pts',(28.0858128238294,21.565376343166,41.3338185259559));
#65853=CARTESIAN_POINT('Ctrl Pts',(28.0674454079982,21.4989843838444,41.3381952011361));
#65854=CARTESIAN_POINT('Ctrl Pts',(28.0525629153372,21.4318754030736,41.3425718763163));
#65855=CARTESIAN_POINT('Ctrl Pts',(28.0376744065389,21.3647392939949,41.346950320735));
#65856=CARTESIAN_POINT('Ctrl Pts',(28.0262737087772,21.296886084571,41.3513287651536));
#65857=CARTESIAN_POINT('Ctrl Pts',(28.0184053946828,21.2287146315338,41.3557072095723));
#65858=CARTESIAN_POINT('Ctrl Pts',(28.0105272702415,21.1604581811784,41.3600911131094));
#65859=CARTESIAN_POINT('Ctrl Pts',(28.0061903409452,21.0918831990938,41.3644750166465));
#65860=CARTESIAN_POINT('Ctrl Pts',(28.0053871417482,21.0233903440865,41.3688589201836));
#65861=CARTESIAN_POINT('Ctrl Pts',(28.0052896752714,21.015078885006,41.369390897349));
#65862=CARTESIAN_POINT('Ctrl Pts',(28.0052441811847,21.0067686302078,41.3699228745145));
#65863=CARTESIAN_POINT('Ctrl Pts',(28.0052505942364,20.9984602903498,41.3704548516799));
#65864=CARTESIAN_POINT('Ctrl Pts',(28.0036353960762,20.9984585791442,41.3704548813952));
#65865=CARTESIAN_POINT('Ctrl Pts',(28.0027728315258,20.8973635887888,41.3769226390681));
#65866=CARTESIAN_POINT('Ctrl Pts',(28.0556922101652,20.1358392039252,41.4257006531513));
#65867=CARTESIAN_POINT('Ctrl Pts',(29.0356112395522,18.849087513172,41.5167889236447));
#65868=CARTESIAN_POINT('Ctrl Pts',(31.2827680785228,19.0223811625417,41.6437196928755));
#65869=CARTESIAN_POINT('Ctrl Pts',(32.3572138429301,21.0036208900697,41.7706504621062));
#65870=CARTESIAN_POINT('Ctrl Pts',(31.2766864430049,22.9815503837979,41.8975812313371));
#65871=CARTESIAN_POINT('Ctrl Pts',(29.7146416622772,23.0971840712568,41.9857929285116));
#65872=CARTESIAN_POINT('Ctrl Pts',(29.0759511139292,22.7721646846317,42.0316943692759));
#65873=CARTESIAN_POINT('Ctrl Pts',(29.0271745210922,22.7445458878821,42.0352855536299));
#65874=CARTESIAN_POINT('Origin',(30.,21.,34.5704548813952));
#65875=CARTESIAN_POINT('',(29.0285070614011,22.7421908715042,42.9937555338539));
#65876=CARTESIAN_POINT('',(29.0285070491141,22.7421908646526,42.8352639371872));
#65877=CARTESIAN_POINT('',(29.0285070491141,22.7421908646526,34.5704548813952));
#65878=CARTESIAN_POINT('Ctrl Pts',(29.0285070614011,22.7421908715042,42.9937555338539));
#65879=CARTESIAN_POINT('Ctrl Pts',(29.1131722975557,22.789402506242,42.9881031452504));
#65880=CARTESIAN_POINT('Ctrl Pts',(29.2011688053936,22.8303812505968,42.9823747536447));
#65881=CARTESIAN_POINT('Ctrl Pts',(29.3176329582475,22.8746109505119,42.9747325540344));
#65882=CARTESIAN_POINT('Ctrl Pts',(29.3436632446347,22.8838824121997,42.9730214274946));
#65883=CARTESIAN_POINT('Ctrl Pts',(29.387083207794,22.8983386021807,42.97015763768));
#65884=CARTESIAN_POINT('Ctrl Pts',(29.404366512354,22.9038322289906,42.9690152592499));
#65885=CARTESIAN_POINT('Ctrl Pts',(29.4384672122926,22.9141615985903,42.9667553504867));
#65886=CARTESIAN_POINT('Ctrl Pts',(29.4552781085389,22.9190132167238,42.9656384597143));
#65887=CARTESIAN_POINT('Ctrl Pts',(29.4964416297771,22.9303085331049,42.9628958171125));
#65888=CARTESIAN_POINT('Ctrl Pts',(29.5208561416033,22.9365131374907,42.9612625008648));
#65889=CARTESIAN_POINT('Ctrl Pts',(29.6106466262219,22.9575302119213,42.9552287150087));
#65890=CARTESIAN_POINT('Ctrl Pts',(29.6766342778022,22.9695059083136,42.9507407771113));
#65891=CARTESIAN_POINT('Ctrl Pts',(29.8834078112605,22.9963601773623,42.9365274387593));
#65892=CARTESIAN_POINT('Ctrl Pts',(30.0252591816151,22.9996010059475,42.926532055402));
#65893=CARTESIAN_POINT('Ctrl Pts',(30.2222874831598,22.9831235738724,42.9129008700715));
#65894=CARTESIAN_POINT('Ctrl Pts',(30.2781167819911,22.9760675666802,42.9090725541263));
#65895=CARTESIAN_POINT('Ctrl Pts',(30.3493263429887,22.9639892623982,42.9042913762256));
#65896=CARTESIAN_POINT('Ctrl Pts',(30.3650429114489,22.9611288658656,42.9032426112948));
#65897=CARTESIAN_POINT('Ctrl Pts',(30.3907365660481,22.9561330577973,42.9015405719646));
#65898=CARTESIAN_POINT('Ctrl Pts',(30.400734389264,22.9541094052906,42.9008813991574));
#65899=CARTESIAN_POINT('Ctrl Pts',(30.4209794052883,22.9498497097683,42.8995535462777));
#65900=CARTESIAN_POINT('Ctrl Pts',(30.4312252942863,22.9476093828033,42.8988851131931));
#65901=CARTESIAN_POINT('Ctrl Pts',(30.4583512260463,22.9414535689799,42.8971238137276));
#65902=CARTESIAN_POINT('Ctrl Pts',(30.4751991289391,22.9373986793428,42.8960385034249));
#65903=CARTESIAN_POINT('Ctrl Pts',(30.5629886020416,22.9150556904737,42.8904182960012));
#65904=CARTESIAN_POINT('Ctrl Pts',(30.6329429564656,22.8930874051847,42.8860590350621));
#65905=CARTESIAN_POINT('Ctrl Pts',(30.8174735051296,22.8237607399634,42.8745025201636));
#65906=CARTESIAN_POINT('Ctrl Pts',(30.9291007369645,22.769502311156,42.86743442197));
#65907=CARTESIAN_POINT('Ctrl Pts',(31.0917911560647,22.6707592904019,42.856175996487));
#65908=CARTESIAN_POINT('Ctrl Pts',(31.1468420845006,22.6334615060652,42.8521810270802));
#65909=CARTESIAN_POINT('Ctrl Pts',(31.2195295868456,22.5787265069676,42.8465720621092));
#65910=CARTESIAN_POINT('Ctrl Pts',(31.2388587252173,22.5636044171007,42.8450462444082));
#65911=CARTESIAN_POINT('Ctrl Pts',(31.2715324401546,22.5370560184561,42.8424042989606));
#65912=CARTESIAN_POINT('Ctrl Pts',(31.2850143521467,22.5258027503827,42.8412951787559));
#65913=CARTESIAN_POINT('Ctrl Pts',(31.3106187295469,22.5038508763105,42.8391509224679));
#65914=CARTESIAN_POINT('Ctrl Pts',(31.3227631881306,22.4931799741157,42.838116984273));
#65915=CARTESIAN_POINT('Ctrl Pts',(31.3546353440804,22.4644810643633,42.8353574067444));
#65916=CARTESIAN_POINT('Ctrl Pts',(31.3741321788921,22.4462027324033,42.833621288892));
#65917=CARTESIAN_POINT('Ctrl Pts',(31.4503245480043,22.3718401991719,42.8266385167874));
#65918=CARTESIAN_POINT('Ctrl Pts',(31.5039957008964,22.3127760842138,42.8212641658102));
#65919=CARTESIAN_POINT('Ctrl Pts',(31.6341491941339,22.1510570282978,42.8070089010727));
#65920=CARTESIAN_POINT('Ctrl Pts',(31.7045473017537,22.0439788512633,42.7979868552629));
#65921=CARTESIAN_POINT('Ctrl Pts',(31.7894396706236,21.8830942431126,42.7854603258962));
#65922=CARTESIAN_POINT('Ctrl Pts',(31.8127155072493,21.8342741149423,42.7817856040501));
#65923=CARTESIAN_POINT('Ctrl Pts',(31.8401922657388,21.7700450556076,42.7771629158989));
#65924=CARTESIAN_POINT('Ctrl Pts',(31.8462312440186,21.7554516489772,42.7761263825407));
#65925=CARTESIAN_POINT('Ctrl Pts',(31.8558711027405,21.7313503404955,42.7744388623434));
#65926=CARTESIAN_POINT('Ctrl Pts',(31.8595736652151,21.7218841108678,42.7737821642907));
#65927=CARTESIAN_POINT('Ctrl Pts',(31.8669665885131,21.7025484516337,42.77245378526));
#65928=CARTESIAN_POINT('Ctrl Pts',(31.8706514043428,21.692677345632,42.7717824195852));
#65929=CARTESIAN_POINT('Ctrl Pts',(31.8802665718077,21.6662832262171,42.7700041426011));
#65930=CARTESIAN_POINT('Ctrl Pts',(31.8860574616923,21.6497099502773,42.7689050487369));
#65931=CARTESIAN_POINT('Ctrl Pts',(31.9167087922599,21.558121808924,42.7629158811781));
#65932=CARTESIAN_POINT('Ctrl Pts',(31.9373159251227,21.481749177919,42.7582308773455));
#65933=CARTESIAN_POINT('Ctrl Pts',(31.9853651822983,21.249631006113,42.7443691853903));
#65934=CARTESIAN_POINT('Ctrl Pts',(31.9988962142559,21.0916675219693,42.7353857118885));
#65935=CARTESIAN_POINT('Ctrl Pts',(31.9923824142054,20.8956111834969,42.7235083064355));
#65936=CARTESIAN_POINT('Ctrl Pts',(31.9900200671759,20.8575059524926,42.7211687020365));
#65937=CARTESIAN_POINT('Ctrl Pts',(31.9847349135814,20.7993400669061,42.717537201912));
#65938=CARTESIAN_POINT('Ctrl Pts',(31.9825971572836,20.779216055518,42.7162697488233));
#65939=CARTESIAN_POINT('Ctrl Pts',(31.9780851562366,20.7421238305339,42.7139115173781));
#65940=CARTESIAN_POINT('Ctrl Pts',(31.9757977418035,20.7251468435659,42.7128235801213));
#65941=CARTESIAN_POINT('Ctrl Pts',(31.9702335003833,20.687518527539,42.7103922134088));
#65942=CARTESIAN_POINT('Ctrl Pts',(31.9668500786955,20.6668852609935,42.7090455168679));
#65943=CARTESIAN_POINT('Ctrl Pts',(31.9559753712531,20.6065256703112,42.7050647689384));
#65944=CARTESIAN_POINT('Ctrl Pts',(31.9476004514592,20.5669713713321,42.7024032861881));
#65945=CARTESIAN_POINT('Ctrl Pts',(31.9029670289558,20.3838227163736,42.6898265640264));
#65946=CARTESIAN_POINT('Ctrl Pts',(31.8519944708731,20.2443133884576,42.6794647148638));
#65947=CARTESIAN_POINT('Ctrl Pts',(31.7604616976154,20.060260984309,42.6651552178724));
#65948=CARTESIAN_POINT('Ctrl Pts',(31.7326372664186,20.0098971597511,42.661173137791));
#65949=CARTESIAN_POINT('Ctrl Pts',(31.6843804189731,19.9308305998077,42.6548813651991));
#65950=CARTESIAN_POINT('Ctrl Pts',(31.6652973239925,19.9013436554057,42.6525255883577));
#65951=CARTESIAN_POINT('Ctrl Pts',(31.6377114738966,19.8610900754056,42.6493123636865));
#65952=CARTESIAN_POINT('Ctrl Pts',(31.6298624274414,19.8498855791709,42.6484182833558));
#65953=CARTESIAN_POINT('Ctrl Pts',(31.6161947907119,19.8307960163526,42.6468967694563));
#65954=CARTESIAN_POINT('Ctrl Pts',(31.6104323687032,19.8228716472115,42.6462657359877));
#65955=CARTESIAN_POINT('Ctrl Pts',(31.5978651039826,19.8058544328849,42.6449121583486));
#65956=CARTESIAN_POINT('Ctrl Pts',(31.5910406992015,19.796776814382,42.6441909489661));
#65957=CARTESIAN_POINT('Ctrl Pts',(31.5714518561759,19.7711784258222,42.6421580080922));
#65958=CARTESIAN_POINT('Ctrl Pts',(31.5585046905944,19.7547985677908,42.640858165872));
#65959=CARTESIAN_POINT('Ctrl Pts',(31.4531020366705,19.625670549647,42.6305917799314));
#65960=CARTESIAN_POINT('Ctrl Pts',(31.348783583765,19.5231517071789,42.6222972106831));
#65961=CARTESIAN_POINT('Ctrl Pts',(31.1522192550037,19.3683413067374,42.607733877715));
#65962=CARTESIAN_POINT('Ctrl Pts',(31.065299046134,19.3103095943194,42.6015870998899));
#65963=CARTESIAN_POINT('Ctrl Pts',(30.950210931497,19.2458947260354,42.5934954889346));
#65964=CARTESIAN_POINT('Ctrl Pts',(30.9259022214463,19.2329428170392,42.5917896427069));
#65965=CARTESIAN_POINT('Ctrl Pts',(30.8851705828402,19.2123118602091,42.5889321914148));
#65966=CARTESIAN_POINT('Ctrl Pts',(30.868896778849,19.2043457463301,42.5877907713088));
#65967=CARTESIAN_POINT('Ctrl Pts',(30.8366861879101,19.189118885503,42.5855308771848));
#65968=CARTESIAN_POINT('Ctrl Pts',(30.8207578137248,19.181844130218,42.5844130170794));
#65969=CARTESIAN_POINT('Ctrl Pts',(30.7816198418871,19.1645882685318,42.5816645212597));
#65970=CARTESIAN_POINT('Ctrl Pts',(30.7583129424412,19.1548368133841,42.5800262465445));
#65971=CARTESIAN_POINT('Ctrl Pts',(30.6717441441524,19.1205341771257,42.5739328612329));
#65972=CARTESIAN_POINT('Ctrl Pts',(30.607432564907,19.0987751506924,42.5693878513425));
#65973=CARTESIAN_POINT('Ctrl Pts',(30.4068035182065,19.0421143495591,42.5551699072351));
#65974=CARTESIAN_POINT('Ctrl Pts',(30.2678041893015,19.0183136036796,42.5452358089471));
#65975=CARTESIAN_POINT('Ctrl Pts',(30.0714759004091,19.0057413075797,42.5316735555465));
#65976=CARTESIAN_POINT('Ctrl Pts',(30.0153432144867,19.0045195430497,42.5278542043979));
#65977=CARTESIAN_POINT('Ctrl Pts',(29.9432685360821,19.0059929913088,42.5230821992983));
#65978=CARTESIAN_POINT('Ctrl Pts',(29.9273118104667,19.0065108789484,42.5220340858442));
#65979=CARTESIAN_POINT('Ctrl Pts',(29.9011739047343,19.0076734763786,42.5203327910777));
#65980=CARTESIAN_POINT('Ctrl Pts',(29.8909886550382,19.0082048008787,42.519673722085));
#65981=CARTESIAN_POINT('Ctrl Pts',(29.8703360291569,19.0094410676705,42.5183458022797));
#65982=CARTESIAN_POINT('Ctrl Pts',(29.8598693169807,19.0101505051507,42.5176772020547));
#65983=CARTESIAN_POINT('Ctrl Pts',(29.832117055019,19.0122516296517,42.515914913564));
#65984=CARTESIAN_POINT('Ctrl Pts',(29.8148428197703,19.013786231623,42.514828796724));
#65985=CARTESIAN_POINT('Ctrl Pts',(29.7244158106905,19.0230095849694,42.5091896341956));
#65986=CARTESIAN_POINT('Ctrl Pts',(29.6517023006379,19.0345156504993,42.5048136743417));
#65987=CARTESIAN_POINT('Ctrl Pts',(29.4589537320812,19.0760523840173,42.4932558560802));
#65988=CARTESIAN_POINT('Ctrl Pts',(29.3408069734412,19.1132646027896,42.4862010601942));
#65989=CARTESIAN_POINT('Ctrl Pts',(29.1656538300955,19.1869079081937,42.4749603253847));
#65990=CARTESIAN_POINT('Ctrl Pts',(29.105772867818,19.2156813548934,42.4709688687707));
#65991=CARTESIAN_POINT('Ctrl Pts',(29.0258867155234,19.2591000209484,42.4653640466749));
#65992=CARTESIAN_POINT('Ctrl Pts',(29.0045504669284,19.2712115304458,42.4638386821372));
#65993=CARTESIAN_POINT('Ctrl Pts',(28.9683356797835,19.2926615387827,42.4611972968128));
#65994=CARTESIAN_POINT('Ctrl Pts',(28.9533468636485,19.3018088826655,42.460088276503));
#65995=CARTESIAN_POINT('Ctrl Pts',(28.9247932172954,19.3197561735811,42.4579440574575));
#65996=CARTESIAN_POINT('Ctrl Pts',(28.9112107428233,19.3285255401895,42.456910054544));
#65997=CARTESIAN_POINT('Ctrl Pts',(28.8754577595284,19.3522297362244,42.4541499307802));
#65998=CARTESIAN_POINT('Ctrl Pts',(28.8534789418347,19.3674463436564,42.4524133227249));
#65999=CARTESIAN_POINT('Ctrl Pts',(28.7649288137391,19.4314224938838,42.4452483329025));
#66000=CARTESIAN_POINT('Ctrl Pts',(28.7011153259588,19.4838430678112,42.4396819082959));
#66001=CARTESIAN_POINT('Ctrl Pts',(28.5488401263398,19.6256172376125,42.4253779806786));
#66002=CARTESIAN_POINT('Ctrl Pts',(28.4652322333037,19.719656794287,42.4165202552595));
#66003=CARTESIAN_POINT('Ctrl Pts',(28.3593068162179,19.8642042347369,42.4041826393878));
#66004=CARTESIAN_POINT('Ctrl Pts',(28.3293495268052,19.9087465220196,42.4005363403406));
#66005=CARTESIAN_POINT('Ctrl Pts',(28.2929634341359,19.9678653145508,42.3959431402898));
#66006=CARTESIAN_POINT('Ctrl Pts',(28.2848633239259,19.9813822767893,42.3949089930114));
#66007=CARTESIAN_POINT('Ctrl Pts',(28.2718067787299,20.0037676429474,42.3932243320278));
#66008=CARTESIAN_POINT('Ctrl Pts',(28.2667565152647,20.0125802526857,42.3925681427503));
#66009=CARTESIAN_POINT('Ctrl Pts',(28.2566004007,20.0306205070616,42.39123970046));
#66010=CARTESIAN_POINT('Ctrl Pts',(28.2515000166501,20.0398507487754,42.3905677761661));
#66011=CARTESIAN_POINT('Ctrl Pts',(28.2380841581283,20.0645910968275,42.3887862430811));
#66012=CARTESIAN_POINT('Ctrl Pts',(28.2299001268923,20.0801718969074,42.3876845024781));
#66013=CARTESIAN_POINT('Ctrl Pts',(28.1853895700378,20.1677060834377,42.3815954340543));
#66014=CARTESIAN_POINT('Ctrl Pts',(28.1532401306453,20.241709148683,42.3768216717605));
#66015=CARTESIAN_POINT('Ctrl Pts',(28.0714331083094,20.4663627700938,42.3628489353929));
#66016=CARTESIAN_POINT('Ctrl Pts',(28.0351501701656,20.6211831355658,42.3538334567775));
#66017=CARTESIAN_POINT('Ctrl Pts',(28.0134736397754,20.8153329423209,42.3419885792054));
#66018=CARTESIAN_POINT('Ctrl Pts',(28.0103980253634,20.8521060429817,42.3397247170649));
#66019=CARTESIAN_POINT('Ctrl Pts',(28.0072309898124,20.9089017966257,42.3361856363779));
#66020=CARTESIAN_POINT('Ctrl Pts',(28.0064181275642,20.9288769909065,42.3349328828233));
#66021=CARTESIAN_POINT('Ctrl Pts',(28.0054661545743,20.9659974713025,42.3325883072163));
#66022=CARTESIAN_POINT('Ctrl Pts',(28.0052476073107,20.9831389711664,42.331499083713));
#66023=CARTESIAN_POINT('Ctrl Pts',(28.005253003867,21.0214845179922,42.3290469129572));
#66024=CARTESIAN_POINT('Ctrl Pts',(28.0055940749041,21.0426861968483,42.3276804180085));
#66025=CARTESIAN_POINT('Ctrl Pts',(28.0076641472113,21.1072964704847,42.3234819558119));
#66026=CARTESIAN_POINT('Ctrl Pts',(28.010473113702,21.1506551381818,42.3206170513258));
#66027=CARTESIAN_POINT('Ctrl Pts',(28.0205526017937,21.2538651082452,42.3136814387831));
#66028=CARTESIAN_POINT('Ctrl Pts',(28.0291249580706,21.3135442893453,42.3095764977217));
#66029=CARTESIAN_POINT('Ctrl Pts',(28.054235753666,21.4455599737151,42.3003112452953));
#66030=CARTESIAN_POINT('Ctrl Pts',(28.072134807481,21.5175493049864,42.2951315120848));
#66031=CARTESIAN_POINT('Ctrl Pts',(28.1194852205853,21.6709385020492,42.2839412389321));
#66032=CARTESIAN_POINT('Ctrl Pts',(28.1503132283133,21.7517683944049,42.2779460280712));
#66033=CARTESIAN_POINT('Ctrl Pts',(28.1953214898201,21.8500787316112,42.2707137719031));
#66034=CARTESIAN_POINT('Ctrl Pts',(28.2046755049513,21.8696599470592,42.2692766013212));
#66035=CARTESIAN_POINT('Ctrl Pts',(28.2194867133324,21.8994069941687,42.2671027127666));
#66036=CARTESIAN_POINT('Ctrl Pts',(28.2247153626845,21.9096839986581,42.2663534286036));
#66037=CARTESIAN_POINT('Ctrl Pts',(28.2340824457752,21.9277067737325,42.2650432659876));
#66038=CARTESIAN_POINT('Ctrl Pts',(28.2381831741793,21.9354710807231,42.2644801822454));
#66039=CARTESIAN_POINT('Ctrl Pts',(28.2483629493168,21.9544410444534,42.2631074549902));
#66040=CARTESIAN_POINT('Ctrl Pts',(28.2544983358024,21.9656158788313,42.2623013267773));
#66041=CARTESIAN_POINT('Ctrl Pts',(28.2749674002502,22.0020650085302,42.25967770656));
#66042=CARTESIAN_POINT('Ctrl Pts',(28.2897468288469,22.0270861895767,42.2578858049856));
#66043=CARTESIAN_POINT('Ctrl Pts',(28.3279251125272,22.0886102370481,42.2534799003766));
#66044=CARTESIAN_POINT('Ctrl Pts',(28.3519776719149,22.1246908536007,42.2508961110191));
#66045=CARTESIAN_POINT('Ctrl Pts',(28.4358582534647,22.2420417026369,42.2423947371187));
#66046=CARTESIAN_POINT('Ctrl Pts',(28.5006723639967,22.3195547728393,42.2366100866802));
#66047=CARTESIAN_POINT('Ctrl Pts',(28.6365159271607,22.4590185863475,42.2252465133458));
#66048=CARTESIAN_POINT('Ctrl Pts',(28.7066072725647,22.521498094724,42.2196959689649));
#66049=CARTESIAN_POINT('Ctrl Pts',(28.8025535613142,22.5955886164734,42.2122576568857));
#66050=CARTESIAN_POINT('Ctrl Pts',(28.8246220369402,22.6119142460568,42.2105573881615));
#66051=CARTESIAN_POINT('Ctrl Pts',(28.8617900261346,22.6382408986469,42.2077066846107));
#66052=CARTESIAN_POINT('Ctrl Pts',(28.8767018211409,22.6485012445305,42.206566331019));
#66053=CARTESIAN_POINT('Ctrl Pts',(28.9064919807364,22.6684070549241,42.2042935859165));
#66054=CARTESIAN_POINT('Ctrl Pts',(28.9213634255931,22.6780598904598,42.2031616131502));
#66055=CARTESIAN_POINT('Ctrl Pts',(28.9579321128833,22.701109121116,42.2003833646784));
#66056=CARTESIAN_POINT('Ctrl Pts',(28.97976088241,22.7142898722787,42.198729356614));
#66057=CARTESIAN_POINT('Ctrl Pts',(29.0106880438982,22.7321645307402,42.1963909704906));
#66058=CARTESIAN_POINT('Ctrl Pts',(29.0195788375064,22.7372122513924,42.1957193191245));
#66059=CARTESIAN_POINT('Ctrl Pts',(29.0285070576893,22.7421908694344,42.1950453911705));
#66060=CARTESIAN_POINT('',(28.0052505793236,21.0015202668116,42.170454911886));
#66061=CARTESIAN_POINT('Ctrl Pts',(29.0271745210922,22.7445458878821,42.0352855536299));
#66062=CARTESIAN_POINT('Ctrl Pts',(28.5012799340924,22.4467683092264,42.0740046256861));
#66063=CARTESIAN_POINT('Ctrl Pts',(28.0506268393321,21.8039662264705,42.1190610682745));
#66064=CARTESIAN_POINT('Ctrl Pts',(28.0027407180406,21.1005716660941,42.164117510863));
#66065=CARTESIAN_POINT('Ctrl Pts',(28.0035787417433,21.0015220175284,42.1704548813952));
#66066=CARTESIAN_POINT('Ctrl Pts',(28.0052505793236,21.0015202668116,42.170454911886));
#66067=CARTESIAN_POINT('Ctrl Pts',(28.0051970620983,20.9313000572674,42.1749515213504));
#66068=CARTESIAN_POINT('Ctrl Pts',(28.0088561147499,20.860941689876,42.1794481308147));
#66069=CARTESIAN_POINT('Ctrl Pts',(28.0162421748609,20.7908769412538,42.183944740279));
#66070=CARTESIAN_POINT('Ctrl Pts',(28.0234347506374,20.722647600285,42.1883235571074));
#66071=CARTESIAN_POINT('Ctrl Pts',(28.0341614141149,20.6546972225173,42.1927023739358));
#66072=CARTESIAN_POINT('Ctrl Pts',(28.0483828520568,20.5874250730424,42.1970811907641));
#66073=CARTESIAN_POINT('Ctrl Pts',(28.0625948263002,20.520197690021,42.2014570936958));
#66074=CARTESIAN_POINT('Ctrl Pts',(28.080296861765,20.453648133581,42.2058329966274));
#66075=CARTESIAN_POINT('Ctrl Pts',(28.1013981649582,20.3881678052964,42.210208899559));
#66076=CARTESIAN_POINT('Ctrl Pts',(28.1224930810841,20.3227072969848,42.2145834779664));
#66077=CARTESIAN_POINT('Ctrl Pts',(28.1469850689486,20.258315855221,42.2189580563738));
#66078=CARTESIAN_POINT('Ctrl Pts',(28.1747333854154,20.1953700551291,42.2233326347813));
#66079=CARTESIAN_POINT('Ctrl Pts',(28.2038274734137,20.129371433224,42.2279193768019));
#66080=CARTESIAN_POINT('Ctrl Pts',(28.2365015891748,20.0649628169976,42.2325061188226));
#66081=CARTESIAN_POINT('Ctrl Pts',(28.2725375752561,20.0025526913175,42.2370928608433));
#66082=CARTESIAN_POINT('Ctrl Pts',(28.306945100685,19.9429628695902,42.2414723286995));
#66083=CARTESIAN_POINT('Ctrl Pts',(28.3444168594674,19.8851952172695,42.2458517965558));
#66084=CARTESIAN_POINT('Ctrl Pts',(28.3847181329207,19.8295761227722,42.250231264412));
#66085=CARTESIAN_POINT('Ctrl Pts',(28.425045663941,19.7739207906584,42.2546135856315));
#66086=CARTESIAN_POINT('Ctrl Pts',(28.468206055754,19.720417189919,42.2589959068509));
#66087=CARTESIAN_POINT('Ctrl Pts',(28.5139250492059,19.6693577478817,42.2633782280704));
#66088=CARTESIAN_POINT('Ctrl Pts',(28.559717170636,19.6182166357664,42.2677675588556));
#66089=CARTESIAN_POINT('Ctrl Pts',(28.6080756938063,19.5695278285746,42.2721568896408));
#66090=CARTESIAN_POINT('Ctrl Pts',(28.6586913580752,19.52354522941,42.276546220426));
#66091=CARTESIAN_POINT('Ctrl Pts',(28.6657152795995,19.5171642370299,42.2771553266271));
#66092=CARTESIAN_POINT('Ctrl Pts',(28.6727826196441,19.5108352911583,42.2777644328282));
#66093=CARTESIAN_POINT('Ctrl Pts',(28.6798925075052,19.5045590045879,42.2783735390293));
#66094=CARTESIAN_POINT('Ctrl Pts',(28.7318946680379,19.4586538555678,42.2828285795406));
#66095=CARTESIAN_POINT('Ctrl Pts',(28.7863965406452,19.4153739995667,42.2872836200518));
#66096=CARTESIAN_POINT('Ctrl Pts',(28.8431022646294,19.3750030177276,42.2917386605631));
#66097=CARTESIAN_POINT('Ctrl Pts',(28.8997230566527,19.3346925022121,42.2961870284618));
#66098=CARTESIAN_POINT('Ctrl Pts',(28.9585407531584,19.297282494972,42.3006353963605));
#66099=CARTESIAN_POINT('Ctrl Pts',(29.0192252459494,19.2630174311994,42.3050837642592));
#66100=CARTESIAN_POINT('Ctrl Pts',(29.0798385496435,19.22879256384,42.3095269137688));
#66101=CARTESIAN_POINT('Ctrl Pts',(29.1423138760186,19.1977055517645,42.3139700632784));
#66102=CARTESIAN_POINT('Ctrl Pts',(29.2062923547168,19.1699574495879,42.318413212788));
#66103=CARTESIAN_POINT('Ctrl Pts',(29.2702307173509,19.142226746147,42.3228535763347));
#66104=CARTESIAN_POINT('Ctrl Pts',(29.3356699146653,19.1178309935652,42.3272939398814));
#66105=CARTESIAN_POINT('Ctrl Pts',(29.4022280692487,19.096924520334,42.3317343034281));
#66106=CARTESIAN_POINT('Ctrl Pts',(29.4687670770573,19.076024061265,42.336173389616));
#66107=CARTESIAN_POINT('Ctrl Pts',(29.5364239365347,19.058611035403,42.3406124758039));
#66108=CARTESIAN_POINT('Ctrl Pts',(29.6048001430737,19.044790385768,42.3450515619919));
#66109=CARTESIAN_POINT('Ctrl Pts',(29.6731798828965,19.0309690219623,42.3494908775659));
#66110=CARTESIAN_POINT('Ctrl Pts',(29.7422785635095,19.0207404975009,42.35393019314));
#66111=CARTESIAN_POINT('Ctrl Pts',(29.8116877359986,19.0141586030786,42.358369508714));
#66112=CARTESIAN_POINT('Ctrl Pts',(29.881170258328,19.0075697530785,42.3628135156433));
#66113=CARTESIAN_POINT('Ctrl Pts',(29.9509634393632,19.0046352709168,42.3672575225727));
#66114=CARTESIAN_POINT('Ctrl Pts',(30.02065492408,19.0053569400489,42.371701529502));
#66115=CARTESIAN_POINT('Ctrl Pts',(30.0903872283532,19.0060790318755,42.3761481393661));
#66116=CARTESIAN_POINT('Ctrl Pts',(30.1600172292947,19.0104615066311,42.3805947492303));
#66117=CARTESIAN_POINT('Ctrl Pts',(30.2291365865459,19.0184541420381,42.3850413590944));
#66118=CARTESIAN_POINT('Ctrl Pts',(30.2983756802342,19.0264606232,42.3894956718835));
#66119=CARTESIAN_POINT('Ctrl Pts',(30.3671018821523,19.0380896669233,42.3939499846726));
#66120=CARTESIAN_POINT('Ctrl Pts',(30.4349167450651,19.053239874211,42.3984042974617));
#66121=CARTESIAN_POINT('Ctrl Pts',(30.4699332417016,19.0610627490167,42.4007043010611));
#66122=CARTESIAN_POINT('Ctrl Pts',(30.504706996052,19.069823623548,42.4030043046606));
#66123=CARTESIAN_POINT('Ctrl Pts',(30.5391850306961,19.0795034326578,42.4053043082601));
#66124=CARTESIAN_POINT('Ctrl Pts',(30.6059679644354,19.0982529367134,42.4097593472311));
#66125=CARTESIAN_POINT('Ctrl Pts',(30.6719032715288,19.1205269599281,42.4142143862021));
#66126=CARTESIAN_POINT('Ctrl Pts',(30.7365921789036,19.1462309948437,42.4186694251731));
#66127=CARTESIAN_POINT('Ctrl Pts',(30.8011841973056,19.1718965310795,42.4231177915295));
#66128=CARTESIAN_POINT('Ctrl Pts',(30.864533070189,19.2009817031991,42.4275661578858));
#66129=CARTESIAN_POINT('Ctrl Pts',(30.9262543062639,19.2333419904725,42.4320145242422));
#66130=CARTESIAN_POINT('Ctrl Pts',(30.9879031370722,19.2656643158487,42.4364576722139));
#66131=CARTESIAN_POINT('Ctrl Pts',(31.0479276921306,19.3012538993587,42.4409008201857));
#66132=CARTESIAN_POINT('Ctrl Pts',(31.1059642961495,19.3399185146076,42.4453439681574));
#66133=CARTESIAN_POINT('Ctrl Pts',(31.1639645098387,19.3785588862242,42.4497843301698));
#66134=CARTESIAN_POINT('Ctrl Pts',(31.2199788390351,19.4202701938765,42.4542246921821));
#66135=CARTESIAN_POINT('Ctrl Pts',(31.2736703584782,19.4648155223447,42.4586650541945));
#66136=CARTESIAN_POINT('Ctrl Pts',(31.3273464325552,19.5093480365189,42.463104138854));
#66137=CARTESIAN_POINT('Ctrl Pts',(31.3787006470321,19.5567126407671,42.4675432235135));
#66138=CARTESIAN_POINT('Ctrl Pts',(31.4274285236126,19.6066316450855,42.471982308173));
#66139=CARTESIAN_POINT('Ctrl Pts',(31.4761589182559,19.6565532290195,42.4764216222267));
#66140=CARTESIAN_POINT('Ctrl Pts',(31.5222623655039,19.7090291232722,42.4808609362804));
#66141=CARTESIAN_POINT('Ctrl Pts',(31.5654719459578,19.7637455161178,42.4853002503341));
#66142=CARTESIAN_POINT('Ctrl Pts',(31.6087271894286,19.8185197321484,42.4897442557658));
#66143=CARTESIAN_POINT('Ctrl Pts',(31.6490821584572,19.8755387877348,42.4941882611975));
#66144=CARTESIAN_POINT('Ctrl Pts',(31.6863114886263,19.9344573561669,42.4986322666291));
#66145=CARTESIAN_POINT('Ctrl Pts',(31.7235626247804,19.9934104344173,42.5030788750062));
#66146=CARTESIAN_POINT('Ctrl Pts',(31.757684238794,20.0542648131004,42.5075254833834));
#66147=CARTESIAN_POINT('Ctrl Pts',(31.7884968201451,20.1166503032032,42.5119720917605));
#66148=CARTESIAN_POINT('Ctrl Pts',(31.819362778807,20.1791438650597,42.5164264030949));
#66149=CARTESIAN_POINT('Ctrl Pts',(31.8469080691786,20.2431733833983,42.5208807144293));
#66150=CARTESIAN_POINT('Ctrl Pts',(31.8710015298326,20.3083491936938,42.5253350257637));
#66151=CARTESIAN_POINT('Ctrl Pts',(31.8834423699025,20.342003214756,42.5276350430061));
#66152=CARTESIAN_POINT('Ctrl Pts',(31.8949636840046,20.3759626233232,42.5299350602484));
#66153=CARTESIAN_POINT('Ctrl Pts',(31.905552721466,20.4101725776012,42.5322350774908));
#66154=CARTESIAN_POINT('Ctrl Pts',(31.9260632604963,20.4764358810417,42.5366901182433));
#66155=CARTESIAN_POINT('Ctrl Pts',(31.9431537360617,20.5439008045752,42.5411451589958));
#66156=CARTESIAN_POINT('Ctrl Pts',(31.9566870221979,20.6121811509711,42.5456001997483));
#66157=CARTESIAN_POINT('Ctrl Pts',(31.9702000385908,20.6803592291454,42.5500485678766));
#66158=CARTESIAN_POINT('Ctrl Pts',(31.9801663458684,20.7493498300388,42.5544969360049));
#66159=CARTESIAN_POINT('Ctrl Pts',(31.9864985726956,20.8187515981357,42.5589453041332));
#66160=CARTESIAN_POINT('Ctrl Pts',(31.9928233711497,20.8880719506041,42.5633884538542));
#66161=CARTESIAN_POINT('Ctrl Pts',(31.9955225122191,20.9578020273226,42.5678316035753));
#66162=CARTESIAN_POINT('Ctrl Pts',(31.9945599886851,21.0275320547108,42.5722747532963));
#66163=CARTESIAN_POINT('Ctrl Pts',(31.9935980686792,21.0972183594982,42.5767151170431));
#66164=CARTESIAN_POINT('Ctrl Pts',(31.9889790455858,21.166904126889,42.5811554807899));
#66165=CARTESIAN_POINT('Ctrl Pts',(31.9807189643372,21.2361777864553,42.5855958445367));
#66166=CARTESIAN_POINT('Ctrl Pts',(31.9724612592863,21.3054315178991,42.5900349309133));
#66167=CARTESIAN_POINT('Ctrl Pts',(31.9605646333799,21.374272891263,42.5944740172898));
#66168=CARTESIAN_POINT('Ctrl Pts',(31.9450969895518,21.4422954484692,42.5989131036663));
#66169=CARTESIAN_POINT('Ctrl Pts',(31.9296285464868,21.5103215205051,42.6033524194172));
#66170=CARTESIAN_POINT('Ctrl Pts',(31.910588830009,21.5775282158087,42.6077917351682));
#66171=CARTESIAN_POINT('Ctrl Pts',(31.888096468681,21.6435210077802,42.6122310509191));
#66172=CARTESIAN_POINT('Ctrl Pts',(31.8655803380961,21.7095835389667,42.6166750580065));
#66173=CARTESIAN_POINT('Ctrl Pts',(31.8396044384882,21.7744291424106,42.621119065094));
#66174=CARTESIAN_POINT('Ctrl Pts',(31.8103364247849,21.8376810798848,42.6255630721814));
#66175=CARTESIAN_POINT('Ctrl Pts',(31.7810512683487,21.900970065007,42.6300096821932));
#66176=CARTESIAN_POINT('Ctrl Pts',(31.7484703884075,21.9626630934782,42.634456292205));
#66177=CARTESIAN_POINT('Ctrl Pts',(31.7128072132218,22.0224084373846,42.6389029022169));
#66178=CARTESIAN_POINT('Ctrl Pts',(31.6770822583582,22.0822572787527,42.643357215136));
#66179=CARTESIAN_POINT('Ctrl Pts',(31.6382646224775,22.1401512943898,42.6478115280552));
#66180=CARTESIAN_POINT('Ctrl Pts',(31.5966103379953,22.1957687866417,42.6522658409744));
#66181=CARTESIAN_POINT('Ctrl Pts',(31.5751019851143,22.2244870965245,42.6545658428901));
#66182=CARTESIAN_POINT('Ctrl Pts',(31.5528379692989,22.2525989922404,42.6568658448059));
#66183=CARTESIAN_POINT('Ctrl Pts',(31.5298574234629,22.2800639930783,42.6591658467216));
#66184=CARTESIAN_POINT('Ctrl Pts',(31.4853447119195,22.3332629757552,42.663620889807));
#66185=CARTESIAN_POINT('Ctrl Pts',(31.4379661326844,22.3842421481272,42.6680759328923));
#66186=CARTESIAN_POINT('Ctrl Pts',(31.3879715687025,22.4326766861276,42.6725309759777));
#66187=CARTESIAN_POINT('Ctrl Pts',(31.3380518846869,22.4810386807096,42.6769793464681));
#66188=CARTESIAN_POINT('Ctrl Pts',(31.2855243411721,22.5268632677637,42.6814277169585));
#66189=CARTESIAN_POINT('Ctrl Pts',(31.2306785626744,22.5698591777206,42.6858760874489));
#66190=CARTESIAN_POINT('Ctrl Pts',(31.1758971236654,22.6128046492493,42.6903192395635));
#66191=CARTESIAN_POINT('Ctrl Pts',(31.1188032342992,22.652927733948,42.694762391678));
#66192=CARTESIAN_POINT('Ctrl Pts',(31.059721474027,22.6899757276322,42.6992055437926));
#66193=CARTESIAN_POINT('Ctrl Pts',(31.0006767593462,22.7270004913918,42.703645909951));
#66194=CARTESIAN_POINT('Ctrl Pts',(30.9396470600594,22.760953729899,42.7080862761093));
#66195=CARTESIAN_POINT('Ctrl Pts',(30.8769867235981,22.7916254768039,42.7125266422677));
#66196=CARTESIAN_POINT('Ctrl Pts',(30.8143444125776,22.8222884003957,42.71696573107));
#66197=CARTESIAN_POINT('Ctrl Pts',(30.750072834872,22.8496714914036,42.7214048198724));
#66198=CARTESIAN_POINT('Ctrl Pts',(30.6845501981602,22.8736111092483,42.7258439086747));
#66199=CARTESIAN_POINT('Ctrl Pts',(30.6190241756402,22.8975519641458,42.730283226862));
#66200=CARTESIAN_POINT('Ctrl Pts',(30.5522474261718,22.9180488269678,42.7347225450492));
#66201=CARTESIAN_POINT('Ctrl Pts',(30.4846156762315,22.9349871340272,42.7391618632364));
#66202=CARTESIAN_POINT('Ctrl Pts',(30.4169124551307,22.9519433409703,42.7436058727591));
#66203=CARTESIAN_POINT('Ctrl Pts',(30.3483529057536,22.9653333673321,42.7480498822817));
#66204=CARTESIAN_POINT('Ctrl Pts',(30.2793444322409,22.9750934789716,42.7524938918044));
#66205=CARTESIAN_POINT('Ctrl Pts',(30.2102955393635,22.9848593072643,42.7569405042544));
#66206=CARTESIAN_POINT('Ctrl Pts',(30.1407976865188,22.9909909460442,42.7613871167043));
#66207=CARTESIAN_POINT('Ctrl Pts',(30.0712621244812,22.9934766796014,42.7658337291543));
#66208=CARTESIAN_POINT('Ctrl Pts',(30.0016061056918,22.9959667192053,42.7702880444901));
#66209=CARTESIAN_POINT('Ctrl Pts',(29.9319127364352,22.9947982547328,42.7747423598258));
#66210=CARTESIAN_POINT('Ctrl Pts',(29.8625911778383,22.9900116527529,42.7791966751616));
#66211=CARTESIAN_POINT('Ctrl Pts',(29.8267970760302,22.9875400966878,42.7814966554252));
#66212=CARTESIAN_POINT('Ctrl Pts',(29.7911019902177,22.9841047330446,42.7837966356888));
#66213=CARTESIAN_POINT('Ctrl Pts',(29.7555611596385,22.9797164483387,42.7860966159524));
#66214=CARTESIAN_POINT('Ctrl Pts',(29.6867386212903,22.9712188165295,42.7905503801811));
#66215=CARTESIAN_POINT('Ctrl Pts',(29.618224219805,22.9591113772544,42.7950041444097));
#66216=CARTESIAN_POINT('Ctrl Pts',(29.5504260531578,22.9434275980393,42.7994579086384));
#66217=CARTESIAN_POINT('Ctrl Pts',(29.4827165833195,22.9277643370953,42.8039058462394));
#66218=CARTESIAN_POINT('Ctrl Pts',(29.4157219628788,22.9085341218107,42.8083537838404));
#66219=CARTESIAN_POINT('Ctrl Pts',(29.3498439234632,22.8858220060871,42.8128017214414));
#66220=CARTESIAN_POINT('Ctrl Pts',(29.2840380275424,22.8631347625579,42.8172447880753));
#66221=CARTESIAN_POINT('Ctrl Pts',(29.2193467454641,22.8369733467923,42.8216878547091));
#66222=CARTESIAN_POINT('Ctrl Pts',(29.1561584967993,22.8074731201254,42.826130921343));
#66223=CARTESIAN_POINT('Ctrl Pts',(29.1128626290442,22.7872599010618,42.8291752599577));
#66224=CARTESIAN_POINT('Ctrl Pts',(29.0702721587262,22.7654802242769,42.8322195985724));
#66225=CARTESIAN_POINT('Ctrl Pts',(29.0285070491141,22.7421908646526,42.8352639371872));
#66226=CARTESIAN_POINT('Origin',(30.,21.,34.5704548813952));
#66227=CARTESIAN_POINT('',(29.028507049119,22.7421908646553,43.7914234503344));
#66228=CARTESIAN_POINT('',(29.0285070491141,22.7421908646526,43.6351577566542));
#66229=CARTESIAN_POINT('',(29.0285070491141,22.7421908646526,34.5704548813952));
#66230=CARTESIAN_POINT('',(28.0052507762699,20.9981806434564,43.1283622955703));
#66231=CARTESIAN_POINT('Ctrl Pts',(29.0285070491189,22.7421908646553,43.7914234503344));
#66232=CARTESIAN_POINT('Ctrl Pts',(29.0340273848418,22.7452691538084,43.7910133702931));
#66233=CARTESIAN_POINT('Ctrl Pts',(29.0395624335134,22.7483212509773,43.7906048846172));
#66234=CARTESIAN_POINT('Ctrl Pts',(29.0537612093712,22.7560628579687,43.7895640570721));
#66235=CARTESIAN_POINT('Ctrl Pts',(29.0624452059104,22.7607145201542,43.7889342315292));
#66236=CARTESIAN_POINT('Ctrl Pts',(29.0821081154594,22.7710604162975,43.7875226205212));
#66237=CARTESIAN_POINT('Ctrl Pts',(29.0931064029216,22.7767173471975,43.7867430971221));
#66238=CARTESIAN_POINT('Ctrl Pts',(29.1338241456339,22.7971837588092,43.7838913701655));
#66239=CARTESIAN_POINT('Ctrl Pts',(29.1638610224724,22.8113536287464,43.7818542848881));
#66240=CARTESIAN_POINT('Ctrl Pts',(29.3160179525479,22.8785413743455,43.7717959176446));
#66241=CARTESIAN_POINT('Ctrl Pts',(29.4428836549757,22.9199939837615,43.7642179727341));
#66242=CARTESIAN_POINT('Ctrl Pts',(29.651716483836,22.9657643593753,43.7517609748197));
#66243=CARTESIAN_POINT('Ctrl Pts',(29.7314590819623,22.9782353345783,43.7470120566413));
#66244=CARTESIAN_POINT('Ctrl Pts',(29.8484626241887,22.9893278339625,43.7398884212674));
#66245=CARTESIAN_POINT('Ctrl Pts',(29.8852805793769,22.9917901492472,43.7376252659074));
#66246=CARTESIAN_POINT('Ctrl Pts',(29.9420485298013,22.9940075191057,43.73409144637));
#66247=CARTESIAN_POINT('Ctrl Pts',(29.9619630338499,22.9944867767253,43.7328434158399));
#66248=CARTESIAN_POINT('Ctrl Pts',(29.9989185556292,22.9948224736714,43.7305103597175));
#66249=CARTESIAN_POINT('Ctrl Pts',(30.0159571248355,22.9947589356791,43.729427960581));
#66250=CARTESIAN_POINT('Ctrl Pts',(30.0540024418684,22.9941295953132,43.7269951208517));
#66251=CARTESIAN_POINT('Ctrl Pts',(30.0750050120175,22.9934500992956,43.7256412157507));
#66252=CARTESIAN_POINT('Ctrl Pts',(30.1387078797509,22.9903810048485,43.7215000096877));
#66253=CARTESIAN_POINT('Ctrl Pts',(30.1813433050626,22.9869500656659,43.7186807099601));
#66254=CARTESIAN_POINT('Ctrl Pts',(30.2824167806174,22.9755364208924,43.7118807382848));
#66255=CARTESIAN_POINT('Ctrl Pts',(30.3406738782713,22.9663274651409,43.7078673643025));
#66256=CARTESIAN_POINT('Ctrl Pts',(30.4733184724307,22.9392879990787,43.6985373903687));
#66257=CARTESIAN_POINT('Ctrl Pts',(30.5472616256829,22.9197323239257,43.6931933372861));
#66258=CARTESIAN_POINT('Ctrl Pts',(30.7030379367426,22.8688008233273,43.6817588242744));
#66259=CARTESIAN_POINT('Ctrl Pts',(30.7843081090591,22.8361759992622,43.6756835567845));
#66260=CARTESIAN_POINT('Ctrl Pts',(30.8827700000907,22.7889150029293,43.6683753942372));
#66261=CARTESIAN_POINT('Ctrl Pts',(30.9022062758258,22.7791918639423,43.6669356887867));
#66262=CARTESIAN_POINT('Ctrl Pts',(30.9316720992258,22.7638442971712,43.6647618579755));
#66263=CARTESIAN_POINT('Ctrl Pts',(30.9418177474226,22.7584478813632,43.6640149904719));
#66264=CARTESIAN_POINT('Ctrl Pts',(30.9596077181047,22.748787348043,43.6627090189521));
#66265=CARTESIAN_POINT('Ctrl Pts',(30.967271096338,22.7445603431741,43.6621477128134));
#66266=CARTESIAN_POINT('Ctrl Pts',(30.9859657770612,22.7340875783383,43.6607811848628));
#66267=CARTESIAN_POINT('Ctrl Pts',(30.996965742365,22.7277868999449,43.6599794320797));
#66268=CARTESIAN_POINT('Ctrl Pts',(31.0326055503892,22.7069190404219,43.6573868350295));
#66269=CARTESIAN_POINT('Ctrl Pts',(31.0569931660467,22.6919256694566,43.6556207495053));
#66270=CARTESIAN_POINT('Ctrl Pts',(31.1167032477845,22.6534210215687,43.6512949769937));
#66271=CARTESIAN_POINT('Ctrl Pts',(31.1516151086528,22.6292974777441,43.6487640962835));
#66272=CARTESIAN_POINT('Ctrl Pts',(31.2686821724623,22.5427615951591,43.6401770480633));
#66273=CARTESIAN_POINT('Ctrl Pts',(31.3467523299261,22.4751024562536,43.6342661234127));
#66274=CARTESIAN_POINT('Ctrl Pts',(31.4848108660949,22.3353169195962,43.6227967418756));
#66275=CARTESIAN_POINT('Ctrl Pts',(31.5456345966708,22.2644150647385,43.6172730168325));
#66276=CARTESIAN_POINT('Ctrl Pts',(31.6176464029118,22.1674767146497,43.6098629474364));
#66277=CARTESIAN_POINT('Ctrl Pts',(31.6335654845117,22.1450962658228,43.6081617725193));
#66278=CARTESIAN_POINT('Ctrl Pts',(31.6592155570573,22.107411317016,43.6053085806497));
#66279=CARTESIAN_POINT('Ctrl Pts',(31.6692092342644,22.0922896077635,43.6041666298346));
#66280=CARTESIAN_POINT('Ctrl Pts',(31.6885883553778,22.0620793774653,43.6018898434879));
#66281=CARTESIAN_POINT('Ctrl Pts',(31.6979810113567,22.0469974638815,43.6007554162696));
#66282=CARTESIAN_POINT('Ctrl Pts',(31.7204028198375,22.0098990598059,43.597969305621));
#66283=CARTESIAN_POINT('Ctrl Pts',(31.7332120151956,21.9877540094034,43.5963098388384));
#66284=CARTESIAN_POINT('Ctrl Pts',(31.7824419432471,21.8987359405158,43.5896504570738));
#66285=CARTESIAN_POINT('Ctrl Pts',(31.8154427331912,21.8300547352672,43.5845340171021));
#66286=CARTESIAN_POINT('Ctrl Pts',(31.8764962800721,21.6818187765773,43.5735569566942));
#66287=CARTESIAN_POINT('Ctrl Pts',(31.90359579206,21.6020272022508,43.5676849094183));
#66288=CARTESIAN_POINT('Ctrl Pts',(31.951384729378,21.4253243950347,43.5549249165706));
#66289=CARTESIAN_POINT('Ctrl Pts',(31.9700678350653,21.32808486326,43.5480545005772));
#66290=CARTESIAN_POINT('Ctrl Pts',(31.9835296442544,21.2120363407314,43.5402927020212));
#66291=CARTESIAN_POINT('Ctrl Pts',(31.9853560760063,21.1941920816117,43.5391114915081));
#66292=CARTESIAN_POINT('Ctrl Pts',(31.9878819023384,21.1657294547423,43.5372494680481));
#66293=CARTESIAN_POINT('Ctrl Pts',(31.9887374213521,21.155126372079,43.5365606831562));
#66294=CARTESIAN_POINT('Ctrl Pts',(31.9902420389055,21.1344128517457,43.5352252778318));
#66295=CARTESIAN_POINT('Ctrl Pts',(31.9908990016263,21.1243034951469,43.5345782986958));
#66296=CARTESIAN_POINT('Ctrl Pts',(31.9923707061805,21.0986367658887,43.5329468400452));
#66297=CARTESIAN_POINT('Ctrl Pts',(31.9930802915876,21.0830736382594,43.5319679792066));
#66298=CARTESIAN_POINT('Ctrl Pts',(31.9953517571622,21.0159892800327,43.527787203557));
#66299=CARTESIAN_POINT('Ctrl Pts',(31.9950988573542,20.9644224949877,43.524671268508));
#66300=CARTESIAN_POINT('Ctrl Pts',(31.9878505935331,20.7985454912254,43.5148003657302));
#66301=CARTESIAN_POINT('Ctrl Pts',(31.9730158214738,20.6848095369619,43.5082551062922));
#66302=CARTESIAN_POINT('Ctrl Pts',(31.9283014350427,20.480781310097,43.4960647628718));
#66303=CARTESIAN_POINT('Ctrl Pts',(31.9015829706425,20.3901526504345,43.4904806667342));
#66304=CARTESIAN_POINT('Ctrl Pts',(31.8589352006138,20.2760231828673,43.4830045821435));
#66305=CARTESIAN_POINT('Ctrl Pts',(31.8487870602047,20.2504876226934,43.4813025943932));
#66306=CARTESIAN_POINT('Ctrl Pts',(31.8310797665129,20.2084808921122,43.4784493971274));
#66307=CARTESIAN_POINT('Ctrl Pts',(31.8238176276996,20.1918881045496,43.4773082886313));
#66308=CARTESIAN_POINT('Ctrl Pts',(31.8089987390734,20.1592469417025,43.4750343079978));
#66309=CARTESIAN_POINT('Ctrl Pts',(31.8014518725999,20.1431959032608,43.4739018586037));
#66310=CARTESIAN_POINT('Ctrl Pts',(31.782534687863,20.1043170371959,43.471122900093));
#66311=CARTESIAN_POINT('Ctrl Pts',(31.770938953892,20.0816030243807,43.4694686639209));
#66312=CARTESIAN_POINT('Ctrl Pts',(31.7233421620989,19.9926241996373,43.4628628046646));
#66313=CARTESIAN_POINT('Ctrl Pts',(31.6840350887696,19.9282081847288,43.4577968185174));
#66314=CARTESIAN_POINT('Ctrl Pts',(31.5413784611171,19.7217161722009,43.4406146360501));
#66315=CARTESIAN_POINT('Ctrl Pts',(31.4229490004582,19.5910752817616,43.4280771356335));
#66316=CARTESIAN_POINT('Ctrl Pts',(31.2709972643198,19.4624216554745,43.4147291983983));
#66317=CARTESIAN_POINT('Ctrl Pts',(31.2527710256067,19.4475354808809,43.4131679682555));
#66318=CARTESIAN_POINT('Ctrl Pts',(31.2250472564142,19.4256985506448,43.4108573565383));
#66319=CARTESIAN_POINT('Ctrl Pts',(31.2157453348637,19.4185041475645,43.4100926319294));
#66320=CARTESIAN_POINT('Ctrl Pts',(31.1986340863152,19.4055099590714,43.4087058441411));
#66321=CARTESIAN_POINT('Ctrl Pts',(31.1908454628857,19.3996846394145,43.4080821205776));
#66322=CARTESIAN_POINT('Ctrl Pts',(31.1725200444757,19.3861864484507,43.4066317361962));
#66323=CARTESIAN_POINT('Ctrl Pts',(31.1619502316944,19.3785595555996,43.4058081575944));
#66324=CARTESIAN_POINT('Ctrl Pts',(31.1261208434795,19.3532363396745,43.4030569789227));
#66325=CARTESIAN_POINT('Ctrl Pts',(31.1005246078938,19.33602147598,43.4011585570759));
#66326=CARTESIAN_POINT('Ctrl Pts',(31.0346986335612,19.2939336725087,43.3964156204727));
#66327=CARTESIAN_POINT('Ctrl Pts',(30.9939637494232,19.269884347901,43.3936076573272));
#66328=CARTESIAN_POINT('Ctrl Pts',(30.8489025580446,19.1910584671423,43.383909854898));
#66329=CARTESIAN_POINT('Ctrl Pts',(30.7406158838818,19.1440921324093,43.3771827697945));
#66330=CARTESIAN_POINT('Ctrl Pts',(30.5586975361323,19.0836639849032,43.3658981599773));
#66331=CARTESIAN_POINT('Ctrl Pts',(30.4873455567504,19.0642884203696,43.3614792345496));
#66332=CARTESIAN_POINT('Ctrl Pts',(30.3898087282433,19.0435377101883,43.3553456285742));
#66333=CARTESIAN_POINT('Ctrl Pts',(30.3644281339738,19.0386515925899,43.3537415699144));
#66334=CARTESIAN_POINT('Ctrl Pts',(30.3231856491976,19.0315399804467,43.3511186350178));
#66335=CARTESIAN_POINT('Ctrl Pts',(30.3073788591667,19.0290098870719,43.3501094953364));
#66336=CARTESIAN_POINT('Ctrl Pts',(30.2740533736098,19.0240863127295,43.3479729721359));
#66337=CARTESIAN_POINT('Ctrl Pts',(30.2565299557451,19.0217349773851,43.346844349799));
#66338=CARTESIAN_POINT('Ctrl Pts',(30.2138821295975,19.016588551608,43.3440839754862));
#66339=CARTESIAN_POINT('Ctrl Pts',(30.1887319229865,19.0140375878038,43.3424447043373));
#66340=CARTESIAN_POINT('Ctrl Pts',(30.0904452194266,19.00595226514,43.3359910516247));
#66341=CARTESIAN_POINT('Ctrl Pts',(30.0170817699942,19.0039757621825,43.3310689079429));
#66342=CARTESIAN_POINT('Ctrl Pts',(29.7843679209693,19.0105368229914,43.3151489816202));
#66343=CARTESIAN_POINT('Ctrl Pts',(29.6260817985685,19.0341309674039,43.3038147911729));
#66344=CARTESIAN_POINT('Ctrl Pts',(29.4377187319013,19.0858022009012,43.2905305088687));
#66345=CARTESIAN_POINT('Ctrl Pts',(29.4033967692643,19.096219976235,43.2881215268011));
#66346=CARTESIAN_POINT('Ctrl Pts',(29.3559646359744,19.1120260238118,43.2848255770495));
#66347=CARTESIAN_POINT('Ctrl Pts',(29.3426045357498,19.1166363823728,43.2839009580244));
#66348=CARTESIAN_POINT('Ctrl Pts',(29.3200101810381,19.1247030671766,43.2823449731727));
#66349=CARTESIAN_POINT('Ctrl Pts',(29.3107506811249,19.1280865047484,43.2817095546446));
#66350=CARTESIAN_POINT('Ctrl Pts',(29.2910993191093,19.1354327417787,43.2803661908165));
#66351=CARTESIAN_POINT('Ctrl Pts',(29.2807149857724,19.1394139852677,43.2796593137605));
#66352=CARTESIAN_POINT('Ctrl Pts',(29.2514427676125,19.1509183489061,43.2776737386625));
#66353=CARTESIAN_POINT('Ctrl Pts',(29.2326352716421,19.1586438881002,43.2764063304131));
#66354=CARTESIAN_POINT('Ctrl Pts',(29.1895969138712,19.1770967107957,43.2735180699403));
#66355=CARTESIAN_POINT('Ctrl Pts',(29.1654547828793,19.1880220824636,43.2719068328023));
#66356=CARTESIAN_POINT('Ctrl Pts',(29.0813298082701,19.2281305227763,43.2662997701629));
#66357=CARTESIAN_POINT('Ctrl Pts',(29.0225969355971,19.2598388824206,43.2623976737636));
#66358=CARTESIAN_POINT('Ctrl Pts',(28.8357247808209,19.3731782763768,43.249687921577));
#66359=CARTESIAN_POINT('Ctrl Pts',(28.715318195442,19.4664831235668,43.2409774235967));
#66360=CARTESIAN_POINT('Ctrl Pts',(28.58462819906,19.5940489199549,43.2298230006952));
#66361=CARTESIAN_POINT('Ctrl Pts',(28.5630944216885,19.6160643166225,43.2279226427976));
#66362=CARTESIAN_POINT('Ctrl Pts',(28.5292651093641,19.6522912138913,43.2248280116066));
#66363=CARTESIAN_POINT('Ctrl Pts',(28.5166452869764,19.666193849358,43.2236477555485));
#66364=CARTESIAN_POINT('Ctrl Pts',(28.4927276307034,19.6933020587124,43.2213590918447));
#66365=CARTESIAN_POINT('Ctrl Pts',(28.4814023913869,19.7064812422387,43.2202519819266));
#66366=CARTESIAN_POINT('Ctrl Pts',(28.4552608911049,19.7377186513514,43.2176398380794));
#66367=CARTESIAN_POINT('Ctrl Pts',(28.4405870448702,19.7558921766655,43.216129211817));
#66368=CARTESIAN_POINT('Ctrl Pts',(28.3914121465172,19.8190322978477,43.2109092976681));
#66369=CARTESIAN_POINT('Ctrl Pts',(28.358512638366,19.8652058332883,43.2071392820906));
#66370=CARTESIAN_POINT('Ctrl Pts',(28.2776772929377,19.9895401042565,43.1971085462961));
#66371=CARTESIAN_POINT('Ctrl Pts',(28.2330863828662,20.0697106599523,43.1907536704131));
#66372=CARTESIAN_POINT('Ctrl Pts',(28.1471594836605,20.2528350855162,43.1766482753025));
#66373=CARTESIAN_POINT('Ctrl Pts',(28.108566446692,20.356761116617,43.1689034170037));
#66374=CARTESIAN_POINT('Ctrl Pts',(28.0730720104802,20.4838333496819,43.1600844304603));
#66375=CARTESIAN_POINT('Ctrl Pts',(28.0676802889236,20.5043992455265,43.1586771868361));
#66376=CARTESIAN_POINT('Ctrl Pts',(28.0598942369577,20.5361594384987,43.1565387148991));
#66377=CARTESIAN_POINT('Ctrl Pts',(28.0572658950715,20.547294078642,43.1557955172322));
#66378=CARTESIAN_POINT('Ctrl Pts',(28.0525678977407,20.5679913466663,43.1544268973397));
#66379=CARTESIAN_POINT('Ctrl Pts',(28.0504726747473,20.5775470653204,43.1538001653878));
#66380=CARTESIAN_POINT('Ctrl Pts',(28.0456444465739,20.6003684754785,43.1523151272805));
#66381=CARTESIAN_POINT('Ctrl Pts',(28.0429761116337,20.6136471700731,43.1514604052235));
#66382=CARTESIAN_POINT('Ctrl Pts',(28.0375339726221,20.6422338227295,43.1496383806582));
#66383=CARTESIAN_POINT('Ctrl Pts',(28.0348035627497,20.6575492134602,43.1486732776327));
#66384=CARTESIAN_POINT('Ctrl Pts',(28.0143824897498,20.780395314158,43.1410090841369));
#66385=CARTESIAN_POINT('Ctrl Pts',(28.0053502109873,20.8891881959974,43.1346859693093));
#66386=CARTESIAN_POINT('Ctrl Pts',(28.0052508292294,20.9981811514481,43.1283621734979));
#66387=CARTESIAN_POINT('Ctrl Pts',(28.0052508296975,20.9981806381507,43.1283622032795));
#66388=CARTESIAN_POINT('Ctrl Pts',(28.0051575468002,21.100456049772,43.1224281608178));
#66389=CARTESIAN_POINT('Ctrl Pts',(28.0129302759012,21.2025865436209,43.1165093493538));
#66390=CARTESIAN_POINT('Ctrl Pts',(28.0348692664432,21.3450208815619,43.1078833761945));
#66391=CARTESIAN_POINT('Ctrl Pts',(28.0425379878242,21.3861610186594,43.1053486980223));
#66392=CARTESIAN_POINT('Ctrl Pts',(28.057019440693,21.4522391565893,43.1011874450745));
#66393=CARTESIAN_POINT('Ctrl Pts',(28.0630332747366,21.4773400446866,43.0995854429704));
#66394=CARTESIAN_POINT('Ctrl Pts',(28.0740113161425,21.5195301039075,43.0968530359029));
#66395=CARTESIAN_POINT('Ctrl Pts',(28.078720336925,21.5366827390298,43.0957309424151));
#66396=CARTESIAN_POINT('Ctrl Pts',(28.0886634353991,21.5710912275362,43.093456247345));
#66397=CARTESIAN_POINT('Ctrl Pts',(28.0939033635702,21.5883436331431,43.092303545833));
#66398=CARTESIAN_POINT('Ctrl Pts',(28.1075990639989,21.6313319391092,43.0893996912599));
#66399=CARTESIAN_POINT('Ctrl Pts',(28.116346347439,21.656970408273,43.0876391223986));
#66400=CARTESIAN_POINT('Ctrl Pts',(28.1553294756208,21.7640441893786,43.0801614552955));
#66401=CARTESIAN_POINT('Ctrl Pts',(28.1903421633059,21.8436278410252,43.0742899891985));
#66402=CARTESIAN_POINT('Ctrl Pts',(28.3002606114928,22.0548971436403,43.0578838579579));
#66403=CARTESIAN_POINT('Ctrl Pts',(28.3851390032103,22.1807392304034,43.0471438130278));
#66404=CARTESIAN_POINT('Ctrl Pts',(28.5026476520882,22.3182712363283,43.0349254220984));
#66405=CARTESIAN_POINT('Ctrl Pts',(28.5223682166808,22.3403386262353,43.0329498539754));
#66406=CARTESIAN_POINT('Ctrl Pts',(28.5513376477725,22.3713386570934,43.0301624731613));
#66407=CARTESIAN_POINT('Ctrl Pts',(28.5601922592514,22.3806324688641,43.0293251988895));
#66408=CARTESIAN_POINT('Ctrl Pts',(28.5752607218007,22.3961457004857,43.0279258671541));
#66409=CARTESIAN_POINT('Ctrl Pts',(28.5814268631953,22.4024104585032,43.0273603147149));
#66410=CARTESIAN_POINT('Ctrl Pts',(28.5957329398242,22.4167544249713,43.0260644996492));
#66411=CARTESIAN_POINT('Ctrl Pts',(28.6039013996792,22.4248044744791,43.0253364793193));
#66412=CARTESIAN_POINT('Ctrl Pts',(28.6275141550667,22.4476768850051,43.0232640588527));
#66413=CARTESIAN_POINT('Ctrl Pts',(28.6431286927497,22.4623221598299,43.0219322806814));
#66414=CARTESIAN_POINT('Ctrl Pts',(28.7646585951437,22.5726850625445,43.0118306323689));
#66415=CARTESIAN_POINT('Ctrl Pts',(28.8803508011276,22.6570463917626,43.0036987174494));
#66416=CARTESIAN_POINT('Ctrl Pts',(29.0121854654742,22.7330140496434,42.9948466360735));
#66417=CARTESIAN_POINT('Ctrl Pts',(29.0203307266711,22.7376315252329,42.9943013992332));
#66418=CARTESIAN_POINT('Ctrl Pts',(29.0285070614011,22.7421908715042,42.9937555338539));
#66419=CARTESIAN_POINT('',(28.0052500657895,21.0005123153922,42.9704548813466));
#66420=CARTESIAN_POINT('Ctrl Pts',(29.0285070491141,22.7421908646526,42.8352639371872));
#66421=CARTESIAN_POINT('Ctrl Pts',(28.9676043214511,22.7082298493501,42.8397032533362));
#66422=CARTESIAN_POINT('Ctrl Pts',(28.9084579756291,22.6710567323345,42.8441425694852));
#66423=CARTESIAN_POINT('Ctrl Pts',(28.8514195787486,22.630886439461,42.8485818856342));
#66424=CARTESIAN_POINT('Ctrl Pts',(28.7943843275944,22.5907183620206,42.8530209569504));
#66425=CARTESIAN_POINT('Ctrl Pts',(28.7394571936289,22.5475537200229,42.8574600282666));
#66426=CARTESIAN_POINT('Ctrl Pts',(28.6869597943234,22.5016500859976,42.8618990995827));
#66427=CARTESIAN_POINT('Ctrl Pts',(28.6344105100008,22.4557010838044,42.8663425581884));
#66428=CARTESIAN_POINT('Ctrl Pts',(28.5842961259823,22.407008005524,42.8707860167941));
#66429=CARTESIAN_POINT('Ctrl Pts',(28.5369035317666,22.3558673560282,42.8752294753998));
#66430=CARTESIAN_POINT('Ctrl Pts',(28.4894877185934,22.3047016512978,42.8796751109802));
#66431=CARTESIAN_POINT('Ctrl Pts',(28.4447966652341,22.2510863630922,42.8841207465606));
#66432=CARTESIAN_POINT('Ctrl Pts',(28.4030770036123,22.1953512061767,42.8885663821409));
#66433=CARTESIAN_POINT('Ctrl Pts',(28.3612809330586,22.1395139711608,42.8930201598359));
#66434=CARTESIAN_POINT('Ctrl Pts',(28.3224673990012,22.0815495186362,42.8974739375308));
#66435=CARTESIAN_POINT('Ctrl Pts',(28.2868393962484,22.0218161812447,42.9019277152258));
#66436=CARTESIAN_POINT('Ctrl Pts',(28.2572421195932,21.9721938624023,42.9056276052116));
#66437=CARTESIAN_POINT('Ctrl Pts',(28.2298424575127,21.9213514203603,42.9093274951974));
#66438=CARTESIAN_POINT('Ctrl Pts',(28.2047316173072,21.8695050296597,42.9130273851831));
#66439=CARTESIAN_POINT('Ctrl Pts',(28.172226069602,21.802390774921,42.9178168286845));
#66440=CARTESIAN_POINT('Ctrl Pts',(28.1434437524186,21.7333607547642,42.9226062721859));
#66441=CARTESIAN_POINT('Ctrl Pts',(28.1185963344277,21.6628331688072,42.9273957156873));
#66442=CARTESIAN_POINT('Ctrl Pts',(28.0938078213605,21.5924727801853,42.9321738050188));
#66443=CARTESIAN_POINT('Ctrl Pts',(28.0729357673716,21.5206222383229,42.9369518943504));
#66444=CARTESIAN_POINT('Ctrl Pts',(28.0561447218307,21.4477211409275,42.9417299836819));
#66445=CARTESIAN_POINT('Ctrl Pts',(28.0393206654845,21.3746767216689,42.946517466626));
#66446=CARTESIAN_POINT('Ctrl Pts',(28.026593877544,21.3005779437398,42.9513049495702));
#66447=CARTESIAN_POINT('Ctrl Pts',(28.018081031935,21.2258866231632,42.9560924325143));
#66448=CARTESIAN_POINT('Ctrl Pts',(28.009568186326,21.1511953025866,42.9608799154584));
#66449=CARTESIAN_POINT('Ctrl Pts',(28.0052694307819,21.0759118017932,42.9656673984025));
#66450=CARTESIAN_POINT('Ctrl Pts',(28.0052500657895,21.0005123153922,42.9704548813466));
#66451=CARTESIAN_POINT('Ctrl Pts',(28.0052500657893,21.0005123146269,42.9704548813952));
#66452=CARTESIAN_POINT('Ctrl Pts',(28.0052315890006,20.9285710288132,42.9750227862344));
#66453=CARTESIAN_POINT('Ctrl Pts',(28.0091093251767,20.8566709192213,42.9795906910737));
#66454=CARTESIAN_POINT('Ctrl Pts',(28.0168438583246,20.7852460006537,42.9841585959129));
#66455=CARTESIAN_POINT('Ctrl Pts',(28.0247173355178,20.7125379966142,42.9888085591213));
#66456=CARTESIAN_POINT('Ctrl Pts',(28.0365874783279,20.6403229044772,42.9934585223298));
#66457=CARTESIAN_POINT('Ctrl Pts',(28.0523582884808,20.5690483483606,42.9981084855382));
#66458=CARTESIAN_POINT('Ctrl Pts',(28.0678961341488,20.4988266512979,43.0026897600569));
#66459=CARTESIAN_POINT('Ctrl Pts',(28.0872199703106,20.4295183000286,43.0072710345757));
#66460=CARTESIAN_POINT('Ctrl Pts',(28.110187832642,20.3615350169306,43.0118523090945));
#66461=CARTESIAN_POINT('Ctrl Pts',(28.1336722430523,20.2920227872651,43.0165366166477));
#66462=CARTESIAN_POINT('Ctrl Pts',(28.1609663851651,20.2238964124189,43.021220924201));
#66463=CARTESIAN_POINT('Ctrl Pts',(28.1918677488796,20.1575717686602,43.0259052317542));
#66464=CARTESIAN_POINT('Ctrl Pts',(28.2227691125942,20.0912471249015,43.0305895393075));
#66465=CARTESIAN_POINT('Ctrl Pts',(28.2572774009503,20.0267246113575,43.0352738468607));
#66466=CARTESIAN_POINT('Ctrl Pts',(28.2951427975274,19.9643893194461,43.0399581544139));
#66467=CARTESIAN_POINT('Ctrl Pts',(28.3311550803602,19.9051046858306,43.0444132142768));
#66468=CARTESIAN_POINT('Ctrl Pts',(28.370334308345,19.8475839752533,43.0488682741397));
#66469=CARTESIAN_POINT('Ctrl Pts',(28.4124822494109,19.7921858776846,43.0533233340026));
#66470=CARTESIAN_POINT('Ctrl Pts',(28.4545670645535,19.7368707510979,43.0577717214217));
#66471=CARTESIAN_POINT('Ctrl Pts',(28.4996114739023,19.6836723139527,43.0622201088408));
#66472=CARTESIAN_POINT('Ctrl Pts',(28.5473729125965,19.6329220550964,43.0666684962599));
#66473=CARTESIAN_POINT('Ctrl Pts',(28.5950783241406,19.582231329463,43.0711116654428));
#66474=CARTESIAN_POINT('Ctrl Pts',(28.6454941009277,19.5339834327497,43.0755548346257));
#66475=CARTESIAN_POINT('Ctrl Pts',(28.6983373245162,19.488476979417,43.0799980038085));
#66476=CARTESIAN_POINT('Ctrl Pts',(28.7511474152525,19.4429990587606,43.0844383871116));
#66477=CARTESIAN_POINT('Ctrl Pts',(28.806381563471,19.4002594900602,43.0888787704147));
#66478=CARTESIAN_POINT('Ctrl Pts',(28.8637209981286,19.3605191088621,43.0933191537178));
#66479=CARTESIAN_POINT('Ctrl Pts',(28.921043938715,19.3207901592502,43.097758259715));
#66480=CARTESIAN_POINT('Ctrl Pts',(28.9804705615396,19.2840589629842,43.1021973657121));
#66481=CARTESIAN_POINT('Ctrl Pts',(29.041651544354,19.2505441417227,43.1066364717093));
#66482=CARTESIAN_POINT('Ctrl Pts',(29.1028356889423,19.2170275884477,43.1110758071152));
#66483=CARTESIAN_POINT('Ctrl Pts',(29.1657739432408,19.1867279731321,43.1155151425211));
#66484=CARTESIAN_POINT('Ctrl Pts',(29.2300922897317,19.1598180306911,43.1199544779269));
#66485=CARTESIAN_POINT('Ctrl Pts',(29.2944786044112,19.1328796512622,43.124398504585));
#66486=CARTESIAN_POINT('Ctrl Pts',(29.3602474698537,19.109338283279,43.1288425312431));
#66487=CARTESIAN_POINT('Ctrl Pts',(29.4270056846385,19.0893181643551,43.1332865579012));
#66488=CARTESIAN_POINT('Ctrl Pts',(29.4938030002935,19.0692863194725,43.1377331874646));
#66489=CARTESIAN_POINT('Ctrl Pts',(29.5615903431448,19.0527799444847,43.1421798170279));
#66490=CARTESIAN_POINT('Ctrl Pts',(29.6299628912134,19.0398724274627,43.1466264465913));
#66491=CARTESIAN_POINT('Ctrl Pts',(29.6984538775444,19.0269425514103,43.1510807788233));
#66492=CARTESIAN_POINT('Ctrl Pts',(29.7675316077972,19.0176240426951,43.1555351110552));
#66493=CARTESIAN_POINT('Ctrl Pts',(29.836785498685,19.0119384845884,43.1599894432872));
#66494=CARTESIAN_POINT('Ctrl Pts',(29.8725421385118,19.0090029606659,43.162289270073));
#66495=CARTESIAN_POINT('Ctrl Pts',(29.9083457252291,19.0070350495679,43.1645890968589));
#66496=CARTESIAN_POINT('Ctrl Pts',(29.9441400223946,19.0060322907825,43.1668889236447));
#66497=CARTESIAN_POINT('Ctrl Pts',(30.013476684111,19.0040898599434,43.1713438878285));
#66498=CARTESIAN_POINT('Ctrl Pts',(30.0830513640872,19.0057644992935,43.1757988520123));
#66499=CARTESIAN_POINT('Ctrl Pts',(30.1524552307818,19.0110844751204,43.1802538161961));
#66500=CARTESIAN_POINT('Ctrl Pts',(30.2217551433558,19.0163964826101,43.1847021076697));
#66501=CARTESIAN_POINT('Ctrl Pts',(30.2908842665054,19.025342952452,43.1891503991434));
#66502=CARTESIAN_POINT('Ctrl Pts',(30.3594325425419,19.0379001529326,43.1935986906171));
#66503=CARTESIAN_POINT('Ctrl Pts',(30.4279004065346,19.0504426229165,43.1980417639258));
#66504=CARTESIAN_POINT('Ctrl Pts',(30.4957882977253,19.0665873231396,43.2024848372346));
#66505=CARTESIAN_POINT('Ctrl Pts',(30.5626918572463,19.0862587854444,43.2069279105433));
#66506=CARTESIAN_POINT('Ctrl Pts',(30.6295534686227,19.1059179138562,43.2113681980708));
#66507=CARTESIAN_POINT('Ctrl Pts',(30.6954315043164,19.1290992798999,43.2158084855983));
#66508=CARTESIAN_POINT('Ctrl Pts',(30.7599338670361,19.1556767961576,43.2202487731258));
#66509=CARTESIAN_POINT('Ctrl Pts',(30.8244176783201,19.1822466684924,43.2246877835883));
#66510=CARTESIAN_POINT('Ctrl Pts',(30.8875261499109,19.212210565625,43.2291267940508));
#66511=CARTESIAN_POINT('Ctrl Pts',(30.9488860490246,19.2453938252512,43.2335658045134));
#66512=CARTESIAN_POINT('Ctrl Pts',(31.0102491245282,19.2785788026602,43.2380050447681));
#66513=CARTESIAN_POINT('Ctrl Pts',(31.0698630185928,19.3149832385465,43.2424442850229));
#66514=CARTESIAN_POINT('Ctrl Pts',(31.1273796268829,19.3543868196355,43.2468835252776));
#66515=CARTESIAN_POINT('Ctrl Pts',(31.1849570328943,19.3938320521364,43.2513274580151));
#66516=CARTESIAN_POINT('Ctrl Pts',(31.2404323239127,19.4362824802109,43.2557713907526));
#66517=CARTESIAN_POINT('Ctrl Pts',(31.2934877086317,19.481475350836,43.2602153234901));
#66518=CARTESIAN_POINT('Ctrl Pts',(31.3465741757035,19.5266946975814,43.2646618596935));
#66519=CARTESIAN_POINT('Ctrl Pts',(31.3972375592853,19.5746593482535,43.269108395897));
#66520=CARTESIAN_POINT('Ctrl Pts',(31.4451964630248,19.6250691851003,43.2735549321004));
#66521=CARTESIAN_POINT('Ctrl Pts',(31.4932384653383,19.6755663672623,43.2780091728339));
#66522=CARTESIAN_POINT('Ctrl Pts',(31.5385663157919,19.728516821037,43.2824634135674));
#66523=CARTESIAN_POINT('Ctrl Pts',(31.5809389961577,19.7835874659771,43.2869176543009));
#66524=CARTESIAN_POINT('Ctrl Pts',(31.6028250961605,19.8120322476614,43.2892183338258));
#66525=CARTESIAN_POINT('Ctrl Pts',(31.6239235044829,19.841042193907,43.2915190133506));
#66526=CARTESIAN_POINT('Ctrl Pts',(31.64420572578,19.8705686856598,43.2938196928755));
#66527=CARTESIAN_POINT('Ctrl Pts',(31.6834810122304,19.9277449389153,43.2982748186748));
#66528=CARTESIAN_POINT('Ctrl Pts',(31.7198476813952,19.987084883945,43.3027299444742));
#66529=CARTESIAN_POINT('Ctrl Pts',(31.7530600371333,20.0482605037583,43.3071850702736));
#66530=CARTESIAN_POINT('Ctrl Pts',(31.7862226458395,20.1093444918449,43.3116335229755));
#66531=CARTESIAN_POINT('Ctrl Pts',(31.816240087075,20.1722582708793,43.3160819756775));
#66532=CARTESIAN_POINT('Ctrl Pts',(31.842909667823,20.2366445659166,43.3205304283794));
#66533=CARTESIAN_POINT('Ctrl Pts',(31.8695479563459,20.3009553145682,43.3249736615774));
#66534=CARTESIAN_POINT('Ctrl Pts',(31.8928459999688,20.3667346977639,43.3294168947754));
#66535=CARTESIAN_POINT('Ctrl Pts',(31.9126476483465,20.4336021400337,43.3338601279733));
#66536=CARTESIAN_POINT('Ctrl Pts',(31.9324368775625,20.5004276445029,43.3383005744724));
#66537=CARTESIAN_POINT('Ctrl Pts',(31.9487339231779,20.5683393862088,43.3427410209715));
#66538=CARTESIAN_POINT('Ctrl Pts',(31.9614318018113,20.6369396064796,43.3471814674706));
#66539=CARTESIAN_POINT('Ctrl Pts',(31.9741260252756,20.7055200797189,43.3516206357575));
#66540=CARTESIAN_POINT('Ctrl Pts',(31.9832230495419,20.7747881572225,43.3560598040443));
#66541=CARTESIAN_POINT('Ctrl Pts',(31.9886669258629,20.8443355516529,43.3604989723312));
#66542=CARTESIAN_POINT('Ctrl Pts',(31.9941110822947,20.9138865245966,43.3649383690325));
#66543=CARTESIAN_POINT('Ctrl Pts',(31.9959016818207,20.9837163550337,43.3693777657337));
#66544=CARTESIAN_POINT('Ctrl Pts',(31.9940347554633,21.0534130742823,43.373817162435));
#66545=CARTESIAN_POINT('Ctrl Pts',(31.992165857069,21.1231834142757,43.3782612484774));
#66546=CARTESIAN_POINT('Ctrl Pts',(31.986631734867,21.1928198723889,43.3827053345197));
#66547=CARTESIAN_POINT('Ctrl Pts',(31.9774805175999,21.2619128958506,43.3871494205621));
#66548=CARTESIAN_POINT('Ctrl Pts',(31.9683239425112,21.3310463716458,43.3915961085119));
#66549=CARTESIAN_POINT('Ctrl Pts',(31.9555461468695,21.3996352983827,43.3960427964617));
#66550=CARTESIAN_POINT('Ctrl Pts',(31.9392463972668,21.467280401031,43.4004894844115));
#66551=CARTESIAN_POINT('Ctrl Pts',(31.9229184207272,21.5350426474448,43.404943872871));
#66552=CARTESIAN_POINT('Ctrl Pts',(31.9030564551207,21.6018573383214,43.4093982613305));
#66553=CARTESIAN_POINT('Ctrl Pts',(31.8798093706742,21.6673412113945,43.41385264979));
#66554=CARTESIAN_POINT('Ctrl Pts',(31.8678096669461,21.7011427436964,43.4161519205621));
#66555=CARTESIAN_POINT('Ctrl Pts',(31.8549088062018,21.7345900268675,43.4184511913341));
#66556=CARTESIAN_POINT('Ctrl Pts',(31.8411320983547,21.7676328281854,43.4207504621062));
#66557=CARTESIAN_POINT('Ctrl Pts',(31.8144377949317,21.8316578894787,43.4252056216641));
#66558=CARTESIAN_POINT('Ctrl Pts',(31.7843472742764,21.8944148897016,43.4296607812221));
#66559=CARTESIAN_POINT('Ctrl Pts',(31.7510026322809,21.955519410711,43.43411594078));
#66560=CARTESIAN_POINT('Ctrl Pts',(31.7177079207047,22.0165324335313,43.4385644291616));
#66561=CARTESIAN_POINT('Ctrl Pts',(31.6811689916526,22.0758974623613,43.4430129175432));
#66562=CARTESIAN_POINT('Ctrl Pts',(31.6415758573719,22.1332503108289,43.4474614059249));
#66563=CARTESIAN_POINT('Ctrl Pts',(31.6020291550945,22.1905358999674,43.4519046774367));
#66564=CARTESIAN_POINT('Ctrl Pts',(31.5594356381618,22.2458135948522,43.4563479489484));
#66565=CARTESIAN_POINT('Ctrl Pts',(31.5140301536994,22.2987456472261,43.4607912204603));
#66566=CARTESIAN_POINT('Ctrl Pts',(31.4686531299256,22.3516445211707,43.4652317068775));
#66567=CARTESIAN_POINT('Ctrl Pts',(31.4204679530832,22.4022002988704,43.4696721932948));
#66568=CARTESIAN_POINT('Ctrl Pts',(31.3697505923319,22.4501071951088,43.4741126797121));
#66569=CARTESIAN_POINT('Ctrl Pts',(31.3190478133056,22.4980003176575,43.4785518894471));
#66570=CARTESIAN_POINT('Ctrl Pts',(31.2658146511744,22.5432457348615,43.4829910991822));
#66571=CARTESIAN_POINT('Ctrl Pts',(31.2103636225341,22.5855748054715,43.4874303089173));
#66572=CARTESIAN_POINT('Ctrl Pts',(31.1549097225232,22.6279060679697,43.4918697485239));
#66573=CARTESIAN_POINT('Ctrl Pts',(31.0972381183589,22.6673203891063,43.4963091881306));
#66574=CARTESIAN_POINT('Ctrl Pts',(31.0376926367861,22.7035907824533,43.5007486277373));
#66575=CARTESIAN_POINT('Ctrl Pts',(30.9780842325639,22.739899503297,43.5051927585698));
#66576=CARTESIAN_POINT('Ctrl Pts',(30.9165984174146,22.7730574104877,43.5096368894023));
#66577=CARTESIAN_POINT('Ctrl Pts',(30.8536052719579,22.802882581364,43.5140810202348));
#66578=CARTESIAN_POINT('Ctrl Pts',(30.7905752297746,22.8327252216199,43.5185277541105));
#66579=CARTESIAN_POINT('Ctrl Pts',(30.7260365526935,22.8592310542391,43.5229744879862));
#66580=CARTESIAN_POINT('Ctrl Pts',(30.6603784516242,22.8822666822558,43.5274212218619));
#66581=CARTESIAN_POINT('Ctrl Pts',(30.5946066304212,22.9053422080865,43.5318756575012));
#66582=CARTESIAN_POINT('Ctrl Pts',(30.5277119845147,22.9249353943831,43.5363300931405));
#66583=CARTESIAN_POINT('Ctrl Pts',(30.4600972060717,22.9409631947734,43.5407845287798));
#66584=CARTESIAN_POINT('Ctrl Pts',(30.4252017256148,22.9492350224443,43.5430834296322));
#66585=CARTESIAN_POINT('Ctrl Pts',(30.3901145785427,22.9565580456331,43.5453823304846));
#66586=CARTESIAN_POINT('Ctrl Pts',(30.3548916630846,22.9629262517917,43.547681231337));
#66587=CARTESIAN_POINT('Ctrl Pts',(30.2866570000519,22.9752628910422,43.5521347163188));
#66588=CARTESIAN_POINT('Ctrl Pts',(30.2176437364889,22.9840616924254,43.5565882013007));
#66589=CARTESIAN_POINT('Ctrl Pts',(30.1482514638409,22.9892332859594,43.5610416862825));
#66590=CARTESIAN_POINT('Ctrl Pts',(30.0789558713456,22.9943976742178,43.5654889664869));
#66591=CARTESIAN_POINT('Ctrl Pts',(30.0092828009534,22.9959448432096,43.5699362466913));
#66592=CARTESIAN_POINT('Ctrl Pts',(29.939641000981,22.9938365915334,43.5743835268957));
#66593=CARTESIAN_POINT('Ctrl Pts',(29.8700725681683,22.9917305608859,43.5788261219209));
#66594=CARTESIAN_POINT('Ctrl Pts',(29.8005358271373,22.9859767667221,43.583268716946));
#66595=CARTESIAN_POINT('Ctrl Pts',(29.7314418222075,22.9765889981584,43.5877113119711));
#66596=CARTESIAN_POINT('Ctrl Pts',(29.6623891556608,22.9672068462205,43.5921512490277));
#66597=CARTESIAN_POINT('Ctrl Pts',(29.5937791838954,22.954195096957,43.5965911860842));
#66598=CARTESIAN_POINT('Ctrl Pts',(29.5260184772164,22.9376194359471,43.6010311231407));
#66599=CARTESIAN_POINT('Ctrl Pts',(29.4582822691053,22.9210497677901,43.6054694549587));
#66600=CARTESIAN_POINT('Ctrl Pts',(29.3913951906568,22.9009188664662,43.6099077867767));
#66601=CARTESIAN_POINT('Ctrl Pts',(29.325752376959,22.8773432571918,43.6143461185947));
#66602=CARTESIAN_POINT('Ctrl Pts',(29.2600881752145,22.8537599664028,43.6187858965306));
#66603=CARTESIAN_POINT('Ctrl Pts',(29.1956695092175,22.826729890824,43.6232256744665));
#66604=CARTESIAN_POINT('Ctrl Pts',(29.1328738433149,22.7964186012432,43.6276654524023));
#66605=CARTESIAN_POINT('Ctrl Pts',(29.0975504373971,22.7793680935312,43.630162887153));
#66606=CARTESIAN_POINT('Ctrl Pts',(29.0627402181288,22.7612802096027,43.6326603219036));
#66607=CARTESIAN_POINT('Ctrl Pts',(29.0285070491141,22.7421908646526,43.6351577566542));
#66608=CARTESIAN_POINT('Origin',(30.,21.,36.25));
#66609=CARTESIAN_POINT('',(28.0000000001618,21.,36.5000000001618));
#66610=CARTESIAN_POINT('',(27.6389480828464,21.,36.1389480828464));
#66611=CARTESIAN_POINT('',(27.75,21.,36.25));
#66612=CARTESIAN_POINT('',(30.5154785150505,22.9324290162917,36.5000000000579));
#66613=CARTESIAN_POINT('Origin',(30.,21.,36.5));
#66614=CARTESIAN_POINT('Ctrl Pts',(30.5154785148818,22.9324290155263,36.5000000001618));
#66615=CARTESIAN_POINT('Ctrl Pts',(30.6725470225254,22.896963831748,36.493784254721));
#66616=CARTESIAN_POINT('Ctrl Pts',(30.8251103005109,22.8429178203948,36.4872213037502));
#66617=CARTESIAN_POINT('Ctrl Pts',(31.1331843487363,22.6910303567306,36.4725748213189));
#66618=CARTESIAN_POINT('Ctrl Pts',(31.2856502416904,22.5886637756194,36.464438023848));
#66619=CARTESIAN_POINT('Ctrl Pts',(31.6661050171744,22.2496122793256,36.4431572700421));
#66620=CARTESIAN_POINT('Ctrl Pts',(31.8103111325502,22.0141644029362,36.4343345358605));
#66621=CARTESIAN_POINT('Ctrl Pts',(32.00016320241,21.6224137148118,36.4188105171623));
#66622=CARTESIAN_POINT('Ctrl Pts',(32.0670581843828,21.3910802024333,36.4097864347362));
#66623=CARTESIAN_POINT('Ctrl Pts',(32.1218713381998,20.9151685390699,36.3901049253534));
#66624=CARTESIAN_POINT('Ctrl Pts',(32.1136324505546,20.6320256169199,36.3776789419417));
#66625=CARTESIAN_POINT('Ctrl Pts',(31.951644176216,20.0746445603385,36.3565413848938));
#66626=CARTESIAN_POINT('Ctrl Pts',(31.8286906741857,19.8349686552164,36.3481325716929));
#66627=CARTESIAN_POINT('Ctrl Pts',(31.5113517074335,19.4215656049671,36.3295587365625));
#66628=CARTESIAN_POINT('Ctrl Pts',(31.321691587591,19.2472068145484,36.3195469325908));
#66629=CARTESIAN_POINT('Ctrl Pts',(30.94481536976,19.00542470332,36.3014090707333));
#66630=CARTESIAN_POINT('Ctrl Pts',(30.7179098068827,18.8887223990991,36.2911367581791));
#66631=CARTESIAN_POINT('Ctrl Pts',(30.1336842972584,18.7558473108252,36.2709813071793));
#66632=CARTESIAN_POINT('Ctrl Pts',(29.8370876005783,18.7487109423105,36.261878322807));
#66633=CARTESIAN_POINT('Ctrl Pts',(29.250115499477,18.8471938271965,36.2404374312578));
#66634=CARTESIAN_POINT('Ctrl Pts',(28.9634161890183,18.9559319623666,36.2281041314165));
#66635=CARTESIAN_POINT('Ctrl Pts',(28.4570688608167,19.2758936012752,36.2053867063752));
#66636=CARTESIAN_POINT('Ctrl Pts',(28.2858618512514,19.4533624013602,36.1980121961921));
#66637=CARTESIAN_POINT('Ctrl Pts',(27.9798579491602,19.8253250174455,36.1831156023108));
#66638=CARTESIAN_POINT('Ctrl Pts',(27.8339165836195,20.0979204036427,36.1734663861722));
#66639=CARTESIAN_POINT('Ctrl Pts',(27.6821082997652,20.5873295890753,36.1548008720659));
#66640=CARTESIAN_POINT('Ctrl Pts',(27.6467202808314,20.7929343118159,36.1467202808314));
#66641=CARTESIAN_POINT('Ctrl Pts',(27.6389480828464,21.,36.1389480828464));
#66642=CARTESIAN_POINT('Origin',(30.,21.,36.25));
#66643=CARTESIAN_POINT('',(28.9249115396486,23.2020751695661,36.0495));
#66644=CARTESIAN_POINT('Ctrl Pts',(27.6389480828464,21.,36.1389480828464));
#66645=CARTESIAN_POINT('Ctrl Pts',(27.6350634289606,21.1034943437831,36.1350634289606));
#66646=CARTESIAN_POINT('Ctrl Pts',(27.6380797522175,21.2073543905297,36.1312731650575));
#66647=CARTESIAN_POINT('Ctrl Pts',(27.6738431552335,21.573368653005,36.1187710246431));
#66648=CARTESIAN_POINT('Ctrl Pts',(27.7446488307736,21.8299158156141,36.1113213734728));
#66649=CARTESIAN_POINT('Ctrl Pts',(27.9565827158724,22.2893220308902,36.0959653167334));
#66650=CARTESIAN_POINT('Ctrl Pts',(28.090608564173,22.4931862828733,36.0881804309061));
#66651=CARTESIAN_POINT('Ctrl Pts',(28.4431040524274,22.8879945187574,36.0697652258806));
#66652=CARTESIAN_POINT('Ctrl Pts',(28.6710763004339,23.0676251036898,36.0589567700887));
#66653=CARTESIAN_POINT('Ctrl Pts',(28.9249115396486,23.202075169566,36.0495));
#66654=CARTESIAN_POINT('',(31.0750884603512,23.2020751695661,36.0495));
#66655=CARTESIAN_POINT('Origin',(30.,21.,36.0495));
#66656=CARTESIAN_POINT('',(28.2709700121084,22.006441477355,36.4978425793705));
#66657=CARTESIAN_POINT('Ctrl Pts',(31.0750884603512,23.2020751695661,36.0495000000001));
#66658=CARTESIAN_POINT('Ctrl Pts',(30.7766255492167,23.3049251530177,36.0880189295469));
#66659=CARTESIAN_POINT('Ctrl Pts',(30.4645526145668,23.3541452362613,36.1209468496696));
#66660=CARTESIAN_POINT('Ctrl Pts',(29.8990342120443,23.3201776314801,36.1910429955509));
#66661=CARTESIAN_POINT('Ctrl Pts',(29.6557904663614,23.2623988165233,36.2250071891161));
#66662=CARTESIAN_POINT('Ctrl Pts',(29.3141204560412,23.1149875707035,36.2798402082991));
#66663=CARTESIAN_POINT('Ctrl Pts',(29.2069006842352,23.0575773165827,36.2981495320029));
#66664=CARTESIAN_POINT('Ctrl Pts',(28.9421107872916,22.8873688916963,36.3448128907834));
#66665=CARTESIAN_POINT('Ctrl Pts',(28.770120719906,22.7481449934132,36.3747716297848));
#66666=CARTESIAN_POINT('Ctrl Pts',(28.5396314493269,22.4860562450386,36.4198294545293));
#66667=CARTESIAN_POINT('Ctrl Pts',(28.4689142907509,22.3904700508477,36.435114483917));
#66668=CARTESIAN_POINT('Ctrl Pts',(28.353116026781,22.1991945540512,36.4654153193861));
#66669=CARTESIAN_POINT('Ctrl Pts',(28.3064636933393,22.1056760884109,36.4801215118855));
#66670=CARTESIAN_POINT('Ctrl Pts',(28.2679218920155,22.0085551104088,36.495685158741));
#66671=CARTESIAN_POINT('Origin',(30.,21.,36.5));
#66672=CARTESIAN_POINT('Origin',(30.,21.,40.25));
#66673=CARTESIAN_POINT('',(27.5481783129142,21.0004035148025,36.3073275271523));
#66674=CARTESIAN_POINT('Ctrl Pts',(27.5451094726466,21.0004046124501,36.3073274962121));
#66675=CARTESIAN_POINT('Ctrl Pts',(27.5450545228292,21.0257377592651,36.3060055102952));
#66676=CARTESIAN_POINT('Ctrl Pts',(27.5572991467173,21.8618031372997,36.2623732679693));
#66677=CARTESIAN_POINT('Ctrl Pts',(28.5079104395216,23.4802670136419,36.1764307692296));
#66678=CARTESIAN_POINT('Ctrl Pts',(30.3433301243472,23.5593313403256,36.0918102564103));
#66679=CARTESIAN_POINT('Ctrl Pts',(31.0750884603513,23.2020751695661,36.0495));
#66680=CARTESIAN_POINT('',(27.549294249036,21.0022449162321,36.1916725037879));
#66681=CARTESIAN_POINT('Ctrl Pts',(28.9249115396486,23.2020751695661,36.0495));
#66682=CARTESIAN_POINT('Ctrl Pts',(28.192355923267,22.8444297537228,36.0918563551502));
#66683=CARTESIAN_POINT('Ctrl Pts',(27.5953569563779,22.006174763075,36.1392471897461));
#66684=CARTESIAN_POINT('Ctrl Pts',(27.5465802851334,21.0987581685929,36.1866380243421));
#66685=CARTESIAN_POINT('Ctrl Pts',(27.5473247562997,21.0022467203435,36.1916725037879));
#66686=CARTESIAN_POINT('',(27.5495002532104,21.0011139947484,36.9916725037394));
#66687=CARTESIAN_POINT('Ctrl Pts',(27.5495010281166,21.0022447268166,36.1916725037879));
#66688=CARTESIAN_POINT('Ctrl Pts',(27.549428428816,20.9229903114318,36.195810481644));
#66689=CARTESIAN_POINT('Ctrl Pts',(27.553204866294,20.8435626405268,36.1999484595));
#66690=CARTESIAN_POINT('Ctrl Pts',(27.5608542041623,20.7643773426696,36.2040864373561));
#66691=CARTESIAN_POINT('Ctrl Pts',(27.5685220450517,20.6850005031061,36.2082344245871));
#66692=CARTESIAN_POINT('Ctrl Pts',(27.5800816086064,20.6058676998867,36.2123824118181));
#66693=CARTESIAN_POINT('Ctrl Pts',(27.5955043182853,20.5273999930013,36.2165303990492));
#66694=CARTESIAN_POINT('Ctrl Pts',(27.6108544724337,20.4493014343532,36.2206588722376));
#66695=CARTESIAN_POINT('Ctrl Pts',(27.6300314369191,20.3718622124444,36.2247873454261));
#66696=CARTESIAN_POINT('Ctrl Pts',(27.6529551516149,20.295492562375,36.2289158186145));
#66697=CARTESIAN_POINT('Ctrl Pts',(27.6758677400832,20.2191599789903,36.233042288012));
#66698=CARTESIAN_POINT('Ctrl Pts',(27.7025233332778,20.1438964028512,36.2371687574095));
#66699=CARTESIAN_POINT('Ctrl Pts',(27.7327913448585,20.0700993794758,36.241295226807));
#66700=CARTESIAN_POINT('Ctrl Pts',(27.7630547940436,19.9963134797649,36.2454210742084));
#66701=CARTESIAN_POINT('Ctrl Pts',(27.796929395648,19.9239941434461,36.2495469216097));
#66702=CARTESIAN_POINT('Ctrl Pts',(27.8342361287632,19.8535196887669,36.2536727690111));
#66703=CARTESIAN_POINT('Ctrl Pts',(27.8718858574065,19.7823972968176,36.2578365491686));
#66704=CARTESIAN_POINT('Ctrl Pts',(27.9130309380522,19.7131543408591,36.2620003293261));
#66705=CARTESIAN_POINT('Ctrl Pts',(27.9574405506607,19.6461532044154,36.2661641094836));
#66706=CARTESIAN_POINT('Ctrl Pts',(28.0015021788096,19.5796770748988,36.2702952631284));
#66707=CARTESIAN_POINT('Ctrl Pts',(28.0487770158858,19.5154081132134,36.2744264167733));
#66708=CARTESIAN_POINT('Ctrl Pts',(28.0989980217184,19.4536682993066,36.2785575704181));
#66709=CARTESIAN_POINT('Ctrl Pts',(28.1498139713933,19.3911970838377,36.282737663832));
#66710=CARTESIAN_POINT('Ctrl Pts',(28.203646008288,19.3313157126013,36.2869177572458));
#66711=CARTESIAN_POINT('Ctrl Pts',(28.2601795210837,19.2743189891688,36.2910978506596));
#66712=CARTESIAN_POINT('Ctrl Pts',(28.3167130338795,19.2173222657362,36.2952779440734));
#66713=CARTESIAN_POINT('Ctrl Pts',(28.3759475971239,19.1632104753326,36.2994580374872));
#66714=CARTESIAN_POINT('Ctrl Pts',(28.4375364339365,19.1122346928911,36.303638130901));
#66715=CARTESIAN_POINT('Ctrl Pts',(28.499918561709,19.0606023202381,36.307872065733));
#66716=CARTESIAN_POINT('Ctrl Pts',(28.5649795566333,19.0119687699261,36.312106000565));
#66717=CARTESIAN_POINT('Ctrl Pts',(28.632399355623,18.9666238106293,36.316339935397));
#66718=CARTESIAN_POINT('Ctrl Pts',(28.6997218908088,18.9213442686624,36.3205677621032));
#66719=CARTESIAN_POINT('Ctrl Pts',(28.7693960893656,18.8793441517372,36.3247955888095));
#66720=CARTESIAN_POINT('Ctrl Pts',(28.8410686199956,18.840873253734,36.3290234155158));
#66721=CARTESIAN_POINT('Ctrl Pts',(28.9128936812984,18.8023204834724,36.3332602397173));
#66722=CARTESIAN_POINT('Ctrl Pts',(28.9867252206828,18.7673122618253,36.3374970639188));
#66723=CARTESIAN_POINT('Ctrl Pts',(29.0621781153025,18.7360564577308,36.3417338881202));
#66724=CARTESIAN_POINT('Ctrl Pts',(29.1373332467312,18.7049239998381,36.3459539923496));
#66725=CARTESIAN_POINT('Ctrl Pts',(29.2140965340676,18.6775145881152,36.350174096579));
#66726=CARTESIAN_POINT('Ctrl Pts',(29.29206414284,18.653986983807,36.3543942008084));
#66727=CARTESIAN_POINT('Ctrl Pts',(29.3700050755609,18.6304674292978,36.3586128611597));
#66728=CARTESIAN_POINT('Ctrl Pts',(29.4491490673368,18.6108271786092,36.362831521511));
#66729=CARTESIAN_POINT('Ctrl Pts',(29.5290758863624,18.5951755304816,36.3670501818624));
#66730=CARTESIAN_POINT('Ctrl Pts',(29.6089997573466,18.5795244596534,36.3712686866116));
#66731=CARTESIAN_POINT('Ctrl Pts',(29.6897059423986,18.5678617870917,36.3754871913607));
#66732=CARTESIAN_POINT('Ctrl Pts',(29.7707641540447,18.5602456728332,36.3797056961099));
#66733=CARTESIAN_POINT('Ctrl Pts',(29.8524299465205,18.5525724711443,36.38395582113));
#66734=CARTESIAN_POINT('Ctrl Pts',(29.934452591178,18.5490068081063,36.3882059461502));
#66735=CARTESIAN_POINT('Ctrl Pts',(30.016388781063,18.5495548041519,36.3924560711703));
#66736=CARTESIAN_POINT('Ctrl Pts',(30.0978305074078,18.5500994931842,36.3966805477942));
#66737=CARTESIAN_POINT('Ctrl Pts',(30.1791863549369,18.5547082439169,36.4009050244181));
#66738=CARTESIAN_POINT('Ctrl Pts',(30.2600248042397,18.56333478886,36.405129501042));
#66739=CARTESIAN_POINT('Ctrl Pts',(30.3415994547678,18.5720398963312,36.4093924502602));
#66740=CARTESIAN_POINT('Ctrl Pts',(30.4226467581714,18.5848362767889,36.4136553994785));
#66741=CARTESIAN_POINT('Ctrl Pts',(30.5027343439812,18.6016237931922,36.4179183486967));
#66742=CARTESIAN_POINT('Ctrl Pts',(30.582821929791,18.6184113095955,36.422181297915));
#66743=CARTESIAN_POINT('Ctrl Pts',(30.6619493505619,18.639189779902,36.4264442471332));
#66744=CARTESIAN_POINT('Ctrl Pts',(30.7397022172849,18.663808466811,36.4307071963514));
#66745=CARTESIAN_POINT('Ctrl Pts',(30.8169981552416,18.6882824775595,36.4349450935786));
#66746=CARTESIAN_POINT('Ctrl Pts',(30.893217937062,18.7166410105943,36.4391829908057));
#66747=CARTESIAN_POINT('Ctrl Pts',(30.9679441397284,18.7487704709725,36.4434208880328));
#66748=CARTESIAN_POINT('Ctrl Pts',(31.0425656986694,18.7808549384793,36.4476528506702));
#66749=CARTESIAN_POINT('Ctrl Pts',(31.1156974107722,18.8166996628448,36.4518848133076));
#66750=CARTESIAN_POINT('Ctrl Pts',(31.1869376197398,18.8561414839485,36.4561167759451));
#66751=CARTESIAN_POINT('Ctrl Pts',(31.2582426267828,18.8956191802151,36.4603525878558));
#66752=CARTESIAN_POINT('Ctrl Pts',(31.3276522509388,18.9387003571713,36.4645883997665));
#66753=CARTESIAN_POINT('Ctrl Pts',(31.3947844469337,18.9851733085469,36.4688242116772));
#66754=CARTESIAN_POINT('Ctrl Pts',(31.4617394788274,19.031523616256,36.4730488451392));
#66755=CARTESIAN_POINT('Ctrl Pts',(31.5264286954501,19.0812475704348,36.4772734786011));
#66756=CARTESIAN_POINT('Ctrl Pts',(31.5884998541784,19.1340904461161,36.4814981120631));
#66757=CARTESIAN_POINT('Ctrl Pts',(31.6505518312119,19.1869169918959,36.4857214399972));
#66758=CARTESIAN_POINT('Ctrl Pts',(31.7099870047576,19.2428602448719,36.4899447679313));
#66759=CARTESIAN_POINT('Ctrl Pts',(31.7664859421674,19.3016249924928,36.4941680958654));
#66760=CARTESIAN_POINT('Ctrl Pts',(31.8229845685898,19.3603894166546,36.498391400553));
#66761=CARTESIAN_POINT('Ctrl Pts',(31.8765466708863,19.4219749698148,36.5026147052406));
#66762=CARTESIAN_POINT('Ctrl Pts',(31.9268904472431,19.4860503791991,36.5068380099283));
#66763=CARTESIAN_POINT('Ctrl Pts',(31.9774911053774,19.5504527367435,36.5110828642511));
#66764=CARTESIAN_POINT('Ctrl Pts',(32.0248402008895,19.6173700673117,36.5153277185739));
#66765=CARTESIAN_POINT('Ctrl Pts',(32.0686944067583,19.6864347365103,36.5195725728967));
#66766=CARTESIAN_POINT('Ctrl Pts',(32.112390543616,19.7552504675797,36.5238021269783));
#66767=CARTESIAN_POINT('Ctrl Pts',(32.1526167538075,19.8261976542578,36.52803168106));
#66768=CARTESIAN_POINT('Ctrl Pts',(32.1891783485836,19.8988876496502,36.5322612351417));
#66769=CARTESIAN_POINT('Ctrl Pts',(32.2259383334994,19.9719720747285,36.5365137395851));
#66770=CARTESIAN_POINT('Ctrl Pts',(32.258993628189,20.0468178436806,36.5407662440284));
#66771=CARTESIAN_POINT('Ctrl Pts',(32.2881959469411,20.1230110842193,36.5450187484718));
#66772=CARTESIAN_POINT('Ctrl Pts',(32.3173982656932,20.199204324758,36.5492712529152));
#66773=CARTESIAN_POINT('Ctrl Pts',(32.3427475219628,20.2767445716513,36.5535237573586));
#66774=CARTESIAN_POINT('Ctrl Pts',(32.3641469546119,20.3552059034085,36.557776261802));
#66775=CARTESIAN_POINT('Ctrl Pts',(32.3854168641285,20.4331923367125,36.5620030273529));
#66776=CARTESIAN_POINT('Ctrl Pts',(32.4028644942027,20.5123815769929,36.5662297929038));
#66777=CARTESIAN_POINT('Ctrl Pts',(32.4163574191108,20.5923640434059,36.5704565584547));
#66778=CARTESIAN_POINT('Ctrl Pts',(32.4298307746883,20.6722305080378,36.5746771937579));
#66779=CARTESIAN_POINT('Ctrl Pts',(32.4393607388843,20.7528874585296,36.578897829061));
#66780=CARTESIAN_POINT('Ctrl Pts',(32.4448649901705,20.8339113795637,36.5831184643642));
#66781=CARTESIAN_POINT('Ctrl Pts',(32.4503926948848,20.9152805407766,36.5873570836512));
#66782=CARTESIAN_POINT('Ctrl Pts',(32.4518601720758,20.9970193484073,36.5915957029382));
#66783=CARTESIAN_POINT('Ctrl Pts',(32.4492362431956,21.0786897389583,36.5958343222252));
#66784=CARTESIAN_POINT('Ctrl Pts',(32.4466282274135,21.1598648306634,36.6000472359508));
#66785=CARTESIAN_POINT('Ctrl Pts',(32.4399783047359,21.2409718618635,36.6042601496764));
#66786=CARTESIAN_POINT('Ctrl Pts',(32.4293080078248,21.3215786888434,36.608473063402));
#66787=CARTESIAN_POINT('Ctrl Pts',(32.4186413254627,21.4021582103671,36.6126845500086));
#66788=CARTESIAN_POINT('Ctrl Pts',(32.4039570342971,21.4822374024858,36.6168960366152));
#66789=CARTESIAN_POINT('Ctrl Pts',(32.3853284935868,21.5613895507426,36.6211075232219));
#66790=CARTESIAN_POINT('Ctrl Pts',(32.3667005227754,21.6405392775149,36.6253188809874));
#66791=CARTESIAN_POINT('Ctrl Pts',(32.3441286501096,21.7187615633856,36.6295302387529));
#66792=CARTESIAN_POINT('Ctrl Pts',(32.3177369713169,21.7956416164272,36.6337415965184));
#66793=CARTESIAN_POINT('Ctrl Pts',(32.2910489583739,21.8733849031178,36.6380002407463));
#66794=CARTESIAN_POINT('Ctrl Pts',(32.2604549617917,21.9497551595125,36.6422588849741));
#66795=CARTESIAN_POINT('Ctrl Pts',(32.2261338987918,22.0243427720495,36.6465175292019));
#66796=CARTESIAN_POINT('Ctrl Pts',(32.1921446677931,22.0982092368547,36.6507349988765));
#66797=CARTESIAN_POINT('Ctrl Pts',(32.1545004036852,22.1703269912888,36.6549524685511));
#66798=CARTESIAN_POINT('Ctrl Pts',(32.1134209899573,22.2403233325258,36.6591699382257));
#66799=CARTESIAN_POINT('Ctrl Pts',(32.0717399975677,22.3113447201659,36.6634491697301));
#66800=CARTESIAN_POINT('Ctrl Pts',(32.0265227061001,22.3801816435532,36.6677284012346));
#66801=CARTESIAN_POINT('Ctrl Pts',(31.9780429219995,22.4464772548255,36.6720076327391));
#66802=CARTESIAN_POINT('Ctrl Pts',(31.9295631378989,22.5127728660979,36.6762868642435));
#66803=CARTESIAN_POINT('Ctrl Pts',(31.8778212239518,22.5765268236252,36.680566095748));
#66804=CARTESIAN_POINT('Ctrl Pts',(31.8231303902993,22.6374204805019,36.6848453272525));
#66805=CARTESIAN_POINT('Ctrl Pts',(31.7690469632885,22.6976378410205,36.6890770328104));
#66806=CARTESIAN_POINT('Ctrl Pts',(31.71187556473,22.755285608444,36.6933087383683));
#66807=CARTESIAN_POINT('Ctrl Pts',(31.6518899209919,22.8100303696141,36.6975404439262));
#66808=CARTESIAN_POINT('Ctrl Pts',(31.5919903334818,22.8646965931983,36.7017660786212));
#66809=CARTESIAN_POINT('Ctrl Pts',(31.529284859754,22.9164677712883,36.7059917133163));
#66810=CARTESIAN_POINT('Ctrl Pts',(31.4640860108728,22.9650451401346,36.7102173480113));
#66811=CARTESIAN_POINT('Ctrl Pts',(31.3987059878403,23.013757495468,36.7144547248734));
#66812=CARTESIAN_POINT('Ctrl Pts',(31.3308190323845,23.0592579186859,36.7186921017356));
#66813=CARTESIAN_POINT('Ctrl Pts',(31.2607759414872,23.1012839587659,36.7229294785978));
#66814=CARTESIAN_POINT('Ctrl Pts',(31.1910527978004,23.1431180296722,36.7271474997049));
#66815=CARTESIAN_POINT('Ctrl Pts',(31.1191935713334,23.1815091424984,36.7313655208121));
#66816=CARTESIAN_POINT('Ctrl Pts',(31.0455741187681,23.2162411899796,36.7355835419192));
#66817=CARTESIAN_POINT('Ctrl Pts',(30.9719790620954,23.2509617280123,36.7398001652655));
#66818=CARTESIAN_POINT('Ctrl Pts',(30.8966253577217,23.2820254104759,36.7440167886118));
#66819=CARTESIAN_POINT('Ctrl Pts',(30.8199123304505,23.3092626572946,36.7482334119581));
#66820=CARTESIAN_POINT('Ctrl Pts',(30.7432012379335,23.3364992171715,36.7524499289583));
#66821=CARTESIAN_POINT('Ctrl Pts',(30.6651313290609,23.3599093787962,36.7566664459585));
#66822=CARTESIAN_POINT('Ctrl Pts',(30.586119361691,23.3793726786384,36.7608829629587));
#66823=CARTESIAN_POINT('Ctrl Pts',(30.5064308877364,23.3990026247615,36.765135582104));
#66824=CARTESIAN_POINT('Ctrl Pts',(30.4257846079184,23.4146176654465,36.7693882012494));
#66825=CARTESIAN_POINT('Ctrl Pts',(30.3446191376693,23.4261467185544,36.7736408203948));
#66826=CARTESIAN_POINT('Ctrl Pts',(30.2640260045932,23.4375944747063,36.777863452256));
#66827=CARTESIAN_POINT('Ctrl Pts',(30.1829214530076,23.4450137026212,36.7820860841172));
#66828=CARTESIAN_POINT('Ctrl Pts',(30.1017387329028,23.4483871181305,36.7863087159784));
#66829=CARTESIAN_POINT('Ctrl Pts',(30.0196912265546,23.4517964684215,36.7905763287658));
#66830=CARTESIAN_POINT('Ctrl Pts',(29.9375643634526,23.451073303568,36.7948439415532));
#66831=CARTESIAN_POINT('Ctrl Pts',(29.8558020879835,23.4462537096896,36.7991115543407));
#66832=CARTESIAN_POINT('Ctrl Pts',(29.7740398125144,23.4414341158111,36.8033791671281));
#66833=CARTESIAN_POINT('Ctrl Pts',(29.6926425978752,23.4325182093514,36.8076467799155));
#66834=CARTESIAN_POINT('Ctrl Pts',(29.6120438764149,23.4195950686371,36.811914392703));
#66835=CARTESIAN_POINT('Ctrl Pts',(29.5321215868013,23.4067803865159,36.8161461891754));
#66836=CARTESIAN_POINT('Ctrl Pts',(29.4526855303043,23.3899775974669,36.8203779856478));
#66837=CARTESIAN_POINT('Ctrl Pts',(29.3741642773118,23.3692361423478,36.8246097821202));
#66838=CARTESIAN_POINT('Ctrl Pts',(29.2957553799135,23.3485243660537,36.8288355233401));
#66839=CARTESIAN_POINT('Ctrl Pts',(29.218259131837,23.3238852346488,36.8330612645601));
#66840=CARTESIAN_POINT('Ctrl Pts',(29.1420959899604,23.2954195606812,36.8372870057801));
#66841=CARTESIAN_POINT('Ctrl Pts',(29.0657235765456,23.2668756723014,36.8415243579623));
#66842=CARTESIAN_POINT('Ctrl Pts',(28.9906920707856,23.2344842641582,36.8457617101445));
#66843=CARTESIAN_POINT('Ctrl Pts',(28.9174121060829,23.1983979853394,36.8499990623268));
#66844=CARTESIAN_POINT('Ctrl Pts',(28.8444639585092,23.1624751078742,36.8542172274632));
#66845=CARTESIAN_POINT('Ctrl Pts',(28.7732519469577,23.1228909491638,36.8584353925997));
#66846=CARTESIAN_POINT('Ctrl Pts',(28.7041613718838,23.079844345109,36.8626535577362));
#66847=CARTESIAN_POINT('Ctrl Pts',(28.6350934641233,23.0368118638324,36.8668703389723));
#66848=CARTESIAN_POINT('Ctrl Pts',(28.5681460048312,22.9903194386782,36.8710871202084));
#66849=CARTESIAN_POINT('Ctrl Pts',(28.5036779004829,22.9406108379829,36.8753039014445));
#66850=CARTESIAN_POINT('Ctrl Pts',(28.439211212496,22.8909033293833,36.8795205900381));
#66851=CARTESIAN_POINT('Ctrl Pts',(28.3772241385323,22.8379800704191,36.8837372786318));
#66852=CARTESIAN_POINT('Ctrl Pts',(28.3180437454976,22.7821260920429,36.8879539672254));
#66853=CARTESIAN_POINT('Ctrl Pts',(28.2583613418289,22.725798320073,36.8922064248027));
#66854=CARTESIAN_POINT('Ctrl Pts',(28.2015338236149,22.6664901878068,36.8964588823801));
#66855=CARTESIAN_POINT('Ctrl Pts',(28.1478585223756,22.6045317687298,36.9007113399574));
#66856=CARTESIAN_POINT('Ctrl Pts',(28.0945571147198,22.5430049421135,36.9049341755938));
#66857=CARTESIAN_POINT('Ctrl Pts',(28.044364387583,22.4788650428754,36.9091570112302));
#66858=CARTESIAN_POINT('Ctrl Pts',(27.9975296225177,22.4124668623744,36.9133798468667));
#66859=CARTESIAN_POINT('Ctrl Pts',(27.95020205945,22.3453700365259,36.9176471154145));
#66860=CARTESIAN_POINT('Ctrl Pts',(27.9063037987182,22.2759675382794,36.9219143839623));
#66861=CARTESIAN_POINT('Ctrl Pts',(27.8660449782421,22.2046519062013,36.9261816525101));
#66862=CARTESIAN_POINT('Ctrl Pts',(27.8257861577661,22.1333362741232,36.9304489210579));
#66863=CARTESIAN_POINT('Ctrl Pts',(27.7891669358602,22.0601079687253,36.9347161896056));
#66864=CARTESIAN_POINT('Ctrl Pts',(27.7563472401053,21.9853793903959,36.9389834581534));
#66865=CARTESIAN_POINT('Ctrl Pts',(27.7205636960295,21.9039022982149,36.9436360909293));
#66866=CARTESIAN_POINT('Ctrl Pts',(27.6891806545381,21.8203795186194,36.9482887237052));
#66867=CARTESIAN_POINT('Ctrl Pts',(27.6624130257218,21.7352804823228,36.9529413564811));
#66868=CARTESIAN_POINT('Ctrl Pts',(27.6357210655907,21.6504220101879,36.9575808368553));
#66869=CARTESIAN_POINT('Ctrl Pts',(27.6136186222774,21.5639964464178,36.9622203172296));
#66870=CARTESIAN_POINT('Ctrl Pts',(27.5962726571912,21.4764925093148,36.9668597976038));
#66871=CARTESIAN_POINT('Ctrl Pts',(27.5790101229767,21.3894094499039,36.9714769629388));
#66872=CARTESIAN_POINT('Ctrl Pts',(27.5664585478923,21.3012586502107,36.9760941282738));
#66873=CARTESIAN_POINT('Ctrl Pts',(27.5587346158157,21.2125407584051,36.9807112936088));
#66874=CARTESIAN_POINT('Ctrl Pts',(27.5526223776505,21.1423349514595,36.984365030319));
#66875=CARTESIAN_POINT('Ctrl Pts',(27.5495323753805,21.0717744441211,36.9880187670292));
#66876=CARTESIAN_POINT('Ctrl Pts',(27.5495002532104,21.0011139947484,36.9916725037394));
#66877=CARTESIAN_POINT('',(27.5495009409694,20.9978525154208,37.7916725038249));
#66878=CARTESIAN_POINT('Ctrl Pts',(27.54950025321,21.0011139938109,36.9916725037879));
#66879=CARTESIAN_POINT('Ctrl Pts',(27.5494625484464,20.9181732154581,36.9959612363013));
#66880=CARTESIAN_POINT('Ctrl Pts',(27.5536400688284,20.8352469267231,37.0002499688148));
#66881=CARTESIAN_POINT('Ctrl Pts',(27.5620020596278,20.7527829036236,37.0045387013282));
#66882=CARTESIAN_POINT('Ctrl Pts',(27.5703679671343,20.6702802548621,37.0088294426586));
#66883=CARTESIAN_POINT('Ctrl Pts',(27.582922197871,20.5882407421637,37.0131201839891));
#66884=CARTESIAN_POINT('Ctrl Pts',(27.5995823369894,20.5071051906271,37.0174109253195));
#66885=CARTESIAN_POINT('Ctrl Pts',(27.616268339477,20.4258436834359,37.0217083276404));
#66886=CARTESIAN_POINT('Ctrl Pts',(27.6370728896858,20.3454893738916,37.0260057299613));
#66887=CARTESIAN_POINT('Ctrl Pts',(27.6618628128603,20.2664710338954,37.0303031322822));
#66888=CARTESIAN_POINT('Ctrl Pts',(27.6866728284728,20.1873886488805,37.0346040176832));
#66889=CARTESIAN_POINT('Ctrl Pts',(27.7154744977915,20.10964480498,37.0389049030842));
#66890=CARTESIAN_POINT('Ctrl Pts',(27.7480861756485,20.0336489366206,37.0432057884853));
#66891=CARTESIAN_POINT('Ctrl Pts',(27.7807657956125,19.9574947409454,37.0475156342108));
#66892=CARTESIAN_POINT('Ctrl Pts',(27.8172710887893,19.8830961945644,37.0518254799363));
#66893=CARTESIAN_POINT('Ctrl Pts',(27.8573740094553,19.8108389029898,37.0561353256619));
#66894=CARTESIAN_POINT('Ctrl Pts',(27.8881337030832,19.7554162027401,37.0594410583092));
#66895=CARTESIAN_POINT('Ctrl Pts',(27.9210089886355,19.7012527444393,37.0627467909566));
#66896=CARTESIAN_POINT('Ctrl Pts',(27.9558803703251,19.648510011292,37.066052523604));
#66897=CARTESIAN_POINT('Ctrl Pts',(28.0005141389927,19.5810017326942,37.070283709726));
#66898=CARTESIAN_POINT('Ctrl Pts',(28.0485794793119,19.515580281312,37.074514895848));
#66899=CARTESIAN_POINT('Ctrl Pts',(28.0998547638172,19.4526156484532,37.0787460819699));
#66900=CARTESIAN_POINT('Ctrl Pts',(28.1510564908356,19.3897413421562,37.0829711982004));
#66901=CARTESIAN_POINT('Ctrl Pts',(28.2054587253515,19.3293172120294,37.0871963144308));
#66902=CARTESIAN_POINT('Ctrl Pts',(28.262796377712,19.2716846859703,37.0914214306612));
#66903=CARTESIAN_POINT('Ctrl Pts',(28.3203021756688,19.2138831495828,37.0956589372609));
#66904=CARTESIAN_POINT('Ctrl Pts',(28.3807603696501,19.1588900069677,37.0998964438606));
#66905=CARTESIAN_POINT('Ctrl Pts',(28.4438625134499,19.1070165418172,37.1041339504603));
#66906=CARTESIAN_POINT('Ctrl Pts',(28.5066668664837,19.0553878772074,37.1083514594774));
#66907=CARTESIAN_POINT('Ctrl Pts',(28.5720899129141,19.0068498136686,37.1125689684945));
#66908=CARTESIAN_POINT('Ctrl Pts',(28.6397917395243,18.9616713370671,37.1167864775115));
#66909=CARTESIAN_POINT('Ctrl Pts',(28.7074711859686,18.9165077950967,37.1210025923483));
#66910=CARTESIAN_POINT('Ctrl Pts',(28.7774275302302,18.8747018924866,37.1252187071851));
#66911=CARTESIAN_POINT('Ctrl Pts',(28.8492908033865,18.8364800451974,37.1294348220219));
#66912=CARTESIAN_POINT('Ctrl Pts',(28.9211523372027,18.7982591230092,37.1336508348141));
#66913=CARTESIAN_POINT('Ctrl Pts',(28.9949202971459,18.7636223010184,37.1378668476063));
#66914=CARTESIAN_POINT('Ctrl Pts',(29.0702002488022,18.7327499757035,37.1420828603985));
#66915=CARTESIAN_POINT('Ctrl Pts',(29.146144693929,18.7016051414651,37.1463360877865));
#66916=CARTESIAN_POINT('Ctrl Pts',(29.2236275173701,18.6742917902894,37.1505893151745));
#66917=CARTESIAN_POINT('Ctrl Pts',(29.302225073654,18.6509447852035,37.1548425425625));
#66918=CARTESIAN_POINT('Ctrl Pts',(29.3802482153376,18.6277684070585,37.1590646860845));
#66919=CARTESIAN_POINT('Ctrl Pts',(29.4593693789546,18.6085006425033,37.1632868296064));
#66920=CARTESIAN_POINT('Ctrl Pts',(29.5391626477447,18.5932222402627,37.1675089731284));
#66921=CARTESIAN_POINT('Ctrl Pts',(29.6198370862289,18.5777751162084,37.1717777424494));
#66922=CARTESIAN_POINT('Ctrl Pts',(29.7011980821515,18.566406074593,37.1760465117704));
#66923=CARTESIAN_POINT('Ctrl Pts',(29.7828007895734,18.5591446677466,37.1803152810914));
#66924=CARTESIAN_POINT('Ctrl Pts',(29.8644034969953,18.5518832609002,37.1845840504124));
#66925=CARTESIAN_POINT('Ctrl Pts',(29.9462474296876,18.5487294429638,37.1888528197334));
#66926=CARTESIAN_POINT('Ctrl Pts',(30.0278903659876,18.5496587222419,37.1931215890545));
#66927=CARTESIAN_POINT('Ctrl Pts',(30.1088136713796,18.5505798105102,37.1973527318706));
#66928=CARTESIAN_POINT('Ctrl Pts',(30.1898430919246,18.5555157117039,37.2015838746867));
#66929=CARTESIAN_POINT('Ctrl Pts',(30.2705475791037,18.5644807006634,37.2058150175028));
#66930=CARTESIAN_POINT('Ctrl Pts',(30.3511363101597,18.5734328309529,37.2100400915028));
#66931=CARTESIAN_POINT('Ctrl Pts',(30.4314005752773,18.5864025205923,37.2142651655029));
#66932=CARTESIAN_POINT('Ctrl Pts',(30.5109097747488,18.6033520383531,37.2184902395029));
#66933=CARTESIAN_POINT('Ctrl Pts',(30.5906531372581,18.6203514742441,37.2227277567947));
#66934=CARTESIAN_POINT('Ctrl Pts',(30.6696365071895,18.6413542062004,37.2269652740864));
#66935=CARTESIAN_POINT('Ctrl Pts',(30.7474311038938,18.6662697253255,37.2312027913782));
#66936=CARTESIAN_POINT('Ctrl Pts',(30.8248576571974,18.6910673700381,37.2354202611301));
#66937=CARTESIAN_POINT('Ctrl Pts',(30.9011062121426,18.7197407256736,37.2396377308821));
#66938=CARTESIAN_POINT('Ctrl Pts',(30.9757664962261,18.752149917178,37.243855200634));
#66939=CARTESIAN_POINT('Ctrl Pts',(31.0504021211007,18.7845484043966,37.2480712774169));
#66940=CARTESIAN_POINT('Ctrl Pts',(31.1234500906999,18.8206800921638,37.2522873541997));
#66941=CARTESIAN_POINT('Ctrl Pts',(31.1945196187994,18.8603567749965,37.2565034309826));
#66942=CARTESIAN_POINT('Ctrl Pts',(31.2655874481501,18.9000325094521,37.2607194069901));
#66943=CARTESIAN_POINT('Ctrl Pts',(31.3346765246005,18.943252842894,37.2649353829977));
#66944=CARTESIAN_POINT('Ctrl Pts',(31.4014214770758,18.9897840679194,37.2691513590052));
#66945=CARTESIAN_POINT('Ctrl Pts',(31.4687569202096,19.0367269533429,37.2734046336302));
#66946=CARTESIAN_POINT('Ctrl Pts',(31.5337061518539,19.0870393434789,37.2776579082552));
#66947=CARTESIAN_POINT('Ctrl Pts',(31.5959262161907,19.1404382875324,37.2819111828801));
#66948=CARTESIAN_POINT('Ctrl Pts',(31.6576903850589,19.1934459697497,37.2861332931428));
#66949=CARTESIAN_POINT('Ctrl Pts',(31.7167649504446,19.2494947557925,37.2903554034055));
#66950=CARTESIAN_POINT('Ctrl Pts',(31.772851223516,19.3082704739593,37.2945775136681));
#66951=CARTESIAN_POINT('Ctrl Pts',(31.8295584750173,19.3676969476709,37.2988463704743));
#66952=CARTESIAN_POINT('Ctrl Pts',(31.8832105353156,19.4299107406748,37.3031152272804));
#66953=CARTESIAN_POINT('Ctrl Pts',(31.9335414607419,19.4945539964541,37.3073840840866));
#66954=CARTESIAN_POINT('Ctrl Pts',(31.9838723861681,19.5591972522335,37.3116529408927));
#66955=CARTESIAN_POINT('Ctrl Pts',(32.030881951721,19.6262695372291,37.3159217976988));
#66956=CARTESIAN_POINT('Ctrl Pts',(32.0743510604301,19.695385908365,37.320190654505));
#66957=CARTESIAN_POINT('Ctrl Pts',(32.1174346839632,19.763889353741,37.324421654979));
#66958=CARTESIAN_POINT('Ctrl Pts',(32.1572021458296,19.8346578788659,37.328652655453));
#66959=CARTESIAN_POINT('Ctrl Pts',(32.1934078163849,19.9073370139783,37.332883655927));
#66960=CARTESIAN_POINT('Ctrl Pts',(32.229561531102,19.979911853125,37.3371085848334));
#66961=CARTESIAN_POINT('Ctrl Pts',(32.2621634001933,20.0543914442578,37.3413335137398));
#66962=CARTESIAN_POINT('Ctrl Pts',(32.2910117400239,20.1303935044674,37.3455584426463));
#66963=CARTESIAN_POINT('Ctrl Pts',(32.3199462802455,20.2066226629204,37.3497959958675));
#66964=CARTESIAN_POINT('Ctrl Pts',(32.3451045767018,20.2843830005105,37.3540335490887));
#66965=CARTESIAN_POINT('Ctrl Pts',(32.3663302640897,20.3632651012758,37.3582711023099));
#66966=CARTESIAN_POINT('Ctrl Pts',(32.3874545993782,20.4417705420834,37.3624884213259));
#66967=CARTESIAN_POINT('Ctrl Pts',(32.4046836691473,20.5213866067705,37.3667057403418));
#66968=CARTESIAN_POINT('Ctrl Pts',(32.4179126465887,20.6016927273245,37.3709230593578));
#66969=CARTESIAN_POINT('Ctrl Pts',(32.4311372489152,20.681972288871,37.3751389836133));
#66970=CARTESIAN_POINT('Ctrl Pts',(32.4403643105116,20.7629409946457,37.3793549078687));
#66971=CARTESIAN_POINT('Ctrl Pts',(32.4455401815834,20.8441684555014,37.3835708321242));
#66972=CARTESIAN_POINT('Ctrl Pts',(32.4507159269834,20.925393944127,37.3877866540155));
#66973=CARTESIAN_POINT('Ctrl Pts',(32.4518406489614,21.0068777112335,37.3920024759069));
#66974=CARTESIAN_POINT('Ctrl Pts',(32.4489127114645,21.0881860625473,37.3962182977983));
#66975=CARTESIAN_POINT('Ctrl Pts',(32.4459586395247,21.170220163118,37.4004717496447));
#66976=CARTESIAN_POINT('Ctrl Pts',(32.4388791979954,21.2520752191937,37.4047252014912));
#66977=CARTESIAN_POINT('Ctrl Pts',(32.4277262971736,21.3333095798381,37.4089786533376));
#66978=CARTESIAN_POINT('Ctrl Pts',(32.4166559868236,21.4139423764337,37.413200607137));
#66979=CARTESIAN_POINT('Ctrl Pts',(32.4015724942055,21.4939631896608,37.4174225609363));
#66980=CARTESIAN_POINT('Ctrl Pts',(32.3825779496656,21.5729507516071,37.4216445147357));
#66981=CARTESIAN_POINT('Ctrl Pts',(32.3633708408417,21.6528222481231,37.4259137156057));
#66982=CARTESIAN_POINT('Ctrl Pts',(32.3401647367117,21.7316367547278,37.4301829164756));
#66983=CARTESIAN_POINT('Ctrl Pts',(32.313116285293,21.808976699734,37.4344521173456));
#66984=CARTESIAN_POINT('Ctrl Pts',(32.2860678338742,21.8863166447401,37.4387213182155));
#66985=CARTESIAN_POINT('Ctrl Pts',(32.2551772777423,21.9621816037963,37.4429905190855));
#66986=CARTESIAN_POINT('Ctrl Pts',(32.2206494406737,22.0361787064187,37.4472597199555));
#66987=CARTESIAN_POINT('Ctrl Pts',(32.1864298465991,22.1095152090616,37.4514908080628));
#66988=CARTESIAN_POINT('Ctrl Pts',(32.1485092525824,22.1812923581581,37.4557218961701));
#66989=CARTESIAN_POINT('Ctrl Pts',(32.1070524450565,22.2511116032479,37.4599529842774));
#66990=CARTESIAN_POINT('Ctrl Pts',(32.0656551156771,22.3208306785576,37.4641780020361));
#66991=CARTESIAN_POINT('Ctrl Pts',(32.0207318843165,22.3885970323327,37.4684030197947));
#66992=CARTESIAN_POINT('Ctrl Pts',(31.9724947283962,22.4540339736228,37.4726280375533));
#66993=CARTESIAN_POINT('Ctrl Pts',(31.9241147065866,22.5196647220855,37.4768655687138));
#66994=CARTESIAN_POINT('Ctrl Pts',(31.8724013039645,22.5829518120537,37.4811030998743));
#66995=CARTESIAN_POINT('Ctrl Pts',(31.8176138401004,22.6435419612154,37.4853406310349));
#66996=CARTESIAN_POINT('Ctrl Pts',(31.7630865224159,22.703844411427,37.489558041214));
#66997=CARTESIAN_POINT('Ctrl Pts',(31.7055145802611,22.7614751231916,37.4937754513931));
#66998=CARTESIAN_POINT('Ctrl Pts',(31.645194657271,22.8161180549973,37.4979928615722));
#66999=CARTESIAN_POINT('Ctrl Pts',(31.5848946734435,22.8707429242086,37.5022088776575));
#67000=CARTESIAN_POINT('Ctrl Pts',(31.5218488569751,22.9223816628367,37.5064248937429));
#67001=CARTESIAN_POINT('Ctrl Pts',(31.4563898413395,22.970755915897,37.5106409098283));
#67002=CARTESIAN_POINT('Ctrl Pts',(31.3909324066066,23.0191290006693,37.5148568240925));
#67003=CARTESIAN_POINT('Ctrl Pts',(31.32306226317,23.0642374811803,37.5190727383567));
#67004=CARTESIAN_POINT('Ctrl Pts',(31.2531430119955,23.1058449234184,37.5232886526209));
#67005=CARTESIAN_POINT('Ctrl Pts',(31.1826029970165,23.1478217688422,37.5275419970197));
#67006=CARTESIAN_POINT('Ctrl Pts',(31.1099777121315,23.1862348383738,37.5317953414184));
#67007=CARTESIAN_POINT('Ctrl Pts',(31.0356664090088,23.2208884121565,37.5360486858172));
#67008=CARTESIAN_POINT('Ctrl Pts',(30.9619019186093,23.2552869908812,37.5402707323819));
#67009=CARTESIAN_POINT('Ctrl Pts',(30.8864765989373,23.2859810985366,37.5444927789466));
#67010=CARTESIAN_POINT('Ctrl Pts',(30.8097998461114,23.3128282381617,37.5487148255113));
#67011=CARTESIAN_POINT('Ctrl Pts',(30.7322704915026,23.3399739026755,37.5529838188271));
#67012=CARTESIAN_POINT('Ctrl Pts',(30.653462169298,23.3631863789658,37.5572528121428));
#67013=CARTESIAN_POINT('Ctrl Pts',(30.5738106252478,23.3823710072851,37.5615218054586));
#67014=CARTESIAN_POINT('Ctrl Pts',(30.4941590811977,23.4015556356044,37.5657907987744));
#67015=CARTESIAN_POINT('Ctrl Pts',(30.4136648031984,23.4167123898188,37.5700597920902));
#67016=CARTESIAN_POINT('Ctrl Pts',(30.3327688885244,23.4278004689081,37.574328785406));
#67017=CARTESIAN_POINT('Ctrl Pts',(30.2525914914025,23.4387900636737,37.5785598615211));
#67018=CARTESIAN_POINT('Ctrl Pts',(30.1717186653201,23.4458242593714,37.5827909376363));
#67019=CARTESIAN_POINT('Ctrl Pts',(30.0905746568081,23.4488255310544,37.5870220137514));
#67020=CARTESIAN_POINT('Ctrl Pts',(30.0095470655888,23.4518224968136,37.5912470195425));
#67021=CARTESIAN_POINT('Ctrl Pts',(29.9282495253672,23.4507980129853,37.5954720253336));
#67022=CARTESIAN_POINT('Ctrl Pts',(29.8471134892017,23.4457260608694,37.5996970311247));
#67023=CARTESIAN_POINT('Ctrl Pts',(29.7657368612176,23.4406390689483,37.6039345652802));
#67024=CARTESIAN_POINT('Ctrl Pts',(29.6845231655729,23.4314805080844,37.6081720994357));
#67025=CARTESIAN_POINT('Ctrl Pts',(29.6039098464817,23.4182768328473,37.6124096335912));
#67026=CARTESIAN_POINT('Ctrl Pts',(29.5236795834133,23.4051358984497,37.6166270319552));
#67027=CARTESIAN_POINT('Ctrl Pts',(29.4440444673046,23.3879882755164,37.6208444303193));
#67028=CARTESIAN_POINT('Ctrl Pts',(29.3654308702183,23.3669119691125,37.6250618286833));
#67029=CARTESIAN_POINT('Ctrl Pts',(29.2868432578898,23.3458426292225,37.6292778330382));
#67030=CARTESIAN_POINT('Ctrl Pts',(29.2092769428068,23.3208473049538,37.6334938373931));
#67031=CARTESIAN_POINT('Ctrl Pts',(29.1331461317234,23.2920546723527,37.637709841748));
#67032=CARTESIAN_POINT('Ctrl Pts',(29.0570171574561,23.2632627344345,37.6419257443829));
#67033=CARTESIAN_POINT('Ctrl Pts',(28.9823240528332,23.2306738358525,37.6461416470178));
#67034=CARTESIAN_POINT('Ctrl Pts',(28.9094625786465,23.1944653979108,37.6503575496527));
#67035=CARTESIAN_POINT('Ctrl Pts',(28.8359537734017,23.1579352694363,37.6546109080863));
#67036=CARTESIAN_POINT('Ctrl Pts',(28.7643097455512,23.1177211641151,37.65886426652));
#67037=CARTESIAN_POINT('Ctrl Pts',(28.6949113690655,23.074052534389,37.6631176249536));
#67038=CARTESIAN_POINT('Ctrl Pts',(28.6260240650023,23.0307054947852,37.6673396602597));
#67039=CARTESIAN_POINT('Ctrl Pts',(28.5593497956466,22.9839549628578,37.6715616955658));
#67040=CARTESIAN_POINT('Ctrl Pts',(28.4952301982313,22.9340677582972,37.6757837308719));
#67041=CARTESIAN_POINT('Ctrl Pts',(28.4303970493476,22.8836253866816,37.6800527508694));
#67042=CARTESIAN_POINT('Ctrl Pts',(28.3681761538577,22.8299764158856,37.6843217708668));
#67043=CARTESIAN_POINT('Ctrl Pts',(28.3088832363183,22.7734357449862,37.6885907908642));
#67044=CARTESIAN_POINT('Ctrl Pts',(28.2495903187789,22.7168950740868,37.6928598108616));
#67045=CARTESIAN_POINT('Ctrl Pts',(28.1932256655969,22.6574630989647,37.697128830859));
#67046=CARTESIAN_POINT('Ctrl Pts',(28.1400626378422,22.5954884076199,37.7013978508565));
#67047=CARTESIAN_POINT('Ctrl Pts',(28.0877693370062,22.5345275986595,37.70559703131));
#67048=CARTESIAN_POINT('Ctrl Pts',(28.0383698377252,22.4708688955375,37.7097962117636));
#67049=CARTESIAN_POINT('Ctrl Pts',(27.9921578849601,22.4048203767998,37.7139953922172));
#67050=CARTESIAN_POINT('Ctrl Pts',(27.9460081015478,22.3388607137244,37.7181889234758));
#67051=CARTESIAN_POINT('Ctrl Pts',(27.9030376245187,22.2705179968799,37.7223824547344));
#67052=CARTESIAN_POINT('Ctrl Pts',(27.8635012387214,22.2001346978798,37.726575985993));
#67053=CARTESIAN_POINT('Ctrl Pts',(27.8240054789372,22.1298237219504,37.7307652081461));
#67054=CARTESIAN_POINT('Ctrl Pts',(27.7879370364907,22.0574767349971,37.7349544302993));
#67055=CARTESIAN_POINT('Ctrl Pts',(27.7555076055583,21.9834653737135,37.7391436524524));
#67056=CARTESIAN_POINT('Ctrl Pts',(27.7216214270493,21.9061293820526,37.7435210567304));
#67057=CARTESIAN_POINT('Ctrl Pts',(27.6917091889156,21.8269764095386,37.7478984610083));
#67058=CARTESIAN_POINT('Ctrl Pts',(27.665958510845,21.7464586906875,37.7522758652863));
#67059=CARTESIAN_POINT('Ctrl Pts',(27.6413376838498,21.6694738120588,37.7564612041391));
#67060=CARTESIAN_POINT('Ctrl Pts',(27.6205210305988,21.5912419318454,37.7606465429919));
#67061=CARTESIAN_POINT('Ctrl Pts',(27.603622382931,21.5121763040309,37.7648318818448));
#67062=CARTESIAN_POINT('Ctrl Pts',(27.586725155894,21.4331173230834,37.7690168688457));
#67063=CARTESIAN_POINT('Ctrl Pts',(27.5737453711307,21.3532251972858,37.7732018558466));
#67064=CARTESIAN_POINT('Ctrl Pts',(27.5647458291997,21.2729237505235,37.7773868428476));
#67065=CARTESIAN_POINT('Ctrl Pts',(27.5557418328296,21.1925825575264,37.7815739012617));
#67066=CARTESIAN_POINT('Ctrl Pts',(27.550722051835,21.111832109761,37.7857609596758));
#67067=CARTESIAN_POINT('Ctrl Pts',(27.5496973641803,21.0311005288507,37.7899480180899));
#67068=CARTESIAN_POINT('Ctrl Pts',(27.5495566879162,21.0200171346639,37.790522846656));
#67069=CARTESIAN_POINT('Ctrl Pts',(27.5494912296765,21.0089340952719,37.791097675222));
#67070=CARTESIAN_POINT('Ctrl Pts',(27.5495009409688,20.9978525161318,37.791672503788));
#67071=CARTESIAN_POINT('',(27.5495000018184,21.000094404414,38.5916725038344));
#67072=CARTESIAN_POINT('Ctrl Pts',(27.5495009409694,20.9978525154208,37.7916725038249));
#67073=CARTESIAN_POINT('Ctrl Pts',(27.5495877392395,20.8988068312588,37.7968102452855));
#67074=CARTESIAN_POINT('Ctrl Pts',(27.5556832349185,20.800025431165,37.8019479867462));
#67075=CARTESIAN_POINT('Ctrl Pts',(27.5676691624476,20.7021460984115,37.8070857282068));
#67076=CARTESIAN_POINT('Ctrl Pts',(27.5798394239549,20.6027614598102,37.8123024840216));
#67077=CARTESIAN_POINT('Ctrl Pts',(27.5980826296213,20.5043067985095,37.8175192398364));
#67078=CARTESIAN_POINT('Ctrl Pts',(27.6222262848908,20.4074272958228,37.8227359956512));
#67079=CARTESIAN_POINT('Ctrl Pts',(27.6310673716759,20.3719513050752,37.8246463025364));
#67080=CARTESIAN_POINT('Ctrl Pts',(27.6406992042418,20.3366863206436,37.8265566094216));
#67081=CARTESIAN_POINT('Ctrl Pts',(27.6511117280305,20.3016633077059,37.8284669163068));
#67082=CARTESIAN_POINT('Ctrl Pts',(27.6741740636527,20.2240920583861,37.8326979883718));
#67083=CARTESIAN_POINT('Ctrl Pts',(27.7011264532798,20.1475189097962,37.8369290604367));
#67084=CARTESIAN_POINT('Ctrl Pts',(27.7318645173868,20.0723623107533,37.8411601325017));
#67085=CARTESIAN_POINT('Ctrl Pts',(27.7625584804569,19.9973135416613,37.8453851340911));
#67086=CARTESIAN_POINT('Ctrl Pts',(27.7970271562525,19.9236777123993,37.8496101356806));
#67087=CARTESIAN_POINT('Ctrl Pts',(27.8351162725447,19.8518585903298,37.85383513727));
#67088=CARTESIAN_POINT('Ctrl Pts',(27.873318381375,19.7798264146199,37.858072672457));
#67089=CARTESIAN_POINT('Ctrl Pts',(27.9151623051707,19.709622193279,37.862310207644));
#67090=CARTESIAN_POINT('Ctrl Pts',(27.9604434986149,19.6416335076064,37.8665477428309));
#67091=CARTESIAN_POINT('Ctrl Pts',(28.0055094667055,19.5739679779242,37.8707651366537));
#67092=CARTESIAN_POINT('Ctrl Pts',(28.0539798483688,19.5084973634363,37.8749825304765));
#67093=CARTESIAN_POINT('Ctrl Pts',(28.1056077059987,19.4455778930971,37.8791999242993));
#67094=CARTESIAN_POINT('Ctrl Pts',(28.1572184972102,19.3826792218004,37.8834159239947));
#67095=CARTESIAN_POINT('Ctrl Pts',(28.2119843969412,19.3223303791028,37.8876319236902));
#67096=CARTESIAN_POINT('Ctrl Pts',(28.269617326673,19.2648556100861,37.8918479233856));
#67097=CARTESIAN_POINT('Ctrl Pts',(28.3272488643532,19.2073822293007,37.8960638212488));
#67098=CARTESIAN_POINT('Ctrl Pts',(28.3877469643417,19.1527831117174,37.9002797191121));
#67099=CARTESIAN_POINT('Ctrl Pts',(28.4507867522404,19.1013455914869,37.9044956169753));
#67100=CARTESIAN_POINT('Ctrl Pts',(28.5143867625375,19.0494509559661,37.9087489807071));
#67101=CARTESIAN_POINT('Ctrl Pts',(28.5805734995497,19.0007747090515,37.913002344439));
#67102=CARTESIAN_POINT('Ctrl Pts',(28.6489808289029,18.9555691624982,37.9172557081708));
#67103=CARTESIAN_POINT('Ctrl Pts',(28.7168842192202,18.9106966334704,37.9214777384763));
#67104=CARTESIAN_POINT('Ctrl Pts',(28.7869751575657,18.8692440248076,37.9256997687818));
#67105=CARTESIAN_POINT('Ctrl Pts',(28.8588696574109,18.8314124893788,37.9299217990873));
#67106=CARTESIAN_POINT('Ctrl Pts',(28.9315644953121,18.7931598088333,37.9341908295323));
#67107=CARTESIAN_POINT('Ctrl Pts',(29.0061028556114,18.758609527363,37.9384598599774));
#67108=CARTESIAN_POINT('Ctrl Pts',(29.0820676379718,18.7279193613031,37.9427288904224));
#67109=CARTESIAN_POINT('Ctrl Pts',(29.1580324203322,18.6972291952432,37.9469979208675));
#67110=CARTESIAN_POINT('Ctrl Pts',(29.2354231459706,18.6703992421989,37.9512669513125));
#67111=CARTESIAN_POINT('Ctrl Pts',(29.3138095002204,18.6475347296905,37.9555359817575));
#67112=CARTESIAN_POINT('Ctrl Pts',(29.3914988350456,18.62487353075,37.9597670515502));
#67113=CARTESIAN_POINT('Ctrl Pts',(29.4704577320105,18.6060224369706,37.9639981213429));
#67114=CARTESIAN_POINT('Ctrl Pts',(29.5502779601612,18.5911205225493,37.9682291911355));
#67115=CARTESIAN_POINT('Ctrl Pts',(29.6299836670217,18.5762399885036,37.9724541904423));
#67116=CARTESIAN_POINT('Ctrl Pts',(29.7105477975081,18.5652974652656,37.976679189749));
#67117=CARTESIAN_POINT('Ctrl Pts',(29.7915474176048,18.5583821406918,37.9809041890557));
#67118=CARTESIAN_POINT('Ctrl Pts',(29.8727873803813,18.5514462969151,37.9851417248121));
#67119=CARTESIAN_POINT('Ctrl Pts',(29.9544649660325,18.5485617158995,37.9893792605684));
#67120=CARTESIAN_POINT('Ctrl Pts',(30.0361435948961,18.5497665640703,37.9936167963248));
#67121=CARTESIAN_POINT('Ctrl Pts',(30.1174339432304,18.5509656846831,37.9978341878568));
#67122=CARTESIAN_POINT('Ctrl Pts',(30.1987248564328,18.5562154411305,38.0020515793887));
#67123=CARTESIAN_POINT('Ctrl Pts',(30.2795831278049,18.56550138126,38.0062689709207));
#67124=CARTESIAN_POINT('Ctrl Pts',(30.3604146702023,18.5747842517759,38.0104849683275));
#67125=CARTESIAN_POINT('Ctrl Pts',(30.4408133932167,18.5881006033968,38.0147009657343));
#67126=CARTESIAN_POINT('Ctrl Pts',(30.5203506711986,18.6053840748498,38.0189169631411));
#67127=CARTESIAN_POINT('Ctrl Pts',(30.5998860281561,18.6226671288636,38.023132858721));
#67128=CARTESIAN_POINT('Ctrl Pts',(30.6785595273242,18.6439170123943,38.0273487543009));
#67129=CARTESIAN_POINT('Ctrl Pts',(30.7559536196955,18.6690164361649,38.0315646498808));
#67130=CARTESIAN_POINT('Ctrl Pts',(30.8340355904679,18.6943389435194,38.0358180163248));
#67131=CARTESIAN_POINT('Ctrl Pts',(30.9108148351232,18.7235796304054,38.0400713827687));
#67132=CARTESIAN_POINT('Ctrl Pts',(30.9858808732983,18.7565675509023,38.0443247492126));
#67133=CARTESIAN_POINT('Ctrl Pts',(31.0603938322985,18.7893124196505,38.0485467772715));
#67134=CARTESIAN_POINT('Ctrl Pts',(31.1332183541381,18.8257492212204,38.0527688053305));
#67135=CARTESIAN_POINT('Ctrl Pts',(31.2039772776005,18.8656642801514,38.0569908333894));
#67136=CARTESIAN_POINT('Ctrl Pts',(31.275524022823,18.9060237487828,38.0612598690258));
#67137=CARTESIAN_POINT('Ctrl Pts',(31.344958475327,18.9499391472324,38.0655289046623));
#67138=CARTESIAN_POINT('Ctrl Pts',(31.411922028399,18.9971454282146,38.0697979402987));
#67139=CARTESIAN_POINT('Ctrl Pts',(31.4788855814709,19.0443517091968,38.0740669759351));
#67140=CARTESIAN_POINT('Ctrl Pts',(31.5433778935879,19.0948485232448,38.0783360115715));
#67141=CARTESIAN_POINT('Ctrl Pts',(31.6050773073057,19.1483312694836,38.0826050472079));
#67142=CARTESIAN_POINT('Ctrl Pts',(31.6662279866382,19.2013383576875,38.0868361154391));
#67143=CARTESIAN_POINT('Ctrl Pts',(31.7248647884748,19.2574773912429,38.0910671836702));
#67144=CARTESIAN_POINT('Ctrl Pts',(31.780649581212,19.3164806746195,38.0952982519014));
#67145=CARTESIAN_POINT('Ctrl Pts',(31.8363543367703,19.3753993030908,38.0995232496114));
#67146=CARTESIAN_POINT('Ctrl Pts',(31.8892148933253,19.4371736846638,38.1037482473214));
#67147=CARTESIAN_POINT('Ctrl Pts',(31.9389270742472,19.5014967298163,38.1079732450314));
#67148=CARTESIAN_POINT('Ctrl Pts',(31.9887867850132,19.5660106651823,38.1122107811825));
#67149=CARTESIAN_POINT('Ctrl Pts',(32.0354790502061,19.6330881017077,38.1164483173336));
#67150=CARTESIAN_POINT('Ctrl Pts',(32.0787351748207,19.7023828288115,38.1206858534848));
#67151=CARTESIAN_POINT('Ctrl Pts',(32.1217856491692,19.7713481117223,38.1249032433457));
#67152=CARTESIAN_POINT('Ctrl Pts',(32.1614323284732,19.8425092556063,38.1291206332067));
#67153=CARTESIAN_POINT('Ctrl Pts',(32.1974525662052,19.9154943664148,38.1333380230677));
#67154=CARTESIAN_POINT('Ctrl Pts',(32.2334608966685,19.988455350416,38.1375540187793));
#67155=CARTESIAN_POINT('Ctrl Pts',(32.2658449605813,20.0632386873489,38.1417700144908));
#67156=CARTESIAN_POINT('Ctrl Pts',(32.2944282180476,20.1394481989869,38.1459860102023));
#67157=CARTESIAN_POINT('Ctrl Pts',(32.3230107850069,20.2156558695752,38.1502019040649));
#67158=CARTESIAN_POINT('Ctrl Pts',(32.347792565828,20.2932892106309,38.1544177979275));
#67159=CARTESIAN_POINT('Ctrl Pts',(32.3686458232528,20.3719337503202,38.1586336917901));
#67160=CARTESIAN_POINT('Ctrl Pts',(32.3896844426245,20.4512773512972,38.1628870601958));
#67161=CARTESIAN_POINT('Ctrl Pts',(32.4067242093454,20.5316497569512,38.1671404286015));
#67162=CARTESIAN_POINT('Ctrl Pts',(32.4196863094521,20.6126133535473,38.1713937970072));
#67163=CARTESIAN_POINT('Ctrl Pts',(32.4325528948016,20.6929803478788,38.1756158233119));
#67164=CARTESIAN_POINT('Ctrl Pts',(32.4414017193707,20.7739293757007,38.1798378496166));
#67165=CARTESIAN_POINT('Ctrl Pts',(32.4462079373079,20.855027666598,38.1840598759212));
#67166=CARTESIAN_POINT('Ctrl Pts',(32.4510676734933,20.9370290040333,38.1883289153775));
#67167=CARTESIAN_POINT('Ctrl Pts',(32.4517942096248,21.0191824609694,38.1925979548337));
#67168=CARTESIAN_POINT('Ctrl Pts',(32.4484159285209,21.1010430154209,38.1968669942899));
#67169=CARTESIAN_POINT('Ctrl Pts',(32.445037647417,21.1829035698723,38.2011360337461));
#67170=CARTESIAN_POINT('Ctrl Pts',(32.4375546576655,21.2644707454179,38.2054050732023));
#67171=CARTESIAN_POINT('Ctrl Pts',(32.426048608691,21.345309134354,38.2096741126585));
#67172=CARTESIAN_POINT('Ctrl Pts',(32.4146448971588,21.4254285280921,38.2139051822973));
#67173=CARTESIAN_POINT('Ctrl Pts',(32.3992466487324,21.5051327585229,38.2181362519361));
#67174=CARTESIAN_POINT('Ctrl Pts',(32.3798955692347,21.5839925766113,38.2223673215748));
#67175=CARTESIAN_POINT('Ctrl Pts',(32.3605722535719,21.6627392510907,38.2265923207141));
#67176=CARTESIAN_POINT('Ctrl Pts',(32.3373074803006,21.7406434716311,38.2308173198533));
#67177=CARTESIAN_POINT('Ctrl Pts',(32.3101944645759,21.8172831735957,38.2350423189926));
#67178=CARTESIAN_POINT('Ctrl Pts',(32.283000997572,21.8941502852344,38.2392798547891));
#67179=CARTESIAN_POINT('Ctrl Pts',(32.2519364864172,21.969744894976,38.2435173905856));
#67180=CARTESIAN_POINT('Ctrl Pts',(32.2171462534557,22.0436535540051,38.2477549263821));
#67181=CARTESIAN_POINT('Ctrl Pts',(32.1825214068497,22.1172108648909,38.2519723177145));
#67182=CARTESIAN_POINT('Ctrl Pts',(32.1442063752251,22.1890977918698,38.2561897090468));
#67183=CARTESIAN_POINT('Ctrl Pts',(32.1023930227776,22.2589256641185,38.2604071003791));
#67184=CARTESIAN_POINT('Ctrl Pts',(32.0605934925087,22.3287304534697,38.2646230975746));
#67185=CARTESIAN_POINT('Ctrl Pts',(32.0152981766068,22.3964771411798,38.2688390947701));
#67186=CARTESIAN_POINT('Ctrl Pts',(31.9667443365176,22.4618026422112,38.2730550919655));
#67187=CARTESIAN_POINT('Ctrl Pts',(31.9181916692574,22.5271265652905,38.2772709873226));
#67188=CARTESIAN_POINT('Ctrl Pts',(31.8663809125555,22.5900290454566,38.2814868826797));
#67189=CARTESIAN_POINT('Ctrl Pts',(31.811591151904,22.650178095947,38.2857027780368));
#67190=CARTESIAN_POINT('Ctrl Pts',(31.7563144141723,22.710861757442,38.2899561447095));
#67191=CARTESIAN_POINT('Ctrl Pts',(31.6980057637354,22.7687424318833,38.2942095113822));
#67192=CARTESIAN_POINT('Ctrl Pts',(31.6369902492213,22.8235167051482,38.2984628780549));
#67193=CARTESIAN_POINT('Ctrl Pts',(31.5764242978359,22.8778874008334,38.3026849058649));
#67194=CARTESIAN_POINT('Ctrl Pts',(31.5131916421712,22.9291970715396,38.3069069336749));
#67195=CARTESIAN_POINT('Ctrl Pts',(31.4476425112592,22.9771902815852,38.3111289614849));
#67196=CARTESIAN_POINT('Ctrl Pts',(31.3813635526542,23.0257178507182,38.3153979975889));
#67197=CARTESIAN_POINT('Ctrl Pts',(31.3127166233379,23.070854381438,38.3196670336929));
#67198=CARTESIAN_POINT('Ctrl Pts',(31.2420910962522,23.1123825313165,38.3239360697969));
#67199=CARTESIAN_POINT('Ctrl Pts',(31.1714655691666,23.1539106811949,38.3282051059009));
#67200=CARTESIAN_POINT('Ctrl Pts',(31.0988619035401,23.1918302832754,38.3324741420049));
#67201=CARTESIAN_POINT('Ctrl Pts',(31.0246902622514,23.2259739702987,38.3367431781089));
#67202=CARTESIAN_POINT('Ctrl Pts',(30.9511782693252,23.2598139991199,38.3409742473751));
#67203=CARTESIAN_POINT('Ctrl Pts',(30.8758501925449,23.2900720565571,38.3452053166413));
#67204=CARTESIAN_POINT('Ctrl Pts',(30.7990893713817,23.3165505447852,38.3494363859075));
#67205=CARTESIAN_POINT('Ctrl Pts',(30.7224386823683,23.3429910431536,38.3536613846712));
#67206=CARTESIAN_POINT('Ctrl Pts',(30.644359767411,23.3656625918616,38.3578863834349));
#67207=CARTESIAN_POINT('Ctrl Pts',(30.5652578456333,23.3844147747298,38.3621113821986));
#67208=CARTESIAN_POINT('Ctrl Pts',(30.4859211993408,23.4032226022263,38.3663489180886));
#67209=CARTESIAN_POINT('Ctrl Pts',(30.4055558968884,23.4180875738996,38.3705864539787));
#67210=CARTESIAN_POINT('Ctrl Pts',(30.324588158273,23.4289077334285,38.3748239898687));
#67211=CARTESIAN_POINT('Ctrl Pts',(30.2440053344,23.4396764547057,38.3790413808212));
#67212=CARTESIAN_POINT('Ctrl Pts',(30.1628262527814,23.4464386664054,38.3832587717737));
#67213=CARTESIAN_POINT('Ctrl Pts',(30.0814815351787,23.4491449547597,38.3874761627262));
#67214=CARTESIAN_POINT('Ctrl Pts',(30.0001637075973,23.4518503484996,38.3916921595411));
#67215=CARTESIAN_POINT('Ctrl Pts',(29.9186808171045,23.4505024659984,38.395908156356));
#67216=CARTESIAN_POINT('Ctrl Pts',(29.8374665881496,23.4451039119089,38.4001241531708));
#67217=CARTESIAN_POINT('Ctrl Pts',(29.7562543209474,23.439705488223,38.4043400481471));
#67218=CARTESIAN_POINT('Ctrl Pts',(29.6753111662452,23.4302566194287,38.4085559431233));
#67219=CARTESIAN_POINT('Ctrl Pts',(29.5950673819249,23.4168119134138,38.4127718380996));
#67220=CARTESIAN_POINT('Ctrl Pts',(29.514110366661,23.4032477067991,38.4170252052213));
#67221=CARTESIAN_POINT('Ctrl Pts',(29.4338656936714,23.3856163381214,38.4212785723429));
#67222=CARTESIAN_POINT('Ctrl Pts',(29.35476452036,23.3640265281535,38.4255319394645));
#67223=CARTESIAN_POINT('Ctrl Pts',(29.2762461808626,23.3425957963733,38.4297539668971));
#67224=CARTESIAN_POINT('Ctrl Pts',(29.1988549730422,23.3172649678906,38.4339759943296));
#67225=CARTESIAN_POINT('Ctrl Pts',(29.1229953809785,23.2881899283528,38.4381980217621));
#67226=CARTESIAN_POINT('Ctrl Pts',(29.0462911416199,23.2587911571308,38.4424670587283));
#67227=CARTESIAN_POINT('Ctrl Pts',(28.971153283341,23.2255644764019,38.4467360956945));
#67228=CARTESIAN_POINT('Ctrl Pts',(28.8979754928976,23.1887193140615,38.4510051326607));
#67229=CARTESIAN_POINT('Ctrl Pts',(28.8247977024543,23.1518741517211,38.4552741696269));
#67230=CARTESIAN_POINT('Ctrl Pts',(28.7535803690505,23.1114108032114,38.4595432065931));
#67231=CARTESIAN_POINT('Ctrl Pts',(28.6846864487342,23.0675832539118,38.4638122435594));
#67232=CARTESIAN_POINT('Ctrl Pts',(28.6164052553478,23.0241454969133,38.4680433126773));
#67233=CARTESIAN_POINT('Ctrl Pts',(28.5501500146718,22.97724014817,38.4722743817952));
#67234=CARTESIAN_POINT('Ctrl Pts',(28.4862945500099,22.9270822661916,38.4765054509131));
#67235=CARTESIAN_POINT('Ctrl Pts',(28.4225307016716,22.8769963479953,38.4807304495248));
#67236=CARTESIAN_POINT('Ctrl Pts',(28.3611601537357,22.823667449454,38.4849554481365));
#67237=CARTESIAN_POINT('Ctrl Pts',(28.3025289370975,22.7673545882501,38.4891804467482));
#67238=CARTESIAN_POINT('Ctrl Pts',(28.2437237374235,22.7108746235286,38.4934179826757));
#67239=CARTESIAN_POINT('Ctrl Pts',(28.1876745481238,22.6513932170041,38.4976555186033));
#67240=CARTESIAN_POINT('Ctrl Pts',(28.1346980572471,22.5892132998318,38.5018930545309));
#67241=CARTESIAN_POINT('Ctrl Pts',(28.0819734152257,22.5273289843633,38.5061104453232));
#67242=CARTESIAN_POINT('Ctrl Pts',(28.0322926309513,22.4627721102107,38.5103278361156));
#67243=CARTESIAN_POINT('Ctrl Pts',(27.9859306220108,22.3958777849963,38.5145452269079));
#67244=CARTESIAN_POINT('Ctrl Pts',(27.9395839389319,22.329005572999,38.5187612235599));
#67245=CARTESIAN_POINT('Ctrl Pts',(27.8965541171862,22.2597978262391,38.5229772202119));
#67246=CARTESIAN_POINT('Ctrl Pts',(27.857074040336,22.1886204530455,38.5271932168639));
#67247=CARTESIAN_POINT('Ctrl Pts',(27.8175949171616,22.1174447992037,38.5314091116748));
#67248=CARTESIAN_POINT('Ctrl Pts',(27.7816655929627,22.0443000206626,38.5356250064857));
#67249=CARTESIAN_POINT('Ctrl Pts',(27.7494733695953,21.9695772975061,38.5398409012966));
#67250=CARTESIAN_POINT('Ctrl Pts',(27.7169950093346,21.8941904099764,38.544094268606));
#67251=CARTESIAN_POINT('Ctrl Pts',(27.6883207216346,21.817197821933,38.5483476359155));
#67252=CARTESIAN_POINT('Ctrl Pts',(27.6635928201128,21.7390207979288,38.5526010032249));
#67253=CARTESIAN_POINT('Ctrl Pts',(27.6390471209577,21.6614198049636,38.5568230304876));
#67254=CARTESIAN_POINT('Ctrl Pts',(27.6183899040228,21.5826522427068,38.5610450577502));
#67255=CARTESIAN_POINT('Ctrl Pts',(27.6017093895468,21.5031425223654,38.5652670850129));
#67256=CARTESIAN_POINT('Ctrl Pts',(27.5848431462474,21.4227475027822,38.5695361223457));
#67257=CARTESIAN_POINT('Ctrl Pts',(27.5720427878845,21.341594177903,38.5738051596785));
#67258=CARTESIAN_POINT('Ctrl Pts',(27.5633456864671,21.2601269043015,38.5780741970114));
#67259=CARTESIAN_POINT('Ctrl Pts',(27.5546485850497,21.1786596307001,38.5823432343442));
#67260=CARTESIAN_POINT('Ctrl Pts',(27.550054703235,21.0968788955847,38.5866122716771));
#67261=CARTESIAN_POINT('Ctrl Pts',(27.5495473118384,21.0152273793423,38.5908813090099));
#67262=CARTESIAN_POINT('Ctrl Pts',(27.5495159663311,21.0101831310155,38.5911450406026));
#67263=CARTESIAN_POINT('Ctrl Pts',(27.5495001961528,21.0051387858016,38.5914087721953));
#67264=CARTESIAN_POINT('Ctrl Pts',(27.5495000018185,21.0000944053028,38.5916725037879));
#67265=CARTESIAN_POINT('',(27.5495008920499,21.0020909174755,39.3916725037448));
#67266=CARTESIAN_POINT('Ctrl Pts',(27.5495000018184,21.000094404414,38.5916725038344));
#67267=CARTESIAN_POINT('Ctrl Pts',(27.5494968875853,20.9192567836295,38.5958988770199));
#67268=CARTESIAN_POINT('Ctrl Pts',(27.5534981084526,20.8382656888067,38.6001252502055));
#67269=CARTESIAN_POINT('Ctrl Pts',(27.5615232630837,20.7575511321572,38.604351623391));
#67270=CARTESIAN_POINT('Ctrl Pts',(27.5695369025683,20.6769523913385,38.6085719322315));
#67271=CARTESIAN_POINT('Ctrl Pts',(27.5815629634692,20.5966298605576,38.612792241072));
#67272=CARTESIAN_POINT('Ctrl Pts',(27.5975690364578,20.5170137523555,38.6170125499125));
#67273=CARTESIAN_POINT('Ctrl Pts',(27.6135565785834,20.437489818867,38.6212279727348));
#67274=CARTESIAN_POINT('Ctrl Pts',(27.6335148842582,20.3586711372262,38.625443395557));
#67275=CARTESIAN_POINT('Ctrl Pts',(27.657359896073,20.280981506863,38.6296588183792));
#67276=CARTESIAN_POINT('Ctrl Pts',(27.6811897786626,20.2033411691538,38.6338715665925));
#67277=CARTESIAN_POINT('Ctrl Pts',(27.7089013361122,20.1268289052043,38.6380843148059));
#67278=CARTESIAN_POINT('Ctrl Pts',(27.7403599824137,20.0518558965418,38.6422970630192));
#67279=CARTESIAN_POINT('Ctrl Pts',(27.7718083666841,19.9769073446006,38.6465084370045));
#67280=CARTESIAN_POINT('Ctrl Pts',(27.8070012323353,19.9034974803584,38.6507198109898));
#67281=CARTESIAN_POINT('Ctrl Pts',(27.8457554312733,19.8320185840041,38.6549311849751));
#67282=CARTESIAN_POINT('Ctrl Pts',(27.8845089350744,19.7605409697722,38.6591424834206));
#67283=CARTESIAN_POINT('Ctrl Pts',(27.9268234218982,19.6909946637565,38.6633537818662));
#67284=CARTESIAN_POINT('Ctrl Pts',(27.9724699464796,19.6237470682786,38.6675650803118));
#67285=CARTESIAN_POINT('Ctrl Pts',(28.0181616309772,19.5564329420889,38.6717805451618));
#67286=CARTESIAN_POINT('Ctrl Pts',(28.0671916763067,19.4914224562388,38.6759960100119));
#67287=CARTESIAN_POINT('Ctrl Pts',(28.1192882731924,19.4290532629499,38.6802114748619));
#67288=CARTESIAN_POINT('Ctrl Pts',(28.1714094082835,19.366654692923,38.6844289252532));
#67289=CARTESIAN_POINT('Ctrl Pts',(28.2265996556414,19.3069002367344,38.6886463756445));
#67290=CARTESIAN_POINT('Ctrl Pts',(28.2845491494127,19.250091822632,38.6928638260358));
#67291=CARTESIAN_POINT('Ctrl Pts',(28.3426040636323,19.1931800639085,38.6970889487204));
#67292=CARTESIAN_POINT('Ctrl Pts',(28.4034279052085,19.1392253670635,38.701314071405));
#67293=CARTESIAN_POINT('Ctrl Pts',(28.4666765370618,19.0884902804319,38.7055391940896));
#67294=CARTESIAN_POINT('Ctrl Pts',(28.5286069026978,19.038812645144,38.7096762542132));
#67295=CARTESIAN_POINT('Ctrl Pts',(28.5928615630646,18.9922218662125,38.7138133143368));
#67296=CARTESIAN_POINT('Ctrl Pts',(28.6590926403957,18.9489227944909,38.7179503744604));
#67297=CARTESIAN_POINT('Ctrl Pts',(28.7268287296149,18.904639809774,38.7221814436945));
#67298=CARTESIAN_POINT('Ctrl Pts',(28.7968879321114,18.8636327712722,38.7264125129286));
#67299=CARTESIAN_POINT('Ctrl Pts',(28.8689201357594,18.8261535034162,38.7306435821627));
#67300=CARTESIAN_POINT('Ctrl Pts',(28.9408489915871,18.7887280087401,38.7348685808928));
#67301=CARTESIAN_POINT('Ctrl Pts',(29.0147448175114,18.7548204451191,38.7390935796229));
#67302=CARTESIAN_POINT('Ctrl Pts',(29.0902289209727,18.7246391860266,38.7433185783529));
#67303=CARTESIAN_POINT('Ctrl Pts',(29.1659370143001,18.6943683677307,38.7475561142512));
#67304=CARTESIAN_POINT('Ctrl Pts',(29.2432424276188,18.667846257808,38.7517936501494));
#67305=CARTESIAN_POINT('Ctrl Pts',(29.3217385691692,18.6452363852294,38.7560311860477));
#67306=CARTESIAN_POINT('Ctrl Pts',(29.3998615449285,18.6227339985835,38.7602485769629));
#67307=CARTESIAN_POINT('Ctrl Pts',(29.4791635047628,18.6041068717068,38.7644659678782));
#67308=CARTESIAN_POINT('Ctrl Pts',(29.5592257759526,18.589467209637,38.7686833587934));
#67309=CARTESIAN_POINT('Ctrl Pts',(29.6392615810333,18.5748323869863,38.7728993555698));
#67310=CARTESIAN_POINT('Ctrl Pts',(29.7200567413363,18.5641824950953,38.7771153523461));
#67311=CARTESIAN_POINT('Ctrl Pts',(29.8011818652027,18.5575787424615,38.7813313491225));
#67312=CARTESIAN_POINT('Ctrl Pts',(29.8823050294451,18.5509751493452,38.785547244059));
#67313=CARTESIAN_POINT('Ctrl Pts',(29.9637576778849,18.5484175377863,38.7897631389955));
#67314=CARTESIAN_POINT('Ctrl Pts',(30.0451061999861,18.5499151686681,38.793979033932));
#67315=CARTESIAN_POINT('Ctrl Pts',(30.1271777738817,18.5514261109742,38.7982324010969));
#67316=CARTESIAN_POINT('Ctrl Pts',(30.2091428798303,18.5570647529042,38.8024857682618));
#67317=CARTESIAN_POINT('Ctrl Pts',(30.2905590595226,18.5667869631022,38.8067391354267));
#67318=CARTESIAN_POINT('Ctrl Pts',(30.3713753463214,18.5764375378486,38.8109611628168));
#67319=CARTESIAN_POINT('Ctrl Pts',(30.4516503165892,18.590111563357,38.815183190207));
#67320=CARTESIAN_POINT('Ctrl Pts',(30.5309609591426,18.6077143335575,38.8194052175971));
#67321=CARTESIAN_POINT('Ctrl Pts',(30.6111546766192,18.6255130997106,38.8236742546494));
#67322=CARTESIAN_POINT('Ctrl Pts',(30.6903619879445,18.6473285118998,38.8279432917017));
#67323=CARTESIAN_POINT('Ctrl Pts',(30.7681626877384,18.6730113160639,38.832212328754));
#67324=CARTESIAN_POINT('Ctrl Pts',(30.8459633875323,18.698694120228,38.8364813658063));
#67325=CARTESIAN_POINT('Ctrl Pts',(30.9223570473736,18.7282440813745,38.8407504028586));
#67326=CARTESIAN_POINT('Ctrl Pts',(30.9969473057037,18.7614633530697,38.8450194399109));
#67327=CARTESIAN_POINT('Ctrl Pts',(31.070874175486,18.7943871802268,38.8492505091326));
#67328=CARTESIAN_POINT('Ctrl Pts',(31.1433070747894,18.8310388393118,38.8534815783543));
#67329=CARTESIAN_POINT('Ctrl Pts',(31.2138446176822,18.8712605856696,38.857712647576));
#67330=CARTESIAN_POINT('Ctrl Pts',(31.2842809572046,18.9114246240873,38.8619376462933));
#67331=CARTESIAN_POINT('Ctrl Pts',(31.3528269406415,18.9551483484349,38.8661626450106));
#67332=CARTESIAN_POINT('Ctrl Pts',(31.4191022075216,19.0022264456132,38.8703876437279));
#67333=CARTESIAN_POINT('Ctrl Pts',(31.4855741384192,19.0494442414779,38.8746251796293));
#67334=CARTESIAN_POINT('Ctrl Pts',(31.5497614257093,19.1000361519305,38.8788627155307));
#67335=CARTESIAN_POINT('Ctrl Pts',(31.6113062747142,19.153749112643,38.8831002514321));
#67336=CARTESIAN_POINT('Ctrl Pts',(31.6725585430787,19.2072067250574,38.8873176423338));
#67337=CARTESIAN_POINT('Ctrl Pts',(31.7311930835111,19.2637554767435,38.8915350332354));
#67338=CARTESIAN_POINT('Ctrl Pts',(31.7868886856299,19.3231043338454,38.895752424137));
#67339=CARTESIAN_POINT('Ctrl Pts',(31.8425658765024,19.3824335720478,38.8999684208995));
#67340=CARTESIAN_POINT('Ctrl Pts',(31.8953057404331,19.4445607387253,38.9041844176619));
#67341=CARTESIAN_POINT('Ctrl Pts',(31.9448241143915,19.509158152559,38.9084004144243));
#67342=CARTESIAN_POINT('Ctrl Pts',(31.9943412922019,19.5737540060009,38.9126163093467));
#67343=CARTESIAN_POINT('Ctrl Pts',(32.0406368527598,19.6408196182743,38.916832204269));
#67344=CARTESIAN_POINT('Ctrl Pts',(32.0834680025975,19.7099956077004,38.9210480991913));
#67345=CARTESIAN_POINT('Ctrl Pts',(32.12667984976,19.7797864560367,38.9253014663722));
#67346=CARTESIAN_POINT('Ctrl Pts',(32.1663651249108,19.8517249844587,38.929554833553));
#67347=CARTESIAN_POINT('Ctrl Pts',(32.2023211093903,19.925415437886,38.9338082007338));
#67348=CARTESIAN_POINT('Ctrl Pts',(32.238012161756,19.9985629227956,38.9380302281092));
#67349=CARTESIAN_POINT('Ctrl Pts',(32.2700285698777,20.0734361449724,38.9422522554846));
#67350=CARTESIAN_POINT('Ctrl Pts',(32.2982206575318,20.1496282816944,38.94647428286));
#67351=CARTESIAN_POINT('Ctrl Pts',(32.3267266469434,20.22666877154,38.9507433199436));
#67352=CARTESIAN_POINT('Ctrl Pts',(32.3513224783992,20.3050572627901,38.9550123570271));
#67353=CARTESIAN_POINT('Ctrl Pts',(32.3719058378373,20.3843597264366,38.9592813941107));
#67354=CARTESIAN_POINT('Ctrl Pts',(32.3924891972755,20.4636621900832,38.9635504311943));
#67355=CARTESIAN_POINT('Ctrl Pts',(32.4090600499826,20.5438781387238,38.9678194682778));
#67356=CARTESIAN_POINT('Ctrl Pts',(32.4215698413416,20.6245672450295,38.9720885053614));
#67357=CARTESIAN_POINT('Ctrl Pts',(32.4339683734725,20.7045387208463,38.9763195746038));
#67358=CARTESIAN_POINT('Ctrl Pts',(32.4424243708411,20.7852751140938,38.9805506438462));
#67359=CARTESIAN_POINT('Ctrl Pts',(32.4468528546562,20.8663536096225,38.9847817130886));
#67360=CARTESIAN_POINT('Ctrl Pts',(32.4512749847276,20.9473157782114,38.989006711827));
#67361=CARTESIAN_POINT('Ctrl Pts',(32.4516810525102,21.0286186139134,38.9932317105654));
#67362=CARTESIAN_POINT('Ctrl Pts',(32.4480374506469,21.1098311896978,38.9974567093037));
#67363=CARTESIAN_POINT('Ctrl Pts',(32.4443830368485,21.1912847536914,39.0016942451999));
#67364=CARTESIAN_POINT('Ctrl Pts',(32.4366548144621,21.2726470533978,39.0059317810961));
#67365=CARTESIAN_POINT('Ctrl Pts',(32.4248715360129,21.3534802453242,39.0101693169922));
#67366=CARTESIAN_POINT('Ctrl Pts',(32.4131442745107,21.433929161461,39.0143867079156));
#67367=CARTESIAN_POINT('Ctrl Pts',(32.3974004863793,21.5138535247576,39.018604098839));
#67368=CARTESIAN_POINT('Ctrl Pts',(32.3777106614346,21.5928256577614,39.0228214897623));
#67369=CARTESIAN_POINT('Ctrl Pts',(32.358027345337,21.6717716850206,39.0270374865467));
#67370=CARTESIAN_POINT('Ctrl Pts',(32.3344006952404,21.7497656562931,39.0312534833311));
#67371=CARTESIAN_POINT('Ctrl Pts',(32.3069520781732,21.8263911658604,39.0354694801155));
#67372=CARTESIAN_POINT('Ctrl Pts',(32.2795041241438,21.9030148244929,39.0396853750599));
#67373=CARTESIAN_POINT('Ctrl Pts',(32.2482345445415,21.9782696497905,39.0439012700044));
#67374=CARTESIAN_POINT('Ctrl Pts',(32.2133137687003,22.051756821362,39.0481171649488));
#67375=CARTESIAN_POINT('Ctrl Pts',(32.1780826059329,22.1258971702114,39.0523705321041));
#67376=CARTESIAN_POINT('Ctrl Pts',(32.1391352075502,22.1982378434502,39.0566238992593));
#67377=CARTESIAN_POINT('Ctrl Pts',(32.0966942906118,22.2683939852096,39.0608772664146));
#67378=CARTESIAN_POINT('Ctrl Pts',(32.0545660878117,22.338033200875,39.0650992938124));
#67379=CARTESIAN_POINT('Ctrl Pts',(32.0089959918147,22.4055196158146,39.0693213212101));
#67380=CARTESIAN_POINT('Ctrl Pts',(31.960244769042,22.4705069518515,39.0735433486079));
#67381=CARTESIAN_POINT('Ctrl Pts',(31.9109507318739,22.5362178812571,39.0778123856419));
#67382=CARTESIAN_POINT('Ctrl Pts',(31.8584046011056,22.5993733597426,39.0820814226759));
#67383=CARTESIAN_POINT('Ctrl Pts',(31.8029156765867,22.6596521663041,39.0863504597099));
#67384=CARTESIAN_POINT('Ctrl Pts',(31.7474267520679,22.7199309728656,39.0906194967439));
#67385=CARTESIAN_POINT('Ctrl Pts',(31.6889954245913,22.7773328141653,39.0948885337779));
#67386=CARTESIAN_POINT('Ctrl Pts',(31.627965423889,22.8315782343711,39.0991575708119));
#67387=CARTESIAN_POINT('Ctrl Pts',(31.5674782094927,22.8853412087157,39.1033886400462));
#67388=CARTESIAN_POINT('Ctrl Pts',(31.5042113702353,22.9362054998204,39.1076197092805));
#67389=CARTESIAN_POINT('Ctrl Pts',(31.4384741774593,22.9838705327674,39.1118507785148));
#67390=CARTESIAN_POINT('Ctrl Pts',(31.3728313007722,23.031467178561,39.116075777245));
#67391=CARTESIAN_POINT('Ctrl Pts',(31.3047254830865,23.0758734118581,39.1203007759751));
#67392=CARTESIAN_POINT('Ctrl Pts',(31.2345006554552,23.1168274331368,39.1245257747053));
#67393=CARTESIAN_POINT('Ctrl Pts',(31.164067444219,23.1579029804751,39.1287633106035));
#67394=CARTESIAN_POINT('Ctrl Pts',(31.0915029841239,23.1955054853551,39.1330008465017));
#67395=CARTESIAN_POINT('Ctrl Pts',(31.017185397046,23.2294134022286,39.1372383823999));
#67396=CARTESIAN_POINT('Ctrl Pts',(30.943221111174,23.2631601229654,39.1414557733149));
#67397=CARTESIAN_POINT('Ctrl Pts',(30.8675207528168,23.2932471040874,39.1456731642299));
#67398=CARTESIAN_POINT('Ctrl Pts',(30.7904819413076,23.3195017892786,39.1498905551449));
#67399=CARTESIAN_POINT('Ctrl Pts',(30.7134685964475,23.3457477954826,39.1541065519209));
#67400=CARTESIAN_POINT('Ctrl Pts',(30.6351181168376,23.3681638716389,39.1583225486969));
#67401=CARTESIAN_POINT('Ctrl Pts',(30.5558462239094,23.3866263271333,39.1625385454729));
#67402=CARTESIAN_POINT('Ctrl Pts',(30.4765762458415,23.4050883366559,39.1667544404089));
#67403=CARTESIAN_POINT('Ctrl Pts',(30.396385351801,23.4195968110048,39.1709703353449));
#67404=CARTESIAN_POINT('Ctrl Pts',(30.3157010757981,23.4300788219191,39.175186230281));
#67405=CARTESIAN_POINT('Ctrl Pts',(30.2342996520202,23.4406540003152,39.1794395974461));
#67406=CARTESIAN_POINT('Ctrl Pts',(30.152396506657,23.447130701546,39.1836929646112));
#67407=CARTESIAN_POINT('Ctrl Pts',(30.0704357773143,23.4494875078828,39.1879463317763));
#67408=CARTESIAN_POINT('Ctrl Pts',(29.9890789532496,23.451826948735,39.1921683591657));
#67409=CARTESIAN_POINT('Ctrl Pts',(29.9076658592812,23.4501070776601,39.196390386555));
#67410=CARTESIAN_POINT('Ctrl Pts',(29.8266288350047,23.4443593617036,39.2006124139443));
#67411=CARTESIAN_POINT('Ctrl Pts',(29.7446895135839,23.4385476484849,39.2048814509973));
#67412=CARTESIAN_POINT('Ctrl Pts',(29.6631351732003,23.4286178978568,39.2091504880503));
#67413=CARTESIAN_POINT('Ctrl Pts',(29.5824034001455,23.4146559443925,39.2134195251033));
#67414=CARTESIAN_POINT('Ctrl Pts',(29.5016716270906,23.4006939909282,39.2176885621563));
#67415=CARTESIAN_POINT('Ctrl Pts',(29.4217628796863,23.3827000040603,39.2219575992094));
#67416=CARTESIAN_POINT('Ctrl Pts',(29.3430983057943,23.3608113889402,39.2262266362624));
#67417=CARTESIAN_POINT('Ctrl Pts',(29.2651333562676,23.3391174460557,39.2304577054959));
#67418=CARTESIAN_POINT('Ctrl Pts',(29.188097907312,23.3135164956762,39.2346887747295));
#67419=CARTESIAN_POINT('Ctrl Pts',(29.1124121790456,23.2841055383001,39.238919843963));
#67420=CARTESIAN_POINT('Ctrl Pts',(29.0368350404775,23.2547367781397,39.2431448426924));
#67421=CARTESIAN_POINT('Ctrl Pts',(28.9626042062942,23.2215690345955,39.2473698414217));
#67422=CARTESIAN_POINT('Ctrl Pts',(28.8901260953187,23.1847494514721,39.251594840151));
#67423=CARTESIAN_POINT('Ctrl Pts',(28.8174329143776,23.1478206107208,39.2558323760495));
#67424=CARTESIAN_POINT('Ctrl Pts',(28.7465033289733,23.1072183551549,39.2600699119479));
#67425=CARTESIAN_POINT('Ctrl Pts',(28.6777284599249,23.0631403792053,39.2643074478463));
#67426=CARTESIAN_POINT('Ctrl Pts',(28.6092805423615,23.0192719472345,39.2685248387604));
#67427=CARTESIAN_POINT('Ctrl Pts',(28.5429672982889,22.9719610146033,39.2727422296745));
#67428=CARTESIAN_POINT('Ctrl Pts',(28.4791492459235,22.9214482126315,39.2769596205887));
#67429=CARTESIAN_POINT('Ctrl Pts',(28.4153522898335,22.8709521086307,39.2811756173637));
#67430=CARTESIAN_POINT('Ctrl Pts',(28.3540492517466,22.8172565255332,39.2853916141388));
#67431=CARTESIAN_POINT('Ctrl Pts',(28.2955693948253,22.7606437919533,39.2896076109139));
#67432=CARTESIAN_POINT('Ctrl Pts',(28.2370909505208,22.7040324258887,39.2938235058489));
#67433=CARTESIAN_POINT('Ctrl Pts',(28.1814358850927,22.6445043736385,39.298039400784));
#67434=CARTESIAN_POINT('Ctrl Pts',(28.1288972038969,22.582379403435,39.3022552957191));
#67435=CARTESIAN_POINT('Ctrl Pts',(28.0758915419931,22.5197022465014,39.3065086628852));
#67436=CARTESIAN_POINT('Ctrl Pts',(28.0260582638189,22.4543821326794,39.3107620300514));
#67437=CARTESIAN_POINT('Ctrl Pts',(27.979656084827,22.3867807016337,39.3150153972175));
#67438=CARTESIAN_POINT('Ctrl Pts',(27.9335958076563,22.3196773733256,39.3192374246059));
#67439=CARTESIAN_POINT('Ctrl Pts',(27.8909164286964,22.2503266672343,39.3234594519942));
#67440=CARTESIAN_POINT('Ctrl Pts',(27.8518258253334,22.1791089709164,39.3276814793825));
#67441=CARTESIAN_POINT('Ctrl Pts',(27.8122999722509,22.1070983095459,39.3319505164376));
#67442=CARTESIAN_POINT('Ctrl Pts',(27.7764435212813,22.0331792638651,39.3362195534926));
#67443=CARTESIAN_POINT('Ctrl Pts',(27.7444215036457,21.9577660971156,39.3404885905477));
#67444=CARTESIAN_POINT('Ctrl Pts',(27.7123994860101,21.8823529303662,39.3447576276027));
#67445=CARTESIAN_POINT('Ctrl Pts',(27.6842120077232,21.8054461195461,39.3490266646578));
#67446=CARTESIAN_POINT('Ctrl Pts',(27.6599718513331,21.7274740637621,39.3532957017129));
#67447=CARTESIAN_POINT('Ctrl Pts',(27.6307739903376,21.6335548163087,39.3584378612152));
#67448=CARTESIAN_POINT('Ctrl Pts',(27.6072124747056,21.5378055642196,39.3635800207174));
#67449=CARTESIAN_POINT('Ctrl Pts',(27.5894793038261,21.4408403603544,39.3687221802197));
#67450=CARTESIAN_POINT('Ctrl Pts',(27.5719783728498,21.3451450472329,39.3737969961751));
#67451=CARTESIAN_POINT('Ctrl Pts',(27.560154166145,21.2482654276719,39.3788718121305));
#67452=CARTESIAN_POINT('Ctrl Pts',(27.5541451768665,21.1508125795628,39.3839466280858));
#67453=CARTESIAN_POINT('Ctrl Pts',(27.5510958246397,21.1013586621714,39.3865219199722));
#67454=CARTESIAN_POINT('Ctrl Pts',(27.5495432706177,21.0517574604063,39.3890972118585));
#67455=CARTESIAN_POINT('Ctrl Pts',(27.5495008920499,21.0020909174755,39.3916725037448));
#67456=CARTESIAN_POINT('',(27.5495003167105,20.9987541275197,40.1916725038142));
#67457=CARTESIAN_POINT('Ctrl Pts',(27.5495008920492,21.0020909166425,39.391672503788));
#67458=CARTESIAN_POINT('Ctrl Pts',(27.5494318810471,20.9212118439509,39.3958662166454));
#67459=CARTESIAN_POINT('Ctrl Pts',(27.553371295196,20.8402633153025,39.4000599295028));
#67460=CARTESIAN_POINT('Ctrl Pts',(27.5613130467361,20.7596748161747,39.4042536423602));
#67461=CARTESIAN_POINT('Ctrl Pts',(27.5692519940786,20.6791147724934,39.408445874436));
#67462=CARTESIAN_POINT('Ctrl Pts',(27.581190427325,20.5989149738489,39.4126381065117));
#67463=CARTESIAN_POINT('Ctrl Pts',(27.5970702728484,20.5195013253181,39.4168303385874));
#67464=CARTESIAN_POINT('Ctrl Pts',(27.6129495126589,20.4400907059015,39.4210224107568));
#67465=CARTESIAN_POINT('Ctrl Pts',(27.6327697726531,20.3614666382289,39.4252144829261));
#67466=CARTESIAN_POINT('Ctrl Pts',(27.6564218627886,20.2840448583991,39.4294065550955));
#67467=CARTESIAN_POINT('Ctrl Pts',(27.6803811398932,20.205617545369,39.4336530727678));
#67468=CARTESIAN_POINT('Ctrl Pts',(27.7082723719833,20.1284244542174,39.4378995904401));
#67469=CARTESIAN_POINT('Ctrl Pts',(27.7399305388862,20.0528800071055,39.4421461081125));
#67470=CARTESIAN_POINT('Ctrl Pts',(27.7712287202026,19.978194577263,39.4463443385558));
#67471=CARTESIAN_POINT('Ctrl Pts',(27.8062083394607,19.9051208898304,39.4505425689992));
#67472=CARTESIAN_POINT('Ctrl Pts',(27.8446630165833,19.8340357046993,39.4547407994425));
#67473=CARTESIAN_POINT('Ctrl Pts',(27.8837811410171,19.7617241076342,39.4590114607293));
#67474=CARTESIAN_POINT('Ctrl Pts',(27.9264950968783,19.6914707088051,39.4632821220161));
#67475=CARTESIAN_POINT('Ctrl Pts',(27.9725421441624,19.6236407108598,39.467552783303));
#67476=CARTESIAN_POINT('Ctrl Pts',(28.0185891914466,19.5558107129145,39.4718234445898));
#67477=CARTESIAN_POINT('Ctrl Pts',(28.0679689693166,19.4904044755504,39.4760941058766));
#67478=CARTESIAN_POINT('Ctrl Pts',(28.1203778365118,19.4277497742014,39.4803647671634));
#67479=CARTESIAN_POINT('Ctrl Pts',(28.1723008364246,19.365675926267,39.4845958363983));
#67480=CARTESIAN_POINT('Ctrl Pts',(28.2273995277617,19.3060604645673,39.4888269056331));
#67481=CARTESIAN_POINT('Ctrl Pts',(28.2854122053,19.2492461782804,39.493057974868));
#67482=CARTESIAN_POINT('Ctrl Pts',(28.3433416494564,19.1925134059899,39.4972829735987));
#67483=CARTESIAN_POINT('Ctrl Pts',(28.4041764470199,19.1385741497362,39.5015079723293));
#67484=CARTESIAN_POINT('Ctrl Pts',(28.4676149074809,19.0877379420631,39.50573297106));
#67485=CARTESIAN_POINT('Ctrl Pts',(28.5312416138204,19.0367508841564,39.5099705069581));
#67486=CARTESIAN_POINT('Ctrl Pts',(28.597487152285,18.988885678891,39.5142080428562));
#67487=CARTESIAN_POINT('Ctrl Pts',(28.6660100934245,18.9444170707182,39.5184455787543));
#67488=CARTESIAN_POINT('Ctrl Pts',(28.7342072807563,18.9001598635476,39.5226629696698));
#67489=CARTESIAN_POINT('Ctrl Pts',(28.8046598767883,18.8592672920668,39.5268803605853));
#67490=CARTESIAN_POINT('Ctrl Pts',(28.8769999621023,18.8219685115036,39.5310977515008));
#67491=CARTESIAN_POINT('Ctrl Pts',(28.9493161340208,18.784682060764,39.5353137482773));
#67492=CARTESIAN_POINT('Ctrl Pts',(29.0235181432202,18.7509872546709,39.5395297450538));
#67493=CARTESIAN_POINT('Ctrl Pts',(29.0992129786693,18.7210675762098,39.5437457418303));
#67494=CARTESIAN_POINT('Ctrl Pts',(29.1749059856636,18.6911486204768,39.5479616367668));
#67495=CARTESIAN_POINT('Ctrl Pts',(29.2520913143972,18.6650047809581,39.5521775317033));
#67496=CARTESIAN_POINT('Ctrl Pts',(29.3303568044323,18.642771067412,39.5563934266398));
#67497=CARTESIAN_POINT('Ctrl Pts',(29.4093179432751,18.6203397334803,39.5606467938043));
#67498=CARTESIAN_POINT('Ctrl Pts',(29.4893780829221,18.6018885298034,39.5649001609688));
#67499=CARTESIAN_POINT('Ctrl Pts',(29.5701010645751,18.5875039574498,39.5691535281333));
#67500=CARTESIAN_POINT('Ctrl Pts',(29.6502292609765,18.5732253738903,39.5733755555231));
#67501=CARTESIAN_POINT('Ctrl Pts',(29.7310100900831,18.562953690652,39.5775975829129));
#67502=CARTESIAN_POINT('Ctrl Pts',(29.8120112854347,18.5567213639873,39.5818196103027));
#67503=CARTESIAN_POINT('Ctrl Pts',(29.8939143789668,18.5504196442223,39.5860886473545));
#67504=CARTESIAN_POINT('Ctrl Pts',(29.9760422882747,18.548247803433,39.5903576844064));
#67505=CARTESIAN_POINT('Ctrl Pts',(30.0579495617972,18.5501852930706,39.5946267214583));
#67506=CARTESIAN_POINT('Ctrl Pts',(30.1398568353197,18.5521227827082,39.5988957585101));
#67507=CARTESIAN_POINT('Ctrl Pts',(30.2215429948011,18.5581695025844,39.603164795562));
#67508=CARTESIAN_POINT('Ctrl Pts',(30.3025712642528,18.5682514768076,39.6074338326139));
#67509=CARTESIAN_POINT('Ctrl Pts',(30.3828788872287,18.5782437843103,39.6116649018487));
#67510=CARTESIAN_POINT('Ctrl Pts',(30.4628416922434,18.5922373140605,39.6158959710836));
#67511=CARTESIAN_POINT('Ctrl Pts',(30.5420297629938,18.6101979190676,39.6201270403184));
#67512=CARTESIAN_POINT('Ctrl Pts',(30.6211042190791,18.6281327551918,39.6243520390491));
#67513=CARTESIAN_POINT('Ctrl Pts',(30.6994056988939,18.6500232604064,39.6285770377798));
#67514=CARTESIAN_POINT('Ctrl Pts',(30.7765105631452,18.6757836599568,39.6328020365105));
#67515=CARTESIAN_POINT('Ctrl Pts',(30.8538442266582,18.7016205003446,39.6370395724086));
#67516=CARTESIAN_POINT('Ctrl Pts',(30.9299736934121,18.7313501746332,39.6412771083066));
#67517=CARTESIAN_POINT('Ctrl Pts',(31.004483021658,18.7648346573014,39.6455146442047));
#67518=CARTESIAN_POINT('Ctrl Pts',(31.0786381371836,18.798159956818,39.6497320351202));
#67519=CARTESIAN_POINT('Ctrl Pts',(31.151188053749,18.8352042586239,39.6539494260358));
#67520=CARTESIAN_POINT('Ctrl Pts',(31.2217407850415,18.8757825666457,39.6581668169513));
#67521=CARTESIAN_POINT('Ctrl Pts',(31.2922701937822,18.9163474607335,39.6623828137277));
#67522=CARTESIAN_POINT('Ctrl Pts',(31.3608033255887,18.9604438094675,39.6665988105042));
#67523=CARTESIAN_POINT('Ctrl Pts',(31.4269729772403,19.0078407763871,39.6708148072807));
#67524=CARTESIAN_POINT('Ctrl Pts',(31.4931410305236,19.0552365984041,39.6750307022172));
#67525=CARTESIAN_POINT('Ctrl Pts',(31.5569453398099,19.1059326084342,39.6792465971537));
#67526=CARTESIAN_POINT('Ctrl Pts',(31.6180490594758,19.159655605293,39.6834624920902));
#67527=CARTESIAN_POINT('Ctrl Pts',(31.6796958886238,19.2138561093994,39.6877158592547));
#67528=CARTESIAN_POINT('Ctrl Pts',(31.7385935081576,19.2711373741441,39.6919692264192));
#67529=CARTESIAN_POINT('Ctrl Pts',(31.7944328317891,19.3311797393975,39.6962225935837));
#67530=CARTESIAN_POINT('Ctrl Pts',(31.8498607186091,19.3907796988747,39.7004446209735));
#67531=CARTESIAN_POINT('Ctrl Pts',(31.9022749734291,19.4530998057375,39.7046666483633));
#67532=CARTESIAN_POINT('Ctrl Pts',(31.9514140381495,19.5177943794085,39.708888675753));
#67533=CARTESIAN_POINT('Ctrl Pts',(32.001100235945,19.58320928712,39.7131577128049));
#67534=CARTESIAN_POINT('Ctrl Pts',(32.0474375813126,19.6510514628234,39.7174267498568));
#67535=CARTESIAN_POINT('Ctrl Pts',(32.0902019145975,19.7209354174973,39.7216957869087));
#67536=CARTESIAN_POINT('Ctrl Pts',(32.1329662478825,19.7908193721712,39.7259648239606));
#67537=CARTESIAN_POINT('Ctrl Pts',(32.1721573940739,19.8627446495949,39.7302338610125));
#67538=CARTESIAN_POINT('Ctrl Pts',(32.207600795234,19.9363040947327,39.7345028980644));
#67539=CARTESIAN_POINT('Ctrl Pts',(32.2427289710765,20.0092093193755,39.7387339672995));
#67540=CARTESIAN_POINT('Ctrl Pts',(32.2743076826463,20.0839933687258,39.7429650365346));
#67541=CARTESIAN_POINT('Ctrl Pts',(32.3021326181401,20.16027643924,39.7471961057698));
#67542=CARTESIAN_POINT('Ctrl Pts',(32.3299176319551,20.236450063023,39.7514211045007));
#67543=CARTESIAN_POINT('Ctrl Pts',(32.3539594081034,20.3141180033863,39.7556461032317));
#67544=CARTESIAN_POINT('Ctrl Pts',(32.3741004241681,20.3928777503957,39.7598711019627));
#67545=CARTESIAN_POINT('Ctrl Pts',(32.394301206235,20.4718712073225,39.7641086378607));
#67546=CARTESIAN_POINT('Ctrl Pts',(32.4105778411914,20.5519625326692,39.7683461737587));
#67547=CARTESIAN_POINT('Ctrl Pts',(32.4228208894798,20.6327273662515,39.7725837096567));
#67548=CARTESIAN_POINT('Ctrl Pts',(32.4350057350778,20.7131082488363,39.7768011005725));
#67549=CARTESIAN_POINT('Ctrl Pts',(32.4431951820262,20.7941557882775,39.7810184914883));
#67550=CARTESIAN_POINT('Ctrl Pts',(32.4473322477455,20.8754402988734,39.7852358824041));
#67551=CARTESIAN_POINT('Ctrl Pts',(32.4514679458789,20.9566979393232,39.7894518791809));
#67552=CARTESIAN_POINT('Ctrl Pts',(32.4515538993977,21.0381919313699,39.7936678759576));
#67553=CARTESIAN_POINT('Ctrl Pts',(32.4475850815018,21.1194885718798,39.7978838727344));
#67554=CARTESIAN_POINT('Ctrl Pts',(32.4436163594751,21.2007832486199,39.8020997676712));
#67555=CARTESIAN_POINT('Ctrl Pts',(32.4355930845468,21.2818801189463,39.806315662608));
#67556=CARTESIAN_POINT('Ctrl Pts',(32.4235622860938,21.3623480307987,39.8105315575448));
#67557=CARTESIAN_POINT('Ctrl Pts',(32.4114245540427,21.4435311672794,39.814784924709));
#67558=CARTESIAN_POINT('Ctrl Pts',(32.3952077562772,21.524073630282,39.8190382918731));
#67559=CARTESIAN_POINT('Ctrl Pts',(32.3750130108635,21.6035424162633,39.8232916590373));
#67560=CARTESIAN_POINT('Ctrl Pts',(32.354967064915,21.6824256582027,39.8275136864274));
#67561=CARTESIAN_POINT('Ctrl Pts',(32.3310017950156,21.7602505621038,39.8317357138175));
#67562=CARTESIAN_POINT('Ctrl Pts',(32.3032659460962,21.8366099638145,39.8359577412075));
#67563=CARTESIAN_POINT('Ctrl Pts',(32.2752212756702,21.9138195801895,39.8402267782588));
#67564=CARTESIAN_POINT('Ctrl Pts',(32.2433217288294,21.9895304069517,39.84449581531));
#67565=CARTESIAN_POINT('Ctrl Pts',(32.2077697744543,22.0633451335318,39.8487648523612));
#67566=CARTESIAN_POINT('Ctrl Pts',(32.1722178200793,22.137159860112,39.8530338894124));
#67567=CARTESIAN_POINT('Ctrl Pts',(32.133013746719,22.209078092168,39.8573029264636));
#67568=CARTESIAN_POINT('Ctrl Pts',(32.0904051145294,22.2787324611306,39.8615719635149));
#67569=CARTESIAN_POINT('Ctrl Pts',(32.0481754335407,22.3477673404405,39.8658030327499));
#67570=CARTESIAN_POINT('Ctrl Pts',(32.0024430523482,22.4148375899673,39.8700341019848));
#67571=CARTESIAN_POINT('Ctrl Pts',(31.9534164190798,22.4795656604793,39.8742651712198));
#67572=CARTESIAN_POINT('Ctrl Pts',(31.9044601265138,22.544200862735,39.8784901699507));
#67573=CARTESIAN_POINT('Ctrl Pts',(31.8522192472137,22.6065001925079,39.8827151686815));
#67574=CARTESIAN_POINT('Ctrl Pts',(31.7969466706598,22.666113115249,39.8869401674123));
#67575=CARTESIAN_POINT('Ctrl Pts',(31.741510079492,22.7259029320507,39.8911777033103));
#67576=CARTESIAN_POINT('Ctrl Pts',(31.6830240213945,22.7829899730464,39.8954152392084));
#67577=CARTESIAN_POINT('Ctrl Pts',(31.6217858087531,22.8370522694052,39.8996527751064));
#67578=CARTESIAN_POINT('Ctrl Pts',(31.5608387187701,22.8908575569659,39.9038701660221));
#67579=CARTESIAN_POINT('Ctrl Pts',(31.4971659294199,22.9416664792799,39.9080875569377));
#67580=CARTESIAN_POINT('Ctrl Pts',(31.4310976595226,22.9891982653595,39.9123049478534));
#67581=CARTESIAN_POINT('Ctrl Pts',(31.3650512297526,23.0367143389,39.91652094463));
#67582=CARTESIAN_POINT('Ctrl Pts',(31.2966112691117,23.0809551561929,39.9207369414066));
#67583=CARTESIAN_POINT('Ctrl Pts',(31.2261395319125,23.1216814318558,39.9249529381832));
#67584=CARTESIAN_POINT('Ctrl Pts',(31.1556694970008,23.1624067237507,39.9291688331199));
#67585=CARTESIAN_POINT('Ctrl Pts',(31.0831681862348,23.1996174111144,39.9333847280565));
#67586=CARTESIAN_POINT('Ctrl Pts',(31.0090234237429,23.2331193385796,39.9376006229931));
#67587=CARTESIAN_POINT('Ctrl Pts',(30.9342196387978,23.2669190419319,39.9418539901575));
#67588=CARTESIAN_POINT('Ctrl Pts',(30.8577434724237,23.2969435128454,39.9461073573218));
#67589=CARTESIAN_POINT('Ctrl Pts',(30.7800136200119,23.3230430479429,39.9503607244862));
#67590=CARTESIAN_POINT('Ctrl Pts',(30.7028564987912,23.3489502757432,39.9545827518761));
#67591=CARTESIAN_POINT('Ctrl Pts',(30.6244645740498,23.370990147871,39.958804779266));
#67592=CARTESIAN_POINT('Ctrl Pts',(30.5452606391552,23.389066990561,39.9630268066559));
#67593=CARTESIAN_POINT('Ctrl Pts',(30.4651748174707,23.4073451077052,39.9672958437075));
#67594=CARTESIAN_POINT('Ctrl Pts',(30.3842592719849,23.4215713116105,39.9715648807591));
#67595=CARTESIAN_POINT('Ctrl Pts',(30.3029576328519,23.4317004179579,39.9758339178106));
#67596=CARTESIAN_POINT('Ctrl Pts',(30.2216559937188,23.4418295243054,39.9801029548622));
#67597=CARTESIAN_POINT('Ctrl Pts',(30.1399687487282,23.4478615618603,39.9843719919138));
#67598=CARTESIAN_POINT('Ctrl Pts',(30.0583388039753,23.4498054685935,39.9886410289654));
#67599=CARTESIAN_POINT('Ctrl Pts',(29.9774348568495,23.4517320866751,39.9928720982004));
#67600=CARTESIAN_POINT('Ctrl Pts',(29.8962835467492,23.4496502773267,39.9971031674354));
#67601=CARTESIAN_POINT('Ctrl Pts',(29.8153151373108,23.4435305914789,40.0013342366704));
#67602=CARTESIAN_POINT('Ctrl Pts',(29.7344628968688,23.437419685818,40.0055592354012));
#67603=CARTESIAN_POINT('Ctrl Pts',(29.6537934956345,23.4272824443422,40.009784234132));
#67604=CARTESIAN_POINT('Ctrl Pts',(29.5737385810179,23.4131414075199,40.0140092328629));
#67605=CARTESIAN_POINT('Ctrl Pts',(29.4934461132292,23.3989584088998,40.0182467687609));
#67606=CARTESIAN_POINT('Ctrl Pts',(29.4137722572628,23.3807478098741,40.0224843046589));
#67607=CARTESIAN_POINT('Ctrl Pts',(29.3351487308337,23.3585849655859,40.026721840557));
#67608=CARTESIAN_POINT('Ctrl Pts',(29.2568989757643,23.3365274820825,40.0309392314726));
#67609=CARTESIAN_POINT('Ctrl Pts',(29.1796900388715,23.3105553671463,40.0351566223883));
#67610=CARTESIAN_POINT('Ctrl Pts',(29.1039368505293,23.2807939587259,40.039374013304));
#67611=CARTESIAN_POINT('Ctrl Pts',(29.0282087038492,23.2510423885071,40.0435900100806));
#67612=CARTESIAN_POINT('Ctrl Pts',(28.9539357824988,23.2175041822141,40.0478060068572));
#67613=CARTESIAN_POINT('Ctrl Pts',(28.8815152446484,23.1803536644421,40.0520220036338));
#67614=CARTESIAN_POINT('Ctrl Pts',(28.8090964561599,23.1432040440634,40.0562378985705));
#67615=CARTESIAN_POINT('Ctrl Pts',(28.7385303754074,23.1024424988996,40.0604537935071));
#67616=CARTESIAN_POINT('Ctrl Pts',(28.6701903633218,23.0582897221231,40.0646696884438));
#67617=CARTESIAN_POINT('Ctrl Pts',(28.6012429232688,23.0137445012918,40.0689230556081));
#67618=CARTESIAN_POINT('Ctrl Pts',(28.534561735099,22.9657477095122,40.0731764227725));
#67619=CARTESIAN_POINT('Ctrl Pts',(28.4704995346241,22.9145700761306,40.0774297899368));
#67620=CARTESIAN_POINT('Ctrl Pts',(28.4069093589788,22.8637695311647,40.0816518173267));
#67621=CARTESIAN_POINT('Ctrl Pts',(28.3459000154409,22.8098352208492,40.0858738447167));
#67622=CARTESIAN_POINT('Ctrl Pts',(28.2877810550468,22.7530706016996,40.0900958721066));
#67623=CARTESIAN_POINT('Ctrl Pts',(28.2290149760035,22.6956739436522,40.0943649091581));
#67624=CARTESIAN_POINT('Ctrl Pts',(28.1732043764096,22.635383916685,40.0986339462097));
#67625=CARTESIAN_POINT('Ctrl Pts',(28.1206276698347,22.572548852853,40.1029029832612));
#67626=CARTESIAN_POINT('Ctrl Pts',(28.0680509632599,22.5097137890209,40.1071720203128));
#67627=CARTESIAN_POINT('Ctrl Pts',(28.0187083899052,22.4443341138468,40.1114410573643));
#67628=CARTESIAN_POINT('Ctrl Pts',(27.9728324872057,22.3767868844056,40.1157100944159));
#67629=CARTESIAN_POINT('Ctrl Pts',(27.9266694884468,22.3088169375408,40.1200058475349));
#67630=CARTESIAN_POINT('Ctrl Pts',(27.8838466951709,22.2384023151295,40.124301600654));
#67631=CARTESIAN_POINT('Ctrl Pts',(27.8446277155084,22.1658990373294,40.1285973537731));
#67632=CARTESIAN_POINT('Ctrl Pts',(27.8054697114269,22.0935084837643,40.132886428084));
#67633=CARTESIAN_POINT('Ctrl Pts',(27.7699045982222,22.0190361163048,40.1371755023949));
#67634=CARTESIAN_POINT('Ctrl Pts',(27.7381530541333,21.9428672459438,40.1414645767059));
#67635=CARTESIAN_POINT('Ctrl Pts',(27.7064501225189,21.8668149921874,40.1457470843278));
#67636=CARTESIAN_POINT('Ctrl Pts',(27.6785493147091,21.7890718124622,40.1500295919497));
#67637=CARTESIAN_POINT('Ctrl Pts',(27.6546249595839,21.7100465969167,40.1543120995716));
#67638=CARTESIAN_POINT('Ctrl Pts',(27.6307223085427,21.6310930727464,40.1585907221189));
#67639=CARTESIAN_POINT('Ctrl Pts',(27.6107890710512,21.5508602491011,40.1628693446662));
#67640=CARTESIAN_POINT('Ctrl Pts',(27.5949508390342,21.4697752476854,40.1671479672134));
#67641=CARTESIAN_POINT('Ctrl Pts',(27.5791219983052,21.3887383256638,40.1714240527492));
#67642=CARTESIAN_POINT('Ctrl Pts',(27.5673834247026,21.3068506668956,40.175700138285));
#67643=CARTESIAN_POINT('Ctrl Pts',(27.5598100877106,21.2245516465335,40.1799762238208));
#67644=CARTESIAN_POINT('Ctrl Pts',(27.5529050286324,21.149514764077,40.1838749838099));
#67645=CARTESIAN_POINT('Ctrl Pts',(27.5494619912402,21.0741363136556,40.1877737437989));
#67646=CARTESIAN_POINT('Ctrl Pts',(27.5495003167103,20.9987541280282,40.1916725037879));
#67647=CARTESIAN_POINT('',(27.5495004369098,20.998536683703,40.9916725037587));
#67648=CARTESIAN_POINT('Ctrl Pts',(27.5495003167105,20.9987541275197,40.1916725038142));
#67649=CARTESIAN_POINT('Ctrl Pts',(27.5495460863282,20.9087301200364,40.1963285375377));
#67650=CARTESIAN_POINT('Ctrl Pts',(27.5545568244828,20.8188767932227,40.2009845712612));
#67651=CARTESIAN_POINT('Ctrl Pts',(27.5644515219164,20.7297152225801,40.2056406049846));
#67652=CARTESIAN_POINT('Ctrl Pts',(27.5743801343139,20.6402480426492,40.2103125976817));
#67653=CARTESIAN_POINT('Ctrl Pts',(27.5892261144754,20.5514776431576,40.2149845903788));
#67654=CARTESIAN_POINT('Ctrl Pts',(27.60885757913,20.4639140245109,40.2196565830759));
#67655=CARTESIAN_POINT('Ctrl Pts',(27.6285833211493,20.3759298938268,40.2243510123647));
#67656=CARTESIAN_POINT('Ctrl Pts',(27.6531404882094,20.2891644297647,40.2290454416536));
#67657=CARTESIAN_POINT('Ctrl Pts',(27.6823468164612,20.2041143481427,40.2337398709425));
#67658=CARTESIAN_POINT('Ctrl Pts',(27.7010927543397,20.1495253723252,40.2367529672504));
#67659=CARTESIAN_POINT('Ctrl Pts',(27.7217530099953,20.0956426438008,40.2397660635584));
#67660=CARTESIAN_POINT('Ctrl Pts',(27.7442693557824,20.0425922964913,40.2427791598663));
#67661=CARTESIAN_POINT('Ctrl Pts',(27.7758874018746,19.9680976008471,40.2470102291013));
#67662=CARTESIAN_POINT('Ctrl Pts',(27.8112589881166,19.8950310561913,40.2512412983363));
#67663=CARTESIAN_POINT('Ctrl Pts',(27.8502334563358,19.8237967617192,40.2554723675714));
#67664=CARTESIAN_POINT('Ctrl Pts',(27.8891520061431,19.752664670274,40.2596973663022));
#67665=CARTESIAN_POINT('Ctrl Pts',(27.9316629502183,19.6833600124647,40.263922365033));
#67666=CARTESIAN_POINT('Ctrl Pts',(27.9775676993811,19.6162667022098,40.2681473637638));
#67667=CARTESIAN_POINT('Ctrl Pts',(28.0236086652751,19.548974300759,40.2723848996619));
#67668=CARTESIAN_POINT('Ctrl Pts',(28.0730634199664,19.4839068243992,40.2766224355599));
#67669=CARTESIAN_POINT('Ctrl Pts',(28.1256852334135,19.4214264648881,40.280859971458));
#67670=CARTESIAN_POINT('Ctrl Pts',(28.178056886029,19.3592431331241,40.2850773623736));
#67671=CARTESIAN_POINT('Ctrl Pts',(28.2335652563088,19.299622737962,40.2892947532893));
#67672=CARTESIAN_POINT('Ctrl Pts',(28.2919250068862,19.2428915605748,40.293512144205));
#67673=CARTESIAN_POINT('Ctrl Pts',(28.3502654655344,19.1861791367608,40.2977281409816));
#67674=CARTESIAN_POINT('Ctrl Pts',(28.411455099526,19.132354357901,40.3019441377583));
#67675=CARTESIAN_POINT('Ctrl Pts',(28.4751712778851,19.0817071083347,40.3061601345349));
#67676=CARTESIAN_POINT('Ctrl Pts',(28.5388859171412,19.0310610821835,40.3103760294716));
#67677=CARTESIAN_POINT('Ctrl Pts',(28.6051266147554,18.9835927211783,40.3145919244082));
#67678=CARTESIAN_POINT('Ctrl Pts',(28.6735383164339,18.9395511042418,40.3188078193449));
#67679=CARTESIAN_POINT('Ctrl Pts',(28.7425580832798,18.895118031275,40.3230611865092));
#67680=CARTESIAN_POINT('Ctrl Pts',(28.8137872449956,18.8541731976804,40.3273145536736));
#67681=CARTESIAN_POINT('Ctrl Pts',(28.8868336744412,18.8169262537326,40.3315679208379));
#67682=CARTESIAN_POINT('Ctrl Pts',(28.9593418812197,18.7799537537195,40.3357899482278));
#67683=CARTESIAN_POINT('Ctrl Pts',(29.0336402106091,18.7466249661912,40.3400119756178));
#67684=CARTESIAN_POINT('Ctrl Pts',(29.1093245362922,18.7170967019278,40.3442340030077));
#67685=CARTESIAN_POINT('Ctrl Pts',(29.1858515600938,18.6872396587196,40.3485030400592));
#67686=CARTESIAN_POINT('Ctrl Pts',(29.263795172758,18.6612684511329,40.3527720771108));
#67687=CARTESIAN_POINT('Ctrl Pts',(29.3427232126071,18.6392930137871,40.3570411141623));
#67688=CARTESIAN_POINT('Ctrl Pts',(29.4216512524562,18.6173175764413,40.3613101512138));
#67689=CARTESIAN_POINT('Ctrl Pts',(29.5015632327741,18.59933795262,40.3655791882654));
#67690=CARTESIAN_POINT('Ctrl Pts',(29.5820197486823,18.5854104366356,40.3698482253169));
#67691=CARTESIAN_POINT('Ctrl Pts',(29.6617607031666,18.571606788719,40.3740792945519));
#67692=CARTESIAN_POINT('Ctrl Pts',(29.7423358224686,18.5617316071648,40.3783103637869));
#67693=CARTESIAN_POINT('Ctrl Pts',(29.8233238520227,18.5558772967103,40.382541433022));
#67694=CARTESIAN_POINT('Ctrl Pts',(29.9041956844304,18.5500313856968,40.3867664317528));
#67695=CARTESIAN_POINT('Ctrl Pts',(29.9854787906683,18.5481949215412,40.3909914304837));
#67696=CARTESIAN_POINT('Ctrl Pts',(30.0667429017055,18.5504090882207,40.3952164292145));
#67697=CARTESIAN_POINT('Ctrl Pts',(30.1482481540567,18.552629825169,40.3994539651126));
#67698=CARTESIAN_POINT('Ctrl Pts',(30.2297338316988,18.558925345847,40.4036915010106));
#67699=CARTESIAN_POINT('Ctrl Pts',(30.3107618289751,18.5692846041439,40.4079290369086));
#67700=CARTESIAN_POINT('Ctrl Pts',(30.3914046241873,18.5795946151705,40.4121464278243));
#67701=CARTESIAN_POINT('Ctrl Pts',(30.4715936153757,18.5939297601873,40.41636381874));
#67702=CARTESIAN_POINT('Ctrl Pts',(30.5508999510761,18.6122270849379,40.4205812096557));
#67703=CARTESIAN_POINT('Ctrl Pts',(30.6301800705538,18.6305183611585,40.4247972064324));
#67704=CARTESIAN_POINT('Ctrl Pts',(30.708577661269,18.6527691116501,40.429013203209));
#67705=CARTESIAN_POINT('Ctrl Pts',(30.7856742466026,18.6788653145013,40.4332291999857));
#67706=CARTESIAN_POINT('Ctrl Pts',(30.8627689696215,18.7049608869828,40.4374450949223));
#67707=CARTESIAN_POINT('Ctrl Pts',(30.9385623096799,18.7349015770176,40.441660989859));
#67708=CARTESIAN_POINT('Ctrl Pts',(31.0126525095517,18.7685239985833,40.4458768847957));
#67709=CARTESIAN_POINT('Ctrl Pts',(31.0874012469051,18.8024452670257,40.45013025196));
#67710=CARTESIAN_POINT('Ctrl Pts',(31.1604159714467,18.8401138597372,40.4543836191243));
#67711=CARTESIAN_POINT('Ctrl Pts',(31.2313079683454,18.8813138653663,40.4586369862886));
#67712=CARTESIAN_POINT('Ctrl Pts',(31.3016776169255,18.9222103000056,40.4628590136786));
#67713=CARTESIAN_POINT('Ctrl Pts',(31.3699553554139,18.9665859718893,40.4670810410685));
#67714=CARTESIAN_POINT('Ctrl Pts',(31.4357903712559,19.014186247452,40.4713030684585));
#67715=CARTESIAN_POINT('Ctrl Pts',(31.5023584192471,19.0623165226182,40.4755721055099));
#67716=CARTESIAN_POINT('Ctrl Pts',(31.566428629876,19.1137433491633,40.4798411425614));
#67717=CARTESIAN_POINT('Ctrl Pts',(31.6276743899694,19.1681631267393,40.4841101796129));
#67718=CARTESIAN_POINT('Ctrl Pts',(31.6889201500628,19.2225829043152,40.4883792166644));
#67719=CARTESIAN_POINT('Ctrl Pts',(31.7473411594526,19.2799952473507,40.4926482537159));
#67720=CARTESIAN_POINT('Ctrl Pts',(31.8026519579067,19.3400613961188,40.4969172907674));
#67721=CARTESIAN_POINT('Ctrl Pts',(31.8574708350635,19.3995933306167,40.5011483600024));
#67722=CARTESIAN_POINT('Ctrl Pts',(31.9094403829716,19.461955459761,40.5053794292374));
#67723=CARTESIAN_POINT('Ctrl Pts',(31.9582546318543,19.5268438484597,40.5096104984724));
#67724=CARTESIAN_POINT('Ctrl Pts',(32.0069988447519,19.5916391388863,40.5138354972032));
#67725=CARTESIAN_POINT('Ctrl Pts',(32.0525964724986,19.6589531218623,40.518060495934));
#67726=CARTESIAN_POINT('Ctrl Pts',(32.094779704901,19.7284465257274,40.5222854946648));
#67727=CARTESIAN_POINT('Ctrl Pts',(32.1370881108886,19.7981461427727,40.5265230305629));
#67728=CARTESIAN_POINT('Ctrl Pts',(32.1759615096516,19.8700377842204,40.5307605664609));
#67729=CARTESIAN_POINT('Ctrl Pts',(32.2111717371794,19.9437472846429,40.534998102359));
#67730=CARTESIAN_POINT('Ctrl Pts',(32.2462145774731,20.0171063746802,40.5392154932746));
#67731=CARTESIAN_POINT('Ctrl Pts',(32.2776287894671,20.0922656587053,40.5434328841903));
#67732=CARTESIAN_POINT('Ctrl Pts',(32.3052348477571,20.1688306149247,40.547650275106));
#67733=CARTESIAN_POINT('Ctrl Pts',(32.3328317803376,20.2453702611367,40.5518662718826));
#67734=CARTESIAN_POINT('Ctrl Pts',(32.3566229015349,20.3233142197191,40.5560822686592));
#67735=CARTESIAN_POINT('Ctrl Pts',(32.3764772255902,20.4022490098284,40.5602982654358));
#67736=CARTESIAN_POINT('Ctrl Pts',(32.3963310700522,20.4811818932199,40.5645141603725));
#67737=CARTESIAN_POINT('Ctrl Pts',(32.4122481940969,20.5611051093655,40.5687300553092));
#67738=CARTESIAN_POINT('Ctrl Pts',(32.4241481586286,20.6415924735481,40.5729459502458));
#67739=CARTESIAN_POINT('Ctrl Pts',(32.4361538938655,20.7227952352634,40.5771993174102));
#67740=CARTESIAN_POINT('Ctrl Pts',(32.4440706137376,20.8045717503721,40.5814526845745));
#67741=CARTESIAN_POINT('Ctrl Pts',(32.4478690895806,20.8864783268449,40.5857060517388));
#67742=CARTESIAN_POINT('Ctrl Pts',(32.4516395773916,20.9677813970766,40.5899280791288));
#67743=CARTESIAN_POINT('Ctrl Pts',(32.4513523716402,21.0492121488906,40.5941501065187));
#67744=CARTESIAN_POINT('Ctrl Pts',(32.4470313278271,21.1303377559753,40.5983721339086));
#67745=CARTESIAN_POINT('Ctrl Pts',(32.4426621718658,21.2123666464792,40.6026411709602));
#67746=CARTESIAN_POINT('Ctrl Pts',(32.4341688424918,21.2940830691546,40.6069102080117));
#67747=CARTESIAN_POINT('Ctrl Pts',(32.4216294620063,21.3750479952526,40.6111792450632));
#67748=CARTESIAN_POINT('Ctrl Pts',(32.4090900815209,21.4560129213506,40.6154482821148));
#67749=CARTESIAN_POINT('Ctrl Pts',(32.3925048112666,21.5362258896395,40.6197173191663));
#67750=CARTESIAN_POINT('Ctrl Pts',(32.3720036253616,21.6152633999123,40.6239863562179));
#67751=CARTESIAN_POINT('Ctrl Pts',(32.3516847722065,21.6935979690641,40.6282174254529));
#67752=CARTESIAN_POINT('Ctrl Pts',(32.3274431624911,21.7710719222324,40.6324484946878));
#67753=CARTESIAN_POINT('Ctrl Pts',(32.2993683882583,21.8472633976979,40.6366795639228));
#67754=CARTESIAN_POINT('Ctrl Pts',(32.271333894159,21.9233455578475,40.6409045626537));
#67755=CARTESIAN_POINT('Ctrl Pts',(32.2394773175561,21.998148462118,40.6451295613845));
#67756=CARTESIAN_POINT('Ctrl Pts',(32.2039386288593,22.0712631657168,40.6493545601153));
#67757=CARTESIAN_POINT('Ctrl Pts',(32.1682944834485,22.1445948282604,40.6535920960133));
#67758=CARTESIAN_POINT('Ctrl Pts',(32.1289464627612,22.2162277990869,40.6578296319114));
#67759=CARTESIAN_POINT('Ctrl Pts',(32.0860853491656,22.2857675396418,40.6620671678094));
#67760=CARTESIAN_POINT('Ctrl Pts',(32.0434279946412,22.3549766925905,40.6662845587251));
#67761=CARTESIAN_POINT('Ctrl Pts',(31.997291114425,22.4221120705536,40.6705019496407));
#67762=CARTESIAN_POINT('Ctrl Pts',(31.9479089595562,22.4868089774012,40.6747193405564));
#67763=CARTESIAN_POINT('Ctrl Pts',(31.898543128901,22.5514844974516,40.678935337333));
#67764=CARTESIAN_POINT('Ctrl Pts',(31.8459344358771,22.613722777839,40.6831513341096));
#67765=CARTESIAN_POINT('Ctrl Pts',(31.7903593722719,22.6731896390183,40.6873673308862));
#67766=CARTESIAN_POINT('Ctrl Pts',(31.734785651116,22.7326550637395,40.6915832258228));
#67767=CARTESIAN_POINT('Ctrl Pts',(31.6762460201253,22.7893488634034,40.6957991207595));
#67768=CARTESIAN_POINT('Ctrl Pts',(31.6150550428373,22.8429724519389,40.7000150156961));
#67769=CARTESIAN_POINT('Ctrl Pts',(31.553320180498,22.8970726641451,40.7042683828605));
#67770=CARTESIAN_POINT('Ctrl Pts',(31.48888695479,22.9480474844173,40.7085217500248));
#67771=CARTESIAN_POINT('Ctrl Pts',(31.4221123975052,22.9956318745856,40.7127751171892));
#67772=CARTESIAN_POINT('Ctrl Pts',(31.3558298503109,23.0428656521693,40.7169971445791));
#67773=CARTESIAN_POINT('Ctrl Pts',(31.2872407889696,23.0867585957071,40.721219171969));
#67774=CARTESIAN_POINT('Ctrl Pts',(31.2167218847191,23.1270961673713,40.7254411993589));
#67775=CARTESIAN_POINT('Ctrl Pts',(31.1454177961193,23.167882872928,40.7297102364105));
#67776=CARTESIAN_POINT('Ctrl Pts',(31.0721410583789,23.2050343208802,40.7339792734621));
#67777=CARTESIAN_POINT('Ctrl Pts',(30.9973029670206,23.2383782169178,40.7382483105136));
#67778=CARTESIAN_POINT('Ctrl Pts',(30.9224648756623,23.2717221129554,40.7425173475652));
#67779=CARTESIAN_POINT('Ctrl Pts',(30.846065905745,23.3012583426877,40.7467863846168));
#67780=CARTESIAN_POINT('Ctrl Pts',(30.7685324057423,23.3268666036806,40.7510554216683));
#67781=CARTESIAN_POINT('Ctrl Pts',(30.691688470543,23.3522471107934,40.7552864909035));
#67782=CARTESIAN_POINT('Ctrl Pts',(30.6134417082201,23.3738645400482,40.7595175601386));
#67783=CARTESIAN_POINT('Ctrl Pts',(30.5341952037729,23.3915655404496,40.7637486293738));
#67784=CARTESIAN_POINT('Ctrl Pts',(30.4550623978283,23.4092411444344,40.7679736281047));
#67785=CARTESIAN_POINT('Ctrl Pts',(30.3749331484721,23.4230113789361,40.7721986268357));
#67786=CARTESIAN_POINT('Ctrl Pts',(30.294226989835,23.4327722311085,40.7764236255667));
#67787=CARTESIAN_POINT('Ctrl Pts',(30.2132813455421,23.442562047416,40.7806611614647));
#67788=CARTESIAN_POINT('Ctrl Pts',(30.1317558131787,23.448318505887,40.7848986973627));
#67789=CARTESIAN_POINT('Ctrl Pts',(30.050085359408,23.4499881033942,40.7891362332607));
#67790=CARTESIAN_POINT('Ctrl Pts',(29.9688031618969,23.4516497637386,40.7933536241765));
#67791=CARTESIAN_POINT('Ctrl Pts',(29.8873778859494,23.4492633170818,40.7975710150923));
#67792=CARTESIAN_POINT('Ctrl Pts',(29.8062429784239,23.4428279650008,40.8017884060081));
#67793=CARTESIAN_POINT('Ctrl Pts',(29.7251348915903,23.4363947402483,40.8060044027848));
#67794=CARTESIAN_POINT('Ctrl Pts',(29.6443174457049,23.4259153047548,40.8102203995616));
#67795=CARTESIAN_POINT('Ctrl Pts',(29.5642213357481,23.4114408982562,40.8144363963384));
#67796=CARTESIAN_POINT('Ctrl Pts',(29.4841271605615,23.3969668413957,40.8186522912752));
#67797=CARTESIAN_POINT('Ctrl Pts',(29.4047547440148,23.3784980891681,40.822868186212));
#67798=CARTESIAN_POINT('Ctrl Pts',(29.3265255031183,23.3561371674947,40.8270840811488));
#67799=CARTESIAN_POINT('Ctrl Pts',(29.2476009356196,23.3335774947723,40.8313374483129));
#67800=CARTESIAN_POINT('Ctrl Pts',(29.1698404344567,23.3070562328267,40.8355908154771));
#67801=CARTESIAN_POINT('Ctrl Pts',(29.0936602405861,23.2767297798609,40.8398441826413));
#67802=CARTESIAN_POINT('Ctrl Pts',(29.0180413596646,23.2466267790798,40.8440662100313));
#67803=CARTESIAN_POINT('Ctrl Pts',(28.943979976671,23.2127747277735,40.8482882374214));
#67804=CARTESIAN_POINT('Ctrl Pts',(28.8718605369971,23.1753738993597,40.8525102648114));
#67805=CARTESIAN_POINT('Ctrl Pts',(28.7989380920113,23.1375566358762,40.8567793018627));
#67806=CARTESIAN_POINT('Ctrl Pts',(28.7280015249602,23.0961113245285,40.8610483389139));
#67807=CARTESIAN_POINT('Ctrl Pts',(28.6594185461734,23.0512902319409,40.8653173759651));
#67808=CARTESIAN_POINT('Ctrl Pts',(28.5908355673866,23.0064691393533,40.8695864130163));
#67809=CARTESIAN_POINT('Ctrl Pts',(28.5246065304716,22.9582726027613,40.8738554500675));
#67810=CARTESIAN_POINT('Ctrl Pts',(28.4610636109115,22.9069937179601,40.8781244871188));
#67811=CARTESIAN_POINT('Ctrl Pts',(28.3988991871278,22.8568272737991,40.8823009119704));
#67812=CARTESIAN_POINT('Ctrl Pts',(28.3390590737905,22.8035117847631,40.8864773368221));
#67813=CARTESIAN_POINT('Ctrl Pts',(28.2818859516553,22.7472934404045,40.8906537616738));
#67814=CARTESIAN_POINT('Ctrl Pts',(28.2242653283127,22.690635068004,40.8948628759274));
#67815=CARTESIAN_POINT('Ctrl Pts',(28.1693540614958,22.6310284373932,40.8990719901809));
#67816=CARTESIAN_POINT('Ctrl Pts',(28.1174713076324,22.568768935316,40.9032811044344));
#67817=CARTESIAN_POINT('Ctrl Pts',(28.0661251752047,22.5071533810039,40.9074466839723));
#67818=CARTESIAN_POINT('Ctrl Pts',(28.0177455279077,22.4429399392236,40.9116122635103));
#67819=CARTESIAN_POINT('Ctrl Pts',(27.9726054180359,22.3764524906521,40.9157778430482));
#67820=CARTESIAN_POINT('Ctrl Pts',(27.9274926432361,22.3100053042598,40.9199409000753));
#67821=CARTESIAN_POINT('Ctrl Pts',(27.8856157817235,22.2412872376611,40.9241039571024));
#67822=CARTESIAN_POINT('Ctrl Pts',(27.8472064165828,22.1706536794449,40.9282670141295));
#67823=CARTESIAN_POINT('Ctrl Pts',(27.8088078168249,22.1000399184133,40.9324289043343));
#67824=CARTESIAN_POINT('Ctrl Pts',(27.7738750118051,22.0275121516492,40.9365907945391));
#67825=CARTESIAN_POINT('Ctrl Pts',(27.7425943696033,21.9534516609945,40.9407526847439));
#67826=CARTESIAN_POINT('Ctrl Pts',(27.7107017166422,21.8779421650148,40.9449960029952));
#67827=CARTESIAN_POINT('Ctrl Pts',(27.6826058921223,21.8008397889873,40.9492393212464));
#67828=CARTESIAN_POINT('Ctrl Pts',(27.6584528198875,21.7225697567066,40.9534826394976));
#67829=CARTESIAN_POINT('Ctrl Pts',(27.6347410320592,21.645729743117,40.9576484309581));
#67830=CARTESIAN_POINT('Ctrl Pts',(27.6148291982902,21.5677648703724,40.9618142224187));
#67831=CARTESIAN_POINT('Ctrl Pts',(27.5988043145566,21.4890905133083,40.9659800138792));
#67832=CARTESIAN_POINT('Ctrl Pts',(27.5823320880484,21.4082199215771,40.9702620955257));
#67833=CARTESIAN_POINT('Ctrl Pts',(27.5699671547341,21.3266001775221,40.9745441771723));
#67834=CARTESIAN_POINT('Ctrl Pts',(27.5617470040674,21.2446887366138,40.9788262588189));
#67835=CARTESIAN_POINT('Ctrl Pts',(27.5535268534007,21.1627772957055,40.9831083404655));
#67836=CARTESIAN_POINT('Ctrl Pts',(27.5494514478907,21.0805747024057,40.9873904221121));
#67837=CARTESIAN_POINT('Ctrl Pts',(27.5495004369098,20.998536683703,40.9916725037586));
#67838=CARTESIAN_POINT('',(27.5495009231109,21.0021270086603,41.7916725038169));
#67839=CARTESIAN_POINT('Ctrl Pts',(27.5495004369101,20.9985366831405,40.991672503788));
#67840=CARTESIAN_POINT('Ctrl Pts',(27.5495519993063,20.912189267378,40.9961795200484));
#67841=CARTESIAN_POINT('Ctrl Pts',(27.5541671351712,20.8259795206028,41.0006865363089));
#67842=CARTESIAN_POINT('Ctrl Pts',(27.5633043849036,20.7402602660931,41.0051935525694));
#67843=CARTESIAN_POINT('Ctrl Pts',(27.5718821964757,20.6597892671807,41.0094246218043));
#67844=CARTESIAN_POINT('Ctrl Pts',(27.5844666777454,20.5795926345089,41.0136556910392));
#67845=CARTESIAN_POINT('Ctrl Pts',(27.6010312510458,20.5001008186231,41.0178867602741));
#67846=CARTESIAN_POINT('Ctrl Pts',(27.6175720584124,20.4207230531991,41.0221117590048));
#67847=CARTESIAN_POINT('Ctrl Pts',(27.6380815224783,20.3420485475221,41.0263367577355));
#67848=CARTESIAN_POINT('Ctrl Pts',(27.6624813353646,20.2645023844489,41.0305617564662));
#67849=CARTESIAN_POINT('Ctrl Pts',(27.6869535517137,20.1867261126142,41.0347992923643));
#67850=CARTESIAN_POINT('Ctrl Pts',(27.7153391862825,20.1100853598019,41.0390368282624));
#67851=CARTESIAN_POINT('Ctrl Pts',(27.7475075530817,20.0349984318273,41.0432743641604));
#67852=CARTESIAN_POINT('Ctrl Pts',(27.7795229934625,19.9602684624459,41.047491755076));
#67853=CARTESIAN_POINT('Ctrl Pts',(27.8152851026761,19.8870780106468,41.0517091459915));
#67854=CARTESIAN_POINT('Ctrl Pts',(27.8546158099747,19.815822256927,41.055926536907));
#67855=CARTESIAN_POINT('Ctrl Pts',(27.8939335157574,19.7445900581565,41.0601425336835));
#67856=CARTESIAN_POINT('Ctrl Pts',(27.9368172524685,19.67529169416,41.06435853046));
#67857=CARTESIAN_POINT('Ctrl Pts',(27.9830426800296,19.6082983727042,41.0685745272364));
#67858=CARTESIAN_POINT('Ctrl Pts',(28.0292669909874,19.5413066695127,41.072790422173));
#67859=CARTESIAN_POINT('Ctrl Pts',(28.0788325673311,19.4766202802318,41.0770063171095));
#67860=CARTESIAN_POINT('Ctrl Pts',(28.1314721766981,19.4145808051034,41.081222212046));
#67861=CARTESIAN_POINT('Ctrl Pts',(28.1845796638163,19.3519899031984,41.0854755792104));
#67862=CARTESIAN_POINT('Ctrl Pts',(28.240815804874,19.2920935818062,41.0897289463749));
#67863=CARTESIAN_POINT('Ctrl Pts',(28.2998664273511,19.2352065035387,41.0939823135394));
#67864=CARTESIAN_POINT('Ctrl Pts',(28.3584819514384,19.1787385821762,41.0982043409291));
#67865=CARTESIAN_POINT('Ctrl Pts',(28.4198702243352,19.1252359674877,41.1024263683189));
#67866=CARTESIAN_POINT('Ctrl Pts',(28.4836902208801,19.0749662590631,41.1066483957087));
#67867=CARTESIAN_POINT('Ctrl Pts',(28.5482208135895,19.0241368285462,41.1109174327605));
#67868=CARTESIAN_POINT('Ctrl Pts',(28.6152372189881,18.9766130262241,41.1151864698123));
#67869=CARTESIAN_POINT('Ctrl Pts',(28.6843579516364,18.9326257594287,41.1194555068642));
#67870=CARTESIAN_POINT('Ctrl Pts',(28.7534786842848,18.8886384926333,41.123724543916));
#67871=CARTESIAN_POINT('Ctrl Pts',(28.8247032911121,18.8481879443753,41.1279935809678));
#67872=CARTESIAN_POINT('Ctrl Pts',(28.8976277513153,18.8114558091439,41.1322626180197));
#67873=CARTESIAN_POINT('Ctrl Pts',(28.9699036384469,18.7750503609214,41.1364936872557));
#67874=CARTESIAN_POINT('Ctrl Pts',(29.0441205094844,18.742160771114,41.1407247564917));
#67875=CARTESIAN_POINT('Ctrl Pts',(29.1199022143788,18.712998002243,41.1449558257277));
#67876=CARTESIAN_POINT('Ctrl Pts',(29.1955751918736,18.6838770745001,41.1491808244596));
#67877=CARTESIAN_POINT('Ctrl Pts',(29.2728081139551,18.658472513689,41.1534058231914));
#67878=CARTESIAN_POINT('Ctrl Pts',(29.3512013044756,18.636948899688,41.1576308219233));
#67879=CARTESIAN_POINT('Ctrl Pts',(29.4298271171814,18.6153614170003,41.161868357821));
#67880=CARTESIAN_POINT('Ctrl Pts',(29.5096196706376,18.5976781578755,41.1661058937188));
#67881=CARTESIAN_POINT('Ctrl Pts',(29.5901565958493,18.5840160112132,41.1703434296166));
#67882=CARTESIAN_POINT('Ctrl Pts',(29.6703106535468,18.5704188135431,41.1745608205333));
#67883=CARTESIAN_POINT('Ctrl Pts',(29.7512015607937,18.560804666775,41.17877821145));
#67884=CARTESIAN_POINT('Ctrl Pts',(29.8324007009626,18.5552381046486,41.1829956023667));
#67885=CARTESIAN_POINT('Ctrl Pts',(29.9135729992062,18.5496733826555,41.1872115991444));
#67886=CARTESIAN_POINT('Ctrl Pts',(29.9950528645208,18.5481536199984,41.191427595922));
#67887=CARTESIAN_POINT('Ctrl Pts',(30.0764067493481,18.5506914733635,41.1956435926997));
#67888=CARTESIAN_POINT('Ctrl Pts',(30.1577586690228,18.5532292654253,41.1998594876374));
#67889=CARTESIAN_POINT('Ctrl Pts',(30.238984149559,18.5598244630332,41.2040753825751));
#67890=CARTESIAN_POINT('Ctrl Pts',(30.3196512781898,18.57043762987,41.2082912775127));
#67891=CARTESIAN_POINT('Ctrl Pts',(30.4010354021145,18.5811451299354,41.2125446446759));
#67892=CARTESIAN_POINT('Ctrl Pts',(30.4818507196718,18.5959423364578,41.216798011839));
#67893=CARTESIAN_POINT('Ctrl Pts',(30.561662515251,18.614735765379,41.2210513790021));
#67894=CARTESIAN_POINT('Ctrl Pts',(30.6408862394515,18.6333907200613,41.2252734063931));
#67895=CARTESIAN_POINT('Ctrl Pts',(30.719120746844,18.6559830126456,41.229495433784));
#67896=CARTESIAN_POINT('Ctrl Pts',(30.7959563192517,18.682371084957,41.233717461175));
#67897=CARTESIAN_POINT('Ctrl Pts',(30.8736474081375,18.709052972099,41.2379864982242));
#67898=CARTESIAN_POINT('Ctrl Pts',(30.9499077629167,18.7396155089754,41.2422555352734));
#67899=CARTESIAN_POINT('Ctrl Pts',(31.0243365722403,18.773863248412,41.2465245723226));
#67900=CARTESIAN_POINT('Ctrl Pts',(31.0987653815639,18.8081109878485,41.2507936093719));
#67901=CARTESIAN_POINT('Ctrl Pts',(31.171362246074,18.846043648279,41.2550626464211));
#67902=CARTESIAN_POINT('Ctrl Pts',(31.2417554984415,18.8874201714277,41.2593316834703));
#67903=CARTESIAN_POINT('Ctrl Pts',(31.3115226897067,18.9284287014689,41.2635627527037));
#67904=CARTESIAN_POINT('Ctrl Pts',(31.3793871825405,18.9729739556384,41.2677938219371));
#67905=CARTESIAN_POINT('Ctrl Pts',(31.444967818672,19.0208541607546,41.2720248911705));
#67906=CARTESIAN_POINT('Ctrl Pts',(31.5104543633331,19.0686656700002,41.2762498898998));
#67907=CARTESIAN_POINT('Ctrl Pts',(31.5736631867936,19.1198023553884,41.280474888629));
#67908=CARTESIAN_POINT('Ctrl Pts',(31.6342393593733,19.1740175339628,41.2846998873582));
#67909=CARTESIAN_POINT('Ctrl Pts',(31.6949952843682,19.2283935894773,41.2889374232567));
#67910=CARTESIAN_POINT('Ctrl Pts',(31.7531025048827,19.2858661931019,41.2931749591551));
#67911=CARTESIAN_POINT('Ctrl Pts',(31.8082338709465,19.3461437432589,41.2974124950535));
#67912=CARTESIAN_POINT('Ctrl Pts',(31.8631031458958,19.4061347376594,41.3016298859676));
#67913=CARTESIAN_POINT('Ctrl Pts',(31.9150244759364,19.468903728195,41.3058472768817));
#67914=CARTESIAN_POINT('Ctrl Pts',(31.963711323602,19.5341254871043,41.3100646677958));
#67915=CARTESIAN_POINT('Ctrl Pts',(32.0123820769012,19.5993256857168,41.3142806645709));
#67916=CARTESIAN_POINT('Ctrl Pts',(32.057820193218,19.6669766702517,41.3184966613459));
#67917=CARTESIAN_POINT('Ctrl Pts',(32.0997800594278,19.7367209524301,41.322712658121));
#67918=CARTESIAN_POINT('Ctrl Pts',(32.1417389120718,19.8064635498931,41.3269285530561));
#67919=CARTESIAN_POINT('Ctrl Pts',(32.1802194429077,19.8782989454798,41.3311444479912));
#67920=CARTESIAN_POINT('Ctrl Pts',(32.2150207031626,19.9518427911037,41.3353603429263));
#67921=CARTESIAN_POINT('Ctrl Pts',(32.2501312882196,20.0260403180981,41.3396137100925));
#67922=CARTESIAN_POINT('Ctrl Pts',(32.2814966494339,20.1019763898893,41.3438670772587));
#67923=CARTESIAN_POINT('Ctrl Pts',(32.3089597399857,20.1792350098078,41.3481204444249));
#67924=CARTESIAN_POINT('Ctrl Pts',(32.3362204762329,20.2559243706229,41.3523424718133));
#67925=CARTESIAN_POINT('Ctrl Pts',(32.3596361808314,20.333916386892,41.3565644992017));
#67926=CARTESIAN_POINT('Ctrl Pts',(32.3791037561101,20.4127900139962,41.3607865265902));
#67927=CARTESIAN_POINT('Ctrl Pts',(32.3987880908128,20.4925418502114,41.3650555636453));
#67928=CARTESIAN_POINT('Ctrl Pts',(32.414435737801,20.5731945720105,41.3693246007004));
#67929=CARTESIAN_POINT('Ctrl Pts',(32.4259937144277,20.65430541289,41.3735936377554));
#67930=CARTESIAN_POINT('Ctrl Pts',(32.4375516910545,20.7354162537694,41.3778626748105));
#67931=CARTESIAN_POINT('Ctrl Pts',(32.4450200174982,20.8169847255092,41.3821317118656));
#67932=CARTESIAN_POINT('Ctrl Pts',(32.4483998377637,20.8985678333135,41.3864007489207));
#67933=CARTESIAN_POINT('Ctrl Pts',(32.4517495986954,20.9794253599701,41.3906318181552));
#67934=CARTESIAN_POINT('Ctrl Pts',(32.4510959048197,21.0606007364284,41.3948628873896));
#67935=CARTESIAN_POINT('Ctrl Pts',(32.4464017414766,21.1416642837855,41.3990939566241));
#67936=CARTESIAN_POINT('Ctrl Pts',(32.4417143130594,21.222611525647,41.4033189553543));
#67937=CARTESIAN_POINT('Ctrl Pts',(32.4329979551542,21.3034467968029,41.4075439540846));
#67938=CARTESIAN_POINT('Ctrl Pts',(32.4202676102448,21.3837381200763,41.4117689528148));
#67939=CARTESIAN_POINT('Ctrl Pts',(32.4074994895911,21.4642676980495,41.416006488713));
#67940=CARTESIAN_POINT('Ctrl Pts',(32.3906935079778,21.5442496224051,41.4202440246112));
#67941=CARTESIAN_POINT('Ctrl Pts',(32.3699174131512,21.6232509164394,41.4244815605094));
#67942=CARTESIAN_POINT('Ctrl Pts',(32.3492400865923,21.7018766432162,41.4286989514244));
#67943=CARTESIAN_POINT('Ctrl Pts',(32.3246304221739,21.7795305877749,41.4329163423395));
#67944=CARTESIAN_POINT('Ctrl Pts',(32.2962064380711,21.8557956787463,41.4371337332545));
#67945=CARTESIAN_POINT('Ctrl Pts',(32.2677918500587,21.9320355588364,41.4413497300305));
#67946=CARTESIAN_POINT('Ctrl Pts',(32.2355656085661,22.0068870617242,41.4455657268065));
#67947=CARTESIAN_POINT('Ctrl Pts',(32.1996950235204,22.079950023612,41.4497817235825));
#67948=CARTESIAN_POINT('Ctrl Pts',(32.1638253049505,22.1530112206193,41.4539976185185));
#67949=CARTESIAN_POINT('Ctrl Pts',(32.1243116237569,22.2242835456374,41.4582135134545));
#67950=CARTESIAN_POINT('Ctrl Pts',(32.0813680699598,22.2933898126056,41.4624294083905));
#67951=CARTESIAN_POINT('Ctrl Pts',(32.0380428200558,22.3631103182832,41.4666827755556));
#67952=CARTESIAN_POINT('Ctrl Pts',(31.9912266605584,22.4306256505362,41.4709361427207));
#67953=CARTESIAN_POINT('Ctrl Pts',(31.9411840727999,22.4955783648837,41.4751895098857));
#67954=CARTESIAN_POINT('Ctrl Pts',(31.8915102101996,22.560052492872,41.479411537275));
#67955=CARTESIAN_POINT('Ctrl Pts',(31.8386576596229,22.6220013243684,41.4836335646642));
#67956=CARTESIAN_POINT('Ctrl Pts',(31.7829243843073,22.6811100171739,41.4878555920535));
#67957=CARTESIAN_POINT('Ctrl Pts',(31.7265705534414,22.7408768487159,41.4921246291065));
#67958=CARTESIAN_POINT('Ctrl Pts',(31.6672718021908,22.7977395648272,41.4963936661594));
#67959=CARTESIAN_POINT('Ctrl Pts',(31.6053715102256,22.8514136664063,41.5006627032124));
#67960=CARTESIAN_POINT('Ctrl Pts',(31.5434712182605,22.9050877679853,41.5049317402654));
#67961=CARTESIAN_POINT('Ctrl Pts',(31.4789698068114,22.9555730073813,41.5092007773183));
#67962=CARTESIAN_POINT('Ctrl Pts',(31.4122401832769,23.0026302491319,41.5134698143713));
#67963=CARTESIAN_POINT('Ctrl Pts',(31.3461040372992,23.0492689748563,41.5177008836141));
#67964=CARTESIAN_POINT('Ctrl Pts',(31.277530958774,23.0927155165667,41.5219319528568));
#67965=CARTESIAN_POINT('Ctrl Pts',(31.2068619831371,23.1327058877535,41.5261630220996));
#67966=CARTESIAN_POINT('Ctrl Pts',(31.1362943994381,23.1726388829673,41.5303880208382));
#67967=CARTESIAN_POINT('Ctrl Pts',(31.0636372921346,23.2091253289662,41.5346130195768));
#67968=CARTESIAN_POINT('Ctrl Pts',(30.9892617881354,23.2419436577522,41.5388380183154));
#67969=CARTESIAN_POINT('Ctrl Pts',(30.9146655840924,23.2748593708409,41.5430755542115));
#67970=CARTESIAN_POINT('Ctrl Pts',(30.8383411582727,23.3040848949014,41.5473130901076));
#67971=CARTESIAN_POINT('Ctrl Pts',(30.7606890972723,23.329442497099,41.5515506260037));
#67972=CARTESIAN_POINT('Ctrl Pts',(30.683406189167,23.3546795508895,41.5557680169272));
#67973=CARTESIAN_POINT('Ctrl Pts',(30.6048086837415,23.3760852242856,41.5599854078507));
#67974=CARTESIAN_POINT('Ctrl Pts',(30.5253110468039,23.3935326515646,41.5642027987741));
#67975=CARTESIAN_POINT('Ctrl Pts',(30.4458396893275,23.4109743112635,41.5684187955585));
#67976=CARTESIAN_POINT('Ctrl Pts',(30.3654692450358,23.4244602236845,41.5726347923429));
#67977=CARTESIAN_POINT('Ctrl Pts',(30.2846266862501,23.4339141109485,41.5768507891273));
#67978=CARTESIAN_POINT('Ctrl Pts',(30.2037860802659,23.4433677698481,41.5810666840717));
#67979=CARTESIAN_POINT('Ctrl Pts',(30.1224738444053,23.4487895443275,41.5852825790161));
#67980=CARTESIAN_POINT('Ctrl Pts',(30.0411229949267,23.450154923528,41.5894984739605));
#67981=CARTESIAN_POINT('Ctrl Pts',(29.9590490733099,23.4515324386515,41.5937518411156));
#67982=CARTESIAN_POINT('Ctrl Pts',(29.876936328975,23.4487810638216,41.5980052082707));
#67983=CARTESIAN_POINT('Ctrl Pts',(29.7952284989678,23.4419293360712,41.6022585754258));
#67984=CARTESIAN_POINT('Ctrl Pts',(29.7141227104706,23.4351280933785,41.6064806028234));
#67985=CARTESIAN_POINT('Ctrl Pts',(29.6334163464032,23.4242868457514,41.6107026302209));
#67986=CARTESIAN_POINT('Ctrl Pts',(29.5535354881006,23.4094853578336,41.6149246576184));
#67987=CARTESIAN_POINT('Ctrl Pts',(29.4727652063653,23.3945190645985,41.6191936946523));
#67988=CARTESIAN_POINT('Ctrl Pts',(29.3928394025217,23.3755039074134,41.6234627316862));
#67989=CARTESIAN_POINT('Ctrl Pts',(29.3141832729915,23.3525742638555,41.6277317687201));
#67990=CARTESIAN_POINT('Ctrl Pts',(29.2355271434614,23.3296446202977,41.632000805754));
#67991=CARTESIAN_POINT('Ctrl Pts',(29.1581411246682,23.3028007101411,41.6362698427879));
#67992=CARTESIAN_POINT('Ctrl Pts',(29.0824282935996,23.2722263121471,41.6405388798218));
#67993=CARTESIAN_POINT('Ctrl Pts',(29.0073888346806,23.2419238356729,41.6447699490422));
#67994=CARTESIAN_POINT('Ctrl Pts',(28.9337112650968,23.207843272893,41.6490010182627));
#67995=CARTESIAN_POINT('Ctrl Pts',(28.8618022722028,23.1701281488514,41.6532320874831));
#67996=CARTESIAN_POINT('Ctrl Pts',(28.7899964503554,23.1324671363842,41.6574570861995));
#67997=CARTESIAN_POINT('Ctrl Pts',(28.7199545739187,23.0911821334844,41.6616820849158));
#67998=CARTESIAN_POINT('Ctrl Pts',(28.652063991403,23.0464649439283,41.6659070836321));
#67999=CARTESIAN_POINT('Ctrl Pts',(28.5839719515911,23.0016150613865,41.6701446195337));
#68000=CARTESIAN_POINT('Ctrl Pts',(28.5180444295562,22.9533127726564,41.6743821554354));
#68001=CARTESIAN_POINT('Ctrl Pts',(28.4546479020158,22.9017983971115,41.6786196913371));
#68002=CARTESIAN_POINT('Ctrl Pts',(28.3915527578972,22.8505289179257,41.6828370822384));
#68003=CARTESIAN_POINT('Ctrl Pts',(28.3309649655752,22.7960781137796,41.6870544731397));
#68004=CARTESIAN_POINT('Ctrl Pts',(28.2732157760017,22.7387255372113,41.691271864041));
#68005=CARTESIAN_POINT('Ctrl Pts',(28.2154856765237,22.6813919196304,41.6954878608034));
#68006=CARTESIAN_POINT('Ctrl Pts',(28.1605926460114,22.6211587619126,41.6997038575658));
#68007=CARTESIAN_POINT('Ctrl Pts',(28.1088322003689,22.5583435448059,41.7039198543281));
#68008=CARTESIAN_POINT('Ctrl Pts',(28.0570730050299,22.4955298450372,41.7081357492506));
#68009=CARTESIAN_POINT('Ctrl Pts',(28.008446538943,22.4301345694235,41.7123516441731));
#68010=CARTESIAN_POINT('Ctrl Pts',(27.9632080893745,22.3625083349508,41.7165675390956));
#68011=CARTESIAN_POINT('Ctrl Pts',(27.9175675456066,22.2942810162927,41.720820906277));
#68012=CARTESIAN_POINT('Ctrl Pts',(27.8753758287363,22.223783271918,41.7250742734584));
#68013=CARTESIAN_POINT('Ctrl Pts',(27.8368494557566,22.1514034796453,41.7293276406398));
#68014=CARTESIAN_POINT('Ctrl Pts',(27.7986069541128,22.0795569986277,41.733549668016));
#68015=CARTESIAN_POINT('Ctrl Pts',(27.7639761051277,22.0058565638607,41.7377716953922));
#68016=CARTESIAN_POINT('Ctrl Pts',(27.7331208055899,21.9307034801432,41.7419937227684));
#68017=CARTESIAN_POINT('Ctrl Pts',(27.7019219510522,21.8547136125324,41.7462627598523));
#68018=CARTESIAN_POINT('Ctrl Pts',(27.6745834069441,21.777239007102,41.7505317969363));
#68019=CARTESIAN_POINT('Ctrl Pts',(27.6512226944134,21.6987098244344,41.7548008340203));
#68020=CARTESIAN_POINT('Ctrl Pts',(27.6278619818826,21.6201806417669,41.7590698711043));
#68021=CARTESIAN_POINT('Ctrl Pts',(27.6084791527692,21.5405973677416,41.7633389081883));
#68022=CARTESIAN_POINT('Ctrl Pts',(27.5931382236528,21.4603983487793,41.7676079452723));
#68023=CARTESIAN_POINT('Ctrl Pts',(27.5707299436689,21.3432527666765,41.773843667862));
#68024=CARTESIAN_POINT('Ctrl Pts',(27.5568689197519,21.2244236305085,41.7800793904518));
#68025=CARTESIAN_POINT('Ctrl Pts',(27.5517475311304,21.1049290173105,41.7863151130416));
#68026=CARTESIAN_POINT('Ctrl Pts',(27.5502808590853,21.0707079453196,41.7881009099571));
#68027=CARTESIAN_POINT('Ctrl Pts',(27.5495306999149,21.036432469201,41.7898867068725));
#68028=CARTESIAN_POINT('Ctrl Pts',(27.5495009231114,21.0021270092151,41.791672503788));
#68029=CARTESIAN_POINT('',(27.5495000081341,21.0001996626194,42.5916725037481));
#68030=CARTESIAN_POINT('Ctrl Pts',(27.5495009231109,21.0021270086603,41.7916725038169));
#68031=CARTESIAN_POINT('Ctrl Pts',(27.5494293597252,20.9196797606114,41.7959643582713));
#68032=CARTESIAN_POINT('Ctrl Pts',(27.5535234877986,20.837092575959,41.8002562127257));
#68033=CARTESIAN_POINT('Ctrl Pts',(27.5617955596507,20.7548279031765,41.8045480671801));
#68034=CARTESIAN_POINT('Ctrl Pts',(27.5698087291806,20.6751379801294,41.8087055936083));
#68035=CARTESIAN_POINT('Ctrl Pts',(27.5817421408007,20.5957511991929,41.8128631200365));
#68036=CARTESIAN_POINT('Ctrl Pts',(27.5975541099105,20.5170880047132,41.8170206464647));
#68037=CARTESIAN_POINT('Ctrl Pts',(27.6133577590071,20.4384662015873,41.8211759852669));
#68038=CARTESIAN_POINT('Ctrl Pts',(27.6330358229658,20.3605676992317,41.8253313240692));
#68039=CARTESIAN_POINT('Ctrl Pts',(27.6564951166518,20.2838051161009,41.8294866628714));
#68040=CARTESIAN_POINT('Ctrl Pts',(27.6799497481538,20.2070577883864,41.8336411758621));
#68041=CARTESIAN_POINT('Ctrl Pts',(27.7071839769369,20.1314463904358,41.8377956888529));
#68042=CARTESIAN_POINT('Ctrl Pts',(27.7380545492334,20.0573690925095,41.8419502018436));
#68043=CARTESIAN_POINT('Ctrl Pts',(27.768929095014,19.9832822597759,41.8461052495795));
#68044=CARTESIAN_POINT('Ctrl Pts',(27.8034407258317,19.9107303607031,41.8502602973155));
#68045=CARTESIAN_POINT('Ctrl Pts',(27.8413984224977,19.8400907450992,41.8544153450514));
#68046=CARTESIAN_POINT('Ctrl Pts',(27.8793960608656,19.7693767976281,41.8585747650147));
#68047=CARTESIAN_POINT('Ctrl Pts',(27.9208467696119,19.7005795699702,41.862734184978));
#68048=CARTESIAN_POINT('Ctrl Pts',(27.9655144623797,19.6340502032601,41.8668936049412));
#68049=CARTESIAN_POINT('Ctrl Pts',(28.0102106244738,19.5674784335036,41.8710556759455));
#68050=CARTESIAN_POINT('Ctrl Pts',(28.0581275598252,19.5031777817647,41.8752177469497));
#68051=CARTESIAN_POINT('Ctrl Pts',(28.1089884823503,19.4414668145605,41.879379817954));
#68052=CARTESIAN_POINT('Ctrl Pts',(28.1599291773465,19.3796590572058,41.8835484169304));
#68053=CARTESIAN_POINT('Ctrl Pts',(28.2138227429899,19.3204494349801,41.8877170159069));
#68054=CARTESIAN_POINT('Ctrl Pts',(28.2703557697157,19.2641195068081,41.8918856148834));
#68055=CARTESIAN_POINT('Ctrl Pts',(28.282974402217,19.2515462075599,41.8928160801632));
#68056=CARTESIAN_POINT('Ctrl Pts',(28.2957244110023,19.2391162178597,41.8937465454429));
#68057=CARTESIAN_POINT('Ctrl Pts',(28.3086021002813,19.2268323838883,41.8946770107227));
#68058=CARTESIAN_POINT('Ctrl Pts',(28.3671603257765,19.1709745739927,41.8989080800154));
#68059=CARTESIAN_POINT('Ctrl Pts',(28.4285984395889,19.1179158573553,41.9031391493081));
#68060=CARTESIAN_POINT('Ctrl Pts',(28.4926179369572,19.0679675038921,41.9073702186008));
#68061=CARTESIAN_POINT('Ctrl Pts',(28.5565455826954,19.0180908135609,41.9115952173895));
#68062=CARTESIAN_POINT('Ctrl Pts',(28.6230468928422,18.9713159070137,41.9158202161782));
#68063=CARTESIAN_POINT('Ctrl Pts',(28.6917873601505,18.9279165222082,41.920045214967));
#68064=CARTESIAN_POINT('Ctrl Pts',(28.7607318052119,18.8843883557789,41.9242827508506));
#68065=CARTESIAN_POINT('Ctrl Pts',(28.8319283715699,18.8442560979162,41.9285202867341));
#68066=CARTESIAN_POINT('Ctrl Pts',(28.9050069660881,18.8077544604483,41.9327578226177));
#68067=CARTESIAN_POINT('Ctrl Pts',(28.9777381507575,18.7714263488731,41.9369752135915));
#68068=CARTESIAN_POINT('Ctrl Pts',(29.0523330936432,18.738694631029,41.9411926045652));
#68069=CARTESIAN_POINT('Ctrl Pts',(29.1284004926172,18.709745745833,41.9454099955389));
#68070=CARTESIAN_POINT('Ctrl Pts',(29.20444274606,18.6808064302437,41.9496259923735));
#68071=CARTESIAN_POINT('Ctrl Pts',(29.2819560547665,18.655647629269,41.9538419892081));
#68072=CARTESIAN_POINT('Ctrl Pts',(29.3605293064773,18.6344075832626,41.9580579860427));
#68073=CARTESIAN_POINT('Ctrl Pts',(29.4391006602005,18.6131680503232,41.9622738810372));
#68074=CARTESIAN_POINT('Ctrl Pts',(29.5187314568824,18.5958472044146,41.9664897760316));
#68075=CARTESIAN_POINT('Ctrl Pts',(29.5989969930278,18.5825329705663,41.9707056710261));
#68076=CARTESIAN_POINT('Ctrl Pts',(29.6799759526077,18.5691003959344,41.9749590381217));
#68077=CARTESIAN_POINT('Ctrl Pts',(29.7616005197291,18.5597461088512,41.9792124052173));
#68078=CARTESIAN_POINT('Ctrl Pts',(29.8434275853269,18.5545071398666,41.9834657723129));
#68079=CARTESIAN_POINT('Ctrl Pts',(29.9246517329442,18.5493067726402,41.9876877997597));
#68080=CARTESIAN_POINT('Ctrl Pts',(30.0060749342987,18.5481612245314,41.9919098272065));
#68081=CARTESIAN_POINT('Ctrl Pts',(30.0872640103474,18.5510542589722,41.9961318546533));
#68082=CARTESIAN_POINT('Ctrl Pts',(30.169357072868,18.5539795054312,42.0004008915733));
#68083=CARTESIAN_POINT('Ctrl Pts',(30.2512102775175,18.5610337842884,42.0046699284933));
#68084=CARTESIAN_POINT('Ctrl Pts',(30.3323832890513,18.5721467097126,42.0089389654133));
#68085=CARTESIAN_POINT('Ctrl Pts',(30.4135563005851,18.5832596351368,42.0132080023333));
#68086=CARTESIAN_POINT('Ctrl Pts',(30.4940486550042,18.5984310539254,42.0174770392533));
#68087=CARTESIAN_POINT('Ctrl Pts',(30.5734346309067,18.6175384632534,42.0217460761733));
#68088=CARTESIAN_POINT('Ctrl Pts',(30.6521145665756,18.6364759357684,42.0259771452811));
#68089=CARTESIAN_POINT('Ctrl Pts',(30.7300030373767,18.6593506992851,42.0302082143889));
#68090=CARTESIAN_POINT('Ctrl Pts',(30.8066766706075,18.6860805979685,42.0344392834967));
#68091=CARTESIAN_POINT('Ctrl Pts',(30.8832402967475,18.7127721460709,42.0386642821004));
#68092=CARTESIAN_POINT('Ctrl Pts',(30.9585921116628,18.7433076923567,42.0428892807042));
#68093=CARTESIAN_POINT('Ctrl Pts',(31.0323207712093,18.7775544831583,42.0471142793079));
#68094=CARTESIAN_POINT('Ctrl Pts',(31.1062682143186,18.8119028984157,42.0513518152377));
#68095=CARTESIAN_POINT('Ctrl Pts',(31.1785823954215,18.8499845028644,42.0555893511676));
#68096=CARTESIAN_POINT('Ctrl Pts',(31.2488654803406,18.8916154852557,42.0598268870974));
#68097=CARTESIAN_POINT('Ctrl Pts',(31.3188144412274,18.9330485549953,42.0640442778871));
#68098=CARTESIAN_POINT('Ctrl Pts',(31.3867511677669,18.9779970980926,42.0682616686769));
#68099=CARTESIAN_POINT('Ctrl Pts',(31.4523068988343,19.0262333163217,42.0724790594666));
#68100=CARTESIAN_POINT('Ctrl Pts',(31.5178409592142,19.0744535891561,42.076695056118));
#68101=CARTESIAN_POINT('Ctrl Pts',(31.5809952129406,19.1259591035466,42.0809110527694));
#68102=CARTESIAN_POINT('Ctrl Pts',(31.6414306675575,19.1804792901421,42.0851270494208));
#68103=CARTESIAN_POINT('Ctrl Pts',(31.7018646623319,19.2349981597808,42.0893429442331));
#68104=CARTESIAN_POINT('Ctrl Pts',(31.7595796440716,19.2925312445725,42.0935588390454));
#68105=CARTESIAN_POINT('Ctrl Pts',(31.8142715384427,19.3527692830702,42.0977747338578));
#68106=CARTESIAN_POINT('Ctrl Pts',(31.8694495554961,19.4135427405216,42.1020281011716));
#68107=CARTESIAN_POINT('Ctrl Pts',(31.92155013975,19.4770691326891,42.1062814684854));
#68108=CARTESIAN_POINT('Ctrl Pts',(31.970302012333,19.5429961461284,42.1105348357993));
#68109=CARTESIAN_POINT('Ctrl Pts',(32.0186946669692,19.6084373901982,42.1147568630682));
#68110=CARTESIAN_POINT('Ctrl Pts',(32.0637875861554,19.6762435705913,42.1189788903372));
#68111=CARTESIAN_POINT('Ctrl Pts',(32.1053596380592,19.7460418490112,42.1232009176062));
#68112=CARTESIAN_POINT('Ctrl Pts',(32.1473945730361,19.8166172947859,42.1274699549425));
#68113=CARTESIAN_POINT('Ctrl Pts',(32.1858295198242,19.889229044105,42.1317389922787));
#68114=CARTESIAN_POINT('Ctrl Pts',(32.2204849743354,19.9634688963902,42.136008029615));
#68115=CARTESIAN_POINT('Ctrl Pts',(32.2551404288467,20.0377087486754,42.1402770669512));
#68116=CARTESIAN_POINT('Ctrl Pts',(32.2860162683499,20.113576230954,42.1445461042875));
#68117=CARTESIAN_POINT('Ctrl Pts',(32.3129847077609,20.1906471772681,42.1488151416238));
#68118=CARTESIAN_POINT('Ctrl Pts',(32.3397132946812,20.2670326683299,42.1530462109033));
#68119=CARTESIAN_POINT('Ctrl Pts',(32.3627040678191,20.3448869777792,42.1572772801828));
#68120=CARTESIAN_POINT('Ctrl Pts',(32.3817966079494,20.423809781096,42.1615083494623));
#68121=CARTESIAN_POINT('Ctrl Pts',(32.4008617551541,20.5026193503185,42.1657333482365));
#68122=CARTESIAN_POINT('Ctrl Pts',(32.4160396689735,20.5824939206251,42.1699583470106));
#68123=CARTESIAN_POINT('Ctrl Pts',(32.427218971285,20.6630158528444,42.1741833457848));
#68124=CARTESIAN_POINT('Ctrl Pts',(32.4384314466653,20.7437767230157,42.1784208816719));
#68125=CARTESIAN_POINT('Ctrl Pts',(32.445621391254,20.8251883552419,42.1826584175589));
#68126=CARTESIAN_POINT('Ctrl Pts',(32.4487276573074,20.9068167915449,42.186895953446));
#68127=CARTESIAN_POINT('Ctrl Pts',(32.4518191564025,20.9880571723197,42.1911133444019));
#68128=CARTESIAN_POINT('Ctrl Pts',(32.450865692402,21.0695118326457,42.1953307353578));
#68129=CARTESIAN_POINT('Ctrl Pts',(32.4458588408457,21.1507474068,42.1995481263138));
#68130=CARTESIAN_POINT('Ctrl Pts',(32.4408536444012,21.2319561269616,42.2037641231294));
#68131=CARTESIAN_POINT('Ctrl Pts',(32.4317977498745,21.312945441057,42.2079801199451));
#68132=CARTESIAN_POINT('Ctrl Pts',(32.4187348113261,21.393283819244,42.2121961167607));
#68133=CARTESIAN_POINT('Ctrl Pts',(32.4056721883249,21.4736202567844,42.2164120117352));
#68134=CARTESIAN_POINT('Ctrl Pts',(32.3886027894625,21.5533053309216,42.2206279067096));
#68135=CARTESIAN_POINT('Ctrl Pts',(32.367621710285,21.6319158860063,42.224843801684));
#68136=CARTESIAN_POINT('Ctrl Pts',(32.3464541449708,21.7112251553278,42.2290971687998));
#68137=CARTESIAN_POINT('Ctrl Pts',(32.321305122915,21.7894402395756,42.2333505359157));
#68138=CARTESIAN_POINT('Ctrl Pts',(32.2923236946659,21.8661422105367,42.2376039030316));
#68139=CARTESIAN_POINT('Ctrl Pts',(32.2635558075951,21.9422790254564,42.2418259304557));
#68140=CARTESIAN_POINT('Ctrl Pts',(32.2310120473007,22.0169245451166,42.2460479578799));
#68141=CARTESIAN_POINT('Ctrl Pts',(32.194885892181,22.0896908599713,42.2502699853041));
#68142=CARTESIAN_POINT('Ctrl Pts',(32.1583574957506,22.1632673805554,42.2545390222658));
#68143=CARTESIAN_POINT('Ctrl Pts',(32.118166673225,22.2349221633375,42.2588080592275));
#68144=CARTESIAN_POINT('Ctrl Pts',(32.0745591825804,22.304283116494,42.2630770961892));
#68145=CARTESIAN_POINT('Ctrl Pts',(32.0309516919358,22.3736440696506,42.2673461331509));
#68146=CARTESIAN_POINT('Ctrl Pts',(31.9839278641339,22.4407108336954,42.2716151701126));
#68147=CARTESIAN_POINT('Ctrl Pts',(31.933774905206,22.5051461277881,42.2758842070743));
#68148=CARTESIAN_POINT('Ctrl Pts',(31.8840679890306,22.5690083570698,42.2801152767248));
#68149=CARTESIAN_POINT('Ctrl Pts',(31.8311008536773,22.6305254517548,42.2843463463754));
#68150=CARTESIAN_POINT('Ctrl Pts',(31.7751229820897,22.6893456272939,42.2885774160259));
#68151=CARTESIAN_POINT('Ctrl Pts',(31.7192254244211,22.7480814109353,42.2928024151744));
#68152=CARTESIAN_POINT('Ctrl Pts',(31.6603260274446,22.804127626336,42.2970274143229));
#68153=CARTESIAN_POINT('Ctrl Pts',(31.5987154046977,22.8571643181965,42.3012524134714));
#68154=CARTESIAN_POINT('Ctrl Pts',(31.5369219675871,22.9103583833904,42.3054899492653));
#68155=CARTESIAN_POINT('Ctrl Pts',(31.4724014839592,22.9605246670681,42.3097274850591));
#68156=CARTESIAN_POINT('Ctrl Pts',(31.4054855055089,23.0073765824589,42.313965020853));
#68157=CARTESIAN_POINT('Ctrl Pts',(31.3388876331981,23.0540057725413,42.3181824121884));
#68158=CARTESIAN_POINT('Ctrl Pts',(31.2699173703278,23.0973517613215,42.3223998035238));
#68159=CARTESIAN_POINT('Ctrl Pts',(31.1989343462416,23.1371725909252,42.3266171948591));
#68160=CARTESIAN_POINT('Ctrl Pts',(31.1279747869491,23.1769802569936,42.3308331920553));
#68161=CARTESIAN_POINT('Ctrl Pts',(31.0550041929314,23.2132648507062,42.3350491892514));
#68162=CARTESIAN_POINT('Ctrl Pts',(30.9804088764946,23.2458291753583,42.3392651864476));
#68163=CARTESIAN_POINT('Ctrl Pts',(30.9058153619657,23.2783927133938,42.3434810818031));
#68164=CARTESIAN_POINT('Ctrl Pts',(30.8295976296179,23.3072359760307,42.3476969771585));
#68165=CARTESIAN_POINT('Ctrl Pts',(30.7521628347386,23.332209536049,42.351912872514));
#68166=CARTESIAN_POINT('Ctrl Pts',(30.6740397914275,23.3574050636408,42.3561662391815));
#68167=CARTESIAN_POINT('Ctrl Pts',(30.5946783953211,23.3786615921939,42.3604196058491));
#68168=CARTESIAN_POINT('Ctrl Pts',(30.5145114916103,23.3958773288716,42.3646729725167));
#68169=CARTESIAN_POINT('Ctrl Pts',(30.434935258764,23.4129662197614,42.3688950003193));
#68170=CARTESIAN_POINT('Ctrl Pts',(30.3545658224632,23.4260736518788,42.373117028122));
#68171=CARTESIAN_POINT('Ctrl Pts',(30.273834039708,23.4351519806158,42.3773390559246));
#68172=CARTESIAN_POINT('Ctrl Pts',(30.1922033846978,23.4443313879807,42.3816080920246));
#68173=CARTESIAN_POINT('Ctrl Pts',(30.1102027518452,23.4493913847828,42.3858771281247));
#68174=CARTESIAN_POINT('Ctrl Pts',(30.0282780395337,23.4503368344944,42.3901461642247));
#68175=CARTESIAN_POINT('Ctrl Pts',(29.9463533272223,23.451282284206,42.3944152003247));
#68176=CARTESIAN_POINT('Ctrl Pts',(29.8645050169356,23.4481132701266,42.3986842364247));
#68177=CARTESIAN_POINT('Ctrl Pts',(29.7831722166065,23.4408883551586,42.4029532725248));
#68178=CARTESIAN_POINT('Ctrl Pts',(29.7025627738389,23.4337276971305,42.4071843406767));
#68179=CARTESIAN_POINT('Ctrl Pts',(29.6221571600935,23.4225561642766,42.4114154088286));
#68180=CARTESIAN_POINT('Ctrl Pts',(29.5423862267232,23.4073927565953,42.4156464769805));
#68181=CARTESIAN_POINT('Ctrl Pts',(29.462729744305,23.3922511045381,42.4198714746283));
#68182=CARTESIAN_POINT('Ctrl Pts',(29.3837065866612,23.3731290386071,42.4240964722761));
#68183=CARTESIAN_POINT('Ctrl Pts',(29.3057431484531,23.3500973754464,42.4283214699239));
#68184=CARTESIAN_POINT('Ctrl Pts',(29.2275483382329,23.3269973612436,42.4325590060927));
#68185=CARTESIAN_POINT('Ctrl Pts',(29.150420017547,23.2999645552081,42.4367965422615));
#68186=CARTESIAN_POINT('Ctrl Pts',(29.0747787270261,23.2691222633513,42.4410340784303));
#68187=CARTESIAN_POINT('Ctrl Pts',(28.999497054501,23.2384266036197,42.4452514682709));
#68188=CARTESIAN_POINT('Ctrl Pts',(28.9256887406675,23.2039577700228,42.4494688581115));
#68189=CARTESIAN_POINT('Ctrl Pts',(28.8537520377168,23.1658868527607,42.4536862479521));
#68190=CARTESIAN_POINT('Ctrl Pts',(28.7818391147307,23.1278285205216,42.4579022436591));
#68191=CARTESIAN_POINT('Ctrl Pts',(28.7117969846284,23.0861706865561,42.462118239366));
#68192=CARTESIAN_POINT('Ctrl Pts',(28.6440007446553,23.0411311250149,42.4663342350729));
#68193=CARTESIAN_POINT('Ctrl Pts',(28.5762061422333,22.9960926513598,42.4705501289466));
#68194=CARTESIAN_POINT('Ctrl Pts',(28.5106577087616,22.9476728707419,42.4747660228203));
#68195=CARTESIAN_POINT('Ctrl Pts',(28.4477016931987,22.8961329638772,42.478981916694));
#68196=CARTESIAN_POINT('Ctrl Pts',(28.3841860692927,22.8441349250671,42.4832352851341));
#68197=CARTESIAN_POINT('Ctrl Pts',(28.3233095641587,22.7889613054111,42.4874886535742));
#68198=CARTESIAN_POINT('Ctrl Pts',(28.2653923196798,22.7309206929765,42.4917420220143));
#68199=CARTESIAN_POINT('Ctrl Pts',(28.2079018539464,22.6733077683572,42.4959640483686));
#68200=CARTESIAN_POINT('Ctrl Pts',(28.1533274502599,22.6128703532463,42.5001860747229));
#68201=CARTESIAN_POINT('Ctrl Pts',(28.1019426666762,22.5499447117287,42.5044081010772));
#68202=CARTESIAN_POINT('Ctrl Pts',(28.0499857029963,22.4863183802966,42.5086771405602));
#68203=CARTESIAN_POINT('Ctrl Pts',(28.0012901237273,22.4201484581849,42.5129461800432));
#68204=CARTESIAN_POINT('Ctrl Pts',(27.9560935127577,22.3518123099783,42.5172152195262));
#68205=CARTESIAN_POINT('Ctrl Pts',(27.9108969017881,22.2834761617717,42.5214842590092));
#68206=CARTESIAN_POINT('Ctrl Pts',(27.8691994500721,22.2129742372533,42.5257532984923));
#68207=CARTESIAN_POINT('Ctrl Pts',(27.8311899325944,22.1407072987932,42.5300223379753));
#68208=CARTESIAN_POINT('Ctrl Pts',(27.7913112811431,22.0648866033058,42.5345013092665));
#68209=CARTESIAN_POINT('Ctrl Pts',(27.7553561644625,21.9868657022069,42.5389802805577));
#68210=CARTESIAN_POINT('Ctrl Pts',(27.7235581914406,21.907062810528,42.5434592518489));
#68211=CARTESIAN_POINT('Ctrl Pts',(27.6918561073449,21.827500569836,42.5479247165009));
#68212=CARTESIAN_POINT('Ctrl Pts',(27.6642863325223,21.7461673995204,42.552390181153));
#68213=CARTESIAN_POINT('Ctrl Pts',(27.6410356048089,21.6635037544889,42.556855645805));
#68214=CARTESIAN_POINT('Ctrl Pts',(27.6178276006091,21.5809920049766,42.5613129051078));
#68215=CARTESIAN_POINT('Ctrl Pts',(27.5989229557308,21.4971550122848,42.5657701644107));
#68216=CARTESIAN_POINT('Ctrl Pts',(27.5844599283427,21.4124517089524,42.5702274237136));
#68217=CARTESIAN_POINT('Ctrl Pts',(27.5700323064602,21.327955759392,42.5746737716412));
#68218=CARTESIAN_POINT('Ctrl Pts',(27.560024706694,21.2425981005171,42.5791201195687));
#68219=CARTESIAN_POINT('Ctrl Pts',(27.5545249146432,21.1568497908799,42.5835664674963));
#68220=CARTESIAN_POINT('Ctrl Pts',(27.5511827325148,21.1047411901609,42.5862684795803));
#68221=CARTESIAN_POINT('Ctrl Pts',(27.5495042685491,21.0524886039351,42.5889704916642));
#68222=CARTESIAN_POINT('Ctrl Pts',(27.5495000081341,21.0001996626194,42.5916725037481));
#68223=CARTESIAN_POINT('',(27.5495010068324,20.9977786299922,43.3916725037471));
#68224=CARTESIAN_POINT('Ctrl Pts',(27.549500008134,21.0001996618478,42.591672503788));
#68225=CARTESIAN_POINT('Ctrl Pts',(27.549493086791,20.9152522810414,42.5960621288915));
#68226=CARTESIAN_POINT('Ctrl Pts',(27.5539075740442,20.8303783217193,42.600451753995));
#68227=CARTESIAN_POINT('Ctrl Pts',(27.5626947630161,20.746044429534,42.6048413790985));
#68228=CARTESIAN_POINT('Ctrl Pts',(27.5715034330423,20.6615043757502,42.6092417350257));
#68229=CARTESIAN_POINT('Ctrl Pts',(27.5847061246101,20.5775074337583,42.6136420909529));
#68230=CARTESIAN_POINT('Ctrl Pts',(27.602202470725,20.4945128502102,42.6180424468801));
#68231=CARTESIAN_POINT('Ctrl Pts',(27.6197201796934,20.4114169311539,42.6224481755953));
#68232=CARTESIAN_POINT('Ctrl Pts',(27.641541890222,20.3293262038286,42.6268539043105));
#68233=CARTESIAN_POINT('Ctrl Pts',(27.6675172453543,20.2486848535533,42.6312596330258));
#68234=CARTESIAN_POINT('Ctrl Pts',(27.6935620327325,20.1678279485709,42.6356771382745));
#68235=CARTESIAN_POINT('Ctrl Pts',(27.7237825197494,20.088428549067,42.6400946435232));
#68236=CARTESIAN_POINT('Ctrl Pts',(27.7579797073247,20.0109119062327,42.6445121487719));
#68237=CARTESIAN_POINT('Ctrl Pts',(27.7904395918625,19.9373333035882,42.6487052336565));
#68238=CARTESIAN_POINT('Ctrl Pts',(27.8264818567594,19.8654510897126,42.6528983185412));
#68239=CARTESIAN_POINT('Ctrl Pts',(27.8658994649333,19.7956058966318,42.6570914034258));
#68240=CARTESIAN_POINT('Ctrl Pts',(27.9056741766947,19.7251279414386,42.6613224755381));
#68241=CARTESIAN_POINT('Ctrl Pts',(27.9490185459123,19.6564901683137,42.6655535476503));
#68242=CARTESIAN_POINT('Ctrl Pts',(27.9957375362144,19.5900772268453,42.6697846197626));
#68243=CARTESIAN_POINT('Ctrl Pts',(28.0423894969425,19.5237595706378,42.6740096213892));
#68244=CARTESIAN_POINT('Ctrl Pts',(28.09240619754,19.4596607835253,42.6782346230158));
#68245=CARTESIAN_POINT('Ctrl Pts',(28.1455472373667,19.3981400806681,42.6824596246424));
#68246=CARTESIAN_POINT('Ctrl Pts',(28.1988459211258,19.3364368754447,42.6866971598188));
#68247=CARTESIAN_POINT('Ctrl Pts',(28.2552872733254,19.2773274835091,42.6909346949952));
#68248=CARTESIAN_POINT('Ctrl Pts',(28.3145854936707,19.2211441340416,42.6951722301716));
#68249=CARTESIAN_POINT('Ctrl Pts',(28.3736018648619,19.1652278284993,42.6993896240065));
#68250=CARTESIAN_POINT('Ctrl Pts',(28.435447671836,19.1122101393852,42.7036070178415));
#68251=CARTESIAN_POINT('Ctrl Pts',(28.4998027780823,19.0623832821349,42.7078244116764));
#68252=CARTESIAN_POINT('Ctrl Pts',(28.5641366105701,19.0125728960644,42.7120404113746));
#68253=CARTESIAN_POINT('Ctrl Pts',(28.6309777277201,18.9659515316314,42.7162564110728));
#68254=CARTESIAN_POINT('Ctrl Pts',(28.6999730174825,18.9227710538492,42.720472410771));
#68255=CARTESIAN_POINT('Ctrl Pts',(28.768966640596,18.8795916191339,42.7246883086276));
#68256=CARTESIAN_POINT('Ctrl Pts',(28.8401139381397,18.8398531515447,42.7289042064842));
#68257=CARTESIAN_POINT('Ctrl Pts',(28.9130341565902,18.8037633312276,42.7331201043407));
#68258=CARTESIAN_POINT('Ctrl Pts',(28.9866024026739,18.7673527877786,42.737373468052));
#68259=CARTESIAN_POINT('Ctrl Pts',(29.0619748147519,18.7346562940568,42.7416268317633));
#68260=CARTESIAN_POINT('Ctrl Pts',(29.1387382250637,18.7058381911832,42.7458801954746));
#68261=CARTESIAN_POINT('Ctrl Pts',(29.2149361390944,18.6772323838542,42.7501022257505));
#68262=CARTESIAN_POINT('Ctrl Pts',(29.2925041588335,18.6524480987598,42.7543242560263));
#68263=CARTESIAN_POINT('Ctrl Pts',(29.3710231183096,18.6315958258146,42.7585462863022));
#68264=CARTESIAN_POINT('Ctrl Pts',(29.4504161603667,18.6105114228375,42.7628153167312));
#68265=CARTESIAN_POINT('Ctrl Pts',(29.5307809677201,18.5934472196906,42.7670843471602));
#68266=CARTESIAN_POINT('Ctrl Pts',(29.6116757770617,18.5804639808675,42.7713533775892));
#68267=CARTESIAN_POINT('Ctrl Pts',(29.6925705864033,18.5674807420445,42.7756224080182));
#68268=CARTESIAN_POINT('Ctrl Pts',(29.7739949092396,18.5585784559607,42.7798914384472));
#68269=CARTESIAN_POINT('Ctrl Pts',(29.8555058016396,18.5537637733366,42.7841604688763));
#68270=CARTESIAN_POINT('Ctrl Pts',(29.9362917085614,18.5489919141301,42.788391529103));
#68271=CARTESIAN_POINT('Ctrl Pts',(30.0174658560517,18.5482172809471,42.7926225893298));
#68272=CARTESIAN_POINT('Ctrl Pts',(30.0985992845727,18.5514844433654,42.7968536495566));
#68273=CARTESIAN_POINT('Ctrl Pts',(30.1796163069832,18.5547469182254,42.8010786392737));
#68274=CARTESIAN_POINT('Ctrl Pts',(30.260592265792,18.562039652997,42.8053036289908));
#68275=CARTESIAN_POINT('Ctrl Pts',(30.3410949892738,18.5733553086015,42.8095286187079));
#68276=CARTESIAN_POINT('Ctrl Pts',(30.4218368099261,18.584704572277,42.8137661568587));
#68277=CARTESIAN_POINT('Ctrl Pts',(30.5021021076208,18.6001007137476,42.8180036950095));
#68278=CARTESIAN_POINT('Ctrl Pts',(30.5814567786513,18.6194836138853,42.8222412331603));
#68279=CARTESIAN_POINT('Ctrl Pts',(30.6604339926941,18.6387743176721,42.826458615114));
#68280=CARTESIAN_POINT('Ctrl Pts',(30.7385087669624,18.6620138338785,42.8306759970678));
#68281=CARTESIAN_POINT('Ctrl Pts',(30.8152620195595,18.6890915012784,42.8348933790215));
#68282=CARTESIAN_POINT('Ctrl Pts',(30.8919899005624,18.7161602178708,42.8391093668753));
#68283=CARTESIAN_POINT('Ctrl Pts',(30.9673966892661,18.747064411558,42.8433253547292));
#68284=CARTESIAN_POINT('Ctrl Pts',(31.0410793414582,18.7816438395089,42.847541342583));
#68285=CARTESIAN_POINT('Ctrl Pts',(31.114760214688,18.8162224325889,42.8517572286478));
#68286=CARTESIAN_POINT('Ctrl Pts',(31.1867166137223,18.8544758849736,42.8559731147126));
#68287=CARTESIAN_POINT('Ctrl Pts',(31.2565676454783,18.8961967767072,42.8601890007775));
#68288=CARTESIAN_POINT('Ctrl Pts',(31.3270398600767,18.9382886909077,42.8644423785732));
#68289=CARTESIAN_POINT('Ctrl Pts',(31.395368652384,18.9839097925061,42.868695756369));
#68290=CARTESIAN_POINT('Ctrl Pts',(31.4611919764053,19.0328019270829,42.8729491341648));
#68291=CARTESIAN_POINT('Ctrl Pts',(31.5265300019485,19.0813335924969,42.8771711528975));
#68292=CARTESIAN_POINT('Ctrl Pts',(31.5893990575742,19.1330878717429,42.8813931716302));
#68293=CARTESIAN_POINT('Ctrl Pts',(31.6494791089642,19.187772387615,42.8856151903628));
#68294=CARTESIAN_POINT('Ctrl Pts',(31.7102285276313,19.2430661577178,42.8898842476902));
#68295=CARTESIAN_POINT('Ctrl Pts',(31.7681260661066,19.3013555162733,42.8941533050175));
#68296=CARTESIAN_POINT('Ctrl Pts',(31.8228812237863,19.3623021359337,42.8984223623448));
#68297=CARTESIAN_POINT('Ctrl Pts',(31.8776363814661,19.4232487555941,42.9026914196721));
#68298=CARTESIAN_POINT('Ctrl Pts',(31.9292489033193,19.4868522195339,42.9069604769995));
#68299=CARTESIAN_POINT('Ctrl Pts',(31.9774731271901,19.5527438784925,42.9112295343268));
#68300=CARTESIAN_POINT('Ctrl Pts',(32.0252683195604,19.6180493258951,42.9154606115702));
#68301=CARTESIAN_POINT('Ctrl Pts',(32.069914686428,19.6858474989918,42.9196916888135));
#68302=CARTESIAN_POINT('Ctrl Pts',(32.1111422814506,19.7558020585647,42.9239227660569));
#68303=CARTESIAN_POINT('Ctrl Pts',(32.1523107249026,19.8256562503607,42.9281477727336));
#68304=CARTESIAN_POINT('Ctrl Pts',(32.1900699043101,19.8976602867672,42.9323727794103));
#68305=CARTESIAN_POINT('Ctrl Pts',(32.2241917558679,19.9714469954693,42.936597786087));
#68306=CARTESIAN_POINT('Ctrl Pts',(32.25841477938,20.0454524831993,42.9408353199908));
#68307=CARTESIAN_POINT('Ctrl Pts',(32.2889785966458,20.1212508467144,42.9450728538945));
#68308=CARTESIAN_POINT('Ctrl Pts',(32.3156984551624,20.198444690144,42.9493103877983));
#68309=CARTESIAN_POINT('Ctrl Pts',(32.3422913504427,20.2752717359655,42.9535277864525));
#68310=CARTESIAN_POINT('Ctrl Pts',(32.3650765757841,20.3534805893461,42.9577451851068));
#68311=CARTESIAN_POINT('Ctrl Pts',(32.3839199923844,20.4326590796445,42.961962583761));
#68312=CARTESIAN_POINT('Ctrl Pts',(32.4027571795232,20.5118113942566,42.9661785881817));
#68313=CARTESIAN_POINT('Ctrl Pts',(32.4176550381721,20.5919322572445,42.9703945926024));
#68314=CARTESIAN_POINT('Ctrl Pts',(32.4285297894867,20.6725961032983,42.9746105970231));
#68315=CARTESIAN_POINT('Ctrl Pts',(32.439404277847,20.7532579988783,42.9788264994997));
#68316=CARTESIAN_POINT('Ctrl Pts',(32.4462557912599,20.8344623904805,42.9830424019763));
#68317=CARTESIAN_POINT('Ctrl Pts',(32.4490522035399,20.9157767589296,42.9872583044529));
#68318=CARTESIAN_POINT('Ctrl Pts',(32.4518734600683,20.9978135510283,42.9915116623966));
#68319=CARTESIAN_POINT('Ctrl Pts',(32.450567168116,21.0799618036545,42.9957650203403));
#68320=CARTESIAN_POINT('Ctrl Pts',(32.4451540521899,21.1617773502671,43.000018378284));
#68321=CARTESIAN_POINT('Ctrl Pts',(32.4397808005059,21.2429903761122,43.0042404128839));
#68322=CARTESIAN_POINT('Ctrl Pts',(32.4303611284438,21.3238751206313,43.0084624474838));
#68323=CARTESIAN_POINT('Ctrl Pts',(32.4169672910001,21.4040041636366,43.0126844820837));
#68324=CARTESIAN_POINT('Ctrl Pts',(32.4034243999077,21.4850249246634,43.0169535016993));
#68325=CARTESIAN_POINT('Ctrl Pts',(32.3858184464448,21.5652725831967,43.0212225213149));
#68326=CARTESIAN_POINT('Ctrl Pts',(32.3642763033408,21.6443196500661,43.0254915409305));
#68327=CARTESIAN_POINT('Ctrl Pts',(32.3427341602367,21.7233667169355,43.0297605605461));
#68328=CARTESIAN_POINT('Ctrl Pts',(32.3172560395432,21.8012127519313,43.0340295801617));
#68329=CARTESIAN_POINT('Ctrl Pts',(32.2880185956719,21.8774515119707,43.0382985997773));
#68330=CARTESIAN_POINT('Ctrl Pts',(32.259040935268,21.9530128677363,43.0425296878718));
#68331=CARTESIAN_POINT('Ctrl Pts',(32.2262617796299,22.0272789944634,43.0467607759663));
#68332=CARTESIAN_POINT('Ctrl Pts',(32.1898174801253,22.0998407401701,43.0509918640608));
#68333=CARTESIAN_POINT('Ctrl Pts',(32.1534254672907,22.1722983814735,43.0552168818094));
#68334=CARTESIAN_POINT('Ctrl Pts',(32.1133789610299,22.2430560862626,43.0594418995579));
#68335=CARTESIAN_POINT('Ctrl Pts',(32.0698629240861,22.3117231893558,43.0636669173065));
#68336=CARTESIAN_POINT('Ctrl Pts',(32.0262180038441,22.38059366673,43.0679044484699));
#68337=CARTESIAN_POINT('Ctrl Pts',(31.9790831429959,22.4473606998694,43.0721419796333));
#68338=CARTESIAN_POINT('Ctrl Pts',(31.9286921753868,22.5116536450529,43.0763795107966));
#68339=CARTESIAN_POINT('Ctrl Pts',(31.8785404782383,22.5756413092836,43.0805969209725));
#68340=CARTESIAN_POINT('Ctrl Pts',(31.8251638105296,22.6371779554607,43.0848143311483));
#68341=CARTESIAN_POINT('Ctrl Pts',(31.7688358566356,22.6959274637437,43.0890317413241));
#68342=CARTESIAN_POINT('Ctrl Pts',(31.7125265222976,22.7546575520108,43.0932477574087));
#68343=CARTESIAN_POINT('Ctrl Pts',(31.6532681606354,22.8106019966062,43.0974637734933));
#68344=CARTESIAN_POINT('Ctrl Pts',(31.5913730069765,22.8634597400176,43.1016797895779));
#68345=CARTESIAN_POINT('Ctrl Pts',(31.5294793481123,22.9163162068917,43.1058957038439));
#68346=CARTESIAN_POINT('Ctrl Pts',(31.464949378151,22.9660858196879,43.1101116181099));
#68347=CARTESIAN_POINT('Ctrl Pts',(31.3981291712374,23.0125071603686,43.1143275323759));
#68348=CARTESIAN_POINT('Ctrl Pts',(31.3307157146918,23.0593406434918,43.1185808767802));
#68349=CARTESIAN_POINT('Ctrl Pts',(31.2609715366747,23.1027658152123,43.1228342211846));
#68350=CARTESIAN_POINT('Ctrl Pts',(31.1892811368985,23.1425593638024,43.1270875655889));
#68351=CARTESIAN_POINT('Ctrl Pts',(31.1181182641333,23.1820600953373,43.1313096121616));
#68352=CARTESIAN_POINT('Ctrl Pts',(31.0450381656912,23.2179823208382,43.1355316587343));
#68353=CARTESIAN_POINT('Ctrl Pts',(30.9704392033924,23.2501551063247,43.139753705307));
#68354=CARTESIAN_POINT('Ctrl Pts',(30.8950107432233,23.2826856348176,43.1440226986272));
#68355=CARTESIAN_POINT('Ctrl Pts',(30.8180298896953,23.3113826528595,43.1482916919473));
#68356=CARTESIAN_POINT('Ctrl Pts',(30.7399246530609,23.3361210922794,43.1525606852674));
#68357=CARTESIAN_POINT('Ctrl Pts',(30.6618194164265,23.3608595316993,43.1568296785875));
#68358=CARTESIAN_POINT('Ctrl Pts',(30.5825902815366,23.3816393321179,43.1610986719076));
#68359=CARTESIAN_POINT('Ctrl Pts',(30.5026743844033,23.3983887744202,43.1653676652278));
#68360=CARTESIAN_POINT('Ctrl Pts',(30.4234698009203,23.4149891336567,43.1695986611865));
#68361=CARTESIAN_POINT('Ctrl Pts',(30.3432933544925,23.4276929462028,43.1738296571453));
#68362=CARTESIAN_POINT('Ctrl Pts',(30.262562773737,23.4363930388686,43.1780606531041));
#68363=CARTESIAN_POINT('Ctrl Pts',(30.181948024525,23.4450806487163,43.1822855784662));
#68364=CARTESIAN_POINT('Ctrl Pts',(30.1007811784374,23.4497758982526,43.1865105038283));
#68365=CARTESIAN_POINT('Ctrl Pts',(30.0194907761083,23.4504224859495,43.1907354291904));
#68366=CARTESIAN_POINT('Ctrl Pts',(29.9379573859028,23.4510710063834,43.1949729834191));
#68367=CARTESIAN_POINT('Ctrl Pts',(29.8563001633159,23.4476465305232,43.1992105376478));
#68368=CARTESIAN_POINT('Ctrl Pts',(29.7749573475945,23.44014467903,43.2034480918764));
#68369=CARTESIAN_POINT('Ctrl Pts',(29.6940029832178,23.4326786525113,43.2076654097311));
#68370=CARTESIAN_POINT('Ctrl Pts',(29.6133604966496,23.421174142012,43.2118827275858));
#68371=CARTESIAN_POINT('Ctrl Pts',(29.5334606770915,23.4056789707233,43.2161000454405));
#68372=CARTESIAN_POINT('Ctrl Pts',(29.4535872651673,23.3901889207328,43.2203159694324));
#68373=CARTESIAN_POINT('Ctrl Pts',(29.374456488926,23.3707109176446,43.2245318934243));
#68374=CARTESIAN_POINT('Ctrl Pts',(29.2964905660705,23.3473441857496,43.2287478174162));
#68375=CARTESIAN_POINT('Ctrl Pts',(29.2185265196641,23.3239780162346,43.2329636399411));
#68376=CARTESIAN_POINT('Ctrl Pts',(29.1417277159923,23.2967234385438,43.237179462466));
#68377=CARTESIAN_POINT('Ctrl Pts',(29.0665014004674,23.2657295987541,43.241395284991));
#68378=CARTESIAN_POINT('Ctrl Pts',(28.9906035996739,23.2344591016978,43.2456487387982));
#68379=CARTESIAN_POINT('Ctrl Pts',(28.9163069520686,23.199382420127,43.2499021926055));
#68380=CARTESIAN_POINT('Ctrl Pts',(28.8440075601775,23.1607016751679,43.2541556464128));
#68381=CARTESIAN_POINT('Ctrl Pts',(28.772243551341,23.1223073643661,43.2583776030382));
#68382=CARTESIAN_POINT('Ctrl Pts',(28.7024476878714,23.0803624840626,43.2625995596637));
#68383=CARTESIAN_POINT('Ctrl Pts',(28.6349795107216,23.0351091650941,43.2668215162891));
#68384=CARTESIAN_POINT('Ctrl Pts',(28.5667563314609,22.9893494392122,43.2710907186873));
#68385=CARTESIAN_POINT('Ctrl Pts',(28.5009136506876,22.9402070591589,43.2753599210855));
#68386=CARTESIAN_POINT('Ctrl Pts',(28.4377886014137,22.8879739924392,43.2796291234837));
#68387=CARTESIAN_POINT('Ctrl Pts',(28.3746635521398,22.8357409257196,43.2838983258819));
#68388=CARTESIAN_POINT('Ctrl Pts',(28.3142564479958,22.7804175472364,43.2881675282801));
#68389=CARTESIAN_POINT('Ctrl Pts',(28.2568645214409,22.7223324166341,43.2924367306782));
#68390=CARTESIAN_POINT('Ctrl Pts',(28.2007779866314,22.6655684448528,43.2966088291473));
#68391=CARTESIAN_POINT('Ctrl Pts',(28.1473479519389,22.605941111798,43.3007809276163));
#68392=CARTESIAN_POINT('Ctrl Pts',(28.0968868343006,22.5437326609688,43.3049530260853));
#68393=CARTESIAN_POINT('Ctrl Pts',(28.0464909074219,22.4816045772886,43.3091197346169));
#68394=CARTESIAN_POINT('Ctrl Pts',(27.9990565902623,22.4169023559389,43.3132864431485));
#68395=CARTESIAN_POINT('Ctrl Pts',(27.9548600169935,22.349945443308,43.31745315168));
#68396=CARTESIAN_POINT('Ctrl Pts',(27.910706113351,22.2830531742962,43.3216158374587));
#68397=CARTESIAN_POINT('Ctrl Pts',(27.8697840150892,22.2139109292311,43.3257785232373));
#68398=CARTESIAN_POINT('Ctrl Pts',(27.8323290073754,22.1428703853605,43.3299412090159));
#68399=CARTESIAN_POINT('Ctrl Pts',(27.7948979409024,22.0718752506051,43.3341012340058));
#68400=CARTESIAN_POINT('Ctrl Pts',(27.7609297891928,21.9989846476863,43.3382612589956));
#68401=CARTESIAN_POINT('Ctrl Pts',(27.7306151223929,21.9245769450339,43.3424212839855));
#68402=CARTESIAN_POINT('Ctrl Pts',(27.7002985254673,21.8501645048654,43.3465815738429));
#68403=CARTESIAN_POINT('Ctrl Pts',(27.673636076591,21.7742352081396,43.3507418637004));
#68404=CARTESIAN_POINT('Ctrl Pts',(27.6507706882892,21.6971885620109,43.3549021535578));
#68405=CARTESIAN_POINT('Ctrl Pts',(27.6279060413098,21.6201444138239,43.3590623085338));
#68406=CARTESIAN_POINT('Ctrl Pts',(27.6088383386126,21.5419834500785,43.3632224635098));
#68407=CARTESIAN_POINT('Ctrl Pts',(27.5936603281247,21.4631194592749,43.3673826184857));
#68408=CARTESIAN_POINT('Ctrl Pts',(27.5784668653675,21.3841751794489,43.3715470087886));
#68409=CARTESIAN_POINT('Ctrl Pts',(27.567171087686,21.304526915724,43.3757113990914));
#68410=CARTESIAN_POINT('Ctrl Pts',(27.559814264702,21.2245970330348,43.3798757893942));
#68411=CARTESIAN_POINT('Ctrl Pts',(27.5528675623857,21.1491229999606,43.3838080275118));
#68412=CARTESIAN_POINT('Ctrl Pts',(27.5494324578582,21.0733982663518,43.3877402656295));
#68413=CARTESIAN_POINT('Ctrl Pts',(27.5495010068324,20.9977786299922,43.3916725037471));
#68414=CARTESIAN_POINT('',(27.549500297338,21.0012071676208,44.1916725038378));
#68415=CARTESIAN_POINT('Ctrl Pts',(27.5495010068331,20.9977786292072,43.3916725037879));
#68416=CARTESIAN_POINT('Ctrl Pts',(27.5496021452566,20.8862080595143,43.3974741985338));
#68417=CARTESIAN_POINT('Ctrl Pts',(27.5573265235963,20.7749710520682,43.4032758932798));
#68418=CARTESIAN_POINT('Ctrl Pts',(27.5725171141633,20.6649222642881,43.4090775880257));
#68419=CARTESIAN_POINT('Ctrl Pts',(27.5816185145056,20.5989868373306,43.4125536573934));
#68420=CARTESIAN_POINT('Ctrl Pts',(27.5933992287848,20.5334773180416,43.416029726761));
#68421=CARTESIAN_POINT('Ctrl Pts',(27.6078177664,20.4685732305873,43.4195057961287));
#68422=CARTESIAN_POINT('Ctrl Pts',(27.6253684716024,20.3895698991994,43.4237369789548));
#68423=CARTESIAN_POINT('Ctrl Pts',(27.646870004191,20.311288753792,43.4279681617809));
#68424=CARTESIAN_POINT('Ctrl Pts',(27.6722476464476,20.2341545648558,43.432199344607));
#68425=CARTESIAN_POINT('Ctrl Pts',(27.6975888871691,20.1571310167292,43.4364244582503));
#68426=CARTESIAN_POINT('Ctrl Pts',(27.726795051179,20.0812515955261,43.4406495718936));
#68427=CARTESIAN_POINT('Ctrl Pts',(27.7597406196658,20.0069299325705,43.4448746855369));
#68428=CARTESIAN_POINT('Ctrl Pts',(27.7927828286825,19.9323902589617,43.449112192872));
#68429=CARTESIAN_POINT('Ctrl Pts',(27.8295863064312,19.8594179568088,43.4533497002071));
#68430=CARTESIAN_POINT('Ctrl Pts',(27.8699742662314,19.788414004916,43.4575872075422));
#68431=CARTESIAN_POINT('Ctrl Pts',(27.9101716126747,19.7177451603595,43.4618047157116));
#68432=CARTESIAN_POINT('Ctrl Pts',(27.9539194565869,19.6490265384259,43.4660222238811));
#68433=CARTESIAN_POINT('Ctrl Pts',(28.0009965032448,19.5826308631974,43.4702397320505));
#68434=CARTESIAN_POINT('Ctrl Pts',(28.048057994974,19.5162571260484,43.474455846695));
#68435=CARTESIAN_POINT('Ctrl Pts',(28.0984462362708,19.4522051903639,43.4786719613395));
#68436=CARTESIAN_POINT('Ctrl Pts',(28.1518966449034,19.3908187675465,43.482888075984));
#68437=CARTESIAN_POINT('Ctrl Pts',(28.2053457681527,19.3294338209588,43.4871040892388));
#68438=CARTESIAN_POINT('Ctrl Pts',(28.2618566061826,19.2707146097055,43.4913201024935));
#68439=CARTESIAN_POINT('Ctrl Pts',(28.3211252769315,19.2149706124991,43.4955361157483));
#68440=CARTESIAN_POINT('Ctrl Pts',(28.3809171237012,19.1587345522471,43.4997893445675));
#68441=CARTESIAN_POINT('Ctrl Pts',(28.4435153941032,19.1055268343405,43.5040425733868));
#68442=CARTESIAN_POINT('Ctrl Pts',(28.5085726479575,19.0556248552351,43.508295802206));
#68443=CARTESIAN_POINT('Ctrl Pts',(28.5731544536407,19.0060875672794,43.512517947791));
#68444=CARTESIAN_POINT('Ctrl Pts',(28.6401589983129,18.9598080756316,43.5167400933759));
#68445=CARTESIAN_POINT('Ctrl Pts',(28.7092173758703,18.9170140501566,43.5209622389609));
#68446=CARTESIAN_POINT('Ctrl Pts',(28.7790383601472,18.8737474533219,43.5252310093972));
#68447=CARTESIAN_POINT('Ctrl Pts',(28.8509583897956,18.8340440118049,43.5294997798336));
#68448=CARTESIAN_POINT('Ctrl Pts',(28.924572579229,18.7980903486623,43.53376855027));
#68449=CARTESIAN_POINT('Ctrl Pts',(28.9981867686625,18.7621366855198,43.5380373207064));
#68450=CARTESIAN_POINT('Ctrl Pts',(29.0734946473876,18.7299329317349,43.5423060911428));
#68451=CARTESIAN_POINT('Ctrl Pts',(29.150074461334,18.7016142993998,43.5465748615792));
#68452=CARTESIAN_POINT('Ctrl Pts',(29.2259674738007,18.6735496410246,43.5508053478033));
#68453=CARTESIAN_POINT('Ctrl Pts',(29.3033946777195,18.6491952695504,43.5550358340274));
#68454=CARTESIAN_POINT('Ctrl Pts',(29.3819587508262,18.6287186450529,43.5592663202515));
#68455=CARTESIAN_POINT('Ctrl Pts',(29.4604100683231,18.6082714087248,43.5634907348575));
#68456=CARTESIAN_POINT('Ctrl Pts',(29.5399945682253,18.5916909825737,43.5677151494634));
#68457=CARTESIAN_POINT('Ctrl Pts',(29.6202967452597,18.5790961009698,43.5719395640694));
#68458=CARTESIAN_POINT('Ctrl Pts',(29.7008511190746,18.5664616639179,43.5761772458594));
#68459=CARTESIAN_POINT('Ctrl Pts',(29.7821272402639,18.5578380076049,43.5804149276494));
#68460=CARTESIAN_POINT('Ctrl Pts',(29.8636921726964,18.5532939640783,43.5846526094394));
#68461=CARTESIAN_POINT('Ctrl Pts',(29.9448553424021,18.5487723030543,43.5888694177666));
#68462=CARTESIAN_POINT('Ctrl Pts',(30.0263040170551,18.5482901901487,43.5930862260937));
#68463=CARTESIAN_POINT('Ctrl Pts',(30.107605143246,18.5518636918776,43.5973030344208));
#68464=CARTESIAN_POINT('Ctrl Pts',(30.1888794259112,18.5554360137289,43.601518450467));
#68465=CARTESIAN_POINT('Ctrl Pts',(30.2700057925672,18.5630612706616,43.6057338665133));
#68466=CARTESIAN_POINT('Ctrl Pts',(30.3505521070748,18.5747034263362,43.6099492825595));
#68467=CARTESIAN_POINT('Ctrl Pts',(30.4310965259356,18.5863453080142,43.6141645993965));
#68468=CARTESIAN_POINT('Ctrl Pts',(30.5110604596274,18.6020038328427,43.6183799162335));
#68469=CARTESIAN_POINT('Ctrl Pts',(30.5900192397141,18.6215913835577,43.6225952330705));
#68470=CARTESIAN_POINT('Ctrl Pts',(30.6697036927838,18.6413589542317,43.6268492909004));
#68471=CARTESIAN_POINT('Ctrl Pts',(30.7483639492194,18.6651280441937,43.6311033487304));
#68472=CARTESIAN_POINT('Ctrl Pts',(30.8255782474139,18.6927568816016,43.6353574065603));
#68473=CARTESIAN_POINT('Ctrl Pts',(30.9022008998325,18.7201740161859,43.6395788681561));
#68474=CARTESIAN_POINT('Ctrl Pts',(30.9773992665641,18.7513917143964,43.6438003297518));
#68475=CARTESIAN_POINT('Ctrl Pts',(31.0507822000554,18.7862233585913,43.6480217913476));
#68476=CARTESIAN_POINT('Ctrl Pts',(31.1250150787245,18.821458434301,43.6522921472946));
#68477=CARTESIAN_POINT('Ctrl Pts',(31.1973897680754,18.8603914793856,43.6565625032417));
#68478=CARTESIAN_POINT('Ctrl Pts',(31.2675295345076,18.9027830037998,43.6608328591887));
#68479=CARTESIAN_POINT('Ctrl Pts',(31.3376693009398,18.945174528214,43.6651032151357));
#68480=CARTESIAN_POINT('Ctrl Pts',(31.4055737783894,18.9910242064388,43.6693735710827));
#68481=CARTESIAN_POINT('Ctrl Pts',(31.4709003813,19.040050429656,43.6736439270298));
#68482=CARTESIAN_POINT('Ctrl Pts',(31.5356384035015,19.0886349355952,43.677875807853));
#68483=CARTESIAN_POINT('Ctrl Pts',(31.5980879816993,19.1405214056606,43.6821076886763));
#68484=CARTESIAN_POINT('Ctrl Pts',(31.6578929244885,19.1954664589066,43.6863395694996));
#68485=CARTESIAN_POINT('Ctrl Pts',(31.717612038061,19.2503326576189,43.6905653769283));
#68486=CARTESIAN_POINT('Ctrl Pts',(31.7746937149698,19.3082484097147,43.6947911843569));
#68487=CARTESIAN_POINT('Ctrl Pts',(31.8288128709315,19.3689286548053,43.6990169917856));
#68488=CARTESIAN_POINT('Ctrl Pts',(31.8830796374524,19.4297744058937,43.7032543251479));
#68489=CARTESIAN_POINT('Ctrl Pts',(31.9343673257176,19.493399463376,43.7074916585102));
#68490=CARTESIAN_POINT('Ctrl Pts',(31.9823837021845,19.5594774880921,43.7117289918724));
#68491=CARTESIAN_POINT('Ctrl Pts',(32.0301831149951,19.6252569369702,43.7159471786975));
#68492=CARTESIAN_POINT('Ctrl Pts',(32.0747404343294,19.6934668590254,43.7201653655225));
#68493=CARTESIAN_POINT('Ctrl Pts',(32.1158073434469,19.7637518309755,43.7243835523476));
#68494=CARTESIAN_POINT('Ctrl Pts',(32.1568606160447,19.8340134643687,43.7286003384978));
#68495=CARTESIAN_POINT('Ctrl Pts',(32.1944255457942,19.9063483783473,43.732817124648));
#68496=CARTESIAN_POINT('Ctrl Pts',(32.2282981000228,19.9803736824529,43.7370339107981));
#68497=CARTESIAN_POINT('Ctrl Pts',(32.2621697754284,20.0543970659728,43.7412505875439));
#68498=CARTESIAN_POINT('Ctrl Pts',(32.2923490733916,20.1301103293388,43.7454672642896));
#68499=CARTESIAN_POINT('Ctrl Pts',(32.3186793550125,20.2071088986255,43.7496839410353));
#68500=CARTESIAN_POINT('Ctrl Pts',(32.3452328349292,20.2847601745446,43.753936361989));
#68501=CARTESIAN_POINT('Ctrl Pts',(32.367871560611,20.3637182022701,43.7581887829428));
#68502=CARTESIAN_POINT('Ctrl Pts',(32.3864861868637,20.4435524014708,43.7624412038965));
#68503=CARTESIAN_POINT('Ctrl Pts',(32.4049710746478,20.5228301797903,43.7666639867273));
#68504=CARTESIAN_POINT('Ctrl Pts',(32.4194877563476,20.6029714819369,43.770886769558));
#68505=CARTESIAN_POINT('Ctrl Pts',(32.4299809185601,20.6835462349192,43.7751095523888));
#68506=CARTESIAN_POINT('Ctrl Pts',(32.4405845521055,20.7649692736884,43.779376792404));
#68507=CARTESIAN_POINT('Ctrl Pts',(32.4470794111771,20.8468344584216,43.7836440324193));
#68508=CARTESIAN_POINT('Ctrl Pts',(32.4494624033538,20.928696531949,43.7879112724345));
#68509=CARTESIAN_POINT('Ctrl Pts',(32.4518453955305,21.0105586054765,43.7921785124497));
#68510=CARTESIAN_POINT('Ctrl Pts',(32.4501165951023,21.0924170865121,43.7964457524649));
#68511=CARTESIAN_POINT('Ctrl Pts',(32.444326595155,21.1738325234752,43.8007129924802));
#68512=CARTESIAN_POINT('Ctrl Pts',(32.4385848805194,21.2545690019261,43.8049446461369));
#68513=CARTESIAN_POINT('Ctrl Pts',(32.4288280197687,21.3351717365329,43.8091762997935));
#68514=CARTESIAN_POINT('Ctrl Pts',(32.415067561655,21.4152094924755,43.8134079534502));
#68515=CARTESIAN_POINT('Ctrl Pts',(32.4013268084274,21.4951326348746,43.8176335474065));
#68516=CARTESIAN_POINT('Ctrl Pts',(32.3835939224315,21.5744919512168,43.8218591413628));
#68517=CARTESIAN_POINT('Ctrl Pts',(32.3619323386008,21.6528597689182,43.8260847353191));
#68518=CARTESIAN_POINT('Ctrl Pts',(32.3402102929162,21.7314463270209,43.8303221237612));
#68519=CARTESIAN_POINT('Ctrl Pts',(32.3145376254357,21.8090353729155,43.8345595122034));
#68520=CARTESIAN_POINT('Ctrl Pts',(32.2850302874115,21.8852044032945,43.8387969006455));
#68521=CARTESIAN_POINT('Ctrl Pts',(32.2556579080544,21.9610250569137,43.843014908407));
#68522=CARTESIAN_POINT('Ctrl Pts',(32.2224860218687,22.0354382173368,43.8472329161685));
#68523=CARTESIAN_POINT('Ctrl Pts',(32.1856788016498,22.1080426102,43.85145092393));
#68524=CARTESIAN_POINT('Ctrl Pts',(32.1488836885224,22.1806231211176,43.8556675442515));
#68525=CARTESIAN_POINT('Ctrl Pts',(32.1084558260338,22.2513956317458,43.8598841645731));
#68526=CARTESIAN_POINT('Ctrl Pts',(32.0646064667045,22.3199812073063,43.8641007848947));
#68527=CARTESIAN_POINT('Ctrl Pts',(32.0207581060368,22.3885652208422,43.8683173091834));
#68528=CARTESIAN_POINT('Ctrl Pts',(31.9734886547699,22.4549620073315,43.8725338334722));
#68529=CARTESIAN_POINT('Ctrl Pts',(31.9230532683568,22.518820719197,43.876750357761));
#68530=CARTESIAN_POINT('Ctrl Pts',(31.8721858686315,22.5832264242669,43.8810029994418));
#68531=CARTESIAN_POINT('Ctrl Pts',(31.8180983200932,22.6450499771179,43.8852556411226));
#68532=CARTESIAN_POINT('Ctrl Pts',(31.7610933379343,22.7039661103096,43.8895082828034));
#68533=CARTESIAN_POINT('Ctrl Pts',(31.7044901900368,22.7624669373302,43.8937309471548));
#68534=CARTESIAN_POINT('Ctrl Pts',(31.6450109930267,22.8181009278192,43.8979536115062));
#68535=CARTESIAN_POINT('Ctrl Pts',(31.5829872353128,22.8705885872732,43.9021762758576));
#68536=CARTESIAN_POINT('Ctrl Pts',(31.5203030036198,22.9236351734122,43.9064439062031));
#68537=CARTESIAN_POINT('Ctrl Pts',(31.4550200838409,22.9734677261952,43.9107115365487));
#68538=CARTESIAN_POINT('Ctrl Pts',(31.3875111489145,23.0198423358366,43.9149791668942));
#68539=CARTESIAN_POINT('Ctrl Pts',(31.3200022139882,23.066216945478,43.9192467972397));
#68540=CARTESIAN_POINT('Ctrl Pts',(31.2502677090293,23.109133413648,43.9235144275852));
#68541=CARTESIAN_POINT('Ctrl Pts',(31.1787045179634,23.1483961248644,43.9277820579308));
#68542=CARTESIAN_POINT('Ctrl Pts',(31.1078303443356,23.1872808108379,43.9320085991118));
#68543=CARTESIAN_POINT('Ctrl Pts',(31.0348951900078,23.2227285053627,43.9362351402929));
#68544=CARTESIAN_POINT('Ctrl Pts',(30.9602666044256,23.2545150916383,43.940461681474));
#68545=CARTESIAN_POINT('Ctrl Pts',(30.8857454103099,23.2862559366194,43.9446821406095));
#68546=CARTESIAN_POINT('Ctrl Pts',(30.8095360495221,23.3143459549914,43.948902599745));
#68547=CARTESIAN_POINT('Ctrl Pts',(30.7320312767652,23.3386065209516,43.9531230588805));
#68548=CARTESIAN_POINT('Ctrl Pts',(30.6541920904257,23.3629717651464,43.9573617282347));
#68549=CARTESIAN_POINT('Ctrl Pts',(30.575046703461,23.3834742016837,43.9616003975889));
#68550=CARTESIAN_POINT('Ctrl Pts',(30.4950139674654,23.399981546182,43.9658390669431));
#68551=CARTESIAN_POINT('Ctrl Pts',(30.4154686292597,23.4163883612766,43.9700519228842));
#68552=CARTESIAN_POINT('Ctrl Pts',(30.3350471806115,23.4288485106995,43.9742647788253));
#68553=CARTESIAN_POINT('Ctrl Pts',(30.2541749284838,23.4372823709473,43.9784776347664));
#68554=CARTESIAN_POINT('Ctrl Pts',(30.1733292166686,23.4457134634065,43.9826891081503));
#68555=CARTESIAN_POINT('Ctrl Pts',(30.0920334583339,23.4501208421543,43.9869005815342));
#68556=CARTESIAN_POINT('Ctrl Pts',(30.0107197320548,23.4504765531106,43.9911120549181));
#68557=CARTESIAN_POINT('Ctrl Pts',(29.9294076336576,23.4508322569456,43.9953234439893));
#68558=CARTESIAN_POINT('Ctrl Pts',(29.8480780341017,23.4471364533416,43.9995348330605));
#68559=CARTESIAN_POINT('Ctrl Pts',(29.7671632146717,23.439413306801,44.0037462221316));
#68560=CARTESIAN_POINT('Ctrl Pts',(29.6853385920691,23.4316033214925,44.0080049639024));
#68561=CARTESIAN_POINT('Ctrl Pts',(29.6039386220286,23.4196748863583,44.0122637056732));
#68562=CARTESIAN_POINT('Ctrl Pts',(29.5234033041919,23.4037066875026,44.016522447444));
#68563=CARTESIAN_POINT('Ctrl Pts',(29.4436458131195,23.3878927128157,44.0207400574056));
#68564=CARTESIAN_POINT('Ctrl Pts',(29.364736785917,23.3681168484542,44.0249576673671));
#68565=CARTESIAN_POINT('Ctrl Pts',(29.287089848896,23.3445062095147,44.0291752773286));
#68566=CARTESIAN_POINT('Ctrl Pts',(29.2083070461721,23.3205501800675,44.0334545850041));
#68567=CARTESIAN_POINT('Ctrl Pts',(29.1308240250191,23.2926464458688,44.0377338926795));
#68568=CARTESIAN_POINT('Ctrl Pts',(29.0550514991216,23.2609782353414,44.0420132003549));
#68569=CARTESIAN_POINT('Ctrl Pts',(28.979278973224,23.229310024814,44.0462925080303));
#68570=CARTESIAN_POINT('Ctrl Pts',(28.9052173589904,23.1938776115835,44.0505718157057));
#68571=CARTESIAN_POINT('Ctrl Pts',(28.8332493702964,23.154911417689,44.0548511233811));
#68572=CARTESIAN_POINT('Ctrl Pts',(28.7619658003649,23.1163157940256,44.0590897346509));
#68573=CARTESIAN_POINT('Ctrl Pts',(28.6924677344914,23.0741080608761,44.0633283459206));
#68574=CARTESIAN_POINT('Ctrl Pts',(28.625144019835,23.0284775778412,44.0675669571904));
#68575=CARTESIAN_POINT('Ctrl Pts',(28.5579170096759,22.9829126389158,44.071799480074));
#68576=CARTESIAN_POINT('Ctrl Pts',(28.4928585273544,22.9339349732179,44.0760320029576));
#68577=CARTESIAN_POINT('Ctrl Pts',(28.4303327142287,22.8817797060175,44.0802645258412));
#68578=CARTESIAN_POINT('Ctrl Pts',(28.3677606663616,22.8295858725807,44.0845001784658));
#68579=CARTESIAN_POINT('Ctrl Pts',(28.3077254335474,22.7742099779915,44.0887358310904));
#68580=CARTESIAN_POINT('Ctrl Pts',(28.2505627290682,22.7159310840109,44.092971483715));
#68581=CARTESIAN_POINT('Ctrl Pts',(28.1935462621439,22.6578012830977,44.0971963004023));
#68582=CARTESIAN_POINT('Ctrl Pts',(28.1393879844096,22.596783633823,44.1014211170895));
#68583=CARTESIAN_POINT('Ctrl Pts',(28.0883864516113,22.5331940162996,44.1056459337768));
#68584=CARTESIAN_POINT('Ctrl Pts',(28.0374023959192,22.4696261895426,44.1098693027121));
#68585=CARTESIAN_POINT('Ctrl Pts',(27.9895732262693,22.4034885060055,44.1140926716474));
#68586=CARTESIAN_POINT('Ctrl Pts',(27.9451577368483,22.3351305267897,44.1183160405828));
#68587=CARTESIAN_POINT('Ctrl Pts',(27.9007439865072,22.2667752241171,44.1225392441529));
#68588=CARTESIAN_POINT('Ctrl Pts',(27.8597439021257,22.1962001875561,44.126762447723));
#68589=CARTESIAN_POINT('Ctrl Pts',(27.8223726012033,22.1237834141906,44.1309856512932));
#68590=CARTESIAN_POINT('Ctrl Pts',(27.7848124509112,22.0510006952556,44.135230196088));
#68591=CARTESIAN_POINT('Ctrl Pts',(27.750918089743,21.9763579869771,44.1394747408829));
#68592=CARTESIAN_POINT('Ctrl Pts',(27.720860061516,21.9002618456911,44.1437192856778));
#68593=CARTESIAN_POINT('Ctrl Pts',(27.690911361364,21.8244424838589,44.1479483920711));
#68594=CARTESIAN_POINT('Ctrl Pts',(27.6647712405932,21.7471807006239,44.1521774984643));
#68595=CARTESIAN_POINT('Ctrl Pts',(27.6425585506347,21.6688946574868,44.1564066048576));
#68596=CARTESIAN_POINT('Ctrl Pts',(27.6202242291552,21.5901799381961,44.1606588688533));
#68597=CARTESIAN_POINT('Ctrl Pts',(27.6018605828103,21.5104301698075,44.164911132849));
#68598=CARTESIAN_POINT('Ctrl Pts',(27.5875361912525,21.4300797850207,44.1691633968447));
#68599=CARTESIAN_POINT('Ctrl Pts',(27.5732117996947,21.3497294002339,44.1734156608404));
#68600=CARTESIAN_POINT('Ctrl Pts',(27.5629266624284,21.2687788724357,44.177667924836));
#68601=CARTESIAN_POINT('Ctrl Pts',(27.5566964741207,21.1876649419204,44.1819201888317));
#68602=CARTESIAN_POINT('Ctrl Pts',(27.5519336184847,21.1256549476737,44.1851709604838));
#68603=CARTESIAN_POINT('Ctrl Pts',(27.5495309641018,21.0634593640365,44.1884217321359));
#68604=CARTESIAN_POINT('Ctrl Pts',(27.5495002973385,21.001207168577,44.1916725037879));
#68605=CARTESIAN_POINT('',(28.3849103233787,19.1570578993166,44.2999992595396));
#68606=CARTESIAN_POINT('Ctrl Pts',(27.549500297338,21.0012071676208,44.1916725038378));
#68607=CARTESIAN_POINT('Ctrl Pts',(27.5494613164988,20.9220776968105,44.1958045965079));
#68608=CARTESIAN_POINT('Ctrl Pts',(27.5532593294191,20.8427755817736,44.1999366891779));
#68609=CARTESIAN_POINT('Ctrl Pts',(27.5609182421575,20.7637153653744,44.2040687818479));
#68610=CARTESIAN_POINT('Ctrl Pts',(27.568565872763,20.6847716103984,44.2081947876462));
#68611=CARTESIAN_POINT('Ctrl Pts',(27.5800630653957,20.6060695276488,44.2123207934445));
#68612=CARTESIAN_POINT('Ctrl Pts',(27.5953817158509,20.5280241981458,44.2164467992429));
#68613=CARTESIAN_POINT('Ctrl Pts',(27.6106878555248,20.4500426084648,44.2205694353216));
#68614=CARTESIAN_POINT('Ctrl Pts',(27.6298091738289,20.3727171850489,44.2246920714003));
#68615=CARTESIAN_POINT('Ctrl Pts',(27.6526658524374,20.2964570733163,44.2288147074791));
#68616=CARTESIAN_POINT('Ctrl Pts',(27.6755115528644,20.2202335897118,44.2329353634343));
#68617=CARTESIAN_POINT('Ctrl Pts',(27.7020889161023,20.1450748694144,44.2370560193895));
#68618=CARTESIAN_POINT('Ctrl Pts',(27.7322676052255,20.0713773448326,44.2411766753447));
#68619=CARTESIAN_POINT('Ctrl Pts',(27.7624419464753,19.9976904379254,44.2452967376329));
#68620=CARTESIAN_POINT('Ctrl Pts',(27.796216397791,19.9254647595421,44.2494167999212));
#68621=CARTESIAN_POINT('Ctrl Pts',(27.8334122084363,19.8550774736048,44.2535368622095));
#68622=CARTESIAN_POINT('Ctrl Pts',(27.8706384784948,19.7846325479659,44.2576602983906));
#68623=CARTESIAN_POINT('Ctrl Pts',(27.9112914753926,19.7160294535448,44.2617837345717));
#68624=CARTESIAN_POINT('Ctrl Pts',(27.9551465739149,19.6496205289519,44.2659071707528));
#68625=CARTESIAN_POINT('Ctrl Pts',(27.9990196432335,19.5831843915309,44.2700322966218));
#68626=CARTESIAN_POINT('Ctrl Pts',(28.046097135931,19.5189446060218,44.2741574224909));
#68627=CARTESIAN_POINT('Ctrl Pts',(28.0961127707103,19.4572220937064,44.2782825483599));
#68628=CARTESIAN_POINT('Ctrl Pts',(28.1462101040697,19.3953987600851,44.2824144124605));
#68629=CARTESIAN_POINT('Ctrl Pts',(28.1992548350109,19.3361012714435,44.2865462765611));
#68630=CARTESIAN_POINT('Ctrl Pts',(28.2549427764082,19.279614712807,44.2906781406616));
#68631=CARTESIAN_POINT('Ctrl Pts',(28.2968184616681,19.2371384909981,44.2937851802876));
#68632=CARTESIAN_POINT('Ctrl Pts',(28.3401879810753,19.1962509880967,44.2968922199136));
#68633=CARTESIAN_POINT('Ctrl Pts',(28.3849103233787,19.1570578993166,44.2999992595396));
#68634=CARTESIAN_POINT('',(27.5495,21.,44.3));
#68635=CARTESIAN_POINT('Origin',(30.,21.,44.3));
#68636=CARTESIAN_POINT('',(27.5535569140831,21.1409484919019,44.3));
#68637=CARTESIAN_POINT('Origin',(30.,21.,44.3));
#68638=CARTESIAN_POINT('',(27.5495009938442,20.9977930044395,43.5073274962121));
#68639=CARTESIAN_POINT('Ctrl Pts',(27.5535569140831,21.1409484919019,44.3));
#68640=CARTESIAN_POINT('Ctrl Pts',(27.6003946584625,21.9539112583056,44.2576897435897));
#68641=CARTESIAN_POINT('Ctrl Pts',(28.5681046611841,23.5154982516648,44.1730692307693));
#68642=CARTESIAN_POINT('Ctrl Pts',(31.3397609818422,23.5691170566576,44.0461384615384));
#68643=CARTESIAN_POINT('Ctrl Pts',(32.8826594919807,21.2691366249369,43.9192076923077));
#68644=CARTESIAN_POINT('Ctrl Pts',(31.792118108548,18.7255142460077,43.792276923077));
#68645=CARTESIAN_POINT('Ctrl Pts',(29.0622776960464,18.2600412506062,43.6653461538461));
#68646=CARTESIAN_POINT('Ctrl Pts',(27.6613697729277,19.7865866467302,43.5703630540116));
#68647=CARTESIAN_POINT('Ctrl Pts',(27.5479559594343,20.7983452768987,43.5176902105872));
#68648=CARTESIAN_POINT('Ctrl Pts',(27.5497643553418,20.9977907903747,43.507327623573));
#68649=CARTESIAN_POINT('',(27.5495000808206,21.0006293661639,42.707327496182));
#68650=CARTESIAN_POINT('Ctrl Pts',(27.5495009938442,20.9977930044395,43.5073274962121));
#68651=CARTESIAN_POINT('Ctrl Pts',(27.5494286713727,21.0780949985435,43.5031556579785));
#68652=CARTESIAN_POINT('Ctrl Pts',(27.5533077961739,21.158500472361,43.498983819745));
#68653=CARTESIAN_POINT('Ctrl Pts',(27.5611421721604,21.2385848813008,43.4948119815114));
#68654=CARTESIAN_POINT('Ctrl Pts',(27.5689715766591,21.3186184707931,43.490642790616));
#68655=CARTESIAN_POINT('Ctrl Pts',(27.5807512071824,21.3983309264438,43.4864735997207));
#68656=CARTESIAN_POINT('Ctrl Pts',(27.5964328306478,21.4772998139662,43.4823044088253));
#68657=CARTESIAN_POINT('Ctrl Pts',(27.6121095754188,21.5562441335559,43.4781365150028));
#68658=CARTESIAN_POINT('Ctrl Pts',(27.6316858108099,21.6344448768983,43.4739686211803));
#68659=CARTESIAN_POINT('Ctrl Pts',(27.6550619445421,21.7114884159741,43.4698007273578));
#68660=CARTESIAN_POINT('Ctrl Pts',(27.678438366853,21.7885329061537,43.4656327820825));
#68661=CARTESIAN_POINT('Ctrl Pts',(27.7056146401583,21.8644197081247,43.4614648368073));
#68662=CARTESIAN_POINT('Ctrl Pts',(27.7364413729418,21.9387505482663,43.4572968915321));
#68663=CARTESIAN_POINT('Ctrl Pts',(27.7672986247002,22.0131549771682,43.4531248199221));
#68664=CARTESIAN_POINT('Ctrl Pts',(27.8018133675902,22.0859999278558,43.4489527483122));
#68665=CARTESIAN_POINT('Ctrl Pts',(27.8397884237585,22.1569080325904,43.4447806767022));
#68666=CARTESIAN_POINT('Ctrl Pts',(27.8777834423162,22.2278534116662,43.4406064119548));
#68667=CARTESIAN_POINT('Ctrl Pts',(27.9192421474788,22.2968595105345,43.4364321472074));
#68668=CARTESIAN_POINT('Ctrl Pts',(27.9639231871326,22.3635767166184,43.43225788246));
#68669=CARTESIAN_POINT('Ctrl Pts',(28.0086803306937,22.430407560167,43.4280765078096));
#68670=CARTESIAN_POINT('Ctrl Pts',(28.0566704805754,22.4949413460911,43.4238951331592));
#68671=CARTESIAN_POINT('Ctrl Pts',(28.1076113994249,22.5568608269249,43.4197137585088));
#68672=CARTESIAN_POINT('Ctrl Pts',(28.1410294454937,22.5974809827798,43.4169707108008));
#68673=CARTESIAN_POINT('Ctrl Pts',(28.1757165693982,22.6369767694273,43.4142276630927));
#68674=CARTESIAN_POINT('Ctrl Pts',(28.2115849037342,22.6752676483024,43.4114846153846));
#68675=CARTESIAN_POINT('Ctrl Pts',(28.2669112616675,22.7343307441901,43.4072535061866));
#68676=CARTESIAN_POINT('Ctrl Pts',(28.325270368973,22.7907608722937,43.4030223969887));
#68677=CARTESIAN_POINT('Ctrl Pts',(28.3863816544145,22.8442304858097,43.3987912877907));
#68678=CARTESIAN_POINT('Ctrl Pts',(28.4474053256908,22.8976234408899,43.3945662446589));
#68679=CARTESIAN_POINT('Ctrl Pts',(28.5111729915882,22.9480640075706,43.390341201527));
#68680=CARTESIAN_POINT('Ctrl Pts',(28.5773660289269,22.995260091905,43.3861161583952));
#68681=CARTESIAN_POINT('Ctrl Pts',(28.6436643454633,23.042531241021,43.3818843953852));
#68682=CARTESIAN_POINT('Ctrl Pts',(28.7123954226579,23.0865472464855,43.3776526323751));
#68683=CARTESIAN_POINT('Ctrl Pts',(28.7832044057296,23.1270540030202,43.373420869365));
#68684=CARTESIAN_POINT('Ctrl Pts',(28.8537738259422,23.1674237160049,43.3692034233696));
#68685=CARTESIAN_POINT('Ctrl Pts',(28.9264067172877,23.2043076417871,43.3649859773742));
#68686=CARTESIAN_POINT('Ctrl Pts',(29.0007228872578,23.2374975981997,43.3607685313787));
#68687=CARTESIAN_POINT('Ctrl Pts',(29.0750145191491,23.2706765957893,43.3565524779204));
#68688=CARTESIAN_POINT('Ctrl Pts',(29.150987901736,23.300163856706,43.352336424462));
#68689=CARTESIAN_POINT('Ctrl Pts',(29.2282403505548,23.3257982056679,43.3481203710036));
#68690=CARTESIAN_POINT('Ctrl Pts',(29.3054909610785,23.3514319446363,43.3439044178702));
#68691=CARTESIAN_POINT('Ctrl Pts',(29.3840201356804,23.3732128085744,43.3396884647369));
#68692=CARTESIAN_POINT('Ctrl Pts',(29.4634087876326,23.3910290924224,43.3354725116035));
#68693=CARTESIAN_POINT('Ctrl Pts',(29.5433109291996,23.4089606128501,43.3312292894827));
#68694=CARTESIAN_POINT('Ctrl Pts',(29.6240832450702,23.4228759621529,43.3269860673619));
#68695=CARTESIAN_POINT('Ctrl Pts',(29.705288575144,23.4327135931012,43.3227428452411));
#68696=CARTESIAN_POINT('Ctrl Pts',(29.7860891322218,23.4425021877689,43.3185207737237));
#68697=CARTESIAN_POINT('Ctrl Pts',(29.8673179250657,23.4482536436492,43.3142987022063));
#68698=CARTESIAN_POINT('Ctrl Pts',(29.9485415435488,23.449959648088,43.3100766306889));
#68699=CARTESIAN_POINT('Ctrl Pts',(30.0303755005355,23.4516784719532,43.3058228332664));
#68700=CARTESIAN_POINT('Ctrl Pts',(30.112203725588,23.449290807471,43.3015690358439));
#68701=CARTESIAN_POINT('Ctrl Pts',(30.1935873294616,23.4428414184862,43.2973152384213));
#68702=CARTESIAN_POINT('Ctrl Pts',(30.2749709333352,23.4363920295015,43.2930614409988));
#68703=CARTESIAN_POINT('Ctrl Pts',(30.3559094524285,23.4258810401938,43.2888076435763));
#68704=CARTESIAN_POINT('Ctrl Pts',(30.4359754457396,23.4114053289964,43.2845538461538));
#68705=CARTESIAN_POINT('Ctrl Pts',(30.5156268278807,23.3970045783573,43.2803220764594));
#68706=CARTESIAN_POINT('Ctrl Pts',(30.5947128374763,23.3786262068457,43.2760903067649));
#68707=CARTESIAN_POINT('Ctrl Pts',(30.672805973043,23.3563281547012,43.2718585370705));
#68708=CARTESIAN_POINT('Ctrl Pts',(30.7507873255897,23.334062020133,43.2676328247585));
#68709=CARTESIAN_POINT('Ctrl Pts',(30.827778183594,23.3078874747667,43.2634071124466));
#68710=CARTESIAN_POINT('Ctrl Pts',(30.9033601775532,23.2779136593846,43.2591814001347));
#68711=CARTESIAN_POINT('Ctrl Pts',(30.9790474227333,23.2478981041582,43.2549498033342));
#68712=CARTESIAN_POINT('Ctrl Pts',(31.053321418879,23.214072790252,43.2507182065337));
#68713=CARTESIAN_POINT('Ctrl Pts',(31.1257762843647,23.1765978056504,43.2464866097332));
#68714=CARTESIAN_POINT('Ctrl Pts',(31.1980005894887,23.1392420710943,43.2422684783982));
#68715=CARTESIAN_POINT('Ctrl Pts',(31.2684169019442,23.0982600572565,43.2380503470632));
#68716=CARTESIAN_POINT('Ctrl Pts',(31.336643916087,23.0538581478738,43.2338322157282));
#68717=CARTESIAN_POINT('Ctrl Pts',(31.4048484800272,23.0094708490068,43.2296154723757));
#68718=CARTESIAN_POINT('Ctrl Pts',(31.4708647870291,22.9616661426764,43.2253987290232));
#68719=CARTESIAN_POINT('Ctrl Pts',(31.5343388049374,22.9106948164642,43.2211819856707));
#68720=CARTESIAN_POINT('Ctrl Pts',(31.5978113671367,22.8597246592251,43.2169653390247));
#68721=CARTESIAN_POINT('Ctrl Pts',(31.6587413944808,22.8055883183896,43.2127486923787));
#68722=CARTESIAN_POINT('Ctrl Pts',(31.7168075005881,22.7485772090258,43.2085320457327));
#68723=CARTESIAN_POINT('Ctrl Pts',(31.7752284416995,22.6912177116162,43.2042896316653));
#68724=CARTESIAN_POINT('Ctrl Pts',(31.8307499903644,22.6309485138542,43.2000472175978));
#68725=CARTESIAN_POINT('Ctrl Pts',(31.8830833737838,22.5681030761335,43.1958048035303));
#68726=CARTESIAN_POINT('Ctrl Pts',(31.9351743937326,22.5055486847277,43.1915820366962));
#68727=CARTESIAN_POINT('Ctrl Pts',(31.9841064758759,22.4404422706323,43.1873592698621));
#68728=CARTESIAN_POINT('Ctrl Pts',(32.0296372758375,22.3731433932882,43.183136503028));
#68729=CARTESIAN_POINT('Ctrl Pts',(32.0754858369806,22.3053748345241,43.1788842653438));
#68730=CARTESIAN_POINT('Ctrl Pts',(32.1178852100249,22.2353835011774,43.1746320276597));
#68731=CARTESIAN_POINT('Ctrl Pts',(32.1566349538099,22.1635617413809,43.1703797899755));
#68732=CARTESIAN_POINT('Ctrl Pts',(32.1953846975949,22.0917399815844,43.1661275522914));
#68733=CARTESIAN_POINT('Ctrl Pts',(32.2304846650877,22.0180882506895,43.1618753146072));
#68734=CARTESIAN_POINT('Ctrl Pts',(32.2617842872632,21.9430175437865,43.1576230769231));
#68735=CARTESIAN_POINT('Ctrl Pts',(32.2929329194873,21.8683089793506,43.1533913521115));
#68736=CARTESIAN_POINT('Ctrl Pts',(32.3204342772004,21.7919158010366,43.1491596272999));
#68737=CARTESIAN_POINT('Ctrl Pts',(32.3441049330204,21.7142284739421,43.1449279024883));
#68738=CARTESIAN_POINT('Ctrl Pts',(32.367741711881,21.636652331364,43.1407022340349));
#68739=CARTESIAN_POINT('Ctrl Pts',(32.3875585431245,21.5577861594449,43.1364765655815));
#68740=CARTESIAN_POINT('Ctrl Pts',(32.4034199553765,21.4780405506839,43.1322508971281));
#68741=CARTESIAN_POINT('Ctrl Pts',(32.4193036618295,21.3981828545116,43.1280192892349));
#68742=CARTESIAN_POINT('Ctrl Pts',(32.4312206572839,21.3174436868484,43.1237876813418));
#68743=CARTESIAN_POINT('Ctrl Pts',(32.4390850326013,21.2362508280205,43.1195560734486));
#68744=CARTESIAN_POINT('Ctrl Pts',(32.4469242857399,21.1553173339147,43.1153379831212));
#68745=CARTESIAN_POINT('Ctrl Pts',(32.4507367093211,21.0739335052662,43.1111198927937));
#68746=CARTESIAN_POINT('Ctrl Pts',(32.4504886192374,20.9925316007048,43.1069018024663));
#68747=CARTESIAN_POINT('Ctrl Pts',(32.4502406107199,20.9111564591811,43.1026850989481));
#68748=CARTESIAN_POINT('Ctrl Pts',(32.445934741115,20.82976371797,43.0984683954298));
#68749=CARTESIAN_POINT('Ctrl Pts',(32.4375894233738,20.7487868374147,43.0942516919116));
#68750=CARTESIAN_POINT('Ctrl Pts',(32.4292442945833,20.6678117902988,43.0900350838659));
#68751=CARTESIAN_POINT('Ctrl Pts',(32.4168599482741,20.5872530473404,43.0858184758203));
#68752=CARTESIAN_POINT('Ctrl Pts',(32.4005066395469,20.5075387086366,43.0816018677746));
#68753=CARTESIAN_POINT('Ctrl Pts',(32.3840530559995,20.4273355794922,43.0773594044344));
#68754=CARTESIAN_POINT('Ctrl Pts',(32.3635817510493,20.3479877143646,43.0731169410942));
#68755=CARTESIAN_POINT('Ctrl Pts',(32.3392160031704,20.2699186754126,43.068874477754));
#68756=CARTESIAN_POINT('Ctrl Pts',(32.314963580141,20.1922127347789,43.0646517460684));
#68757=CARTESIAN_POINT('Ctrl Pts',(32.2868530740405,20.1157741716784,43.0604290143827));
#68758=CARTESIAN_POINT('Ctrl Pts',(32.2550548796411,20.0410016997893,43.056206282697));
#68759=CARTESIAN_POINT('Ctrl Pts',(32.223033809021,19.9657051413519,43.0519539535296));
#68760=CARTESIAN_POINT('Ctrl Pts',(32.1872733645652,19.8920985502412,43.0477016243621));
#68761=CARTESIAN_POINT('Ctrl Pts',(32.1479942456607,19.8205632824909,43.0434492951947));
#68762=CARTESIAN_POINT('Ctrl Pts',(32.1087151267562,19.7490280147407,43.0391969660272));
#68763=CARTESIAN_POINT('Ctrl Pts',(32.0659176360555,19.6795644410844,43.0349446368598));
#68764=CARTESIAN_POINT('Ctrl Pts',(32.0198652116927,19.6125221527557,43.0306923076923));
#68765=CARTESIAN_POINT('Ctrl Pts',(31.9740374401133,19.545806909895,43.0264607222229));
#68766=CARTESIAN_POINT('Ctrl Pts',(31.9248150219584,19.4812398037033,43.0222291367535));
#68767=CARTESIAN_POINT('Ctrl Pts',(31.8724262453245,19.4191868529709,43.017997551284));
#68768=CARTESIAN_POINT('Ctrl Pts',(31.8201124824235,19.3572227537783,43.01377202488));
#68769=CARTESIAN_POINT('Ctrl Pts',(31.7646416629189,19.2977660124396,43.0095464984759));
#68770=CARTESIAN_POINT('Ctrl Pts',(31.7062850155279,19.2411533052068,43.0053209720718));
#68771=CARTESIAN_POINT('Ctrl Pts',(31.6478438939406,19.1844586482192,43.0010893290047));
#68772=CARTESIAN_POINT('Ctrl Pts',(31.5865088627317,19.130616642487,42.9968576859376));
#68773=CARTESIAN_POINT('Ctrl Pts',(31.5225925351889,19.0799317142906,42.9926260428705));
#68774=CARTESIAN_POINT('Ctrl Pts',(31.4588831426806,19.029410883247,42.9884081001401));
#68775=CARTESIAN_POINT('Ctrl Pts',(31.3926094975944,18.9820270212694,42.9841901574096));
#68776=CARTESIAN_POINT('Ctrl Pts',(31.3241162903053,18.9380430897451,42.9799722146792));
#68777=CARTESIAN_POINT('Ctrl Pts',(31.2556456313987,18.8940736379998,42.9757556605212));
#68778=CARTESIAN_POINT('Ctrl Pts',(31.1849572521773,18.8535021449235,42.9715391063633));
#68779=CARTESIAN_POINT('Ctrl Pts',(31.1124251378782,18.8165484748645,42.9673225522054));
#68780=CARTESIAN_POINT('Ctrl Pts',(31.0398946927739,18.779595655227,42.9631060950838));
#68781=CARTESIAN_POINT('Ctrl Pts',(30.9655210116341,18.7462607030743,42.9588896379622));
#68782=CARTESIAN_POINT('Ctrl Pts',(30.8897017252006,18.7167170367703,42.9546731808406));
#68783=CARTESIAN_POINT('Ctrl Pts',(30.8134116811143,18.6869899355164,42.9504305439756));
#68784=CARTESIAN_POINT('Ctrl Pts',(30.7356584561104,18.6611015497436,42.9461879071107));
#68785=CARTESIAN_POINT('Ctrl Pts',(30.6568647556537,18.6391783331264,42.9419452702458));
#68786=CARTESIAN_POINT('Ctrl Pts',(30.57844357748,18.6173587654894,42.9377226917962));
#68787=CARTESIAN_POINT('Ctrl Pts',(30.4989922097044,18.5994670063165,42.9335001133467));
#68788=CARTESIAN_POINT('Ctrl Pts',(30.418937973609,18.585576419874,42.9292775348971));
#68789=CARTESIAN_POINT('Ctrl Pts',(30.338313317874,18.5715868572411,42.9250248688245));
#68790=CARTESIAN_POINT('Ctrl Pts',(30.2570776437222,18.5616557699678,42.9207722027519));
#68791=CARTESIAN_POINT('Ctrl Pts',(30.1756711583688,18.5558048576029,42.9165195366793));
#68792=CARTESIAN_POINT('Ctrl Pts',(30.0942646730153,18.5499539452381,42.9122668706067));
#68793=CARTESIAN_POINT('Ctrl Pts',(30.0126878524215,18.5481831548462,42.9080142045341));
#68794=CARTESIAN_POINT('Ctrl Pts',(29.931377428188,18.5504610244705,42.9037615384615));
#68795=CARTESIAN_POINT('Ctrl Pts',(29.8504684104,18.5527276489002,42.8995298665922));
#68796=CARTESIAN_POINT('Ctrl Pts',(29.7695205115425,18.5590114931233,42.8952981947228));
#68797=CARTESIAN_POINT('Ctrl Pts',(29.6889650674848,18.5693195354479,42.8910665228535));
#68798=CARTESIAN_POINT('Ctrl Pts',(29.6085249427001,18.5796128212783,42.8868409088407));
#68799=CARTESIAN_POINT('Ctrl Pts',(29.5284766140614,18.5939188051355,42.8826152948279));
#68800=CARTESIAN_POINT('Ctrl Pts',(29.4492500856818,18.6121924738626,42.8783896808151));
#68801=CARTESIAN_POINT('Ctrl Pts',(29.3699109256761,18.6304921211737,42.8741580594991));
#68802=CARTESIAN_POINT('Ctrl Pts',(29.291396372574,18.6527707129078,42.869926438183));
#68803=CARTESIAN_POINT('Ctrl Pts',(29.2141317794757,18.6789309812136,42.865694816867));
#68804=CARTESIAN_POINT('Ctrl Pts',(29.1371153003262,18.7050072430268,42.8614767842368));
#68805=CARTESIAN_POINT('Ctrl Pts',(29.0613412126541,18.7349401559119,42.8572587516065));
#68806=CARTESIAN_POINT('Ctrl Pts',(28.9872174939851,18.7685829960516,42.8530407189762));
#68807=CARTESIAN_POINT('Ctrl Pts',(28.913118165142,18.8022147662796,42.8488240742564));
#68808=CARTESIAN_POINT('Ctrl Pts',(28.8406685498018,18.8395538475973,42.8446074295365));
#68809=CARTESIAN_POINT('Ctrl Pts',(28.770256335599,18.8804055175894,42.8403907848167));
#68810=CARTESIAN_POINT('Ctrl Pts',(28.6998457327647,18.9212562526996,42.8361742365938));
#68811=CARTESIAN_POINT('Ctrl Pts',(28.6314728398337,18.9656191824287,42.831957688371));
#68812=CARTESIAN_POINT('Ctrl Pts',(28.5654991754205,19.0132545119516,42.8277411401482));
#68813=CARTESIAN_POINT('Ctrl Pts',(28.4991189763304,19.061183373954,42.8234986092384));
#68814=CARTESIAN_POINT('Ctrl Pts',(28.4351680702968,19.1124248375287,42.8192560783286));
#68815=CARTESIAN_POINT('Ctrl Pts',(28.3739821015297,19.1666925942837,42.8150135474188));
#68816=CARTESIAN_POINT('Ctrl Pts',(28.3130825684725,19.2207063022144,42.8107908774735));
#68817=CARTESIAN_POINT('Ctrl Pts',(28.2549224384151,19.277717663908,42.8065682075282));
#68818=CARTESIAN_POINT('Ctrl Pts',(28.1997953246124,19.3374076336298,42.8023455375829));
#68819=CARTESIAN_POINT('Ctrl Pts',(28.1442792823603,19.3975187233008,42.7980930761909));
#68820=CARTESIAN_POINT('Ctrl Pts',(28.0918395262494,19.4603459967167,42.7938406147989));
#68821=CARTESIAN_POINT('Ctrl Pts',(28.0427332253885,19.5255316134274,42.7895881534068));
#68822=CARTESIAN_POINT('Ctrl Pts',(27.9936269245276,19.5907172301381,42.7853356920148));
#68823=CARTESIAN_POINT('Ctrl Pts',(27.9478542927836,19.6582607618668,42.7810832306228));
#68824=CARTESIAN_POINT('Ctrl Pts',(27.9056259808701,19.7277784320356,42.7768307692308));
#68825=CARTESIAN_POINT('Ctrl Pts',(27.8622815994516,19.7991334134351,42.7724659177794));
#68826=CARTESIAN_POINT('Ctrl Pts',(27.8225174834268,19.872820964484,42.7681010663281));
#68827=CARTESIAN_POINT('Ctrl Pts',(27.7865834615437,19.948459474253,42.7637362148767));
#68828=CARTESIAN_POINT('Ctrl Pts',(27.7507120037736,20.0239662911021,42.7593789629938));
#68829=CARTESIAN_POINT('Ctrl Pts',(27.7186575600616,20.1014169309921,42.7550217111109));
#68830=CARTESIAN_POINT('Ctrl Pts',(27.6906253887226,20.1804030534542,42.750664459228));
#68831=CARTESIAN_POINT('Ctrl Pts',(27.6626474697683,20.2592363092169,42.7463156402026));
#68832=CARTESIAN_POINT('Ctrl Pts',(27.6386764648641,20.3395987325073,42.7419668211772));
#68833=CARTESIAN_POINT('Ctrl Pts',(27.6188700035032,20.4210611519486,42.7376180021518));
#68834=CARTESIAN_POINT('Ctrl Pts',(27.5990863563522,20.5024297383373,42.7332741923437));
#68835=CARTESIAN_POINT('Ctrl Pts',(27.5834578152745,20.5848953908551,42.7289303825357));
#68836=CARTESIAN_POINT('Ctrl Pts',(27.5720924813575,20.668013056101,42.7245865727276));
#68837=CARTESIAN_POINT('Ctrl Pts',(27.5607401778493,20.7510354265526,42.7202477431179));
#68838=CARTESIAN_POINT('Ctrl Pts',(27.5536414091132,20.8347079019049,42.7159089135083));
#68839=CARTESIAN_POINT('Ctrl Pts',(27.5508531415515,20.9185757053959,42.7115700838986));
#68840=CARTESIAN_POINT('Ctrl Pts',(27.5499443350539,20.9459115342094,42.7101558880031));
#68841=CARTESIAN_POINT('Ctrl Pts',(27.549493053573,20.9732680513757,42.7087416921076));
#68842=CARTESIAN_POINT('Ctrl Pts',(27.5495000808205,21.0006293655811,42.7073274962121));
#68843=CARTESIAN_POINT('',(27.5495007121296,21.0018681933898,41.907327496261));
#68844=CARTESIAN_POINT('Ctrl Pts',(27.5495000808206,21.0006293661639,42.707327496182));
#68845=CARTESIAN_POINT('Ctrl Pts',(27.5495225090421,21.0879558832018,42.7028139409837));
#68846=CARTESIAN_POINT('Ctrl Pts',(27.554217143938,21.1751558760659,42.6983003857854));
#68847=CARTESIAN_POINT('Ctrl Pts',(27.5635183022074,21.2617387749678,42.6937868305871));
#68848=CARTESIAN_POINT('Ctrl Pts',(27.5728554788347,21.3486569626314,42.6892557968295));
#68849=CARTESIAN_POINT('Ctrl Pts',(27.5868348224921,21.4349529215464,42.6847247630719));
#68850=CARTESIAN_POINT('Ctrl Pts',(27.6053392195364,21.5201442074171,42.6801937293143));
#68851=CARTESIAN_POINT('Ctrl Pts',(27.6238820452469,21.6055124127238,42.6756532858157));
#68852=CARTESIAN_POINT('Ctrl Pts',(27.6469685873783,21.6897710242904,42.6711128423172));
#68853=CARTESIAN_POINT('Ctrl Pts',(27.6744321572847,21.7724535318893,42.6665723988186));
#68854=CARTESIAN_POINT('Ctrl Pts',(27.701978129605,21.8553841222485,42.6620183320544));
#68855=CARTESIAN_POINT('Ctrl Pts',(27.7339272591392,21.9367288224191,42.6574642652903));
#68856=CARTESIAN_POINT('Ctrl Pts',(27.770064716571,22.0160407874285,42.6529101985262));
#68857=CARTESIAN_POINT('Ctrl Pts',(27.7780268982673,22.033515627137,42.6519067990175));
#68858=CARTESIAN_POINT('Ctrl Pts',(27.7861922314723,22.0508918886417,42.6509033995088));
#68859=CARTESIAN_POINT('Ctrl Pts',(27.7945581291948,22.0681649706386,42.6499000000001));
#68860=CARTESIAN_POINT('Ctrl Pts',(27.8298396974189,22.1410108792463,42.645668355125));
#68861=CARTESIAN_POINT('Ctrl Pts',(27.868800287091,22.2122431200328,42.64143671025));
#68862=CARTESIAN_POINT('Ctrl Pts',(27.9112691944474,22.2814655172635,42.637205065375));
#68863=CARTESIAN_POINT('Ctrl Pts',(27.9536773020586,22.3505888136608,42.632979478648));
#68864=CARTESIAN_POINT('Ctrl Pts',(27.9995835109626,22.4177075883245,42.6287538919211));
#68865=CARTESIAN_POINT('Ctrl Pts',(28.0487702554109,22.4824482229848,42.6245283051941));
#68866=CARTESIAN_POINT('Ctrl Pts',(28.0980273227617,22.5472814181385,42.6202966770931));
#68867=CARTESIAN_POINT('Ctrl Pts',(28.1505740934964,22.6097292533655,42.6160650489921));
#68868=CARTESIAN_POINT('Ctrl Pts',(28.2061472559131,22.6694437943614,42.611833420891));
#68869=CARTESIAN_POINT('Ctrl Pts',(28.2615415066392,22.7289660909534,42.6076154160517));
#68870=CARTESIAN_POINT('Ctrl Pts',(28.3199423871311,22.7857723127494,42.6033974112124));
#68871=CARTESIAN_POINT('Ctrl Pts',(28.3810486282775,22.8395506804646,42.5991794063731));
#68872=CARTESIAN_POINT('Ctrl Pts',(28.4421347609133,22.8933113510861,42.594962789572));
#68873=CARTESIAN_POINT('Ctrl Pts',(28.5059241375879,22.9440458394996,42.5907461727709));
#68874=CARTESIAN_POINT('Ctrl Pts',(28.5720800508865,22.9914805720679,42.5865295559697));
#68875=CARTESIAN_POINT('Ctrl Pts',(28.6382344488063,23.0389142180879,42.5823130357552));
#68876=CARTESIAN_POINT('Ctrl Pts',(28.7067548971705,23.0830479886162,42.5780965155406));
#68877=CARTESIAN_POINT('Ctrl Pts',(28.777274332073,23.1236506753683,42.573879995326));
#68878=CARTESIAN_POINT('Ctrl Pts',(28.8482293329644,23.1645041461694,42.569637431613));
#68879=CARTESIAN_POINT('Ctrl Pts',(28.9212076942577,23.2017825127837,42.5653948678999));
#68880=CARTESIAN_POINT('Ctrl Pts',(28.9958105432727,23.2352972475708,42.5611523041868));
#68881=CARTESIAN_POINT('Ctrl Pts',(29.0700630814104,23.2686546079909,42.5569296621823));
#68882=CARTESIAN_POINT('Ctrl Pts',(29.145924428273,23.2982834848223,42.5527070201778));
#68883=CARTESIAN_POINT('Ctrl Pts',(29.2229831312913,23.3240471242516,42.5484843781733));
#68884=CARTESIAN_POINT('Ctrl Pts',(29.3005871591401,23.3499930864006,42.544231853606));
#68885=CARTESIAN_POINT('Ctrl Pts',(29.3794050952921,23.3720187619487,42.5399793290386));
#68886=CARTESIAN_POINT('Ctrl Pts',(29.4590050457112,23.3900365498113,42.5357268044713));
#68887=CARTESIAN_POINT('Ctrl Pts',(29.5386049961303,23.4080543376739,42.5314742799039));
#68888=CARTESIAN_POINT('Ctrl Pts',(29.6189864824365,23.4220642186554,42.5272217553366));
#68889=CARTESIAN_POINT('Ctrl Pts',(29.6997130576233,23.4320316614382,42.5229692307692));
#68890=CARTESIAN_POINT('Ctrl Pts',(29.7800434783921,23.4419501903846,42.5187375748736));
#68891=CARTESIAN_POINT('Ctrl Pts',(29.8610160728231,23.44790300105,42.5145059189779));
#68892=CARTESIAN_POINT('Ctrl Pts',(29.9422054559273,23.4498183689154,42.5102742630823));
#68893=CARTESIAN_POINT('Ctrl Pts',(30.0232786093278,23.4517309947643,42.5060486651722));
#68894=CARTESIAN_POINT('Ctrl Pts',(30.1045674742399,23.4496176464594,42.5018230672621));
#68895=CARTESIAN_POINT('Ctrl Pts',(30.1856401684111,23.4434582005576,42.4975974693521));
#68896=CARTESIAN_POINT('Ctrl Pts',(30.2668285051076,23.4372899687893,42.4933658440265));
#68897=CARTESIAN_POINT('Ctrl Pts',(30.3477995863987,23.4270640473758,42.4891342187009));
#68898=CARTESIAN_POINT('Ctrl Pts',(30.4281182685965,23.4128126736433,42.4849025933753));
#68899=CARTESIAN_POINT('Ctrl Pts',(30.5081786443274,23.39860713261,42.4806845770403));
#68900=CARTESIAN_POINT('Ctrl Pts',(30.5875903487649,23.3804020565635,42.4764665607053));
#68901=CARTESIAN_POINT('Ctrl Pts',(30.6659279899837,23.3582811881021,42.4722485443703));
#68902=CARTESIAN_POINT('Ctrl Pts',(30.7442398540569,23.3361675985534,42.4680319159814));
#68903=CARTESIAN_POINT('Ctrl Pts',(30.8214779098029,23.3101409016125,42.4638152875924));
#68904=CARTESIAN_POINT('Ctrl Pts',(30.8972296111156,23.2803353426497,42.4595986592035));
#68905=CARTESIAN_POINT('Ctrl Pts',(30.9729795786242,23.2505304658763,42.4553821273247));
#68906=CARTESIAN_POINT('Ctrl Pts',(31.0472428272243,23.2169470702818,42.4511655954459));
#68907=CARTESIAN_POINT('Ctrl Pts',(31.1196259088075,23.1797678945996,42.4469490635671));
#68908=CARTESIAN_POINT('Ctrl Pts',(31.1924556332908,23.1423593032239,42.442706513398));
#68909=CARTESIAN_POINT('Ctrl Pts',(31.2633814775535,23.1013106072616,42.438463963229));
#68910=CARTESIAN_POINT('Ctrl Pts',(31.3320285743873,23.0568544253339,42.4342214130599));
#68911=CARTESIAN_POINT('Ctrl Pts',(31.4003537345997,23.0126067310725,42.4299987593225));
#68912=CARTESIAN_POINT('Ctrl Pts',(31.4664211256126,22.9649837593646,42.4257761055851));
#68913=CARTESIAN_POINT('Ctrl Pts',(31.5298925234446,22.9142568053185,42.4215534518476));
#68914=CARTESIAN_POINT('Ctrl Pts',(31.5938125210454,22.8631713260054,42.4173009534628));
#68915=CARTESIAN_POINT('Ctrl Pts',(31.6550993282679,22.8089381338788,42.4130484550779));
#68916=CARTESIAN_POINT('Ctrl Pts',(31.7134449099166,22.7518723671207,42.408795956693));
#68917=CARTESIAN_POINT('Ctrl Pts',(31.7717904915653,22.6948066003625,42.4045434583082));
#68918=CARTESIAN_POINT('Ctrl Pts',(31.8271945718215,22.6349086502739,42.4002909599233));
#68919=CARTESIAN_POINT('Ctrl Pts',(31.8793912100242,22.5725262890279,42.3960384615384));
#68920=CARTESIAN_POINT('Ctrl Pts',(31.9313319922345,22.510449711861,42.3918068079289));
#68921=CARTESIAN_POINT('Ctrl Pts',(31.9802910094292,22.4456808587614,42.3875751543193));
#68922=CARTESIAN_POINT('Ctrl Pts',(32.025977086745,22.3785380277614,42.3833435007097));
#68923=CARTESIAN_POINT('Ctrl Pts',(32.0715977602865,22.3114913178299,42.3791179050971));
#68924=CARTESIAN_POINT('Ctrl Pts',(32.1139545405212,22.2420777609168,42.3748923094845));
#68925=CARTESIAN_POINT('Ctrl Pts',(32.1527960597098,22.1706491256127,42.3706667138719));
#68926=CARTESIAN_POINT('Ctrl Pts',(32.1916930090643,22.0991185555445,42.3664350879734));
#68927=CARTESIAN_POINT('Ctrl Pts',(32.2270643687437,22.0255675219382,42.3622034620749));
#68928=CARTESIAN_POINT('Ctrl Pts',(32.2587009724443,21.9503789597203,42.3579718361764));
#68929=CARTESIAN_POINT('Ctrl Pts',(32.2902358106805,21.8754322565538,42.3537538221491));
#68930=CARTESIAN_POINT('Ctrl Pts',(32.3180596871435,21.7988589668682,42.3495358081218));
#68931=CARTESIAN_POINT('Ctrl Pts',(32.3420119842269,21.721061797447,42.3453177940945));
#68932=CARTESIAN_POINT('Ctrl Pts',(32.3659563997663,21.6432902273167,42.3411011680118));
#68933=CARTESIAN_POINT('Ctrl Pts',(32.3860316291797,21.5642960210873,42.3368845419292));
#68934=CARTESIAN_POINT('Ctrl Pts',(32.4021264409799,21.4844985155242,42.3326679158466));
#68935=CARTESIAN_POINT('Ctrl Pts',(32.4182208844196,21.4047028362795,42.3284513862695));
#68936=CARTESIAN_POINT('Ctrl Pts',(32.4303350005836,21.3241043501087,42.3242348566925));
#68937=CARTESIAN_POINT('Ctrl Pts',(32.4384086509051,21.2431326822768,42.3200183271154));
#68938=CARTESIAN_POINT('Ctrl Pts',(32.446532129696,21.1616612783767,42.3157757742147));
#68939=CARTESIAN_POINT('Ctrl Pts',(32.4505650354488,21.0798125425336,42.3115332213141));
#68940=CARTESIAN_POINT('Ctrl Pts',(32.450499206192,20.9980275770685,42.3072906684135));
#68941=CARTESIAN_POINT('Ctrl Pts',(32.4504336857344,20.9166262574379,42.3030680169426));
#68942=CARTESIAN_POINT('Ctrl Pts',(32.446307877626,20.8352885765009,42.2988453654717));
#68943=CARTESIAN_POINT('Ctrl Pts',(32.4381659939532,20.7544458594729,42.2946227140009));
#68944=CARTESIAN_POINT('Ctrl Pts',(32.4299665510215,20.6730316227487,42.2903702103854));
#68945=CARTESIAN_POINT('Ctrl Pts',(32.4176940990985,20.5921198486564,42.2861177067698));
#68946=CARTESIAN_POINT('Ctrl Pts',(32.4014460596138,20.5121403144701,42.2818652031543));
#68947=CARTESIAN_POINT('Ctrl Pts',(32.3851980201291,20.4321607802837,42.2776126995387));
#68948=CARTESIAN_POINT('Ctrl Pts',(32.3649745719575,20.3531139300766,42.2733601959232));
#68949=CARTESIAN_POINT('Ctrl Pts',(32.3409233958904,20.2754119069616,42.2691076923077));
#68950=CARTESIAN_POINT('Ctrl Pts',(32.3169901510793,20.1980908838092,42.2648760401919));
#68951=CARTESIAN_POINT('Ctrl Pts',(32.2891771448335,20.1218123082809,42.2606443880762));
#68952=CARTESIAN_POINT('Ctrl Pts',(32.257593604598,20.0469935118384,42.2564127359604));
#68953=CARTESIAN_POINT('Ctrl Pts',(32.226055279343,19.9722818259475,42.2521871418757));
#68954=CARTESIAN_POINT('Ctrl Pts',(32.1907573200585,19.8990261931905,42.247961547791));
#68955=CARTESIAN_POINT('Ctrl Pts',(32.1518586739458,19.8276286862242,42.2437359537063));
#68956=CARTESIAN_POINT('Ctrl Pts',(32.1129044985799,19.7561292566814,42.2395043274301));
#68957=CARTESIAN_POINT('Ctrl Pts',(32.070339503299,19.6864937049849,42.2352727011539));
#68958=CARTESIAN_POINT('Ctrl Pts',(32.0243717201438,19.6191055838038,42.2310410748776));
#68959=CARTESIAN_POINT('Ctrl Pts',(31.9785518230268,19.5519342614669,42.2268230624501));
#68960=CARTESIAN_POINT('Ctrl Pts',(31.9293512482011,19.4869963256597,42.2226050500226));
#68961=CARTESIAN_POINT('Ctrl Pts',(31.877020988831,19.4246452915334,42.2183870375951));
#68962=CARTESIAN_POINT('Ctrl Pts',(31.8247079491204,19.3623147744768,42.2141704131358));
#68963=CARTESIAN_POINT('Ctrl Pts',(31.7692675685974,19.3025698243909,42.2099537886765));
#68964=CARTESIAN_POINT('Ctrl Pts',(31.7109916179181,19.245731510454,42.2057371642172));
#68965=CARTESIAN_POINT('Ctrl Pts',(31.6527170012917,19.1888944976596,42.2015206362849));
#68966=CARTESIAN_POINT('Ctrl Pts',(31.5916072771051,19.134964312447,42.1973041083526));
#68967=CARTESIAN_POINT('Ctrl Pts',(31.5279905945585,19.0842247018659,42.1930875804203));
#68968=CARTESIAN_POINT('Ctrl Pts',(31.463981233096,19.0331718970961,42.1888450256417));
#68969=CARTESIAN_POINT('Ctrl Pts',(31.3974342205449,18.9853494990763,42.184602470863));
#68970=CARTESIAN_POINT('Ctrl Pts',(31.3287155634666,18.9410038364772,42.1803599160844));
#68971=CARTESIAN_POINT('Ctrl Pts',(31.260319316858,18.8968662324537,42.1761372662943));
#68972=CARTESIAN_POINT('Ctrl Pts',(31.1897721917849,18.8561729984999,42.1719146165042));
#68973=CARTESIAN_POINT('Ctrl Pts',(31.1174604169032,18.8191211710289,42.1676919667141));
#68974=CARTESIAN_POINT('Ctrl Pts',(31.044637340427,18.781807357754,42.1634394594412));
#68975=CARTESIAN_POINT('Ctrl Pts',(30.9700249980049,18.7481868438762,42.1591869521684));
#68976=CARTESIAN_POINT('Ctrl Pts',(30.8940372071709,18.7184111408507,42.1549344448955));
#68977=CARTESIAN_POINT('Ctrl Pts',(30.8180494163369,18.6886354378252,42.1506819376227));
#68978=CARTESIAN_POINT('Ctrl Pts',(30.7406866471373,18.6627046365206,42.1464294303498));
#68979=CARTESIAN_POINT('Ctrl Pts',(30.6623751937441,18.6407184668394,42.142176923077));
#68980=CARTESIAN_POINT('Ctrl Pts',(30.5844477702936,18.6188401146884,42.137945269588));
#68981=CARTESIAN_POINT('Ctrl Pts',(30.5052894772563,18.6007859263887,42.133713616099));
#68982=CARTESIAN_POINT('Ctrl Pts',(30.4253100886864,18.5866907412307,42.12948196261));
#68983=CARTESIAN_POINT('Ctrl Pts',(30.3454451981305,18.5726157346555,42.1252563671308));
#68984=CARTESIAN_POINT('Ctrl Pts',(30.2647620005521,18.5624885546738,42.1210307716517));
#68985=CARTESIAN_POINT('Ctrl Pts',(30.1836844484152,18.5563940020105,42.1168051761725));
#68986=CARTESIAN_POINT('Ctrl Pts',(30.1024911885124,18.5502907516614,42.1125735502422));
#68987=CARTESIAN_POINT('Ctrl Pts',(30.0209029037114,18.5482317578359,42.108341924312));
#68988=CARTESIAN_POINT('Ctrl Pts',(29.9393546409158,18.5502505453778,42.1041102983817));
#68989=CARTESIAN_POINT('Ctrl Pts',(29.8580686981897,18.5522628389925,42.0998922845183));
#68990=CARTESIAN_POINT('Ctrl Pts',(29.7768229869487,18.5583267248655,42.095674270655));
#68991=CARTESIAN_POINT('Ctrl Pts',(29.6960506526685,18.5684233418918,42.0914562567916));
#68992=CARTESIAN_POINT('Ctrl Pts',(29.6153048968771,18.5785166365822,42.0872396308841));
#68993=CARTESIAN_POINT('Ctrl Pts',(29.535032669569,18.5926399695743,42.0830230049766));
#68994=CARTESIAN_POINT('Ctrl Pts',(29.4556620061474,18.6107226200274,42.0788063790691));
#68995=CARTESIAN_POINT('Ctrl Pts',(29.3762931594821,18.6288048565774,42.0745898496781));
#68996=CARTESIAN_POINT('Ctrl Pts',(29.2978262886152,18.6508461260489,42.0703733202871));
#68997=CARTESIAN_POINT('Ctrl Pts',(29.2206778357139,18.6767248948408,42.0661567908961));
#68998=CARTESIAN_POINT('Ctrl Pts',(29.1430532357876,18.702763382957,42.0619142378086));
#68999=CARTESIAN_POINT('Ctrl Pts',(29.0667638397788,18.732686765123,42.0576716847211));
#69000=CARTESIAN_POINT('Ctrl Pts',(28.9922152177433,18.7663214012191,42.0534291316336));
#69001=CARTESIAN_POINT('Ctrl Pts',(28.918016303495,18.7997982571465,42.0492064803741));
#69002=CARTESIAN_POINT('Ctrl Pts',(28.8455422592944,18.8369513621315,42.0449838291146));
#69003=CARTESIAN_POINT('Ctrl Pts',(28.7751682390831,18.8775633325234,42.0407611778551));
#69004=CARTESIAN_POINT('Ctrl Pts',(28.7042966979216,18.9184624160579,42.0365086738536));
#69005=CARTESIAN_POINT('Ctrl Pts',(28.6355553915385,18.9628692023489,42.0322561698521));
#69006=CARTESIAN_POINT('Ctrl Pts',(28.5692962188833,19.010518424137,42.0280036658506));
#69007=CARTESIAN_POINT('Ctrl Pts',(28.5030370462281,19.058167645925,42.0237511618491));
#69008=CARTESIAN_POINT('Ctrl Pts',(28.4392603387971,19.1090589578006,42.0194986578476));
#69009=CARTESIAN_POINT('Ctrl Pts',(28.378281283189,19.162888502691,42.0152461538461));
#69010=CARTESIAN_POINT('Ctrl Pts',(28.3184922830461,19.2156675205858,42.0110766408909));
#69011=CARTESIAN_POINT('Ctrl Pts',(28.2611548731725,19.2714813445731,42.0069071279358));
#69012=CARTESIAN_POINT('Ctrl Pts',(28.2065999168397,19.3300699440634,42.0027376149806));
#69013=CARTESIAN_POINT('Ctrl Pts',(28.152135917368,19.3885608615929,41.9985750536543));
#69014=CARTESIAN_POINT('Ctrl Pts',(28.1004454793629,19.4498170163631,41.994412492328));
#69015=CARTESIAN_POINT('Ctrl Pts',(28.0518254290861,19.5135390717397,41.9902499310017));
#69016=CARTESIAN_POINT('Ctrl Pts',(28.0032509230386,19.5772014362711,41.9860912689031));
#69017=CARTESIAN_POINT('Ctrl Pts',(27.957741390077,19.6433247413285,41.9819326068045));
#69018=CARTESIAN_POINT('Ctrl Pts',(27.9155551164059,19.7115746908499,41.9777739447059));
#69019=CARTESIAN_POINT('Ctrl Pts',(27.8733945481879,19.7797830534824,41.9736178166139));
#69020=CARTESIAN_POINT('Ctrl Pts',(27.8345534731361,19.8501150825003,41.9694616885218));
#69021=CARTESIAN_POINT('Ctrl Pts',(27.7992473896177,19.9222067926103,41.9653055604298));
#69022=CARTESIAN_POINT('Ctrl Pts',(27.7639512633416,19.9942781709655,41.961150604475));
#69023=CARTESIAN_POINT('Ctrl Pts',(27.7321883591814,20.0681078141059,41.9569956485201));
#69024=CARTESIAN_POINT('Ctrl Pts',(27.7041278797455,20.1433078397475,41.9528406925653));
#69025=CARTESIAN_POINT('Ctrl Pts',(27.6760519557122,20.2185492557767,41.9486834497066));
#69026=CARTESIAN_POINT('Ctrl Pts',(27.6516826987285,20.2951621122091,41.9445262068478));
#69027=CARTESIAN_POINT('Ctrl Pts',(27.6311404814675,20.3727402201176,41.940368963989));
#69028=CARTESIAN_POINT('Ctrl Pts',(27.6105925262874,20.4503399973964,41.9362105599156));
#69029=CARTESIAN_POINT('Ctrl Pts',(27.5938738431589,20.5289050941591,41.9320521558421));
#69030=CARTESIAN_POINT('Ctrl Pts',(27.5810538343781,20.6080182429969,41.9278937517687));
#69031=CARTESIAN_POINT('Ctrl Pts',(27.5682168450155,20.6872361801638,41.9237298397333));
#69032=CARTESIAN_POINT('Ctrl Pts',(27.5592888964614,20.7670031419257,41.9195659276979));
#69033=CARTESIAN_POINT('Ctrl Pts',(27.5542875075751,20.8468965892053,41.9154020156625));
#69034=CARTESIAN_POINT('Ctrl Pts',(27.5510546653782,20.8985388256912,41.9127105091953));
#69035=CARTESIAN_POINT('Ctrl Pts',(27.5494613475282,20.9502338560456,41.9100190027281));
#69036=CARTESIAN_POINT('Ctrl Pts',(27.5495007121296,21.0018681933898,41.907327496261));
#69037=CARTESIAN_POINT('',(27.5495007304439,20.9981079363645,41.1073274961648));
#69038=CARTESIAN_POINT('Ctrl Pts',(27.5495007121303,21.0018681943271,41.9073274962121));
#69039=CARTESIAN_POINT('Ctrl Pts',(27.5495933993273,21.1234454344049,41.9009901256798));
#69040=CARTESIAN_POINT('Ctrl Pts',(27.5587352425817,21.2446839676752,41.8946527551476));
#69041=CARTESIAN_POINT('Ctrl Pts',(27.5767683012454,21.3645523064678,41.8883153846154));
#69042=CARTESIAN_POINT('Ctrl Pts',(27.5888095170788,21.4445920027784,41.8840837316375));
#69043=CARTESIAN_POINT('Ctrl Pts',(27.6048430969206,21.5241841611566,41.8798520786596));
#69044=CARTESIAN_POINT('Ctrl Pts',(27.6248237724488,21.6028997744862,41.8756204256817));
#69045=CARTESIAN_POINT('Ctrl Pts',(27.6447758437266,21.6815026988775,41.8713948307203));
#69046=CARTESIAN_POINT('Ctrl Pts',(27.668663674594,21.7592311237478,41.8671692357589));
#69047=CARTESIAN_POINT('Ctrl Pts',(27.6963905484858,21.8356636553629,41.8629436407975));
#69048=CARTESIAN_POINT('Ctrl Pts',(27.7241569963262,21.9122052774254,41.8587120147386));
#69049=CARTESIAN_POINT('Ctrl Pts',(27.7557733676511,21.9874468430298,41.8544803886797));
#69050=CARTESIAN_POINT('Ctrl Pts',(27.7910916353731,22.0609778917025,41.8502487626209));
#69051=CARTESIAN_POINT('Ctrl Pts',(27.8262962876953,22.1342723982106,41.8460307492876));
#69052=CARTESIAN_POINT('Ctrl Pts',(27.865178868721,22.205866948534,41.8418127359543));
#69053=CARTESIAN_POINT('Ctrl Pts',(27.9075443638631,22.2753743218361,41.837594722621));
#69054=CARTESIAN_POINT('Ctrl Pts',(27.9498959184177,22.3448588233739,41.833378097247));
#69055=CARTESIAN_POINT('Ctrl Pts',(27.9957278694024,22.4122571152052,41.8291614718731));
#69056=CARTESIAN_POINT('Ctrl Pts',(28.0448000117159,22.4772079257213,41.8249448464991));
#69057=CARTESIAN_POINT('Ctrl Pts',(28.0938710307598,22.5421572495025,41.8207283176444));
#69058=CARTESIAN_POINT('Ctrl Pts',(28.1461818125716,22.6046588331796,41.8165117887897));
#69059=CARTESIAN_POINT('Ctrl Pts',(28.2014505777085,22.6643828362414,41.812295259935));
#69060=CARTESIAN_POINT('Ctrl Pts',(28.257060467454,22.7244754621071,41.8080527062224));
#69061=CARTESIAN_POINT('Ctrl Pts',(28.3156646680406,22.7817557429214,41.8038101525099));
#69062=CARTESIAN_POINT('Ctrl Pts',(28.3769383496614,22.8359251425917,41.7995675987974));
#69063=CARTESIAN_POINT('Ctrl Pts',(28.4379245795284,22.8898404186558,41.7953449480753));
#69064=CARTESIAN_POINT('Ctrl Pts',(28.5015548986921,22.940673687582,41.7911222973533));
#69065=CARTESIAN_POINT('Ctrl Pts',(28.567477076571,22.9881721061946,41.7868996466313));
#69066=CARTESIAN_POINT('Ctrl Pts',(28.6338653296365,23.0360063425097,41.7826471414235));
#69067=CARTESIAN_POINT('Ctrl Pts',(28.7025775734487,23.0804581291693,41.7783946362157));
#69068=CARTESIAN_POINT('Ctrl Pts',(28.7732274609767,23.1213154851408,41.7741421310079));
#69069=CARTESIAN_POINT('Ctrl Pts',(28.8438773485047,23.1621728411124,41.7698896258001));
#69070=CARTESIAN_POINT('Ctrl Pts',(28.9164644286987,23.199435605919,41.7656371205923));
#69071=CARTESIAN_POINT('Ctrl Pts',(28.9905822376341,23.232941116783,41.7613846153845));
#69072=CARTESIAN_POINT('Ctrl Pts',(29.0643366115777,23.2662823341359,41.7571529622394));
#69073=CARTESIAN_POINT('Ctrl Pts',(29.1398825912997,23.29602780231,41.7529213090942));
#69074=CARTESIAN_POINT('Ctrl Pts',(29.2168353211374,23.3219826303791,41.7486896559491));
#69075=CARTESIAN_POINT('Ctrl Pts',(29.2936778858269,23.3479003016444,41.7444640608177));
#69076=CARTESIAN_POINT('Ctrl Pts',(29.3719227641181,23.3700379633509,41.7402384656863));
#69077=CARTESIAN_POINT('Ctrl Pts',(29.4511635628977,23.3882480640228,41.7360128705549));
#69078=CARTESIAN_POINT('Ctrl Pts',(29.5305174563198,23.4064841546501,41.7317812445382));
#69079=CARTESIAN_POINT('Ctrl Pts',(29.6108696808612,23.4207812870483,41.7275496185215));
#69080=CARTESIAN_POINT('Ctrl Pts',(29.6917951688212,23.4310409359034,41.7233179925048));
#69081=CARTESIAN_POINT('Ctrl Pts',(29.7724603315873,23.4412675810023,41.7190999789962));
#69082=CARTESIAN_POINT('Ctrl Pts',(29.853694614712,23.4474826035878,41.7148819654876));
#69083=CARTESIAN_POINT('Ctrl Pts',(29.9350669576142,23.4496395551196,41.7106639519791));
#69084=CARTESIAN_POINT('Ctrl Pts',(30.0164125245543,23.4517957968961,41.7064473264282));
#69085=CARTESIAN_POINT('Ctrl Pts',(30.097895596774,23.4498966071184,41.7022307008773));
#69086=CARTESIAN_POINT('Ctrl Pts',(30.1790823719664,23.4439475759621,41.6980140753264));
#69087=CARTESIAN_POINT('Ctrl Pts',(30.2602672888064,23.4379986809782,41.6937975462935));
#69088=CARTESIAN_POINT('Ctrl Pts',(30.3411554586236,23.4280001640218,41.6895810172605));
#69089=CARTESIAN_POINT('Ctrl Pts',(30.4213169042637,23.4140095932249,41.6853644882275));
#69090=CARTESIAN_POINT('Ctrl Pts',(30.5019731074102,23.3999326724393,41.6811219347214));
#69091=CARTESIAN_POINT('Ctrl Pts',(30.5818931135361,23.3818143172013,41.6768793812152));
#69092=CARTESIAN_POINT('Ctrl Pts',(30.6606498630408,23.3597652443546,41.6726368277091));
#69093=CARTESIAN_POINT('Ctrl Pts',(30.7390371500469,23.3378196077925,41.6684141768072));
#69094=CARTESIAN_POINT('Ctrl Pts',(30.8162716434374,23.3119802524962,41.6641915259054));
#69095=CARTESIAN_POINT('Ctrl Pts',(30.8919497805055,23.2824057130704,41.6599688750035));
#69096=CARTESIAN_POINT('Ctrl Pts',(30.9681629577825,23.2526220833,41.6557163701952));
#69097=CARTESIAN_POINT('Ctrl Pts',(31.0427972497349,23.2190504444013,41.651463865387));
#69098=CARTESIAN_POINT('Ctrl Pts',(31.1154648880174,23.1819001658189,41.6472113605787));
#69099=CARTESIAN_POINT('Ctrl Pts',(31.1881325262999,23.1447498872364,41.6429588557704));
#69100=CARTESIAN_POINT('Ctrl Pts',(31.2588331312703,23.1040212606382,41.6387063509621));
#69101=CARTESIAN_POINT('Ctrl Pts',(31.3272094305348,23.0599673243767,41.6344538461539));
#69102=CARTESIAN_POINT('Ctrl Pts',(31.3952504536625,23.0161294020515,41.6302221930647));
#69103=CARTESIAN_POINT('Ctrl Pts',(31.4612444318076,22.9688347660637,41.6259905399755));
#69104=CARTESIAN_POINT('Ctrl Pts',(31.5248187584053,22.91830081166,41.6217588868863));
#69105=CARTESIAN_POINT('Ctrl Pts',(31.5883020723011,22.8678392014237,41.6175332918114));
#69106=CARTESIAN_POINT('Ctrl Pts',(31.6493722535907,22.8141477698547,41.6133076967365));
#69107=CARTESIAN_POINT('Ctrl Pts',(31.707684758663,22.7574876998233,41.6090821016616));
#69108=CARTESIAN_POINT('Ctrl Pts',(31.7660804899176,22.7007467620378,41.6048504756308));
#69109=CARTESIAN_POINT('Ctrl Pts',(31.8217102822432,22.6410289737294,41.6006188496001));
#69110=CARTESIAN_POINT('Ctrl Pts',(31.8742606257078,22.5786378168919,41.5963872235693));
#69111=CARTESIAN_POINT('Ctrl Pts',(31.9266419216878,22.5164473641305,41.5921692101182));
#69112=CARTESIAN_POINT('Ctrl Pts',(31.9759632377043,22.4516010621735,41.5879511966671));
#69113=CARTESIAN_POINT('Ctrl Pts',(32.0219515443117,22.3844356982017,41.583733183216));
#69114=CARTESIAN_POINT('Ctrl Pts',(32.0679247182423,22.317292435321,41.5795165577228));
#69115=CARTESIAN_POINT('Ctrl Pts',(32.1105667983761,22.2478320090719,41.5752999322296));
#69116=CARTESIAN_POINT('Ctrl Pts',(32.1496469688242,22.1764217608601,41.5710833067364));
#69117=CARTESIAN_POINT('Ctrl Pts',(32.1887262447319,22.10501314722,41.5668667777612));
#69118=CARTESIAN_POINT('Ctrl Pts',(32.2242435509093,22.0316552086384,41.5626502487861));
#69119=CARTESIAN_POINT('Ctrl Pts',(32.2560137991448,21.9567402929051,41.5584337198109));
#69120=CARTESIAN_POINT('Ctrl Pts',(32.2879801347238,21.8813629990782,41.5541911662369));
#69121=CARTESIAN_POINT('Ctrl Pts',(32.3161527995833,21.8044098746383,41.5499486126629));
#69122=CARTESIAN_POINT('Ctrl Pts',(32.3403929236425,21.7262996715986,41.5457060590889));
#69123=CARTESIAN_POINT('Ctrl Pts',(32.3645193320751,21.6485559002924,41.5414834082447));
#69124=CARTESIAN_POINT('Ctrl Pts',(32.3847499518859,21.5696663502626,41.5372607574004));
#69125=CARTESIAN_POINT('Ctrl Pts',(32.4009988267127,21.4900560010084,41.5330381065562));
#69126=CARTESIAN_POINT('Ctrl Pts',(32.4173625809041,21.4098828074685,41.5287856016173));
#69127=CARTESIAN_POINT('Ctrl Pts',(32.4296879964447,21.328979055862,41.5245330966785));
#69128=CARTESIAN_POINT('Ctrl Pts',(32.4379403827214,21.2477840598103,41.5202805917396));
#69129=CARTESIAN_POINT('Ctrl Pts',(32.4461927689982,21.1665890637587,41.5160280868008));
#69130=CARTESIAN_POINT('Ctrl Pts',(32.4503721648465,21.0851033004309,41.5117755818619));
#69131=CARTESIAN_POINT('Ctrl Pts',(32.450497108944,21.003764180767,41.507523076923));
#69132=CARTESIAN_POINT('Ctrl Pts',(32.450621440387,20.9228239017932,41.503291423845));
#69133=CARTESIAN_POINT('Ctrl Pts',(32.446731491831,20.8417260842945,41.499059770767));
#69134=CARTESIAN_POINT('Ctrl Pts',(32.4388075440206,20.7609016661948,41.494828117689));
#69135=CARTESIAN_POINT('Ctrl Pts',(32.4308949400967,20.6801929559527,41.4906025226257));
#69136=CARTESIAN_POINT('Ctrl Pts',(32.418959851677,20.5997573264625,41.4863769275624));
#69137=CARTESIAN_POINT('Ctrl Pts',(32.4030345676143,20.5200259206469,41.482151332499));
#69138=CARTESIAN_POINT('Ctrl Pts',(32.3870865542285,20.440180718376,41.4779197064654));
#69139=CARTESIAN_POINT('Ctrl Pts',(32.3671369628849,20.361042220484,41.4736880804318));
#69140=CARTESIAN_POINT('Ctrl Pts',(32.343270453307,20.2830384719816,41.4694564543982));
#69141=CARTESIAN_POINT('Ctrl Pts',(32.3194807192105,20.2052856514719,41.4652384409594));
#69142=CARTESIAN_POINT('Ctrl Pts',(32.2917993492479,20.1286607416087,41.4610204275207));
#69143=CARTESIAN_POINT('Ctrl Pts',(32.2603609495727,20.0535758732752,41.4568024140819));
#69144=CARTESIAN_POINT('Ctrl Pts',(32.2289328948586,19.9785157119892,41.4525857886014));
#69145=CARTESIAN_POINT('Ctrl Pts',(32.1937504448952,19.9049950142763,41.4483691631209));
#69146=CARTESIAN_POINT('Ctrl Pts',(32.154996782894,19.8334070479742,41.4441525376403));
#69147=CARTESIAN_POINT('Ctrl Pts',(32.1162440079618,19.7618207203161,41.4399360086781));
#69148=CARTESIAN_POINT('Ctrl Pts',(32.0739204057914,19.692167444326,41.4357194797158));
#69149=CARTESIAN_POINT('Ctrl Pts',(32.0282549853941,19.6248156617297,41.4315029507536));
#69150=CARTESIAN_POINT('Ctrl Pts',(31.9823077157539,19.5570481805859,41.4272603971651));
#69151=CARTESIAN_POINT('Ctrl Pts',(31.9329774887394,19.4916111026947,41.4230178435767));
#69152=CARTESIAN_POINT('Ctrl Pts',(31.8805405793361,19.4288483906795,41.4187752899883));
#69153=CARTESIAN_POINT('Ctrl Pts',(31.8283496630769,19.3663801124333,41.4145526391574));
#69154=CARTESIAN_POINT('Ctrl Pts',(31.7730815067821,19.3065614702871,41.4103299883266));
#69155=CARTESIAN_POINT('Ctrl Pts',(31.7150463420298,19.2496953708882,41.4061073374958));
#69156=CARTESIAN_POINT('Ctrl Pts',(31.6566008687312,19.1924272282336,41.4018548325285));
#69157=CARTESIAN_POINT('Ctrl Pts',(31.5953494668567,19.1381538576023,41.3976023275613));
#69158=CARTESIAN_POINT('Ctrl Pts',(31.5316422378551,19.0871428947205,41.3933498225941));
#69159=CARTESIAN_POINT('Ctrl Pts',(31.4679350088536,19.0361319318388,41.3890973176268));
#69160=CARTESIAN_POINT('Ctrl Pts',(31.4017723745344,18.988383603147,41.3848448126596));
#69161=CARTESIAN_POINT('Ctrl Pts',(31.3335317365672,18.9441198095297,41.3805923076924));
#69162=CARTESIAN_POINT('Ctrl Pts',(31.265625711934,18.9000730604185,41.3763606545944));
#69163=CARTESIAN_POINT('Ctrl Pts',(31.195408041103,18.8593119702202,41.3721290014965));
#69164=CARTESIAN_POINT('Ctrl Pts',(31.1232299195457,18.8220870545779,41.3678973483986));
#69165=CARTESIAN_POINT('Ctrl Pts',(31.0511551278423,18.7849154299468,41.3636717533151));
#69166=CARTESIAN_POINT('Ctrl Pts',(30.9771258691552,18.7512701368023,41.3594461582315));
#69167=CARTESIAN_POINT('Ctrl Pts',(30.901521746224,18.7213581257501,41.3552205631479));
#69168=CARTESIAN_POINT('Ctrl Pts',(30.8258097179442,18.6914034230316,41.3509889371193));
#69169=CARTESIAN_POINT('Ctrl Pts',(30.7485187292922,18.6651929079815,41.3467573110907));
#69170=CARTESIAN_POINT('Ctrl Pts',(30.6700542134318,18.6428878683732,41.3425256850621));
#69171=CARTESIAN_POINT('Ctrl Pts',(30.5918421073127,18.6206545810623,41.3383076716025));
#69172=CARTESIAN_POINT('Ctrl Pts',(30.5124644565581,18.6023018244049,41.3340896581428));
#69173=CARTESIAN_POINT('Ctrl Pts',(30.4323404455075,18.5879403014895,41.3298716446831));
#69174=CARTESIAN_POINT('Ctrl Pts',(30.3522427996554,18.5735835043036,41.3256550191815));
#69175=CARTESIAN_POINT('Ctrl Pts',(30.2713997383858,18.5632154146701,41.3214383936798));
#69176=CARTESIAN_POINT('Ctrl Pts',(30.1902409772808,18.5568957000236,41.3172217681781));
#69177=CARTESIAN_POINT('Ctrl Pts',(30.1090840738914,18.5505761300347,41.3130052391946));
#69178=CARTESIAN_POINT('Ctrl Pts',(30.0276119485251,18.5483047857458,41.3087887102111));
#69179=CARTESIAN_POINT('Ctrl Pts',(29.9462583465789,18.550089372102,41.3045721812275));
#69180=CARTESIAN_POINT('Ctrl Pts',(29.8644026270489,18.5518849729943,41.3003296276637));
#69181=CARTESIAN_POINT('Ctrl Pts',(29.7826673750212,18.557786748148,41.2960870740998));
#69182=CARTESIAN_POINT('Ctrl Pts',(29.7014914389796,18.5677494189542,41.291844520536));
#69183=CARTESIAN_POINT('Ctrl Pts',(29.6206963163348,18.5776653527754,41.2876218696837));
#69184=CARTESIAN_POINT('Ctrl Pts',(29.5404557258618,18.5916040309419,41.2833992188313));
#69185=CARTESIAN_POINT('Ctrl Pts',(29.461192472287,18.6094693689309,41.2791765679789));
#69186=CARTESIAN_POINT('Ctrl Pts',(29.3813688289045,18.627461014545,41.2749240630594));
#69187=CARTESIAN_POINT('Ctrl Pts',(29.3025368568059,18.6494349311086,41.2706715581398));
#69188=CARTESIAN_POINT('Ctrl Pts',(29.2251113855144,18.6752424029287,41.2664190532202));
#69189=CARTESIAN_POINT('Ctrl Pts',(29.147685914223,18.7010498747488,41.2621665483007));
#69190=CARTESIAN_POINT('Ctrl Pts',(29.0716673629024,18.7306906705246,41.2579140433811));
#69191=CARTESIAN_POINT('Ctrl Pts',(28.9974469742688,18.7639683185167,41.2536615384615));
#69192=CARTESIAN_POINT('Ctrl Pts',(28.9235905195819,18.7970827921305,41.2494298853716));
#69193=CARTESIAN_POINT('Ctrl Pts',(28.8512383675905,18.8339223611666,41.2451982322817));
#69194=CARTESIAN_POINT('Ctrl Pts',(28.7807915643565,18.8743280967055,41.2409665791917));
#69195=CARTESIAN_POINT('Ctrl Pts',(28.7104456124311,18.9146759875855,41.2367409841162));
#69196=CARTESIAN_POINT('Ctrl Pts',(28.6419999916318,18.958579676045,41.2325153890407));
#69197=CARTESIAN_POINT('Ctrl Pts',(28.5758345844244,19.0058327254018,41.2282897939653));
#69198=CARTESIAN_POINT('Ctrl Pts',(28.5095747430381,19.0531532163886,41.2240581679347));
#69199=CARTESIAN_POINT('Ctrl Pts',(28.4456020499601,19.103832428829,41.219826541904));
#69200=CARTESIAN_POINT('Ctrl Pts',(28.3842720633739,19.1576174434157,41.2155949158734));
#69201=CARTESIAN_POINT('Ctrl Pts',(28.3231393672129,19.2112294387506,41.211376902422));
#69202=CARTESIAN_POINT('Ctrl Pts',(28.2646327626603,19.2679269899824,41.2071588889706));
#69203=CARTESIAN_POINT('Ctrl Pts',(28.2090727924445,19.3274181672523,41.2029408755192));
#69204=CARTESIAN_POINT('Ctrl Pts',(28.1535311045098,19.3868897686582,41.1987242500258));
#69205=CARTESIAN_POINT('Ctrl Pts',(28.1009344423944,19.4491528311307,41.1945076245324));
#69206=CARTESIAN_POINT('Ctrl Pts',(28.0515662065552,19.5138788735226,41.190290999039));
#69207=CARTESIAN_POINT('Ctrl Pts',(28.0021991007501,19.5786034343417,41.1860744700638));
#69208=CARTESIAN_POINT('Ctrl Pts',(27.9560605552787,19.6457904927276,41.1818579410886));
#69209=CARTESIAN_POINT('Ctrl Pts',(27.9133925203572,19.715079972956,41.1776414121133));
#69210=CARTESIAN_POINT('Ctrl Pts',(27.8704611364877,19.7847971108387,41.1733988585398));
#69211=CARTESIAN_POINT('Ctrl Pts',(27.8310435131495,19.8566423151158,41.1691563049662));
#69212=CARTESIAN_POINT('Ctrl Pts',(27.7953398755101,19.930222459815,41.1649137513927));
#69213=CARTESIAN_POINT('Ctrl Pts',(27.7598037312989,20.0034574242611,41.1606911005486));
#69214=CARTESIAN_POINT('Ctrl Pts',(27.7279469362205,20.0784106342766,41.1564684497046));
#69215=CARTESIAN_POINT('Ctrl Pts',(27.6999183385823,20.1546748549758,41.1522457988605));
#69216=CARTESIAN_POINT('Ctrl Pts',(27.6716915790724,20.2314782628624,41.1479932939223));
#69217=CARTESIAN_POINT('Ctrl Pts',(27.647347501305,20.3096108346374,41.143740788984));
#69218=CARTESIAN_POINT('Ctrl Pts',(27.6269864242887,20.3886434596001,41.1394882840457));
#69219=CARTESIAN_POINT('Ctrl Pts',(27.6066253472723,20.4676760845629,41.1352357791074));
#69220=CARTESIAN_POINT('Ctrl Pts',(27.5902473043242,20.5476082851275,41.1309832741691));
#69221=CARTESIAN_POINT('Ctrl Pts',(27.5778997037597,20.6280048320844,41.1267307692308));
#69222=CARTESIAN_POINT('Ctrl Pts',(27.5591198811724,20.7502822640921,41.1202630115579));
#69223=CARTESIAN_POINT('Ctrl Pts',(27.5495965430392,20.8740166648451,41.113795253885));
#69224=CARTESIAN_POINT('Ctrl Pts',(27.5495007304446,20.9981079354573,41.1073274962121));
#69225=CARTESIAN_POINT('',(27.5495000708749,20.9994106292385,40.3073274962403));
#69226=CARTESIAN_POINT('Ctrl Pts',(27.5495007304439,20.9981079363645,41.1073274961648));
#69227=CARTESIAN_POINT('Ctrl Pts',(27.549439041719,21.0780038617879,41.1031632428524));
#69228=CARTESIAN_POINT('Ctrl Pts',(27.5532889456246,21.1580443678395,41.0989989895401));
#69229=CARTESIAN_POINT('Ctrl Pts',(27.5610663166378,21.237808196161,41.0948347362277));
#69230=CARTESIAN_POINT('Ctrl Pts',(27.5688342345066,21.317475074114,41.0906755444313));
#69231=CARTESIAN_POINT('Ctrl Pts',(27.5805200929035,21.3968654676096,41.0865163526349));
#69232=CARTESIAN_POINT('Ctrl Pts',(27.596087728639,21.4755586626274,41.0823571608385));
#69233=CARTESIAN_POINT('Ctrl Pts',(27.6116451315382,21.5542001314491,41.0782007029402));
#69234=CARTESIAN_POINT('Ctrl Pts',(27.6310791585009,21.6321448414503,41.0740442450419));
#69235=CARTESIAN_POINT('Ctrl Pts',(27.6543020436233,21.7089790881615,41.0698877871435));
#69236=CARTESIAN_POINT('Ctrl Pts',(27.6775172663571,21.7857879834207,41.065732700668));
#69237=CARTESIAN_POINT('Ctrl Pts',(27.7045187276538,21.8614866835657,41.0615776141926));
#69238=CARTESIAN_POINT('Ctrl Pts',(27.7351683756534,21.9356751377266,41.0574225277171));
#69239=CARTESIAN_POINT('Ctrl Pts',(27.7658179436624,22.0098633982674,41.0532674520857));
#69240=CARTESIAN_POINT('Ctrl Pts',(27.8001154941532,22.0825409780566,41.0491123764544));
#69241=CARTESIAN_POINT('Ctrl Pts',(27.8378748814851,22.1533278900151,41.044957300823));
#69242=CARTESIAN_POINT('Ctrl Pts',(27.8756707991451,22.2241832847885,41.0407982053628));
#69243=CARTESIAN_POINT('Ctrl Pts',(27.9169350126861,22.2931439364258,41.0366391099025));
#69244=CARTESIAN_POINT('Ctrl Pts',(27.9614358506387,22.3598553080893,41.0324800144422));
#69245=CARTESIAN_POINT('Ctrl Pts',(28.0059598064528,22.4266013358252,41.0283187583621));
#69246=CARTESIAN_POINT('Ctrl Pts',(28.0537234454411,22.4910953739531,41.024157502282));
#69247=CARTESIAN_POINT('Ctrl Pts',(28.1044538453399,22.5530148182015,41.0199962462019));
#69248=CARTESIAN_POINT('Ctrl Pts',(28.1552691739708,22.615037922975,41.0158280236835));
#69249=CARTESIAN_POINT('Ctrl Pts',(28.20906085445,22.6744774761023,41.011659801165));
#69250=CARTESIAN_POINT('Ctrl Pts',(28.2655184966037,22.7310471294497,41.0074915786466));
#69251=CARTESIAN_POINT('Ctrl Pts',(28.3002454010097,22.7658429315615,41.0049277190978));
#69252=CARTESIAN_POINT('Ctrl Pts',(28.3359802668707,22.7995536911752,41.0023638595489));
#69253=CARTESIAN_POINT('Ctrl Pts',(28.372645018108,22.8321206327399,40.9998000000001));
#69254=CARTESIAN_POINT('Ctrl Pts',(28.4331602315863,22.8858724067085,40.9955683469084));
#69255=CARTESIAN_POINT('Ctrl Pts',(28.4964546234175,22.9367232445843,40.9913366938168));
#69256=CARTESIAN_POINT('Ctrl Pts',(28.5622186355986,22.9843726963905,40.9871050407252));
#69257=CARTESIAN_POINT('Ctrl Pts',(28.6278885003328,23.0319539334683,40.982879445648));
#69258=CARTESIAN_POINT('Ctrl Pts',(28.6960205903648,23.0763426164863,40.9786538505708));
#69259=CARTESIAN_POINT('Ctrl Pts',(28.7662707158692,23.1172770965271,40.9744282554936));
#69260=CARTESIAN_POINT('Ctrl Pts',(28.8366211054066,23.1582700000373,40.9701966294634));
#69261=CARTESIAN_POINT('Ctrl Pts',(28.9090952189794,23.1957985344274,40.9659650034332));
#69262=CARTESIAN_POINT('Ctrl Pts',(28.9833164672467,23.2296423130691,40.9617333774031));
#69263=CARTESIAN_POINT('Ctrl Pts',(29.0572989556487,23.2633772207848,40.9575153639499));
#69264=CARTESIAN_POINT('Ctrl Pts',(29.1330169379909,23.2934508345848,40.9532973504968));
#69265=CARTESIAN_POINT('Ctrl Pts',(29.2100726278002,23.3196907114203,40.9490793370437));
#69266=CARTESIAN_POINT('Ctrl Pts',(29.2871029620564,23.3459219538955,40.9448627115486));
#69267=CARTESIAN_POINT('Ctrl Pts',(29.3654696899833,23.3683218149037,40.9406460860535));
#69268=CARTESIAN_POINT('Ctrl Pts',(29.4447569435623,23.3867667247299,40.9364294605584));
#69269=CARTESIAN_POINT('Ctrl Pts',(29.5240423822635,23.4052112123538,40.9322129315815));
#69270=CARTESIAN_POINT('Ctrl Pts',(29.6042478517499,23.4197008245721,40.9279964026045));
#69271=CARTESIAN_POINT('Ctrl Pts',(29.6849456907566,23.4301627583821,40.9237798736276));
#69272=CARTESIAN_POINT('Ctrl Pts',(29.7661416002276,23.4406892636886,40.9195373200561));
#69273=CARTESIAN_POINT('Ctrl Pts',(29.8478355080976,23.4471381254094,40.9152947664845));
#69274=CARTESIAN_POINT('Ctrl Pts',(29.9295867453177,23.4494881554245,40.911052212913));
#69275=CARTESIAN_POINT('Ctrl Pts',(30.0109544700066,23.4518271609465,40.9068295620673));
#69276=CARTESIAN_POINT('Ctrl Pts',(30.0923785199467,23.4501057717376,40.9026069112215));
#69277=CARTESIAN_POINT('Ctrl Pts',(30.1734264522537,23.4443554397139,40.8983842603758));
#69278=CARTESIAN_POINT('Ctrl Pts',(30.2550473924294,23.4385644529145,40.8941317554414));
#69279=CARTESIAN_POINT('Ctrl Pts',(30.3362864009185,23.4286873894784,40.889879250507));
#69280=CARTESIAN_POINT('Ctrl Pts',(30.4167110097646,23.4148089332991,40.8856267455725));
#69281=CARTESIAN_POINT('Ctrl Pts',(30.4971356186106,23.4009304771198,40.8813742406381));
#69282=CARTESIAN_POINT('Ctrl Pts',(30.5767453786491,23.383050793877,40.8771217357037));
#69283=CARTESIAN_POINT('Ctrl Pts',(30.6551239638149,23.3613053258813,40.8728692307692));
#69284=CARTESIAN_POINT('Ctrl Pts',(30.7331182253765,23.3396664851821,40.8686375776787));
#69285=CARTESIAN_POINT('Ctrl Pts',(30.8101850962609,23.3141187815989,40.8644059245882));
#69286=CARTESIAN_POINT('Ctrl Pts',(30.8859042005362,23.2847590677076,40.8601742714976));
#69287=CARTESIAN_POINT('Ctrl Pts',(30.961514905702,23.2554413850431,40.8559486764215));
#69288=CARTESIAN_POINT('Ctrl Pts',(31.0357812466064,23.2223226973068,40.8517230813454));
#69289=CARTESIAN_POINT('Ctrl Pts',(31.1082966308324,23.1855500058533,40.8474974862693));
#69290=CARTESIAN_POINT('Ctrl Pts',(31.1809155121908,23.1487248308041,40.8432658602389));
#69291=CARTESIAN_POINT('Ctrl Pts',(31.2517779876693,23.1082353556078,40.8390342342084));
#69292=CARTESIAN_POINT('Ctrl Pts',(31.3204945272184,23.0642781919079,40.834802608178));
#69293=CARTESIAN_POINT('Ctrl Pts',(31.3889900147937,23.0204624325606,40.830584594726));
#69294=CARTESIAN_POINT('Ctrl Pts',(31.4553529499075,22.9732014979876,40.826366581274));
#69295=CARTESIAN_POINT('Ctrl Pts',(31.5192225575701,22.9227358296371,40.822148567822));
#69296=CARTESIAN_POINT('Ctrl Pts',(31.5830711486246,22.8722867672626,40.817931942328));
#69297=CARTESIAN_POINT('Ctrl Pts',(31.6444276771133,22.8186353532303,40.8137153168341));
#69298=CARTESIAN_POINT('Ctrl Pts',(31.702962595359,22.7620637470898,40.8094986913401));
#69299=CARTESIAN_POINT('Ctrl Pts',(31.7614961737458,22.7054934358682,40.8052821623644));
#69300=CARTESIAN_POINT('Ctrl Pts',(31.817207936864,22.6460033892658,40.8010656333886));
#69301=CARTESIAN_POINT('Ctrl Pts',(31.8698045683117,22.5839132319419,40.7968491044128));
#69302=CARTESIAN_POINT('Ctrl Pts',(31.922725828417,22.5214398515128,40.7926065508399));
#69303=CARTESIAN_POINT('Ctrl Pts',(31.9724930520762,22.4563345072282,40.7883639972671));
#69304=CARTESIAN_POINT('Ctrl Pts',(32.0188492070839,22.3889557692946,40.7841214436942));
#69305=CARTESIAN_POINT('Ctrl Pts',(32.064987895431,22.3218931194647,40.7798987928496));
#69306=CARTESIAN_POINT('Ctrl Pts',(32.1077472493203,22.2525787865955,40.7756761420051));
#69307=CARTESIAN_POINT('Ctrl Pts',(32.1469189095396,22.1813930107553,40.7714534911605));
#69308=CARTESIAN_POINT('Ctrl Pts',(32.1863675129417,22.1097039523066,40.7672009862235));
#69309=CARTESIAN_POINT('Ctrl Pts',(32.222177285331,22.0361173156651,40.7629484812865));
#69310=CARTESIAN_POINT('Ctrl Pts',(32.2541845580174,21.9610422615037,40.7586959763495));
#69311=CARTESIAN_POINT('Ctrl Pts',(32.2861918307037,21.8859672073422,40.7544434714125));
#69312=CARTESIAN_POINT('Ctrl Pts',(32.314396498974,21.8094042028156,40.7501909664754));
#69313=CARTESIAN_POINT('Ctrl Pts',(32.3386862843846,21.731776409316,40.7459384615384));
#69314=CARTESIAN_POINT('Ctrl Pts',(32.3628569666116,21.6545292580156,40.7417068084479));
#69315=CARTESIAN_POINT('Ctrl Pts',(32.3832415129416,21.5759388131944,40.7374751553573));
#69316=CARTESIAN_POINT('Ctrl Pts',(32.3996930386648,21.496410687016,40.7332435022668));
#69317=CARTESIAN_POINT('Ctrl Pts',(32.4161210124619,21.4169964129252,40.7290179071907));
#69318=CARTESIAN_POINT('Ctrl Pts',(32.4286270549614,21.3366475749145,40.7247923121146));
#69319=CARTESIAN_POINT('Ctrl Pts',(32.437113879368,21.255785435457,40.7205667170385));
#69320=CARTESIAN_POINT('Ctrl Pts',(32.4456128165421,21.1748078860125,40.716335091008));
#69321=CARTESIAN_POINT('Ctrl Pts',(32.4500809303349,21.0933160214387,40.7121034649776));
#69322=CARTESIAN_POINT('Ctrl Pts',(32.4504718597259,21.0117437085971,40.7078718389471));
#69323=CARTESIAN_POINT('Ctrl Pts',(32.4508615315489,20.9304338030427,40.7036538254951));
#69324=CARTESIAN_POINT('Ctrl Pts',(32.4472001914478,20.8490444322236,40.6994358120431));
#69325=CARTESIAN_POINT('Ctrl Pts',(32.4394938976771,20.7680091096698,40.6952177985911));
#69326=CARTESIAN_POINT('Ctrl Pts',(32.4317901397002,20.6870004521871,40.6910011730972));
#69327=CARTESIAN_POINT('Ctrl Pts',(32.4200441152582,20.6063460739694,40.6867845476032));
#69328=CARTESIAN_POINT('Ctrl Pts',(32.4043138706571,20.5264759125814,40.6825679221093));
#69329=CARTESIAN_POINT('Ctrl Pts',(32.3885839861198,20.4466075794137,40.6783513931335));
#69330=CARTESIAN_POINT('Ctrl Pts',(32.3688701536744,20.3675238832121,40.6741348641577));
#69331=CARTESIAN_POINT('Ctrl Pts',(32.3452815526646,20.2896446743137,40.6699183351819));
#69332=CARTESIAN_POINT('Ctrl Pts',(32.3215473618013,20.2112847916094,40.665675781609));
#69333=CARTESIAN_POINT('Ctrl Pts',(32.2938905308257,20.134144775369,40.6614332280362));
#69334=CARTESIAN_POINT('Ctrl Pts',(32.2624726441201,20.0586351479855,40.6571906744633));
#69335=CARTESIAN_POINT('Ctrl Pts',(32.231202145456,19.9834797524509,40.6529680236187));
#69336=CARTESIAN_POINT('Ctrl Pts',(32.1962060520371,19.9099398820973,40.6487453727742));
#69337=CARTESIAN_POINT('Ctrl Pts',(32.1576905710454,19.8383969483417,40.6445227219296));
#69338=CARTESIAN_POINT('Ctrl Pts',(32.1189027860505,19.7663482068755,40.6402702169926));
#69339=CARTESIAN_POINT('Ctrl Pts',(32.0765459027894,19.6963251583042,40.6360177120556));
#69340=CARTESIAN_POINT('Ctrl Pts',(32.0308746783301,19.6286873839574,40.6317652071186));
#69341=CARTESIAN_POINT('Ctrl Pts',(31.9852034538708,19.5610496096106,40.6275127021816));
#69342=CARTESIAN_POINT('Ctrl Pts',(31.9362182236805,19.4957974510437,40.6232601972446));
#69343=CARTESIAN_POINT('Ctrl Pts',(31.8842134022846,19.4332549331015,40.6190076923077));
#69344=CARTESIAN_POINT('Ctrl Pts',(31.8324635827178,19.3710190878106,40.6147760392168));
#69345=CARTESIAN_POINT('Ctrl Pts',(31.7775301807484,19.3112335620099,40.610544386126));
#69346=CARTESIAN_POINT('Ctrl Pts',(31.7196740854053,19.2542419153888,40.6063127330352));
#69347=CARTESIAN_POINT('Ctrl Pts',(31.6619008165734,19.1973318577381,40.6020871379589));
#69348=CARTESIAN_POINT('Ctrl Pts',(31.6012134927534,19.143208058933,40.5978615428825));
#69349=CARTESIAN_POINT('Ctrl Pts',(31.5379130727012,19.0921809229346,40.5936359478062));
#69350=CARTESIAN_POINT('Ctrl Pts',(31.4745223075221,19.0410809587768,40.5894043217758));
#69351=CARTESIAN_POINT('Ctrl Pts',(31.4085112943313,18.9930868532024,40.5851726957454));
#69352=CARTESIAN_POINT('Ctrl Pts',(31.3402192245448,18.9484730856846,40.580941069715));
#69353=CARTESIAN_POINT('Ctrl Pts',(31.2721468412633,18.9040028347228,40.5767230562627));
#69354=CARTESIAN_POINT('Ctrl Pts',(31.2018084359025,18.8628914758816,40.5725050428105));
#69355=CARTESIAN_POINT('Ctrl Pts',(31.1295713614834,18.8253692751834,40.5682870293582));
#69356=CARTESIAN_POINT('Ctrl Pts',(31.0573580570284,18.7878594213495,40.5640704038639));
#69357=CARTESIAN_POINT('Ctrl Pts',(30.983247736387,18.7539365943576,40.5598537783697));
#69358=CARTESIAN_POINT('Ctrl Pts',(30.9076329737119,18.7237854593578,40.5556371528755));
#69359=CARTESIAN_POINT('Ctrl Pts',(30.8320199418518,18.6936350145148,40.5514206238994));
#69360=CARTESIAN_POINT('Ctrl Pts',(30.7549029685927,18.6672562611193,40.5472040949233));
#69361=CARTESIAN_POINT('Ctrl Pts',(30.6766939168855,18.6447854465357,40.5429875659473));
#69362=CARTESIAN_POINT('Ctrl Pts',(30.5980021555796,18.6221759411272,40.5387450123747));
#69363=CARTESIAN_POINT('Ctrl Pts',(30.5182052418425,18.6035229263023,40.5345024588022));
#69364=CARTESIAN_POINT('Ctrl Pts',(30.4377356556349,18.5889135756291,40.5302599052297));
#69365=CARTESIAN_POINT('Ctrl Pts',(30.3576435694949,18.5743727605495,40.5260372543848));
#69366=CARTESIAN_POINT('Ctrl Pts',(30.2768855800931,18.5638377600858,40.52181460354));
#69367=CARTESIAN_POINT('Ctrl Pts',(30.195893945677,18.5573424693488,40.5175919526951));
#69368=CARTESIAN_POINT('Ctrl Pts',(30.1143297013638,18.5508012569831,40.5133394477588));
#69369=CARTESIAN_POINT('Ctrl Pts',(30.0325289736827,18.5483571130502,40.5090869428224));
#69370=CARTESIAN_POINT('Ctrl Pts',(29.9509320456543,18.5499913090243,40.504834437886));
#69371=CARTESIAN_POINT('Ctrl Pts',(29.8693351176258,18.5516255049984,40.5005819329497));
#69372=CARTESIAN_POINT('Ctrl Pts',(29.7879424582125,18.5573379445842,40.4963294280133));
#69373=CARTESIAN_POINT('Ctrl Pts',(29.7071860201171,18.5670572914298,40.4920769230769));
#69374=CARTESIAN_POINT('Ctrl Pts',(29.6268255652861,18.5767289801717,40.4878452699863));
#69375=CARTESIAN_POINT('Ctrl Pts',(29.5467945237444,18.5904045107437,40.4836136168956));
#69376=CARTESIAN_POINT('Ctrl Pts',(29.4675230525945,18.6080513068877,40.479381963805));
#69377=CARTESIAN_POINT('Ctrl Pts',(29.3883650661059,18.6256728399622,40.4751563687288));
#69378=CARTESIAN_POINT('Ctrl Pts',(29.3099649402285,18.6472542470397,40.4709307736526));
#69379=CARTESIAN_POINT('Ctrl Pts',(29.2327467417191,18.6727113011795,40.4667051785764));
#69380=CARTESIAN_POINT('Ctrl Pts',(29.1554183340175,18.6982046887411,40.4624735525459));
#69381=CARTESIAN_POINT('Ctrl Pts',(29.0792756935947,18.7275847217899,40.4582419265155));
#69382=CARTESIAN_POINT('Ctrl Pts',(29.0047334743213,18.7607155623138,40.4540103004851));
#69383=CARTESIAN_POINT('Ctrl Pts',(28.930431047456,18.7937398253289,40.449792287033));
#69384=CARTESIAN_POINT('Ctrl Pts',(28.857719193688,18.8304906268936,40.4455742735808));
#69385=CARTESIAN_POINT('Ctrl Pts',(28.7869907253848,18.8707844755174,40.4413562601287));
#69386=CARTESIAN_POINT('Ctrl Pts',(28.7162855306319,18.9110650652523,40.4371396346346));
#69387=CARTESIAN_POINT('Ctrl Pts',(28.6475628288216,18.9548861568875,40.4329230091406));
#69388=CARTESIAN_POINT('Ctrl Pts',(28.5811908292864,19.0020183216308,40.4287063836465));
#69389=CARTESIAN_POINT('Ctrl Pts',(28.514820349,19.0491494075234,40.4244898546706));
#69390=CARTESIAN_POINT('Ctrl Pts',(28.4508008423251,19.0995911457962,40.4202733256947));
#69391=CARTESIAN_POINT('Ctrl Pts',(28.3894703292654,19.1530716230228,40.4160567967187));
#69392=CARTESIAN_POINT('Ctrl Pts',(28.3277612816615,19.2068821840374,40.411814243146));
#69393=CARTESIAN_POINT('Ctrl Pts',(28.2687749035352,19.2637688221892,40.4075716895733));
#69394=CARTESIAN_POINT('Ctrl Pts',(28.212819195729,19.3234156678397,40.4033291360006));
#69395=CARTESIAN_POINT('Ctrl Pts',(28.1571259881399,19.3827826973546,40.3991064851559));
#69396=CARTESIAN_POINT('Ctrl Pts',(28.1044353398793,19.4448837011503,40.3948838343112));
#69397=CARTESIAN_POINT('Ctrl Pts',(28.0550103882544,19.5093740710018,40.3906611834665));
#69398=CARTESIAN_POINT('Ctrl Pts',(28.0052360028003,19.574320387013,40.3864086785298));
#69399=CARTESIAN_POINT('Ctrl Pts',(27.9587739428001,19.6416895926669,40.382156173593));
#69400=CARTESIAN_POINT('Ctrl Pts',(27.9158475089461,19.711101771266,40.3779036686563));
#69401=CARTESIAN_POINT('Ctrl Pts',(27.872921075092,19.7805139498651,40.3736511637196));
#69402=CARTESIAN_POINT('Ctrl Pts',(27.8335304411144,19.8519686552971,40.3693986587829));
#69403=CARTESIAN_POINT('Ctrl Pts',(27.797850205218,19.9250644059565,40.3651461538461));
#69404=CARTESIAN_POINT('Ctrl Pts',(27.7596965548658,20.0032272780009,40.3605988580562));
#69405=CARTESIAN_POINT('Ctrl Pts',(27.7256585715111,20.0835251228355,40.3560515622662));
#69406=CARTESIAN_POINT('Ctrl Pts',(27.6959618808451,20.1655189663742,40.3515042664763));
#69407=CARTESIAN_POINT('Ctrl Pts',(27.6663678835467,20.2472292690967,40.3469726955737));
#69408=CARTESIAN_POINT('Ctrl Pts',(27.6410853849827,20.3306235495274,40.3424411246712));
#69409=CARTESIAN_POINT('Ctrl Pts',(27.6202922314064,20.4152426263011,40.3379095537687));
#69410=CARTESIAN_POINT('Ctrl Pts',(27.5995450215131,20.4996747322999,40.3333879956358));
#69411=CARTESIAN_POINT('Ctrl Pts',(27.5832674962484,20.5853259036227,40.3288664375029));
#69412=CARTESIAN_POINT('Ctrl Pts',(27.5715884749131,20.6717200663683,40.32434487937));
#69413=CARTESIAN_POINT('Ctrl Pts',(27.5599448339301,20.7578525071921,40.3198370188163));
#69414=CARTESIAN_POINT('Ctrl Pts',(27.5528719937193,20.844723103544,40.3153291582625));
#69415=CARTESIAN_POINT('Ctrl Pts',(27.5504479634921,20.9318452463886,40.3108212977088));
#69416=CARTESIAN_POINT('Ctrl Pts',(27.5498217181246,20.954353149859,40.3096566972193));
#69417=CARTESIAN_POINT('Ctrl Pts',(27.5495054902598,20.9768777803791,40.3084920967298));
#69418=CARTESIAN_POINT('Ctrl Pts',(27.5495000708749,20.9994106292385,40.3073274962403));
#69419=CARTESIAN_POINT('',(27.5495010177781,21.0022334121089,39.5073274961711));
#69420=CARTESIAN_POINT('Ctrl Pts',(27.5495000708748,20.9994106297869,40.307327496212));
#69421=CARTESIAN_POINT('Ctrl Pts',(27.5494798595713,21.0834457515148,40.3029841775084));
#69422=CARTESIAN_POINT('Ctrl Pts',(27.5537867160569,21.1674327148593,40.2986408588047));
#69423=CARTESIAN_POINT('Ctrl Pts',(27.562379720821,21.2509135798149,40.2942975401011));
#69424=CARTESIAN_POINT('Ctrl Pts',(27.5709805838758,21.3344707879032,40.2899502494386));
#69425=CARTESIAN_POINT('Ctrl Pts',(27.5838753546468,21.4175205550911,40.2856029587762));
#69426=CARTESIAN_POINT('Ctrl Pts',(27.6009716505737,21.4996130789411,40.2812556681138));
#69427=CARTESIAN_POINT('Ctrl Pts',(27.6181014503126,21.5818664804746,40.2768998580147));
#69428=CARTESIAN_POINT('Ctrl Pts',(27.6394491300605,21.6631584772385,40.2725440479157));
#69429=CARTESIAN_POINT('Ctrl Pts',(27.6648718179047,21.7430522344925,40.2681882378167));
#69430=CARTESIAN_POINT('Ctrl Pts',(27.6903228538513,21.8230350789596,40.2638275706801));
#69431=CARTESIAN_POINT('Ctrl Pts',(27.719857803327,21.9016161811874,40.2594669035434));
#69432=CARTESIAN_POINT('Ctrl Pts',(27.7532856978946,21.9783788094164,40.2551062364068));
#69433=CARTESIAN_POINT('Ctrl Pts',(27.7867835005452,22.0553019720808,40.2507364497643));
#69434=CARTESIAN_POINT('Ctrl Pts',(27.8241903190306,22.1303986869069,40.2463666631219));
#69435=CARTESIAN_POINT('Ctrl Pts',(27.8652693153614,22.2032768401587,40.2419968764794));
#69436=CARTESIAN_POINT('Ctrl Pts',(27.8771188557864,22.2242990826717,40.2407363791914));
#69437=CARTESIAN_POINT('Ctrl Pts',(27.8892736786416,22.245136915382,40.2394758819034));
#69438=CARTESIAN_POINT('Ctrl Pts',(27.9017274553734,22.2657814102231,40.2382153846154));
#69439=CARTESIAN_POINT('Ctrl Pts',(27.9435364011762,22.335087660409,40.2339837315247));
#69440=CARTESIAN_POINT('Ctrl Pts',(27.9888610194208,22.4024498658945,40.229752078434));
#69441=CARTESIAN_POINT('Ctrl Pts',(28.0374950160594,22.4674891611213,40.2255204253432));
#69442=CARTESIAN_POINT('Ctrl Pts',(28.0860593884996,22.5324353464021,40.221294830267));
#69443=CARTESIAN_POINT('Ctrl Pts',(28.1379234538329,22.5950648569889,40.2170692351907));
#69444=CARTESIAN_POINT('Ctrl Pts',(28.1928363205505,22.6550255845994,40.2128436401144));
#69445=CARTESIAN_POINT('Ctrl Pts',(28.2478275613135,22.7150718907832,40.208612014084));
#69446=CARTESIAN_POINT('Ctrl Pts',(28.3058760560055,22.7724413974607,40.2043803880536));
#69447=CARTESIAN_POINT('Ctrl Pts',(28.3666877157555,22.8268117670236,40.2001487620232));
#69448=CARTESIAN_POINT('Ctrl Pts',(28.4273037524828,22.8810072343378,40.195930748571));
#69449=CARTESIAN_POINT('Ctrl Pts',(28.4906648674942,22.9322225074378,40.1917127351188));
#69450=CARTESIAN_POINT('Ctrl Pts',(28.5564424855217,22.9801747277433,40.1874947216666));
#69451=CARTESIAN_POINT('Ctrl Pts',(28.6221984591009,23.0281111691351,40.1832780961725));
#69452=CARTESIAN_POINT('Ctrl Pts',(28.6903689812933,23.0727864164253,40.1790614706784));
#69453=CARTESIAN_POINT('Ctrl Pts',(28.7605936890024,23.1139589036354,40.1748448451842));
#69454=CARTESIAN_POINT('Ctrl Pts',(28.8308167892745,23.1551304484111,40.1706283162083));
#69455=CARTESIAN_POINT('Ctrl Pts',(28.9030935800327,23.1927991584072,40.1664117872323));
#69456=CARTESIAN_POINT('Ctrl Pts',(28.9770373519693,23.2267684367114,40.1621952582563));
#69457=CARTESIAN_POINT('Ctrl Pts',(29.0514375080198,23.26094737485,40.1579527046837));
#69458=CARTESIAN_POINT('Ctrl Pts',(29.127524867365,23.2913808457708,40.153710151111));
#69459=CARTESIAN_POINT('Ctrl Pts',(29.2048849627703,23.3179176705766,40.1494675975384));
#69460=CARTESIAN_POINT('Ctrl Pts',(29.2818821453919,23.3443300054511,40.1452449466936));
#69461=CARTESIAN_POINT('Ctrl Pts',(29.3601396835155,23.366882096564,40.1410222958489));
#69462=CARTESIAN_POINT('Ctrl Pts',(29.439235322132,23.3854754716944,40.1367996450041));
#69463=CARTESIAN_POINT('Ctrl Pts',(29.5188901659834,23.4042003017683,40.1325471400675));
#69464=CARTESIAN_POINT('Ctrl Pts',(29.5993945366168,23.4189101351576,40.1282946351309));
#69465=CARTESIAN_POINT('Ctrl Pts',(29.6803103368298,23.4295573196083,40.1240421301944));
#69466=CARTESIAN_POINT('Ctrl Pts',(29.7612261370428,23.4402045040589,40.1197896252578));
#69467=CARTESIAN_POINT('Ctrl Pts',(29.8425528887275,23.4467890642942,40.1155371203212));
#69468=CARTESIAN_POINT('Ctrl Pts',(29.9238528242053,23.4493166103259,40.1112846153846));
#69469=CARTESIAN_POINT('Ctrl Pts',(30.0047541114153,23.4518317627212,40.107052962294));
#69470=CARTESIAN_POINT('Ctrl Pts',(30.0859314452372,23.4503390402701,40.1028213092033));
#69471=CARTESIAN_POINT('Ctrl Pts',(30.1669546582724,23.4448060029543,40.0985896561126));
#69472=CARTESIAN_POINT('Ctrl Pts',(30.2478618788609,23.4392808867083,40.0943640610364));
#69473=CARTESIAN_POINT('Ctrl Pts',(30.3286149570392,23.4297269747436,40.0901384659602));
#69474=CARTESIAN_POINT('Ctrl Pts',(30.4087819842452,23.4161638063998,40.0859128708839));
#69475=CARTESIAN_POINT('Ctrl Pts',(30.4890634293405,23.4025812801087,40.0816812448535));
#69476=CARTESIAN_POINT('Ctrl Pts',(30.5687566800655,23.3849780468442,40.0774496188231));
#69477=CARTESIAN_POINT('Ctrl Pts',(30.647431377453,23.363426085472,40.0732179927927));
#69478=CARTESIAN_POINT('Ctrl Pts',(30.7258529888,23.3419434538938,40.0689999793405));
#69479=CARTESIAN_POINT('Ctrl Pts',(30.8032621357507,23.3165375675207,40.0647819658884));
#69480=CARTESIAN_POINT('Ctrl Pts',(30.8792428911614,23.2873307999374,40.0605639524363));
#69481=CARTESIAN_POINT('Ctrl Pts',(30.9551986447314,23.2581336429844,40.0563473269422));
#69482=CARTESIAN_POINT('Ctrl Pts',(31.0297265066468,23.2251382552068,40.0521307014481));
#69483=CARTESIAN_POINT('Ctrl Pts',(31.102427969672,23.1885161232408,40.047914075954));
#69484=CARTESIAN_POINT('Ctrl Pts',(31.1751277685676,23.1518948295519,40.0436975469781));
#69485=CARTESIAN_POINT('Ctrl Pts',(31.2460008370891,23.1116471668463,40.0394810180021));
#69486=CARTESIAN_POINT('Ctrl Pts',(31.3146721296427,23.0679911608952,40.0352644890262));
#69487=CARTESIAN_POINT('Ctrl Pts',(31.3837672643444,23.0240657082125,40.0310219354535));
#69488=CARTESIAN_POINT('Ctrl Pts',(31.4506329410647,22.9766899371753,40.0267793818808));
#69489=CARTESIAN_POINT('Ctrl Pts',(31.5149171864598,22.9261298419808,40.0225368283081));
#69490=CARTESIAN_POINT('Ctrl Pts',(31.5788998606836,22.8758069350278,40.0183141774634));
#69491=CARTESIAN_POINT('Ctrl Pts',(31.6403249528404,22.8223298638654,40.0140915266187));
#69492=CARTESIAN_POINT('Ctrl Pts',(31.6988805246043,22.7659997772141,40.009868875774));
#69493=CARTESIAN_POINT('Ctrl Pts',(31.7578500835743,22.7092714375103,40.0056163708373));
#69494=CARTESIAN_POINT('Ctrl Pts',(31.8139090610151,22.6496499318426,40.0013638659006));
#69495=CARTESIAN_POINT('Ctrl Pts',(31.866779596433,22.5874773032523,39.9971113609639));
#69496=CARTESIAN_POINT('Ctrl Pts',(31.9196501318509,22.5253046746621,39.9928588560272));
#69497=CARTESIAN_POINT('Ctrl Pts',(31.9693319864446,22.4605813380857,39.9886063510905));
#69498=CARTESIAN_POINT('Ctrl Pts',(32.0155922081882,22.3936779758219,39.9843538461538));
#69499=CARTESIAN_POINT('Ctrl Pts',(32.0616255963278,22.3271026692874,39.9801221930632));
#69500=CARTESIAN_POINT('Ctrl Pts',(32.1044430424686,22.2581196710003,39.9758905399725));
#69501=CARTESIAN_POINT('Ctrl Pts',(32.1437837664059,22.1870726232605,39.9716588868818));
#69502=CARTESIAN_POINT('Ctrl Pts',(32.1830681703498,22.1161272861364,39.9674332918056));
#69503=CARTESIAN_POINT('Ctrl Pts',(32.2188855141122,22.0431241714434,39.9632076967294));
#69504=CARTESIAN_POINT('Ctrl Pts',(32.2510177243999,21.9684366032102,39.9589821016532));
#69505=CARTESIAN_POINT('Ctrl Pts',(32.2831957951843,21.8936424376114,39.9547504756227));
#69506=CARTESIAN_POINT('Ctrl Pts',(32.3116779526552,21.8171594019872,39.9505188495923));
#69507=CARTESIAN_POINT('Ctrl Pts',(32.3362910034261,21.739387988346,39.9462872235619));
#69508=CARTESIAN_POINT('Ctrl Pts',(32.3608248772853,21.6618667550017,39.9420692101098));
#69509=CARTESIAN_POINT('Ctrl Pts',(32.3815143425697,21.5830658595736,39.9378511966576));
#69510=CARTESIAN_POINT('Ctrl Pts',(32.398236362313,21.503401033451,39.9336331832055));
#69511=CARTESIAN_POINT('Ctrl Pts',(32.4149528795936,21.4237624214309,39.9294165577114));
#69512=CARTESIAN_POINT('Ctrl Pts',(32.42770444851,21.3432608978029,39.9251999322173));
#69513=CARTESIAN_POINT('Ctrl Pts',(32.4364187343998,21.2623242281335,39.9209833067233));
#69514=CARTESIAN_POINT('Ctrl Pts',(32.4451328208203,21.1813894110971,39.9167667777473));
#69515=CARTESIAN_POINT('Ctrl Pts',(32.4498097593208,21.1000199300789,39.9125502487714));
#69516=CARTESIAN_POINT('Ctrl Pts',(32.4504290360183,21.0186491136093,39.9083337197955));
#69517=CARTESIAN_POINT('Ctrl Pts',(32.451052134918,20.9367760729878,39.9040911662228));
#69518=CARTESIAN_POINT('Ctrl Pts',(32.4475672928651,20.8549021560147,39.8998486126501));
#69519=CARTESIAN_POINT('Ctrl Pts',(32.4400068056719,20.7734673571538,39.8956060590774));
#69520=CARTESIAN_POINT('Ctrl Pts',(32.4324817863443,20.6924145863861,39.8913834082327));
#69521=CARTESIAN_POINT('Ctrl Pts',(32.4209193978756,20.6117972789425,39.887160757388));
#69522=CARTESIAN_POINT('Ctrl Pts',(32.4054031937343,20.5320408932685,39.8829381065433));
#69523=CARTESIAN_POINT('Ctrl Pts',(32.3897772902115,20.4517206308823,39.8786856016066));
#69524=CARTESIAN_POINT('Ctrl Pts',(32.3701415606893,20.3722739757231,39.8744330966699));
#69525=CARTESIAN_POINT('Ctrl Pts',(32.3466324024204,20.29411996918,39.8701805917332));
#69526=CARTESIAN_POINT('Ctrl Pts',(32.3231232441516,20.2159659626369,39.8659280867965));
#69527=CARTESIAN_POINT('Ctrl Pts',(32.2957408759543,20.1391050305231,39.8616755818598));
#69528=CARTESIAN_POINT('Ctrl Pts',(32.2646701270147,20.0639340483667,39.8574230769231));
#69529=CARTESIAN_POINT('Ctrl Pts',(32.2337517312124,19.9891316616049,39.8531914238322));
#69530=CARTESIAN_POINT('Ctrl Pts',(32.1990654302537,19.915722886428,39.8489597707414));
#69531=CARTESIAN_POINT('Ctrl Pts',(32.1607582373052,19.8441132884588,39.8447281176506));
#69532=CARTESIAN_POINT('Ctrl Pts',(32.1225058847521,19.7726062064496,39.8405025225742));
#69533=CARTESIAN_POINT('Ctrl Pts',(32.0806431528224,19.7028935924912,39.8362769274979));
#69534=CARTESIAN_POINT('Ctrl Pts',(32.0353651668613,19.6353612611655,39.8320513324215));
#69535=CARTESIAN_POINT('Ctrl Pts',(31.9900225581792,19.5677325447443,39.8278197063911));
#69536=CARTESIAN_POINT('Ctrl Pts',(31.9412551341529,19.5022907661456,39.8235880803608));
#69537=CARTESIAN_POINT('Ctrl Pts',(31.8893052009778,19.4393987993218,39.8193564543304));
#69538=CARTESIAN_POINT('Ctrl Pts',(31.837522383828,19.3767091475902,39.8151384408781));
#69539=CARTESIAN_POINT('Ctrl Pts',(31.7825777857254,19.3165532980507,39.8109204274258));
#69540=CARTESIAN_POINT('Ctrl Pts',(31.7247537407076,19.2592602768033,39.8067024139735));
#69541=CARTESIAN_POINT('Ctrl Pts',(31.6669487229759,19.201986108106,39.8024857884793));
#69542=CARTESIAN_POINT('Ctrl Pts',(31.6062664698693,19.1475732238359,39.7982691629851));
#69543=CARTESIAN_POINT('Ctrl Pts',(31.5430269479006,19.0963146037088,39.7940525374908));
#69544=CARTESIAN_POINT('Ctrl Pts',(31.4797888734788,19.0450571568867,39.7898360085148));
#69545=CARTESIAN_POINT('Ctrl Pts',(31.413994008377,18.9969541224548,39.7856194795387));
#69546=CARTESIAN_POINT('Ctrl Pts',(31.345995124287,18.9522579812399,39.7814029505626));
#69547=CARTESIAN_POINT('Ctrl Pts',(31.2775765481877,18.9072859735375,39.7771603969901));
#69548=CARTESIAN_POINT('Ctrl Pts',(31.2069270421898,18.8657633326497,39.7729178434176));
#69549=CARTESIAN_POINT('Ctrl Pts',(31.1344336463167,18.8279018088253,39.7686752898451));
#69550=CARTESIAN_POINT('Ctrl Pts',(31.0622803324936,18.79021790152,39.7644526390002));
#69551=CARTESIAN_POINT('Ctrl Pts',(30.9883008394824,18.7561609829746,39.7602299881554));
#69552=CARTESIAN_POINT('Ctrl Pts',(30.9128978276724,18.7258918657568,39.7560073373105));
#69553=CARTESIAN_POINT('Ctrl Pts',(30.836961717461,18.6954087462384,39.7517548323742));
#69554=CARTESIAN_POINT('Ctrl Pts',(30.7595823337707,18.6687673523469,39.7475023274378));
#69555=CARTESIAN_POINT('Ctrl Pts',(30.681185636754,18.6460806347115,39.7432498225014));
#69556=CARTESIAN_POINT('Ctrl Pts',(30.6027889397373,18.6233939170762,39.7389973175651));
#69557=CARTESIAN_POINT('Ctrl Pts',(30.5233754057877,18.604661923107,39.7347448126287));
#69558=CARTESIAN_POINT('Ctrl Pts',(30.4433786738126,18.5899448965619,39.7304923076923));
#69559=CARTESIAN_POINT('Ctrl Pts',(30.3637741999414,18.5753000338763,39.7262606546018));
#69560=CARTESIAN_POINT('Ctrl Pts',(30.2832944898639,18.5645760415146,39.7220290015113));
#69561=CARTESIAN_POINT('Ctrl Pts',(30.2023599501657,18.5578696389077,39.7177973484208));
#69562=CARTESIAN_POINT('Ctrl Pts',(30.1215412759699,18.5511728371549,39.7135717533447));
#69563=CARTESIAN_POINT('Ctrl Pts',(30.0402695246898,18.5484822400873,39.7093461582686));
#69564=CARTESIAN_POINT('Ctrl Pts',(29.9589746360341,18.5498434397958,39.7051205631925));
#69565=CARTESIAN_POINT('Ctrl Pts',(29.8775637197526,18.5512065822682,39.7008889371621));
#69566=CARTESIAN_POINT('Ctrl Pts',(29.7961300642939,18.5566331641844,39.6966573111316));
#69567=CARTESIAN_POINT('Ctrl Pts',(29.715109958262,18.5661167008013,39.6924256851012));
#69568=CARTESIAN_POINT('Ctrl Pts',(29.6343504831417,18.5755697301414,39.6882076716492));
#69569=CARTESIAN_POINT('Ctrl Pts',(29.5540023659258,18.5890536150994,39.6839896581971));
#69570=CARTESIAN_POINT('Ctrl Pts',(29.4744952008885,18.6065098796714,39.6797716447451));
#69571=CARTESIAN_POINT('Ctrl Pts',(29.3950141980744,18.6239604001737,39.6755550192512));
#69572=CARTESIAN_POINT('Ctrl Pts',(29.3163740515445,18.6453806048803,39.6713383937572));
#69573=CARTESIAN_POINT('Ctrl Pts',(29.238994514479,18.6706608445727,39.6671217682633));
#69574=CARTESIAN_POINT('Ctrl Pts',(29.1616167486238,18.6959405056027,39.6629052392875));
#69575=CARTESIAN_POINT('Ctrl Pts',(29.0854999763348,18.7250798805249,39.6586887103117));
#69576=CARTESIAN_POINT('Ctrl Pts',(29.0110477497606,18.7579197836058,39.6544721813359));
#69577=CARTESIAN_POINT('Ctrl Pts',(28.9361360008617,18.7909623759721,39.650229627763));
#69578=CARTESIAN_POINT('Ctrl Pts',(28.8629098570549,18.8277511550815,39.6459870741902));
#69579=CARTESIAN_POINT('Ctrl Pts',(28.7917572692283,18.8680760441476,39.6417445206173));
#69580=CARTESIAN_POINT('Ctrl Pts',(28.720938473444,18.9082117605147,39.6375218697727));
#69581=CARTESIAN_POINT('Ctrl Pts',(28.6521741878427,18.9518501852333,39.6332992189281));
#69582=CARTESIAN_POINT('Ctrl Pts',(28.5858180661943,18.9987404695798,39.6290765680836));
#69583=CARTESIAN_POINT('Ctrl Pts',(28.5189928075365,19.0459622676921,39.6248240631466));
#69584=CARTESIAN_POINT('Ctrl Pts',(28.4546102735963,19.0964817907916,39.6205715582096));
#69585=CARTESIAN_POINT('Ctrl Pts',(28.3929965731608,19.1500026388864,39.6163190532725));
#69586=CARTESIAN_POINT('Ctrl Pts',(28.3313828727253,19.2035234869813,39.6120665483355));
#69587=CARTESIAN_POINT('Ctrl Pts',(28.2725383042427,19.2600452857358,39.6078140433985));
#69588=CARTESIAN_POINT('Ctrl Pts',(28.2167488821321,19.3192365720831,39.6035615384615));
#69589=CARTESIAN_POINT('Ctrl Pts',(28.1619247299333,19.3774037293825,39.5993826104664));
#69590=CARTESIAN_POINT('Ctrl Pts',(28.1098346741667,19.4383783064752,39.5952036824712));
#69591=CARTESIAN_POINT('Ctrl Pts',(28.0607848511331,19.5018695462661,39.591024754476));
#69592=CARTESIAN_POINT('Ctrl Pts',(28.0117989128589,19.565278092128,39.5868512693101));
#69593=CARTESIAN_POINT('Ctrl Pts',(27.9658456427512,19.6311964262606,39.5826777841441));
#69594=CARTESIAN_POINT('Ctrl Pts',(27.9231939713022,19.6992975093571,39.5785042989781));
#69595=CARTESIAN_POINT('Ctrl Pts',(27.8805840156664,19.7673319856371,39.5743348957232));
#69596=CARTESIAN_POINT('Ctrl Pts',(27.8412695038561,19.8375445733112,39.5701654924682));
#69597=CARTESIAN_POINT('Ctrl Pts',(27.8054777346368,19.9095770193062,39.5659960892133));
#69598=CARTESIAN_POINT('Ctrl Pts',(27.7697093675961,19.9815623674292,39.5618294120912));
#69599=CARTESIAN_POINT('Ctrl Pts',(27.7374593826102,20.0553647856335,39.5576627349692));
#69600=CARTESIAN_POINT('Ctrl Pts',(27.7089097304738,20.130600421623,39.5534960578471));
#69601=CARTESIAN_POINT('Ctrl Pts',(27.6803605581769,20.2058347931124,39.5493294507552));
#69602=CARTESIAN_POINT('Ctrl Pts',(27.6555117808199,20.2825018947326,39.5451628436633));
#69603=CARTESIAN_POINT('Ctrl Pts',(27.634497180122,20.3601979531531,39.5409962365714));
#69604=CARTESIAN_POINT('Ctrl Pts',(27.613483522936,20.4378905231823,39.5368298165515));
#69605=CARTESIAN_POINT('Ctrl Pts',(27.5963038170669,20.5166114951214,39.5326633965316));
#69606=CARTESIAN_POINT('Ctrl Pts',(27.583041376474,20.5959439863545,39.5284969765117));
#69607=CARTESIAN_POINT('Ctrl Pts',(27.5697678174451,20.675342985197,39.5243270636148));
#69608=CARTESIAN_POINT('Ctrl Pts',(27.5604181510839,20.7553540542034,39.5201571507179));
#69609=CARTESIAN_POINT('Ctrl Pts',(27.5550240342586,20.8355531181594,39.515987237821));
#69610=CARTESIAN_POINT('Ctrl Pts',(27.5512900107855,20.8910701188177,39.5131006572847));
#69611=CARTESIAN_POINT('Ctrl Pts',(27.5494503831303,20.9466770746821,39.5102140767484));
#69612=CARTESIAN_POINT('Ctrl Pts',(27.5495010177774,21.0022334113197,39.5073274962121));
#69613=CARTESIAN_POINT('',(27.5495001606026,20.9991128058326,38.7073274961651));
#69614=CARTESIAN_POINT('Ctrl Pts',(27.5495010177781,21.0022334121089,39.5073274961711));
#69615=CARTESIAN_POINT('Ctrl Pts',(27.549598400284,21.1090814633755,39.501775915131));
#69616=CARTESIAN_POINT('Ctrl Pts',(27.5566877679976,21.2156197797143,39.496224334091));
#69617=CARTESIAN_POINT('Ctrl Pts',(27.5706261347395,21.3210807885708,39.490672753051));
#69618=CARTESIAN_POINT('Ctrl Pts',(27.5823778813055,21.4099973073873,39.4859920917776));
#69619=CARTESIAN_POINT('Ctrl Pts',(27.5989973949366,21.4981487045857,39.4813114305042));
#69620=CARTESIAN_POINT('Ctrl Pts',(27.6203735160512,21.5850880676353,39.4766307692308));
#69621=CARTESIAN_POINT('Ctrl Pts',(27.6396990608233,21.6636874797587,39.4723991161391));
#69622=CARTESIAN_POINT('Ctrl Pts',(27.6629591567608,21.7414753688337,39.4681674630475));
#69623=CARTESIAN_POINT('Ctrl Pts',(27.6900694109329,21.8180286814607,39.4639358099558));
#69624=CARTESIAN_POINT('Ctrl Pts',(27.7171408541942,21.8944724007294,39.4597102148786));
#69625=CARTESIAN_POINT('Ctrl Pts',(27.7480513547551,21.9696846193321,39.4554846198013));
#69626=CARTESIAN_POINT('Ctrl Pts',(27.7826659856413,22.0432545800369,39.4512590247241));
#69627=CARTESIAN_POINT('Ctrl Pts',(27.817330020033,22.1169295429869,39.4470273986939));
#69628=CARTESIAN_POINT('Ctrl Pts',(27.8557086376473,22.1889571053602,39.4427957726638));
#69629=CARTESIAN_POINT('Ctrl Pts',(27.8976168188683,22.2589420994209,39.4385641466336));
#69630=CARTESIAN_POINT('Ctrl Pts',(27.9393901870549,22.3287019610819,39.4343461331805));
#69631=CARTESIAN_POINT('Ctrl Pts',(27.9846702200657,22.3964319670426,39.4301281197273));
#69632=CARTESIAN_POINT('Ctrl Pts',(28.0332272382171,22.4617643974009,39.4259101062742));
#69633=CARTESIAN_POINT('Ctrl Pts',(28.081768278443,22.527075329802,39.4216934807791));
#69634=CARTESIAN_POINT('Ctrl Pts',(28.1335838853661,22.5899898805696,39.417476855284));
#69635=CARTESIAN_POINT('Ctrl Pts',(28.1884017569896,22.6501703111866,39.4132602297889));
#69636=CARTESIAN_POINT('Ctrl Pts',(28.243218373837,22.7103493642791,39.409043700812));
#69637=CARTESIAN_POINT('Ctrl Pts',(28.3010368049129,22.7677940787939,39.4048271718351));
#69638=CARTESIAN_POINT('Ctrl Pts',(28.3615462292325,22.8222018250067,39.4006106428582));
#69639=CARTESIAN_POINT('Ctrl Pts',(28.4224291202698,22.8769453781227,39.3963680892867));
#69640=CARTESIAN_POINT('Ctrl Pts',(28.4860359929807,22.9286140160432,39.3921255357152));
#69641=CARTESIAN_POINT('Ctrl Pts',(28.5520160260383,22.9769402270049,39.3878829821437));
#69642=CARTESIAN_POINT('Ctrl Pts',(28.6176865326547,23.0250397293791,39.383660331298));
#69643=CARTESIAN_POINT('Ctrl Pts',(28.685707561096,23.0698278838322,39.3794376804523));
#69644=CARTESIAN_POINT('Ctrl Pts',(28.7557051918887,23.1110851902534,39.3752150296066));
#69645=CARTESIAN_POINT('Ctrl Pts',(28.826197705057,23.1526341853158,39.3709625246722));
#69646=CARTESIAN_POINT('Ctrl Pts',(28.8986944549242,23.1906019893261,39.3667100197378));
#69647=CARTESIAN_POINT('Ctrl Pts',(28.9727912939311,23.2248129189162,39.3624575148033));
#69648=CARTESIAN_POINT('Ctrl Pts',(29.0468881329381,23.2590238485062,39.3582050098689));
#69649=CARTESIAN_POINT('Ctrl Pts',(29.1225845972269,23.2894777852095,39.3539525049345));
#69650=CARTESIAN_POINT('Ctrl Pts',(29.1994610266245,23.3160499999151,39.3497));
#69651=CARTESIAN_POINT('Ctrl Pts',(29.2759604981033,23.3424919197198,39.3454683469109));
#69652=CARTESIAN_POINT('Ctrl Pts',(29.3539145146842,23.3651890349848,39.3412366938217));
#69653=CARTESIAN_POINT('Ctrl Pts',(29.4329219799901,23.3839825438165,39.3370050407325));
#69654=CARTESIAN_POINT('Ctrl Pts',(29.5118163385842,23.4027491479502,39.3327794456578));
#69655=CARTESIAN_POINT('Ctrl Pts',(29.5917607022621,23.4176231380356,39.3285538505831));
#69656=CARTESIAN_POINT('Ctrl Pts',(29.6723368661057,23.4284948261601,39.3243282555084));
#69657=CARTESIAN_POINT('Ctrl Pts',(29.7530280318121,23.4393820308386,39.3200966294776));
#69658=CARTESIAN_POINT('Ctrl Pts',(29.8343523537307,23.4462553632716,39.3158650034468));
#69659=CARTESIAN_POINT('Ctrl Pts',(29.9158775237706,23.4490556667812,39.311633377416));
#69660=CARTESIAN_POINT('Ctrl Pts',(29.9971404381428,23.4518469620855,39.3074153639653));
#69661=CARTESIAN_POINT('Ctrl Pts',(30.0786024449596,23.4505913604899,39.3031973505147));
#69662=CARTESIAN_POINT('Ctrl Pts',(30.1598300409076,23.4452821121546,39.298979337064));
#69663=CARTESIAN_POINT('Ctrl Pts',(30.2410309085164,23.4399746108536,39.2947627115714));
#69664=CARTESIAN_POINT('Ctrl Pts',(30.3219970549808,23.4306161420215,39.2905460860788));
#69665=CARTESIAN_POINT('Ctrl Pts',(30.4022970157302,23.4172520268136,39.2863294605861));
#69666=CARTESIAN_POINT('Ctrl Pts',(30.4825951384213,23.4038882175091,39.2821129316117));
#69667=CARTESIAN_POINT('Ctrl Pts',(30.5622266474021,23.3865190215507,39.2778964026372));
#69668=CARTESIAN_POINT('Ctrl Pts',(30.6407686505217,23.3652411687836,39.2736798736627));
#69669=CARTESIAN_POINT('Ctrl Pts',(30.7197954182962,23.3438319881849,39.2694373200883));
#69670=CARTESIAN_POINT('Ctrl Pts',(30.7977187218238,23.318465845832,39.2651947665138));
#69671=CARTESIAN_POINT('Ctrl Pts',(30.8741234448468,23.2892921292769,39.2609522129393));
#69672=CARTESIAN_POINT('Ctrl Pts',(30.9501697368838,23.2602552728997,39.256729562096));
#69673=CARTESIAN_POINT('Ctrl Pts',(31.0247112581349,23.2274467268812,39.2525069112527));
#69674=CARTESIAN_POINT('Ctrl Pts',(31.0973606725139,23.191061342003,39.2482842604094));
#69675=CARTESIAN_POINT('Ctrl Pts',(31.1705237174829,23.1544187128391,39.2440317554694));
#69676=CARTESIAN_POINT('Ctrl Pts',(31.2417673802195,23.1141487063814,39.2397792505294));
#69677=CARTESIAN_POINT('Ctrl Pts',(31.3107247110944,23.0704953469464,39.2355267455893));
#69678=CARTESIAN_POINT('Ctrl Pts',(31.3796820419693,23.0268419875113,39.2312742406493));
#69679=CARTESIAN_POINT('Ctrl Pts',(31.446352689667,22.9798056003307,39.2270217357093));
#69680=CARTESIAN_POINT('Ctrl Pts',(31.510404074096,22.9296709001678,39.2227692307692));
#69681=CARTESIAN_POINT('Ctrl Pts',(31.5741413872004,22.8797820318761,39.2185375776792));
#69682=CARTESIAN_POINT('Ctrl Pts',(31.6355234891141,22.8266385909933,39.2143059245891));
#69683=CARTESIAN_POINT('Ctrl Pts',(31.6941992637275,22.7704912043795,39.2100742714991));
#69684=CARTESIAN_POINT('Ctrl Pts',(31.7527910383807,22.7144241980977,39.2058486764235));
#69685=CARTESIAN_POINT('Ctrl Pts',(31.8086838475751,22.655362105796,39.2016230813479));
#69686=CARTESIAN_POINT('Ctrl Pts',(31.8615585328514,22.5935965859553,39.1973974862723));
#69687=CARTESIAN_POINT('Ctrl Pts',(31.9145086832022,22.5317429116502,39.1931658602417));
#69688=CARTESIAN_POINT('Ctrl Pts',(31.9644317291242,22.4671783895145,39.1889342342112));
#69689=CARTESIAN_POINT('Ctrl Pts',(32.0110432916244,22.4002339551705,39.1847026081806));
#69690=CARTESIAN_POINT('Ctrl Pts',(32.0575049109165,22.3335048721838,39.1804845947291));
#69691=CARTESIAN_POINT('Ctrl Pts',(32.1006760392652,22.2644115384322,39.1762665812777));
#69692=CARTESIAN_POINT('Ctrl Pts',(32.1403156599763,22.1933143448648,39.1720485678262));
#69693=CARTESIAN_POINT('Ctrl Pts',(32.1799422370754,22.1222405461785,39.1678319423328));
#69694=CARTESIAN_POINT('Ctrl Pts',(32.2160393880842,22.0491646027831,39.1636153168394));
#69695=CARTESIAN_POINT('Ctrl Pts',(32.2484109322814,21.9744734627468,39.159398691346));
#69696=CARTESIAN_POINT('Ctrl Pts',(32.2807817354968,21.8997840323839,39.1551821623708));
#69697=CARTESIAN_POINT('Ctrl Pts',(32.3094269176567,21.8234799058125,39.1509656333956));
#69698=CARTESIAN_POINT('Ctrl Pts',(32.334198124931,21.7459687416832,39.1467491044204));
#69699=CARTESIAN_POINT('Ctrl Pts',(32.3591222211625,21.6679791753136,39.1425065508469));
#69700=CARTESIAN_POINT('Ctrl Pts',(32.3801241981086,21.5887680689479,39.1382639972734));
#69701=CARTESIAN_POINT('Ctrl Pts',(32.3971041453202,21.5087651388298,39.1340214436999));
#69702=CARTESIAN_POINT('Ctrl Pts',(32.4140044359546,21.4291375196302,39.1297987928559));
#69703=CARTESIAN_POINT('Ctrl Pts',(32.4269203299235,21.3487259609619,39.1255761420119));
#69704=CARTESIAN_POINT('Ctrl Pts',(32.4358051785355,21.2679615312307,39.121353491168));
#69705=CARTESIAN_POINT('Ctrl Pts',(32.444752842928,21.186626097884,39.1171009862297));
#69706=CARTESIAN_POINT('Ctrl Pts',(32.4496122121228,21.1049332620539,39.1128484812915));
#69707=CARTESIAN_POINT('Ctrl Pts',(32.4503890010604,21.0233236678556,39.1085959763532));
#69708=CARTESIAN_POINT('Ctrl Pts',(32.451165789998,20.9417140736573,39.104343471415));
#69709=CARTESIAN_POINT('Ctrl Pts',(32.4478600810791,20.8601881926928,39.1000909664767));
#69710=CARTESIAN_POINT('Ctrl Pts',(32.4405304201813,20.7791798963641,39.0958384615385));
#69711=CARTESIAN_POINT('Ctrl Pts',(32.4332366997276,20.6985688181592,39.0916068084402));
#69712=CARTESIAN_POINT('Ctrl Pts',(32.4219311541044,20.6181687409942,39.087375155342));
#69713=CARTESIAN_POINT('Ctrl Pts',(32.4066336390494,20.5384105965297,39.0831435022437));
#69714=CARTESIAN_POINT('Ctrl Pts',(32.3913580238441,20.4587666334451,39.0789179071599));
#69715=CARTESIAN_POINT('Ctrl Pts',(32.3721018763099,20.3797632305195,39.074692312076));
#69716=CARTESIAN_POINT('Ctrl Pts',(32.3489368602303,20.3018267574222,39.0704667169922));
#69717=CARTESIAN_POINT('Ctrl Pts',(32.3257387820782,20.2237790501559,39.0662350909637));
#69718=CARTESIAN_POINT('Ctrl Pts',(32.2986207283465,20.1468017860686,39.0620034649352));
#69719=CARTESIAN_POINT('Ctrl Pts',(32.2677062294127,20.071313450575,39.0577718389066));
#69720=CARTESIAN_POINT('Ctrl Pts',(32.236891178242,19.9960679508499,39.0535538254469));
#69721=CARTESIAN_POINT('Ctrl Pts',(32.2023042310867,19.9223022528441,39.0493358119872));
#69722=CARTESIAN_POINT('Ctrl Pts',(32.16411719618,19.8504144176277,39.0451177985274));
#69723=CARTESIAN_POINT('Ctrl Pts',(32.1259427269048,19.7785502374569,39.0409011730257));
#69724=CARTESIAN_POINT('Ctrl Pts',(32.0841707402906,19.7085631031235,39.036684547524));
#69725=CARTESIAN_POINT('Ctrl Pts',(32.0390196885697,19.6408278403288,39.0324679220224));
#69726=CARTESIAN_POINT('Ctrl Pts',(31.9938696703524,19.5730941279884,39.0282513930389));
#69727=CARTESIAN_POINT('Ctrl Pts',(31.9453409995579,19.5076125708324,39.0240348640554));
#69728=CARTESIAN_POINT('Ctrl Pts',(31.8936954862696,19.4447290733502,39.0198183350719));
#69729=CARTESIAN_POINT('Ctrl Pts',(31.8417312148731,19.3814574564861,39.0155757815082));
#69730=CARTESIAN_POINT('Ctrl Pts',(31.786611784374,19.3208164575192,39.0113332279445));
#69731=CARTESIAN_POINT('Ctrl Pts',(31.7286438286116,19.2631232732853,39.0070906743809));
#69732=CARTESIAN_POINT('Ctrl Pts',(31.670947812728,19.2057007399192,39.0028680235287));
#69733=CARTESIAN_POINT('Ctrl Pts',(31.6104303236937,19.1511986974807,38.9986453726766));
#69734=CARTESIAN_POINT('Ctrl Pts',(31.5474280466105,19.0998903477527,38.9944227218245));
#69735=CARTESIAN_POINT('Ctrl Pts',(31.4839803445355,19.0482192488939,38.990170216905));
#69736=CARTESIAN_POINT('Ctrl Pts',(31.4180129681252,18.999787460934,38.9859177119856));
#69737=CARTESIAN_POINT('Ctrl Pts',(31.3498990722644,18.9548294093891,38.9816652070661));
#69738=CARTESIAN_POINT('Ctrl Pts',(31.2817851764036,18.9098713578442,38.9774127021467));
#69739=CARTESIAN_POINT('Ctrl Pts',(31.2115252018782,18.8683872295464,38.9731601972272));
#69740=CARTESIAN_POINT('Ctrl Pts',(31.1395152976815,18.8305634057779,38.9689076923078));
#69741=CARTESIAN_POINT('Ctrl Pts',(31.0678584887123,18.7929250483256,38.964676039231));
#69742=CARTESIAN_POINT('Ctrl Pts',(30.9942008652579,18.7587703676255,38.9604443861542));
#69743=CARTESIAN_POINT('Ctrl Pts',(30.9189151027149,18.7283166409021,38.9562127330774));
#69744=CARTESIAN_POINT('Ctrl Pts',(30.8437371189115,18.697906511589,38.951987138015));
#69745=CARTESIAN_POINT('Ctrl Pts',(30.7669360525442,18.6711869862405,38.9477615429526));
#69746=CARTESIAN_POINT('Ctrl Pts',(30.6889088743533,18.6483293570661,38.9435359478903));
#69747=CARTESIAN_POINT('Ctrl Pts',(30.6107703320392,18.6254391043893,38.9393043218564));
#69748=CARTESIAN_POINT('Ctrl Pts',(30.5314025984032,18.6064219829982,38.9350726958225));
#69749=CARTESIAN_POINT('Ctrl Pts',(30.4512241812916,18.591401447269,38.9308410697886));
#69750=CARTESIAN_POINT('Ctrl Pts',(30.371303687812,18.576429230667,38.9266230563502));
#69751=CARTESIAN_POINT('Ctrl Pts',(30.2905781738591,18.565428028317,38.9224050429117));
#69752=CARTESIAN_POINT('Ctrl Pts',(30.2094752049009,18.5584696625822,38.9181870294733));
#69753=CARTESIAN_POINT('Ctrl Pts',(30.1283989232716,18.5515135865316,38.9139704039928));
#69754=CARTESIAN_POINT('Ctrl Pts',(30.0469458960343,18.5485977449462,38.9097537785123));
#69755=CARTESIAN_POINT('Ctrl Pts',(29.9655494985754,18.5497421741883,38.9055371530318));
#69756=CARTESIAN_POINT('Ctrl Pts',(29.8841549642704,18.5508865772346,38.9013206240694));
#69757=CARTESIAN_POINT('Ctrl Pts',(29.8028175219104,18.5560910586578,38.897104095107));
#69758=CARTESIAN_POINT('Ctrl Pts',(29.7219697977931,18.5653235416876,38.8928875661446));
#69759=CARTESIAN_POINT('Ctrl Pts',(29.6406230775002,18.5746130080619,38.8886450125556));
#69760=CARTESIAN_POINT('Ctrl Pts',(29.5597726157875,18.5879803301642,38.8844024589666));
#69761=CARTESIAN_POINT('Ctrl Pts',(29.4798512650611,18.6053402029638,38.8801599053776));
#69762=CARTESIAN_POINT('Ctrl Pts',(29.40030484307,18.62261863676,38.875937254546));
#69763=CARTESIAN_POINT('Ctrl Pts',(29.3216792720991,18.6438520687983,38.8717146037144));
#69764=CARTESIAN_POINT('Ctrl Pts',(29.2443867723394,18.6689060722089,38.8674919528828));
#69765=CARTESIAN_POINT('Ctrl Pts',(29.1665478147042,18.694137207392,38.8632394479152));
#69766=CARTESIAN_POINT('Ctrl Pts',(29.0900612987055,18.7232429775573,38.8589869429475));
#69767=CARTESIAN_POINT('Ctrl Pts',(29.0153266796838,18.7560372769902,38.8547344379799));
#69768=CARTESIAN_POINT('Ctrl Pts',(28.9405920606622,18.7888315764231,38.8504819330122));
#69769=CARTESIAN_POINT('Ctrl Pts',(28.8676097348207,18.825314136383,38.8462294280446));
#69770=CARTESIAN_POINT('Ctrl Pts',(28.7967512934842,18.8652534576048,38.8419769230769));
#69771=CARTESIAN_POINT('Ctrl Pts',(28.7262403018338,18.9049969390035,38.8377452699865));
#69772=CARTESIAN_POINT('Ctrl Pts',(28.6575686579746,18.9483119833915,38.833513616896));
#69773=CARTESIAN_POINT('Ctrl Pts',(28.5911211558115,18.9950035779588,38.8292819638055));
#69774=CARTESIAN_POINT('Ctrl Pts',(28.524768779579,19.0416283290596,38.8250563687297));
#69775=CARTESIAN_POINT('Ctrl Pts',(28.4606345982962,19.0916197648742,38.8208307736538));
#69776=CARTESIAN_POINT('Ctrl Pts',(28.3990779776216,19.1447375042157,38.8166051785779));
#69777=CARTESIAN_POINT('Ctrl Pts',(28.3374335006382,19.1979310555244,38.8123735525474));
#69778=CARTESIAN_POINT('Ctrl Pts',(28.2783743476177,19.2542595960153,38.8081419265169));
#69779=CARTESIAN_POINT('Ctrl Pts',(28.2222314025319,19.3134386866003,38.8039103004865));
#69780=CARTESIAN_POINT('Ctrl Pts',(28.1662690618457,19.3724274059088,38.799692287035));
#69781=CARTESIAN_POINT('Ctrl Pts',(28.1132045287195,19.4342480368791,38.7954742735836));
#69782=CARTESIAN_POINT('Ctrl Pts',(28.0633302440097,19.4985805029132,38.7912562601321));
#69783=CARTESIAN_POINT('Ctrl Pts',(28.0134723706798,19.5628918000313,38.7870396346389));
#69784=CARTESIAN_POINT('Ctrl Pts',(27.9668029456149,19.6297129237595,38.7828230091456));
#69785=CARTESIAN_POINT('Ctrl Pts',(27.9235740740609,19.6986908038103,38.7786063836524));
#69786=CARTESIAN_POINT('Ctrl Pts',(27.880346192013,19.7676671049618,38.7743898546774));
#69787=CARTESIAN_POINT('Ctrl Pts',(27.8405589527655,19.8387996698277,38.7701733257024));
#69788=CARTESIAN_POINT('Ctrl Pts',(27.8044202903554,19.9117077650754,38.7659567967275));
#69789=CARTESIAN_POINT('Ctrl Pts',(27.7680585785642,19.9850658522277,38.761714243154));
#69790=CARTESIAN_POINT('Ctrl Pts',(27.735390861715,20.0602210428876,38.7574716895806));
#69791=CARTESIAN_POINT('Ctrl Pts',(27.7065804955838,20.1367635163158,38.7532291360071));
#69792=CARTESIAN_POINT('Ctrl Pts',(27.6779052850677,20.2129469125621,38.7490064851637));
#69793=CARTESIAN_POINT('Ctrl Pts',(27.6530514045033,20.2905041411395,38.7447838343202));
#69794=CARTESIAN_POINT('Ctrl Pts',(27.6321297560303,20.369016040043,38.7405611834768));
#69795=CARTESIAN_POINT('Ctrl Pts',(27.611060191733,20.4480830172075,38.7363086785383));
#69796=CARTESIAN_POINT('Ctrl Pts',(27.5939787781578,20.5281177484648,38.7320561735999));
#69797=CARTESIAN_POINT('Ctrl Pts',(27.5809460876128,20.6086837353699,38.7278036686615));
#69798=CARTESIAN_POINT('Ctrl Pts',(27.5679133970677,20.689249722275,38.723551163723));
#69799=CARTESIAN_POINT('Ctrl Pts',(27.5589294189629,20.7703464861984,38.7192986587846));
#69800=CARTESIAN_POINT('Ctrl Pts',(27.5540014768481,20.8515362847741,38.7150461538462));
#69801=CARTESIAN_POINT('Ctrl Pts',(27.5510199323564,20.9006584114312,38.7124732679681));
#69802=CARTESIAN_POINT('Ctrl Pts',(27.5495179883392,20.949871249837,38.7099003820901));
#69803=CARTESIAN_POINT('Ctrl Pts',(27.549500160603,20.9991128049331,38.7073274962121));
#69804=CARTESIAN_POINT('',(27.5495005462907,20.99836373272,37.907327496241));
#69805=CARTESIAN_POINT('Ctrl Pts',(27.5495001606026,20.9991128058326,38.7073274961651));
#69806=CARTESIAN_POINT('Ctrl Pts',(27.5494711067375,21.0793618588582,38.7031344593114));
#69807=CARTESIAN_POINT('Ctrl Pts',(27.5533883013094,21.1597704716766,38.6989414224577));
#69808=CARTESIAN_POINT('Ctrl Pts',(27.5612725675742,21.2399140686456,38.6947483856039));
#69809=CARTESIAN_POINT('Ctrl Pts',(27.5691459480749,21.3199470117787,38.6905611380538));
#69810=CARTESIAN_POINT('Ctrl Pts',(27.5809754805987,21.3997151977181,38.6863738905036));
#69811=CARTESIAN_POINT('Ctrl Pts',(27.5967299704161,21.478793708087,38.6821866429535));
#69812=CARTESIAN_POINT('Ctrl Pts',(27.6124677386434,21.5577882856565,38.678003839688));
#69813=CARTESIAN_POINT('Ctrl Pts',(27.6321220969125,21.6360941791158,38.6738210364225));
#69814=CARTESIAN_POINT('Ctrl Pts',(27.6556101820904,21.7132928092179,38.6696382331569));
#69815=CARTESIAN_POINT('Ctrl Pts',(27.6790850761053,21.7904480837333,38.665457778999));
#69816=CARTESIAN_POINT('Ctrl Pts',(27.7063892872424,21.8664968763102,38.6612773248411));
#69817=CARTESIAN_POINT('Ctrl Pts',(27.7373894349208,21.941033304826,38.6570968706832));
#69818=CARTESIAN_POINT('Ctrl Pts',(27.7683820864734,22.0155517097361,38.6529174273983));
#69819=CARTESIAN_POINT('Ctrl Pts',(27.8030687180136,22.088558039289,38.6487379841133));
#69820=CARTESIAN_POINT('Ctrl Pts',(27.8412674537946,22.1596654879549,38.6445585408283));
#69821=CARTESIAN_POINT('Ctrl Pts',(27.8794691687436,22.2307784823811,38.6403787715833));
#69822=CARTESIAN_POINT('Ctrl Pts',(27.9211833053754,22.2999918854674,38.6361990023382));
#69823=CARTESIAN_POINT('Ctrl Pts',(27.9661823386697,22.3669440260892,38.6320192330931));
#69824=CARTESIAN_POINT('Ctrl Pts',(28.0112278203437,22.4339652752721,38.6278351494552));
#69825=CARTESIAN_POINT('Ctrl Pts',(28.059564700567,22.4987202098391,38.6236510658172));
#69826=CARTESIAN_POINT('Ctrl Pts',(28.1109228983345,22.5608773026612,38.6194669821793));
#69827=CARTESIAN_POINT('Ctrl Pts',(28.1623107882717,22.6230703309139,38.61528047956));
#69828=CARTESIAN_POINT('Ctrl Pts',(28.2167231511567,22.6826621798126,38.6110939769407));
#69829=CARTESIAN_POINT('Ctrl Pts',(28.2738522415331,22.7393574002889,38.6069074743215));
#69830=CARTESIAN_POINT('Ctrl Pts',(28.3310758382662,22.7961464093884,38.6027140461393));
#69831=CARTESIAN_POINT('Ctrl Pts',(28.3910247788405,22.8500289114947,38.5985206179571));
#69832=CARTESIAN_POINT('Ctrl Pts',(28.453357875113,22.9007494278639,38.5943271897749));
#69833=CARTESIAN_POINT('Ctrl Pts',(28.484136276635,22.9257938506756,38.5922565880551));
#69834=CARTESIAN_POINT('Ctrl Pts',(28.5154955090315,22.9500680076986,38.5901859863352));
#69835=CARTESIAN_POINT('Ctrl Pts',(28.5473920865824,22.9735451603337,38.5881153846154));
#69836=CARTESIAN_POINT('Ctrl Pts',(28.6125785711537,23.0215250116385,38.5838837316473));
#69837=CARTESIAN_POINT('Ctrl Pts',(28.6802666916773,23.0663614446907,38.5796520786793));
#69838=CARTESIAN_POINT('Ctrl Pts',(28.7501206589528,23.107783642318,38.5754204257113));
#69839=CARTESIAN_POINT('Ctrl Pts',(28.8198746236198,23.1491465401236,38.5711948307576));
#69840=CARTESIAN_POINT('Ctrl Pts',(28.8917878804878,23.187104675046,38.5669692358039));
#69841=CARTESIAN_POINT('Ctrl Pts',(28.9654937100691,23.2214290414266,38.5627436408502));
#69842=CARTESIAN_POINT('Ctrl Pts',(29.0393047385103,23.2558023982904,38.5585120147891));
#69843=CARTESIAN_POINT('Ctrl Pts',(29.114913072776,23.2865313416713,38.554280388728));
#69844=CARTESIAN_POINT('Ctrl Pts',(29.1919235115136,23.3134309237052,38.550048762667));
#69845=CARTESIAN_POINT('Ctrl Pts',(29.2686862151446,23.3402439723946,38.5458307493362));
#69846=CARTESIAN_POINT('Ctrl Pts',(29.3468415814648,23.3632520899016,38.5416127360055));
#69847=CARTESIAN_POINT('Ctrl Pts',(29.4259776948736,23.3823200127643,38.5373947226747));
#69848=CARTESIAN_POINT('Ctrl Pts',(29.5050877681678,23.4013816612363,38.5331780973013));
#69849=CARTESIAN_POINT('Ctrl Pts',(29.5851774961455,23.4165055810472,38.5289614719279));
#69850=CARTESIAN_POINT('Ctrl Pts',(29.6658214365974,23.4276068334395,38.5247448465545));
#69851=CARTESIAN_POINT('Ctrl Pts',(29.7464635311333,23.4387078317274,38.5205283176984));
#69852=CARTESIAN_POINT('Ctrl Pts',(29.8276593523034,23.4457862834033,38.5163117888423));
#69853=CARTESIAN_POINT('Ctrl Pts',(29.9089763666407,23.4488088835534,38.5120952599862));
#69854=CARTESIAN_POINT('Ctrl Pts',(29.9907952781647,23.4518501395103,38.5078527062694));
#69855=CARTESIAN_POINT('Ctrl Pts',(30.0727364091553,23.4507852726604,38.5036101525526));
#69856=CARTESIAN_POINT('Ctrl Pts',(30.1543590031072,23.4456335678429,38.4993675988358));
#69857=CARTESIAN_POINT('Ctrl Pts',(30.235598682978,23.4405060310923,38.4951449481076));
#69858=CARTESIAN_POINT('Ctrl Pts',(30.316522348417,23.4313300241304,38.4909222973795));
#69859=CARTESIAN_POINT('Ctrl Pts',(30.3967022585897,23.4181764964596,38.4866996466513));
#69860=CARTESIAN_POINT('Ctrl Pts',(30.4774490472264,23.404929972282,38.4824471414402));
#69861=CARTESIAN_POINT('Ctrl Pts',(30.5574410550114,23.3876495660561,38.4781946362291));
#69862=CARTESIAN_POINT('Ctrl Pts',(30.6362553943134,23.3664592375968,38.473942131018));
#69863=CARTESIAN_POINT('Ctrl Pts',(30.7150697336155,23.3452689091375,38.4696896258069));
#69864=CARTESIAN_POINT('Ctrl Pts',(30.7927059723433,23.3201688645899,38.4654371205957));
#69865=CARTESIAN_POINT('Ctrl Pts',(30.8687619484462,23.291332129337,38.4611846153846));
#69866=CARTESIAN_POINT('Ctrl Pts',(30.9444449854619,23.2626367944878,38.456952962255));
#69867=CARTESIAN_POINT('Ctrl Pts',(31.0188463182413,23.2301340330647,38.4527213091254));
#69868=CARTESIAN_POINT('Ctrl Pts',(31.0915562155446,23.1939588141772,38.4484896559958));
#69869=CARTESIAN_POINT('Ctrl Pts',(31.1641620216863,23.1578353835702,38.4442640608817));
#69870=CARTESIAN_POINT('Ctrl Pts',(31.2350807889251,23.1180501426292,38.4400384657677));
#69871=CARTESIAN_POINT('Ctrl Pts',(31.3039211072694,23.0747867350688,38.4358128706536));
#69872=CARTESIAN_POINT('Ctrl Pts',(31.3728596767549,23.031461580566,38.4315812446328));
#69873=CARTESIAN_POINT('Ctrl Pts',(31.4397134275358,22.9846485057952,38.427349618612));
#69874=CARTESIAN_POINT('Ctrl Pts',(31.5041124865869,22.9345789923633,38.4231179925912));
#69875=CARTESIAN_POINT('Ctrl Pts',(31.5683043831035,22.8846705453733,38.4188999791042));
#69876=CARTESIAN_POINT('Ctrl Pts',(31.6300569781506,22.8315268517084,38.4146819656172));
#69877=CARTESIAN_POINT('Ctrl Pts',(31.6890330493998,22.7754204031821,38.4104639521303));
#69878=CARTESIAN_POINT('Ctrl Pts',(31.7479897142665,22.719332416774,38.4062473266025));
#69879=CARTESIAN_POINT('Ctrl Pts',(31.8041713332021,22.6602839316853,38.4020307010748));
#69880=CARTESIAN_POINT('Ctrl Pts',(31.857275602916,22.5985861205494,38.3978140755471));
#69881=CARTESIAN_POINT('Ctrl Pts',(31.9103786570626,22.5368897216885,38.3935975465388));
#69882=CARTESIAN_POINT('Ctrl Pts',(31.9604041996819,22.4725444703764,38.3893810175304));
#69883=CARTESIAN_POINT('Ctrl Pts',(32.0070894396749,22.4058955263979,38.3851644885221));
#69884=CARTESIAN_POINT('Ctrl Pts',(32.0540628221351,22.3388352234724,38.3809219349914));
#69885=CARTESIAN_POINT('Ctrl Pts',(32.0976542419384,22.2694430741771,38.3766793814607));
#69886=CARTESIAN_POINT('Ctrl Pts',(32.1376406085571,22.1980996947865,38.37243682793));
#69887=CARTESIAN_POINT('Ctrl Pts',(32.1774393912293,22.1270910012851,38.3682141770562));
#69888=CARTESIAN_POINT('Ctrl Pts',(32.2136667108561,22.0541497886899,38.3639915261824));
#69889=CARTESIAN_POINT('Ctrl Pts',(32.2461499309449,21.9796737914818,38.3597688753086));
#69890=CARTESIAN_POINT('Ctrl Pts',(32.2788628061968,21.9046712517313,38.3555163704495));
#69891=CARTESIAN_POINT('Ctrl Pts',(32.3077782648604,21.8281125885284,38.3512638655903));
#69892=CARTESIAN_POINT('Ctrl Pts',(32.3327708232583,21.7504202397021,38.3470113607312));
#69893=CARTESIAN_POINT('Ctrl Pts',(32.3577633816563,21.6727278908758,38.3427588558721));
#69894=CARTESIAN_POINT('Ctrl Pts',(32.3788329783271,21.593902331211,38.338506351013));
#69895=CARTESIAN_POINT('Ctrl Pts',(32.3959065866391,21.5143752308377,38.3342538461538));
#69896=CARTESIAN_POINT('Ctrl Pts',(32.4128964777229,21.4352380766486,38.3300221926527));
#69897=CARTESIAN_POINT('Ctrl Pts',(32.4259930619774,21.3551102505546,38.3257905391517));
#69898=CARTESIAN_POINT('Ctrl Pts',(32.4350872439232,21.2744091188031,38.3215588856506));
#69899=CARTESIAN_POINT('Ctrl Pts',(32.4441684066871,21.1938235183582,38.3173332901619));
#69900=CARTESIAN_POINT('Ctrl Pts',(32.4492584954736,21.1126667003274,38.3131076946732));
#69901=CARTESIAN_POINT('Ctrl Pts',(32.4502992382381,21.0313670701525,38.3088820991846));
#69902=CARTESIAN_POINT('Ctrl Pts',(32.4513414662691,20.9499514155135,38.304650473257));
#69903=CARTESIAN_POINT('Ctrl Pts',(32.4483226999183,20.8683930028803,38.3004188473294));
#69904=CARTESIAN_POINT('Ctrl Pts',(32.4412365337121,20.7871281219388,38.2961872214019));
#69905=CARTESIAN_POINT('Ctrl Pts',(32.4341731618949,20.7061246493881,38.2919692075354));
#69906=CARTESIAN_POINT('Ctrl Pts',(32.4230685416578,20.6254132889681,38.2877511936689));
#69907=CARTESIAN_POINT('Ctrl Pts',(32.4079684338373,20.5454251748686,38.2835331798025));
#69908=CARTESIAN_POINT('Ctrl Pts',(32.3928732947817,20.4654633812526,38.2793165538943));
#69909=CARTESIAN_POINT('Ctrl Pts',(32.3737853652095,20.3862248177235,38.2750999279861));
#69910=CARTESIAN_POINT('Ctrl Pts',(32.3508018475349,20.3081322932622,38.2708833020779));
#69911=CARTESIAN_POINT('Ctrl Pts',(32.327818855955,20.2300415563456,38.2666667726886));
#69912=CARTESIAN_POINT('Ctrl Pts',(32.3009405858815,20.1530972519152,38.2624502432993));
#69913=CARTESIAN_POINT('Ctrl Pts',(32.2703142331859,20.077707458236,38.2582337139101));
#69914=CARTESIAN_POINT('Ctrl Pts',(32.2394988599176,20.0018523717381,38.2539911608278));
#69915=CARTESIAN_POINT('Ctrl Pts',(32.2048891449142,19.9275714968123,38.2497486077456));
#69916=CARTESIAN_POINT('Ctrl Pts',(32.1666836136029,19.8552588202809,38.2455060546633));
#69917=CARTESIAN_POINT('Ctrl Pts',(32.1286573045634,19.7832853627505,38.2412834034114));
#69918=CARTESIAN_POINT('Ctrl Pts',(32.087069127314,19.7132620536026,38.2370607521594));
#69919=CARTESIAN_POINT('Ctrl Pts',(32.0421593746451,19.6455498021155,38.2328381009075));
#69920=CARTESIAN_POINT('Ctrl Pts',(31.9969321249024,19.5773588474421,38.2285855969101));
#69921=CARTESIAN_POINT('Ctrl Pts',(31.9483364356444,19.5115121398233,38.2243330929127));
#69922=CARTESIAN_POINT('Ctrl Pts',(31.8966589444221,19.4483444007952,38.2200805889153));
#69923=CARTESIAN_POINT('Ctrl Pts',(31.8449814531997,19.385176661767,38.2158280849179));
#69924=CARTESIAN_POINT('Ctrl Pts',(31.7902225253688,19.3246882007041,38.2115755809205));
#69925=CARTESIAN_POINT('Ctrl Pts',(31.7327050305537,19.2671746980455,38.2073230769231));
#69926=CARTESIAN_POINT('Ctrl Pts',(31.6754695701505,19.2099432102233,38.203091424885));
#69927=CARTESIAN_POINT('Ctrl Pts',(31.615288477062,19.1554434792139,38.1988597728469));
#69928=CARTESIAN_POINT('Ctrl Pts',(31.5524530267996,19.1039937105641,38.1946281208089));
#69929=CARTESIAN_POINT('Ctrl Pts',(31.4897075314897,19.0526175971753,38.1904025267852));
#69930=CARTESIAN_POINT('Ctrl Pts',(31.4243155826979,19.0042830662424,38.1861769327614));
#69931=CARTESIAN_POINT('Ctrl Pts',(31.356605318602,18.9592716350428,38.1819513387377));
#69932=CARTESIAN_POINT('Ctrl Pts',(31.2887983943488,18.9141959475288,38.1777197124441));
#69933=CARTESIAN_POINT('Ctrl Pts',(31.2186668743795,18.8724531743048,38.1734880861506));
#69934=CARTESIAN_POINT('Ctrl Pts',(31.1465736768083,18.8342855558384,38.169256459857));
#69935=CARTESIAN_POINT('Ctrl Pts',(31.0747124157323,18.7962407293128,38.1650384474495));
#69936=CARTESIAN_POINT('Ctrl Pts',(31.0009024841709,18.7617483218529,38.1608204350419));
#69937=CARTESIAN_POINT('Ctrl Pts',(30.925530791204,18.7310039655096,38.1566024226343));
#69938=CARTESIAN_POINT('Ctrl Pts',(30.8501838995748,18.7002697257118,38.1523857981795));
#69939=CARTESIAN_POINT('Ctrl Pts',(30.7732766971362,18.6732812632354,38.1481691737247));
#69940=CARTESIAN_POINT('Ctrl Pts',(30.6952170290165,18.6501864898325,38.1439525492699));
#69941=CARTESIAN_POINT('Ctrl Pts',(30.6171591475524,18.6270922450306,38.1397360213266));
#69942=CARTESIAN_POINT('Ctrl Pts',(30.5379492988818,18.6078916428931,38.1355194933833));
#69943=CARTESIAN_POINT('Ctrl Pts',(30.45801009866,18.5926826134626,38.13130296544));
#69944=CARTESIAN_POINT('Ctrl Pts',(30.3775774670841,18.5773797050345,38.1270604106277));
#69945=CARTESIAN_POINT('Ctrl Pts',(30.2964069135791,18.5661179192298,38.1228178558154));
#69946=CARTESIAN_POINT('Ctrl Pts',(30.2149370875309,18.5589444294724,38.1185753010031));
#69947=CARTESIAN_POINT('Ctrl Pts',(30.1338494969048,18.5518045958797,38.1143526511643));
#69948=CARTESIAN_POINT('Ctrl Pts',(30.0524659061688,18.5487147433998,38.1101300013255));
#69949=CARTESIAN_POINT('Ctrl Pts',(29.9712198606749,18.5496690114231,38.1059073514867));
#69950=CARTESIAN_POINT('Ctrl Pts',(29.8893993416474,18.5506300268729,38.1016548441876));
#69951=CARTESIAN_POINT('Ctrl Pts',(29.8077187981425,18.5556925467721,38.0974023368886));
#69952=CARTESIAN_POINT('Ctrl Pts',(29.7266149449956,18.5647975727467,38.0931498295895));
#69953=CARTESIAN_POINT('Ctrl Pts',(29.6455110918486,18.5739025987214,38.0888973222905));
#69954=CARTESIAN_POINT('Ctrl Pts',(29.5649843872258,18.5870499919039,38.0846448149914));
#69955=CARTESIAN_POINT('Ctrl Pts',(29.4854584295428,18.6041291307186,38.0803923076923));
#69956=CARTESIAN_POINT('Ctrl Pts',(29.4063224535612,18.6211245163561,38.0761606539621));
#69957=CARTESIAN_POINT('Ctrl Pts',(29.3278814250196,18.6420767085657,38.0719290002319));
#69958=CARTESIAN_POINT('Ctrl Pts',(29.2505607056619,18.6669138476897,38.0676973465016));
#69959=CARTESIAN_POINT('Ctrl Pts',(29.1733506784166,18.691715430039,38.0634717507943));
#69960=CARTESIAN_POINT('Ctrl Pts',(29.0972582138182,18.7203907723405,38.059246155087));
#69961=CARTESIAN_POINT('Ctrl Pts',(29.022697875521,18.7528171397305,38.0550205593797));
#69962=CARTESIAN_POINT('Ctrl Pts',(28.9480311354006,18.7852897813823,38.0507889335081));
#69963=CARTESIAN_POINT('Ctrl Pts',(28.8749013526776,18.8215240469643,38.0465573076365));
#69964=CARTESIAN_POINT('Ctrl Pts',(28.8037089877696,18.8613466704356,38.0423256817649));
#69965=CARTESIAN_POINT('Ctrl Pts',(28.7327456263722,18.9010411970164,38.0381076677066));
#69966=CARTESIAN_POINT('Ctrl Pts',(28.6637076528252,18.9443008184763,38.0338896536484));
#69967=CARTESIAN_POINT('Ctrl Pts',(28.5969694111176,18.9909068173277,38.0296716395901));
#69968=CARTESIAN_POINT('Ctrl Pts',(28.5302531301217,19.0374974801307,38.0254550135005));
#69969=CARTESIAN_POINT('Ctrl Pts',(28.4658354589435,19.0874320676519,38.0212383874109));
#69970=CARTESIAN_POINT('Ctrl Pts',(28.4040620322853,19.1404483730731,38.0170217613214));
#69971=CARTESIAN_POINT('Ctrl Pts',(28.3422900197819,19.1934634648128,38.0128052317613));
#69972=CARTESIAN_POINT('Ctrl Pts',(28.2831624834224,19.2495598306128,38.0085887022013));
#69973=CARTESIAN_POINT('Ctrl Pts',(28.2269911022462,19.3084357244001,38.0043721726413));
#69974=CARTESIAN_POINT('Ctrl Pts',(28.1704730463874,19.3676749843957,38.000129619793));
#69975=CARTESIAN_POINT('Ctrl Pts',(28.1169480997675,19.4297278655877,37.9958870669447));
#69976=CARTESIAN_POINT('Ctrl Pts',(28.0666940201099,19.4942516019862,37.9916445140964));
#69977=CARTESIAN_POINT('Ctrl Pts',(28.0166756780481,19.5584726630478,37.9874218627011));
#69978=CARTESIAN_POINT('Ctrl Pts',(27.9698978081486,19.6251410341167,37.9831992113059));
#69979=CARTESIAN_POINT('Ctrl Pts',(27.9265908599889,19.6938894426128,37.9789765599106));
#69980=CARTESIAN_POINT('Ctrl Pts',(27.8829777518662,19.7631238703528,37.9747240563358));
#69981=CARTESIAN_POINT('Ctrl Pts',(27.8428850670919,19.8344674429904,37.9704715527609));
#69982=CARTESIAN_POINT('Ctrl Pts',(27.806500350291,19.9075213792816,37.9662190491861));
#69983=CARTESIAN_POINT('Ctrl Pts',(27.7701156334902,19.9805753155728,37.9619665456112));
#69984=CARTESIAN_POINT('Ctrl Pts',(27.7374390167793,20.0553391553627,37.9577140420364));
#69985=CARTESIAN_POINT('Ctrl Pts',(27.7086075710818,20.1313971064427,37.9534615384615));
#69986=CARTESIAN_POINT('Ctrl Pts',(27.6758375656571,20.217845059682,37.9486281157231));
#69987=CARTESIAN_POINT('Ctrl Pts',(27.6479320020787,20.3062327244513,37.9437946929847));
#69988=CARTESIAN_POINT('Ctrl Pts',(27.6250935584466,20.3960383755005,37.9389612702462));
#69989=CARTESIAN_POINT('Ctrl Pts',(27.6023501396508,20.4854703685444,37.9341479581253));
#69990=CARTESIAN_POINT('Ctrl Pts',(27.5846318881965,20.5763083907836,37.9293346460044));
#69991=CARTESIAN_POINT('Ctrl Pts',(27.5720921426097,20.6680155334625,37.9245213338835));
#69992=CARTESIAN_POINT('Ctrl Pts',(27.559640925248,20.7590752411098,37.9197420028331));
#69993=CARTESIAN_POINT('Ctrl Pts',(27.5522954629206,20.8509916422353,37.9149626717827));
#69994=CARTESIAN_POINT('Ctrl Pts',(27.5501578939433,20.943220554848,37.9101833407323));
#69995=CARTESIAN_POINT('Ctrl Pts',(27.5497321325049,20.9615907290592,37.9092313925685));
#69996=CARTESIAN_POINT('Ctrl Pts',(27.5495128261339,20.9799732476796,37.9082794444048));
#69997=CARTESIAN_POINT('Ctrl Pts',(27.5495005462907,20.99836373272,37.907327496241));
#69998=CARTESIAN_POINT('',(27.5495007214883,21.0018804290879,37.1073274961852));
#69999=CARTESIAN_POINT('Ctrl Pts',(27.5495005462904,20.9983637332799,37.907327496212));
#70000=CARTESIAN_POINT('Ctrl Pts',(27.5494458819207,21.0802299757675,37.9030898472844));
#70001=CARTESIAN_POINT('Ctrl Pts',(27.5534980267667,21.1621217478089,37.8988521983568));
#70002=CARTESIAN_POINT('Ctrl Pts',(27.5616380823687,21.2436009208633,37.8946145494291));
#70003=CARTESIAN_POINT('Ctrl Pts',(27.569778459134,21.325083308653,37.8903767333064));
#70004=CARTESIAN_POINT('Ctrl Pts',(27.5820070209178,21.4061526093791,37.8861389171837));
#70005=CARTESIAN_POINT('Ctrl Pts',(27.5982530209687,21.4863760877286,37.8819011010609));
#70006=CARTESIAN_POINT('Ctrl Pts',(27.6145044466303,21.5666263579873,37.8776618696519));
#70007=CARTESIAN_POINT('Ctrl Pts',(27.6347758841636,21.6460297961296,37.8734226382429));
#70008=CARTESIAN_POINT('Ctrl Pts',(27.6589458233662,21.7241654452301,37.869183406834));
#70009=CARTESIAN_POINT('Ctrl Pts',(27.6831472745969,21.8024029652023,37.8649386484446));
#70010=CARTESIAN_POINT('Ctrl Pts',(27.711257234633,21.8793689596193,37.8606938900552));
#70011=CARTESIAN_POINT('Ctrl Pts',(27.7431049575806,21.9546596343739,37.8564491316659));
#70012=CARTESIAN_POINT('Ctrl Pts',(27.7749767907757,22.0300073077653,37.8522011597917));
#70013=CARTESIAN_POINT('Ctrl Pts',(27.8105918197602,22.1036767254342,37.8479531879175));
#70014=CARTESIAN_POINT('Ctrl Pts',(27.8497330746425,22.175288219848,37.8437052160432));
#70015=CARTESIAN_POINT('Ctrl Pts',(27.8889430848691,22.2470255066765,37.8394497822016));
#70016=CARTESIAN_POINT('Ctrl Pts',(27.9316914436912,22.3166972664765,37.83519434836));
#70017=CARTESIAN_POINT('Ctrl Pts',(27.9777178442663,22.3839527205079,37.8309389145183));
#70018=CARTESIAN_POINT('Ctrl Pts',(27.9936105490094,22.4071757199153,37.8294695327558));
#70019=CARTESIAN_POINT('Ctrl Pts',(28.0098937420718,22.4301109208238,37.8280001509933));
#70020=CARTESIAN_POINT('Ctrl Pts',(28.026555639737,22.4527448526656,37.8265307692308));
#70021=CARTESIAN_POINT('Ctrl Pts',(28.0745399183696,22.5179278776648,37.8222991249531));
#70022=CARTESIAN_POINT('Ctrl Pts',(28.125846908268,22.5808528674656,37.8180674806755));
#70023=CARTESIAN_POINT('Ctrl Pts',(28.1802364650657,22.6411614566895,37.8138358363979));
#70024=CARTESIAN_POINT('Ctrl Pts',(28.2345481578057,22.7013837081725,37.8096102501397));
#70025=CARTESIAN_POINT('Ctrl Pts',(28.2919333441418,22.7589966559853,37.8053846638815));
#70026=CARTESIAN_POINT('Ctrl Pts',(28.3521099219312,22.8136726663327,37.8011590776233));
#70027=CARTESIAN_POINT('Ctrl Pts',(28.4123725435083,22.8684268554533,37.796927449389));
#70028=CARTESIAN_POINT('Ctrl Pts',(28.4754342534545,22.9202353343615,37.7926958211547));
#70029=CARTESIAN_POINT('Ctrl Pts',(28.5409726596603,22.9688040710394,37.7884641929204));
#70030=CARTESIAN_POINT('Ctrl Pts',(28.606300067735,23.0172164427205,37.7842461882345));
#70031=CARTESIAN_POINT('Ctrl Pts',(28.6740878845252,23.0624096096378,37.7800281835486));
#70032=CARTESIAN_POINT('Ctrl Pts',(28.7439829970004,23.1041320153868,37.7758101788627));
#70033=CARTESIAN_POINT('Ctrl Pts',(28.8138551107407,23.1458406925286,37.771593562096));
#70034=CARTESIAN_POINT('Ctrl Pts',(28.8858327443596,23.1840806384094,37.7673769453293));
#70035=CARTESIAN_POINT('Ctrl Pts',(28.9595349148795,23.2186443285586,37.7631603285627));
#70036=CARTESIAN_POINT('Ctrl Pts',(29.0332353992417,23.2532072279599,37.7589438082637));
#70037=CARTESIAN_POINT('Ctrl Pts',(29.108659920751,23.284093842521,37.7547272879648));
#70038=CARTESIAN_POINT('Ctrl Pts',(29.1854053821451,23.3111438420319,37.7505107676658));
#70039=CARTESIAN_POINT('Ctrl Pts',(29.2626248679896,23.3383609180176,37.7462682036937));
#70040=CARTESIAN_POINT('Ctrl Pts',(29.3411812239746,23.3616936490656,37.7420256397215));
#70041=CARTESIAN_POINT('Ctrl Pts',(29.4206478681953,23.3810294742765,37.7377830757494));
#70042=CARTESIAN_POINT('Ctrl Pts',(29.4997413649096,23.4002745052299,37.7335604333705));
#70043=CARTESIAN_POINT('Ctrl Pts',(29.5797361492946,23.4155600496186,37.7293377909916));
#70044=CARTESIAN_POINT('Ctrl Pts',(29.6602027203592,23.4268267467515,37.7251151486128));
#70045=CARTESIAN_POINT('Ctrl Pts',(29.7412387295238,23.4381731749644,37.720862623844));
#70046=CARTESIAN_POINT('Ctrl Pts',(29.822752752235,23.4454436107238,37.7166100990752));
#70047=CARTESIAN_POINT('Ctrl Pts',(29.9043041605924,23.4486307513221,37.7123575743064));
#70048=CARTESIAN_POINT('Ctrl Pts',(29.9858555689497,23.4518178919203,37.7081050495376));
#70049=CARTESIAN_POINT('Ctrl Pts',(30.0674438891054,23.4509218057965,37.7038525247687));
#70050=CARTESIAN_POINT('Ctrl Pts',(30.1486337027279,23.4459881995654,37.6995999999999));
#70051=CARTESIAN_POINT('Ctrl Pts',(30.2294251782622,23.4410787988743,37.6953683392104));
#70052=CARTESIAN_POINT('Ctrl Pts',(30.31012424687,23.4321530785102,37.6911366784209));
#70053=CARTESIAN_POINT('Ctrl Pts',(30.3902995772568,23.4192181567592,37.6869050176313));
#70054=CARTESIAN_POINT('Ctrl Pts',(30.4703601280599,23.4063017527358,37.682679414918));
#70055=CARTESIAN_POINT('Ctrl Pts',(30.549897974771,23.3893876201113,37.6784538122047));
#70056=CARTESIAN_POINT('Ctrl Pts',(30.6284848157943,23.3685347973623,37.6742282094914));
#70057=CARTESIAN_POINT('Ctrl Pts',(30.7071836415084,23.3476522597541,37.669996585378));
#70058=CARTESIAN_POINT('Ctrl Pts',(30.7849282821077,23.3228198438784,37.6657649612645));
#70059=CARTESIAN_POINT('Ctrl Pts',(30.8612967875742,23.2941486642575,37.6615333371511));
#70060=CARTESIAN_POINT('Ctrl Pts',(30.9374197943529,23.2655696526963,37.6573153162654));
#70061=CARTESIAN_POINT('Ctrl Pts',(31.0121750576729,23.2331766685513,37.6530972953796));
#70062=CARTESIAN_POINT('Ctrl Pts',(31.0851596140347,23.19712968713,37.6488792744939));
#70063=CARTESIAN_POINT('Ctrl Pts',(31.158120152912,23.1610945679144,37.6446626416586));
#70064=CARTESIAN_POINT('Ctrl Pts',(31.2293107255803,23.1214080450065,37.6404460088234));
#70065=CARTESIAN_POINT('Ctrl Pts',(31.2983502159259,23.0782774037181,37.6362293759882));
#70066=CARTESIAN_POINT('Ctrl Pts',(31.3673881242992,23.035147750726,37.632012839773));
#70067=CARTESIAN_POINT('Ctrl Pts',(31.4342746547473,22.988574383489,37.6277963035577));
#70068=CARTESIAN_POINT('Ctrl Pts',(31.4986563189566,22.9388087805793,37.6235797673425));
#70069=CARTESIAN_POINT('Ctrl Pts',(31.5634351030713,22.8887362127633,37.6193372226281));
#70070=CARTESIAN_POINT('Ctrl Pts',(31.6256776279625,22.8354321721218,37.6150946779136));
#70071=CARTESIAN_POINT('Ctrl Pts',(31.6850577799362,22.7791937860381,37.6108521331992));
#70072=CARTESIAN_POINT('Ctrl Pts',(31.7441595871266,22.723219017693,37.606629475436));
#70073=CARTESIAN_POINT('Ctrl Pts',(31.8004255129353,22.6643377295476,37.6024068176729));
#70074=CARTESIAN_POINT('Ctrl Pts',(31.8535725280332,22.6028783900598,37.5981841599097));
#70075=CARTESIAN_POINT('Ctrl Pts',(31.9070949934372,22.5409848789109,37.5939316717196));
#70076=CARTESIAN_POINT('Ctrl Pts',(31.9574540155029,22.4764771268603,37.5896791835296));
#70077=CARTESIAN_POINT('Ctrl Pts',(32.0044042507991,22.4097211956193,37.5854266953395));
#70078=CARTESIAN_POINT('Ctrl Pts',(32.0513544860953,22.3429652643783,37.5811742071494));
#70079=CARTESIAN_POINT('Ctrl Pts',(32.0948957348547,22.2739615890068,37.5769217189593));
#70080=CARTESIAN_POINT('Ctrl Pts',(32.1348299965297,22.2031006341603,37.5726692307693));
#70081=CARTESIAN_POINT('Ctrl Pts',(32.1745687764439,22.1325865499868,37.5684375588869));
#70082=CARTESIAN_POINT('Ctrl Pts',(32.2108844632371,22.0599696106442,37.5642058870045));
#70083=CARTESIAN_POINT('Ctrl Pts',(32.2435488667623,21.9856159152781,37.5599742151221));
#70084=CARTESIAN_POINT('Ctrl Pts',(32.2761665094876,21.9113686611111,37.5557486010991));
#70085=CARTESIAN_POINT('Ctrl Pts',(32.3051430648768,21.835390010831,37.5515229870761));
#70086=CARTESIAN_POINT('Ctrl Pts',(32.3302955902779,21.7580717063256,37.5472973730531));
#70087=CARTESIAN_POINT('Ctrl Pts',(32.3554838734449,21.6806434832421,37.54306575174));
#70088=CARTESIAN_POINT('Ctrl Pts',(32.3768370303003,21.6018722109653,37.5388341304269));
#70089=CARTESIAN_POINT('Ctrl Pts',(32.3942193012643,21.5221725648228,37.5346025091138));
#70090=CARTESIAN_POINT('Ctrl Pts',(32.4115457538807,21.4427288520135,37.5303844764802));
#70091=CARTESIAN_POINT('Ctrl Pts',(32.4249266687656,21.362363170678,37.5261664438465));
#70092=CARTESIAN_POINT('Ctrl Pts',(32.4342776258916,21.2815007816753,37.5219484112129));
#70093=CARTESIAN_POINT('Ctrl Pts',(32.443625506153,21.2006649998545,37.5177317664923));
#70094=CARTESIAN_POINT('Ctrl Pts',(32.4489460086426,21.1193332963,37.5135151217717));
#70095=CARTESIAN_POINT('Ctrl Pts',(32.4502063051429,21.0379382687796,37.5092984770511));
#70096=CARTESIAN_POINT('Ctrl Pts',(32.4514665728008,20.9565451040173,37.5050819288301));
#70097=CARTESIAN_POINT('Ctrl Pts',(32.4486668131505,20.8750890829333,37.5008653806091));
#70098=CARTESIAN_POINT('Ctrl Pts',(32.4418263104952,20.7940035937858,37.4966488323881));
#70099=CARTESIAN_POINT('Ctrl Pts',(32.4349436561549,20.7124184498347,37.492406301484));
#70100=CARTESIAN_POINT('Ctrl Pts',(32.4239703140359,20.6312088953234,37.4881637705799));
#70101=CARTESIAN_POINT('Ctrl Pts',(32.4089787643902,20.5508101039462,37.4839212396757));
#70102=CARTESIAN_POINT('Ctrl Pts',(32.3940573961245,20.4707876911455,37.4796985697386));
#70103=CARTESIAN_POINT('Ctrl Pts',(32.375155521284,20.3915689103076,37.4754758998014));
#70104=CARTESIAN_POINT('Ctrl Pts',(32.3523953318783,20.3135697759006,37.4712532298643));
#70105=CARTESIAN_POINT('Ctrl Pts',(32.3294745665654,20.2350203481043,37.4670007684767));
#70106=CARTESIAN_POINT('Ctrl Pts',(32.3026409897418,20.1577082952858,37.462748307089));
#70107=CARTESIAN_POINT('Ctrl Pts',(32.2720688187676,20.082038381639,37.4584958457014));
#70108=CARTESIAN_POINT('Ctrl Pts',(32.2414966477935,20.0063684679922,37.4542433843137));
#70109=CARTESIAN_POINT('Ctrl Pts',(32.2071861395641,19.9323410974537,37.4499909229261));
#70110=CARTESIAN_POINT('Ctrl Pts',(32.1693577057091,19.8603345250994,37.4457384615384));
#70111=CARTESIAN_POINT('Ctrl Pts',(32.1317150165931,19.7886815185849,37.4415068805376));
#70112=CARTESIAN_POINT('Ctrl Pts',(32.0904480968269,19.7187614710945,37.4372752995367));
#70113=CARTESIAN_POINT('Ctrl Pts',(32.0457404954556,19.6509647613005,37.4330437185359));
#70114=CARTESIAN_POINT('Ctrl Pts',(32.0010968993028,19.5832651120306,37.4288181956383));
#70115=CARTESIAN_POINT('Ctrl Pts',(31.9530226584073,19.5176831478165,37.4245926727407));
#70116=CARTESIAN_POINT('Ctrl Pts',(31.9017474219834,19.4545851712308,37.4203671498431));
#70117=CARTESIAN_POINT('Ctrl Pts',(31.850397907355,19.3913957898125,37.4161355057791));
#70118=CARTESIAN_POINT('Ctrl Pts',(31.795838349081,19.3306980056242,37.4119038617151));
#70119=CARTESIAN_POINT('Ctrl Pts',(31.7383432947695,19.2728309754022,37.4076722176512));
#70120=CARTESIAN_POINT('Ctrl Pts',(31.6810344151152,19.2151513243322,37.4034542760681));
#70121=CARTESIAN_POINT('Ctrl Pts',(31.6208093379655,19.1602844654005,37.399236334485));
#70122=CARTESIAN_POINT('Ctrl Pts',(31.5579793517154,19.1085321600333,37.395018392902));
#70123=CARTESIAN_POINT('Ctrl Pts',(31.4951700362354,19.0567968809312,37.3908018390018));
#70124=CARTESIAN_POINT('Ctrl Pts',(31.4297578720651,19.0081744158085,37.3865852851017));
#70125=CARTESIAN_POINT('Ctrl Pts',(31.3620883185178,18.9629271828044,37.3823687312016));
#70126=CARTESIAN_POINT('Ctrl Pts',(31.2944203079969,18.9176809815445,37.3781522734489));
#70127=CARTESIAN_POINT('Ctrl Pts',(31.2244953974724,18.875810116809,37.3739358156962));
#70128=CARTESIAN_POINT('Ctrl Pts',(31.1526880019738,18.837533671914,37.3697193579435));
#70129=CARTESIAN_POINT('Ctrl Pts',(31.0804347362346,18.7990195589129,37.3654767191405));
#70130=CARTESIAN_POINT('Ctrl Pts',(31.0062759397416,18.7641448948097,37.3612340803376));
#70131=CARTESIAN_POINT('Ctrl Pts',(30.9306164637358,18.7330850815648,37.3569914415346));
#70132=CARTESIAN_POINT('Ctrl Pts',(30.8553146764312,18.7021721070882,37.3527688602848));
#70133=CARTESIAN_POINT('Ctrl Pts',(30.778526827634,18.6750380975155,37.348546279035));
#70134=CARTESIAN_POINT('Ctrl Pts',(30.7006686104187,18.6518062796324,37.3443236977852));
#70135=CARTESIAN_POINT('Ctrl Pts',(30.6222556453229,18.628408932635,37.3400710302056));
#70136=CARTESIAN_POINT('Ctrl Pts',(30.5427574637281,18.608969716988,37.335818362626));
#70137=CARTESIAN_POINT('Ctrl Pts',(30.4626086443515,18.5935620739002,37.3315656950465));
#70138=CARTESIAN_POINT('Ctrl Pts',(30.3824598249749,18.5781544308125,37.3273130274669));
#70139=CARTESIAN_POINT('Ctrl Pts',(30.3016608466984,18.5667783638181,37.3230603598873));
#70140=CARTESIAN_POINT('Ctrl Pts',(30.2206491032623,18.5594541136808,37.3188076923077));
#70141=CARTESIAN_POINT('Ctrl Pts',(30.140036127004,18.5521659159778,37.3145759577951));
#70142=CARTESIAN_POINT('Ctrl Pts',(30.0589109219233,18.5488624374712,37.3103442232825));
#70143=CARTESIAN_POINT('Ctrl Pts',(29.9777010025348,18.5496014600249,37.3061124887699));
#70144=CARTESIAN_POINT('Ctrl Pts',(29.896607348942,18.5503394245423,37.3018868127041));
#70145=CARTESIAN_POINT('Ctrl Pts',(29.8154296827866,18.5551083913551,37.2976611366383));
#70146=CARTESIAN_POINT('Ctrl Pts',(29.7346003255107,18.5639143564355,37.2934354605725));
#70147=CARTESIAN_POINT('Ctrl Pts',(29.6536575447593,18.5727326784516,37.2892038548436));
#70148=CARTESIAN_POINT('Ctrl Pts',(29.5730645196653,18.58559936205,37.2849722491146));
#70149=CARTESIAN_POINT('Ctrl Pts',(29.4932550900962,18.6024679676203,37.2807406433856));
#70150=CARTESIAN_POINT('Ctrl Pts',(29.413700518321,18.6192827061774,37.2765225505674));
#70151=CARTESIAN_POINT('Ctrl Pts',(29.3349250047692,18.6400737666865,37.2723044577492));
#70152=CARTESIAN_POINT('Ctrl Pts',(29.2573509894203,18.6647435478978,37.268086364931));
#70153=CARTESIAN_POINT('Ctrl Pts',(29.1798025140915,18.689405206973,37.2638696608532));
#70154=CARTESIAN_POINT('Ctrl Pts',(29.103455193983,18.7179429100095,37.2596529567755));
#70155=CARTESIAN_POINT('Ctrl Pts',(29.0287169800055,18.7502089996912,37.2554362526978));
#70156=CARTESIAN_POINT('Ctrl Pts',(28.953980492419,18.7824743440529,37.2512196460224));
#70157=CARTESIAN_POINT('Ctrl Pts',(28.8808534633331,18.8184677185667,37.2470030393471));
#70158=CARTESIAN_POINT('Ctrl Pts',(28.8097231716269,18.8579936223629,37.2427864326717));
#70159=CARTESIAN_POINT('Ctrl Pts',(28.7381567726455,18.8977618636188,37.2385439735388));
#70160=CARTESIAN_POINT('Ctrl Pts',(28.6686121021959,18.94110588085,37.2343015144059));
#70161=CARTESIAN_POINT('Ctrl Pts',(28.6014561967581,18.9877809561547,37.230059055273));
#70162=CARTESIAN_POINT('Ctrl Pts',(28.5346126627082,19.0342389253396,37.2258363296667));
#70163=CARTESIAN_POINT('Ctrl Pts',(28.4701360575167,19.0839967024078,37.2216136040605));
#70164=CARTESIAN_POINT('Ctrl Pts',(28.4083555741484,19.1367720827404,37.2173908784542));
#70165=CARTESIAN_POINT('Ctrl Pts',(28.3461420244647,19.189917405784,37.213138552558));
#70166=CARTESIAN_POINT('Ctrl Pts',(28.2866628888177,19.2461224725628,37.2088862266617));
#70167=CARTESIAN_POINT('Ctrl Pts',(28.2302157062022,19.3050623010191,37.2046339007655));
#70168=CARTESIAN_POINT('Ctrl Pts',(28.1737685235867,19.3640021294754,37.2003815748693));
#70169=CARTESIAN_POINT('Ctrl Pts',(28.1203535568256,19.4256763196491,37.1961292489731));
#70170=CARTESIAN_POINT('Ctrl Pts',(28.0702252177862,19.4897286535422,37.1918769230769));
#70171=CARTESIAN_POINT('Ctrl Pts',(28.0203683885972,19.5534340611271,37.1876476290304));
#70172=CARTESIAN_POINT('Ctrl Pts',(27.9735727040171,19.6197345946428,37.1834183349838));
#70173=CARTESIAN_POINT('Ctrl Pts',(27.930119809746,19.6883040565764,37.1791890409373));
#70174=CARTESIAN_POINT('Ctrl Pts',(27.8867277353166,19.7567775436872,37.1749656665193));
#70175=CARTESIAN_POINT('Ctrl Pts',(27.8466694096143,19.8275132663813,37.1707422921013));
#70176=CARTESIAN_POINT('Ctrl Pts',(27.8101858643266,19.9001526009463,37.1665189176833));
#70177=CARTESIAN_POINT('Ctrl Pts',(27.7737422108834,19.9727125101977,37.1623001611881));
#70178=CARTESIAN_POINT('Ctrl Pts',(27.7408657831866,20.0471714851209,37.1580814046929));
#70179=CARTESIAN_POINT('Ctrl Pts',(27.7117531859141,20.1231438157681,37.1538626481977));
#70180=CARTESIAN_POINT('Ctrl Pts',(27.6826622239771,20.1990596867719,37.1496470269162));
#70181=CARTESIAN_POINT('Ctrl Pts',(27.6573297031452,20.2764862472493,37.1454314056346));
#70182=CARTESIAN_POINT('Ctrl Pts',(27.6359047284464,20.3550164366296,37.1412157843531));
#70183=CARTESIAN_POINT('Ctrl Pts',(27.6144894075789,20.4335112412679,37.1370020625789));
#70184=CARTESIAN_POINT('Ctrl Pts',(27.5969782550267,20.5131082384583,37.1327883408046));
#70185=CARTESIAN_POINT('Ctrl Pts',(27.5834705400339,20.5933851710573,37.1285746190304));
#70186=CARTESIAN_POINT('Ctrl Pts',(27.5699608051698,20.6736741078388,37.1243602671588));
#70187=CARTESIAN_POINT('Ctrl Pts',(27.5604557878433,20.7546427257951,37.1201459152872));
#70188=CARTESIAN_POINT('Ctrl Pts',(27.5550034413766,20.8358595774352,37.1159315634156));
#70189=CARTESIAN_POINT('Ctrl Pts',(27.5512929178413,20.8911306504147,37.1130635410144));
#70190=CARTESIAN_POINT('Ctrl Pts',(27.5494582371227,20.9465165035797,37.1101955186133));
#70191=CARTESIAN_POINT('Ctrl Pts',(27.5495007214879,21.0018804285691,37.1073274962121));
#70192=CARTESIAN_POINT('Ctrl Pts',(27.5495007214883,21.0018804290879,37.1073274961852));
#70193=CARTESIAN_POINT('Ctrl Pts',(27.5495734263339,21.0966264490123,37.102419359567));
#70194=CARTESIAN_POINT('Ctrl Pts',(27.5551449651667,21.1911451718291,37.0975112229488));
#70195=CARTESIAN_POINT('Ctrl Pts',(27.5661129364305,21.2848578799844,37.0926030863306));
#70196=CARTESIAN_POINT('Ctrl Pts',(27.5771936827079,21.3795341621384,37.0876444832076));
#70197=CARTESIAN_POINT('Ctrl Pts',(27.5937823092464,21.4733876385682,37.0826858800847));
#70198=CARTESIAN_POINT('Ctrl Pts',(27.615723715063,21.5658417155771,37.0777272769618));
#70199=CARTESIAN_POINT('Ctrl Pts',(27.6345755168118,21.6452771877251,37.0734669025899));
#70200=CARTESIAN_POINT('Ctrl Pts',(27.6573779156586,21.7236799129869,37.069206528218));
#70201=CARTESIAN_POINT('Ctrl Pts',(27.6840045937171,21.8006969015031,37.0649461538461));
#70202=CARTESIAN_POINT('Ctrl Pts',(27.7104481669317,21.8771842639191,37.0607150769774));
#70203=CARTESIAN_POINT('Ctrl Pts',(27.7407344179044,21.9525035155541,37.0564840001087));
#70204=CARTESIAN_POINT('Ctrl Pts',(27.7747406301215,22.0262411932719,37.0522529232399));
#70205=CARTESIAN_POINT('Ctrl Pts',(27.8086981438002,22.0998732750736,37.0480279054776));
#70206=CARTESIAN_POINT('Ctrl Pts',(27.8463648454955,22.171927862545,37.0438028877154));
#70207=CARTESIAN_POINT('Ctrl Pts',(27.8875688214277,22.242008359793,37.0395778699531));
#70208=CARTESIAN_POINT('Ctrl Pts',(27.9288386499126,22.312200860301,37.0353460997307));
#70209=CARTESIAN_POINT('Ctrl Pts',(27.973656900648,22.3804125166,37.0311143295082));
#70210=CARTESIAN_POINT('Ctrl Pts',(28.0218030873939,22.4462666507099,37.0268825592858));
#70211=CARTESIAN_POINT('Ctrl Pts',(28.0697862084264,22.5118977442826,37.0226651215927));
#70212=CARTESIAN_POINT('Ctrl Pts',(28.1210744961541,22.5751868734316,37.0184476838995));
#70213=CARTESIAN_POINT('Ctrl Pts',(28.175405613739,22.6357889764957,37.0142302462064));
#70214=CARTESIAN_POINT('Ctrl Pts',(28.2297188748722,22.6963711620875,37.0100141946153));
#70215=CARTESIAN_POINT('Ctrl Pts',(28.2870726697613,22.754267729426,37.0057981430241));
#70216=CARTESIAN_POINT('Ctrl Pts',(28.347164964824,22.8091673765837,37.001582091433));
#70217=CARTESIAN_POINT('Ctrl Pts',(28.407255921585,22.864065801084,36.9973661337366));
#70218=CARTESIAN_POINT('Ctrl Pts',(28.4700849132321,22.9159671253415,36.9931501760402));
#70219=CARTESIAN_POINT('Ctrl Pts',(28.5353147666167,22.9645985384065,36.9889342183438));
#70220=CARTESIAN_POINT('Ctrl Pts',(28.6009666757401,23.0135446105717,36.9846909821998));
#70221=CARTESIAN_POINT('Ctrl Pts',(28.66905025467,23.0591780068706,36.9804477460557));
#70222=CARTESIAN_POINT('Ctrl Pts',(28.7391913838261,23.1012643535219,36.9762045099117));
#70223=CARTESIAN_POINT('Ctrl Pts',(28.8089829943779,23.143140980693,36.9719824181375));
#70224=CARTESIAN_POINT('Ctrl Pts',(28.8808112568981,23.1815056551039,36.9677603263633));
#70225=CARTESIAN_POINT('Ctrl Pts',(28.9542837808468,23.2161741445563,36.9635382345891));
#70226=CARTESIAN_POINT('Ctrl Pts',(29.0283082338989,23.2511030653547,36.9592844262601));
#70227=CARTESIAN_POINT('Ctrl Pts',(29.1040013112907,23.2822798553515,36.9550306179312));
#70228=CARTESIAN_POINT('Ctrl Pts',(29.1809439930593,23.3095665193916,36.9507768096022));
#70229=CARTESIAN_POINT('Ctrl Pts',(29.257886674828,23.3368531834316,36.9465230012733));
#70230=CARTESIAN_POINT('Ctrl Pts',(29.3360784870119,23.3602496460209,36.9422691929443));
#70231=CARTESIAN_POINT('Ctrl Pts',(29.4150896273457,23.3796701674731,36.9380153846154));
#70232=CARTESIAN_POINT('Ctrl Pts',(29.4937041069858,23.3989931918194,36.9337829317378));
#70233=CARTESIAN_POINT('Ctrl Pts',(29.5734239395721,23.4144524666238,36.9295504788602));
#70234=CARTESIAN_POINT('Ctrl Pts',(29.6538350226455,23.4259266391326,36.9253180259826));
#70235=CARTESIAN_POINT('Ctrl Pts',(29.7341309568104,23.4373843805925,36.92109163399));
#70236=CARTESIAN_POINT('Ctrl Pts',(29.8151157193599,23.4448682887738,36.9168652419974));
#70237=CARTESIAN_POINT('Ctrl Pts',(29.8963626798454,23.4483074880152,36.9126388500048));
#70238=CARTESIAN_POINT('Ctrl Pts',(29.9777064211677,23.4517507840077,36.9084074235623));
#70239=CARTESIAN_POINT('Ctrl Pts',(30.059312526285,23.4511396355139,36.9041759971198));
#70240=CARTESIAN_POINT('Ctrl Pts',(30.1407452638531,23.4464547861555,36.8999445706773));
#70241=CARTESIAN_POINT('Ctrl Pts',(30.221934964488,23.4417839187833,36.8957257729752));
#70242=CARTESIAN_POINT('Ctrl Pts',(30.3029518648406,23.43306364041,36.8915069752731));
#70243=CARTESIAN_POINT('Ctrl Pts',(30.383363542695,23.4203269705005,36.8872881775711));
#70244=CARTESIAN_POINT('Ctrl Pts',(30.4637486421758,23.407594510427,36.8830707743031));
#70245=CARTESIAN_POINT('Ctrl Pts',(30.5435284578888,23.3908483678063,36.878853371035));
#70246=CARTESIAN_POINT('Ctrl Pts',(30.6222773685781,23.3701732271198,36.874635967767));
#70247=CARTESIAN_POINT('Ctrl Pts',(30.7010243370977,23.3494985963404,36.870418668512));
#70248=CARTESIAN_POINT('Ctrl Pts',(30.778740002042,23.3248952792246,36.8662013692571));
#70249=CARTESIAN_POINT('Ctrl Pts',(30.8550119861844,23.2964983678376,36.8619840700021));
#70250=CARTESIAN_POINT('Ctrl Pts',(30.9317238452976,23.2679376860872,36.8577424487839));
#70251=CARTESIAN_POINT('Ctrl Pts',(31.0069748683008,23.2355396652763,36.8535008275658));
#70252=CARTESIAN_POINT('Ctrl Pts',(31.0803657137938,23.1994908898331,36.8492592063477));
#70253=CARTESIAN_POINT('Ctrl Pts',(31.1534412005239,23.1635970151429,36.8450358112777));
#70254=CARTESIAN_POINT('Ctrl Pts',(31.2246720794835,23.1240839695699,36.8408124162077));
#70255=CARTESIAN_POINT('Ctrl Pts',(31.2936903488492,23.08118128266,36.8365890211377));
#70256=CARTESIAN_POINT('Ctrl Pts',(31.3631553928521,23.0380008746111,36.8323382868455));
#70257=CARTESIAN_POINT('Ctrl Pts',(31.4303786881534,22.9913870572403,36.8280875525533));
#70258=CARTESIAN_POINT('Ctrl Pts',(31.4950176219411,22.9416159661698,36.8238368182612));
#70259=CARTESIAN_POINT('Ctrl Pts',(31.5596565557289,22.8918448750993,36.819586083969));
#70260=CARTESIAN_POINT('Ctrl Pts',(31.6217108088404,22.8389168650207,36.8153353496768));
#70261=CARTESIAN_POINT('Ctrl Pts',(31.6808756159897,22.7831453708465,36.8110846153846));
#70262=CARTESIAN_POINT('Ctrl Pts',(31.7397829612703,22.7276165721833,36.8068523786089));
#70263=CARTESIAN_POINT('Ctrl Pts',(31.7960455326341,22.6690620488109,36.8026201418332));
#70264=CARTESIAN_POINT('Ctrl Pts',(31.8493366530194,22.6077637244941,36.7983879050575));
#70265=CARTESIAN_POINT('Ctrl Pts',(31.9025516273736,22.5465529874539,36.7941617155938));
#70266=CARTESIAN_POINT('Ctrl Pts',(31.9528032811068,22.4826065838145,36.7899355261301));
#70267=CARTESIAN_POINT('Ctrl Pts',(31.9998005337598,22.4162443557431,36.7857093366664));
#70268=CARTESIAN_POINT('Ctrl Pts',(32.0468566060492,22.3497990717075,36.781477857895));
#70269=CARTESIAN_POINT('Ctrl Pts',(32.0906497976773,22.2809322469608,36.7772463791236));
#70270=CARTESIAN_POINT('Ctrl Pts',(32.1309274021744,22.2099994449016,36.7730149003523));
#70271=CARTESIAN_POINT('Ctrl Pts',(32.1710826970664,22.1392820420232,36.7687962711658));
#70272=CARTESIAN_POINT('Ctrl Pts',(32.2077434797372,22.0665115874194,36.7645776419794));
#70273=CARTESIAN_POINT('Ctrl Pts',(32.2407027904726,21.9920691784188,36.7603590127929));
#70274=CARTESIAN_POINT('Ctrl Pts',(32.2736513089402,21.9176511450009,36.7561417649634));
#70275=CARTESIAN_POINT('Ctrl Pts',(32.3029005744618,21.8415626689452,36.751924517134));
#70276=CARTESIAN_POINT('Ctrl Pts',(32.3282907129676,21.7642071747301,36.7477072693046));
#70277=CARTESIAN_POINT('Ctrl Pts',(32.3536803047399,21.6868533462341,36.7434901122864));
#70278=CARTESIAN_POINT('Ctrl Pts',(32.3752107909009,21.6082329956549,36.7392729552682));
#70279=CARTESIAN_POINT('Ctrl Pts',(32.3927718235932,21.5287657801129,36.73505579825));
#70280=CARTESIAN_POINT('Ctrl Pts',(32.4104355964662,21.4488336445275,36.7308139689087));
#70281=CARTESIAN_POINT('Ctrl Pts',(32.4240832019679,21.3680451633441,36.7265721395673));
#70282=CARTESIAN_POINT('Ctrl Pts',(32.4336546040302,21.2868370936308,36.722330310226));
#70283=CARTESIAN_POINT('Ctrl Pts',(32.4431841648433,21.20598402385,36.7181070239818));
#70284=CARTESIAN_POINT('Ctrl Pts',(32.4486731082285,21.1247154972942,36.7138837377377));
#70285=CARTESIAN_POINT('Ctrl Pts',(32.4501144933605,21.0434651518448,36.7096604514935));
#70286=CARTESIAN_POINT('Ctrl Pts',(32.4515653714831,20.9616796900313,36.7054093506036));
#70287=CARTESIAN_POINT('Ctrl Pts',(32.4489151997653,20.8799131266057,36.7011582497136));
#70288=CARTESIAN_POINT('Ctrl Pts',(32.4422099791544,20.7986032082709,36.6969071488237));
#70289=CARTESIAN_POINT('Ctrl Pts',(32.4355047585435,20.7172932899361,36.6926560479337));
#70290=CARTESIAN_POINT('Ctrl Pts',(32.4247446139307,20.6364404775047,36.6884049470438));
#70291=CARTESIAN_POINT('Ctrl Pts',(32.4100274355389,20.5564709592938,36.6841538461538));
#70292=CARTESIAN_POINT('Ctrl Pts',(32.395393134607,20.4769517767627,36.6799266846655));
#70293=CARTESIAN_POINT('Ctrl Pts',(32.3767912539051,20.3980070206159,36.6756995231771));
#70294=CARTESIAN_POINT('Ctrl Pts',(32.3542804263525,20.3200632940535,36.6714723616887));
#70295=CARTESIAN_POINT('Ctrl Pts',(32.3318019203877,20.2422314809689,36.6672512696605));
#70296=CARTESIAN_POINT('Ctrl Pts',(32.3054257420964,20.1653982868145,36.6630301776323));
#70297=CARTESIAN_POINT('Ctrl Pts',(32.2752617080485,20.0899810936645,36.658809085604));
#70298=CARTESIAN_POINT('Ctrl Pts',(32.2450143632446,20.0143556039924,36.6545763352423));
#70299=CARTESIAN_POINT('Ctrl Pts',(32.2109583004433,19.9401544127064,36.6503435848806));
#70300=CARTESIAN_POINT('Ctrl Pts',(32.1732549515911,19.8677839581666,36.6461108345189));
#70301=CARTESIAN_POINT('Ctrl Pts',(32.1357229412312,19.7957423827569,36.6418973193999));
#70302=CARTESIAN_POINT('Ctrl Pts',(32.0945769325993,19.7255153603938,36.6376838042809));
#70303=CARTESIAN_POINT('Ctrl Pts',(32.0500239675645,19.6574829675527,36.6334702891619));
#70304=CARTESIAN_POINT('Ctrl Pts',(32.0054855560905,19.5894727980039,36.6292581504192));
#70305=CARTESIAN_POINT('Ctrl Pts',(31.9575426532041,19.5236562238784,36.6250460116766));
#70306=CARTESIAN_POINT('Ctrl Pts',(31.9064466291453,19.4603859249083,36.6208338729339));
#70307=CARTESIAN_POINT('Ctrl Pts',(31.8553515634987,19.3971168127042,36.6166218131987));
#70308=CARTESIAN_POINT('Ctrl Pts',(31.8011037878849,19.3363942424423,36.6124097534635));
#70309=CARTESIAN_POINT('Ctrl Pts',(31.7439952000058,19.2785381234669,36.6081976937283));
#70310=CARTESIAN_POINT('Ctrl Pts',(31.6864008841917,19.2201899185507,36.6039498089945));
#70311=CARTESIAN_POINT('Ctrl Pts',(31.6258971853853,19.1647575126242,36.5997019242607));
#70312=CARTESIAN_POINT('Ctrl Pts',(31.5628203493671,19.1125300517348,36.5954540395269));
#70313=CARTESIAN_POINT('Ctrl Pts',(31.5001832688747,19.06066670731,36.5912357699563));
#70314=CARTESIAN_POINT('Ctrl Pts',(31.4350092306898,19.0119639924745,36.5870175003856));
#70315=CARTESIAN_POINT('Ctrl Pts',(31.3676580729662,18.9666624369155,36.5827992308149));
#70316=CARTESIAN_POINT('Ctrl Pts',(31.2995976378414,18.9208838090881,36.5785365384996));
#70317=CARTESIAN_POINT('Ctrl Pts',(31.2293143776745,18.878578647648,36.5742738461843));
#70318=CARTESIAN_POINT('Ctrl Pts',(31.1572049201268,18.8399474490573,36.570011153869));
#70319=CARTESIAN_POINT('Ctrl Pts',(31.0850954625791,18.8013162504665,36.5657484615537));
#70320=CARTESIAN_POINT('Ctrl Pts',(31.0111602729967,18.766359162102,36.5614857692384));
#70321=CARTESIAN_POINT('Ctrl Pts',(30.9358146226311,18.7352260064038,36.5572230769231));
#70322=CARTESIAN_POINT('Ctrl Pts',(30.8608852465432,18.7042648570767,36.5529839353921));
#70323=CARTESIAN_POINT('Ctrl Pts',(30.7842798019212,18.6769692289837,36.5487447938612));
#70324=CARTESIAN_POINT('Ctrl Pts',(30.7063906892555,18.6535212670614,36.5445056523303));
#70325=CARTESIAN_POINT('Ctrl Pts',(30.6286132109143,18.6301069118564,36.5402725865355));
#70326=CARTESIAN_POINT('Ctrl Pts',(30.5495561586416,18.6105294015379,36.5360395207408));
#70327=CARTESIAN_POINT('Ctrl Pts',(30.4696318358586,18.5949228310202,36.5318064549461));
#70328=CARTESIAN_POINT('Ctrl Pts',(30.3897700025997,18.5793284626348,36.5275766988105));
#70329=CARTESIAN_POINT('Ctrl Pts',(30.3090426948968,18.5676989705192,36.5233469426749));
#70330=CARTESIAN_POINT('Ctrl Pts',(30.2278763899687,18.5601183223577,36.5191171865393));
#70331=CARTESIAN_POINT('Ctrl Pts',(30.1467939365032,18.5525455056285,36.5148918000894));
#70332=CARTESIAN_POINT('Ctrl Pts',(30.0652738489759,18.5490132479074,36.5106664136395));
#70333=CARTESIAN_POINT('Ctrl Pts',(29.9837496684643,18.5495538821013,36.5064410271896));
#70334=CARTESIAN_POINT('Ctrl Pts',(29.9022532963383,18.5500943318815,36.5022170820443));
#70335=CARTESIAN_POINT('Ctrl Pts',(29.8207532966366,18.5547049112194,36.497993136899));
#70336=CARTESIAN_POINT('Ctrl Pts',(29.7396842522887,18.5633658539917,36.4937691917536));
#70337=CARTESIAN_POINT('Ctrl Pts',(29.658618274113,18.5720264691921,36.4895454063653));
#70338=CARTESIAN_POINT('Ctrl Pts',(29.5779836791669,18.5847370930045,36.4853216209769));
#70339=CARTESIAN_POINT('Ctrl Pts',(29.4982095547469,18.6014261322501,36.4810978355885));
#70340=CARTESIAN_POINT('Ctrl Pts',(29.4182463990515,18.6181547175314,36.4768640415972));
#70341=CARTESIAN_POINT('Ctrl Pts',(29.3391482536535,18.6388805002022,36.4726302476058));
#70342=CARTESIAN_POINT('Ctrl Pts',(29.2613348834451,18.6634803455599,36.4683964536145));
#70343=CARTESIAN_POINT('Ctrl Pts',(29.1835971414072,18.6880562818992,36.4641667745213));
#70344=CARTESIAN_POINT('Ctrl Pts',(29.107142105256,18.7164985677058,36.4599370954281));
#70345=CARTESIAN_POINT('Ctrl Pts',(29.0323693455972,18.7486357099172,36.4557074163349));
#70346=CARTESIAN_POINT('Ctrl Pts',(28.9574636806604,18.7808299744796,36.4514702191739));
#70347=CARTESIAN_POINT('Ctrl Pts',(28.8842466854363,18.8167320167715,36.447233022013));
#70348=CARTESIAN_POINT('Ctrl Pts',(28.8130947299534,18.8561235740053,36.442995824852));
#70349=CARTESIAN_POINT('Ctrl Pts',(28.7419879697471,18.8954901099686,36.4387613191321));
#70350=CARTESIAN_POINT('Ctrl Pts',(28.6729439830911,18.9383414323312,36.4345268134122));
#70351=CARTESIAN_POINT('Ctrl Pts',(28.6063074191304,18.9844178905266,36.4302923076924));
#70352=CARTESIAN_POINT('Ctrl Pts',(28.5400362733839,19.0302416769745,36.4260810229405));
#70353=CARTESIAN_POINT('Ctrl Pts',(28.4758993258002,19.0794261131487,36.4218697381886));
#70354=CARTESIAN_POINT('Ctrl Pts',(28.4142597267235,19.131744654575,36.4176584534367));
#70355=CARTESIAN_POINT('Ctrl Pts',(28.3527073376953,19.1839891737396,36.4134531269705));
#70356=CARTESIAN_POINT('Ctrl Pts',(28.293645636355,19.2393586920566,36.4092478005044));
#70357=CARTESIAN_POINT('Ctrl Pts',(28.2374084176009,19.2975837278574,36.4050424740383));
#70358=CARTESIAN_POINT('Ctrl Pts',(28.1812341943487,19.3557435414544,36.4008418582719));
#70359=CARTESIAN_POINT('Ctrl Pts',(28.1278784918971,19.4167521808891,36.3966412425055));
#70360=CARTESIAN_POINT('Ctrl Pts',(28.0776404842038,19.4803012989321,36.3924406267391));
#70361=CARTESIAN_POINT('Ctrl Pts',(28.0274328768808,19.5438119616936,36.3882425528784));
#70362=CARTESIAN_POINT('Ctrl Pts',(27.9803395107438,19.6098596845769,36.3840444790176));
#70363=CARTESIAN_POINT('Ctrl Pts',(27.9366204240837,19.6781017528979,36.3798464051569));
#70364=CARTESIAN_POINT('Ctrl Pts',(27.8929140772019,19.7463239354233,36.3756495546183));
#70365=CARTESIAN_POINT('Ctrl Pts',(27.852580310588,19.8167387984264,36.3714527040798));
#70366=CARTESIAN_POINT('Ctrl Pts',(27.8158359544079,19.888974495368,36.3672558535413));
#70367=CARTESIAN_POINT('Ctrl Pts',(27.7790907779861,19.961211804822,36.3630589093167));
#70368=CARTESIAN_POINT('Ctrl Pts',(27.745935382464,20.0352696094488,36.3588619650922));
#70369=CARTESIAN_POINT('Ctrl Pts',(27.7165400357545,20.1107526543825,36.3546650208676));
#70370=CARTESIAN_POINT('Ctrl Pts',(27.6871151990702,20.1863114253523,36.3504638661883));
#70371=CARTESIAN_POINT('Ctrl Pts',(27.661458114269,20.2632978531103,36.3462627115089));
#70372=CARTESIAN_POINT('Ctrl Pts',(27.6396901352626,20.3412985559275,36.3420615568296));
#70373=CARTESIAN_POINT('Ctrl Pts',(27.6179108952965,20.4193396098846,36.3378582288188));
#70374=CARTESIAN_POINT('Ctrl Pts',(27.6000248701609,20.498395525103,36.333654900808));
#70375=CARTESIAN_POINT('Ctrl Pts',(27.5861023566467,20.5780421615688,36.3294515727972));
#70376=CARTESIAN_POINT('Ctrl Pts',(27.5721556922805,20.6578269580107,36.3252409534339));
#70377=CARTESIAN_POINT('Ctrl Pts',(27.5621863282676,20.7382040556211,36.3210303340707));
#70378=CARTESIAN_POINT('Ctrl Pts',(27.5562126715831,20.8187439836334,36.3168197147074));
#70379=CARTESIAN_POINT('Ctrl Pts',(27.5517237840708,20.8792654859884,36.3136556566309));
#70380=CARTESIAN_POINT('Ctrl Pts',(27.5494900785215,20.9398788267477,36.3104915985544));
#70381=CARTESIAN_POINT('Ctrl Pts',(27.5495000331448,21.0004030420562,36.3073275404779));
#70382=CARTESIAN_POINT('Origin',(30.,21.,34.5704548813952));
#70383=CARTESIAN_POINT('',(28.0052508090074,20.9982034660445,43.7704548814489));
#70384=CARTESIAN_POINT('Ctrl Pts',(29.0285070491141,22.7421908646526,43.6351577566542));
#70385=CARTESIAN_POINT('Ctrl Pts',(28.9675818954129,22.708217343982,43.639602469207));
#70386=CARTESIAN_POINT('Ctrl Pts',(28.908486328592,22.6710694864593,43.6440471817597));
#70387=CARTESIAN_POINT('Ctrl Pts',(28.8515575689449,22.6309836127479,43.6484918943125));
#70388=CARTESIAN_POINT('Ctrl Pts',(28.7945220419805,22.590822559791,43.6529449427229));
#70389=CARTESIAN_POINT('Ctrl Pts',(28.7396618290827,22.5477127828589,43.6573979911333));
#70390=CARTESIAN_POINT('Ctrl Pts',(28.6872817167157,22.5019315134956,43.6618510395437));
#70391=CARTESIAN_POINT('Ctrl Pts',(28.6372470355454,22.4582001980658,43.6661046932184));
#70392=CARTESIAN_POINT('Ctrl Pts',(28.5894753228672,22.4120318333357,43.6703583468931));
#70393=CARTESIAN_POINT('Ctrl Pts',(28.5441987295342,22.3636972623754,43.6746120005678));
#70394=CARTESIAN_POINT('Ctrl Pts',(28.4973458543333,22.3136799475913,43.6790137430598));
#70395=CARTESIAN_POINT('Ctrl Pts',(28.4529706563383,22.2611349777435,43.6834154855518));
#70396=CARTESIAN_POINT('Ctrl Pts',(28.4113623498905,22.2063407392418,43.6878172280439));
#70397=CARTESIAN_POINT('Ctrl Pts',(28.3698108377044,22.151621293458,43.6922129622713));
#70398=CARTESIAN_POINT('Ctrl Pts',(28.331019032848,22.0946590590543,43.6966086964987));
#70399=CARTESIAN_POINT('Ctrl Pts',(28.2952385622418,22.0357683152292,43.7010044307261));
#70400=CARTESIAN_POINT('Ctrl Pts',(28.2594940914354,21.9769368231398,43.7053957422741));
#70401=CARTESIAN_POINT('Ctrl Pts',(28.2267552069749,21.9161810952028,43.709787053822));
#70402=CARTESIAN_POINT('Ctrl Pts',(28.1972313706564,21.8538459062117,43.71417836537));
#70403=CARTESIAN_POINT('Ctrl Pts',(28.1677266502282,21.7915510775799,43.7185668336618));
#70404=CARTESIAN_POINT('Ctrl Pts',(28.1414330620072,21.7276792694403,43.7229553019535));
#70405=CARTESIAN_POINT('Ctrl Pts',(28.1185141209499,21.6625997656468,43.7273437702453));
#70406=CARTESIAN_POINT('Ctrl Pts',(28.0955949794947,21.5975196928129,43.7317322769088));
#70407=CARTESIAN_POINT('Ctrl Pts',(28.0760507245765,21.5312323717174,43.7361207835724));
#70408=CARTESIAN_POINT('Ctrl Pts',(28.0599961095465,21.4641254868301,43.7405092902359));
#70409=CARTESIAN_POINT('Ctrl Pts',(28.043941154452,21.3970171805032,43.7448978898556));
#70410=CARTESIAN_POINT('Ctrl Pts',(28.0313760922087,21.3290897666479,43.7492864894753));
#70411=CARTESIAN_POINT('Ctrl Pts',(28.0223647706706,21.2607421373988,43.7536750890949));
#70412=CARTESIAN_POINT('Ctrl Pts',(28.0133463364229,21.192340560808,43.7580671526721));
#70413=CARTESIAN_POINT('Ctrl Pts',(28.0078872889507,21.1235186065601,43.7624592162493));
#70414=CARTESIAN_POINT('Ctrl Pts',(28.0059995797444,21.0546798547944,43.7668512798264));
#70415=CARTESIAN_POINT('Ctrl Pts',(28.0054833036828,21.0358529086072,43.7680524803494));
#70416=CARTESIAN_POINT('Ctrl Pts',(28.0052338580162,21.0170247032861,43.7692536808723));
#70417=CARTESIAN_POINT('Ctrl Pts',(28.0052508090066,20.9982034668865,43.7704548813952));
#70418=CARTESIAN_POINT('',(31.0476776298179,22.697468452278,44.2999965101293));
#70419=CARTESIAN_POINT('Ctrl Pts',(28.0052508090074,20.9982034660445,43.7704548814489));
#70420=CARTESIAN_POINT('Ctrl Pts',(28.0053328331714,20.9071294095688,43.7762673691061));
#70421=CARTESIAN_POINT('Ctrl Pts',(28.0116558478415,20.8163314699453,43.7820798567633));
#70422=CARTESIAN_POINT('Ctrl Pts',(28.0240847802233,20.7265285997501,43.7878923444204));
#70423=CARTESIAN_POINT('Ctrl Pts',(28.0338144188917,20.6562289592379,43.7924424862131));
#70424=CARTESIAN_POINT('Ctrl Pts',(28.047284839067,20.5865384317374,43.7969926280058));
#70425=CARTESIAN_POINT('Ctrl Pts',(28.0644114788864,20.5177919127253,43.8015427697985));
#70426=CARTESIAN_POINT('Ctrl Pts',(28.0811824707744,20.4504729683883,43.8059984243752));
#70427=CARTESIAN_POINT('Ctrl Pts',(28.1015025590443,20.383897827886,43.8104540789519));
#70428=CARTESIAN_POINT('Ctrl Pts',(28.1252889150972,20.3184679679995,43.8149097335286));
#70429=CARTESIAN_POINT('Ctrl Pts',(28.149039712796,20.2531359195697,43.8193587273228));
#70430=CARTESIAN_POINT('Ctrl Pts',(28.1762463277037,20.1889462095843,43.823807721117));
#70431=CARTESIAN_POINT('Ctrl Pts',(28.2067755219195,20.1262874993954,43.8282567149113));
#70432=CARTESIAN_POINT('Ctrl Pts',(28.237269005219,20.0637020829835,43.8327005045837));
#70433=CARTESIAN_POINT('Ctrl Pts',(28.2710771353077,20.002644547045,43.8371442942561));
#70434=CARTESIAN_POINT('Ctrl Pts',(28.3080183796402,19.9434841416881,43.8415880839285));
#70435=CARTESIAN_POINT('Ctrl Pts',(28.3449365344237,19.8843607136204,43.8460290960795));
#70436=CARTESIAN_POINT('Ctrl Pts',(28.3849836600036,19.82713247769,43.8504701082304));
#70437=CARTESIAN_POINT('Ctrl Pts',(28.4279327706877,19.7721432538679,43.8549111203814));
#70438=CARTESIAN_POINT('Ctrl Pts',(28.4708695994956,19.7171697549542,43.8593508625651));
#70439=CARTESIAN_POINT('Ctrl Pts',(28.5167064649867,19.6644343823259,43.8637906047489));
#70440=CARTESIAN_POINT('Ctrl Pts',(28.5651746726225,19.6142497185943,43.8682303469327));
#70441=CARTESIAN_POINT('Ctrl Pts',(28.6136454537636,19.564062390219,43.8726703248524));
#70442=CARTESIAN_POINT('Ctrl Pts',(28.6647475129065,19.516426389776,43.8771103027722));
#70443=CARTESIAN_POINT('Ctrl Pts',(28.7181749463016,19.4716178180144,43.8815502806919));
#70444=CARTESIAN_POINT('Ctrl Pts',(28.7716588913163,19.4267618510327,43.8859949548946));
#70445=CARTESIAN_POINT('Ctrl Pts',(28.8274727442014,19.3847395966743,43.8904396290973));
#70446=CARTESIAN_POINT('Ctrl Pts',(28.8852778776969,19.3457865456513,43.8948843032999));
#70447=CARTESIAN_POINT('Ctrl Pts',(28.9431169127208,19.3068106494607,43.8993315842131));
#70448=CARTESIAN_POINT('Ctrl Pts',(29.0029491333274,19.270907791132,43.9037788651263));
#70449=CARTESIAN_POINT('Ctrl Pts',(29.0644097102805,19.238268359743,43.9082261460394));
#70450=CARTESIAN_POINT('Ctrl Pts',(29.1259767210557,19.2055724053013,43.9126811284928));
#70451=CARTESIAN_POINT('Ctrl Pts',(29.18917727366,19.17615136503,43.9171361109462));
#70452=CARTESIAN_POINT('Ctrl Pts',(29.2536256467657,19.150147874198,43.9215910933996));
#70453=CARTESIAN_POINT('Ctrl Pts',(29.2868141369158,19.1367570536426,43.9238852419429));
#70454=CARTESIAN_POINT('Ctrl Pts',(29.320333266343,19.1242717121239,43.9261793904861));
#70455=CARTESIAN_POINT('Ctrl Pts',(29.3541290211179,19.1127061063158,43.9284735390293));
#70456=CARTESIAN_POINT('Ctrl Pts',(29.4196878237881,19.0902705290076,43.9329238503966));
#70457=CARTESIAN_POINT('Ctrl Pts',(29.4865478267324,19.0712102377844,43.9373741617639));
#70458=CARTESIAN_POINT('Ctrl Pts',(29.5543279193972,19.0556739061898,43.9418244731312));
#70459=CARTESIAN_POINT('Ctrl Pts',(29.6220061951333,19.0401609127393,43.9462680993935));
#70460=CARTESIAN_POINT('Ctrl Pts',(29.6906013434222,19.0281614816811,43.9507117256559));
#70461=CARTESIAN_POINT('Ctrl Pts',(29.7597155666627,19.0197750244995,43.9551553519182));
#70462=CARTESIAN_POINT('Ctrl Pts',(29.8287486916828,19.0113984079372,43.9595937640558));
#70463=CARTESIAN_POINT('Ctrl Pts',(29.8982991975004,19.0066264044798,43.9640321761933));
#70464=CARTESIAN_POINT('Ctrl Pts',(29.9679592990589,19.0055073437129,43.9684705883309));
#70465=CARTESIAN_POINT('Ctrl Pts',(30.0375757569679,19.0043889840632,43.9729062197016));
#70466=CARTESIAN_POINT('Ctrl Pts',(30.1073011851581,19.0069190350564,43.9773418510723));
#70467=CARTESIAN_POINT('Ctrl Pts',(30.1767244254279,19.0130938522524,43.981777482443));
#70468=CARTESIAN_POINT('Ctrl Pts',(30.2461278629675,19.019266908104,43.9862118485657));
#70469=CARTESIAN_POINT('Ctrl Pts',(30.315228795419,19.0290826229272,43.9906462146885));
#70470=CARTESIAN_POINT('Ctrl Pts',(30.3836196189453,19.0424853639218,43.9950805808113));
#70471=CARTESIAN_POINT('Ctrl Pts',(30.452014273844,19.0558888557612,43.9995151953549));
#70472=CARTESIAN_POINT('Ctrl Pts',(30.5196982600174,19.0728796760039,44.0039498098985));
#70473=CARTESIAN_POINT('Ctrl Pts',(30.5862743933617,19.0933511340081,44.0083844244422));
#70474=CARTESIAN_POINT('Ctrl Pts',(30.6529218696097,19.1138445292017,44.0128237911133));
#70475=CARTESIAN_POINT('Ctrl Pts',(30.7184586538887,19.1378258619552,44.0172631577845));
#70476=CARTESIAN_POINT('Ctrl Pts',(30.7825038930611,19.1651389099323,44.0217025244557));
#70477=CARTESIAN_POINT('Ctrl Pts',(30.8465870812085,19.1924681418162,44.0261445216021));
#70478=CARTESIAN_POINT('Ctrl Pts',(30.9091765248711,19.2231328019344,44.0305865187486));
#70479=CARTESIAN_POINT('Ctrl Pts',(30.9699150404523,19.2569301859064,44.035028515895));
#70480=CARTESIAN_POINT('Ctrl Pts',(31.0307601390871,19.2907868770306,44.0394783077926));
#70481=CARTESIAN_POINT('Ctrl Pts',(31.0897474111735,19.3277870042404,44.0439280996903));
#70482=CARTESIAN_POINT('Ctrl Pts',(31.1465484532773,19.3676844034356,44.048377891588));
#70483=CARTESIAN_POINT('Ctrl Pts',(31.1764455659519,19.3886843181375,44.0507200304787));
#70484=CARTESIAN_POINT('Ctrl Pts',(31.2057375495987,19.4104862182316,44.0530621693694));
#70485=CARTESIAN_POINT('Ctrl Pts',(31.2343804588746,19.4330499544502,44.0554043082601));
#70486=CARTESIAN_POINT('Ctrl Pts',(31.2889592555873,19.4760449435517,44.0598672320908));
#70487=CARTESIAN_POINT('Ctrl Pts',(31.3413948198101,19.5219782247501,44.0643301559215));
#70488=CARTESIAN_POINT('Ctrl Pts',(31.3913545013924,19.5706084462418,44.0687930797522));
#70489=CARTESIAN_POINT('Ctrl Pts',(31.4412392636534,19.6191657420649,44.0732493110018));
#70490=CARTESIAN_POINT('Ctrl Pts',(31.488655166713,19.670411612911,44.0777055422513));
#70491=CARTESIAN_POINT('Ctrl Pts',(31.5333019901385,19.7240640417571,44.0821617735008));
#70492=CARTESIAN_POINT('Ctrl Pts',(31.5778958543375,19.777652829096,44.0866127188523));
#70493=CARTESIAN_POINT('Ctrl Pts',(31.6197268532869,19.8336421310425,44.0910636642037));
#70494=CARTESIAN_POINT('Ctrl Pts',(31.6585323280854,19.8917139001162,44.0955146095551));
#70495=CARTESIAN_POINT('Ctrl Pts',(31.6973131081661,19.9497487139417,44.0999627224495));
#70496=CARTESIAN_POINT('Ctrl Pts',(31.7330719139705,20.0098629612187,44.1044108353439));
#70497=CARTESIAN_POINT('Ctrl Pts',(31.7655879444851,20.0717076038289,44.1088589482383));
#70498=CARTESIAN_POINT('Ctrl Pts',(31.7980942134645,20.1335336802537,44.1133057257787));
#70499=CARTESIAN_POINT('Ctrl Pts',(31.827359413291,20.1970886894234,44.1177525033191));
#70500=CARTESIAN_POINT('Ctrl Pts',(31.8532083461037,20.2619983818231,44.1221992808596));
#70501=CARTESIAN_POINT('Ctrl Pts',(31.8790582080234,20.3269104073192,44.1266462182338));
#70502=CARTESIAN_POINT('Ctrl Pts',(31.9014913810092,20.3931767590138,44.131093155608));
#70503=CARTESIAN_POINT('Ctrl Pts',(31.9203811980705,20.4604042099892,44.1355400929822));
#70504=CARTESIAN_POINT('Ctrl Pts',(31.939290276191,20.527700209639,44.1399915646895));
#70505=CARTESIAN_POINT('Ctrl Pts',(31.9546486547361,20.5959587944747,44.1444430363969));
#70506=CARTESIAN_POINT('Ctrl Pts',(31.9663801219466,20.6647735414483,44.1488945081043));
#70507=CARTESIAN_POINT('Ctrl Pts',(31.9781182417616,20.7336273114429,44.1533485041234));
#70508=CARTESIAN_POINT('Ctrl Pts',(31.9862252989082,20.8030373871522,44.1578025001425));
#70509=CARTESIAN_POINT('Ctrl Pts',(31.9906769543349,20.8725918920163,44.1622564961616));
#70510=CARTESIAN_POINT('Ctrl Pts',(31.9951361092244,20.9422635715885,44.1667179955867));
#70511=CARTESIAN_POINT('Ctrl Pts',(31.9959275639082,21.0120796786559,44.1711794950117));
#70512=CARTESIAN_POINT('Ctrl Pts',(31.9930790999361,21.081628817816,44.1756409944367));
#70513=CARTESIAN_POINT('Ctrl Pts',(31.9916544776593,21.1164129168766,44.1778723554548));
#70514=CARTESIAN_POINT('Ctrl Pts',(31.9893201909051,21.1511303235671,44.1801037164728));
#70515=CARTESIAN_POINT('Ctrl Pts',(31.9860845360349,21.1857303912212,44.1823350774908));
#70516=CARTESIAN_POINT('Ctrl Pts',(31.9796904185953,21.2541050803869,44.1867445664418));
#70517=CARTESIAN_POINT('Ctrl Pts',(31.9697474260424,21.3222956334465,44.1911540553928));
#70518=CARTESIAN_POINT('Ctrl Pts',(31.9562734759691,21.3898995379838,44.1955635443437));
#70519=CARTESIAN_POINT('Ctrl Pts',(31.9428220864341,21.4573902477656,44.1999656501261));
#70520=CARTESIAN_POINT('Ctrl Pts',(31.9258515746657,21.5242957730104,44.2043677559085));
#70521=CARTESIAN_POINT('Ctrl Pts',(31.9054316214507,21.5902185175643,44.2087698616909));
#70522=CARTESIAN_POINT('Ctrl Pts',(31.8850307753997,21.656079577516,44.2131678483769));
#70523=CARTESIAN_POINT('Ctrl Pts',(31.8611870322523,21.7209592040553,44.2175658350628));
#70524=CARTESIAN_POINT('Ctrl Pts',(31.8340208395287,21.7844712376336,44.2219638217487));
#70525=CARTESIAN_POINT('Ctrl Pts',(31.8068703863029,21.8479464737289,44.2263592603374));
#70526=CARTESIAN_POINT('Ctrl Pts',(31.7764014968065,21.9100552290098,44.2307546989261));
#70527=CARTESIAN_POINT('Ctrl Pts',(31.7427834152148,21.9704295596035,44.2351501375147));
#70528=CARTESIAN_POINT('Ctrl Pts',(31.7091728334126,22.0307904214105,44.2395445955339));
#70529=CARTESIAN_POINT('Ctrl Pts',(31.6724146977926,22.08941718992,44.2439390535531));
#70530=CARTESIAN_POINT('Ctrl Pts',(31.6327241542048,22.1459665783853,44.2483335115723));
#70531=CARTESIAN_POINT('Ctrl Pts',(31.5930017075813,22.2025614209311,44.2527315018322));
#70532=CARTESIAN_POINT('Ctrl Pts',(31.5503424298924,22.2570751355507,44.257129492092));
#70533=CARTESIAN_POINT('Ctrl Pts',(31.5050041369246,22.3091944509277,44.2615274823519));
#70534=CARTESIAN_POINT('Ctrl Pts',(31.4596489554362,22.3613331807571,44.2659271108637));
#70535=CARTESIAN_POINT('Ctrl Pts',(31.4116131179426,22.411075373252,44.2703267393756));
#70536=CARTESIAN_POINT('Ctrl Pts',(31.3611920146618,22.458143978392,44.2747263678874));
#70537=CARTESIAN_POINT('Ctrl Pts',(31.3106822662604,22.5052953346404,44.2791337313669));
#70538=CARTESIAN_POINT('Ctrl Pts',(31.2577792577581,22.5497633897621,44.2835410948463));
#70539=CARTESIAN_POINT('Ctrl Pts',(31.2028116783259,22.5913112922942,44.2879484583258));
#70540=CARTESIAN_POINT('Ctrl Pts',(31.1527248749113,22.6291700018809,44.2919644755936));
#70541=CARTESIAN_POINT('Ctrl Pts',(31.1009244884018,22.6646044879896,44.2959804928615));
#70542=CARTESIAN_POINT('Ctrl Pts',(31.0476776298179,22.697468452278,44.2999965101293));
#70543=CARTESIAN_POINT('',(31.9448291324621,20.5565282331122,44.3));
#70544=CARTESIAN_POINT('Origin',(30.,21.,44.3));
#70545=CARTESIAN_POINT('Ctrl Pts',(31.9448291324621,20.5565282331122,44.3));
#70546=CARTESIAN_POINT('Ctrl Pts',(31.9434341237209,20.5504104735555,44.2995994828922));
#70547=CARTESIAN_POINT('Ctrl Pts',(31.9420102376063,20.5442992487752,44.2992002906137));
#70548=CARTESIAN_POINT('Ctrl Pts',(31.9388490264969,20.5310154843226,44.2983343572612));
#70549=CARTESIAN_POINT('Ctrl Pts',(31.9371006814741,20.5238456379719,44.2978681050606));
#70550=CARTESIAN_POINT('Ctrl Pts',(31.9302822551317,20.4965429444236,44.2960964363976));
#70551=CARTESIAN_POINT('Ctrl Pts',(31.9249376115805,20.4764793757493,44.2948024403774));
#70552=CARTESIAN_POINT('Ctrl Pts',(31.8850789379699,20.3357244790958,44.2857598111901));
#70553=CARTESIAN_POINT('Ctrl Pts',(31.8395502834143,20.218434501564,44.2783986236436));
#70554=CARTESIAN_POINT('Ctrl Pts',(31.7403021141881,20.0204172501169,44.2652348708085));
#70555=CARTESIAN_POINT('Ctrl Pts',(31.6911800408815,19.9378599127613,44.2594922868282));
#70556=CARTESIAN_POINT('Ctrl Pts',(31.6202738014925,19.8361586323494,44.251833574737));
#70557=CARTESIAN_POINT('Ctrl Pts',(31.6037532576586,19.8134970278139,44.2500870503018));
#70558=CARTESIAN_POINT('Ctrl Pts',(31.5748580673,19.7755672983547,44.2470893540965));
#70559=CARTESIAN_POINT('Ctrl Pts',(31.5627252727568,19.7601197417334,44.2458466737178));
#70560=CARTESIAN_POINT('Ctrl Pts',(31.5390912707049,19.7309268221743,44.2434543449884));
#70561=CARTESIAN_POINT('Ctrl Pts',(31.5276290235602,19.7171523064516,44.2423062033946));
#70562=CARTESIAN_POINT('Ctrl Pts',(31.4968352044298,19.681144480257,44.2392517230607));
#70563=CARTESIAN_POINT('Ctrl Pts',(31.4771945495343,19.6591824771764,44.2373337287763));
#70564=CARTESIAN_POINT('Ctrl Pts',(31.3953917591754,19.5716909362662,44.2294580918896));
#70565=CARTESIAN_POINT('Ctrl Pts',(31.3293067501396,19.5099917109462,44.223343944255));
#70566=CARTESIAN_POINT('Ctrl Pts',(31.153516201105,19.3668971435795,44.2076775235069));
#70567=CARTESIAN_POINT('Ctrl Pts',(31.0392125324802,19.2918843519338,44.1979865621142));
#70568=CARTESIAN_POINT('Ctrl Pts',(30.8674702770602,19.2028404416543,44.1845936060368));
#70569=CARTESIAN_POINT('Ctrl Pts',(30.8156749929514,19.1787469412871,44.1806954665008));
#70570=CARTESIAN_POINT('Ctrl Pts',(30.7479157348429,19.1506993044561,44.1758293491229));
#70571=CARTESIAN_POINT('Ctrl Pts',(30.7328429118829,19.1446746062218,44.1747613604616));
#70572=CARTESIAN_POINT('Ctrl Pts',(30.7080722645547,19.135122616491,44.1730315622435));
#70573=CARTESIAN_POINT('Ctrl Pts',(30.6984179649346,19.1314855244572,44.1723636043077));
#70574=CARTESIAN_POINT('Ctrl Pts',(30.6803701863742,19.124845759858,44.1711270292059));
#70575=CARTESIAN_POINT('Ctrl Pts',(30.6719845429981,19.1218243447877,44.1705573744103));
#70576=CARTESIAN_POINT('Ctrl Pts',(30.6492634307127,19.113809400193,44.1690265898844));
#70577=CARTESIAN_POINT('Ctrl Pts',(30.6348907043012,19.108923108541,44.1680717854463));
#70578=CARTESIAN_POINT('Ctrl Pts',(30.5764365610879,19.0897920506394,44.1642376028347));
#70579=CARTESIAN_POINT('Ctrl Pts',(30.5319176847037,19.0769197069819,44.1614295950262));
#70580=CARTESIAN_POINT('Ctrl Pts',(30.344094779711,19.0296348695956,44.1498867395038));
#70581=CARTESIAN_POINT('Ctrl Pts',(30.1976508102751,19.0096031788969,44.141581842313));
#70582=CARTESIAN_POINT('Ctrl Pts',(29.9797068464994,19.0041026333218,44.1287496328143));
#70583=CARTESIAN_POINT('Ctrl Pts',(29.9090472334075,19.0060731760548,44.1245226979111));
#70584=CARTESIAN_POINT('Ctrl Pts',(29.8143918401592,19.0137549757,44.1186802605285));
#70585=CARTESIAN_POINT('Ctrl Pts',(29.7901769533301,19.0161668690963,44.1171699639898));
#70586=CARTESIAN_POINT('Ctrl Pts',(29.7491995082393,19.0210069945519,44.1145843950081));
#70587=CARTESIAN_POINT('Ctrl Pts',(29.7324123691852,19.0232068817404,44.113516659659));
#70588=CARTESIAN_POINT('Ctrl Pts',(29.6985766404238,19.0280798026475,44.1113463537843));
#70589=CARTESIAN_POINT('Ctrl Pts',(29.6815307075488,19.0307609124588,44.1102436023418));
#70590=CARTESIAN_POINT('Ctrl Pts',(29.6388756411331,19.0380383161197,44.1074595371683));
#70591=CARTESIAN_POINT('Ctrl Pts',(29.6133183095037,19.0429150222135,44.1057690623826));
#70592=CARTESIAN_POINT('Ctrl Pts',(29.5111896500796,19.0644811501401,44.0989203643151));
#70593=CARTESIAN_POINT('Ctrl Pts',(29.4355451836378,19.0851744811417,44.093631610921));
#70594=CARTESIAN_POINT('Ctrl Pts',(29.2306762636094,19.1544143677903,44.0787351828451));
#70595=CARTESIAN_POINT('Ctrl Pts',(29.1049738117217,19.2119929358024,44.0689159558757));
#70596=CARTESIAN_POINT('Ctrl Pts',(28.9536059122473,19.3013178496884,44.056741005391));
#70597=CARTESIAN_POINT('Ctrl Pts',(28.9215447122107,19.3214898956802,44.0541427708433));
#70598=CARTESIAN_POINT('Ctrl Pts',(28.8682915300466,19.3571516045234,44.0498173886977));
#70599=CARTESIAN_POINT('Ctrl Pts',(28.846795937031,19.3721684775037,44.0480686809835));
#70600=CARTESIAN_POINT('Ctrl Pts',(28.8160184572405,19.3945854679002,44.045568163435));
#70601=CARTESIAN_POINT('Ctrl Pts',(28.8064976028942,19.4016508017566,44.0447951148783));
#70602=CARTESIAN_POINT('Ctrl Pts',(28.7902319383214,19.4139477813066,44.0434760750596));
#70603=CARTESIAN_POINT('Ctrl Pts',(28.7834569623165,19.4191383857587,44.0429272185943));
#70604=CARTESIAN_POINT('Ctrl Pts',(28.7676038716615,19.4314463965378,44.0416437408695));
#70605=CARTESIAN_POINT('Ctrl Pts',(28.7585536040441,19.438599511443,44.0409116461403));
#70606=CARTESIAN_POINT('Ctrl Pts',(28.7325964807534,19.4594837767966,44.0388120545902));
#70607=CARTESIAN_POINT('Ctrl Pts',(28.7158512568176,19.4734142637928,44.0374577484468));
#70608=CARTESIAN_POINT('Ctrl Pts',(28.6324696291209,19.5451232207159,44.0306952999249));
#70609=CARTESIAN_POINT('Ctrl Pts',(28.5694825819699,19.6070072090484,44.0255224834918));
#70610=CARTESIAN_POINT('Ctrl Pts',(28.4391897744712,19.7532113638835,44.0141326645876));
#70611=CARTESIAN_POINT('Ctrl Pts',(28.3742085905228,19.8392192795495,44.0079492782131));
#70612=CARTESIAN_POINT('Ctrl Pts',(28.2830417138283,19.9826658339708,43.9978668915263));
#70613=CARTESIAN_POINT('Ctrl Pts',(28.2520883539796,20.0368186272763,43.9941094895549));
#70614=CARTESIAN_POINT('Ctrl Pts',(28.2127028900028,20.1138943953514,43.9887693158053));
#70615=CARTESIAN_POINT('Ctrl Pts',(28.2020767659583,20.1356585933408,43.9872624131843));
#70616=CARTESIAN_POINT('Ctrl Pts',(28.1843870541664,20.1736287264136,43.9846323230322));
#70617=CARTESIAN_POINT('Ctrl Pts',(28.1771376361307,20.1897453357007,43.9835156339193));
#70618=CARTESIAN_POINT('Ctrl Pts',(28.162622978667,20.2231947566915,43.9811962821705));
#70619=CARTESIAN_POINT('Ctrl Pts',(28.1553866715127,20.2405381290434,43.9799927779853));
#70620=CARTESIAN_POINT('Ctrl Pts',(28.1371717116799,20.2859909618703,43.9768351449418));
#70621=CARTESIAN_POINT('Ctrl Pts',(28.1265843196647,20.3142510190077,43.9748683662749));
#70622=CARTESIAN_POINT('Ctrl Pts',(28.0666613934466,20.4859580264117,43.9628918679428));
#70623=CARTESIAN_POINT('Ctrl Pts',(28.0331874819878,20.6343895543651,43.9523734764335));
#70624=CARTESIAN_POINT('Ctrl Pts',(28.0100422816045,20.8480265193637,43.9374458910679));
#70625=CARTESIAN_POINT('Ctrl Pts',(28.0062240924429,20.9111964719612,43.9330659629323));
#70626=CARTESIAN_POINT('Ctrl Pts',(28.0049358837812,21.0117371358053,43.9262358786079));
#70627=CARTESIAN_POINT('Ctrl Pts',(28.0055040430015,21.0490392613042,43.9237329406731));
#70628=CARTESIAN_POINT('Ctrl Pts',(28.0077299826456,21.1004382239322,43.9203457283881));
#70629=CARTESIAN_POINT('Ctrl Pts',(28.0084923414103,21.1145640945553,43.9194212722629));
#70630=CARTESIAN_POINT('Ctrl Pts',(28.0100506279022,21.1386695514292,43.917856060892));
#70631=CARTESIAN_POINT('Ctrl Pts',(28.0107715164431,21.148653307395,43.9172114414416));
#70632=CARTESIAN_POINT('Ctrl Pts',(28.0124768064266,21.1700289388491,43.9158395624887));
#70633=CARTESIAN_POINT('Ctrl Pts',(28.0134840410073,21.1814184245903,43.9151135253773));
#70634=CARTESIAN_POINT('Ctrl Pts',(28.0166135546796,21.2136456250799,43.9130715667147));
#70635=CARTESIAN_POINT('Ctrl Pts',(28.0189662306404,21.2344600798231,43.9117674433768));
#70636=CARTESIAN_POINT('Ctrl Pts',(28.0365042699389,21.3703995258375,43.9033242060423));
#70637=CARTESIAN_POINT('Ctrl Pts',(28.0613916600583,21.4840613045464,43.8966043146279));
#70638=CARTESIAN_POINT('Ctrl Pts',(28.122258555724,21.678857585042,43.8847528504098));
#70639=CARTESIAN_POINT('Ctrl Pts',(28.154006040805,21.7609636447577,43.8796461401918));
#70640=CARTESIAN_POINT('Ctrl Pts',(28.2144316857153,21.8909810290603,43.8710939289265));
#70641=CARTESIAN_POINT('Ctrl Pts',(28.239882461285,21.9402589313771,43.8677368774083));
#70642=CARTESIAN_POINT('Ctrl Pts',(28.2788407859681,22.0085515453623,43.8628762981749));
#70643=CARTESIAN_POINT('Ctrl Pts',(28.2906806585351,22.0284904367803,43.8614310521531));
#70644=CARTESIAN_POINT('Ctrl Pts',(28.3120232764009,22.0630455680405,43.8588775283063));
#70645=CARTESIAN_POINT('Ctrl Pts',(28.321375194925,22.0777523053833,43.8577748301383));
#70646=CARTESIAN_POINT('Ctrl Pts',(28.3413259836677,22.1082370171956,43.8554545567587));
#70647=CARTESIAN_POINT('Ctrl Pts',(28.3519600234487,22.1239897567119,43.8542357429379));
#70648=CARTESIAN_POINT('Ctrl Pts',(28.3808708824625,22.1655243923786,43.8509676018097));
#70649=CARTESIAN_POINT('Ctrl Pts',(28.3995374150165,22.1910270921372,43.8489036608418));
#70650=CARTESIAN_POINT('Ctrl Pts',(28.5086300313856,22.3328746005923,43.8370880648462));
#70651=CARTESIAN_POINT('Ctrl Pts',(28.6111104106896,22.4393438778738,43.8268576130645));
#70652=CARTESIAN_POINT('Ctrl Pts',(28.8010860846217,22.5973712411959,43.809619513463));
#70653=CARTESIAN_POINT('Ctrl Pts',(28.8825082063805,22.6553565383366,43.8026740450259));
#70654=CARTESIAN_POINT('Ctrl Pts',(28.9840587730104,22.7167544829962,43.7947754624454));
#70655=CARTESIAN_POINT('Ctrl Pts',(29.0003196373933,22.7262739544709,43.7935327649782));
#70656=CARTESIAN_POINT('Ctrl Pts',(29.0206372328177,22.7377849317006,43.7920094303564));
#70657=CARTESIAN_POINT('Ctrl Pts',(29.0245683961202,22.7399945647539,43.7917160345296));
#70658=CARTESIAN_POINT('Ctrl Pts',(29.0285070491189,22.7421908646553,43.7914234503344));
#70659=CARTESIAN_POINT('Ctrl Pts',(31.0764316815492,23.2048264539079,36.0477323453659));
#70660=CARTESIAN_POINT('Ctrl Pts',(30.343759082817,23.5625289824132,36.0900426017762));
#70661=CARTESIAN_POINT('Ctrl Pts',(28.5060462149485,23.4833658723433,36.1746631145967));
#70662=CARTESIAN_POINT('Ctrl Pts',(27.1003088914074,21.0900268756385,36.3015938838274));
#70663=CARTESIAN_POINT('Ctrl Pts',(28.3516935167001,18.6154236179253,36.4285246530582));
#70664=CARTESIAN_POINT('Ctrl Pts',(31.106936958626,18.3203304537226,36.555455422289));
#70665=CARTESIAN_POINT('Ctrl Pts',(32.8517167152586,20.4752346214199,36.6823861915197));
#70666=CARTESIAN_POINT('Ctrl Pts',(31.9886999989277,23.1097649269993,36.8093169607505));
#70667=CARTESIAN_POINT('Ctrl Pts',(29.307978492492,23.8155985483982,36.9362477299812));
#70668=CARTESIAN_POINT('Ctrl Pts',(27.2597204992662,21.947373336303,37.0631784992121));
#70669=CARTESIAN_POINT('Ctrl Pts',(27.71672768337,19.2130704126436,37.1901092684428));
#70670=CARTESIAN_POINT('Ctrl Pts',(30.2610646213885,18.1123776609252,37.3170400376736));
#70671=CARTESIAN_POINT('Ctrl Pts',(32.5667581606509,19.6515629228612,37.4439708069043));
#70672=CARTESIAN_POINT('Ctrl Pts',(32.5259010455236,22.4234923255752,37.5709015761352));
#70673=CARTESIAN_POINT('Ctrl Pts',(30.1758619809016,23.8940609300158,37.6978323453659));
#70674=CARTESIAN_POINT('Ctrl Pts',(27.6650464678629,22.7188684463249,37.8247631145967));
#70675=CARTESIAN_POINT('Ctrl Pts',(27.2888550599909,19.9722806185091,37.9516938838274));
#70676=CARTESIAN_POINT('Ctrl Pts',(29.3912011683962,18.1652373451714,38.0786246530582));
#70677=CARTESIAN_POINT('Ctrl Pts',(32.050113649744,18.9497440858611,38.2055554222889));
#70678=CARTESIAN_POINT('Ctrl Pts',(32.8348048707721,21.6086019464631,38.3324861915198));
#70679=CARTESIAN_POINT('Ctrl Pts',(31.0279076233404,23.7110737866463,38.4594169607505));
#70680=CARTESIAN_POINT('Ctrl Pts',(28.281293579258,23.335072457048,38.5863477299813));
#70681=CARTESIAN_POINT('Ctrl Pts',(27.1059269935297,20.8243397017099,38.7132784992121));
#70682=CARTESIAN_POINT('Ctrl Pts',(28.5763320889074,18.4741962054449,38.8402092684428));
#70683=CARTESIAN_POINT('Ctrl Pts',(31.3482593864868,18.4331513966575,38.9671400376736));
#70684=CARTESIAN_POINT('Ctrl Pts',(32.8876032221475,20.7387285822562,39.0940708069044));
#70685=CARTESIAN_POINT('Ctrl Pts',(31.7870900669591,23.2831610144047,39.2210015761351));
#70686=CARTESIAN_POINT('Ctrl Pts',(29.0528129048075,23.7403196403237,39.3479323453659));
#70687=CARTESIAN_POINT('Ctrl Pts',(27.18445750707,21.6922684411505,39.4748631145967));
#70688=CARTESIAN_POINT('Ctrl Pts',(27.8900809299641,19.0113430053537,39.6017938838274));
#70689=CARTESIAN_POINT('Ctrl Pts',(30.5245997659872,18.1484547680464,39.7287246530582));
#70690=CARTESIAN_POINT('Ctrl Pts',(32.6795276561991,19.8924591817973,39.855655422289));
#70691=CARTESIAN_POINT('Ctrl Pts',(32.3848219663657,22.6489812955596,39.9825861915197));
#70692=CARTESIAN_POINT('Ctrl Pts',(29.9099036715976,23.8979989261478,40.1095169607505));
#70693=CARTESIAN_POINT('Ctrl Pts',(27.5173517562181,22.4976557755345,40.2364477299813));
#70694=CARTESIAN_POINT('Ctrl Pts',(27.3944455716353,19.7281504628318,40.363378499212));
#70695=CARTESIAN_POINT('Ctrl Pts',(29.6535463828245,18.1213744572335,40.4903092684429));
#70696=CARTESIAN_POINT('Ctrl Pts',(32.2293763057922,19.1462480177964,40.6172400376735));
#70697=CARTESIAN_POINT('Ctrl Pts',(32.7671025918857,21.8658281413979,40.7441708069044));
#70698=CARTESIAN_POINT('Ctrl Pts',(30.7751339845446,23.7938651417188,40.8711015761351));
#70699=CARTESIAN_POINT('Ctrl Pts',(28.0745351703353,23.1677408318724,40.9980323453659));
#70700=CARTESIAN_POINT('Ctrl Pts',(27.1342030555683,20.5598602512758,41.1249631145967));
#70701=CARTESIAN_POINT('Ctrl Pts',(28.8137925577971,18.3543569729932,41.2518938838274));
#70702=CARTESIAN_POINT('Ctrl Pts',(31.5778170627554,18.5675098269038,41.3788246530582));
#70703=CARTESIAN_POINT('Ctrl Pts',(32.8993956773707,21.004453729579,41.5057554222889));
#70704=CARTESIAN_POINT('Ctrl Pts',(31.5703365926297,23.4373260128722,41.6326861915198));
#70705=CARTESIAN_POINT('Ctrl Pts',(28.8056702945361,23.6419863162043,41.7596169607505));
#70706=CARTESIAN_POINT('Ctrl Pts',(27.1328643882722,21.4313334472583,41.8865477299813));
#70707=CARTESIAN_POINT('Ctrl Pts',(28.0812039396034,18.8263540621345,42.0134784992121));
#70708=CARTESIAN_POINT('Ctrl Pts',(30.7837135247371,18.2085293479113,42.1404092684429));
#70709=CARTESIAN_POINT('Ctrl Pts',(32.7697495648629,20.1426770302188,42.2673400376736));
#70710=CARTESIAN_POINT('Ctrl Pts',(32.2236706232122,22.8605921026094,42.3942708069045));
#70711=CARTESIAN_POINT('Ctrl Pts',(29.6447046345813,23.8775479033933,42.5212015761351));
#70712=CARTESIAN_POINT('Ctrl Pts',(27.3905500410461,22.2638382074801,42.6481323453659));
#70713=CARTESIAN_POINT('Ctrl Pts',(27.521965507246,19.4947254252231,42.7750631145966));
#70714=CARTESIAN_POINT('Ctrl Pts',(29.918805267606,18.1017354465642,42.9019938838274));
#70715=CARTESIAN_POINT('Ctrl Pts',(32.3898806293322,19.3583581123743,43.0289246530583));
#70716=CARTESIAN_POINT('Ctrl Pts',(32.6761044863914,22.1157574108982,43.1558554222889));
#70717=CARTESIAN_POINT('Ctrl Pts',(30.5158528780656,23.8531638208612,43.2827861915198));
#70718=CARTESIAN_POINT('Ctrl Pts',(27.8839492041854,22.9821246131684,43.4097169607505));
#70719=CARTESIAN_POINT('Ctrl Pts',(27.1866622496698,20.2991673270333,43.5366477299814));
#70720=CARTESIAN_POINT('Ctrl Pts',(29.0611061008494,18.2566179316801,43.663578499212));
#70721=CARTESIAN_POINT('Ctrl Pts',(31.7943571903737,18.7226724914995,43.7905092684428));
#70722=CARTESIAN_POINT('Ctrl Pts',(32.8862611019678,21.2694728856569,43.9174400376736));
#70723=CARTESIAN_POINT('Ctrl Pts',(31.3414348862857,23.5723269250707,44.0443708069043));
#70724=CARTESIAN_POINT('Ctrl Pts',(28.5663156435887,23.5186411284601,44.1713015761352));
#70725=CARTESIAN_POINT('Ctrl Pts',(27.597396578881,21.9551030800674,44.2559220889556));
#70726=CARTESIAN_POINT('Ctrl Pts',(27.5505003151765,21.1411245936918,44.2982323453659));
#70727=CARTESIAN_POINT('Ctrl Pts',(31.0089644699886,23.0666351544788,36.1365179670879));
#70728=CARTESIAN_POINT('Ctrl Pts',(30.3222133896125,23.4019180602806,36.1788282234981));
#70729=CARTESIAN_POINT('Ctrl Pts',(28.5996823442128,23.3277166346227,36.2634487363187));
#70730=CARTESIAN_POINT('Ctrl Pts',(27.2820520311131,21.0843842859889,36.3903795055494));
#70731=CARTESIAN_POINT('Ctrl Pts',(28.4550039674528,18.7648810540163,36.5173102747802));
#70732=CARTESIAN_POINT('Ctrl Pts',(31.0375577762294,18.4882833626621,36.644241044011));
#70733=CARTESIAN_POINT('Ctrl Pts',(32.6729804533697,20.5081251962915,36.7711718132417));
#70734=CARTESIAN_POINT('Ctrl Pts',(31.8640547976968,22.9775317726687,36.8981025824725));
#70735=CARTESIAN_POINT('Ctrl Pts',(29.3513521336173,23.6391260548901,37.0250333517032));
#70736=CARTESIAN_POINT('Ctrl Pts',(27.4314722416013,21.8879950790455,37.1519641209341));
#70737=CARTESIAN_POINT('Ctrl Pts',(27.8598357124969,19.3250693054486,37.2788948901648));
#70738=CARTESIAN_POINT('Ctrl Pts',(30.2447019461309,18.2933643696932,37.4058256593956));
#70739=CARTESIAN_POINT('Ctrl Pts',(32.4058821674807,19.7360785415657,37.5327564286263));
#70740=CARTESIAN_POINT('Ctrl Pts',(32.3675858424873,22.3342724897691,37.6596871978572));
#70741=CARTESIAN_POINT('Ctrl Pts',(30.1648395280379,23.7126706714596,37.7866179670878));
#70742=CARTESIAN_POINT('Ctrl Pts',(27.8113937062773,22.6111354028808,37.9135487363187));
#70743=CARTESIAN_POINT('Ctrl Pts',(27.4587807435006,20.0366947026765,38.0404795055494));
#70744=CARTESIAN_POINT('Ctrl Pts',(29.4293586848217,18.3429109820917,38.1674102747802));
#70745=CARTESIAN_POINT('Ctrl Pts',(31.9216192420625,19.0782474102089,38.2943410440109));
#70746=CARTESIAN_POINT('Ctrl Pts',(32.6571285878948,21.5704567701534,38.4212718132418));
#70747=CARTESIAN_POINT('Ctrl Pts',(30.9634817407904,23.5411525627962,38.5482025824725));
#70748=CARTESIAN_POINT('Ctrl Pts',(28.3890164674693,23.1887177648098,38.6751333517033));
#70749=CARTESIAN_POINT('Ctrl Pts',(27.2873180089985,20.8353495137682,38.802064120934));
#70750=CARTESIAN_POINT('Ctrl Pts',(28.6655629298386,18.6325053131091,38.9289948901648));
#70751=CARTESIAN_POINT('Ctrl Pts',(31.2637549048502,18.5940330584795,39.0559256593956));
#70752=CARTESIAN_POINT('Ctrl Pts',(32.7066177115661,20.7551042188318,39.1828564286264));
#70753=CARTESIAN_POINT('Ctrl Pts',(31.6750811158181,23.1400599613368,39.3097871978571));
#70754=CARTESIAN_POINT('Ctrl Pts',(29.1121794890824,23.5685653821706,39.4367179670879));
#70755=CARTESIAN_POINT('Ctrl Pts',(27.360926487205,21.6488793230334,39.5636487363187));
#70756=CARTESIAN_POINT('Ctrl Pts',(28.0223237454753,19.1359855112171,39.6905795055494));
#70757=CARTESIAN_POINT('Ctrl Pts',(30.4917195711702,18.3271802819235,39.8175102747802));
#70758=CARTESIAN_POINT('Ctrl Pts',(32.511583640465,19.961876212134,39.944441044011));
#70759=CARTESIAN_POINT('Ctrl Pts',(32.2353491378557,22.5456285497852,40.0713718132417));
#70760=CARTESIAN_POINT('Ctrl Pts',(29.9155506143189,23.7163618468944,40.1983025824725));
#70761=CARTESIAN_POINT('Ctrl Pts',(27.6729560153313,22.4037876176339,40.3252333517033));
#70762=CARTESIAN_POINT('Ctrl Pts',(27.5577531877748,19.8078658254209,40.452164120934));
#70763=CARTESIAN_POINT('Ctrl Pts',(29.6752609606157,18.3017972762811,40.5790948901649));
#70764=CARTESIAN_POINT('Ctrl Pts',(32.0896463020688,19.2624351194098,40.7060256593955));
#70765=CARTESIAN_POINT('Ctrl Pts',(32.5936696660659,21.8115608698265,40.8329564286264));
#70766=CARTESIAN_POINT('Ctrl Pts',(30.7265511256235,23.6187548269458,40.9598871978571));
#70767=CARTESIAN_POINT('Ctrl Pts',(28.1952169983062,23.0318739377452,41.0868179670879));
#70768=CARTESIAN_POINT('Ctrl Pts',(27.3138218200968,20.5874467688898,41.2137487363186));
#70769=CARTESIAN_POINT('Ctrl Pts',(28.8881401544254,18.5201772111709,41.3406795055495));
#70770=CARTESIAN_POINT('Ctrl Pts',(31.478924657969,18.7199703424573,41.4676102747802));
#70771=CARTESIAN_POINT('Ctrl Pts',(32.7176710543262,21.0041745843987,41.594541044011));
#70772=CARTESIAN_POINT('Ctrl Pts',(31.4719130392057,23.2845624027232,41.7214718132416));
#70773=CARTESIAN_POINT('Ctrl Pts',(28.8805269680182,23.4763952686807,41.8484025824725));
#70774=CARTESIAN_POINT('Ctrl Pts',(27.3125670560817,21.4042988797719,41.9753333517032));
#70775=CARTESIAN_POINT('Ctrl Pts',(28.2014677909627,18.9625910689611,42.1022641209341));
#70776=CARTESIAN_POINT('Ctrl Pts',(30.734592928342,18.3834895839184,42.2291948901648));
#70777=CARTESIAN_POINT('Ctrl Pts',(32.5961507354479,20.1964112254951,42.3561256593956));
#70778=CARTESIAN_POINT('Ctrl Pts',(32.0842982329819,22.7439762846564,42.4830564286263));
#70779=CARTESIAN_POINT('Ctrl Pts',(29.6669733841881,23.6971926272514,42.6099871978571));
#70780=CARTESIAN_POINT('Ctrl Pts',(27.5541018162817,22.1846249687918,42.7369179670879));
#70781=CARTESIAN_POINT('Ctrl Pts',(27.6772805915587,19.589071104502,42.8638487363187));
#70782=CARTESIAN_POINT('Ctrl Pts',(29.9238942874499,18.2833891744659,42.9907795055494));
#70783=CARTESIAN_POINT('Ctrl Pts',(32.240090740399,19.4612508481023,43.1177102747802));
#70784=CARTESIAN_POINT('Ctrl Pts',(32.5083750237268,22.0458253914477,43.244641044011));
#70785=CARTESIAN_POINT('Ctrl Pts',(30.4835209095301,23.6743368591337,43.3715718132417));
#70786=CARTESIAN_POINT('Ctrl Pts',(28.0165763361817,22.8578915355769,43.4985025824725));
#70787=CARTESIAN_POINT('Ctrl Pts',(27.362993043761,20.3430932231455,43.6254333517033));
#70788=CARTESIAN_POINT('Ctrl Pts',(29.1199528947636,18.428564132788,43.752364120934));
#70789=CARTESIAN_POINT('Ctrl Pts',(31.6818927597432,18.8654079195272,43.8792948901649));
#70790=CARTESIAN_POINT('Ctrl Pts',(32.7053597110826,21.2525832079393,44.0062256593955));
#70791=CARTESIAN_POINT('Ctrl Pts',(31.2573581419655,23.4111018999891,44.1331564286264));
#70792=CARTESIAN_POINT('Ctrl Pts',(28.6561742824999,23.3607809532429,44.2600871978571));
#70793=CARTESIAN_POINT('Ctrl Pts',(27.7479838907253,21.8952403477924,44.3447077106776));
#70794=CARTESIAN_POINT('Ctrl Pts',(27.7040269312043,21.1322793664635,44.3870179670879));
#70795=CARTESIAN_POINT('Ctrl Pts',(30.9414972584282,22.9284438550497,36.2253035888098));
#70796=CARTESIAN_POINT('Ctrl Pts',(30.3006676964081,23.2413071381481,36.26761384522));
#70797=CARTESIAN_POINT('Ctrl Pts',(28.693318473477,23.1720673969021,36.3522343580406));
#70798=CARTESIAN_POINT('Ctrl Pts',(27.4637951708188,21.0787416963392,36.4791651272713));
#70799=CARTESIAN_POINT('Ctrl Pts',(28.5583144182053,18.9143384901075,36.6060958965021));
#70800=CARTESIAN_POINT('Ctrl Pts',(30.9681785938328,18.6562362716017,36.7330266657328));
#70801=CARTESIAN_POINT('Ctrl Pts',(32.4942441914807,20.5410157711632,36.8599574349636));
#70802=CARTESIAN_POINT('Ctrl Pts',(31.739409596466,22.8452986183379,36.9868882041944));
#70803=CARTESIAN_POINT('Ctrl Pts',(29.3947257747426,23.462653561382,37.1138189734251));
#70804=CARTESIAN_POINT('Ctrl Pts',(27.6032239839365,21.828616821788,37.240749742656));
#70805=CARTESIAN_POINT('Ctrl Pts',(28.0029437416238,19.4370681982537,37.3676805118867));
#70806=CARTESIAN_POINT('Ctrl Pts',(30.2283392708734,18.474351078461,37.4946112811175));
#70807=CARTESIAN_POINT('Ctrl Pts',(32.2450061743102,19.8205941602703,37.6215420503482));
#70808=CARTESIAN_POINT('Ctrl Pts',(32.209270639451,22.245052653963,37.748472819579));
#70809=CARTESIAN_POINT('Ctrl Pts',(30.1538170751741,23.5312804129035,37.8754035888098));
#70810=CARTESIAN_POINT('Ctrl Pts',(27.9577409446919,22.5034023594369,38.0023343580406));
#70811=CARTESIAN_POINT('Ctrl Pts',(27.6287064270102,20.1011087868441,38.1292651272713));
#70812=CARTESIAN_POINT('Ctrl Pts',(29.4675162012472,18.520584619012,38.2561958965021));
#70813=CARTESIAN_POINT('Ctrl Pts',(31.793124834381,19.2067507345566,38.3831266657329));
#70814=CARTESIAN_POINT('Ctrl Pts',(32.4794523050175,21.5323115938435,38.5100574349637));
#70815=CARTESIAN_POINT('Ctrl Pts',(30.8990558582405,23.3712313389463,38.6369882041944));
#70816=CARTESIAN_POINT('Ctrl Pts',(28.4967393556804,23.0423630725713,38.7639189734252));
#70817=CARTESIAN_POINT('Ctrl Pts',(27.4687090244673,20.8463593258267,38.8908497426559));
#70818=CARTESIAN_POINT('Ctrl Pts',(28.7547937707697,18.7908144207732,39.0177805118867));
#70819=CARTESIAN_POINT('Ctrl Pts',(31.1792504232137,18.7549147203014,39.1447112811175));
#70820=CARTESIAN_POINT('Ctrl Pts',(32.5256322009844,20.7714798554076,39.2716420503482));
#70821=CARTESIAN_POINT('Ctrl Pts',(31.5630721646773,22.9969589082687,39.398572819579));
#70822=CARTESIAN_POINT('Ctrl Pts',(29.171546073357,23.3968111240174,39.5255035888098));
#70823=CARTESIAN_POINT('Ctrl Pts',(27.53739546734,21.6054902049163,39.6524343580406));
#70824=CARTESIAN_POINT('Ctrl Pts',(28.1545665609866,19.2606280170804,39.7793651272713));
#70825=CARTESIAN_POINT('Ctrl Pts',(30.4588393763534,18.5059057958006,39.9062958965021));
#70826=CARTESIAN_POINT('Ctrl Pts',(32.3436396247307,20.0312932424708,40.0332266657328));
#70827=CARTESIAN_POINT('Ctrl Pts',(32.0858763093458,22.4422758040107,40.1601574349636));
#70828=CARTESIAN_POINT('Ctrl Pts',(29.9211975570403,23.5347247676409,40.2870882041944));
#70829=CARTESIAN_POINT('Ctrl Pts',(27.8285602744445,22.3099194597335,40.4140189734252));
#70830=CARTESIAN_POINT('Ctrl Pts',(27.7210608039143,19.8875811880102,40.5409497426559));
#70831=CARTESIAN_POINT('Ctrl Pts',(29.6969755384068,18.4822200953287,40.6678805118867));
#70832=CARTESIAN_POINT('Ctrl Pts',(31.9499162983454,19.3786222210231,40.7948112811175));
#70833=CARTESIAN_POINT('Ctrl Pts',(32.420236740246,21.7572935982551,40.9217420503482));
#70834=CARTESIAN_POINT('Ctrl Pts',(30.6779682667023,23.4436445121727,41.048672819579));
#70835=CARTESIAN_POINT('Ctrl Pts',(28.3158988262772,22.896007043618,41.1756035888098));
#70836=CARTESIAN_POINT('Ctrl Pts',(27.4934405846254,20.6150332865038,41.3025343580405));
#70837=CARTESIAN_POINT('Ctrl Pts',(28.9624877510537,18.6859974493487,41.4294651272713));
#70838=CARTESIAN_POINT('Ctrl Pts',(31.3800322531826,18.8724308580108,41.5563958965021));
#70839=CARTESIAN_POINT('Ctrl Pts',(32.5359464312817,21.0038954392185,41.6833266657329));
#70840=CARTESIAN_POINT('Ctrl Pts',(31.3734894857819,23.1317987925741,41.8102574349636));
#70841=CARTESIAN_POINT('Ctrl Pts',(28.9553836415003,23.3108042211572,41.9371882041944));
#70842=CARTESIAN_POINT('Ctrl Pts',(27.4922697238911,21.3772643122856,42.0641189734252));
#70843=CARTESIAN_POINT('Ctrl Pts',(28.3217316423219,19.0988280757876,42.1910497426559));
#70844=CARTESIAN_POINT('Ctrl Pts',(30.685472331947,18.5584498199254,42.3179805118868));
#70845=CARTESIAN_POINT('Ctrl Pts',(32.422551906033,20.2501454207713,42.4449112811174));
#70846=CARTESIAN_POINT('Ctrl Pts',(31.9449258427517,22.6273604667032,42.5718420503483));
#70847=CARTESIAN_POINT('Ctrl Pts',(29.6892421337947,23.5168373511096,42.698772819579));
#70848=CARTESIAN_POINT('Ctrl Pts',(27.7176535915173,22.1054117301034,42.8257035888098));
#70849=CARTESIAN_POINT('Ctrl Pts',(27.8325956758717,19.6834167837808,42.9526343580406));
#70850=CARTESIAN_POINT('Ctrl Pts',(29.9289833072939,18.4650429023676,43.0795651272713));
#70851=CARTESIAN_POINT('Ctrl Pts',(32.0903008514657,19.5641435838305,43.2064958965021));
#70852=CARTESIAN_POINT('Ctrl Pts',(32.3406455610623,21.9758933719972,43.3334266657328));
#70853=CARTESIAN_POINT('Ctrl Pts',(30.4511889409944,23.4955098974062,43.4603574349637));
#70854=CARTESIAN_POINT('Ctrl Pts',(28.1492034681781,22.7336584579854,43.5872882041943));
#70855=CARTESIAN_POINT('Ctrl Pts',(27.5393238378524,20.3870191192575,43.7142189734252));
#70856=CARTESIAN_POINT('Ctrl Pts',(29.1787996886778,18.6005103338958,43.8411497426559));
#70857=CARTESIAN_POINT('Ctrl Pts',(31.5694283291128,19.0081433475549,43.9680805118867));
#70858=CARTESIAN_POINT('Ctrl Pts',(32.5244583201973,21.2356935302216,44.0950112811175));
#70859=CARTESIAN_POINT('Ctrl Pts',(31.1732813976455,23.2498768749074,44.2219420503483));
#70860=CARTESIAN_POINT('Ctrl Pts',(28.7460329214112,23.2029207780256,44.348872819579));
#70861=CARTESIAN_POINT('Ctrl Pts',(27.8985712025696,21.8353776155173,44.4334933323995));
#70862=CARTESIAN_POINT('Ctrl Pts',(27.857553547232,21.1234341392353,44.4758035888098));
#70863=CARTESIAN_POINT('Ctrl Pts',(30.8740300468677,22.7902525556206,36.3140892105317));
#70864=CARTESIAN_POINT('Ctrl Pts',(30.2791220032035,23.0806962160155,36.356399466942));
#70865=CARTESIAN_POINT('Ctrl Pts',(28.7869546027412,23.0164181591815,36.4410199797625));
#70866=CARTESIAN_POINT('Ctrl Pts',(27.6455383105245,21.0730991066897,36.5679507489932));
#70867=CARTESIAN_POINT('Ctrl Pts',(28.6616248689581,19.0637959261985,36.6948815182241));
#70868=CARTESIAN_POINT('Ctrl Pts',(30.8987994114361,18.8241891805412,36.8218122874547));
#70869=CARTESIAN_POINT('Ctrl Pts',(32.3155079295918,20.573906346035,36.9487430566855));
#70870=CARTESIAN_POINT('Ctrl Pts',(31.614764395235,22.7130654640073,37.0756738259163));
#70871=CARTESIAN_POINT('Ctrl Pts',(29.4380994158679,23.2861810678738,37.202604595147));
#70872=CARTESIAN_POINT('Ctrl Pts',(27.7749757262716,21.7692385645306,37.3295353643779));
#70873=CARTESIAN_POINT('Ctrl Pts',(28.1460517707507,19.5490670910589,37.4564661336086));
#70874=CARTESIAN_POINT('Ctrl Pts',(30.2119765956158,18.655337787229,37.5833969028394));
#70875=CARTESIAN_POINT('Ctrl Pts',(32.08413018114,19.9051097789748,37.7103276720702));
#70876=CARTESIAN_POINT('Ctrl Pts',(32.0509554364147,22.1558328181569,37.8372584413009));
#70877=CARTESIAN_POINT('Ctrl Pts',(30.1427946223102,23.3498901543472,37.9641892105317));
#70878=CARTESIAN_POINT('Ctrl Pts',(28.1040881831063,22.3956693159929,38.0911199797624));
#70879=CARTESIAN_POINT('Ctrl Pts',(27.7986321105198,20.1655228710115,38.2180507489932));
#70880=CARTESIAN_POINT('Ctrl Pts',(29.5056737176726,18.6982582559323,38.344981518224));
#70881=CARTESIAN_POINT('Ctrl Pts',(31.6646304266995,19.3352540589044,38.4719122874548));
#70882=CARTESIAN_POINT('Ctrl Pts',(32.3017760221401,21.4941664175338,38.5988430566855));
#70883=CARTESIAN_POINT('Ctrl Pts',(30.8346299756906,23.2013101150963,38.7257738259163));
#70884=CARTESIAN_POINT('Ctrl Pts',(28.6044622438917,22.8960083803331,38.852704595147));
#70885=CARTESIAN_POINT('Ctrl Pts',(27.6501000399361,20.857369137885,38.9796353643779));
#70886=CARTESIAN_POINT('Ctrl Pts',(28.8440246117008,18.9491235284374,39.1065661336086));
#70887=CARTESIAN_POINT('Ctrl Pts',(31.0947459415771,18.9157963821233,39.2334969028394));
#70888=CARTESIAN_POINT('Ctrl Pts',(32.3446466904029,20.7878554919833,39.3604276720701));
#70889=CARTESIAN_POINT('Ctrl Pts',(31.4510632135363,22.8538578552008,39.4873584413009));
#70890=CARTESIAN_POINT('Ctrl Pts',(29.2309126576318,23.2250568658642,39.6142892105317));
#70891=CARTESIAN_POINT('Ctrl Pts',(27.713864447475,21.5621010867992,39.7412199797624));
#70892=CARTESIAN_POINT('Ctrl Pts',(28.2868093764979,19.3852705229439,39.8681507489932));
#70893=CARTESIAN_POINT('Ctrl Pts',(30.4259591815364,18.6846313096777,39.9950815182239));
#70894=CARTESIAN_POINT('Ctrl Pts',(32.1756956089965,20.1007102728075,40.1220122874548));
#70895=CARTESIAN_POINT('Ctrl Pts',(31.9364034808358,22.3389230582362,40.2489430566856));
#70896=CARTESIAN_POINT('Ctrl Pts',(29.9268444997616,23.3530876883875,40.3758738259163));
#70897=CARTESIAN_POINT('Ctrl Pts',(27.9841645335578,22.2160513018329,40.5028045951471));
#70898=CARTESIAN_POINT('Ctrl Pts',(27.8843684200537,19.9672965505993,40.6297353643778));
#70899=CARTESIAN_POINT('Ctrl Pts',(29.718690116198,18.6626429143762,40.7566661336087));
#70900=CARTESIAN_POINT('Ctrl Pts',(31.8101862946221,19.4948093226364,40.8835969028394));
#70901=CARTESIAN_POINT('Ctrl Pts',(32.246803814426,21.7030263266837,41.0105276720702));
#70902=CARTESIAN_POINT('Ctrl Pts',(30.6293854077811,23.2685341973996,41.1374584413009));
#70903=CARTESIAN_POINT('Ctrl Pts',(28.4365806542482,22.7601401494908,41.2643892105318));
#70904=CARTESIAN_POINT('Ctrl Pts',(27.6730593491541,20.6426198041178,41.3913199797624));
#70905=CARTESIAN_POINT('Ctrl Pts',(29.0368353476819,18.8518176875265,41.5182507489933));
#70906=CARTESIAN_POINT('Ctrl Pts',(31.2811398483962,19.0248913735642,41.645181518224));
#70907=CARTESIAN_POINT('Ctrl Pts',(32.3542218082372,21.0036162940384,41.7721122874547));
#70908=CARTESIAN_POINT('Ctrl Pts',(31.275065932358,22.979035182425,41.8990430566856));
#70909=CARTESIAN_POINT('Ctrl Pts',(29.0302403149823,23.1452131736336,42.0259738259164));
#70910=CARTESIAN_POINT('Ctrl Pts',(27.6719723917006,21.3502297447993,42.152904595147));
#70911=CARTESIAN_POINT('Ctrl Pts',(28.4419954936812,19.2350650826142,42.2798353643778));
#70912=CARTESIAN_POINT('Ctrl Pts',(30.6363517355519,18.7334100559325,42.4067661336086));
#70913=CARTESIAN_POINT('Ctrl Pts',(32.248953076618,20.3038796160475,42.5336969028394));
#70914=CARTESIAN_POINT('Ctrl Pts',(31.8055534525214,22.5107446487501,42.6606276720701));
#70915=CARTESIAN_POINT('Ctrl Pts',(29.7115108834014,23.3364820749677,42.7875584413009));
#70916=CARTESIAN_POINT('Ctrl Pts',(27.8812053667529,22.026198491415,42.9144892105316));
#70917=CARTESIAN_POINT('Ctrl Pts',(27.9879107601844,19.7777624630598,43.0414199797625));
#70918=CARTESIAN_POINT('Ctrl Pts',(29.9340723271378,18.6466966302693,43.1683507489932));
#70919=CARTESIAN_POINT('Ctrl Pts',(31.9405109625326,19.6670363195586,43.295281518224));
#70920=CARTESIAN_POINT('Ctrl Pts',(32.1729160983978,21.9059613525467,43.4222122874547));
#70921=CARTESIAN_POINT('Ctrl Pts',(30.4188569724588,23.3166829356786,43.5491430566855));
#70922=CARTESIAN_POINT('Ctrl Pts',(28.2818306001745,22.6094253803939,43.6760738259163));
#70923=CARTESIAN_POINT('Ctrl Pts',(27.7156546319436,20.4309450153696,43.8030045951471));
#70924=CARTESIAN_POINT('Ctrl Pts',(29.237646482592,18.7724565350037,43.9299353643778));
#70925=CARTESIAN_POINT('Ctrl Pts',(31.4569638984824,19.1508787755826,44.0568661336086));
#70926=CARTESIAN_POINT('Ctrl Pts',(32.3435569293119,21.218803852504,44.1837969028393));
#70927=CARTESIAN_POINT('Ctrl Pts',(31.0892046533254,23.0886518498259,44.3107276720702));
#70928=CARTESIAN_POINT('Ctrl Pts',(28.8358915603223,23.0450606028084,44.4376584413009));
#70929=CARTESIAN_POINT('Ctrl Pts',(28.049158514414,21.7755148832423,44.5222789541214));
#70930=CARTESIAN_POINT('Ctrl Pts',(28.0110801632598,21.114588912007,44.5645892105317));
#70931=CARTESIAN_POINT('Ctrl Pts',(31.0493358146879,22.7002587726697,44.3));
#70932=CARTESIAN_POINT('Ctrl Pts',(31.0110837864123,22.7305054804131,44.3));
#70933=CARTESIAN_POINT('Ctrl Pts',(30.9717244691516,22.7591991002977,44.3));
#70934=CARTESIAN_POINT('Ctrl Pts',(30.9313170587865,22.7862512397935,44.3));
#70935=CARTESIAN_POINT('Ctrl Pts',(30.8717553609692,22.8261268800139,44.3));
#70936=CARTESIAN_POINT('Ctrl Pts',(30.8099181934742,22.8624382115192,44.3));
#70937=CARTESIAN_POINT('Ctrl Pts',(30.7461536935897,22.8952427892732,44.3));
#70938=CARTESIAN_POINT('Ctrl Pts',(30.710432840364,22.9136199036425,44.3));
#70939=CARTESIAN_POINT('Ctrl Pts',(30.6741064149253,22.93089587639,44.3));
#70940=CARTESIAN_POINT('Ctrl Pts',(30.6372309081889,22.9470757234022,44.3));
#70941=CARTESIAN_POINT('Ctrl Pts',(30.6230043527359,22.9533179017778,44.3));
#70942=CARTESIAN_POINT('Ctrl Pts',(30.6086960404744,22.9593968914265,44.3));
#70943=CARTESIAN_POINT('Ctrl Pts',(30.5943091070883,22.9653128279144,44.3));
#70944=CARTESIAN_POINT('Ctrl Pts',(30.5807067611259,22.9709061404461,44.3));
#70945=CARTESIAN_POINT('Ctrl Pts',(30.5670423559514,22.9763502989973,44.3));
#70946=CARTESIAN_POINT('Ctrl Pts',(30.5533210882546,22.9816450286663,44.3));
#70947=CARTESIAN_POINT('Ctrl Pts',(30.4832690776367,23.0086765294862,44.3));
#70948=CARTESIAN_POINT('Ctrl Pts',(30.4117194145467,23.0318241057179,44.3));
#70949=CARTESIAN_POINT('Ctrl Pts',(30.3390502812968,23.0511463865923,44.3));
#70950=CARTESIAN_POINT('Ctrl Pts',(30.2796354790101,23.0669444214185,44.3));
#70951=CARTESIAN_POINT('Ctrl Pts',(30.2194713251798,23.0801846338831,44.3));
#70952=CARTESIAN_POINT('Ctrl Pts',(30.1587495264957,23.0908780764479,44.3));
#70953=CARTESIAN_POINT('Ctrl Pts',(30.1344248905864,23.0951617785555,44.3));
#70954=CARTESIAN_POINT('Ctrl Pts',(30.1100106469206,23.0990365727744,44.3));
#70955=CARTESIAN_POINT('Ctrl Pts',(30.0855187098372,23.1025022765372,44.3));
#70956=CARTESIAN_POINT('Ctrl Pts',(30.0688128119039,23.1048662256659,44.3));
#70957=CARTESIAN_POINT('Ctrl Pts',(30.0520683767963,23.107039987055,44.3));
#70958=CARTESIAN_POINT('Ctrl Pts',(30.0353127006666,23.1090209570334,44.3));
#70959=CARTESIAN_POINT('Ctrl Pts',(29.9579615115999,23.1181659406286,44.3));
#70960=CARTESIAN_POINT('Ctrl Pts',(29.8802676556082,23.1232220884979,44.3));
#70961=CARTESIAN_POINT('Ctrl Pts',(29.8026183201236,23.1242482721955,44.3));
#70962=CARTESIAN_POINT('Ctrl Pts',(29.7236225788762,23.1252922494728,44.3));
#70963=CARTESIAN_POINT('Ctrl Pts',(29.6446719430159,23.1221656183407,44.3));
#70964=CARTESIAN_POINT('Ctrl Pts',(29.5661502640416,23.114882161993,44.3));
#70965=CARTESIAN_POINT('Ctrl Pts',(29.5085211535759,23.1095366432023,44.3));
#70966=CARTESIAN_POINT('Ctrl Pts',(29.4511225255262,23.1019510687179,44.3));
#70967=CARTESIAN_POINT('Ctrl Pts',(29.3941029595966,23.0921133067172,44.3));
#70968=CARTESIAN_POINT('Ctrl Pts',(29.3510914822676,23.0846924035525,44.3));
#70969=CARTESIAN_POINT('Ctrl Pts',(29.3082956236541,23.0759896795228,44.3));
#70970=CARTESIAN_POINT('Ctrl Pts',(29.265779522772,23.0659940680441,44.3));
#70971=CARTESIAN_POINT('Ctrl Pts',(29.2536330171228,23.0631384028073,44.3));
#70972=CARTESIAN_POINT('Ctrl Pts',(29.241507116384,23.0601766100956,44.3));
#70973=CARTESIAN_POINT('Ctrl Pts',(29.2294106201817,23.0571102122805,44.3));
#70974=CARTESIAN_POINT('Ctrl Pts',(29.1508116985187,23.0371858013084,44.3));
#70975=CARTESIAN_POINT('Ctrl Pts',(29.0736725133479,23.0129060533399,44.3));
#70976=CARTESIAN_POINT('Ctrl Pts',(28.9983903470095,22.9843016580501,44.3));
#70977=CARTESIAN_POINT('Ctrl Pts',(28.9641457091262,22.9712899820289,44.3));
#70978=CARTESIAN_POINT('Ctrl Pts',(28.9302851512349,22.9573827579083,44.3));
#70979=CARTESIAN_POINT('Ctrl Pts',(28.8968456509869,22.9425793284446,44.3));
#70980=CARTESIAN_POINT('Ctrl Pts',(28.8251173759661,22.9108257300968,44.3));
#70981=CARTESIAN_POINT('Ctrl Pts',(28.755325360237,22.8749522429844,44.3));
#70982=CARTESIAN_POINT('Ctrl Pts',(28.6876160787102,22.8352802507896,44.3));
#70983=CARTESIAN_POINT('Ctrl Pts',(28.6199067971835,22.7956082585949,44.3));
#70984=CARTESIAN_POINT('Ctrl Pts',(28.554279656942,22.7521371933869,44.3));
#70985=CARTESIAN_POINT('Ctrl Pts',(28.4908994911728,22.7051394630327,44.3));
#70986=CARTESIAN_POINT('Ctrl Pts',(28.4802385188713,22.6972341271053,44.3));
#70987=CARTESIAN_POINT('Ctrl Pts',(28.4696392286813,22.6892274062858,44.3));
#70988=CARTESIAN_POINT('Ctrl Pts',(28.4591088034363,22.6811253616606,44.3));
#70989=CARTESIAN_POINT('Ctrl Pts',(28.3951127315144,22.6318871762609,44.3));
#70990=CARTESIAN_POINT('Ctrl Pts',(28.3338332975407,22.5792690281287,44.3));
#70991=CARTESIAN_POINT('Ctrl Pts',(28.2754113048987,22.5236317699283,44.3));
#70992=CARTESIAN_POINT('Ctrl Pts',(28.2159087924481,22.4669654958237,44.3));
#70993=CARTESIAN_POINT('Ctrl Pts',(28.1593697260286,22.4071669102395,44.3));
#70994=CARTESIAN_POINT('Ctrl Pts',(28.1059614101741,22.3445654070193,44.3));
#70995=CARTESIAN_POINT('Ctrl Pts',(28.0519240633645,22.2812265975814,44.3));
#70996=CARTESIAN_POINT('Ctrl Pts',(28.0010909162046,22.215017840663,44.3));
#70997=CARTESIAN_POINT('Ctrl Pts',(27.95366470885,22.1462362325089,44.3));
#70998=CARTESIAN_POINT('Ctrl Pts',(27.9242510796939,22.1035780308972,44.3));
#70999=CARTESIAN_POINT('Ctrl Pts',(27.8961485348881,22.0599293588499,44.3));
#71000=CARTESIAN_POINT('Ctrl Pts',(27.8694129519346,22.0153543689321,44.3));
#71001=CARTESIAN_POINT('Ctrl Pts',(27.8627684362021,22.0042762778988,44.3));
#71002=CARTESIAN_POINT('Ctrl Pts',(27.856213317223,21.9931491635314,44.3));
#71003=CARTESIAN_POINT('Ctrl Pts',(27.8497487774402,21.9819753686283,44.3));
#71004=CARTESIAN_POINT('Ctrl Pts',(27.8067383584659,21.9076329380046,44.3));
#71005=CARTESIAN_POINT('Ctrl Pts',(27.7677258289858,21.8312122550966,44.3));
#71006=CARTESIAN_POINT('Ctrl Pts',(27.732887393996,21.7530632053734,44.3));
#71007=CARTESIAN_POINT('Ctrl Pts',(27.6980144559037,21.6748367588131,44.3));
#71008=CARTESIAN_POINT('Ctrl Pts',(27.6673231902278,21.5948777547204,44.3));
#71009=CARTESIAN_POINT('Ctrl Pts',(27.6410257761963,21.5134989584412,44.3));
#71010=CARTESIAN_POINT('Ctrl Pts',(27.6152975322414,21.4338814903161,44.3));
#71011=CARTESIAN_POINT('Ctrl Pts',(27.5937744971102,21.3529042062414,44.3));
#71012=CARTESIAN_POINT('Ctrl Pts',(27.5766978863451,21.2708353686905,44.3));
#71013=CARTESIAN_POINT('Ctrl Pts',(27.5677489591492,21.2278275340327,44.3));
#71014=CARTESIAN_POINT('Ctrl Pts',(27.5600218842896,21.1845195934477,44.3));
#71015=CARTESIAN_POINT('Ctrl Pts',(27.5535569140831,21.1409484919019,44.3));
#71016=CARTESIAN_POINT('Origin',(29.3411117931064,21.1369041098113,36.4999999999305));
#71017=CARTESIAN_POINT('Origin',(30.,21.,44.3));
#71018=CARTESIAN_POINT('',(28.4205166578229,19.1264518629656,44.3));
#71019=CARTESIAN_POINT('Origin',(30.,21.,44.3));
#71020=CARTESIAN_POINT('Ctrl Pts',(28.4205166578229,19.1264518629657,44.3));
#71021=CARTESIAN_POINT('Ctrl Pts',(28.4546614288766,19.1023864633534,44.3));
#71022=CARTESIAN_POINT('Ctrl Pts',(28.4894415473359,19.079285885032,44.3));
#71023=CARTESIAN_POINT('Ctrl Pts',(28.524842571324,19.0571918940411,44.3));
#71024=CARTESIAN_POINT('Ctrl Pts',(28.5971358507719,19.012073225571,44.3));
#71025=CARTESIAN_POINT('Ctrl Pts',(28.6720177454898,18.9711491070475,44.3));
#71026=CARTESIAN_POINT('Ctrl Pts',(28.7490901216485,18.934435204942,44.3));
#71027=CARTESIAN_POINT('Ctrl Pts',(28.7880521274008,18.9158754130124,44.3));
#71028=CARTESIAN_POINT('Ctrl Pts',(28.8275741586732,18.8983923694088,44.3));
#71029=CARTESIAN_POINT('Ctrl Pts',(28.8676055138014,18.8819930200461,44.3));
#71030=CARTESIAN_POINT('Ctrl Pts',(28.888102699806,18.873596089361,44.3));
#71031=CARTESIAN_POINT('Ctrl Pts',(28.9087334189042,18.8654833271773,44.3));
#71032=CARTESIAN_POINT('Ctrl Pts',(28.9294908535282,18.8576560003214,44.3));
#71033=CARTESIAN_POINT('Ctrl Pts',(28.9441432078653,18.852130810495,44.3));
#71034=CARTESIAN_POINT('Ctrl Pts',(28.9588573914148,18.8467484283512,44.3));
#71035=CARTESIAN_POINT('Ctrl Pts',(28.9736195638014,18.8415130807057,44.3));
#71036=CARTESIAN_POINT('Ctrl Pts',(29.0534511507612,18.8132011155095,44.3));
#71037=CARTESIAN_POINT('Ctrl Pts',(29.134775488115,18.7891505943989,44.3));
#71038=CARTESIAN_POINT('Ctrl Pts',(29.2172006713952,18.769378007905,44.3));
#71039=CARTESIAN_POINT('Ctrl Pts',(29.2995426019427,18.7496253925144,44.3));
#71040=CARTESIAN_POINT('Ctrl Pts',(29.3829842205534,18.7341421254923,44.3));
#71041=CARTESIAN_POINT('Ctrl Pts',(29.4671329462824,18.7229959840501,44.3));
#71042=CARTESIAN_POINT('Ctrl Pts',(29.4793170973916,18.7213821001744,44.3));
#71043=CARTESIAN_POINT('Ctrl Pts',(29.491516053808,18.7198592314163,44.3));
#71044=CARTESIAN_POINT('Ctrl Pts',(29.5037286001147,18.7184276719127,44.3));
#71045=CARTESIAN_POINT('Ctrl Pts',(29.517902907794,18.7167661539658,44.3));
#71046=CARTESIAN_POINT('Ctrl Pts',(29.5320955225091,18.7152276354238,44.3));
#71047=CARTESIAN_POINT('Ctrl Pts',(29.5463045291254,18.7138126137682,44.3));
#71048=CARTESIAN_POINT('Ctrl Pts',(29.5608591182573,18.7123631768464,44.3));
#71049=CARTESIAN_POINT('Ctrl Pts',(29.5754224087203,18.7110441895149,44.3));
#71050=CARTESIAN_POINT('Ctrl Pts',(29.5899879093375,18.7098560519243,44.3));
#71051=CARTESIAN_POINT('Ctrl Pts',(29.672786509973,18.7031020012086,44.3));
#71052=CARTESIAN_POINT('Ctrl Pts',(29.7557033576394,18.7005674053427,44.3));
#71053=CARTESIAN_POINT('Ctrl Pts',(29.8383717954221,18.7022736216555,44.3));
#71054=CARTESIAN_POINT('Ctrl Pts',(29.9192747629738,18.7039433999492,44.3));
#71055=CARTESIAN_POINT('Ctrl Pts',(29.9999407278769,18.7096750302976,44.3));
#71056=CARTESIAN_POINT('Ctrl Pts',(30.0800151893485,18.7195360765726,44.3));
#71057=CARTESIAN_POINT('Ctrl Pts',(30.1583858483894,18.7291873022093,44.3));
#71058=CARTESIAN_POINT('Ctrl Pts',(30.2361906578794,18.7427942913507,44.3));
#71059=CARTESIAN_POINT('Ctrl Pts',(30.3130747015946,18.760463173912,44.3));
#71060=CARTESIAN_POINT('Ctrl Pts',(30.3469544935414,18.7682491596144,44.3));
#71061=CARTESIAN_POINT('Ctrl Pts',(30.380655124679,18.776824439382,44.3));
#71062=CARTESIAN_POINT('Ctrl Pts',(30.4141442282618,18.7862006657701,44.3));
#71063=CARTESIAN_POINT('Ctrl Pts',(30.427620745083,18.7899737996889,44.3));
#71064=CARTESIAN_POINT('Ctrl Pts',(30.4410643696255,18.7938771640174,44.3));
#71065=CARTESIAN_POINT('Ctrl Pts',(30.4544553355144,18.7979060130015,44.3));
#71066=CARTESIAN_POINT('Ctrl Pts',(30.5292896225546,18.820420896828,44.3));
#71067=CARTESIAN_POINT('Ctrl Pts',(30.6026067169376,18.8468848998915,44.3));
#71068=CARTESIAN_POINT('Ctrl Pts',(30.6740806949432,18.8773535792392,44.3));
#71069=CARTESIAN_POINT('Ctrl Pts',(30.7023424983408,18.8894013181442,44.3));
#71070=CARTESIAN_POINT('Ctrl Pts',(30.730315878025,18.9020757018371,44.3));
#71071=CARTESIAN_POINT('Ctrl Pts',(30.7579795342966,18.9153821277604,44.3));
#71072=CARTESIAN_POINT('Ctrl Pts',(30.8296349957725,18.9498489415745,44.3));
#71073=CARTESIAN_POINT('Ctrl Pts',(30.8992151722481,18.9885538331303,44.3));
#71074=CARTESIAN_POINT('Ctrl Pts',(30.9664943099138,19.0311976270323,44.3));
#71075=CARTESIAN_POINT('Ctrl Pts',(31.031817757109,19.0726018381415,44.3));
#71076=CARTESIAN_POINT('Ctrl Pts',(31.0949723123221,19.1177202684067,44.3));
#71077=CARTESIAN_POINT('Ctrl Pts',(31.1557122805128,19.1663052414586,44.3));
#71078=CARTESIAN_POINT('Ctrl Pts',(31.1699003354004,19.1776540499106,44.3));
#71079=CARTESIAN_POINT('Ctrl Pts',(31.1839610180611,19.1891960925353,44.3));
#71080=CARTESIAN_POINT('Ctrl Pts',(31.1978653013046,19.2009063118251,44.3));
#71081=CARTESIAN_POINT('Ctrl Pts',(31.2573151687879,19.2509751267932,44.3));
#71082=CARTESIAN_POINT('Ctrl Pts',(31.3139848039203,19.3041725875463,44.3));
#71083=CARTESIAN_POINT('Ctrl Pts',(31.3676843811118,19.3601986999375,44.3));
#71084=CARTESIAN_POINT('Ctrl Pts',(31.4211957053017,19.4160284032622,44.3));
#71085=CARTESIAN_POINT('Ctrl Pts',(31.471758236847,19.4746678992268,44.3));
#71086=CARTESIAN_POINT('Ctrl Pts',(31.5191413084655,19.5358480817005,44.3));
#71087=CARTESIAN_POINT('Ctrl Pts',(31.5661269832405,19.5965151524116,44.3));
#71088=CARTESIAN_POINT('Ctrl Pts',(31.6099867130907,19.6596813525084,44.3));
#71089=CARTESIAN_POINT('Ctrl Pts',(31.6504468767739,19.7250980707919,44.3));
#71090=CARTESIAN_POINT('Ctrl Pts',(31.665885468332,19.7500594625094,44.3));
#71091=CARTESIAN_POINT('Ctrl Pts',(31.6808285446354,19.7753486039029,44.3));
#71092=CARTESIAN_POINT('Ctrl Pts',(31.6952588227872,19.8009518122182,44.3));
#71093=CARTESIAN_POINT('Ctrl Pts',(31.7013523222933,19.8117633250375,44.3));
#71094=CARTESIAN_POINT('Ctrl Pts',(31.7073543860773,19.8226310444429,44.3));
#71095=CARTESIAN_POINT('Ctrl Pts',(31.7132568737193,19.8335409018929,44.3));
#71096=CARTESIAN_POINT('Ctrl Pts',(31.7489430038996,19.8995013268572,44.3));
#71097=CARTESIAN_POINT('Ctrl Pts',(31.7810594676341,19.9671166497836,44.3));
#71098=CARTESIAN_POINT('Ctrl Pts',(31.8094014527161,20.0361358411783,44.3));
#71099=CARTESIAN_POINT('Ctrl Pts',(31.8372817751033,20.1040307787216,44.3));
#71100=CARTESIAN_POINT('Ctrl Pts',(31.8615098401969,20.1732850438433,44.3));
#71101=CARTESIAN_POINT('Ctrl Pts',(31.8818416939127,20.243668178961,44.3));
#71102=CARTESIAN_POINT('Ctrl Pts',(31.9015211854442,20.3117930204471,44.3));
#71103=CARTESIAN_POINT('Ctrl Pts',(31.9175505455949,20.3809761123184,44.3));
#71104=CARTESIAN_POINT('Ctrl Pts',(31.9296601688495,20.4510057916981,44.3));
#71105=CARTESIAN_POINT('Ctrl Pts',(31.9357076145878,20.4859780346176,44.3));
#71106=CARTESIAN_POINT('Ctrl Pts',(31.9407767358369,20.5211613068948,44.3));
#71107=CARTESIAN_POINT('Ctrl Pts',(31.9448291324621,20.5565282331122,44.3));
#71108=CARTESIAN_POINT('Ctrl Pts',(29.1264558385116,22.7892573294893,35.7842713731578));
#71109=CARTESIAN_POINT('Ctrl Pts',(28.5312306963436,22.4986588565127,35.826627728308));
#71110=CARTESIAN_POINT('Ctrl Pts',(27.6641321376413,21.2811530742106,35.9113404386083));
#71111=CARTESIAN_POINT('Ctrl Pts',(28.498480258771,19.1855515705045,36.0384095040588));
#71112=CARTESIAN_POINT('Ctrl Pts',(30.7107013872026,18.7565854023573,36.1654785695093));
#71113=CARTESIAN_POINT('Ctrl Pts',(32.2706914918877,20.3804476459957,36.2925476349598));
#71114=CARTESIAN_POINT('Ctrl Pts',(31.751265422737,22.5729299246014,36.4196167004103));
#71115=CARTESIAN_POINT('Ctrl Pts',(29.6273304332075,23.3240196151812,36.5466857658608));
#71116=CARTESIAN_POINT('Ctrl Pts',(27.8449208232258,21.9465121681938,36.6737548313113));
#71117=CARTESIAN_POINT('Ctrl Pts',(28.0365506611368,19.7018375639597,36.8008238967618));
#71118=CARTESIAN_POINT('Ctrl Pts',(30.0267931275245,18.6463840233588,36.9278929622123));
#71119=CARTESIAN_POINT('Ctrl Pts',(31.992473836526,19.746876227632,37.0549620276628));
#71120=CARTESIAN_POINT('Ctrl Pts',(32.1330009690077,21.9952822113242,37.1820310931133));
#71121=CARTESIAN_POINT('Ctrl Pts',(30.3196338647694,23.3319730130521,37.3091001585638));
#71122=CARTESIAN_POINT('Ctrl Pts',(28.2134753232459,22.5325142575818,37.4361692240143));
#71123=CARTESIAN_POINT('Ctrl Pts',(27.7438231346904,20.3292267213969,37.5632382894648));
#71124=CARTESIAN_POINT('Ctrl Pts',(29.340893789684,18.7403876454215,37.6903073549153));
#71125=CARTESIAN_POINT('Ctrl Pts',(31.5417242248616,19.2214173377329,37.8173764203657));
#71126=CARTESIAN_POINT('Ctrl Pts',(32.3302914952649,21.3316796671695,37.9444454858163));
#71127=CARTESIAN_POINT('Ctrl Pts',(30.984245307654,23.1381138461734,38.0715145512667));
#71128=CARTESIAN_POINT('Ctrl Pts',(28.7366024171385,22.9859749016701,38.1985836167173));
#71129=CARTESIAN_POINT('Ctrl Pts',(27.6462676828056,21.0146263453323,38.3256526821677));
#71130=CARTESIAN_POINT('Ctrl Pts',(28.7120188055034,19.0298796558089,38.4527217476182));
#71131=CARTESIAN_POINT('Ctrl Pts',(30.9575973860193,18.8498193123516,38.5797908130687));
#71132=CARTESIAN_POINT('Ctrl Pts',(32.3259894860523,20.6393857303374,38.7068598785192));
#71133=CARTESIAN_POINT('Ctrl Pts',(31.563708960251,22.7592850894379,38.8339289439697));
#71134=CARTESIAN_POINT('Ctrl Pts',(29.3690264853313,23.2676291945582,38.9609980094202));
#71135=CARTESIAN_POINT('Ctrl Pts',(27.752333722787,21.69876036383,39.0880670748707));
#71136=CARTESIAN_POINT('Ctrl Pts',(28.1945672948102,19.4898071359688,39.2151361403212));
#71137=CARTESIAN_POINT('Ctrl Pts',(30.2906286522575,18.6642335891045,39.3422052057717));
#71138=CARTESIAN_POINT('Ctrl Pts',(32.1204658857473,19.9782886087098,39.4692742712222));
#71139=CARTESIAN_POINT('Ctrl Pts',(32.0078959666568,22.2282603660349,39.5963433366727));
#71140=CARTESIAN_POINT('Ctrl Pts',(30.0560361474382,23.3531106412359,39.7234124021232));
#71141=CARTESIAN_POINT('Ctrl Pts',(28.0528456209794,22.32244454098,39.8504814675737));
#71142=CARTESIAN_POINT('Ctrl Pts',(27.8333039701667,20.0803815715138,39.9775505330242));
#71143=CARTESIAN_POINT('Ctrl Pts',(29.5985176007606,18.6807152777617,40.1046195984747));
#71144=CARTESIAN_POINT('Ctrl Pts',(31.7315005452354,19.4055798541298,40.2316886639252));
#71145=CARTESIAN_POINT('Ctrl Pts',(32.2783796686896,21.5909787009862,40.3587577293757));
#71146=CARTESIAN_POINT('Ctrl Pts',(30.7381981162433,23.2350242237756,40.4858267948262));
#71147=CARTESIAN_POINT('Ctrl Pts',(28.5218060618448,22.8317238931978,40.6128958602767));
#71148=CARTESIAN_POINT('Ctrl Pts',(27.6594817609504,20.7505122999901,40.7399649257271));
#71149=CARTESIAN_POINT('Ctrl Pts',(28.9411388364606,18.8978385466649,40.8670339911777));
#71150=CARTESIAN_POINT('Ctrl Pts',(31.1927428992058,18.9708045643224,40.9941030566281));
#71151=CARTESIAN_POINT('Ctrl Pts',(32.351760491343,20.9025714026366,41.1211721220787));
#71152=CARTESIAN_POINT('Ctrl Pts',(31.3564984833804,22.9235856110073,41.2482411875291));
#71153=CARTESIAN_POINT('Ctrl Pts',(29.1186452257674,23.1825406073307,41.3753102529796));
#71154=CARTESIAN_POINT('Ctrl Pts',(27.6881380449832,21.4422262364366,41.5023793184301));
#71155=CARTESIAN_POINT('Ctrl Pts',(28.3753622714282,19.2968200391992,41.6294483838806));
#71156=CARTESIAN_POINT('Ctrl Pts',(30.5508009281952,18.711575194925,41.7565174493311));
#71157=CARTESIAN_POINT('Ctrl Pts',(32.2216902586076,20.2225926696691,41.8835865147816));
#71158=CARTESIAN_POINT('Ctrl Pts',(31.8574480007175,22.4457373791487,42.0106555802321));
#71159=CARTESIAN_POINT('Ctrl Pts',(29.7917305188365,23.3445455162426,42.1377246456825));
#71160=CARTESIAN_POINT('Ctrl Pts',(27.9167937061589,22.0956830788796,42.2647937111331));
#71161=CARTESIAN_POINT('Ctrl Pts',(27.9501334154122,19.8431439264837,42.3918627765836));
#71162=CARTESIAN_POINT('Ctrl Pts',(29.8612088710918,18.6503174977494,42.5189318420341));
#71163=CARTESIAN_POINT('Ctrl Pts',(31.8994218278085,19.6098679593695,42.6460009074846));
#71164=CARTESIAN_POINT('Ctrl Pts',(32.1977085324443,21.8428173868236,42.7730699729351));
#71165=CARTESIAN_POINT('Ctrl Pts',(30.4828351379126,23.303725253489,42.9001390383856));
#71166=CARTESIAN_POINT('Ctrl Pts',(28.3256639434058,22.6543487986828,43.0272081038361));
#71167=CARTESIAN_POINT('Ctrl Pts',(27.7022464386769,20.4895544998625,43.1542771692865));
#71168=CARTESIAN_POINT('Ctrl Pts',(29.1836082129126,18.7923171725529,43.281346234737));
#71169=CARTESIAN_POINT('Ctrl Pts',(31.4128651827133,19.1174316697178,43.4084153001876));
#71170=CARTESIAN_POINT('Ctrl Pts',(32.3477828809716,21.166929091464,43.535484365638));
#71171=CARTESIAN_POINT('Ctrl Pts',(31.1322944104254,23.0637220008276,43.6625534310885));
#71172=CARTESIAN_POINT('Ctrl Pts',(28.8791307244882,23.0696707559168,43.7896224965391));
#71173=CARTESIAN_POINT('Ctrl Pts',(27.6536416772529,21.1805772409905,43.9166915619895));
#71174=CARTESIAN_POINT('Ctrl Pts',(28.5756138853417,19.124391076752,44.0437606274401));
#71175=CARTESIAN_POINT('Ctrl Pts',(30.8065507606822,18.7896800661229,44.1708475287837));
#71176=CARTESIAN_POINT('Ctrl Pts',(31.794437854879,19.912011627325,44.2555780749772));
#71177=CARTESIAN_POINT('Ctrl Pts',(31.9414666005005,20.5581532204799,44.2979522660205));
#71178=CARTESIAN_POINT('Ctrl Pts',(29.0588050875662,22.9278245677711,35.8732985293678));
#71179=CARTESIAN_POINT('Ctrl Pts',(28.4174833315984,22.6147209876834,35.915654884518));
#71180=CARTESIAN_POINT('Ctrl Pts',(27.48323319519,21.3029266918931,36.0003675948183));
#71181=CARTESIAN_POINT('Ctrl Pts',(28.3821965692544,19.0450334327634,36.1274366602689));
#71182=CARTESIAN_POINT('Ctrl Pts',(30.7657409429135,18.5828464102108,36.2545057257193));
#71183=CARTESIAN_POINT('Ctrl Pts',(32.4465429157353,20.3324670356887,36.3815747911698));
#71184=CARTESIAN_POINT('Ctrl Pts',(31.8868904159268,22.6947439041059,36.5086438566203));
#71185=CARTESIAN_POINT('Ctrl Pts',(29.5984694125981,23.5040009820202,36.6357129220708));
#71186=CARTESIAN_POINT('Ctrl Pts',(27.6780228790999,22.0198138531919,36.7627819875213));
#71187=CARTESIAN_POINT('Ctrl Pts',(27.8844932974987,19.6013026768652,36.8898510529718));
#71188=CARTESIAN_POINT('Ctrl Pts',(30.0288680943975,18.4641105960079,37.0169201184223));
#71189=CARTESIAN_POINT('Ctrl Pts',(32.1467789732582,19.6498293146473,37.1439891838728));
#71190=CARTESIAN_POINT('Ctrl Pts',(32.2981890884896,22.0723608433696,37.2710582493233));
#71191=CARTESIAN_POINT('Ctrl Pts',(30.3443875886594,23.5125703228076,37.3981273147737));
#71192=CARTESIAN_POINT('Ctrl Pts',(28.075119712513,22.6511982863129,37.5251963802243));
#71193=CARTESIAN_POINT('Ctrl Pts',(27.5690957815319,20.2772793579868,37.6522654456748));
#71194=CARTESIAN_POINT('Ctrl Pts',(29.2898499706689,18.5653942342443,37.7793345111252));
#71195=CARTESIAN_POINT('Ctrl Pts',(31.661121510266,19.0836767883417,37.9064035765758));
#71196=CARTESIAN_POINT('Ctrl Pts',(32.5107585815627,21.3573662661379,38.0334726420262));
#71197=CARTESIAN_POINT('Ctrl Pts',(31.0604691977706,23.3036979272963,38.1605417074767));
#71198=CARTESIAN_POINT('Ctrl Pts',(28.6387598592103,23.1397767349144,38.2876107729272));
#71199=CARTESIAN_POINT('Ctrl Pts',(27.4639852455773,21.0157590679684,38.4146798383777));
#71200=CARTESIAN_POINT('Ctrl Pts',(28.6122723944429,18.8773056628579,38.5417489038283));
#71201=CARTESIAN_POINT('Ctrl Pts',(31.0317575545873,18.6833007268003,38.6688179692787));
#71202=CARTESIAN_POINT('Ctrl Pts',(32.5061234075639,20.6114583201161,38.7958870347292));
#71203=CARTESIAN_POINT('Ctrl Pts',(31.6848088314249,22.8955311576673,38.9229561001797));
#71204=CARTESIAN_POINT('Ctrl Pts',(29.3201613746983,23.4432434618624,39.0500251656302));
#71205=CARTESIAN_POINT('Ctrl Pts',(27.5782654635829,21.7528751589692,39.1770942310807));
#71206=CARTESIAN_POINT('Ctrl Pts',(28.0547473707901,19.3728517651606,39.3041632965312));
#71207=CARTESIAN_POINT('Ctrl Pts',(30.3131360965726,18.4833425034599,39.4312323619817));
#71208=CARTESIAN_POINT('Ctrl Pts',(32.2846832382856,19.8991631953448,39.5583014274322));
#71209=CARTESIAN_POINT('Ctrl Pts',(32.1633954547801,22.3233817574676,39.6853704928827));
#71210=CARTESIAN_POINT('Ctrl Pts',(30.0603758106417,23.5353449333936,39.8124395583332));
#71211=CARTESIAN_POINT('Ctrl Pts',(27.9020502041535,22.4248599313233,39.9395086237837));
#71212=CARTESIAN_POINT('Ctrl Pts',(27.6655063705137,20.0091626451984,40.0665776892342));
#71213=CARTESIAN_POINT('Ctrl Pts',(29.5674251992573,18.501100599955,40.1936467546846));
#71214=CARTESIAN_POINT('Ctrl Pts',(31.865594867322,19.2821015860055,40.3207158201352));
#71215=CARTESIAN_POINT('Ctrl Pts',(32.4548264956743,21.6367464534102,40.4477848855856));
#71216=CARTESIAN_POINT('Ctrl Pts',(30.7953671285406,23.408113431838,40.5748539510361));
#71217=CARTESIAN_POINT('Ctrl Pts',(28.4073288157389,22.9735799118887,40.7019230164867));
#71218=CARTESIAN_POINT('Ctrl Pts',(27.478222674743,20.7311909754351,40.8289920819371));
#71219=CARTESIAN_POINT('Ctrl Pts',(28.8591363962653,18.7350387625254,40.9560611473876));
#71220=CARTESIAN_POINT('Ctrl Pts',(31.2851136760633,18.8136555601958,41.0831302128381));
#71221=CARTESIAN_POINT('Ctrl Pts',(32.5338902224971,20.8950261426877,41.2101992782886));
#71222=CARTESIAN_POINT('Ctrl Pts',(31.4615511471183,23.0725557682465,41.3372683437391));
#71223=CARTESIAN_POINT('Ctrl Pts',(29.0503895897562,23.3515652743872,41.4643374091896));
#71224=CARTESIAN_POINT('Ctrl Pts',(27.5090982159349,21.4764740035234,41.5914064746401));
#71225=CARTESIAN_POINT('Ctrl Pts',(28.2495438329364,19.1649189763531,41.7184755400906));
#71226=CARTESIAN_POINT('Ctrl Pts',(30.5934571533256,18.5343504324337,41.8455446055411));
#71227=CARTESIAN_POINT('Ctrl Pts',(32.3937468311188,20.162387139135,41.9726136709916));
#71228=CARTESIAN_POINT('Ctrl Pts',(32.0012961971001,22.5577010596139,42.0996827364421));
#71229=CARTESIAN_POINT('Ctrl Pts',(29.7756012978757,23.5261164908906,42.2267518018926));
#71230=CARTESIAN_POINT('Ctrl Pts',(27.7554618853241,22.1805371553559,42.3538208673431));
#71231=CARTESIAN_POINT('Ctrl Pts',(27.7913835549026,19.7535523688276,42.4808899327936));
#71232=CARTESIAN_POINT('Ctrl Pts',(29.8504603313968,18.4683486943752,42.607958998244));
#71233=CARTESIAN_POINT('Ctrl Pts',(32.0465206451074,19.5022105785432,42.7350280636946));
#71234=CARTESIAN_POINT('Ctrl Pts',(32.3679078642396,21.9080885335408,42.862097129145));
#71235=CARTESIAN_POINT('Ctrl Pts',(30.5202278206214,23.482134943853,42.9891661945956));
#71236=CARTESIAN_POINT('Ctrl Pts',(28.1959966677748,22.782468181183,43.116235260046));
#71237=CARTESIAN_POINT('Ctrl Pts',(27.5242992200198,20.4500235603596,43.2433043254965));
#71238=CARTESIAN_POINT('Ctrl Pts',(29.1203835702476,18.6213453914907,43.3703733909471));
#71239=CARTESIAN_POINT('Ctrl Pts',(31.5222831089145,18.9716380546215,43.4974424563975));
#71240=CARTESIAN_POINT('Ctrl Pts',(32.5296045700822,21.1798567474316,43.624511521848));
#71241=CARTESIAN_POINT('Ctrl Pts',(31.2199838147322,23.2235448801435,43.7515805872985));
#71242=CARTESIAN_POINT('Ctrl Pts',(28.7923261282892,23.2299543306006,43.878649652749));
#71243=CARTESIAN_POINT('Ctrl Pts',(27.4719303116244,21.1945618642016,44.0057187181995));
#71244=CARTESIAN_POINT('Ctrl Pts',(28.4653037321279,18.9791364259494,44.1327877836501));
#71245=CARTESIAN_POINT('Ctrl Pts',(30.869013274933,18.6185040569998,44.2598746849936));
#71246=CARTESIAN_POINT('Ctrl Pts',(31.9334062937505,19.8277534596486,44.3446052311871));
#71247=CARTESIAN_POINT('Ctrl Pts',(32.0918215330268,20.5239348400532,44.3869794222305));
#71248=CARTESIAN_POINT('Ctrl Pts',(28.9911543366207,23.0663918060528,35.9623256855777));
#71249=CARTESIAN_POINT('Ctrl Pts',(28.303735966853,22.7307831188541,36.0046820407279));
#71250=CARTESIAN_POINT('Ctrl Pts',(27.3023342527386,21.3247003095755,36.0893947510282));
#71251=CARTESIAN_POINT('Ctrl Pts',(28.2659128797378,18.9045152950221,36.2164638164787));
#71252=CARTESIAN_POINT('Ctrl Pts',(30.8207804986244,18.4091074180643,36.3435328819292));
#71253=CARTESIAN_POINT('Ctrl Pts',(32.622394339583,20.2844864253816,36.4706019473797));
#71254=CARTESIAN_POINT('Ctrl Pts',(32.0225154091167,22.8165578836103,36.5976710128302));
#71255=CARTESIAN_POINT('Ctrl Pts',(29.5696083919886,23.6839823488592,36.7247400782807));
#71256=CARTESIAN_POINT('Ctrl Pts',(27.511124934974,22.09311553819,36.8518091437312));
#71257=CARTESIAN_POINT('Ctrl Pts',(27.7324359338606,19.5007677897707,36.9788782091817));
#71258=CARTESIAN_POINT('Ctrl Pts',(30.0309430612705,18.2818371686568,37.1059472746322));
#71259=CARTESIAN_POINT('Ctrl Pts',(32.3010841099903,19.5527824016626,37.2330163400826));
#71260=CARTESIAN_POINT('Ctrl Pts',(32.4633772079716,22.1494394754149,37.3600854055332));
#71261=CARTESIAN_POINT('Ctrl Pts',(30.3691413125495,23.693167632563,37.4871544709836));
#71262=CARTESIAN_POINT('Ctrl Pts',(27.93676410178,22.769882315044,37.6142235364341));
#71263=CARTESIAN_POINT('Ctrl Pts',(27.3943684283736,20.2253319945767,37.7412926018847));
#71264=CARTESIAN_POINT('Ctrl Pts',(29.2388061516538,18.3904008230671,37.8683616673351));
#71265=CARTESIAN_POINT('Ctrl Pts',(31.7805187956705,18.9459362389506,37.9954307327856));
#71266=CARTESIAN_POINT('Ctrl Pts',(32.6912256678607,21.3830528651062,38.1224997982362));
#71267=CARTESIAN_POINT('Ctrl Pts',(31.1366930878873,23.4692820084193,38.2495688636866));
#71268=CARTESIAN_POINT('Ctrl Pts',(28.5409173012823,23.2935785681586,38.3766379291371));
#71269=CARTESIAN_POINT('Ctrl Pts',(27.2817028083489,21.0168917906046,38.5037069945876));
#71270=CARTESIAN_POINT('Ctrl Pts',(28.5125259833826,18.7247316699069,38.6307760600381));
#71271=CARTESIAN_POINT('Ctrl Pts',(31.1059177231553,18.5167821412488,38.7578451254886));
#71272=CARTESIAN_POINT('Ctrl Pts',(32.6862573290757,20.5835309098948,38.8849141909391));
#71273=CARTESIAN_POINT('Ctrl Pts',(31.8059087025989,23.0317772258968,39.0119832563896));
#71274=CARTESIAN_POINT('Ctrl Pts',(29.2712962640653,23.6188577291665,39.1390523218401));
#71275=CARTESIAN_POINT('Ctrl Pts',(27.4041972043789,21.8069899541084,39.2661213872906));
#71276=CARTESIAN_POINT('Ctrl Pts',(27.91492744677,19.2558963943526,39.3931904527411));
#71277=CARTESIAN_POINT('Ctrl Pts',(30.3356435408877,18.3024514178153,39.5202595181916));
#71278=CARTESIAN_POINT('Ctrl Pts',(32.4489005908239,19.82003778198,39.6473285836421));
#71279=CARTESIAN_POINT('Ctrl Pts',(32.3188949429034,22.4185031489004,39.7743976490926));
#71280=CARTESIAN_POINT('Ctrl Pts',(30.0647154738453,23.7175792255511,39.901466714543));
#71281=CARTESIAN_POINT('Ctrl Pts',(27.7512547873278,22.5272753216666,40.0285357799936));
#71282=CARTESIAN_POINT('Ctrl Pts',(27.4977087708607,19.9379437188829,40.155604845444));
#71283=CARTESIAN_POINT('Ctrl Pts',(29.5363327977539,18.3214859221484,40.2826739108945));
#71284=CARTESIAN_POINT('Ctrl Pts',(31.9996891894087,19.1586233178813,40.4097429763451));
#71285=CARTESIAN_POINT('Ctrl Pts',(32.631273322659,21.6825142058343,40.5368120417955));
#71286=CARTESIAN_POINT('Ctrl Pts',(30.8525361408378,23.5812026399005,40.6638811072461));
#71287=CARTESIAN_POINT('Ctrl Pts',(28.2928515696329,23.1154359305797,40.7909501726965));
#71288=CARTESIAN_POINT('Ctrl Pts',(27.2969635885356,20.7118696508799,40.918019238147));
#71289=CARTESIAN_POINT('Ctrl Pts',(28.7771339560702,18.5722389783859,41.0450883035975));
#71290=CARTESIAN_POINT('Ctrl Pts',(31.3774844529208,18.656506556069,41.172157369048));
#71291=CARTESIAN_POINT('Ctrl Pts',(32.7160199536512,20.887480882739,41.2992264344985));
#71292=CARTESIAN_POINT('Ctrl Pts',(31.5666038108562,23.2215259254859,41.426295499949));
#71293=CARTESIAN_POINT('Ctrl Pts',(28.9821339537452,23.5205899414438,41.5533645653995));
#71294=CARTESIAN_POINT('Ctrl Pts',(27.3300583868866,21.5107217706103,41.68043363085));
#71295=CARTESIAN_POINT('Ctrl Pts',(28.1237253944445,19.0330179135071,41.8075026963005));
#71296=CARTESIAN_POINT('Ctrl Pts',(30.636113378456,18.3571256699425,41.934571761751));
#71297=CARTESIAN_POINT('Ctrl Pts',(32.5658034036301,20.102181608601,42.0616408272015));
#71298=CARTESIAN_POINT('Ctrl Pts',(32.1451443934826,22.6696647400793,42.188709892652));
#71299=CARTESIAN_POINT('Ctrl Pts',(29.7594720769148,23.7076874655386,42.3157789581025));
#71300=CARTESIAN_POINT('Ctrl Pts',(27.5941300644893,22.2653912318322,42.442848023553));
#71301=CARTESIAN_POINT('Ctrl Pts',(27.6326336943931,19.6639608111716,42.5699170890035));
#71302=CARTESIAN_POINT('Ctrl Pts',(29.8397117917017,18.286379891001,42.6969861544539));
#71303=CARTESIAN_POINT('Ctrl Pts',(32.1936194624063,19.3945531977169,42.8240552199045));
#71304=CARTESIAN_POINT('Ctrl Pts',(32.5381071960349,21.973359680258,42.9511242853549));
#71305=CARTESIAN_POINT('Ctrl Pts',(30.5576205033301,23.6605446342171,43.0781933508055));
#71306=CARTESIAN_POINT('Ctrl Pts',(28.0663293921438,22.9105875636831,43.2052624162559));
#71307=CARTESIAN_POINT('Ctrl Pts',(27.3463520013628,20.4104926208566,43.3323314817064));
#71308=CARTESIAN_POINT('Ctrl Pts',(29.0571589275827,18.4503736104286,43.4594005471569));
#71309=CARTESIAN_POINT('Ctrl Pts',(31.6317010351155,18.8258444395252,43.5864696126075));
#71310=CARTESIAN_POINT('Ctrl Pts',(32.7114262591928,21.1927844033991,43.7135386780579));
#71311=CARTESIAN_POINT('Ctrl Pts',(31.3076732190389,23.3833677594592,43.8406077435085));
#71312=CARTESIAN_POINT('Ctrl Pts',(28.7055215320902,23.3902379052844,43.9676768089589));
#71313=CARTESIAN_POINT('Ctrl Pts',(27.2902189459959,21.2085464874127,44.0947458744094));
#71314=CARTESIAN_POINT('Ctrl Pts',(28.354993578914,18.8338817751468,44.2218149398599));
#71315=CARTESIAN_POINT('Ctrl Pts',(30.9314757891839,18.4473280478767,44.3489018412036));
#71316=CARTESIAN_POINT('Ctrl Pts',(32.0723747326222,19.7434952919723,44.4336323873971));
#71317=CARTESIAN_POINT('Ctrl Pts',(32.242176465553,20.4897164596265,44.4760065784404));
#71318=CARTESIAN_POINT('Ctrl Pts',(28.9235035856754,23.2049590443345,36.0513528417877));
#71319=CARTESIAN_POINT('Ctrl Pts',(28.1899886021078,22.8468452500248,36.0937091969379));
#71320=CARTESIAN_POINT('Ctrl Pts',(27.1214353102873,21.3464739272579,36.1784219072382));
#71321=CARTESIAN_POINT('Ctrl Pts',(28.1496291902213,18.7639971572809,36.3054909726887));
#71322=CARTESIAN_POINT('Ctrl Pts',(30.8758200543354,18.2353684259178,36.4325600381392));
#71323=CARTESIAN_POINT('Ctrl Pts',(32.7982457634307,20.2365058150745,36.5596291035897));
#71324=CARTESIAN_POINT('Ctrl Pts',(32.1581404023066,22.9383718631148,36.6866981690402));
#71325=CARTESIAN_POINT('Ctrl Pts',(29.5407473713791,23.8639637156981,36.8137672344907));
#71326=CARTESIAN_POINT('Ctrl Pts',(27.3442269908482,22.1664172231879,36.9408362999411));
#71327=CARTESIAN_POINT('Ctrl Pts',(27.5803785702225,19.4002329026764,37.0679053653917));
#71328=CARTESIAN_POINT('Ctrl Pts',(30.0330180281436,18.0995637413059,37.1949744308422));
#71329=CARTESIAN_POINT('Ctrl Pts',(32.4553892467225,19.455735488678,37.3220434962926));
#71330=CARTESIAN_POINT('Ctrl Pts',(32.6285653274533,22.2265181074601,37.4491125617432));
#71331=CARTESIAN_POINT('Ctrl Pts',(30.3938950364395,23.8737649423185,37.5761816271937));
#71332=CARTESIAN_POINT('Ctrl Pts',(27.7984084910471,22.8885663437751,37.7032506926441));
#71333=CARTESIAN_POINT('Ctrl Pts',(27.2196410752151,20.1733846311666,37.8303197580947));
#71334=CARTESIAN_POINT('Ctrl Pts',(29.1877623326388,18.21540741189,37.9573888235451));
#71335=CARTESIAN_POINT('Ctrl Pts',(31.8999160810749,18.8081956895594,38.0844578889956));
#71336=CARTESIAN_POINT('Ctrl Pts',(32.8716927541586,21.4087394640746,38.2115269544461));
#71337=CARTESIAN_POINT('Ctrl Pts',(31.2129169780038,23.6348660895422,38.3385960198966));
#71338=CARTESIAN_POINT('Ctrl Pts',(28.4430747433541,23.4473804014028,38.4656650853471));
#71339=CARTESIAN_POINT('Ctrl Pts',(27.0994203711206,21.0180245132406,38.5927341507976));
#71340=CARTESIAN_POINT('Ctrl Pts',(28.4127795723222,18.5721576769558,38.7198032162481));
#71341=CARTESIAN_POINT('Ctrl Pts',(31.1800778917232,18.3502635556974,38.8468722816986));
#71342=CARTESIAN_POINT('Ctrl Pts',(32.8663912505875,20.5556034996735,38.9739413471491));
#71343=CARTESIAN_POINT('Ctrl Pts',(31.9270085737729,23.1680232941261,39.1010104125996));
#71344=CARTESIAN_POINT('Ctrl Pts',(29.2224311534323,23.7944719964707,39.2280794780501));
#71345=CARTESIAN_POINT('Ctrl Pts',(27.2301289451749,21.8611047492476,39.3551485435006));
#71346=CARTESIAN_POINT('Ctrl Pts',(27.77510752275,19.1389410235446,39.4822176089511));
#71347=CARTESIAN_POINT('Ctrl Pts',(30.3581509852028,18.1215603321707,39.6092866744015));
#71348=CARTESIAN_POINT('Ctrl Pts',(32.6131179433622,19.740912368615,39.7363557398521));
#71349=CARTESIAN_POINT('Ctrl Pts',(32.4743944310268,22.5136245403331,39.8634248053025));
#71350=CARTESIAN_POINT('Ctrl Pts',(30.0690551370489,23.8998135177087,39.9904938707531));
#71351=CARTESIAN_POINT('Ctrl Pts',(27.6004593705019,22.6296907120099,40.1175629362035));
#71352=CARTESIAN_POINT('Ctrl Pts',(27.3299111712076,19.8667247925675,40.2446320016541));
#71353=CARTESIAN_POINT('Ctrl Pts',(29.5052403962506,18.1418712443417,40.3717010671045));
#71354=CARTESIAN_POINT('Ctrl Pts',(32.1337835114953,19.0351450497571,40.4987701325551));
#71355=CARTESIAN_POINT('Ctrl Pts',(32.8077201496436,21.7282819582582,40.6258391980055));
#71356=CARTESIAN_POINT('Ctrl Pts',(30.9097051531351,23.7542918479628,40.7529082634561));
#71357=CARTESIAN_POINT('Ctrl Pts',(28.1783743235269,23.2572919492706,40.8799773289065));
#71358=CARTESIAN_POINT('Ctrl Pts',(27.1157045023283,20.6925483263249,41.0070463943571));
#71359=CARTESIAN_POINT('Ctrl Pts',(28.6951315158749,18.4094391942464,41.1341154598075));
#71360=CARTESIAN_POINT('Ctrl Pts',(31.4698552297785,18.4993575519423,41.261184525258));
#71361=CARTESIAN_POINT('Ctrl Pts',(32.8981496848052,20.8799356227902,41.3882535907085));
#71362=CARTESIAN_POINT('Ctrl Pts',(31.6716564745941,23.3704960827252,41.515322656159));
#71363=CARTESIAN_POINT('Ctrl Pts',(28.9138783177342,23.6896146085003,41.6423917216095));
#71364=CARTESIAN_POINT('Ctrl Pts',(27.1510185578384,21.5449695376971,41.76946078706));
#71365=CARTESIAN_POINT('Ctrl Pts',(27.9979069559526,18.9011168506609,41.8965298525105));
#71366=CARTESIAN_POINT('Ctrl Pts',(30.6787696035865,18.1799009074512,42.023598917961));
#71367=CARTESIAN_POINT('Ctrl Pts',(32.7378599761413,20.0419760780668,42.1506679834115));
#71368=CARTESIAN_POINT('Ctrl Pts',(32.2889925898651,22.7816284205446,42.277737048862));
#71369=CARTESIAN_POINT('Ctrl Pts',(29.743342855954,23.8892584401866,42.4048061143125));
#71370=CARTESIAN_POINT('Ctrl Pts',(27.4327982436545,22.3502453083086,42.531875179763));
#71371=CARTESIAN_POINT('Ctrl Pts',(27.4738838338834,19.5743692535154,42.6589442452135));
#71372=CARTESIAN_POINT('Ctrl Pts',(29.8289632520064,18.1044110876269,42.7860133106639));
#71373=CARTESIAN_POINT('Ctrl Pts',(32.3407182797052,19.2868958168906,42.9130823761145));
#71374=CARTESIAN_POINT('Ctrl Pts',(32.7083065278301,22.0386308269752,43.0401514415649));
#71375=CARTESIAN_POINT('Ctrl Pts',(30.5950131860389,23.8389543245811,43.1672205070154));
#71376=CARTESIAN_POINT('Ctrl Pts',(27.9366621165128,23.0387069461834,43.2942895724659));
#71377=CARTESIAN_POINT('Ctrl Pts',(27.1684047827057,20.3709616813536,43.4213586379164));
#71378=CARTESIAN_POINT('Ctrl Pts',(28.9939342849178,18.2794018293665,43.5484277033669));
#71379=CARTESIAN_POINT('Ctrl Pts',(31.7411189613168,18.680050824429,43.6754967688175));
#71380=CARTESIAN_POINT('Ctrl Pts',(32.8932479483033,21.2057120593666,43.8025658342679));
#71381=CARTESIAN_POINT('Ctrl Pts',(31.3953626233458,23.543190638775,43.9296348997184));
#71382=CARTESIAN_POINT('Ctrl Pts',(28.6187169358912,23.5505214799681,44.0567039651689));
#71383=CARTESIAN_POINT('Ctrl Pts',(27.1085075803675,21.2225311106238,44.1837730306194));
#71384=CARTESIAN_POINT('Ctrl Pts',(28.2446834257002,18.6886271243442,44.3108420960699));
#71385=CARTESIAN_POINT('Ctrl Pts',(30.9939383034346,18.2761520387535,44.4379289974135));
#71386=CARTESIAN_POINT('Ctrl Pts',(32.2113431714937,19.659237124296,44.522659543607));
#71387=CARTESIAN_POINT('Ctrl Pts',(32.3925313980793,20.4554980791997,44.5650337346504));
#71388=CARTESIAN_POINT('Origin',(30.4136184579328,21.5025377287161,36.4999999999269));
#71389=CARTESIAN_POINT('Ctrl Pts',(28.3849103233787,19.1570578993166,44.3));
#71390=CARTESIAN_POINT('Ctrl Pts',(28.3967791015268,19.1468558871996,44.3));
#71391=CARTESIAN_POINT('Ctrl Pts',(28.4086478796748,19.1366538750826,44.3));
#71392=CARTESIAN_POINT('Ctrl Pts',(28.4205166578229,19.1264518629656,44.3));
#71393=CARTESIAN_POINT('Origin',(32.,21.,36.5));
#71394=CARTESIAN_POINT('Origin',(30.,21.,44.3));
#71395=CARTESIAN_POINT('',(27.3495,21.,44.5));
#71396=CARTESIAN_POINT('Origin',(30.,21.,44.5));
#71397=CARTESIAN_POINT('Origin',(27.3495,21.,44.3));
#71398=CARTESIAN_POINT('Origin',(34.75,21.,44.5));
#71399=CARTESIAN_POINT('',(25.25,21.,44.5));
#71400=CARTESIAN_POINT('Origin',(30.,21.,44.5));
#71401=CARTESIAN_POINT('Origin',(30.,21.,45.05));
#71402=CARTESIAN_POINT('',(29.1339745962156,19.5,45.05));
#71403=CARTESIAN_POINT('',(28.2679491924311,21.,45.05));
#71404=CARTESIAN_POINT('',(28.2679491924311,21.,45.05));
#71405=CARTESIAN_POINT('Origin',(30.,21.,45.05));
#71406=CARTESIAN_POINT('Origin',(30.,21.,45.05));
#71407=CARTESIAN_POINT('',(29.1339745962156,22.5,45.05));
#71408=CARTESIAN_POINT('',(29.1339745962156,22.5,45.05));
#71409=CARTESIAN_POINT('Origin',(30.,21.,45.05));
#71410=CARTESIAN_POINT('Origin',(30.,21.,45.05));
#71411=CARTESIAN_POINT('',(30.8660254037844,22.5,45.05));
#71412=CARTESIAN_POINT('',(30.8660254037844,22.5,45.05));
#71413=CARTESIAN_POINT('Origin',(30.,21.,45.05));
#71414=CARTESIAN_POINT('Origin',(30.,21.,45.05));
#71415=CARTESIAN_POINT('',(31.7320508075689,21.,45.05));
#71416=CARTESIAN_POINT('',(31.7320508075689,21.,45.05));
#71417=CARTESIAN_POINT('Origin',(30.,21.,45.05));
#71418=CARTESIAN_POINT('Origin',(30.,21.,45.05));
#71419=CARTESIAN_POINT('',(30.8660254037844,19.5,45.05));
#71420=CARTESIAN_POINT('',(30.8660254037844,19.5,45.05));
#71421=CARTESIAN_POINT('Origin',(30.,21.,45.05));
#71422=CARTESIAN_POINT('Origin',(30.,21.,45.05));
#71423=CARTESIAN_POINT('',(29.1339745962156,19.5,45.05));
#71424=CARTESIAN_POINT('Origin',(30.,21.,45.05));
#71425=CARTESIAN_POINT('Origin',(30.,21.,44.5296394397885));
#71426=CARTESIAN_POINT('',(30.,21.,44.009278879577));
#71427=CARTESIAN_POINT('',(29.1339745962156,21.,44.5296394397885));
#71428=CARTESIAN_POINT('Origin',(29.1339745962156,19.5,47.25));
#71429=CARTESIAN_POINT('',(29.1339745962156,19.5,46.996979834127));
#71430=CARTESIAN_POINT('',(28.2679491924311,21.,46.996979834127));
#71431=CARTESIAN_POINT('Origin',(28.7009618943233,20.25,41.1951086956522));
#71432=CARTESIAN_POINT('',(29.1339745962156,19.5,47.25));
#71433=CARTESIAN_POINT('',(28.2679491924311,21.,47.25));
#71434=CARTESIAN_POINT('Origin',(28.2679491924311,21.,47.25));
#71435=CARTESIAN_POINT('',(29.1339745962156,22.5,46.996979834127));
#71436=CARTESIAN_POINT('Origin',(28.7009618943233,21.75,41.1951086956522));
#71437=CARTESIAN_POINT('',(29.1339745962156,22.5,47.25));
#71438=CARTESIAN_POINT('Origin',(29.1339745962156,22.5,47.25));
#71439=CARTESIAN_POINT('',(30.8660254037844,22.5,46.996979834127));
#71440=CARTESIAN_POINT('Origin',(30.,22.5,41.1951086956522));
#71441=CARTESIAN_POINT('',(30.8660254037844,22.5,47.25));
#71442=CARTESIAN_POINT('Origin',(30.8660254037844,22.5,47.25));
#71443=CARTESIAN_POINT('',(31.7320508075689,21.,46.996979834127));
#71444=CARTESIAN_POINT('Origin',(31.2990381056767,21.75,41.1951086956522));
#71445=CARTESIAN_POINT('',(31.7320508075689,21.,47.25));
#71446=CARTESIAN_POINT('Origin',(30.8660254037844,19.5,47.25));
#71447=CARTESIAN_POINT('',(30.8660254037844,19.5,46.996979834127));
#71448=CARTESIAN_POINT('Origin',(30.,19.5,41.1951086956522));
#71449=CARTESIAN_POINT('',(30.8660254037844,19.5,47.25));
#71450=CARTESIAN_POINT('Origin',(31.7320508075689,21.,47.25));
#71451=CARTESIAN_POINT('Origin',(31.2990381056767,20.25,41.1951086956522));
#71452=CARTESIAN_POINT('Origin',(30.,21.,44.725));
#71453=CARTESIAN_POINT('',(25.25,21.,44.95));
#71454=CARTESIAN_POINT('Origin',(30.,21.,44.95));
#71455=CARTESIAN_POINT('',(25.25,21.,44.725));
#71456=CARTESIAN_POINT('Origin',(30.,21.,41.1951086956522));
#71457=CARTESIAN_POINT('Origin',(30.,21.,41.1951086956522));
#71458=CARTESIAN_POINT('',(0.,0.,0.));
#71459=CARTESIAN_POINT('Origin',(197.762132885264,11.,29.5));
#71460=CARTESIAN_POINT('',(199.054667040747,10.1027691233085,30.2629363121594));
#71461=CARTESIAN_POINT('',(198.97225,10.1027690874833,30.2629362700282));
#71462=CARTESIAN_POINT('',(197.762132885264,10.1027690874833,30.2629362700282));
#71463=CARTESIAN_POINT('',(198.972408128224,11.1995478642895,30.6605616167741));
#71464=CARTESIAN_POINT('Ctrl Pts',(199.054667040747,10.1027691233085,30.2629363121594));
#71465=CARTESIAN_POINT('Ctrl Pts',(199.050047837914,10.1510957824736,30.3197695891699));
#71466=CARTESIAN_POINT('Ctrl Pts',(199.045424869181,10.2047250125246,30.3718971729035));
#71467=CARTESIAN_POINT('Ctrl Pts',(199.039436061019,10.2767217856396,30.4296642512059));
#71468=CARTESIAN_POINT('Ctrl Pts',(199.038279532795,10.2907436101604,30.4404054001326));
#71469=CARTESIAN_POINT('Ctrl Pts',(199.03642353782,10.313389255642,30.4569580461726));
#71470=CARTESIAN_POINT('Ctrl Pts',(199.035732005111,10.3218579668715,30.4629778750665));
#71471=CARTESIAN_POINT('Ctrl Pts',(199.034482863418,10.3372030929332,30.4735828723269));
#71472=CARTESIAN_POINT('Ctrl Pts',(199.033926842805,10.344050296774,30.4782092466494));
#71473=CARTESIAN_POINT('Ctrl Pts',(199.033263392418,10.3522381752584,30.4836168364151));
#71474=CARTESIAN_POINT('Ctrl Pts',(199.033158553209,10.3535325562788,30.4844680323103));
#71475=CARTESIAN_POINT('Ctrl Pts',(199.032999120303,10.3555017482171,30.4857574312877));
#71476=CARTESIAN_POINT('Ctrl Pts',(199.032944595149,10.3561753388067,30.4861975033045));
#71477=CARTESIAN_POINT('Ctrl Pts',(199.03285671492,10.3572612100683,30.4869053409987));
#71478=CARTESIAN_POINT('Ctrl Pts',(199.0328233757,10.3576732092472,30.4871735399891));
#71479=CARTESIAN_POINT('Ctrl Pts',(199.032768002488,10.3583575840413,30.4876184374311));
#71480=CARTESIAN_POINT('Ctrl Pts',(199.03274597382,10.3586298653129,30.4877952815448));
#71481=CARTESIAN_POINT('Ctrl Pts',(199.032708712138,10.3590904686424,30.4880941683234));
#71482=CARTESIAN_POINT('Ctrl Pts',(199.032693481273,10.3592787526436,30.488216269875));
#71483=CARTESIAN_POINT('Ctrl Pts',(199.032620047558,10.3601865909939,30.4888046315188));
#71484=CARTESIAN_POINT('Ctrl Pts',(199.032561818005,10.360906617924,30.48927015857));
#71485=CARTESIAN_POINT('Ctrl Pts',(199.032446957709,10.3623272003227,30.4901864253755));
#71486=CARTESIAN_POINT('Ctrl Pts',(199.032390328606,10.3630277270215,30.4906372090209));
#71487=CARTESIAN_POINT('Ctrl Pts',(199.032277593615,10.3644225891859,30.4915327010402));
#71488=CARTESIAN_POINT('Ctrl Pts',(199.032221488307,10.3651169146002,30.4919774242575));
#71489=CARTESIAN_POINT('Ctrl Pts',(199.032108839059,10.3665112685847,30.492868460022));
#71490=CARTESIAN_POINT('Ctrl Pts',(199.032052294787,10.3672113031633,30.4933147622412));
#71491=CARTESIAN_POINT('Ctrl Pts',(199.030942145707,10.3809579693864,30.5020584252807));
#71492=CARTESIAN_POINT('Ctrl Pts',(199.029879335722,10.3941657112817,30.5100984600361));
#71493=CARTESIAN_POINT('Ctrl Pts',(199.027494437902,10.4238941369291,30.5274024155019));
#71494=CARTESIAN_POINT('Ctrl Pts',(199.026168124288,10.4404874614061,30.536532363144));
#71495=CARTESIAN_POINT('Ctrl Pts',(199.021981122858,10.4930527493686,30.5638247225895));
#71496=CARTESIAN_POINT('Ctrl Pts',(199.019078689559,10.5297387387927,30.580542636061));
#71497=CARTESIAN_POINT('Ctrl Pts',(199.011211935375,10.6302098477806,30.6202408078014));
#71498=CARTESIAN_POINT('Ctrl Pts',(199.006198748159,10.6952429953544,30.6396523341107));
#71499=CARTESIAN_POINT('Ctrl Pts',(198.999426957925,10.7872455683046,30.6586704711183));
#71500=CARTESIAN_POINT('Ctrl Pts',(198.997560635733,10.8130790418952,30.6631175727641));
#71501=CARTESIAN_POINT('Ctrl Pts',(198.995140521639,10.8474561228168,30.6678602588841));
#71502=CARTESIAN_POINT('Ctrl Pts',(198.994552261683,10.8558835235845,30.6689301392159));
#71503=CARTESIAN_POINT('Ctrl Pts',(198.993631743619,10.8691949353454,30.6704739048081));
#71504=CARTESIAN_POINT('Ctrl Pts',(198.993296352101,10.8740714055189,30.6710085900895));
#71505=CARTESIAN_POINT('Ctrl Pts',(198.992594277158,10.8843380921291,30.6720694152485));
#71506=CARTESIAN_POINT('Ctrl Pts',(198.992227989733,10.8897288660171,30.6725888751746));
#71507=CARTESIAN_POINT('Ctrl Pts',(198.991302989487,10.9034239764498,30.6738132683551));
#71508=CARTESIAN_POINT('Ctrl Pts',(198.990746959212,10.9117327560362,30.6744672922818));
#71509=CARTESIAN_POINT('Ctrl Pts',(198.989536447892,10.9299700761366,30.675708201186));
#71510=CARTESIAN_POINT('Ctrl Pts',(198.988883754879,10.9399005978941,30.6762576421173));
#71511=CARTESIAN_POINT('Ctrl Pts',(198.982788814076,11.0334047119427,30.6802437892237));
#71512=CARTESIAN_POINT('Ctrl Pts',(198.97769936836,11.1171236786616,30.6748943153088));
#71513=CARTESIAN_POINT('Ctrl Pts',(198.972499309319,11.1995770050681,30.6607170549053));
#71514=CARTESIAN_POINT('Origin',(198.97225,11.,29.5));
#71515=CARTESIAN_POINT('Origin',(197.762132885264,11.,29.5));
#71516=CARTESIAN_POINT('',(199.554117165109,10.1027690888331,30.2629362716156));
#71517=CARTESIAN_POINT('',(199.456018641859,10.1027690874833,30.2629362700282));
#71518=CARTESIAN_POINT('',(197.762132885264,10.1027690874833,30.2629362700282));
#71519=CARTESIAN_POINT('Ctrl Pts',(199.554117165109,10.1027690888331,30.2629362716156));
#71520=CARTESIAN_POINT('Ctrl Pts',(199.55397561361,10.104033743,30.2644235345137));
#71521=CARTESIAN_POINT('Ctrl Pts',(199.553834153139,10.1053021670648,30.2659077375468));
#71522=CARTESIAN_POINT('Ctrl Pts',(199.551475140412,10.1265318427489,30.2906241982884));
#71523=CARTESIAN_POINT('Ctrl Pts',(199.549283840494,10.1473900197398,30.3130742890784));
#71524=CARTESIAN_POINT('Ctrl Pts',(199.546521955864,10.1754176750091,30.3409747178614));
#71525=CARTESIAN_POINT('Ctrl Pts',(199.545904047563,10.181805151833,30.3471904680199));
#71526=CARTESIAN_POINT('Ctrl Pts',(199.544911134781,10.1922692472355,30.3571444860382));
#71527=CARTESIAN_POINT('Ctrl Pts',(199.544532969818,10.1963025831272,30.3609274674216));
#71528=CARTESIAN_POINT('Ctrl Pts',(199.543786434426,10.204363322805,30.3683818490507));
#71529=CARTESIAN_POINT('Ctrl Pts',(199.543418020189,10.2083898433213,30.3720539663394));
#71530=CARTESIAN_POINT('Ctrl Pts',(199.542477546404,10.2187890451231,30.3814064782455));
#71531=CARTESIAN_POINT('Ctrl Pts',(199.541908373359,10.2251984015703,30.3870459003836));
#71532=CARTESIAN_POINT('Ctrl Pts',(199.539410509341,10.2538093262097,30.4116731581275));
#71533=CARTESIAN_POINT('Ctrl Pts',(199.537528526823,10.2766533342977,30.4299023454379));
#71534=CARTESIAN_POINT('Ctrl Pts',(199.531582977554,10.3520366351769,30.4855961135881));
#71535=CARTESIAN_POINT('Ctrl Pts',(199.527635449356,10.4069837312913,30.519602292334));
#71536=CARTESIAN_POINT('Ctrl Pts',(199.519886246082,10.5180487324825,30.5763089044829));
#71537=CARTESIAN_POINT('Ctrl Pts',(199.516103624939,10.5736686306426,30.5995263488409));
#71538=CARTESIAN_POINT('Ctrl Pts',(199.511172823979,10.6454805301191,30.6232317315417));
#71539=CARTESIAN_POINT('Ctrl Pts',(199.510157441837,10.6602392917988,30.6277837570737));
#71540=CARTESIAN_POINT('Ctrl Pts',(199.508480393937,10.6845348883537,30.6347570350474));
#71541=CARTESIAN_POINT('Ctrl Pts',(199.507824282064,10.6940203771917,30.6373514082756));
#71542=CARTESIAN_POINT('Ctrl Pts',(199.506537156815,10.7125823251794,30.6421792746344));
#71543=CARTESIAN_POINT('Ctrl Pts',(199.505906557151,10.7216550977296,30.6444241005806));
#71544=CARTESIAN_POINT('Ctrl Pts',(199.504397279835,10.7433129252783,30.6495100035707));
#71545=CARTESIAN_POINT('Ctrl Pts',(199.503515586384,10.7559196062974,30.6522526811813));
#71546=CARTESIAN_POINT('Ctrl Pts',(199.500356291611,10.8009136317413,30.6612699585049));
#71547=CARTESIAN_POINT('Ctrl Pts',(199.49804382135,10.833513999149,30.6663898793413));
#71548=CARTESIAN_POINT('Ctrl Pts',(199.491839879123,10.9200914554552,30.6762834562131));
#71549=CARTESIAN_POINT('Ctrl Pts',(199.48789226576,10.9742545269602,30.6787129927265));
#71550=CARTESIAN_POINT('Ctrl Pts',(199.479087076369,11.0943445212123,30.6758175991903));
#71551=CARTESIAN_POINT('Ctrl Pts',(199.474232457238,11.1600564508388,30.6686878289023));
#71552=CARTESIAN_POINT('Ctrl Pts',(199.468741914828,11.2365650748656,30.6538088907022));
#71553=CARTESIAN_POINT('Ctrl Pts',(199.467907032434,11.2482656166387,30.6513479932067));
#71554=CARTESIAN_POINT('Ctrl Pts',(199.466649765203,11.2660161440091,30.6473314461284));
#71555=CARTESIAN_POINT('Ctrl Pts',(199.466220929688,11.2720942174386,30.6459052218114));
#71556=CARTESIAN_POINT('Ctrl Pts',(199.465441596703,11.2831884789837,30.643208694156));
#71557=CARTESIAN_POINT('Ctrl Pts',(199.465090325176,11.2882078776386,30.6419536129155));
#71558=CARTESIAN_POINT('Ctrl Pts',(199.464278022546,11.2998570672304,30.6389590753402));
#71559=CARTESIAN_POINT('Ctrl Pts',(199.46381837152,11.3064801642162,30.6371947725203));
#71560=CARTESIAN_POINT('Ctrl Pts',(199.462316399564,11.3282090702536,30.6312028609942));
#71561=CARTESIAN_POINT('Ctrl Pts',(199.461286601463,11.343246523321,30.6267311068583));
#71562=CARTESIAN_POINT('Ctrl Pts',(199.458766387683,11.380247954646,30.6149182265592));
#71563=CARTESIAN_POINT('Ctrl Pts',(199.457290554239,11.4020937856794,30.6072271092186));
#71564=CARTESIAN_POINT('Ctrl Pts',(199.449751762245,11.5136303672644,30.5642221185986));
#71565=CARTESIAN_POINT('Ctrl Pts',(199.443939895019,11.598963682996,30.5186404937894));
#71566=CARTESIAN_POINT('Ctrl Pts',(199.435963409052,11.7013279243578,30.4466057868504));
#71567=CARTESIAN_POINT('Ctrl Pts',(199.434105573168,11.7242480082989,30.4291867373441));
#71568=CARTESIAN_POINT('Ctrl Pts',(199.431467814239,11.7553237250241,30.4037207001819));
#71569=CARTESIAN_POINT('Ctrl Pts',(199.430714595171,11.7640359377842,30.3963671706326));
#71570=CARTESIAN_POINT('Ctrl Pts',(199.429333220759,11.7797104000681,30.382742612754));
#71571=CARTESIAN_POINT('Ctrl Pts',(199.428706751116,11.7867072514395,30.3765127040578));
#71572=CARTESIAN_POINT('Ctrl Pts',(199.427429176894,11.8007454544031,30.3637097605538));
#71573=CARTESIAN_POINT('Ctrl Pts',(199.426777924717,11.8077819637742,30.3571325001384));
#71574=CARTESIAN_POINT('Ctrl Pts',(199.425140993212,11.825165755119,30.3404790992798));
#71575=CARTESIAN_POINT('Ctrl Pts',(199.424150887683,11.835409604665,30.330297778095));
#71576=CARTESIAN_POINT('Ctrl Pts',(199.419872076268,11.8785083437364,30.2858569666828));
#71577=CARTESIAN_POINT('Ctrl Pts',(199.416506222358,11.9094591744748,30.2498207000433));
#71578=CARTESIAN_POINT('Ctrl Pts',(199.409635154824,11.9669869414675,30.1740227900945));
#71579=CARTESIAN_POINT('Ctrl Pts',(199.406135604062,11.9934887826076,30.1343107094375));
#71580=CARTESIAN_POINT('Ctrl Pts',(199.398376805358,12.0467882263918,30.0428719803416));
#71581=CARTESIAN_POINT('Ctrl Pts',(199.39412830673,12.0723112674455,29.9905359262447));
#71582=CARTESIAN_POINT('Ctrl Pts',(199.389359185023,12.0975448000005,29.927304354392));
#71583=CARTESIAN_POINT('Ctrl Pts',(199.388669199555,12.1011074520957,29.9180382689772));
#71584=CARTESIAN_POINT('Ctrl Pts',(199.387589670073,12.1065474324464,29.9033371802295));
#71585=CARTESIAN_POINT('Ctrl Pts',(199.387195948245,12.1085027647167,29.8979318098835));
#71586=CARTESIAN_POINT('Ctrl Pts',(199.386443382754,12.1121861300555,29.8875115554209));
#71587=CARTESIAN_POINT('Ctrl Pts',(199.386084243431,12.1139199709967,29.8824990102202));
#71588=CARTESIAN_POINT('Ctrl Pts',(199.385201684437,12.118119594338,29.8700871010029));
#71589=CARTESIAN_POINT('Ctrl Pts',(199.384680467488,12.1205459062477,29.8626744678721));
#71590=CARTESIAN_POINT('Ctrl Pts',(199.382687517735,12.129604921492,29.834039148791));
#71591=CARTESIAN_POINT('Ctrl Pts',(199.381242265404,12.1357102068358,29.8126530083178));
#71592=CARTESIAN_POINT('Ctrl Pts',(199.377308627066,12.1508818761976,29.7531762123979));
#71593=CARTESIAN_POINT('Ctrl Pts',(199.374864624295,12.1586607634217,29.7147857646126));
#71594=CARTESIAN_POINT('Ctrl Pts',(199.366816968299,12.1780431339211,29.5865973098536));
#71595=CARTESIAN_POINT('Ctrl Pts',(199.361276100427,12.1812137671653,29.49586585006));
#71596=CARTESIAN_POINT('Ctrl Pts',(199.354273251435,12.1725773065496,29.3883835085662));
#71597=CARTESIAN_POINT('Ctrl Pts',(199.353136694342,12.1708068367173,29.3711315306429));
#71598=CARTESIAN_POINT('Ctrl Pts',(199.351311542584,12.1673880671735,29.3437799439687));
#71599=CARTESIAN_POINT('Ctrl Pts',(199.350630593516,12.1659878940476,29.3336514944718));
#71600=CARTESIAN_POINT('Ctrl Pts',(199.349328601689,12.1630764969782,29.3144389358177));
#71601=CARTESIAN_POINT('Ctrl Pts',(199.348708379303,12.1615902487833,29.3053517734548));
#71602=CARTESIAN_POINT('Ctrl Pts',(199.347275314284,12.1579301140469,29.2845103534915));
#71603=CARTESIAN_POINT('Ctrl Pts',(199.346460265098,12.1556835535797,29.272770066573));
#71604=CARTESIAN_POINT('Ctrl Pts',(199.34381309581,12.1478615776771,29.2350158073927));
#71605=CARTESIAN_POINT('Ctrl Pts',(199.341959524407,12.1415836765402,29.2091575333803));
#71606=CARTESIAN_POINT('Ctrl Pts',(199.337359809625,12.1240809675592,29.1464152203365));
#71607=CARTESIAN_POINT('Ctrl Pts',(199.334588554984,12.1119109696819,29.1098285599595));
#71608=CARTESIAN_POINT('Ctrl Pts',(199.326289822645,12.0706235272621,29.003437714297));
#71609=CARTESIAN_POINT('Ctrl Pts',(199.320682692828,12.0365563045028,28.9357660878128));
#71610=CARTESIAN_POINT('Ctrl Pts',(199.313658292782,11.9843372787911,28.8529504484375));
#71611=CARTESIAN_POINT('Ctrl Pts',(199.312075774013,11.9719004748141,28.8344155840126));
#71612=CARTESIAN_POINT('Ctrl Pts',(199.309963024472,11.9542842249072,28.809709414937));
#71613=CARTESIAN_POINT('Ctrl Pts',(199.309407969382,11.9495580027044,28.8032223582065));
#71614=CARTESIAN_POINT('Ctrl Pts',(199.308493925471,11.9416053552586,28.7925380346109));
#71615=CARTESIAN_POINT('Ctrl Pts',(199.308132546753,11.9384163405637,28.7883133741403));
#71616=CARTESIAN_POINT('Ctrl Pts',(199.307389348292,11.9317627189889,28.7796214511788));
#71617=CARTESIAN_POINT('Ctrl Pts',(199.307007797144,11.9282942510155,28.7751573929824));
#71618=CARTESIAN_POINT('Ctrl Pts',(199.305991723728,11.9189208614585,28.7632711050602));
#71619=CARTESIAN_POINT('Ctrl Pts',(199.30536103486,11.9129580649776,28.7558947656303));
#71620=CARTESIAN_POINT('Ctrl Pts',(199.30184787498,11.8789721192224,28.7148757239378));
#71621=CARTESIAN_POINT('Ctrl Pts',(199.299072135445,11.8491760198917,28.682740519812));
#71622=CARTESIAN_POINT('Ctrl Pts',(199.290253089337,11.7476566097271,28.5848149072397));
#71623=CARTESIAN_POINT('Ctrl Pts',(199.284360662411,11.6695677452392,28.526227526484));
#71624=CARTESIAN_POINT('Ctrl Pts',(199.276712481297,11.566567284197,28.4672580955822));
#71625=CARTESIAN_POINT('Ctrl Pts',(199.275316604586,11.5476829573531,28.4571205166682));
#71626=CARTESIAN_POINT('Ctrl Pts',(199.273166243126,11.5185496102897,28.4424905777106));
#71627=CARTESIAN_POINT('Ctrl Pts',(199.272424683742,11.5084951992158,28.4376194209032));
#71628=CARTESIAN_POINT('Ctrl Pts',(199.271067281495,11.4900882642366,28.4290227969557));
#71629=CARTESIAN_POINT('Ctrl Pts',(199.270453095659,11.4817586612533,28.4252501404964));
#71630=CARTESIAN_POINT('Ctrl Pts',(199.269109600489,11.4635419101987,28.4172537035204));
#71631=CARTESIAN_POINT('Ctrl Pts',(199.268379095556,11.4536392362692,28.4130675848045));
#71632=CARTESIAN_POINT('Ctrl Pts',(199.266280443305,11.4252063626599,28.4015044972366));
#71633=CARTESIAN_POINT('Ctrl Pts',(199.264901528461,11.4065449772769,28.3944621585162));
#71634=CARTESIAN_POINT('Ctrl Pts',(199.261710920056,11.3634351727307,28.3794326950577));
#71635=CARTESIAN_POINT('Ctrl Pts',(199.259890231092,11.3388865127897,28.3717659901676));
#71636=CARTESIAN_POINT('Ctrl Pts',(199.252974247716,11.2457828587354,28.346001876214));
#71637=CARTESIAN_POINT('Ctrl Pts',(199.247749983417,11.1758942782619,28.333303594154));
#71638=CARTESIAN_POINT('Ctrl Pts',(199.23914984729,11.058738373807,28.3227872028255));
#71639=CARTESIAN_POINT('Ctrl Pts',(199.235761035929,11.0119679081332,28.321383083587));
#71640=CARTESIAN_POINT('Ctrl Pts',(199.231805665549,10.9554979698128,28.3230507673531));
#71641=CARTESIAN_POINT('Ctrl Pts',(199.231128960288,10.9457659216815,28.32345905004));
#71642=CARTESIAN_POINT('Ctrl Pts',(199.230065343891,10.9303399051886,28.3242980321637));
#71643=CARTESIAN_POINT('Ctrl Pts',(199.229674450539,10.92464231264,28.3246494700024));
#71644=CARTESIAN_POINT('Ctrl Pts',(199.228923235393,10.9136335284199,28.3254088940476));
#71645=CARTESIAN_POINT('Ctrl Pts',(199.228562662267,10.9083222189539,28.3258115060541));
#71646=CARTESIAN_POINT('Ctrl Pts',(199.227670957267,10.8951246071276,28.3269020169546));
#71647=CARTESIAN_POINT('Ctrl Pts',(199.227142132131,10.8872419815451,28.3276334346491));
#71648=CARTESIAN_POINT('Ctrl Pts',(199.225079023685,10.8562998910404,28.330819484723));
#71649=CARTESIAN_POINT('Ctrl Pts',(199.223573649349,10.8333061106647,28.3338756030311));
#71650=CARTESIAN_POINT('Ctrl Pts',(199.219404661186,10.7690025087063,28.344363416282));
#71651=CARTESIAN_POINT('Ctrl Pts',(199.216792037532,10.7279768615204,28.353326713131));
#71652=CARTESIAN_POINT('Ctrl Pts',(199.208900253456,10.6052605522628,28.387096607951));
#71653=CARTESIAN_POINT('Ctrl Pts',(199.203659135385,10.5257176221002,28.4185991700282));
#71654=CARTESIAN_POINT('Ctrl Pts',(199.196975301239,10.4345944234358,28.4666916876087));
#71655=CARTESIAN_POINT('Ctrl Pts',(199.195814223083,10.4191009397079,28.4753216292874));
#71656=CARTESIAN_POINT('Ctrl Pts',(199.193952723513,10.3948363773603,28.4895643048852));
#71657=CARTESIAN_POINT('Ctrl Pts',(199.193260322993,10.3859343657315,28.4949494095047));
#71658=CARTESIAN_POINT('Ctrl Pts',(199.192010618432,10.3700953914079,28.5048198834376));
#71659=CARTESIAN_POINT('Ctrl Pts',(199.191454916925,10.363131989357,28.5092616836714));
#71660=CARTESIAN_POINT('Ctrl Pts',(199.190140095822,10.3468470395989,28.51989212098));
#71661=CARTESIAN_POINT('Ctrl Pts',(199.189378800807,10.3375659644616,28.5261409866342));
#71662=CARTESIAN_POINT('Ctrl Pts',(199.187090830196,10.3101218832859,28.5451926805549));
#71663=CARTESIAN_POINT('Ctrl Pts',(199.18555011509,10.2922315858019,28.5583776812938));
#71664=CARTESIAN_POINT('Ctrl Pts',(199.18000145544,10.2299142066744,28.6070846928884));
#71665=CARTESIAN_POINT('Ctrl Pts',(199.175896219152,10.1877039488176,28.6453050043792));
#71666=CARTESIAN_POINT('Ctrl Pts',(199.166391905083,10.0978706245797,28.7393337318908));
#71667=CARTESIAN_POINT('Ctrl Pts',(199.160975857458,10.0523575066952,28.7968462118573));
#71668=CARTESIAN_POINT('Ctrl Pts',(199.154662411959,10.0038886342109,28.8714258066601));
#71669=CARTESIAN_POINT('Ctrl Pts',(199.153555273488,9.99556733653232,28.884810230761));
#71670=CARTESIAN_POINT('Ctrl Pts',(199.151992354998,9.98404652772017,28.9041982287849));
#71671=CARTESIAN_POINT('Ctrl Pts',(199.151524402698,9.98062683725261,28.9100681657741));
#71672=CARTESIAN_POINT('Ctrl Pts',(199.150705305482,9.97469063139452,28.9204634901362));
#71673=CARTESIAN_POINT('Ctrl Pts',(199.150352892367,9.97215288821443,28.9249763604106));
#71674=CARTESIAN_POINT('Ctrl Pts',(199.149582833646,9.9666431554737,28.9349273546286));
#71675=CARTESIAN_POINT('Ctrl Pts',(199.14916597653,9.96368422436451,28.9403723737055));
#71676=CARTESIAN_POINT('Ctrl Pts',(199.147941808949,9.95507060884029,28.9565257454444));
#71677=CARTESIAN_POINT('Ctrl Pts',(199.147141479161,9.94953775244688,28.9672985902588));
#71678=CARTESIAN_POINT('Ctrl Pts',(199.143255866313,9.92322941367611,29.0205272411553));
#71679=CARTESIAN_POINT('Ctrl Pts',(199.140284425323,9.90485440480586,29.0641260633656));
#71680=CARTESIAN_POINT('Ctrl Pts',(199.131786683405,9.85948500349734,29.1929292189662));
#71681=CARTESIAN_POINT('Ctrl Pts',(199.126343070861,9.83949586739486,29.2802362381936));
#71682=CARTESIAN_POINT('Ctrl Pts',(199.119210658951,9.82718122709295,29.39023097704));
#71683=CARTESIAN_POINT('Ctrl Pts',(199.117816625471,9.82538031996532,29.411560020899));
#71684=CARTESIAN_POINT('Ctrl Pts',(199.115668765839,9.82352582812475,29.4440697822466));
#71685=CARTESIAN_POINT('Ctrl Pts',(199.114927834619,9.82304859034161,29.4552224209926));
#71686=CARTESIAN_POINT('Ctrl Pts',(199.113571434148,9.8224690885387,29.4755147200795));
#71687=CARTESIAN_POINT('Ctrl Pts',(199.112957618516,9.82231455385527,29.4846520900297));
#71688=CARTESIAN_POINT('Ctrl Pts',(199.111614777694,9.82220970707052,29.5045367853038));
#71689=CARTESIAN_POINT('Ctrl Pts',(199.110884555625,9.82230013971825,29.5152834051855));
#71690=CARTESIAN_POINT('Ctrl Pts',(199.108786305008,9.822978319842,29.5459643163472));
#71691=CARTESIAN_POINT('Ctrl Pts',(199.10740750139,9.8239253045106,29.565886126029));
#71692=CARTESIAN_POINT('Ctrl Pts',(199.104216934179,9.8272501695058,29.6114184925363));
#71693=CARTESIAN_POINT('Ctrl Pts',(199.102396165509,9.82996205894455,29.6369938012734));
#71694=CARTESIAN_POINT('Ctrl Pts',(199.095478606081,9.8432901161763,29.7326925542547));
#71695=CARTESIAN_POINT('Ctrl Pts',(199.090252674016,9.85939438164621,29.8018953761779));
#71696=CARTESIAN_POINT('Ctrl Pts',(199.081651486936,9.89627324953134,29.9136019429219));
#71697=CARTESIAN_POINT('Ctrl Pts',(199.078263233059,9.91355511673502,29.9570751827318));
#71698=CARTESIAN_POINT('Ctrl Pts',(199.074308650384,9.93750565007133,30.0082279215158));
#71699=CARTESIAN_POINT('Ctrl Pts',(199.073632156896,9.9417436892029,30.0169946419011));
#71700=CARTESIAN_POINT('Ctrl Pts',(199.07256892404,9.94863690912871,30.0308137783448));
#71701=CARTESIAN_POINT('Ctrl Pts',(199.072178202638,9.95122082324698,30.0359009777559));
#71702=CARTESIAN_POINT('Ctrl Pts',(199.071427261538,9.95628750092329,30.0456992172214));
#71703=CARTESIAN_POINT('Ctrl Pts',(199.071066790771,9.9587653940781,30.0504124935947));
#71704=CARTESIAN_POINT('Ctrl Pts',(199.070175449316,9.96500435338885,30.0620868911616));
#71705=CARTESIAN_POINT('Ctrl Pts',(199.069646882718,9.96880384738301,30.0690273850704));
#71706=CARTESIAN_POINT('Ctrl Pts',(199.067586009318,9.98399792850531,30.0961301702344));
#71707=CARTESIAN_POINT('Ctrl Pts',(199.066082538199,9.99591697761888,30.1159941851323));
#71708=CARTESIAN_POINT('Ctrl Pts',(199.061921643895,10.0310027292842,30.170739690745));
#71709=CARTESIAN_POINT('Ctrl Pts',(199.059314989865,10.0554550527729,30.2047572237535));
#71710=CARTESIAN_POINT('Ctrl Pts',(199.056034177674,10.088584320814,30.2460151023313));
#71711=CARTESIAN_POINT('Ctrl Pts',(199.055350501907,10.0956186699298,30.2545272124069));
#71712=CARTESIAN_POINT('Ctrl Pts',(199.054667040747,10.1027691233085,30.2629363121594));
#71713=CARTESIAN_POINT('',(198.971545633483,9.96489439058431,30.0635599336052));
#71714=CARTESIAN_POINT('Origin',(198.97225,11.,29.5));
#71715=CARTESIAN_POINT('',(199.01213292537,9.82225003050404,29.500268052058));
#71716=CARTESIAN_POINT('Ctrl Pts',(198.972443712976,9.96565131904446,30.0632209767982));
#71717=CARTESIAN_POINT('Ctrl Pts',(198.975807610355,9.94171007452878,30.0192531636212));
#71718=CARTESIAN_POINT('Ctrl Pts',(198.979171507734,9.92061433691864,29.9738270716902));
#71719=CARTESIAN_POINT('Ctrl Pts',(198.982535405113,9.9025075342917,29.927323472575));
#71720=CARTESIAN_POINT('Ctrl Pts',(198.98590663962,9.884361238206,29.8807184426323));
#71721=CARTESIAN_POINT('Ctrl Pts',(198.989277874128,9.86921700580483,29.8330316474283));
#71722=CARTESIAN_POINT('Ctrl Pts',(198.992649108635,9.85716802120539,29.7846579188155));
#71723=CARTESIAN_POINT('Ctrl Pts',(198.996032930337,9.84507404925335,29.7361035769762));
#71724=CARTESIAN_POINT('Ctrl Pts',(198.99941675204,9.83609851197747,29.6868576152335));
#71725=CARTESIAN_POINT('Ctrl Pts',(199.002800573742,9.83028330893629,29.6373241608274));
#71726=CARTESIAN_POINT('Ctrl Pts',(199.004794261458,9.82685709447019,29.6081399282495));
#71727=CARTESIAN_POINT('Ctrl Pts',(199.006787949173,9.82452695210034,29.5788559541146));
#71728=CARTESIAN_POINT('Ctrl Pts',(199.008781636889,9.82329298769148,29.5495547140438));
#71729=CARTESIAN_POINT('Ctrl Pts',(199.00989871968,9.82260158532406,29.5331369416932));
#71730=CARTESIAN_POINT('Ctrl Pts',(199.011015802472,9.82225377973876,29.5167050154579));
#71731=CARTESIAN_POINT('Ctrl Pts',(199.012132885264,9.82225003063834,29.5002686421649));
#71732=CARTESIAN_POINT('Ctrl Pts',(199.012132965476,9.82225003036973,29.500267461951));
#71733=CARTESIAN_POINT('Ctrl Pts',(199.015290203676,9.82223948074753,29.4538129394526));
#71734=CARTESIAN_POINT('Ctrl Pts',(199.018447441875,9.82498170507075,29.4072497693987));
#71735=CARTESIAN_POINT('Ctrl Pts',(199.021604680075,9.83048918351974,29.3609334237292));
#71736=CARTESIAN_POINT('Ctrl Pts',(199.024757398053,9.83598877690527,29.3146833892271));
#71737=CARTESIAN_POINT('Ctrl Pts',(199.027910116031,9.84424573011089,29.2686800365615));
#71738=CARTESIAN_POINT('Ctrl Pts',(199.031062834009,9.85522055611645,29.2232779601086));
#71739=CARTESIAN_POINT('Ctrl Pts',(199.034212471243,9.86618465784211,29.1779202492406));
#71740=CARTESIAN_POINT('Ctrl Pts',(199.037362108477,9.87986124591711,29.1331631992053));
#71741=CARTESIAN_POINT('Ctrl Pts',(199.040511745711,9.89615953926772,29.0893525846296));
#71742=CARTESIAN_POINT('Ctrl Pts',(199.043659736592,9.91244931331107,29.0455648703711));
#71743=CARTESIAN_POINT('Ctrl Pts',(199.046807727474,9.93135788183305,29.0027231407691));
#71744=CARTESIAN_POINT('Ctrl Pts',(199.049955718356,9.95274508255928,28.961156608655));
#71745=CARTESIAN_POINT('Ctrl Pts',(199.053105823233,9.97414664559549,28.9195621630506));
#71746=CARTESIAN_POINT('Ctrl Pts',(199.056255928109,9.99802991680388,28.8792451344006));
#71747=CARTESIAN_POINT('Ctrl Pts',(199.059406032985,10.0242080271693,28.8405114949757));
#71748=CARTESIAN_POINT('Ctrl Pts',(199.062556987811,10.0503932008154,28.8017674045838));
#71749=CARTESIAN_POINT('Ctrl Pts',(199.065707942637,10.0788741100446,28.7646080098553));
#71750=CARTESIAN_POINT('Ctrl Pts',(199.068858897463,10.1094217892156,28.7293084190313));
#71751=CARTESIAN_POINT('Ctrl Pts',(199.072016018166,10.1400292449474,28.6939397529716));
#71752=CARTESIAN_POINT('Ctrl Pts',(199.075173138869,10.1727111597207,28.6604385732073));
#71753=CARTESIAN_POINT('Ctrl Pts',(199.078330259573,10.2072007417723,28.6290439743284));
#71754=CARTESIAN_POINT('Ctrl Pts',(199.081364684923,10.2403499533278,28.5988694654469));
#71755=CARTESIAN_POINT('Ctrl Pts',(199.084399110273,10.2751684678066,28.5706409972311));
#71756=CARTESIAN_POINT('Ctrl Pts',(199.087433535623,10.3113934224206,28.544533598804));
#71757=CARTESIAN_POINT('Ctrl Pts',(199.090710698071,10.3505161712813,28.5163377541728));
#71758=CARTESIAN_POINT('Ctrl Pts',(199.093987860518,10.391458684281,28.4904873589618));
#71759=CARTESIAN_POINT('Ctrl Pts',(199.097265022965,10.433907274098,28.4672202131234));
#71760=CARTESIAN_POINT('Ctrl Pts',(199.100443805193,10.4750815598006,28.4446515456043));
#71761=CARTESIAN_POINT('Ctrl Pts',(199.103622587421,10.5176722408203,28.4245134947446));
#71762=CARTESIAN_POINT('Ctrl Pts',(199.106801369648,10.5613622420152,28.4069803387999));
#71763=CARTESIAN_POINT('Ctrl Pts',(199.109977113254,10.6050104796088,28.389463942931));
#71764=CARTESIAN_POINT('Ctrl Pts',(199.11315285686,10.6497554441766,28.3745477182844));
#71765=CARTESIAN_POINT('Ctrl Pts',(199.116328600465,10.6952577315414,28.3623589264119));
#71766=CARTESIAN_POINT('Ctrl Pts',(199.119502689493,10.7407363119845,28.3501764849615));
#71767=CARTESIAN_POINT('Ctrl Pts',(199.12267677852,10.7869708982647,28.3407188040294));
#71768=CARTESIAN_POINT('Ctrl Pts',(199.125850867547,10.8336070530522,28.3340632737125));
#71769=CARTESIAN_POINT('Ctrl Pts',(199.129024683154,10.8802391905317,28.3274083167129));
#71770=CARTESIAN_POINT('Ctrl Pts',(199.13219849876,10.9272722784719,28.3235551068591));
#71771=CARTESIAN_POINT('Ctrl Pts',(199.135372314367,10.9743444957301,28.3225294663557));
#71772=CARTESIAN_POINT('Ctrl Pts',(199.138549374687,11.0214648367325,28.3215027773004));
#71773=CARTESIAN_POINT('Ctrl Pts',(199.141726435008,11.0686238312664,28.3233094351217));
#71774=CARTESIAN_POINT('Ctrl Pts',(199.144903495329,11.1154593631351,28.3279231262565));
#71775=CARTESIAN_POINT('Ctrl Pts',(199.1480825397,11.1623241434446,28.332539698607));
#71776=CARTESIAN_POINT('Ctrl Pts',(199.151261584071,11.2088645111085,28.3399667052858));
#71777=CARTESIAN_POINT('Ctrl Pts',(199.154440628442,11.2547267752472,28.3501263841308));
#71778=CARTESIAN_POINT('Ctrl Pts',(199.157625293964,11.3006701325216,28.3603040272048));
#71779=CARTESIAN_POINT('Ctrl Pts',(199.160809959485,11.3459324626995,28.3732238252956));
#71780=CARTESIAN_POINT('Ctrl Pts',(199.163994625007,11.3901753816714,28.3887582468079));
#71781=CARTESIAN_POINT('Ctrl Pts',(199.164691561457,11.3998575610712,28.3921578203317));
#71782=CARTESIAN_POINT('Ctrl Pts',(199.165388497907,11.4094910014412,28.3956824317297));
#71783=CARTESIAN_POINT('Ctrl Pts',(199.166085434358,11.4190723032271,28.3993304459703));
#71784=CARTESIAN_POINT('Ctrl Pts',(199.169362596805,11.4641258836326,28.4164842844135));
#71785=CARTESIAN_POINT('Ctrl Pts',(199.172639759252,11.5082278906805,28.4364483183434));
#71786=CARTESIAN_POINT('Ctrl Pts',(199.1759169217,11.551005627053,28.459092770005));
#71787=CARTESIAN_POINT('Ctrl Pts',(199.179088162373,11.592400736286,28.4810053261508));
#71788=CARTESIAN_POINT('Ctrl Pts',(199.182259403045,11.6325553428388,28.5054273755897));
#71789=CARTESIAN_POINT('Ctrl Pts',(199.185430643718,11.6711502036526,28.5321919267556));
#71790=CARTESIAN_POINT('Ctrl Pts',(199.18859872715,11.7097066399855,28.5589298315245));
#71791=CARTESIAN_POINT('Ctrl Pts',(199.191766810582,11.7467059475697,28.5880053056637));
#71792=CARTESIAN_POINT('Ctrl Pts',(199.194934894014,11.7818556691029,28.6192067352712));
#71793=CARTESIAN_POINT('Ctrl Pts',(199.198101220393,11.8169858962251,28.6503908602325));
#71794=CARTESIAN_POINT('Ctrl Pts',(199.201267546772,11.8502681527442,28.6836982352638));
#71795=CARTESIAN_POINT('Ctrl Pts',(199.204433873151,11.8814432170039,28.7188771430192));
#71796=CARTESIAN_POINT('Ctrl Pts',(199.207599839623,11.9126147376819,28.7540520520874));
#71797=CARTESIAN_POINT('Ctrl Pts',(199.210765806094,11.9416791734333,28.7910976527551));
#71798=CARTESIAN_POINT('Ctrl Pts',(199.213931772566,11.9684162106679,28.829727588651));
#71799=CARTESIAN_POINT('Ctrl Pts',(199.217100915189,11.9951800709576,28.8683962787622));
#71800=CARTESIAN_POINT('Ctrl Pts',(199.220270057813,12.0196115576936,28.9086520148148));
#71801=CARTESIAN_POINT('Ctrl Pts',(199.223439200436,12.0415336788053,28.9501794307101));
#71802=CARTESIAN_POINT('Ctrl Pts',(199.226610278997,12.0634691915029,28.9917322144954));
#71803=CARTESIAN_POINT('Ctrl Pts',(199.229781357558,12.0828920580106,29.0345577156462));
#71804=CARTESIAN_POINT('Ctrl Pts',(199.232952436118,12.0996728621035,29.078319245337));
#71805=CARTESIAN_POINT('Ctrl Pts',(199.236129144687,12.116483459233,29.1221584702831));
#71806=CARTESIAN_POINT('Ctrl Pts',(199.239305853255,12.1306424730576,29.1669365062241));
#71807=CARTESIAN_POINT('Ctrl Pts',(199.242482561824,12.1420704636969,29.2123020360671));
#71808=CARTESIAN_POINT('Ctrl Pts',(199.243234152246,12.1447742585622,29.223035251601));
#71809=CARTESIAN_POINT('Ctrl Pts',(199.243985742669,12.147325406606,29.2338013173809));
#71810=CARTESIAN_POINT('Ctrl Pts',(199.244737333092,12.1497232789299,29.2445955278646));
#71811=CARTESIAN_POINT('Ctrl Pts',(199.248014495539,12.1601787303235,29.2916615629988));
#71812=CARTESIAN_POINT('Ctrl Pts',(199.251291657987,12.1677628892916,29.3394767473395));
#71813=CARTESIAN_POINT('Ctrl Pts',(199.254568820434,12.1723798432976,29.387658709597));
#71814=CARTESIAN_POINT('Ctrl Pts',(199.257743090611,12.1768518399255,29.4343279145435));
#71815=CARTESIAN_POINT('Ctrl Pts',(199.260917360789,12.1785401531388,29.4813406030709));
#71816=CARTESIAN_POINT('Ctrl Pts',(199.264091630967,12.1774090365302,29.5283376639313));
#71817=CARTESIAN_POINT('Ctrl Pts',(199.267262773696,12.1762790343537,29.5752884209544));
#71818=CARTESIAN_POINT('Ctrl Pts',(199.270433916425,12.1723351141447,29.6222230266559));
#71819=CARTESIAN_POINT('Ctrl Pts',(199.273605059154,12.1655935328295,29.6687802675847));
#71820=CARTESIAN_POINT('Ctrl Pts',(199.276774468309,12.1588556369463,29.7153120569865));
#71821=CARTESIAN_POINT('Ctrl Pts',(199.279943877464,12.1493231894927,29.761466340247));
#71822=CARTESIAN_POINT('Ctrl Pts',(199.283113286619,12.1370642147272,29.8068876571105));
#71823=CARTESIAN_POINT('Ctrl Pts',(199.286282353072,12.1248065654992,29.8523040626613));
#71824=CARTESIAN_POINT('Ctrl Pts',(199.289451419526,12.1098231214598,29.8969871225891));
#71825=CARTESIAN_POINT('Ctrl Pts',(199.292620485979,12.092232226292,29.9405948551098));
#71826=CARTESIAN_POINT('Ctrl Pts',(199.295792730805,12.0746236885721,29.9842463234201));
#71827=CARTESIAN_POINT('Ctrl Pts',(199.298964975631,12.0544026923683,30.0268197961744));
#71828=CARTESIAN_POINT('Ctrl Pts',(199.302137220457,12.0317356270029,30.0679935373513));
#71829=CARTESIAN_POINT('Ctrl Pts',(199.305311405725,12.0090546963434,30.1091924642338));
#71830=CARTESIAN_POINT('Ctrl Pts',(199.308485590992,11.9839250163396,30.1489894849433));
#71831=CARTESIAN_POINT('Ctrl Pts',(199.311659776259,11.956556948554,30.1870908722091));
#71832=CARTESIAN_POINT('Ctrl Pts',(199.314839567394,11.9291405465495,30.2252595496031));
#71833=CARTESIAN_POINT('Ctrl Pts',(199.318019358529,11.8994782249642,30.2617261911537));
#71834=CARTESIAN_POINT('Ctrl Pts',(199.321199149664,11.8678200524929,30.2962307573757));
#71835=CARTESIAN_POINT('Ctrl Pts',(199.321929177051,11.8605518603507,30.304152434387));
#71836=CARTESIAN_POINT('Ctrl Pts',(199.322659204439,11.8531786159839,30.311970853757));
#71837=CARTESIAN_POINT('Ctrl Pts',(199.323389231826,11.8457035972358,30.3196831632542));
#71838=CARTESIAN_POINT('Ctrl Pts',(199.326666394273,11.812147526388,30.354304454867));
#71839=CARTESIAN_POINT('Ctrl Pts',(199.329943556721,11.7763865406103,30.3869396180561));
#71840=CARTESIAN_POINT('Ctrl Pts',(199.333220719168,11.7386872767217,30.4172982991969));
#71841=CARTESIAN_POINT('Ctrl Pts',(199.336395134308,11.7021699798263,30.4467051591251));
#71842=CARTESIAN_POINT('Ctrl Pts',(199.339569549448,11.6638346296527,30.4739758072547));
#71843=CARTESIAN_POINT('Ctrl Pts',(199.342743964588,11.62396154616,30.4988829017526));
#71844=CARTESIAN_POINT('Ctrl Pts',(199.345915263681,11.5841276026118,30.5237655471181));
#71845=CARTESIAN_POINT('Ctrl Pts',(199.349086562773,11.5427593836559,30.5462889376308));
#71846=CARTESIAN_POINT('Ctrl Pts',(199.352257861865,11.5001675582563,30.5662680132912));
#71847=CARTESIAN_POINT('Ctrl Pts',(199.355427438465,11.4575988666251,30.586236237308));
#71848=CARTESIAN_POINT('Ctrl Pts',(199.358597015065,11.4138083883404,30.603662648244));
#71849=CARTESIAN_POINT('Ctrl Pts',(199.361766591665,11.3691304507295,30.6184085894003));
#71850=CARTESIAN_POINT('Ctrl Pts',(199.364935836341,11.3244571918726,30.633152986335));
#71851=CARTESIAN_POINT('Ctrl Pts',(199.368105081018,11.2788971872386,30.6452172986398));
#71852=CARTESIAN_POINT('Ctrl Pts',(199.371274325694,11.2328011743626,30.6545123107682));
#71853=CARTESIAN_POINT('Ctrl Pts',(199.37444676338,11.1866587198106,30.6638166876098));
#71854=CARTESIAN_POINT('Ctrl Pts',(199.377619201066,11.1399797264185,30.6703460892419));
#71855=CARTESIAN_POINT('Ctrl Pts',(199.380791638752,11.0931244413613,30.6740625626095));
#71856=CARTESIAN_POINT('Ctrl Pts',(199.383966025666,11.0462403672166,30.6777813194735));
#71857=CARTESIAN_POINT('Ctrl Pts',(199.387140412579,10.9991803424814,30.6786836981663));
#71858=CARTESIAN_POINT('Ctrl Pts',(199.390314799492,10.9523053989409,30.6767838746048));
#71859=CARTESIAN_POINT('Ctrl Pts',(199.393494803093,10.9053475159529,30.6748806895391));
#71860=CARTESIAN_POINT('Ctrl Pts',(199.396674806693,10.8585759200923,30.6701654715798));
#71861=CARTESIAN_POINT('Ctrl Pts',(199.399854810294,10.8123453406177,30.6627040858757));
#71862=CARTESIAN_POINT('Ctrl Pts',(199.400583583716,10.8017505043074,30.6609941319647));
#71863=CARTESIAN_POINT('Ctrl Pts',(199.401312357138,10.7911840289986,30.6591401572854));
#71864=CARTESIAN_POINT('Ctrl Pts',(199.40204113056,10.7806500773883,30.6571433247227));
#71865=CARTESIAN_POINT('Ctrl Pts',(199.40522003876,10.7347010016762,30.6484331451052));
#71866=CARTESIAN_POINT('Ctrl Pts',(199.40839894696,10.6891707968276,30.6369627383111));
#71867=CARTESIAN_POINT('Ctrl Pts',(199.41157785516,10.6444148634672,30.6227886146452));
#71868=CARTESIAN_POINT('Ctrl Pts',(199.41475187707,10.5997277243165,30.6086362779819));
#71869=CARTESIAN_POINT('Ctrl Pts',(199.41792589898,10.5558130271195,30.5917886189121));
#71870=CARTESIAN_POINT('Ctrl Pts',(199.42109992089,10.5130152595534,30.5723529852955));
#71871=CARTESIAN_POINT('Ctrl Pts',(199.424270708434,10.4702611034214,30.5529371568207));
#71872=CARTESIAN_POINT('Ctrl Pts',(199.427441495977,10.4286221287092,30.5309388040667));
#71873=CARTESIAN_POINT('Ctrl Pts',(199.430612283521,10.388424431426,30.5065139772618));
#71874=CARTESIAN_POINT('Ctrl Pts',(199.433781106762,10.3482516366209,30.4821042816399));
#71875=CARTESIAN_POINT('Ctrl Pts',(199.436949930002,10.3095188239599,30.4552713815384));
#71876=CARTESIAN_POINT('Ctrl Pts',(199.440118753243,10.2725265199744,30.4262167124164));
#71877=CARTESIAN_POINT('Ctrl Pts',(199.443288375647,10.2355248866845,30.3971547158284));
#71878=CARTESIAN_POINT('Ctrl Pts',(199.446457998052,10.2002650822288,30.3658701688511));
#71879=CARTESIAN_POINT('Ctrl Pts',(199.449627620456,10.1670158662807,30.3326058464075));
#71880=CARTESIAN_POINT('Ctrl Pts',(199.451757960924,10.1446686774975,30.310248504371));
#71881=CARTESIAN_POINT('Ctrl Pts',(199.453888301391,10.1232290655337,30.2869976831466));
#71882=CARTESIAN_POINT('Ctrl Pts',(199.456018641859,10.1027690874833,30.2629362700282));
#71883=CARTESIAN_POINT('Origin',(197.762132885264,11.,29.5));
#71884=CARTESIAN_POINT('',(200.055837189155,10.1027690874889,30.2629362700347));
#71885=CARTESIAN_POINT('',(199.956073744839,10.1027690874833,30.2629362700282));
#71886=CARTESIAN_POINT('',(197.762132885264,10.1027690874833,30.2629362700282));
#71887=CARTESIAN_POINT('Ctrl Pts',(200.055837189155,10.1027690874889,30.2629362700347));
#71888=CARTESIAN_POINT('Ctrl Pts',(200.054854794923,10.1121144588561,30.2739266455208));
#71889=CARTESIAN_POINT('Ctrl Pts',(200.053864348436,10.1216606349857,30.2847439824393));
#71890=CARTESIAN_POINT('Ctrl Pts',(200.049365182412,10.1655617649195,30.3326861750602));
#71891=CARTESIAN_POINT('Ctrl Pts',(200.045767937199,10.2020837943372,30.3677453333879));
#71892=CARTESIAN_POINT('Ctrl Pts',(200.038837688901,10.2752457687659,30.4294426115047));
#71893=CARTESIAN_POINT('Ctrl Pts',(200.035524082849,10.311392956766,30.4565313859838));
#71894=CARTESIAN_POINT('Ctrl Pts',(200.028401485108,10.3923792699774,30.5102481303646));
#71895=CARTESIAN_POINT('Ctrl Pts',(200.024601530178,10.437618439397,30.5361139813143));
#71896=CARTESIAN_POINT('Ctrl Pts',(200.020053351931,10.4956200767861,30.5643547433665));
#71897=CARTESIAN_POINT('Ctrl Pts',(200.019183258542,10.5069022843358,30.5696283465646));
#71898=CARTESIAN_POINT('Ctrl Pts',(200.01788982428,10.523984981196,30.5772854937322));
#71899=CARTESIAN_POINT('Ctrl Pts',(200.017459306931,10.5297239443401,30.5798031158698));
#71900=CARTESIAN_POINT('Ctrl Pts',(200.016678444491,10.5402351998181,30.5843145926775));
#71901=CARTESIAN_POINT('Ctrl Pts',(200.016327303062,10.5450007634233,30.586322928013));
#71902=CARTESIAN_POINT('Ctrl Pts',(200.015517248391,10.556083244364,30.5909076549117));
#71903=CARTESIAN_POINT('Ctrl Pts',(200.015059687144,10.5624095210276,30.5934606420703));
#71904=CARTESIAN_POINT('Ctrl Pts',(200.013572223532,10.5831782529244,30.6016328061134));
#71905=CARTESIAN_POINT('Ctrl Pts',(200.012554514343,10.5977101074211,30.6070221791975));
#71906=CARTESIAN_POINT('Ctrl Pts',(200.01007103355,10.6338376718621,30.6196152364247));
#71907=CARTESIAN_POINT('Ctrl Pts',(200.008619299216,10.655544375205,30.6264828319304));
#71908=CARTESIAN_POINT('Ctrl Pts',(200.001418939159,10.7652834656862,30.657733078677));
#71909=CARTESIAN_POINT('Ctrl Pts',(199.995901338364,10.8557410487224,30.6724453887902));
#71910=CARTESIAN_POINT('Ctrl Pts',(199.988014458571,10.9800048981241,30.6780438333142));
#71911=CARTESIAN_POINT('Ctrl Pts',(199.985890150566,11.0130624903483,30.6781409738603));
#71912=CARTESIAN_POINT('Ctrl Pts',(199.982855920796,11.0593177374628,30.6763298932124));
#71913=CARTESIAN_POINT('Ctrl Pts',(199.981981093508,11.072546943092,30.6755881632937));
#71914=CARTESIAN_POINT('Ctrl Pts',(199.980479725469,11.09504845619,30.673945305938));
#71915=CARTESIAN_POINT('Ctrl Pts',(199.979856690601,11.1043279112443,30.6731570521162));
#71916=CARTESIAN_POINT('Ctrl Pts',(199.978577114593,11.123260700138,30.6713223850789));
#71917=CARTESIAN_POINT('Ctrl Pts',(199.977920326972,11.1329123703985,30.6702664748319));
#71918=CARTESIAN_POINT('Ctrl Pts',(199.976250878958,11.1572712990166,30.6672963421513));
#71919=CARTESIAN_POINT('Ctrl Pts',(199.975233413792,11.1719571299483,30.6652234647745));
#71920=CARTESIAN_POINT('Ctrl Pts',(199.970562150302,11.2386281239938,30.6545251734251));
#71921=CARTESIAN_POINT('Ctrl Pts',(199.966811735006,11.2900308322721,30.6426952886861));
#71922=CARTESIAN_POINT('Ctrl Pts',(199.961855259039,11.355487901505,30.6229290907532));
#71923=CARTESIAN_POINT('Ctrl Pts',(199.960712321334,11.3704201569733,30.6180922494444));
#71924=CARTESIAN_POINT('Ctrl Pts',(199.95443149541,11.4516779504175,30.5899648359673));
#71925=CARTESIAN_POINT('Ctrl Pts',(199.949230212179,11.5159144819989,30.5610698425288));
#71926=CARTESIAN_POINT('Ctrl Pts',(199.942877184629,11.5935008907672,30.5174486727657));
#71927=CARTESIAN_POINT('Ctrl Pts',(199.941556307287,11.6095898585085,30.5078915642802));
#71928=CARTESIAN_POINT('Ctrl Pts',(199.939733840326,11.6318116889657,30.4939645384128));
#71929=CARTESIAN_POINT('Ctrl Pts',(199.939215068181,11.6381399898413,30.4899135692938));
#71930=CARTESIAN_POINT('Ctrl Pts',(199.93833985133,11.648828040544,30.4829266777494));
#71931=CARTESIAN_POINT('Ctrl Pts',(199.937981505076,11.6532076212099,30.4800216773532));
#71932=CARTESIAN_POINT('Ctrl Pts',(199.937227483164,11.6624325651079,30.4738134026796));
#71933=CARTESIAN_POINT('Ctrl Pts',(199.936832263503,11.667272907289,30.4705031259178));
#71934=CARTESIAN_POINT('Ctrl Pts',(199.935737450634,11.6806881675051,30.4611807058516));
#71935=CARTESIAN_POINT('Ctrl Pts',(199.935042781223,11.689208156398,30.455089978089));
#71936=CARTESIAN_POINT('Ctrl Pts',(199.930451061393,11.745476315257,30.4137201443066));
#71937=CARTESIAN_POINT('Ctrl Pts',(199.926748257664,11.7905854465486,30.3749833486178));
#71938=CARTESIAN_POINT('Ctrl Pts',(199.917708597861,11.8936836504557,30.271937123872));
#71939=CARTESIAN_POINT('Ctrl Pts',(199.912405460425,11.947872198007,30.2043394197111));
#71940=CARTESIAN_POINT('Ctrl Pts',(199.905657626896,12.0036306981697,30.1165477964377));
#71941=CARTESIAN_POINT('Ctrl Pts',(199.904503353043,12.0127452620131,30.1014588480852));
#71942=CARTESIAN_POINT('Ctrl Pts',(199.902650331012,12.0266834851289,30.0771687997558));
#71943=CARTESIAN_POINT('Ctrl Pts',(199.90195948037,12.0317301592159,30.0680982918493));
#71944=CARTESIAN_POINT('Ctrl Pts',(199.900649718098,12.041012559231,30.0508830813142));
#71945=CARTESIAN_POINT('Ctrl Pts',(199.9000317723,12.0452742518778,30.0427532109555));
#71946=CARTESIAN_POINT('Ctrl Pts',(199.898619773821,12.054742987249,30.0241648339521));
#71947=CARTESIAN_POINT('Ctrl Pts',(199.897823741306,12.0598902430807,30.0136771340245));
#71948=CARTESIAN_POINT('Ctrl Pts',(199.895308197414,12.0755551712255,29.9805211379587));
#71949=CARTESIAN_POINT('Ctrl Pts',(199.893570135963,12.0855073505922,29.9575949316584));
#71950=CARTESIAN_POINT('Ctrl Pts',(199.889332081664,12.1076935040541,29.9016803379145));
#71951=CARTESIAN_POINT('Ctrl Pts',(199.886812016899,12.1191928487818,29.8684277315629));
#71952=CARTESIAN_POINT('Ctrl Pts',(199.883165679721,12.1334893397921,29.8201971280844));
#71953=CARTESIAN_POINT('Ctrl Pts',(199.882063362434,12.1375117107615,29.8056000228924));
#71954=CARTESIAN_POINT('Ctrl Pts',(199.875902082689,12.1583532616546,29.7238433338055));
#71955=CARTESIAN_POINT('Ctrl Pts',(199.870779935361,12.1695068147498,29.655378487046));
#71956=CARTESIAN_POINT('Ctrl Pts',(199.864401991586,12.1760441257028,29.566432527908));
#71957=CARTESIAN_POINT('Ctrl Pts',(199.862991203876,12.1770007859915,29.5465008095379));
#71958=CARTESIAN_POINT('Ctrl Pts',(199.861067296549,12.1776244839142,29.5188440315771));
#71959=CARTESIAN_POINT('Ctrl Pts',(199.860534530294,12.1777226257001,29.511133170358));
#71960=CARTESIAN_POINT('Ctrl Pts',(199.85964663371,12.1777602419313,29.4981855146602));
#71961=CARTESIAN_POINT('Ctrl Pts',(199.859289391478,12.1777405359075,29.4929491661793));
#71962=CARTESIAN_POINT('Ctrl Pts',(199.858543090051,12.1776257827794,29.4819504014819));
#71963=CARTESIAN_POINT('Ctrl Pts',(199.858154423026,12.1775233663272,29.4761882902396));
#71964=CARTESIAN_POINT('Ctrl Pts',(199.857097505559,12.177127651999,29.4604338590818));
#71965=CARTESIAN_POINT('Ctrl Pts',(199.856433639937,12.176749420163,29.4504439012595));
#71966=CARTESIAN_POINT('Ctrl Pts',(199.851545895265,12.1729965837153,29.3763051770765));
#71967=CARTESIAN_POINT('Ctrl Pts',(199.847553950856,12.1645054653802,29.3125150579678));
#71968=CARTESIAN_POINT('Ctrl Pts',(199.838517384869,12.1335135283684,29.1700010745316));
#71969=CARTESIAN_POINT('Ctrl Pts',(199.833492592613,12.1079397550879,29.092299040243));
#71970=CARTESIAN_POINT('Ctrl Pts',(199.827033682706,12.0671543785838,29.0013996059917));
#71971=CARTESIAN_POINT('Ctrl Pts',(199.825852529094,12.059388569559,28.985105230375));
#71972=CARTESIAN_POINT('Ctrl Pts',(199.823966332002,12.046531021037,28.9596505628223));
#71973=CARTESIAN_POINT('Ctrl Pts',(199.823269690646,12.0416860091204,28.9503683606677));
#71974=CARTESIAN_POINT('Ctrl Pts',(199.821960937804,12.0324099275392,28.9331603097828));
#71975=CARTESIAN_POINT('Ctrl Pts',(199.821349936308,12.028009681516,28.9252186678836));
#71976=CARTESIAN_POINT('Ctrl Pts',(199.819957867093,12.017830520482,28.9073379873598));
#71977=CARTESIAN_POINT('Ctrl Pts',(199.819174914375,12.011997079214,28.8974312278221));
#71978=CARTESIAN_POINT('Ctrl Pts',(199.816746720231,11.9935806748748,28.8671771107269));
#71979=CARTESIAN_POINT('Ctrl Pts',(199.815084732947,11.9805227365437,28.8471275865045));
#71980=CARTESIAN_POINT('Ctrl Pts',(199.811077678076,11.9479938742955,28.8003609578919));
#71981=CARTESIAN_POINT('Ctrl Pts',(199.808715417237,11.9279915437114,28.7740395622481));
#71982=CARTESIAN_POINT('Ctrl Pts',(199.802960947675,11.8772233166769,28.7127646414821));
#71983=CARTESIAN_POINT('Ctrl Pts',(199.799545741574,11.8454399328425,28.678725862665));
#71984=CARTESIAN_POINT('Ctrl Pts',(199.792272262698,11.7735420299162,28.610334106438));
#71985=CARTESIAN_POINT('Ctrl Pts',(199.788422908465,11.7329572433049,28.5766109492801));
#71986=CARTESIAN_POINT('Ctrl Pts',(199.783825097849,11.6801211500669,28.5383938194425));
#71987=CARTESIAN_POINT('Ctrl Pts',(199.782951856447,11.6698793142148,28.531231214252));
#71988=CARTESIAN_POINT('Ctrl Pts',(199.781654723862,11.6543258983543,28.520718600387));
#71989=CARTESIAN_POINT('Ctrl Pts',(199.781223597971,11.6490987206393,28.5172460652825));
#71990=CARTESIAN_POINT('Ctrl Pts',(199.780445546479,11.6395555313057,28.511015665795));
#71991=CARTESIAN_POINT('Ctrl Pts',(199.780097779787,11.635249068207,28.5082440249216));
#71992=CARTESIAN_POINT('Ctrl Pts',(199.779293790955,11.625199002952,28.5018681235561));
#71993=CARTESIAN_POINT('Ctrl Pts',(199.778838918562,11.6194421755478,28.4982852538323));
#71994=CARTESIAN_POINT('Ctrl Pts',(199.777370032423,11.6006342194411,28.4868039176794));
#71995=CARTESIAN_POINT('Ctrl Pts',(199.77636779531,11.5874599505852,28.479108906149));
#71996=CARTESIAN_POINT('Ctrl Pts',(199.769774328673,11.4988182136531,28.4296182046935));
#71997=CARTESIAN_POINT('Ctrl Pts',(199.764541619873,11.4190965963708,28.3959627259269));
#71998=CARTESIAN_POINT('Ctrl Pts',(199.755646199711,11.2821190671527,28.3551363638869));
#71999=CARTESIAN_POINT('Ctrl Pts',(199.752076847629,11.2267418117348,28.3428954407303));
#72000=CARTESIAN_POINT('Ctrl Pts',(199.747382107985,11.1555138718028,28.332461497422));
#72001=CARTESIAN_POINT('Ctrl Pts',(199.746372662018,11.1402834036833,28.3305337752308));
#72002=CARTESIAN_POINT('Ctrl Pts',(199.744702847601,11.1152608433243,28.3278624951988));
#72003=CARTESIAN_POINT('Ctrl Pts',(199.744047937266,11.1054891427547,28.3269427025056));
#72004=CARTESIAN_POINT('Ctrl Pts',(199.742761300309,11.086381992349,28.3253848486058));
#72005=CARTESIAN_POINT('Ctrl Pts',(199.742129965509,11.0770481642694,28.3247357002585));
#72006=CARTESIAN_POINT('Ctrl Pts',(199.740615801925,11.0547682943337,28.3234527281501));
#72007=CARTESIAN_POINT('Ctrl Pts',(199.739729905026,11.041817818214,28.3229212872685));
#72008=CARTESIAN_POINT('Ctrl Pts',(199.736535022065,10.9954336900868,28.3217842681858));
#72009=CARTESIAN_POINT('Ctrl Pts',(199.73419010338,10.961989098956,28.3223888759115));
#72010=CARTESIAN_POINT('Ctrl Pts',(199.727859480885,10.8732788271546,28.3277753887231));
#72011=CARTESIAN_POINT('Ctrl Pts',(199.723814512345,10.8182506426103,28.335038660732));
#72012=CARTESIAN_POINT('Ctrl Pts',(199.715064151226,10.701318257272,28.3589608407561));
#72013=CARTESIAN_POINT('Ctrl Pts',(199.710365728278,10.6398347666837,28.3768510827219));
#72014=CARTESIAN_POINT('Ctrl Pts',(199.705011044746,10.5688344197503,28.4039449013017));
#72015=CARTESIAN_POINT('Ctrl Pts',(199.704168586191,10.5576319123567,28.4084181021858));
#72016=CARTESIAN_POINT('Ctrl Pts',(199.702902311584,10.5407176843702,28.4154751884102));
#72017=CARTESIAN_POINT('Ctrl Pts',(199.702471911415,10.53495495981,28.4179337231796));
#72018=CARTESIAN_POINT('Ctrl Pts',(199.701691155641,10.5244714138408,28.4225055114323));
#72019=CARTESIAN_POINT('Ctrl Pts',(199.701340005253,10.5197446566767,28.4246039723967));
#72020=CARTESIAN_POINT('Ctrl Pts',(199.700529794802,10.5088130857615,28.4295435351708));
#72021=CARTESIAN_POINT('Ctrl Pts',(199.700072088676,10.5026189374618,28.4324075159445));
#72022=CARTESIAN_POINT('Ctrl Pts',(199.698583625748,10.4824292699813,28.4419564511522));
#72023=CARTESIAN_POINT('Ctrl Pts',(199.697565084639,10.4685402440131,28.448864331169));
#72024=CARTESIAN_POINT('Ctrl Pts',(199.695079082979,10.4345917577724,28.4665940423286));
#72025=CARTESIAN_POINT('Ctrl Pts',(199.693625696691,10.4147017799682,28.4777277918263));
#72026=CARTESIAN_POINT('Ctrl Pts',(199.68640322336,10.3164917610084,28.5365092977627));
#72027=CARTESIAN_POINT('Ctrl Pts',(199.680866458342,10.243601968728,28.5926076013548));
#72028=CARTESIAN_POINT('Ctrl Pts',(199.672973748462,10.1544869445651,28.6794656843314));
#72029=CARTESIAN_POINT('Ctrl Pts',(199.670866626089,10.1319868811555,28.7033056873993));
#72030=CARTESIAN_POINT('Ctrl Pts',(199.667852870047,10.1018539577391,28.7380267647443));
#72031=CARTESIAN_POINT('Ctrl Pts',(199.666980677835,10.093365314467,28.7481469234929));
#72032=CARTESIAN_POINT('Ctrl Pts',(199.665482419578,10.0791894484271,28.7656366117744));
#72033=CARTESIAN_POINT('Ctrl Pts',(199.66485982243,10.0734159930168,28.7729348533236));
#72034=CARTESIAN_POINT('Ctrl Pts',(199.663579900077,10.0617898714637,28.7879948723523));
#72035=CARTESIAN_POINT('Ctrl Pts',(199.662922314758,10.0559456202391,28.7957622095911));
#72036=CARTESIAN_POINT('Ctrl Pts',(199.661248224565,10.041396265763,28.8156057149122));
#72037=CARTESIAN_POINT('Ctrl Pts',(199.660226860244,10.0328229620318,28.8277759308807));
#72038=CARTESIAN_POINT('Ctrl Pts',(199.655493041924,9.99448745120509,28.8844469754947));
#72039=CARTESIAN_POINT('Ctrl Pts',(199.651680627031,9.96755429819227,28.9307764298256));
#72040=CARTESIAN_POINT('Ctrl Pts',(199.646579384302,9.93642719480184,28.9938472524547));
#72041=CARTESIAN_POINT('Ctrl Pts',(199.645354115873,9.92931052038818,29.00908072912));
#72042=CARTESIAN_POINT('Ctrl Pts',(199.638720905804,9.89266968857507,29.0921016198844));
#72043=CARTESIAN_POINT('Ctrl Pts',(199.633248825515,9.86925131248244,29.1624056170936));
#72044=CARTESIAN_POINT('Ctrl Pts',(199.626948458616,9.84920719905091,29.2490127335935));
#72045=CARTESIAN_POINT('Ctrl Pts',(199.625899112991,9.84611303482275,29.2636451809904));
#72046=CARTESIAN_POINT('Ctrl Pts',(199.624402282262,9.84204523038445,29.2848718169007));
#72047=CARTESIAN_POINT('Ctrl Pts',(199.623943932103,9.84084765031514,29.2914209524009));
#72048=CARTESIAN_POINT('Ctrl Pts',(199.623135117246,9.83881914602302,29.3030715961609));
#72049=CARTESIAN_POINT('Ctrl Pts',(199.622783503396,9.83796617913246,29.30816889108));
#72050=CARTESIAN_POINT('Ctrl Pts',(199.622007021387,9.83614694049944,29.3194982418318));
#72051=CARTESIAN_POINT('Ctrl Pts',(199.621583042447,9.83519713262357,29.3257326380603));
#72052=CARTESIAN_POINT('Ctrl Pts',(199.620315836725,9.83249193071049,29.3445003938163));
#72053=CARTESIAN_POINT('Ctrl Pts',(199.619480336357,9.83088836259479,29.3570551510618));
#72054=CARTESIAN_POINT('Ctrl Pts',(199.61752747636,9.82758058984638,29.3867545145573));
#72055=CARTESIAN_POINT('Ctrl Pts',(199.616417514124,9.82604953525392,29.4039157677796));
#72056=CARTESIAN_POINT('Ctrl Pts',(199.612204174843,9.82162415768627,29.4698299452879));
#72057=CARTESIAN_POINT('Ctrl Pts',(199.609182308378,9.82138630290501,29.5187140941237));
#72058=CARTESIAN_POINT('Ctrl Pts',(199.601527794205,9.82846865458007,29.6421317640584));
#72059=CARTESIAN_POINT('Ctrl Pts',(199.596900409197,9.83985272435551,29.7162033669141));
#72060=CARTESIAN_POINT('Ctrl Pts',(199.590869040678,9.86266910193541,29.8064454557614));
#72061=CARTESIAN_POINT('Ctrl Pts',(199.589671136954,9.86757098146807,29.8240908039078));
#72062=CARTESIAN_POINT('Ctrl Pts',(199.587764275473,9.8759353353345,29.8516880753779));
#72063=CARTESIAN_POINT('Ctrl Pts',(199.587064041173,9.87912349578678,29.861720504168));
#72064=CARTESIAN_POINT('Ctrl Pts',(199.585746348149,9.88533658157581,29.8804003556873));
#72065=CARTESIAN_POINT('Ctrl Pts',(199.585129988859,9.88832877135777,29.8890578855812));
#72066=CARTESIAN_POINT('Ctrl Pts',(199.583735050144,9.89529106062368,29.9084660901051));
#72067=CARTESIAN_POINT('Ctrl Pts',(199.582954676595,9.89931765584436,29.9191953587669));
#72068=CARTESIAN_POINT('Ctrl Pts',(199.580543419739,9.91215639220565,29.9519445045687));
#72069=CARTESIAN_POINT('Ctrl Pts',(199.578896129357,9.92147714930142,29.9737571875917));
#72070=CARTESIAN_POINT('Ctrl Pts',(199.57493308673,9.94517747832428,30.0248906673563));
#72071=CARTESIAN_POINT('Ctrl Pts',(199.572600660517,9.96012997004526,30.0539230839233));
#72072=CARTESIAN_POINT('Ctrl Pts',(199.564915632292,10.0126960117582,30.1463393717559));
#72073=CARTESIAN_POINT('Ctrl Pts',(199.559458413844,10.0550491246193,30.206816476863));
#72074=CARTESIAN_POINT('Ctrl Pts',(199.554117165109,10.1027690888331,30.2629362716156));
#72075=CARTESIAN_POINT('',(199.512132885214,9.82225014354375,29.5005814785295));
#72076=CARTESIAN_POINT('Ctrl Pts',(199.456018641859,10.1027690874833,30.2629362700282));
#72077=CARTESIAN_POINT('Ctrl Pts',(199.459191357844,10.0722980428734,30.2271016082947));
#72078=CARTESIAN_POINT('Ctrl Pts',(199.462364073829,10.0440019616846,30.1894679089783));
#72079=CARTESIAN_POINT('Ctrl Pts',(199.465536789815,10.018083504747,30.150334574546));
#72080=CARTESIAN_POINT('Ctrl Pts',(199.468715460125,9.99211640591272,30.1111277974852));
#72081=CARTESIAN_POINT('Ctrl Pts',(199.471894130436,9.96853612074149,30.0704162483886));
#72082=CARTESIAN_POINT('Ctrl Pts',(199.475072800746,9.94750007695886,30.0285252827428));
#72083=CARTESIAN_POINT('Ctrl Pts',(199.476946210262,9.93510208636799,30.0038360491928));
#72084=CARTESIAN_POINT('Ctrl Pts',(199.478819619778,9.92358695319116,29.9787375612637));
#72085=CARTESIAN_POINT('Ctrl Pts',(199.480693029294,9.91297891505301,29.9532992647034));
#72086=CARTESIAN_POINT('Ctrl Pts',(199.484218641163,9.8930154074229,29.9054263573039));
#72087=CARTESIAN_POINT('Ctrl Pts',(199.487744253032,9.87619275675429,29.8561715335063));
#72088=CARTESIAN_POINT('Ctrl Pts',(199.491269864901,9.86268036845629,29.805939729694));
#72089=CARTESIAN_POINT('Ctrl Pts',(199.494773776819,9.8492511481827,29.7560170999371));
#72090=CARTESIAN_POINT('Ctrl Pts',(199.498277688736,9.83909172096559,29.70512978883));
#72091=CARTESIAN_POINT('Ctrl Pts',(199.501781600653,9.83232178947454,29.6536966465609));
#72092=CARTESIAN_POINT('Ctrl Pts',(199.50523202884,9.82565519425427,29.6030485800527));
#72093=CARTESIAN_POINT('Ctrl Pts',(199.508682457027,9.82227546647417,29.5518715540156));
#72094=CARTESIAN_POINT('Ctrl Pts',(199.512132885214,9.82225014354375,29.5005814785295));
#72095=CARTESIAN_POINT('Ctrl Pts',(199.512132885264,9.82225014354338,29.5005814777886));
#72096=CARTESIAN_POINT('Ctrl Pts',(199.515343406687,9.82222658133527,29.4528575788382));
#72097=CARTESIAN_POINT('Ctrl Pts',(199.518553928109,9.82510810646364,29.4051355189712));
#72098=CARTESIAN_POINT('Ctrl Pts',(199.521764449532,9.83086776361372,29.3577858082243));
#72099=CARTESIAN_POINT('Ctrl Pts',(199.524979232366,9.83663506571088,29.3103732489391));
#72100=CARTESIAN_POINT('Ctrl Pts',(199.5281940152,9.84528806402763,29.2633345593417));
#72101=CARTESIAN_POINT('Ctrl Pts',(199.531408798033,9.85674805959125,29.2170334591306));
#72102=CARTESIAN_POINT('Ctrl Pts',(199.534625630782,9.86821536265037,29.1707028349044));
#72103=CARTESIAN_POINT('Ctrl Pts',(199.53784246353,9.8824930695955,29.1251112500719));
#72104=CARTESIAN_POINT('Ctrl Pts',(199.541059296278,9.89945259428958,29.0806070216562));
#72105=CARTESIAN_POINT('Ctrl Pts',(199.544283566842,9.91645133203196,29.0359998925703));
#72106=CARTESIAN_POINT('Ctrl Pts',(199.547507837406,9.93614405904267,28.9924856352886));
#72107=CARTESIAN_POINT('Ctrl Pts',(199.55073210797,9.95835447491095,28.950391355088));
#72108=CARTESIAN_POINT('Ctrl Pts',(199.553603047989,9.97813097024559,28.9129099616311));
#72109=CARTESIAN_POINT('Ctrl Pts',(199.556473988009,9.99990278314456,28.8765542520836));
#72110=CARTESIAN_POINT('Ctrl Pts',(199.559344928028,10.0235170635946,28.8415350142877));
#72111=CARTESIAN_POINT('Ctrl Pts',(199.562622090476,10.0504726365378,28.8015607444461));
#72112=CARTESIAN_POINT('Ctrl Pts',(199.565899252923,10.0799476785143,28.7631542676721));
#72113=CARTESIAN_POINT('Ctrl Pts',(199.56917641537,10.1117307368903,28.7266483473124));
#72114=CARTESIAN_POINT('Ctrl Pts',(199.572350409119,10.1425132294368,28.691291673701));
#72115=CARTESIAN_POINT('Ctrl Pts',(199.575524402868,10.1754601677577,28.6577181154801));
#72116=CARTESIAN_POINT('Ctrl Pts',(199.578698396617,10.2103356226518,28.6262006902914));
#72117=CARTESIAN_POINT('Ctrl Pts',(199.581869266297,10.245176750663,28.5947142867759));
#72118=CARTESIAN_POINT('Ctrl Pts',(199.585040135978,10.2819422266949,28.5652803821609));
#72119=CARTESIAN_POINT('Ctrl Pts',(199.588211005658,10.3203588108115,28.5381357078785));
#72120=CARTESIAN_POINT('Ctrl Pts',(199.591380145721,10.3587544398008,28.5110058402249));
#72121=CARTESIAN_POINT('Ctrl Pts',(199.594549285785,10.3987989386431,28.486163049911));
#72122=CARTESIAN_POINT('Ctrl Pts',(199.597718425848,10.4401876200514,28.4638025469264));
#72123=CARTESIAN_POINT('Ctrl Pts',(199.600887227748,10.4815718850841,28.4414444299173));
#72124=CARTESIAN_POINT('Ctrl Pts',(199.604056029649,10.5242995572051,28.4215683368624));
#72125=CARTESIAN_POINT('Ctrl Pts',(199.60722483155,10.5680411049611,28.4043236903644));
#72126=CARTESIAN_POINT('Ctrl Pts',(199.610396820559,10.6118266469678,28.3870616995943));
#72127=CARTESIAN_POINT('Ctrl Pts',(199.613568809568,10.6566275796872,28.3724366387231));
#72128=CARTESIAN_POINT('Ctrl Pts',(199.616740798577,10.702096002898,28.3605491362017));
#72129=CARTESIAN_POINT('Ctrl Pts',(199.619914732898,10.7475923109004,28.3486543433345));
#72130=CARTESIAN_POINT('Ctrl Pts',(199.623088667219,10.7937563777182,28.3395005579516));
#72131=CARTESIAN_POINT('Ctrl Pts',(199.62626260154,10.8402303732158,28.3331372279239));
#72132=CARTESIAN_POINT('Ctrl Pts',(199.629442151318,10.8867865924598,28.3267626396251));
#72133=CARTESIAN_POINT('Ctrl Pts',(199.632621701097,10.933653279433,28.3231883931202));
#72134=CARTESIAN_POINT('Ctrl Pts',(199.635801250876,10.9804697299899,28.3224119433973));
#72135=CARTESIAN_POINT('Ctrl Pts',(199.636533109505,10.9912457912878,28.3222332226761));
#72136=CARTESIAN_POINT('Ctrl Pts',(199.637264968134,11.0020192069751,28.3222025154569));
#72137=CARTESIAN_POINT('Ctrl Pts',(199.637996826763,11.0127856191094,28.322319402196));
#72138=CARTESIAN_POINT('Ctrl Pts',(199.64127398921,11.0609961342868,28.3228428049635));
#72139=CARTESIAN_POINT('Ctrl Pts',(199.644551151657,11.1092832441449,28.3263326393911));
#72140=CARTESIAN_POINT('Ctrl Pts',(199.647828314105,11.1572527280681,28.3327953726895));
#72141=CARTESIAN_POINT('Ctrl Pts',(199.651002230128,11.2037109418765,28.3390544987172));
#72142=CARTESIAN_POINT('Ctrl Pts',(199.654176146152,11.2498706479703,28.3481018880395));
#72143=CARTESIAN_POINT('Ctrl Pts',(199.657350062175,11.2953740813938,28.3598907006165));
#72144=CARTESIAN_POINT('Ctrl Pts',(199.660520852732,11.340832705984,28.3716679043346));
#72145=CARTESIAN_POINT('Ctrl Pts',(199.663691643288,11.3856358003685,28.3861810487819));
#72146=CARTESIAN_POINT('Ctrl Pts',(199.666862433845,11.4294353779103,28.4033321748592));
#72147=CARTESIAN_POINT('Ctrl Pts',(199.670031493551,11.4732110464232,28.4204739385913));
#72148=CARTESIAN_POINT('Ctrl Pts',(199.673200553257,11.5159837656456,28.4402506284899));
#72149=CARTESIAN_POINT('Ctrl Pts',(199.676369612963,11.5574229250327,28.4625151831723));
#72150=CARTESIAN_POINT('Ctrl Pts',(199.679538333435,11.598857648546,28.4847773545353));
#72151=CARTESIAN_POINT('Ctrl Pts',(199.682707053908,11.6389586064701,28.5095265965194));
#72152=CARTESIAN_POINT('Ctrl Pts',(199.68587577438,11.6774197595813,28.5365699133674));
#72153=CARTESIAN_POINT('Ctrl Pts',(199.689047680989,11.7159195852349,28.5636404221673));
#72154=CARTESIAN_POINT('Ctrl Pts',(199.692219587598,11.7527758612525,28.5930092857949));
#72155=CARTESIAN_POINT('Ctrl Pts',(199.695391494207,11.7877131930823,28.6244413280973));
#72156=CARTESIAN_POINT('Ctrl Pts',(199.698565345474,11.822671944569,28.6558926410058));
#72157=CARTESIAN_POINT('Ctrl Pts',(199.70173919674,11.8557090198283,28.6894092530028));
#72158=CARTESIAN_POINT('Ctrl Pts',(199.704913048007,11.8865863041646,28.7247195425088));
#72159=CARTESIAN_POINT('Ctrl Pts',(199.7080925146,11.9175182180377,28.7600923046319));
#72160=CARTESIAN_POINT('Ctrl Pts',(199.711271981192,11.9462823814283,28.7972646323191));
#72161=CARTESIAN_POINT('Ctrl Pts',(199.714451447785,11.9726825192878,28.8359339045155));
#72162=CARTESIAN_POINT('Ctrl Pts',(199.715183873689,11.9787640880893,28.8448418064598));
#72163=CARTESIAN_POINT('Ctrl Pts',(199.715916299593,11.9847203975814,28.8538290392186));
#72164=CARTESIAN_POINT('Ctrl Pts',(199.716648725497,11.9905493962399,28.8628917234028));
#72165=CARTESIAN_POINT('Ctrl Pts',(199.719925887944,12.0166306358653,28.9034417478069));
#72166=CARTESIAN_POINT('Ctrl Pts',(199.723203050392,12.0402766244894,28.9456874097543));
#72167=CARTESIAN_POINT('Ctrl Pts',(199.726480212839,12.061265130975,28.9893030406625));
#72168=CARTESIAN_POINT('Ctrl Pts',(199.729654174801,12.0815926924885,29.031545180228));
#72169=CARTESIAN_POINT('Ctrl Pts',(199.732828136764,12.0994274112475,29.0750717343834));
#72170=CARTESIAN_POINT('Ctrl Pts',(199.736002098726,12.1146116179335,29.119558146798));
#72171=CARTESIAN_POINT('Ctrl Pts',(199.739172935786,12.1297808751082,29.1640007604066));
#72172=CARTESIAN_POINT('Ctrl Pts',(199.742343772845,12.1423046063959,29.2094008370208));
#72173=CARTESIAN_POINT('Ctrl Pts',(199.745514609904,12.1520732126151,29.2554138694147));
#72174=CARTESIAN_POINT('Ctrl Pts',(199.748683716579,12.1618364879259,29.301401791649));
#72175=CARTESIAN_POINT('Ctrl Pts',(199.751852823253,12.1688475013121,29.3480014631884));
#72176=CARTESIAN_POINT('Ctrl Pts',(199.755021929928,12.1730472183889,29.3948558801923));
#72177=CARTESIAN_POINT('Ctrl Pts',(199.75819069774,12.1772464864021,29.4417052871888));
#72178=CARTESIAN_POINT('Ctrl Pts',(199.761359465551,12.1786350075224,29.4888088310685));
#72179=CARTESIAN_POINT('Ctrl Pts',(199.764528233363,12.1772056241259,29.5358047626201));
#72180=CARTESIAN_POINT('Ctrl Pts',(199.767700187501,12.1757748034253,29.5828479505267));
#72181=CARTESIAN_POINT('Ctrl Pts',(199.77087214164,12.1715204436319,29.6297827528572));
#72182=CARTESIAN_POINT('Ctrl Pts',(199.774044095779,12.1644874693901,29.6762498117257));
#72183=CARTESIAN_POINT('Ctrl Pts',(199.777217994735,12.1574501830264,29.7227453609058));
#72184=CARTESIAN_POINT('Ctrl Pts',(199.780391893692,12.147631008309,29.7687720512951));
#72185=CARTESIAN_POINT('Ctrl Pts',(199.783565792648,12.1351258123785,29.8139816118375));
#72186=CARTESIAN_POINT('Ctrl Pts',(199.786745306692,12.1225984929426,29.8592711546497));
#72187=CARTESIAN_POINT('Ctrl Pts',(199.789924820736,12.1073758571237,29.9037401591285));
#72188=CARTESIAN_POINT('Ctrl Pts',(199.793104334781,12.0896026746266,29.9470582444677));
#72189=CARTESIAN_POINT('Ctrl Pts',(199.793836431264,12.0855103245924,29.9570324158379));
#72190=CARTESIAN_POINT('Ctrl Pts',(199.794568527748,12.0812829459443,29.9669456695963));
#72191=CARTESIAN_POINT('Ctrl Pts',(199.795300624231,12.0769226471017,29.976794163827));
#72192=CARTESIAN_POINT('Ctrl Pts',(199.798577786678,12.0574041711255,30.0208800407323));
#72193=CARTESIAN_POINT('Ctrl Pts',(199.801854949126,12.0351300999337,30.0638648594177));
#72194=CARTESIAN_POINT('Ctrl Pts',(199.805132111573,12.0102501699625,30.1053838919155));
#72195=CARTESIAN_POINT('Ctrl Pts',(199.808306067234,11.9861537768636,30.1455953768076));
#72196=CARTESIAN_POINT('Ctrl Pts',(199.811480022895,11.9596135441534,30.1844315167418));
#72197=CARTESIAN_POINT('Ctrl Pts',(199.814653978556,11.9308137911021,30.2215821150736));
#72198=CARTESIAN_POINT('Ctrl Pts',(199.81782480934,11.9020423924787,30.2586961372598));
#72199=CARTESIAN_POINT('Ctrl Pts',(199.820995640123,11.8710162164852,30.2941274644022));
#72200=CARTESIAN_POINT('Ctrl Pts',(199.824166470907,11.8379626851255,30.3275950705733));
#72201=CARTESIAN_POINT('Ctrl Pts',(199.827335571346,11.8049271913131,30.3610444132335));
#72202=CARTESIAN_POINT('Ctrl Pts',(199.830504671784,11.7698669245265,30.3925317623392));
#72203=CARTESIAN_POINT('Ctrl Pts',(199.833673772223,11.7330475563883,30.4218114463236));
#72204=CARTESIAN_POINT('Ctrl Pts',(199.836842533851,11.6962321246362,30.451087999995));
#72205=CARTESIAN_POINT('Ctrl Pts',(199.840011295479,11.6576584019286,30.4781570125518));
#72206=CARTESIAN_POINT('Ctrl Pts',(199.843180057106,11.6176245578356,30.5028135260648));
#72207=CARTESIAN_POINT('Ctrl Pts',(199.846352005186,11.5775504564012,30.5274948337414));
#72208=CARTESIAN_POINT('Ctrl Pts',(199.849523953266,11.5360137799205,30.5497585112635));
#72209=CARTESIAN_POINT('Ctrl Pts',(199.852695901346,11.4933393488691,30.5694444115322));
#72210=CARTESIAN_POINT('Ctrl Pts',(199.85586979431,11.450638751925,30.5891423822407));
#72211=CARTESIAN_POINT('Ctrl Pts',(199.859043687275,11.40679953099,30.6062592279677));
#72212=CARTESIAN_POINT('Ctrl Pts',(199.862217580239,11.3621652685777,30.6206834435897));
#72213=CARTESIAN_POINT('Ctrl Pts',(199.865397088449,11.3174520393221,30.6351331785037));
#72214=CARTESIAN_POINT('Ctrl Pts',(199.868576596658,11.2719415022112,30.6468806455459));
#72215=CARTESIAN_POINT('Ctrl Pts',(199.871756104867,11.2259891979731,30.6558650201903));
#72216=CARTESIAN_POINT('Ctrl Pts',(199.872488244233,11.2154078474385,30.6579338352154));
#72217=CARTESIAN_POINT('Ctrl Pts',(199.873220383599,11.204803095393,30.6598563588498));
#72218=CARTESIAN_POINT('Ctrl Pts',(199.873952522965,11.194179310854,30.661632238592));
#72219=CARTESIAN_POINT('Ctrl Pts',(199.877229685412,11.1466257037727,30.669581334997));
#72220=CARTESIAN_POINT('Ctrl Pts',(199.88050684786,11.0984758947224,30.6746235145448));
#72221=CARTESIAN_POINT('Ctrl Pts',(199.883784010307,11.0501168424284,30.6766832048623));
#72222=CARTESIAN_POINT('Ctrl Pts',(199.886957958635,11.00328085683,30.6786780253038));
#72223=CARTESIAN_POINT('Ctrl Pts',(199.890131906963,10.9562492181484,30.6778754238886));
#72224=CARTESIAN_POINT('Ctrl Pts',(199.893305855292,10.909382364626,30.6742587051665));
#72225=CARTESIAN_POINT('Ctrl Pts',(199.896476678598,10.8625616555079,30.6706455474116));
#72226=CARTESIAN_POINT('Ctrl Pts',(199.899647501904,10.8159059631852,30.6642237993453));
#72227=CARTESIAN_POINT('Ctrl Pts',(199.90281832521,10.7697750735935,30.6550288073295));
#72228=CARTESIAN_POINT('Ctrl Pts',(199.905987418042,10.7236693598957,30.6458388334729));
#72229=CARTESIAN_POINT('Ctrl Pts',(199.909156510874,10.6780884267301,30.6338787226884));
#72230=CARTESIAN_POINT('Ctrl Pts',(199.912325603706,10.6333835740681,30.6192352115337));
#72231=CARTESIAN_POINT('Ctrl Pts',(199.915494357613,10.5886835024526,30.6045932664576));
#72232=CARTESIAN_POINT('Ctrl Pts',(199.91866311152,10.5448598534815,30.5872686661981));
#72233=CARTESIAN_POINT('Ctrl Pts',(199.921831865428,10.5022478017002,30.5673976820228));
#72234=CARTESIAN_POINT('Ctrl Pts',(199.925003805676,10.4595929013577,30.5475067165736));
#72235=CARTESIAN_POINT('Ctrl Pts',(199.928175745925,10.4181525336127,30.5250644958841));
#72236=CARTESIAN_POINT('Ctrl Pts',(199.931347686174,10.3782391096656,30.5002541965673));
#72237=CARTESIAN_POINT('Ctrl Pts',(199.934521571235,10.3383012135965,30.4754286853091));
#72238=CARTESIAN_POINT('Ctrl Pts',(199.937695456295,10.2998925788117,30.4482325280295));
#72239=CARTESIAN_POINT('Ctrl Pts',(199.940869341356,10.2632953143319,30.4188913257914));
#72240=CARTESIAN_POINT('Ctrl Pts',(199.944048841634,10.226633302209,30.3894982132885));
#72241=CARTESIAN_POINT('Ctrl Pts',(199.947228341911,10.1917894624995,30.3579528618704));
#72242=CARTESIAN_POINT('Ctrl Pts',(199.950407842189,10.1590101570364,30.3245187363136));
#72243=CARTESIAN_POINT('Ctrl Pts',(199.951140035359,10.1514615545856,30.316819338216));
#72244=CARTESIAN_POINT('Ctrl Pts',(199.951872228529,10.1440222683806,30.3090199139201));
#72245=CARTESIAN_POINT('Ctrl Pts',(199.9526044217,10.1366949965981,30.3011239190046));
#72246=CARTESIAN_POINT('Ctrl Pts',(199.953760862746,10.1251221519025,30.2886528212227));
#72247=CARTESIAN_POINT('Ctrl Pts',(199.954917303793,10.1138091790481,30.275919676137));
#72248=CARTESIAN_POINT('Ctrl Pts',(199.956073744839,10.1027690874833,30.2629362700282));
#72249=CARTESIAN_POINT('Origin',(197.762132885264,11.,29.5));
#72250=CARTESIAN_POINT('',(200.554352848915,10.1027690892854,30.2629362721474));
#72251=CARTESIAN_POINT('',(200.456078305605,10.1027690874833,30.2629362700282));
#72252=CARTESIAN_POINT('',(197.762132885264,10.1027690874833,30.2629362700282));
#72253=CARTESIAN_POINT('Ctrl Pts',(200.554352848915,10.1027690892854,30.2629362721474));
#72254=CARTESIAN_POINT('Ctrl Pts',(200.554059484652,10.1058259895353,30.2665312583807));
#72255=CARTESIAN_POINT('Ctrl Pts',(200.553766388138,10.1089048112609,30.2701082428271));
#72256=CARTESIAN_POINT('Ctrl Pts',(200.550536613393,10.1430933772254,30.3093489769809));
#72257=CARTESIAN_POINT('Ctrl Pts',(200.547622714416,10.1763032051018,30.3431240866796));
#72258=CARTESIAN_POINT('Ctrl Pts',(200.541663360381,10.2470316592398,30.4068780928422));
#72259=CARTESIAN_POINT('Ctrl Pts',(200.538622129452,10.284528158526,30.4367435503193));
#72260=CARTESIAN_POINT('Ctrl Pts',(200.534546714256,10.3355883625495,30.4725542788059));
#72261=CARTESIAN_POINT('Ctrl Pts',(200.533593209763,10.3475928104203,30.4806474792247));
#72262=CARTESIAN_POINT('Ctrl Pts',(200.531991325723,10.3678328268368,30.4937568255723));
#72263=CARTESIAN_POINT('Ctrl Pts',(200.531347530803,10.3759864869471,30.4988969363709));
#72264=CARTESIAN_POINT('Ctrl Pts',(200.530071145571,10.3921830518015,30.508831641037));
#72265=CARTESIAN_POINT('Ctrl Pts',(200.529438807578,10.4002218725936,30.5136315463267));
#72266=CARTESIAN_POINT('Ctrl Pts',(200.528030316431,10.4181551439961,30.5240513141878));
#72267=CARTESIAN_POINT('Ctrl Pts',(200.52725259088,10.4280754301327,30.5296245924175));
#72268=CARTESIAN_POINT('Ctrl Pts',(200.524500533615,10.4632316690618,30.5487107465772));
#72269=CARTESIAN_POINT('Ctrl Pts',(200.522500074167,10.4888762817245,30.5614456076251));
#72270=CARTESIAN_POINT('Ctrl Pts',(200.51362607943,10.6029782446479,30.6130134453149));
#72271=CARTESIAN_POINT('Ctrl Pts',(200.506454714688,10.6955531740712,30.6418111902866));
#72272=CARTESIAN_POINT('Ctrl Pts',(200.497762726127,10.8133827237603,30.663101814847));
#72273=CARTESIAN_POINT('Ctrl Pts',(200.496094212026,10.836299920532,30.6665480040363));
#72274=CARTESIAN_POINT('Ctrl Pts',(200.49333594951,10.8748854424783,30.6711907070014));
#72275=CARTESIAN_POINT('Ctrl Pts',(200.492233486018,10.8905026494745,30.6727539009854));
#72276=CARTESIAN_POINT('Ctrl Pts',(200.490670876236,10.9129802633747,30.67455081439));
#72277=CARTESIAN_POINT('Ctrl Pts',(200.490198725757,10.9198180654875,30.675037409287));
#72278=CARTESIAN_POINT('Ctrl Pts',(200.489375793352,10.9318237647191,30.6757864739942));
#72279=CARTESIAN_POINT('Ctrl Pts',(200.489023685301,10.9369896891018,30.6760746301657));
#72280=CARTESIAN_POINT('Ctrl Pts',(200.488250947651,10.9483919839721,30.6766353028671));
#72281=CARTESIAN_POINT('Ctrl Pts',(200.487831147444,10.9546288206082,30.6768922991092));
#72282=CARTESIAN_POINT('Ctrl Pts',(200.486614880884,10.972811447002,30.6774967765295));
#72283=CARTESIAN_POINT('Ctrl Pts',(200.485825096764,10.9847612236144,30.6777120540833));
#72284=CARTESIAN_POINT('Ctrl Pts',(200.480719847098,11.0627675401348,30.6779297803596));
#72285=CARTESIAN_POINT('Ctrl Pts',(200.476634144649,11.1287292116464,30.6725567207702));
#72286=CARTESIAN_POINT('Ctrl Pts',(200.469192564894,11.2472661142624,30.6527714160568));
#72287=CARTESIAN_POINT('Ctrl Pts',(200.465847611633,11.2999541125762,30.6401971514624));
#72288=CARTESIAN_POINT('Ctrl Pts',(200.460322517995,11.3830554103551,30.6142040462825));
#72289=CARTESIAN_POINT('Ctrl Pts',(200.458201079678,11.4140927250099,30.6030453409429));
#72290=CARTESIAN_POINT('Ctrl Pts',(200.455191934823,11.4565635036614,30.5857307253838));
#72291=CARTESIAN_POINT('Ctrl Pts',(200.454339602688,11.4684266073093,30.5806655047578));
#72292=CARTESIAN_POINT('Ctrl Pts',(200.452858523142,11.4887374945339,30.5715960382333));
#72293=CARTESIAN_POINT('Ctrl Pts',(200.452232903481,11.4972253560091,30.5676841033738));
#72294=CARTESIAN_POINT('Ctrl Pts',(200.450941877531,11.5145474960536,30.5594492222673));
#72295=CARTESIAN_POINT('Ctrl Pts',(200.450276154236,11.5233759557368,30.5551158131519));
#72296=CARTESIAN_POINT('Ctrl Pts',(200.448554912339,11.5459297889911,30.5436926553971));
#72297=CARTESIAN_POINT('Ctrl Pts',(200.447493967628,11.5595714393206,30.5364426944096));
#72298=CARTESIAN_POINT('Ctrl Pts',(200.442242538002,11.6257974752286,30.499557767425));
#72299=CARTESIAN_POINT('Ctrl Pts',(200.437923038594,11.6761853521179,30.4661830165368));
#72300=CARTESIAN_POINT('Ctrl Pts',(200.42883944463,11.7745687285331,30.3895403135794));
#72301=CARTESIAN_POINT('Ctrl Pts',(200.424079664168,11.8220201767396,30.3458850447106));
#72302=CARTESIAN_POINT('Ctrl Pts',(200.417318014235,11.8854544436937,30.2771210679906));
#72303=CARTESIAN_POINT('Ctrl Pts',(200.415234360185,11.9044398138961,30.2549408238497));
#72304=CARTESIAN_POINT('Ctrl Pts',(200.412603185226,11.9278875828418,30.2253912902484));
#72305=CARTESIAN_POINT('Ctrl Pts',(200.412012102161,11.9331195537026,30.2186485924263));
#72306=CARTESIAN_POINT('Ctrl Pts',(200.411051445604,11.9415712626843,30.2075085220035));
#72307=CARTESIAN_POINT('Ctrl Pts',(200.410679063302,11.9448345036043,30.2031447331425));
#72308=CARTESIAN_POINT('Ctrl Pts',(200.409932988339,11.95134854785,30.1943065511501));
#72309=CARTESIAN_POINT('Ctrl Pts',(200.409559361796,11.9545983451369,30.1898316092028));
#72310=CARTESIAN_POINT('Ctrl Pts',(200.408588722835,11.9630042886497,30.1780835358305));
#72311=CARTESIAN_POINT('Ctrl Pts',(200.407994964603,11.9681096962672,30.1707743057543));
#72312=CARTESIAN_POINT('Ctrl Pts',(200.405379478221,11.9904053376091,30.1380695258264));
#72313=CARTESIAN_POINT('Ctrl Pts',(200.403408726568,12.006684276264,30.1120641797077));
#72314=CARTESIAN_POINT('Ctrl Pts',(200.394470734778,12.0768877995601,29.9895207559541));
#72315=CARTESIAN_POINT('Ctrl Pts',(200.387850735577,12.1180639048314,29.8863326711703));
#72316=CARTESIAN_POINT('Ctrl Pts',(200.379297611381,12.1495271515814,29.7572534919568));
#72317=CARTESIAN_POINT('Ctrl Pts',(200.377846476518,12.1541901879936,29.7354505049964));
#72318=CARTESIAN_POINT('Ctrl Pts',(200.375637595656,12.1602622130009,29.7025144725542));
#72319=CARTESIAN_POINT('Ctrl Pts',(200.37489421003,12.1621356091211,29.691471476532));
#72320=CARTESIAN_POINT('Ctrl Pts',(200.373594121891,12.1651162827878,29.6722420502311));
#72321=CARTESIAN_POINT('Ctrl Pts',(200.373039692123,12.1662954775799,29.6640674537552));
#72322=CARTESIAN_POINT('Ctrl Pts',(200.371781597606,12.168763960336,29.6455810895301));
#72323=CARTESIAN_POINT('Ctrl Pts',(200.371076423746,12.1700029250846,29.6352634171583));
#72324=CARTESIAN_POINT('Ctrl Pts',(200.369159853748,12.172980790786,29.6073488522191));
#72325=CARTESIAN_POINT('Ctrl Pts',(200.367940642929,12.1744601372346,29.5897275853987));
#72326=CARTESIAN_POINT('Ctrl Pts',(200.360731285625,12.180797446691,29.4863740249201));
#72327=CARTESIAN_POINT('Ctrl Pts',(200.354469390862,12.176663075435,29.4003635248952));
#72328=CARTESIAN_POINT('Ctrl Pts',(200.345119803961,12.1566965847986,29.2744234408662));
#72329=CARTESIAN_POINT('Ctrl Pts',(200.342068171672,12.1479907756377,29.233636905313));
#72330=CARTESIAN_POINT('Ctrl Pts',(200.337418516003,12.1311286470107,29.1710982197427));
#72331=CARTESIAN_POINT('Ctrl Pts',(200.335780275352,12.124461550279,29.148980368489));
#72332=CARTESIAN_POINT('Ctrl Pts',(200.33362271666,12.1146452335006,29.1195745401375));
#72333=CARTESIAN_POINT('Ctrl Pts',(200.333076321423,12.1120671593705,29.1121028891281));
#72334=CARTESIAN_POINT('Ctrl Pts',(200.3321688592,12.1076271853072,29.0996433903741));
#72335=CARTESIAN_POINT('Ctrl Pts',(200.331805548495,12.1058063585852,29.0946412721472));
#72336=CARTESIAN_POINT('Ctrl Pts',(200.331056641145,12.1019617983021,29.0842983368615));
#72337=CARTESIAN_POINT('Ctrl Pts',(200.330671332666,12.0999330360039,29.0789596250113));
#72338=CARTESIAN_POINT('Ctrl Pts',(200.329633725258,12.0943343148585,29.0645432134544));
#72339=CARTESIAN_POINT('Ctrl Pts',(200.328985546667,12.0906902022097,29.0554945404971));
#72340=CARTESIAN_POINT('Ctrl Pts',(200.325227415945,12.0687286541792,29.0028587695539));
#72341=CARTESIAN_POINT('Ctrl Pts',(200.322241596036,12.0479103028067,28.9603562586247));
#72342=CARTESIAN_POINT('Ctrl Pts',(200.314897515568,11.989840621697,28.8579125337905));
#72343=CARTESIAN_POINT('Ctrl Pts',(200.310592231576,11.9496600333001,28.7998524987611));
#72344=CARTESIAN_POINT('Ctrl Pts',(200.30374911846,11.8802257868761,28.7165857522622));
#72345=CARTESIAN_POINT('Ctrl Pts',(200.301318596926,11.8545285084103,28.6886333006805));
#72346=CARTESIAN_POINT('Ctrl Pts',(200.29794784292,11.8179118032228,28.6524753631909));
#72347=CARTESIAN_POINT('Ctrl Pts',(200.297055966734,11.808132521011,28.6431455596391));
#72348=CARTESIAN_POINT('Ctrl Pts',(200.295528130128,11.7912434285482,28.6275790694907));
#72349=CARTESIAN_POINT('Ctrl Pts',(200.294895849588,11.7842149666841,28.6212558276166));
#72350=CARTESIAN_POINT('Ctrl Pts',(200.293686178161,11.7706993722206,28.609387652039));
#72351=CARTESIAN_POINT('Ctrl Pts',(200.293109475068,11.7642265823042,28.603827248224));
#72352=CARTESIAN_POINT('Ctrl Pts',(200.291750832384,11.7489128106895,28.5909586217059));
#72353=CARTESIAN_POINT('Ctrl Pts',(200.290966653219,11.7400244840577,28.5837083584018));
#72354=CARTESIAN_POINT('Ctrl Pts',(200.288154721767,11.7079870230235,28.5583454217735));
#72355=CARTESIAN_POINT('Ctrl Pts',(200.286099247846,11.6842691113827,28.5409721088688));
#72356=CARTESIAN_POINT('Ctrl Pts',(200.277227087328,11.5806778014099,28.4708919783731));
#72357=CARTESIAN_POINT('Ctrl Pts',(200.270123378105,11.4951940370528,28.4271399972699));
#72358=CARTESIAN_POINT('Ctrl Pts',(200.261503013554,11.3836905564679,28.3862629228289));
#72359=CARTESIAN_POINT('Ctrl Pts',(200.259839497397,11.3617705403745,28.3789509744218));
#72360=CARTESIAN_POINT('Ctrl Pts',(200.257088480645,11.3246534169226,28.3677719003788));
#72361=CARTESIAN_POINT('Ctrl Pts',(200.255988343416,11.3095688863985,28.3635548969176));
#72362=CARTESIAN_POINT('Ctrl Pts',(200.254428391087,11.2877720155653,28.3579276543517));
#72363=CARTESIAN_POINT('Ctrl Pts',(200.253956625392,11.2811251306517,28.3562733533575));
#72364=CARTESIAN_POINT('Ctrl Pts',(200.253134107645,11.2694329730628,28.3534714568621));
#72365=CARTESIAN_POINT('Ctrl Pts',(200.252782034253,11.2643940425422,28.352298984503));
#72366=CARTESIAN_POINT('Ctrl Pts',(200.252009065786,11.2532546789339,28.349784306714));
#72367=CARTESIAN_POINT('Ctrl Pts',(200.251589003871,11.2471511015586,28.348457377758));
#72368=CARTESIAN_POINT('Ctrl Pts',(200.250346021303,11.2289519220059,28.3446522099588));
#72369=CARTESIAN_POINT('Ctrl Pts',(200.249530397407,11.216827190396,28.3423154587035));
#72370=CARTESIAN_POINT('Ctrl Pts',(200.24474517768,11.1447748205305,28.3296008657922));
#72371=CARTESIAN_POINT('Ctrl Pts',(200.240967562845,11.0841462033348,28.3236858254642));
#72372=CARTESIAN_POINT('Ctrl Pts',(200.233641070254,10.9659126413207,28.3213436918574));
#72373=CARTESIAN_POINT('Ctrl Pts',(200.230100217233,10.9084959559439,28.3244068691112));
#72374=CARTESIAN_POINT('Ctrl Pts',(200.224299513255,10.8176931991688,28.3359454746302));
#72375=CARTESIAN_POINT('Ctrl Pts',(200.222107010803,10.7840585707041,28.3417134707805));
#72376=CARTESIAN_POINT('Ctrl Pts',(200.219014367408,10.7379703431451,28.3516943787717));
#72377=CARTESIAN_POINT('Ctrl Pts',(200.218152394453,10.7252641177713,28.3546679460517));
#72378=CARTESIAN_POINT('Ctrl Pts',(200.216659989514,10.7035223417987,28.3601386570273));
#72379=CARTESIAN_POINT('Ctrl Pts',(200.216032818041,10.6944622083917,28.3625337225281));
#72380=CARTESIAN_POINT('Ctrl Pts',(200.214743513993,10.6759996462505,28.3676508340052));
#72381=CARTESIAN_POINT('Ctrl Pts',(200.214081118694,10.6666006641002,28.3703824824861));
#72382=CARTESIAN_POINT('Ctrl Pts',(200.212379103596,10.6426770114188,28.3776600529432));
#72383=CARTESIAN_POINT('Ctrl Pts',(200.211334291144,10.6282048007064,28.3823708273934));
#72384=CARTESIAN_POINT('Ctrl Pts',(200.206574812341,10.5632664386439,28.4049094352874));
#72385=CARTESIAN_POINT('Ctrl Pts',(200.202760872884,10.5139663428851,28.4258820225373));
#72386=CARTESIAN_POINT('Ctrl Pts',(200.193779476257,10.4036238081094,28.4819778498239));
#72387=CARTESIAN_POINT('Ctrl Pts',(200.188575777683,10.3439576472968,28.5193666753786));
#72388=CARTESIAN_POINT('Ctrl Pts',(200.181293474657,10.2637880328199,28.5802122679365));
#72389=CARTESIAN_POINT('Ctrl Pts',(200.179122409607,10.2403118078168,28.5995047399878));
#72390=CARTESIAN_POINT('Ctrl Pts',(200.176400085364,10.2111494432358,28.6254232593247));
#72391=CARTESIAN_POINT('Ctrl Pts',(200.175801625845,10.2047560700298,28.6312326093909));
#72392=CARTESIAN_POINT('Ctrl Pts',(200.174832111417,10.1944187612633,28.6408353710791));
#72393=CARTESIAN_POINT('Ctrl Pts',(200.174458152519,10.1904364411046,28.6445867436218));
#72394=CARTESIAN_POINT('Ctrl Pts',(200.173712081496,10.1824987047159,28.6521692305461));
#72395=CARTESIAN_POINT('Ctrl Pts',(200.173340003177,10.178543732005,28.6560006017263));
#72396=CARTESIAN_POINT('Ctrl Pts',(200.172378268231,10.1683357528672,28.6660292905499));
#72397=CARTESIAN_POINT('Ctrl Pts',(200.171791756353,10.1621249731353,28.6722693585008));
#72398=CARTESIAN_POINT('Ctrl Pts',(200.169251112088,10.1353193300328,28.6998123232013));
#72399=CARTESIAN_POINT('Ctrl Pts',(200.167344514041,10.115460908333,28.7218201460967));
#72400=CARTESIAN_POINT('Ctrl Pts',(200.158495843839,10.0258960167594,28.8289440453364));
#72401=CARTESIAN_POINT('Ctrl Pts',(200.151911736535,9.96750968453955,28.9227993651366));
#72402=CARTESIAN_POINT('Ctrl Pts',(200.143335232086,9.91350019737522,29.0448478671892));
#72403=CARTESIAN_POINT('Ctrl Pts',(200.141810497993,9.90465136893458,29.0665757907962));
#72404=CARTESIAN_POINT('Ctrl Pts',(200.139512529176,9.89247036635523,29.0992464166315));
#72405=CARTESIAN_POINT('Ctrl Pts',(200.138755506463,9.8886389324939,29.1099975812545));
#72406=CARTESIAN_POINT('Ctrl Pts',(200.13738194268,9.88201630167086,29.1294715159846));
#72407=CARTESIAN_POINT('Ctrl Pts',(200.136767261903,9.87916941976998,29.1381744762926));
#72408=CARTESIAN_POINT('Ctrl Pts',(200.135436551814,9.87325844172585,29.1569839081087));
#72409=CARTESIAN_POINT('Ctrl Pts',(200.134719493643,9.87022824179993,29.1671001046275));
#72410=CARTESIAN_POINT('Ctrl Pts',(200.132736268906,9.86227345488839,29.1950172635262));
#72411=CARTESIAN_POINT('Ctrl Pts',(200.131461340337,9.85763110275377,29.2128947970965));
#72412=CARTESIAN_POINT('Ctrl Pts',(200.125622547261,9.83849657413298,29.2944156284368));
#72413=CARTESIAN_POINT('Ctrl Pts',(200.120913255013,9.82889197068187,29.3590786040561));
#72414=CARTESIAN_POINT('Ctrl Pts',(200.112060591604,9.82110196841747,29.4798577113642));
#72415=CARTESIAN_POINT('Ctrl Pts',(200.107947611176,9.82147055730096,29.5357060292933));
#72416=CARTESIAN_POINT('Ctrl Pts',(200.101963292659,9.82790357899108,29.6184235878555));
#72417=CARTESIAN_POINT('Ctrl Pts',(200.100026127748,9.83094958728436,29.6454494678802));
#72418=CARTESIAN_POINT('Ctrl Pts',(200.097548956439,9.8361499669536,29.6806040431663));
#72419=CARTESIAN_POINT('Ctrl Pts',(200.096971191821,9.83745907640505,29.6888473740811));
#72420=CARTESIAN_POINT('Ctrl Pts',(200.096026483028,9.83976098287463,29.7024098591719));
#72421=CARTESIAN_POINT('Ctrl Pts',(200.095656900399,9.84070297915671,29.7077372121524));
#72422=CARTESIAN_POINT('Ctrl Pts',(200.094910526453,9.84269063863739,29.7185433854436));
#72423=CARTESIAN_POINT('Ctrl Pts',(200.09453386237,9.8437385715646,29.7240216095159));
#72424=CARTESIAN_POINT('Ctrl Pts',(200.093545795538,9.84660512033182,29.7384506948196));
#72425=CARTESIAN_POINT('Ctrl Pts',(200.092937864968,9.84848904711843,29.7473883996157));
#72426=CARTESIAN_POINT('Ctrl Pts',(200.09012203995,9.85776962934379,29.7890118634204));
#72427=CARTESIAN_POINT('Ctrl Pts',(200.087975361377,9.86645583806898,29.8213971653031));
#72428=CARTESIAN_POINT('Ctrl Pts',(200.080242527498,9.90323524412609,29.9383316047272));
#72429=CARTESIAN_POINT('Ctrl Pts',(200.074856723675,9.93950879472617,30.0199874612024));
#72430=CARTESIAN_POINT('Ctrl Pts',(200.066994980489,10.0024382620207,30.1270559970883));
#72431=CARTESIAN_POINT('Ctrl Pts',(200.064739712808,10.0215791908949,30.1565219082427));
#72432=CARTESIAN_POINT('Ctrl Pts',(200.061573506326,10.0496719137213,30.19580545931));
#72433=CARTESIAN_POINT('Ctrl Pts',(200.060703296898,10.0575162334201,30.2063943911513));
#72434=CARTESIAN_POINT('Ctrl Pts',(200.059201175609,10.0712537717106,30.2243022462663));
#72435=CARTESIAN_POINT('Ctrl Pts',(200.058572638595,10.0770600415176,30.2316864936288));
#72436=CARTESIAN_POINT('Ctrl Pts',(200.057284588891,10.0890719337397,30.2465923858502));
#72437=CARTESIAN_POINT('Ctrl Pts',(200.056624858235,10.0952838682443,30.2541079787803));
#72438=CARTESIAN_POINT('Ctrl Pts',(200.055920004199,10.101981501335,30.2620093230676));
#72439=CARTESIAN_POINT('Ctrl Pts',(200.055878603811,10.1023751159753,30.2624729503126));
#72440=CARTESIAN_POINT('Ctrl Pts',(200.055837189155,10.1027690874889,30.2629362700347));
#72441=CARTESIAN_POINT('',(200.012132885299,9.82225044682022,29.498974093169));
#72442=CARTESIAN_POINT('Ctrl Pts',(199.956073744839,10.1027690874833,30.2629362700282));
#72443=CARTESIAN_POINT('Ctrl Pts',(199.959213054861,10.0727993192846,30.2276911210882));
#72444=CARTESIAN_POINT('Ctrl Pts',(199.962352364883,10.0448431166944,30.1905990782524));
#72445=CARTESIAN_POINT('Ctrl Pts',(199.965491674906,10.0191369550365,30.1519223493062));
#72446=CARTESIAN_POINT('Ctrl Pts',(199.968626810549,9.99346497517818,30.1132970492826));
#72447=CARTESIAN_POINT('Ctrl Pts',(199.971761946192,9.97003743285672,30.0730917033196));
#72448=CARTESIAN_POINT('Ctrl Pts',(199.974897081835,9.94905028793591,30.0316011335695));
#72449=CARTESIAN_POINT('Ctrl Pts',(199.978030461699,9.92807489650514,29.9901337999004));
#72450=CARTESIAN_POINT('Ctrl Pts',(199.981163841563,9.90953747036862,29.9473831675551));
#72451=CARTESIAN_POINT('Ctrl Pts',(199.984297221427,9.89358899406756,29.9036703462623));
#72452=CARTESIAN_POINT('Ctrl Pts',(199.987429333019,9.87764697310161,29.859975218253));
#72453=CARTESIAN_POINT('Ctrl Pts',(199.99056144461,9.86429201741278,29.8153192114746));
#72454=CARTESIAN_POINT('Ctrl Pts',(199.993693556202,9.85362646241936,29.7700421723266));
#72455=CARTESIAN_POINT('Ctrl Pts',(199.996828401406,9.84295159885049,29.7247256167412));
#72456=CARTESIAN_POINT('Ctrl Pts',(199.99996324661,9.83497095675816,29.6787875038758));
#72457=CARTESIAN_POINT('Ctrl Pts',(200.003098091814,9.82973604293946,29.63257953577));
#72458=CARTESIAN_POINT('Ctrl Pts',(200.006109689631,9.82470694134145,29.5881882479113));
#72459=CARTESIAN_POINT('Ctrl Pts',(200.009121287447,9.82221161931003,29.5435484194516));
#72460=CARTESIAN_POINT('Ctrl Pts',(200.012132885264,9.82225044681977,29.498974093686));
#72461=CARTESIAN_POINT('Ctrl Pts',(200.012132885299,9.82225044682022,29.498974093169));
#72462=CARTESIAN_POINT('Ctrl Pts',(200.016268643754,9.82230376777885,29.4377611902899));
#72463=CARTESIAN_POINT('Ctrl Pts',(200.020404402209,9.82713317339624,29.3767546330056));
#72464=CARTESIAN_POINT('Ctrl Pts',(200.024540160664,9.83662031468082,29.3165803437833));
#72465=CARTESIAN_POINT('Ctrl Pts',(200.026778880587,9.84175578195748,29.2840075082022));
#72466=CARTESIAN_POINT('Ctrl Pts',(200.029017600511,9.84825520947371,29.2516780823027));
#72467=CARTESIAN_POINT('Ctrl Pts',(200.031256320434,9.85609415083642,29.2196886182308));
#72468=CARTESIAN_POINT('Ctrl Pts',(200.034533482881,9.86756922817513,29.1728606656714));
#72469=CARTESIAN_POINT('Ctrl Pts',(200.037810645328,9.88195041103549,29.1266328620673));
#72470=CARTESIAN_POINT('Ctrl Pts',(200.041087807776,9.89915432543894,29.0813905599485));
#72471=CARTESIAN_POINT('Ctrl Pts',(200.044261760322,9.91581642529061,29.0375731043542));
#72472=CARTESIAN_POINT('Ctrl Pts',(200.047435712868,9.93512587009885,28.9946805581051));
#72473=CARTESIAN_POINT('Ctrl Pts',(200.050609665414,9.95695566619216,28.953050660288));
#72474=CARTESIAN_POINT('Ctrl Pts',(200.053780493005,9.97876396948248,28.9114617497156));
#72475=CARTESIAN_POINT('Ctrl Pts',(200.056951320596,10.0030874548671,28.8711335179084));
#72476=CARTESIAN_POINT('Ctrl Pts',(200.060122148187,10.0297515738821,28.8323825540658));
#72477=CARTESIAN_POINT('Ctrl Pts',(200.063291245362,10.0564011414834,28.7936527377924));
#72478=CARTESIAN_POINT('Ctrl Pts',(200.066460342537,10.0853884970476,28.7564989422275));
#72479=CARTESIAN_POINT('Ctrl Pts',(200.069629439712,10.1164952293694,28.7212096670008));
#72480=CARTESIAN_POINT('Ctrl Pts',(200.072798198011,10.1475986354081,28.685924165302));
#72481=CARTESIAN_POINT('Ctrl Pts',(200.07596695631,10.1808205985382,28.6525032040694));
#72482=CARTESIAN_POINT('Ctrl Pts',(200.079135714609,10.2159035662049,28.6212009074824));
#72483=CARTESIAN_POINT('Ctrl Pts',(200.082307659289,10.2510218119494,28.5898671345144));
#72484=CARTESIAN_POINT('Ctrl Pts',(200.085479603969,10.2880043785701,28.5606566467084));
#72485=CARTESIAN_POINT('Ctrl Pts',(200.088651548649,10.3265596090397,28.5337841326478));
#72486=CARTESIAN_POINT('Ctrl Pts',(200.091825438169,10.3651384791857,28.506895142028));
#72487=CARTESIAN_POINT('Ctrl Pts',(200.094999327689,10.4052914568156,28.4823472681669));
#72488=CARTESIAN_POINT('Ctrl Pts',(200.098173217209,10.4466998741197,28.4603106073443));
#72489=CARTESIAN_POINT('Ctrl Pts',(200.101352721942,10.4881815507756,28.4382349594849));
#72490=CARTESIAN_POINT('Ctrl Pts',(200.104532226675,10.5309225903706,28.4186796147557));
#72491=CARTESIAN_POINT('Ctrl Pts',(200.107711731408,10.5745836545359,28.4017668756079));
#72492=CARTESIAN_POINT('Ctrl Pts',(200.108443893994,10.5846377353961,28.3978722832472));
#72493=CARTESIAN_POINT('Ctrl Pts',(200.109176056581,10.5947405420219,28.3941176101592));
#72494=CARTESIAN_POINT('Ctrl Pts',(200.109908219168,10.6048878347393,28.390503970551));
#72495=CARTESIAN_POINT('Ctrl Pts',(200.113185381615,10.6503071544851,28.3743293062953));
#72496=CARTESIAN_POINT('Ctrl Pts',(200.116462544063,10.6968237837432,28.3609117308587));
#72497=CARTESIAN_POINT('Ctrl Pts',(200.11973970651,10.744070042996,28.3503935805642));
#72498=CARTESIAN_POINT('Ctrl Pts',(200.122913658414,10.7898283344861,28.3402066875758));
#72499=CARTESIAN_POINT('Ctrl Pts',(200.126087610318,10.8362703860954,28.3327394191828));
#72500=CARTESIAN_POINT('Ctrl Pts',(200.129261562222,10.8830442887541,28.3280714936025));
#72501=CARTESIAN_POINT('Ctrl Pts',(200.132432389157,10.9297721393517,28.3234081639098));
#72502=CARTESIAN_POINT('Ctrl Pts',(200.135603216091,10.9768306425947,28.3215387766397));
#72503=CARTESIAN_POINT('Ctrl Pts',(200.138774043026,11.0238593946484,28.3224917020305));
#72504=CARTESIAN_POINT('Ctrl Pts',(200.141943139531,11.0708624814957,28.3234441073772));
#72505=CARTESIAN_POINT('Ctrl Pts',(200.145112236037,11.1178352935069,28.3272157628039));
#72506=CARTESIAN_POINT('Ctrl Pts',(200.148281332542,11.1644167584438,28.3337829567174));
#72507=CARTESIAN_POINT('Ctrl Pts',(200.15145009016,11.2109932421918,28.340349448368));
#72508=CARTESIAN_POINT('Ctrl Pts',(200.154618847778,11.2571779111989,28.3497108050288));
#72509=CARTESIAN_POINT('Ctrl Pts',(200.157787605396,11.3026168713695,28.3617917186813));
#72510=CARTESIAN_POINT('Ctrl Pts',(200.160959549383,11.3481015230396,28.3738847803903));
#72511=CARTESIAN_POINT('Ctrl Pts',(200.164131493369,11.3928384313099,28.3887027101717));
#72512=CARTESIAN_POINT('Ctrl Pts',(200.167303437356,11.4364878766585,28.4061200266802));
#72513=CARTESIAN_POINT('Ctrl Pts',(200.170477326175,11.4801640850382,28.4235480223663));
#72514=CARTESIAN_POINT('Ctrl Pts',(200.173651214994,11.5227509997531,28.4435783392123));
#72515=CARTESIAN_POINT('Ctrl Pts',(200.176825103812,11.5639312842824,28.4660384102359));
#72516=CARTESIAN_POINT('Ctrl Pts',(200.18000460784,11.6051844245113,28.4885382173663));
#72517=CARTESIAN_POINT('Ctrl Pts',(200.183184111867,11.6450255011556,28.5134760551328));
#72518=CARTESIAN_POINT('Ctrl Pts',(200.186363615895,11.6831657218461,28.5406358048194));
#72519=CARTESIAN_POINT('Ctrl Pts',(200.18709578323,11.691948545686,28.5468900763657));
#72520=CARTESIAN_POINT('Ctrl Pts',(200.187827950566,11.7006413193404,28.5532620047846));
#72521=CARTESIAN_POINT('Ctrl Pts',(200.188560117902,11.7092407801928,28.5597486622123));
#72522=CARTESIAN_POINT('Ctrl Pts',(200.191837280349,11.747731749119,28.5887827765331));
#72523=CARTESIAN_POINT('Ctrl Pts',(200.195114442797,11.7845237684032,28.6202498310047));
#72524=CARTESIAN_POINT('Ctrl Pts',(200.198391605244,11.8192957257391,28.6539210578878));
#72525=CARTESIAN_POINT('Ctrl Pts',(200.201565557752,11.852972585822,28.6865318535819));
#72526=CARTESIAN_POINT('Ctrl Pts',(200.20473951026,11.8847543092152,28.7212096153979));
#72527=CARTESIAN_POINT('Ctrl Pts',(200.207913462769,11.9143807522802,28.7577043026129));
#72528=CARTESIAN_POINT('Ctrl Pts',(200.211084290316,11.9439780261994,28.7941630584522));
#72529=CARTESIAN_POINT('Ctrl Pts',(200.214255117863,11.9714238706224,28.8324347683777));
#72530=CARTESIAN_POINT('Ctrl Pts',(200.21742594541,11.9964963515863,28.8722340533485));
#72531=CARTESIAN_POINT('Ctrl Pts',(200.220595042535,12.0215551496956,28.9120116185769));
#72532=CARTESIAN_POINT('Ctrl Pts',(200.22376413966,12.0442428539556,28.9533146369634));
#72533=CARTESIAN_POINT('Ctrl Pts',(200.226933236786,12.0643806578495,28.9958285235201));
#72534=CARTESIAN_POINT('Ctrl Pts',(200.230101995029,12.0845163083457,29.0383378639354));
#72535=CARTESIAN_POINT('Ctrl Pts',(200.233270753273,12.1021023636656,29.0820573115153));
#72536=CARTESIAN_POINT('Ctrl Pts',(200.236439511517,12.1170070553719,29.1266498952064));
#72537=CARTESIAN_POINT('Ctrl Pts',(200.239611456134,12.1319267346233,29.1712873193659));
#72538=CARTESIAN_POINT('Ctrl Pts',(200.242783400751,12.1441594956936,29.2167991018886));
#72539=CARTESIAN_POINT('Ctrl Pts',(200.245955345367,12.1536232681568,29.2628325113615));
#72540=CARTESIAN_POINT('Ctrl Pts',(200.249129234819,12.1630928432044,29.3088941455976));
#72541=CARTESIAN_POINT('Ctrl Pts',(200.252303124271,12.1697899720009,29.3554774919692));
#72542=CARTESIAN_POINT('Ctrl Pts',(200.255477013723,12.173684218576,29.4022226121963));
#72543=CARTESIAN_POINT('Ctrl Pts',(200.258656518381,12.177585354805,29.4490504333251));
#72544=CARTESIAN_POINT('Ctrl Pts',(200.26183602304,12.1786737082398,29.4960400432032));
#72545=CARTESIAN_POINT('Ctrl Pts',(200.265015527699,12.1769709150544,29.5428313858755));
#72546=CARTESIAN_POINT('Ctrl Pts',(200.265747690678,12.1765788029913,29.5536062997454));
#72547=CARTESIAN_POINT('Ctrl Pts',(200.266479853657,12.1760389015659,29.5643707276121));
#72548=CARTESIAN_POINT('Ctrl Pts',(200.267212016636,12.1753518613014,29.5751203343657));
#72549=CARTESIAN_POINT('Ctrl Pts',(200.270489179083,12.1722766681835,29.6232355881859));
#72550=CARTESIAN_POINT('Ctrl Pts',(200.27376634153,12.1662351420622,29.671270243921));
#72551=CARTESIAN_POINT('Ctrl Pts',(200.277043503978,12.1572417049752,29.7188302967281));
#72552=CARTESIAN_POINT('Ctrl Pts',(200.280217456315,12.1485315048796,29.7648925054809));
#72553=CARTESIAN_POINT('Ctrl Pts',(200.283391408652,12.1370526946772,29.8105089694688));
#72554=CARTESIAN_POINT('Ctrl Pts',(200.286565360989,12.1228709980971,29.8553248993983));
#72555=CARTESIAN_POINT('Ctrl Pts',(200.289736188364,12.1087032643188,29.9000967051325));
#72556=CARTESIAN_POINT('Ctrl Pts',(200.292907015739,12.0918380788874,29.944069008322));
#72557=CARTESIAN_POINT('Ctrl Pts',(200.296077843114,12.0723916949562,29.9868994917732));
#72558=CARTESIAN_POINT('Ctrl Pts',(200.299246940066,12.0529559235441,30.0297066012477));
#72559=CARTESIAN_POINT('Ctrl Pts',(200.302416037018,12.0309419740899,30.0713726192533));
#72560=CARTESIAN_POINT('Ctrl Pts',(200.30558513397,12.0065142128789,30.1115751808018));
#72561=CARTESIAN_POINT('Ctrl Pts',(200.30875389204,11.9820890638076,30.15177344336));
#72562=CARTESIAN_POINT('Ctrl Pts',(200.31192265011,11.9552509063891,30.1905080857414));
#72563=CARTESIAN_POINT('Ctrl Pts',(200.31509140818,11.9262086756078,30.2274837123461));
#72564=CARTESIAN_POINT('Ctrl Pts',(200.318263352624,11.8971372411461,30.2644965201297));
#72565=CARTESIAN_POINT('Ctrl Pts',(200.321435297068,11.8658576572764,30.2997463456538));
#72566=CARTESIAN_POINT('Ctrl Pts',(200.324607241512,11.83261935746,30.3329706285836));
#72567=CARTESIAN_POINT('Ctrl Pts',(200.327781130791,11.7993606780257,30.3662152825369));
#72568=CARTESIAN_POINT('Ctrl Pts',(200.33095502007,11.7641413096171,30.3974315531704));
#72569=CARTESIAN_POINT('Ctrl Pts',(200.334128909349,11.7272451060402,30.4263960374703));
#72570=CARTESIAN_POINT('Ctrl Pts',(200.337308413836,11.6902836261191,30.4554117654067));
#72571=CARTESIAN_POINT('Ctrl Pts',(200.340487918324,11.6516398527521,30.4821674469353));
#72572=CARTESIAN_POINT('Ctrl Pts',(200.343667422812,11.6116263804457,30.5064831013201));
#72573=CARTESIAN_POINT('Ctrl Pts',(200.344399586998,11.6024122304139,30.512082417618));
#72574=CARTESIAN_POINT('Ctrl Pts',(200.345131751184,11.5931255453682,30.5175525423206));
#72575=CARTESIAN_POINT('Ctrl Pts',(200.34586391537,11.5837703035305,30.5228916341509));
#72576=CARTESIAN_POINT('Ctrl Pts',(200.349141077817,11.5418962979124,30.5467893767402));
#72577=CARTESIAN_POINT('Ctrl Pts',(200.352418240265,11.4984579624634,30.5681655127757));
#72578=CARTESIAN_POINT('Ctrl Pts',(200.355695402712,11.4537922752884,30.5868153630625));
#72579=CARTESIAN_POINT('Ctrl Pts',(200.358869354999,11.410533278438,30.6048778594851));
#72580=CARTESIAN_POINT('Ctrl Pts',(200.362043307287,11.3661236547293,30.6203830237787));
#72581=CARTESIAN_POINT('Ctrl Pts',(200.365217259574,11.3208958508152,30.6331905909553));
#72582=CARTESIAN_POINT('Ctrl Pts',(200.368388086898,11.275712576633,30.6459855482441));
#72583=CARTESIAN_POINT('Ctrl Pts',(200.371558914222,11.2297132501836,30.656088014506));
#72584=CARTESIAN_POINT('Ctrl Pts',(200.374729741546,11.1832476961478,30.6634067836989));
#72585=CARTESIAN_POINT('Ctrl Pts',(200.377898838446,11.1368074998827,30.6707215588003));
#72586=CARTESIAN_POINT('Ctrl Pts',(200.381067935346,11.0899021292431,30.675255559896));
#72587=CARTESIAN_POINT('Ctrl Pts',(200.384237032245,11.0428912109895,30.6769687364241));
#72588=CARTESIAN_POINT('Ctrl Pts',(200.387405790262,10.995885319783,30.6786817297562));
#72589=CARTESIAN_POINT('Ctrl Pts',(200.390574548279,10.9487744596074,30.6775744794197));
#72590=CARTESIAN_POINT('Ctrl Pts',(200.393743306296,10.9019202494185,30.6736589900929));
#72591=CARTESIAN_POINT('Ctrl Pts',(200.396915250685,10.8550189245692,30.6697395635116));
#72592=CARTESIAN_POINT('Ctrl Pts',(200.400087195074,10.8083753201946,30.6630063121403));
#72593=CARTESIAN_POINT('Ctrl Pts',(200.403259139463,10.762345909839,30.6535231232748));
#72594=CARTESIAN_POINT('Ctrl Pts',(200.406433028687,10.7162882771791,30.6440341199216));
#72595=CARTESIAN_POINT('Ctrl Pts',(200.409606917911,10.6708461256432,30.6317919687924));
#72596=CARTESIAN_POINT('Ctrl Pts',(200.412780807134,10.6263621603328,30.6169108412353));
#72597=CARTESIAN_POINT('Ctrl Pts',(200.415960311566,10.581799494504,30.6020033861588));
#72598=CARTESIAN_POINT('Ctrl Pts',(200.419139815998,10.5381989107945,30.5844478528081));
#72599=CARTESIAN_POINT('Ctrl Pts',(200.422319320429,10.4958826599652,30.5644062992938));
#72600=CARTESIAN_POINT('Ctrl Pts',(200.423051484988,10.4861382297368,30.5597912042402));
#72601=CARTESIAN_POINT('Ctrl Pts',(200.423783649546,10.4764617932563,30.5550444706976));
#72602=CARTESIAN_POINT('Ctrl Pts',(200.424515814104,10.4668570764666,30.5501684082024));
#72603=CARTESIAN_POINT('Ctrl Pts',(200.427694743764,10.4251550864809,30.5289974029764));
#72604=CARTESIAN_POINT('Ctrl Pts',(200.430873673424,10.3846248526976,30.5052922646991));
#72605=CARTESIAN_POINT('Ctrl Pts',(200.434052603084,10.3455918892627,30.4792063557296));
#72606=CARTESIAN_POINT('Ctrl Pts',(200.437226952187,10.306615168875,30.4531580342472));
#72607=CARTESIAN_POINT('Ctrl Pts',(200.440401301291,10.2691319095204,30.4247360359438));
#72608=CARTESIAN_POINT('Ctrl Pts',(200.443575650394,10.233443060636,30.3941395423606));
#72609=CARTESIAN_POINT('Ctrl Pts',(200.446746459659,10.1977940097517,30.3635771680975));
#72610=CARTESIAN_POINT('Ctrl Pts',(200.449917268925,10.1639358250307,30.3308454645624));
#72611=CARTESIAN_POINT('Ctrl Pts',(200.45308807819,10.1321381353714,30.2961851834991));
#72612=CARTESIAN_POINT('Ctrl Pts',(200.454084820662,10.1221425458748,30.2852897396772));
#72613=CARTESIAN_POINT('Ctrl Pts',(200.455081563134,10.1123503133646,30.2742040159438));
#72614=CARTESIAN_POINT('Ctrl Pts',(200.456078305605,10.1027690874833,30.2629362700282));
#72615=CARTESIAN_POINT('Origin',(197.762132885264,11.,29.5));
#72616=CARTESIAN_POINT('',(201.054417864302,10.1027692940023,30.2629365128992));
#72617=CARTESIAN_POINT('',(200.956011803843,10.1027690874833,30.2629362700282));
#72618=CARTESIAN_POINT('',(197.762132885264,10.1027690874833,30.2629362700282));
#72619=CARTESIAN_POINT('Ctrl Pts',(201.054417864302,10.1027692940023,30.2629365128992));
#72620=CARTESIAN_POINT('Ctrl Pts',(201.05141890073,10.1293141722984,30.2941538940201));
#72621=CARTESIAN_POINT('Ctrl Pts',(201.048436058869,10.1574897561157,30.3239877180485));
#72622=CARTESIAN_POINT('Ctrl Pts',(201.044447884818,10.1981927710927,30.3628044051238));
#72623=CARTESIAN_POINT('Ctrl Pts',(201.043380444452,10.2093995741434,30.3730849289079));
#72624=CARTESIAN_POINT('Ctrl Pts',(201.041857920987,10.2258809677539,30.387626411253));
#72625=CARTESIAN_POINT('Ctrl Pts',(201.041391629439,10.2309976879275,30.3920629863274));
#72626=CARTESIAN_POINT('Ctrl Pts',(201.040608655144,10.2397114783181,30.3994877921686));
#72627=CARTESIAN_POINT('Ctrl Pts',(201.040290374247,10.2432884733418,30.402499081806));
#72628=CARTESIAN_POINT('Ctrl Pts',(201.039562110351,10.2515541690651,30.4093738542067));
#72629=CARTESIAN_POINT('Ctrl Pts',(201.039153163814,10.2562549515858,30.4132224677239));
#72630=CARTESIAN_POINT('Ctrl Pts',(201.037999407172,10.2696786500102,30.4240402801249));
#72631=CARTESIAN_POINT('Ctrl Pts',(201.037260282136,10.2784714300278,30.4309222621592));
#72632=CARTESIAN_POINT('Ctrl Pts',(201.03153824864,10.3479287880017,30.4837100942689));
#72633=CARTESIAN_POINT('Ctrl Pts',(201.026869315461,10.4128222971946,30.5237713871246));
#72634=CARTESIAN_POINT('Ctrl Pts',(201.019162536663,10.5245155795484,30.5785846089263));
#72635=CARTESIAN_POINT('Ctrl Pts',(201.016160481788,10.569163570506,30.5971826343835));
#72636=CARTESIAN_POINT('Ctrl Pts',(201.011745153561,10.6347514312984,30.6198808655372));
#72637=CARTESIAN_POINT('Ctrl Pts',(201.010391259537,10.6548583048927,30.626240118351));
#72638=CARTESIAN_POINT('Ctrl Pts',(201.007905342958,10.6916391657401,30.6367954364878));
#72639=CARTESIAN_POINT('Ctrl Pts',(201.006778967143,10.7082551327778,30.6411727093527));
#72640=CARTESIAN_POINT('Ctrl Pts',(201.004966253194,10.7348705325665,30.647564946707));
#72641=CARTESIAN_POINT('Ctrl Pts',(201.004287373938,10.7448110284203,30.6498162980962));
#72642=CARTESIAN_POINT('Ctrl Pts',(201.002986846657,10.7637933712409,30.6538571955829));
#72643=CARTESIAN_POINT('Ctrl Pts',(201.00236598706,10.7728294918616,30.6556701740891));
#72644=CARTESIAN_POINT('Ctrl Pts',(201.000941441793,10.7934975173951,30.659565181058));
#72645=CARTESIAN_POINT('Ctrl Pts',(201.000135681691,10.805141185382,30.661578542035));
#72646=CARTESIAN_POINT('Ctrl Pts',(200.997501904897,10.8430363755375,30.6675453769099));
#72647=CARTESIAN_POINT('Ctrl Pts',(200.995652425535,10.8693900937279,30.6707863371429));
#72648=CARTESIAN_POINT('Ctrl Pts',(200.987854904254,10.9793891975865,30.6805539392231));
#72649=CARTESIAN_POINT('Ctrl Pts',(200.98168349618,11.0634939303877,30.6790238877709));
#72650=CARTESIAN_POINT('Ctrl Pts',(200.973090014501,11.1800188967315,30.6643948450842));
#72651=CARTESIAN_POINT('Ctrl Pts',(200.970646080825,11.2131376043149,30.6587902219369));
#72652=CARTESIAN_POINT('Ctrl Pts',(200.967253722702,11.2595372161782,30.648881137232));
#72653=CARTESIAN_POINT('Ctrl Pts',(200.966269732865,11.2730495631276,30.6457449127133));
#72654=CARTESIAN_POINT('Ctrl Pts',(200.964540836263,11.2969346345543,30.6397545911496));
#72655=CARTESIAN_POINT('Ctrl Pts',(200.963791973521,11.3073294689082,30.6369957444613));
#72656=CARTESIAN_POINT('Ctrl Pts',(200.962642048408,11.3233888242212,30.6324971572702));
#72657=CARTESIAN_POINT('Ctrl Pts',(200.962235899982,11.3290801733011,30.6308564834628));
#72658=CARTESIAN_POINT('Ctrl Pts',(200.961475318814,11.3397790003519,30.6276846669657));
#72659=CARTESIAN_POINT('Ctrl Pts',(200.961120420838,11.3447887920779,30.6261630286523));
#72660=CARTESIAN_POINT('Ctrl Pts',(200.960269321222,11.3568417623379,30.6224141747818));
#72661=CARTESIAN_POINT('Ctrl Pts',(200.959774966841,11.3638744156748,30.6201540249725));
#72662=CARTESIAN_POINT('Ctrl Pts',(200.958100545071,11.38778267967,30.6122214704124));
#72663=CARTESIAN_POINT('Ctrl Pts',(200.956936697517,11.4045515759021,30.6062323930871));
#72664=CARTESIAN_POINT('Ctrl Pts',(200.95120058265,11.4875288311721,30.5744573147878));
#72665=CARTESIAN_POINT('Ctrl Pts',(200.946848776718,11.5514496693805,30.5430954445361));
#72666=CARTESIAN_POINT('Ctrl Pts',(200.94144643856,11.6258878993012,30.4978064342095));
#72667=CARTESIAN_POINT('Ctrl Pts',(200.940448230259,11.6394449639331,30.4891731237403));
#72668=CARTESIAN_POINT('Ctrl Pts',(200.937246351682,11.6821638592468,30.4607238940268));
#72669=CARTESIAN_POINT('Ctrl Pts',(200.935027189226,11.7106127823508,30.4398761332686));
#72670=CARTESIAN_POINT('Ctrl Pts',(200.931162614273,11.7575878965633,30.4020987506594));
#72671=CARTESIAN_POINT('Ctrl Pts',(200.92953860289,11.7765870220306,30.3857957071283));
#72672=CARTESIAN_POINT('Ctrl Pts',(200.927120954748,11.803675566543,30.3610094621293));
#72673=CARTESIAN_POINT('Ctrl Pts',(200.926346201202,11.8121815244313,30.3529905424156));
#72674=CARTESIAN_POINT('Ctrl Pts',(200.924953498105,11.827151474094,30.3384508151227));
#72675=CARTESIAN_POINT('Ctrl Pts',(200.924337640988,11.8336613139201,30.3319784468883));
#72676=CARTESIAN_POINT('Ctrl Pts',(200.923018622269,11.8473662778599,30.3180300125284));
#72677=CARTESIAN_POINT('Ctrl Pts',(200.922314598505,11.8545395587158,30.31053367667));
#72678=CARTESIAN_POINT('Ctrl Pts',(200.920404443354,11.8736159068938,30.2900634714575));
#72679=CARTESIAN_POINT('Ctrl Pts',(200.919190585993,11.8853282214557,30.276916291916));
#72680=CARTESIAN_POINT('Ctrl Pts',(200.911937578125,11.9528725414347,30.1975858463982));
#72681=CARTESIAN_POINT('Ctrl Pts',(200.905621309079,12.0015539060369,30.125681142446));
#72682=CARTESIAN_POINT('Ctrl Pts',(200.896249242902,12.0611497923409,30.0126003882821));
#72683=CARTESIAN_POINT('Ctrl Pts',(200.893228169189,12.0784588816488,29.9751050653797));
#72684=CARTESIAN_POINT('Ctrl Pts',(200.888618226564,12.1022790188109,29.9154553264129));
#72685=CARTESIAN_POINT('Ctrl Pts',(200.886989841909,12.1101688017286,29.8938877445873));
#72686=CARTESIAN_POINT('Ctrl Pts',(200.884842954916,12.1199154875853,29.8646183942858));
#72687=CARTESIAN_POINT('Ctrl Pts',(200.884297700493,12.122332288692,29.8571099480436));
#72688=CARTESIAN_POINT('Ctrl Pts',(200.883391582071,12.1262526233699,29.8444973048884));
#72689=CARTESIAN_POINT('Ctrl Pts',(200.883028488564,12.1277973052589,29.8394062571825));
#72690=CARTESIAN_POINT('Ctrl Pts',(200.882279430934,12.1309301447227,29.8288232794494));
#72691=CARTESIAN_POINT('Ctrl Pts',(200.881893761361,12.1325128993987,29.8233299823168));
#72692=CARTESIAN_POINT('Ctrl Pts',(200.880854080684,12.1366948794347,29.8084079512948));
#72693=CARTESIAN_POINT('Ctrl Pts',(200.880204217992,12.1392168244339,29.7989577821247));
#72694=CARTESIAN_POINT('Ctrl Pts',(200.876366233717,12.1535340615244,29.7424943641798));
#72695=CARTESIAN_POINT('Ctrl Pts',(200.873308747182,12.1625370502276,29.6948154306466));
#72696=CARTESIAN_POINT('Ctrl Pts',(200.865953751255,12.1772382088655,29.577719425106));
#72697=CARTESIAN_POINT('Ctrl Pts',(200.861702868868,12.1797730434681,29.5080968219526));
#72698=CARTESIAN_POINT('Ctrl Pts',(200.854932337871,12.1741873925625,29.4010001848339));
#72699=CARTESIAN_POINT('Ctrl Pts',(200.852516794904,12.1704161585616,29.3634621222647));
#72700=CARTESIAN_POINT('Ctrl Pts',(200.849163476261,12.1628607691475,29.3128321317298));
#72701=CARTESIAN_POINT('Ctrl Pts',(200.848273377335,12.1606411451323,29.2995278389988));
#72702=CARTESIAN_POINT('Ctrl Pts',(200.846747657742,12.1564788131757,29.2769728672643));
#72703=CARTESIAN_POINT('Ctrl Pts',(200.846115691693,12.1546523018101,29.2677019146527));
#72704=CARTESIAN_POINT('Ctrl Pts',(200.844905998779,12.1509634418492,29.2500977929029));
#72705=CARTESIAN_POINT('Ctrl Pts',(200.844328952811,12.1491216296573,29.2417609028978));
#72706=CARTESIAN_POINT('Ctrl Pts',(200.842968538324,12.1445887612333,29.2222525173519));
#72707=CARTESIAN_POINT('Ctrl Pts',(200.842182915249,12.1418245680834,29.2110990894847));
#72708=CARTESIAN_POINT('Ctrl Pts',(200.839352682281,12.1313486659258,29.1713307142085));
#72709=CARTESIAN_POINT('Ctrl Pts',(200.837279827866,12.1227213002895,29.1429706983062));
#72710=CARTESIAN_POINT('Ctrl Pts',(200.828406912823,12.0818411706136,29.0247960786888));
#72711=CARTESIAN_POINT('Ctrl Pts',(200.821323007916,12.0398068727197,28.9387545017789));
#72712=CARTESIAN_POINT('Ctrl Pts',(200.812723621565,11.9753005273021,28.8393815938006));
#72713=CARTESIAN_POINT('Ctrl Pts',(200.811061587052,11.9621662765048,28.8203942505181));
#72714=CARTESIAN_POINT('Ctrl Pts',(200.808312718992,11.9392036366574,28.7892000709783));
#72715=CARTESIAN_POINT('Ctrl Pts',(200.807213272026,11.9296746287227,28.7767813941304));
#72716=CARTESIAN_POINT('Ctrl Pts',(200.805654108371,11.9156243313504,28.7592071562465));
#72717=CARTESIAN_POINT('Ctrl Pts',(200.805182456969,11.9113015981471,28.7538958809825));
#72718=CARTESIAN_POINT('Ctrl Pts',(200.804360062312,11.9036321841737,28.7446386946175));
#72719=CARTESIAN_POINT('Ctrl Pts',(200.804007999141,11.9003054865297,28.7406767089274));
#72720=CARTESIAN_POINT('Ctrl Pts',(200.803234961785,11.8929040484637,28.7319788748419));
#72721=CARTESIAN_POINT('Ctrl Pts',(200.802814821885,11.8888176087104,28.7272533718877));
#72722=CARTESIAN_POINT('Ctrl Pts',(200.801571359817,11.8765396228386,28.7132815376905));
#72723=CARTESIAN_POINT('Ctrl Pts',(200.800755342794,11.8682397300543,28.7041310097451));
#72724=CARTESIAN_POINT('Ctrl Pts',(200.796671911984,11.825570053211,28.6585504123285));
#72725=CARTESIAN_POINT('Ctrl Pts',(200.793532094047,11.7890419363471,28.6242048058001));
#72726=CARTESIAN_POINT('Ctrl Pts',(200.787750698132,11.7173389934812,28.564925816093));
#72727=CARTESIAN_POINT('Ctrl Pts',(200.78510637674,11.6827724458304,28.5393956354292));
#72728=CARTESIAN_POINT('Ctrl Pts',(200.780141790337,11.6161848625346,28.4956289004162));
#72729=CARTESIAN_POINT('Ctrl Pts',(200.777832840778,11.5845550194756,28.4768967607829));
#72730=CARTESIAN_POINT('Ctrl Pts',(200.773830606244,11.5293536503388,28.4476012797737));
#72731=CARTESIAN_POINT('Ctrl Pts',(200.772160983206,11.5062158812604,28.436278380319));
#72732=CARTESIAN_POINT('Ctrl Pts',(200.769688539792,11.4719520432726,28.4208819022617));
#72733=CARTESIAN_POINT('Ctrl Pts',(200.768905897474,11.4611053651756,28.4162027746508));
#72734=CARTESIAN_POINT('Ctrl Pts',(200.767504513069,11.4416961464602,28.4081739715416));
#72735=CARTESIAN_POINT('Ctrl Pts',(200.766887966837,11.433161201807,28.404759876842));
#72736=CARTESIAN_POINT('Ctrl Pts',(200.76557332907,11.4149775618981,28.3977319613854));
#72737=CARTESIAN_POINT('Ctrl Pts',(200.764874442856,11.4053197065782,28.3941441641362));
#72738=CARTESIAN_POINT('Ctrl Pts',(200.76296219031,11.378927012748,28.3847317190714));
#72739=CARTESIAN_POINT('Ctrl Pts',(200.761740882735,11.3621063783595,28.3791574902337));
#72740=CARTESIAN_POINT('Ctrl Pts',(200.754422247733,11.2615715573451,28.3483402238901));
#72741=CARTESIAN_POINT('Ctrl Pts',(200.748041631359,11.1753957457005,28.3321082519489));
#72742=CARTESIAN_POINT('Ctrl Pts',(200.738642497543,11.0475570248609,28.3225037183181));
#72743=CARTESIAN_POINT('Ctrl Pts',(200.735657013185,11.0067448321476,28.3215628951638));
#72744=CARTESIAN_POINT('Ctrl Pts',(200.731093422795,10.9431741770112,28.3234007848732));
#72745=CARTESIAN_POINT('Ctrl Pts',(200.729476614283,10.9204061893324,28.3247213650817));
#72746=CARTESIAN_POINT('Ctrl Pts',(200.727342273112,10.8898507229845,28.3273857797826));
#72747=CARTESIAN_POINT('Ctrl Pts',(200.726798367985,10.8820189432541,28.3281478543253));
#72748=CARTESIAN_POINT('Ctrl Pts',(200.725893837773,10.8689090761659,28.3295562819846));
#72749=CARTESIAN_POINT('Ctrl Pts',(200.72553099998,10.8636267494636,28.3301599817313));
#72750=CARTESIAN_POINT('Ctrl Pts',(200.724781758562,10.8526667944155,28.3314878074478));
#72751=CARTESIAN_POINT('Ctrl Pts',(200.724395657091,10.846990076168,28.3322175783778));
#72752=CARTESIAN_POINT('Ctrl Pts',(200.723353495824,10.8315969876953,28.3343106125086));
#72753=CARTESIAN_POINT('Ctrl Pts',(200.722701618129,10.8218917288532,28.3357539857233));
#72754=CARTESIAN_POINT('Ctrl Pts',(200.718611872454,10.7606084148588,28.3456523838812));
#72755=CARTESIAN_POINT('Ctrl Pts',(200.715326672411,10.7096169660092,28.357412686223));
#72756=CARTESIAN_POINT('Ctrl Pts',(200.707928337667,10.5957520297336,28.3917930172262));
#72757=CARTESIAN_POINT('Ctrl Pts',(200.703845070844,10.533687095696,28.4164451230236));
#72758=CARTESIAN_POINT('Ctrl Pts',(200.697299644535,10.4409956962848,28.4627086610199));
#72759=CARTESIAN_POINT('Ctrl Pts',(200.694932082059,10.4087467309301,28.4807462007063));
#72760=CARTESIAN_POINT('Ctrl Pts',(200.691634671177,10.3660280718114,28.5073499369256));
#72761=CARTESIAN_POINT('Ctrl Pts',(200.69075035783,10.3547777471873,28.5146255665149));
#72762=CARTESIAN_POINT('Ctrl Pts',(200.689231520821,10.3358222235394,28.5273479970769));
#72763=CARTESIAN_POINT('Ctrl Pts',(200.688600569845,10.3280537367478,28.5326984709259));
#72764=CARTESIAN_POINT('Ctrl Pts',(200.687314248257,10.3124357137779,28.543734170488));
#72765=CARTESIAN_POINT('Ctrl Pts',(200.6866587332,10.3045904275246,28.5494241212406));
#72766=CARTESIAN_POINT('Ctrl Pts',(200.684996715318,10.2849904036469,28.5640119299813));
#72767=CARTESIAN_POINT('Ctrl Pts',(200.683985494923,10.2733311455468,28.5730346650608));
#72768=CARTESIAN_POINT('Ctrl Pts',(200.679833388212,10.2265532601005,28.6106595374539));
#72769=CARTESIAN_POINT('Ctrl Pts',(200.676623568423,10.1929327596224,28.6410541879715));
#72770=CARTESIAN_POINT('Ctrl Pts',(200.667735793441,10.106444254334,28.728814537637));
#72771=CARTESIAN_POINT('Ctrl Pts',(200.661957287503,10.0573884775016,28.7896118735937));
#72772=CARTESIAN_POINT('Ctrl Pts',(200.654014115923,9.99732215424863,28.8813415542616));
#72773=CARTESIAN_POINT('Ctrl Pts',(200.651743890046,9.98102347763466,28.9085709260413));
#72774=CARTESIAN_POINT('Ctrl Pts',(200.648918802115,9.96165623380376,28.9441098738704));
#72775=CARTESIAN_POINT('Ctrl Pts',(200.648312456098,9.95755522895397,28.9518389654976));
#72776=CARTESIAN_POINT('Ctrl Pts',(200.647333455453,9.95101951748242,28.9644953780907));
#72777=CARTESIAN_POINT('Ctrl Pts',(200.646957794093,9.9485325764679,28.969395144078));
#72778=CARTESIAN_POINT('Ctrl Pts',(200.646256139448,9.94392541077959,28.9786317762011));
#72779=CARTESIAN_POINT('Ctrl Pts',(200.645929666482,9.94179739581556,28.9829645918203));
#72780=CARTESIAN_POINT('Ctrl Pts',(200.645060668794,9.93617730397211,28.9945876214244));
#72781=CARTESIAN_POINT('Ctrl Pts',(200.644520970184,9.93273346461972,29.0019010616437));
#72782=CARTESIAN_POINT('Ctrl Pts',(200.642476888394,9.91988313897022,29.0299356962415));
#72783=CARTESIAN_POINT('Ctrl Pts',(200.640999905714,9.9110019965769,29.0508937924601));
#72784=CARTESIAN_POINT('Ctrl Pts',(200.634735062853,9.8754324491238,29.1421045074596));
#72785=CARTESIAN_POINT('Ctrl Pts',(200.630156885762,9.854892181428,29.2145684187275));
#72786=CARTESIAN_POINT('Ctrl Pts',(200.623087588231,9.83448916145321,29.3263368932514));
#72787=CARTESIAN_POINT('Ctrl Pts',(200.62067512635,9.82944015372225,29.3644871657389));
#72788=CARTESIAN_POINT('Ctrl Pts',(200.616515395183,9.82407423725943,29.4292923526529));
#72789=CARTESIAN_POINT('Ctrl Pts',(200.614794530274,9.82277856374822,29.4558355737844));
#72790=CARTESIAN_POINT('Ctrl Pts',(200.612260669024,9.82220297591759,29.494344844251));
#72791=CARTESIAN_POINT('Ctrl Pts',(200.611469356697,9.82220621789741,29.5062928901909));
#72792=CARTESIAN_POINT('Ctrl Pts',(200.610058330521,9.82253381610417,29.5274450210217));
#72793=CARTESIAN_POINT('Ctrl Pts',(200.609440926464,9.82278436125572,29.536649354243));
#72794=CARTESIAN_POINT('Ctrl Pts',(200.608130602817,9.823540986179,29.5560702375485));
#72795=CARTESIAN_POINT('Ctrl Pts',(200.607436958707,9.82407229265051,29.5662849794616));
#72796=CARTESIAN_POINT('Ctrl Pts',(200.60555504918,9.82586389627428,29.593812397771));
#72797=CARTESIAN_POINT('Ctrl Pts',(200.604359266947,9.82737396042127,29.6111056808609));
#72798=CARTESIAN_POINT('Ctrl Pts',(200.59686614933,9.83911558100066,29.7181988436053));
#72799=CARTESIAN_POINT('Ctrl Pts',(200.590262393601,9.85927264856534,29.8065923087688));
#72800=CARTESIAN_POINT('Ctrl Pts',(200.580765968669,9.90237090652315,29.9287687957684));
#72801=CARTESIAN_POINT('Ctrl Pts',(200.577899560204,9.91725279626853,29.9650710958159));
#72802=CARTESIAN_POINT('Ctrl Pts',(200.573491864858,9.94337801895126,30.0207114460847));
#72803=CARTESIAN_POINT('Ctrl Pts',(200.571914565533,9.95340740458794,30.040587187807));
#72804=CARTESIAN_POINT('Ctrl Pts',(200.569823138748,9.96770573821754,30.0670312988375));
#72805=CARTESIAN_POINT('Ctrl Pts',(200.569283916213,9.97148489707319,30.0738576722635));
#72806=CARTESIAN_POINT('Ctrl Pts',(200.568384887539,9.97794689830022,30.0852611868707));
#72807=CARTESIAN_POINT('Ctrl Pts',(200.568022926901,9.98059329100803,30.0898585980502));
#72808=CARTESIAN_POINT('Ctrl Pts',(200.567272995235,9.98617141474628,30.0993994411089));
#72809=CARTESIAN_POINT('Ctrl Pts',(200.566885353227,9.98910840193206,30.1043395326335));
#72810=CARTESIAN_POINT('Ctrl Pts',(200.565834336185,9.99721437416923,30.1177495470124));
#72811=CARTESIAN_POINT('Ctrl Pts',(200.565175264433,10.0024545491371,30.1261761760927));
#72812=CARTESIAN_POINT('Ctrl Pts',(200.561011821934,10.0365147245592,30.1794347518356));
#72813=CARTESIAN_POINT('Ctrl Pts',(200.557666169063,10.0682437893456,30.2223337114375));
#72814=CARTESIAN_POINT('Ctrl Pts',(200.554352848915,10.1027690892854,30.2629362721474));
#72815=CARTESIAN_POINT('',(200.512132885305,9.82225021170068,29.5007061592685));
#72816=CARTESIAN_POINT('Ctrl Pts',(200.456078305605,10.1027690874833,30.2629362700282));
#72817=CARTESIAN_POINT('Ctrl Pts',(200.459247165187,10.0723083011789,30.227113672302));
#72818=CARTESIAN_POINT('Ctrl Pts',(200.462416024768,10.0439833305474,30.1894488856546));
#72819=CARTESIAN_POINT('Ctrl Pts',(200.465584884349,10.0180138899712,30.1502294535089));
#72820=CARTESIAN_POINT('Ctrl Pts',(200.468756203967,9.99202428890455,30.1109795746932));
#72821=CARTESIAN_POINT('Ctrl Pts',(200.471927523584,9.96839418568235,30.0701731002698));
#72822=CARTESIAN_POINT('Ctrl Pts',(200.475098843202,9.94730004587657,30.0281267547554));
#72823=CARTESIAN_POINT('Ctrl Pts',(200.478271213189,9.92619891949807,29.9860664831055));
#72824=CARTESIAN_POINT('Ctrl Pts',(200.481443583177,9.90763565733653,29.9427660318742));
#72825=CARTESIAN_POINT('Ctrl Pts',(200.484615953165,9.89173914812929,29.8985636043479));
#72826=CARTESIAN_POINT('Ctrl Pts',(200.487794649595,9.87581093758726,29.8542730269055));
#72827=CARTESIAN_POINT('Ctrl Pts',(200.490973346026,9.86256026986468,29.8090774137332));
#72828=CARTESIAN_POINT('Ctrl Pts',(200.494152042457,9.85206611231544,29.7633303096975));
#72829=CARTESIAN_POINT('Ctrl Pts',(200.497157265917,9.84214465893017,29.7200797907234));
#72830=CARTESIAN_POINT('Ctrl Pts',(200.500162489378,9.83468667522977,29.676336831864));
#72831=CARTESIAN_POINT('Ctrl Pts',(200.503167712838,9.82971621933516,29.6324044380404));
#72832=CARTESIAN_POINT('Ctrl Pts',(200.506156103647,9.82477360361806,29.5887181153357));
#72833=CARTESIAN_POINT('Ctrl Pts',(200.509144494455,9.82227661969029,29.5447500160668));
#72834=CARTESIAN_POINT('Ctrl Pts',(200.512132885264,9.82225021170104,29.5007061598695));
#72835=CARTESIAN_POINT('Ctrl Pts',(200.512132885305,9.82225021170068,29.5007061592685));
#72836=CARTESIAN_POINT('Ctrl Pts',(200.515267830035,9.82222250865862,29.4545023446655));
#72837=CARTESIAN_POINT('Ctrl Pts',(200.518402774765,9.82491796434091,29.408194106874));
#72838=CARTESIAN_POINT('Ctrl Pts',(200.521537719495,9.83034710037947,29.3621335540848));
#72839=CARTESIAN_POINT('Ctrl Pts',(200.524668736786,9.83576943483166,29.316130705657));
#72840=CARTESIAN_POINT('Ctrl Pts',(200.527799754078,9.84391861397454,29.2703754939379));
#72841=CARTESIAN_POINT('Ctrl Pts',(200.530930771369,9.85475316768141,29.2252187132204));
#72842=CARTESIAN_POINT('Ctrl Pts',(200.534059329963,9.86557921332608,29.180097392819));
#72843=CARTESIAN_POINT('Ctrl Pts',(200.537187888557,9.87908632916235,29.1355741295138));
#72844=CARTESIAN_POINT('Ctrl Pts',(200.540316447151,9.89518182682023,29.0919903595358));
#72845=CARTESIAN_POINT('Ctrl Pts',(200.543444011243,9.91127220806062,29.0484204439143));
#72846=CARTESIAN_POINT('Ctrl Pts',(200.546571575334,9.92994914174014,29.0057899667846));
#72847=CARTESIAN_POINT('Ctrl Pts',(200.549699139426,9.95107076630701,28.9644231845904));
#72848=CARTESIAN_POINT('Ctrl Pts',(200.552829311202,9.97221000155768,28.923021911805));
#72849=CARTESIAN_POINT('Ctrl Pts',(200.555959482979,9.99579773645662,28.8828869490627));
#72850=CARTESIAN_POINT('Ctrl Pts',(200.559089654755,10.0216457995202,28.8443185827678));
#72851=CARTESIAN_POINT('Ctrl Pts',(200.562221316338,10.0475061649802,28.8057318598431));
#72852=CARTESIAN_POINT('Ctrl Pts',(200.565352977921,10.0756286526337,28.7687136740076));
#72853=CARTESIAN_POINT('Ctrl Pts',(200.568484639504,10.1057835683042,28.7335327562216));
#72854=CARTESIAN_POINT('Ctrl Pts',(200.571621921098,10.1359925993205,28.6982887035375));
#72855=CARTESIAN_POINT('Ctrl Pts',(200.574759202692,10.1682409342474,28.6648889062404));
#72856=CARTESIAN_POINT('Ctrl Pts',(200.577896484286,10.20226213217,28.6335651457091));
#72857=CARTESIAN_POINT('Ctrl Pts',(200.579204193381,10.2164431448211,28.6205085024544));
#72858=CARTESIAN_POINT('Ctrl Pts',(200.580511902477,10.2309317985967,28.607812070833));
#72859=CARTESIAN_POINT('Ctrl Pts',(200.581819611573,10.2457072655321,28.5954904460268));
#72860=CARTESIAN_POINT('Ctrl Pts',(200.58509677402,10.28273507664,28.5646120448321));
#72861=CARTESIAN_POINT('Ctrl Pts',(200.588373936467,10.3217456398475,28.5359414302213));
#72862=CARTESIAN_POINT('Ctrl Pts',(200.591651098915,10.3624431471825,28.5097392656853));
#72863=CARTESIAN_POINT('Ctrl Pts',(200.594825051242,10.4018589375795,28.4843623054505));
#72864=CARTESIAN_POINT('Ctrl Pts',(200.597999003569,10.4428564756788,28.4613009368035));
#72865=CARTESIAN_POINT('Ctrl Pts',(200.601172955896,10.4851331052859,28.4407516140076));
#72866=CARTESIAN_POINT('Ctrl Pts',(200.60434378326,10.5273681107945,28.4202225233599));
#72867=CARTESIAN_POINT('Ctrl Pts',(200.607514610625,10.5708792164448,28.402200825393));
#72868=CARTESIAN_POINT('Ctrl Pts',(200.610685437989,10.6153380446159,28.3868377285498));
#72869=CARTESIAN_POINT('Ctrl Pts',(200.61385453493,10.6597726101605,28.3714830158476));
#72870=CARTESIAN_POINT('Ctrl Pts',(200.61702363187,10.7051533481686,28.3587842115252));
#72871=CARTESIAN_POINT('Ctrl Pts',(200.620192728811,10.7511332497709,28.3488438841189));
#72872=CARTESIAN_POINT('Ctrl Pts',(200.623361486869,10.7971082345838,28.3389046196661));
#72873=CARTESIAN_POINT('Ctrl Pts',(200.626530244927,10.8436817113453,28.3317233618479));
#72874=CARTESIAN_POINT('Ctrl Pts',(200.629699002986,10.8904955705373,28.32735178232));
#72875=CARTESIAN_POINT('Ctrl Pts',(200.632870947417,10.9373565038202,28.3229758069116));
#72876=CARTESIAN_POINT('Ctrl Pts',(200.636042891848,10.9844577463792,28.3214151967753));
#72877=CARTESIAN_POINT('Ctrl Pts',(200.639214836279,11.0314371450912,28.3226696434694));
#72878=CARTESIAN_POINT('Ctrl Pts',(200.642388725544,11.0784453485838,28.3239248593104));
#72879=CARTESIAN_POINT('Ctrl Pts',(200.64556261481,11.1253310047503,28.3279985183767));
#72880=CARTESIAN_POINT('Ctrl Pts',(200.648736504076,11.1717366866115,28.3348383919079));
#72881=CARTESIAN_POINT('Ctrl Pts',(200.65191600855,11.2182244688689,28.3416903664644));
#72882=CARTESIAN_POINT('Ctrl Pts',(200.655095513024,11.2642300394651,28.3513181999576));
#72883=CARTESIAN_POINT('Ctrl Pts',(200.658275017497,11.3094077005038,28.3636189295096));
#72884=CARTESIAN_POINT('Ctrl Pts',(200.659007181767,11.3198110414896,28.3664514950068));
#72885=CARTESIAN_POINT('Ctrl Pts',(200.659739346037,11.33017055685,28.3694255918482));
#72886=CARTESIAN_POINT('Ctrl Pts',(200.660471510307,11.3404821730351,28.3725396005423));
#72887=CARTESIAN_POINT('Ctrl Pts',(200.663748672754,11.3866368991321,28.3864778829378));
#72888=CARTESIAN_POINT('Ctrl Pts',(200.667025835201,11.4320384548995,28.4032864200174));
#72889=CARTESIAN_POINT('Ctrl Pts',(200.670302997649,11.4763064424699,28.4228615523705));
#72890=CARTESIAN_POINT('Ctrl Pts',(200.673476949983,11.519180265401,28.4418201905292));
#72891=CARTESIAN_POINT('Ctrl Pts',(200.676650902317,11.5609903132395,28.463373491059));
#72892=CARTESIAN_POINT('Ctrl Pts',(200.679824854651,11.6014060442784,28.4873767569301));
#72893=CARTESIAN_POINT('Ctrl Pts',(200.682995682023,11.6417819833963,28.5113563900218));
#72894=CARTESIAN_POINT('Ctrl Pts',(200.686166509394,11.6807658463069,28.5377809307864));
#72895=CARTESIAN_POINT('Ctrl Pts',(200.689337336765,11.718050729299,28.5664593138737));
#72896=CARTESIAN_POINT('Ctrl Pts',(200.692506433713,11.7553152647206,28.5951220462368));
#72897=CARTESIAN_POINT('Ctrl Pts',(200.695675530661,11.7908822164014,28.626035845272));
#72898=CARTESIAN_POINT('Ctrl Pts',(200.698844627609,11.824475053101,28.6589673316011));
#72899=CARTESIAN_POINT('Ctrl Pts',(200.702013385675,11.8580642976036,28.6918952964537));
#72900=CARTESIAN_POINT('Ctrl Pts',(200.70518214374,11.8896794504308,28.7268401290094));
#72901=CARTESIAN_POINT('Ctrl Pts',(200.708350901806,11.9190803799067,28.7635311834364));
#72902=CARTESIAN_POINT('Ctrl Pts',(200.711522846244,11.9485108737482,28.8002591328789));
#72903=CARTESIAN_POINT('Ctrl Pts',(200.714694790682,11.9757223546312,28.8387363712393));
#72904=CARTESIAN_POINT('Ctrl Pts',(200.717866735121,12.0005158768177,28.8786602839543));
#72905=CARTESIAN_POINT('Ctrl Pts',(200.721040624394,12.0253246008159,28.9186086754748));
#72906=CARTESIAN_POINT('Ctrl Pts',(200.724214513667,12.0477121510873,28.9600050165492));
#72907=CARTESIAN_POINT('Ctrl Pts',(200.72738840294,12.0675255417332,29.0025220806435));
#72908=CARTESIAN_POINT('Ctrl Pts',(200.730567907421,12.0873739860007,29.0451143654361));
#72909=CARTESIAN_POINT('Ctrl Pts',(200.733747411902,12.1046389855921,29.0888308097341));
#72910=CARTESIAN_POINT('Ctrl Pts',(200.736926916384,12.1192163758018,29.1333260758697));
#72911=CARTESIAN_POINT('Ctrl Pts',(200.737659080603,12.1225732018677,29.1435722768031));
#72912=CARTESIAN_POINT('Ctrl Pts',(200.738391244822,12.1257877244891,29.1538597273475));
#72913=CARTESIAN_POINT('Ctrl Pts',(200.739123409041,12.1288590554845,29.1641841347546));
#72914=CARTESIAN_POINT('Ctrl Pts',(200.742400571488,12.1426063137344,29.2103961174795));
#72915=CARTESIAN_POINT('Ctrl Pts',(200.745677733935,12.1535422530453,29.2575578966654));
#72916=CARTESIAN_POINT('Ctrl Pts',(200.748954896383,12.1615442035913,29.305294772532));
#72917=CARTESIAN_POINT('Ctrl Pts',(200.752128848714,12.1692941427532,29.3515282354373));
#72918=CARTESIAN_POINT('Ctrl Pts',(200.755302801045,12.1742920693538,29.3983005091628));
#72919=CARTESIAN_POINT('Ctrl Pts',(200.758476753376,12.1764770088296,29.4452559574436));
#72920=CARTESIAN_POINT('Ctrl Pts',(200.761647580744,12.17865979709,29.4921651750252));
#72921=CARTESIAN_POINT('Ctrl Pts',(200.764818408113,12.1780350544799,29.5392566563634));
#72922=CARTESIAN_POINT('Ctrl Pts',(200.767989235481,12.1745935321515,29.5861690009678));
#72923=CARTESIAN_POINT('Ctrl Pts',(200.771158332426,12.1711538879736,29.6330557439832));
#72924=CARTESIAN_POINT('Ctrl Pts',(200.774327429371,12.1649005500777,29.6797629895004));
#72925=CARTESIAN_POINT('Ctrl Pts',(200.777496526315,12.1558763137879,29.7259314270396));
#72926=CARTESIAN_POINT('Ctrl Pts',(200.780665284378,12.1468530424906,29.7720949276293));
#72927=CARTESIAN_POINT('Ctrl Pts',(200.78383404244,12.1350595700837,29.8177191888861));
#72928=CARTESIAN_POINT('Ctrl Pts',(200.787002800503,12.1205898359021,29.8624548001793));
#72929=CARTESIAN_POINT('Ctrl Pts',(200.790174744938,12.1061055515507,29.9072353957635));
#72930=CARTESIAN_POINT('Ctrl Pts',(200.793346689373,12.0889398095057,29.9511250284773));
#72931=CARTESIAN_POINT('Ctrl Pts',(200.796518633808,12.0692359015845,29.9937910988088));
#72932=CARTESIAN_POINT('Ctrl Pts',(200.799692523078,12.0495199124794,30.0364833292627));
#72933=CARTESIAN_POINT('Ctrl Pts',(200.802866412348,12.0272629241048,30.0779500137933));
#72934=CARTESIAN_POINT('Ctrl Pts',(200.806040301618,12.0026540628077,30.1178833974425));
#72935=CARTESIAN_POINT('Ctrl Pts',(200.809219806096,11.9780016637975,30.1578874307729));
#72936=CARTESIAN_POINT('Ctrl Pts',(200.812399310575,11.9509894146852,30.1963522992468));
#72937=CARTESIAN_POINT('Ctrl Pts',(200.815578815053,11.9218484211995,30.2330010578655));
#72938=CARTESIAN_POINT('Ctrl Pts',(200.816310979293,11.9151379436652,30.2414403950999));
#72939=CARTESIAN_POINT('Ctrl Pts',(200.817043143534,11.9083147429375,30.2497835799293));
#72940=CARTESIAN_POINT('Ctrl Pts',(200.817775307775,11.9013819154724,30.2580275093685));
#72941=CARTESIAN_POINT('Ctrl Pts',(200.821052470222,11.8703506241902,30.2949272846798));
#72942=CARTESIAN_POINT('Ctrl Pts',(200.82432963267,11.8369797557264,30.3300016816453));
#72943=CARTESIAN_POINT('Ctrl Pts',(200.827606795117,11.8015147581959,30.3629421503752));
#72944=CARTESIAN_POINT('Ctrl Pts',(200.830780747448,11.7671666862285,30.3948452004064));
#72945=CARTESIAN_POINT('Ctrl Pts',(200.833954699779,11.7308548851155,30.4247463368333));
#72946=CARTESIAN_POINT('Ctrl Pts',(200.83712865211,11.6928428181089,30.4523990192639));
#72947=CARTESIAN_POINT('Ctrl Pts',(200.840299479478,11.65486817646,30.4800244758263));
#72948=CARTESIAN_POINT('Ctrl Pts',(200.843470306847,11.6151970307804,30.5054055340862));
#72949=CARTESIAN_POINT('Ctrl Pts',(200.846641134215,11.574126110073,30.5283356807154));
#72950=CARTESIAN_POINT('Ctrl Pts',(200.84981023116,11.5330776031001,30.5512533136193));
#72951=CARTESIAN_POINT('Ctrl Pts',(200.852979328104,11.4906313198475,30.5717224136642));
#72952=CARTESIAN_POINT('Ctrl Pts',(200.856148425049,11.4471108709277,30.5895810807821));
#72953=CARTESIAN_POINT('Ctrl Pts',(200.859317183112,11.4035950757988,30.6074378382115));
#72954=CARTESIAN_POINT('Ctrl Pts',(200.862485941174,11.3590058587834,30.6226845077689));
#72955=CARTESIAN_POINT('Ctrl Pts',(200.865654699236,11.3136866947387,30.6352073467186));
#72956=CARTESIAN_POINT('Ctrl Pts',(200.868826643672,11.2683219596065,30.6477427781202));
#72957=CARTESIAN_POINT('Ctrl Pts',(200.871998588107,11.222226350993,30.6575487674259));
#72958=CARTESIAN_POINT('Ctrl Pts',(200.875170532542,11.1757564507571,30.6645620346367));
#72959=CARTESIAN_POINT('Ctrl Pts',(200.878344421812,11.1292580581322,30.6715796019372));
#72960=CARTESIAN_POINT('Ctrl Pts',(200.881518311082,11.0823854718833,30.6758009898391));
#72961=CARTESIAN_POINT('Ctrl Pts',(200.884692200352,11.0354997368489,30.6772148619448));
#72962=CARTESIAN_POINT('Ctrl Pts',(200.88787170483,10.9885310521139,30.6786312354566));
#72963=CARTESIAN_POINT('Ctrl Pts',(200.891051209308,10.9415497279046,30.6772302056954));
#72964=CARTESIAN_POINT('Ctrl Pts',(200.894230713786,10.8949141696163,30.6730524416038));
#72965=CARTESIAN_POINT('Ctrl Pts',(200.894962878027,10.8841751099998,30.6720904019222));
#72966=CARTESIAN_POINT('Ctrl Pts',(200.895695042268,10.8734543464279,30.6709813348348));
#72967=CARTESIAN_POINT('Ctrl Pts',(200.896427206509,10.8627561735106,30.6697261194786));
#72968=CARTESIAN_POINT('Ctrl Pts',(200.899606238141,10.8163050793372,30.6642760181234));
#72969=CARTESIAN_POINT('Ctrl Pts',(200.902785269774,10.7700774970728,30.6560427733853));
#72970=CARTESIAN_POINT('Ctrl Pts',(200.905964301406,10.7244319227464,30.6450577702888));
#72971=CARTESIAN_POINT('Ctrl Pts',(200.909138523191,10.6788554097755,30.6340893874061));
#72972=CARTESIAN_POINT('Ctrl Pts',(200.912312744977,10.6338596985013,30.6203776167579));
#72973=CARTESIAN_POINT('Ctrl Pts',(200.915486966762,10.5897959969861,30.6040053162967));
#72974=CARTESIAN_POINT('Ctrl Pts',(200.918657779357,10.5457796209378,30.5876506000769));
#72975=CARTESIAN_POINT('Ctrl Pts',(200.921828591952,10.502693791468,30.5686412074309));
#72976=CARTESIAN_POINT('Ctrl Pts',(200.924999404548,10.4608747409026,30.5471098402284));
#72977=CARTESIAN_POINT('Ctrl Pts',(200.92816893808,10.4190725595717,30.5255871584857));
#72978=CARTESIAN_POINT('Ctrl Pts',(200.931338471613,10.3785366434163,30.5015447637476));
#72979=CARTESIAN_POINT('Ctrl Pts',(200.934508005146,10.3395811204066,30.4751625331075));
#72980=CARTESIAN_POINT('Ctrl Pts',(200.937676853713,10.3006340160467,30.4487860039121));
#72981=CARTESIAN_POINT('Ctrl Pts',(200.94084570228,10.2632670839165,30.4200709604753));
#72982=CARTESIAN_POINT('Ctrl Pts',(200.944014550847,10.2277652659539,30.3892404500655));
#72983=CARTESIAN_POINT('Ctrl Pts',(200.947185350756,10.1922415863641,30.3583909545682));
#72984=CARTESIAN_POINT('Ctrl Pts',(200.950356150665,10.1585857254588,30.3254237667288));
#72985=CARTESIAN_POINT('Ctrl Pts',(200.953526950575,10.1270475916668,30.2906005029629));
#72986=CARTESIAN_POINT('Ctrl Pts',(200.954355234997,10.1188091200833,30.2815038813661));
#72987=CARTESIAN_POINT('Ctrl Pts',(200.95518351942,10.1107149503495,30.2722807907571));
#72988=CARTESIAN_POINT('Ctrl Pts',(200.956011803843,10.1027690874833,30.2629362700282));
#72989=CARTESIAN_POINT('Origin',(197.762132885264,11.,29.5));
#72990=CARTESIAN_POINT('',(201.555825452273,10.1027690875306,30.2629362700837));
#72991=CARTESIAN_POINT('',(201.456090246984,10.1027690874833,30.2629362700282));
#72992=CARTESIAN_POINT('',(197.762132885264,10.1027690874833,30.2629362700282));
#72993=CARTESIAN_POINT('',(201.110124610169,9.82225025635667,29.4992229233845));
#72994=CARTESIAN_POINT('Ctrl Pts',(201.555825452273,10.1027690875306,30.2629362700837));
#72995=CARTESIAN_POINT('Ctrl Pts',(201.555549618905,10.1054509716362,30.2660902285697));
#72996=CARTESIAN_POINT('Ctrl Pts',(201.555273125248,10.1081494677841,30.2692300245477));
#72997=CARTESIAN_POINT('Ctrl Pts',(201.554388159376,10.1168182882239,30.2792095689722));
#72998=CARTESIAN_POINT('Ctrl Pts',(201.553777178604,10.1228510196037,30.2859943681334));
#72999=CARTESIAN_POINT('Ctrl Pts',(201.552385338527,10.1366973122065,30.301208855377));
#73000=CARTESIAN_POINT('Ctrl Pts',(201.551602596718,10.1445569451021,30.3095951608155));
#73001=CARTESIAN_POINT('Ctrl Pts',(201.549175793606,10.1691388209297,30.3350666187593));
#73002=CARTESIAN_POINT('Ctrl Pts',(201.547515014436,10.1862586031458,30.3517578027237));
#73003=CARTESIAN_POINT('Ctrl Pts',(201.543511585319,10.2282022413078,30.3902321071941));
#73004=CARTESIAN_POINT('Ctrl Pts',(201.541151785278,10.2534568057504,30.4115140878609));
#73005=CARTESIAN_POINT('Ctrl Pts',(201.535397084206,10.3164119606738,30.4601933751533));
#73006=CARTESIAN_POINT('Ctrl Pts',(201.531979012937,10.3549096272088,30.4864694451067));
#73007=CARTESIAN_POINT('Ctrl Pts',(201.524701344481,10.4400888838457,30.5374844889861));
#73008=CARTESIAN_POINT('Ctrl Pts',(201.520850663775,10.4870900714472,30.5615078491844));
#73009=CARTESIAN_POINT('Ctrl Pts',(201.516251513878,10.5470315736418,30.5872308226599));
#73010=CARTESIAN_POINT('Ctrl Pts',(201.515378181647,10.5585947989421,30.5919765272682));
#73011=CARTESIAN_POINT('Ctrl Pts',(201.514080942196,10.5760746681723,30.5988274464456));
#73012=CARTESIAN_POINT('Ctrl Pts',(201.51364979859,10.5819357851087,30.6010707337444));
#73013=CARTESIAN_POINT('Ctrl Pts',(201.51287173044,10.5926121856065,30.6050594823032));
#73014=CARTESIAN_POINT('Ctrl Pts',(201.512523964578,10.5974211688158,30.6068204810458));
#73015=CARTESIAN_POINT('Ctrl Pts',(201.511719997017,10.6086234810071,30.6108399759856));
#73016=CARTESIAN_POINT('Ctrl Pts',(201.511265144791,10.6150250266977,30.6130747087543));
#73017=CARTESIAN_POINT('Ctrl Pts',(201.509796398557,10.6358891553626,30.6201566872447));
#73018=CARTESIAN_POINT('Ctrl Pts',(201.508794278056,10.6504273009084,30.6247785077277));
#73019=CARTESIAN_POINT('Ctrl Pts',(201.502202986934,10.7477244750533,30.6536413318068));
#73020=CARTESIAN_POINT('Ctrl Pts',(201.496972088734,10.8328495788635,30.6690147384302));
#73021=CARTESIAN_POINT('Ctrl Pts',(201.488076790026,10.9754427654419,30.6788572922696));
#73022=CARTESIAN_POINT('Ctrl Pts',(201.484505489542,11.0321889077722,30.678673128179));
#73023=CARTESIAN_POINT('Ctrl Pts',(201.479808585131,11.1040058410088,30.6732491369712));
#73024=CARTESIAN_POINT('Ctrl Pts',(201.478799070319,11.1192897628913,30.671793782937));
#73025=CARTESIAN_POINT('Ctrl Pts',(201.477129171945,11.1442910596495,30.668918939284));
#73026=CARTESIAN_POINT('Ctrl Pts',(201.476474247601,11.1540271455874,30.6676759076095));
#73027=CARTESIAN_POINT('Ctrl Pts',(201.475187604885,11.1730116136353,30.6650105501108));
#73028=CARTESIAN_POINT('Ctrl Pts',(201.474556278589,11.1822608431334,30.6635994056202));
#73029=CARTESIAN_POINT('Ctrl Pts',(201.473042171879,11.2042798620371,30.6599710207039));
#73030=CARTESIAN_POINT('Ctrl Pts',(201.472156323961,11.2170315548777,30.6576529324552));
#73031=CARTESIAN_POINT('Ctrl Pts',(201.468961859277,11.2625324210609,30.6486032979458));
#73032=CARTESIAN_POINT('Ctrl Pts',(201.466617322494,11.2950272742429,30.6406889769245));
#73033=CARTESIAN_POINT('Ctrl Pts',(201.46028820531,11.3803838628948,30.6160086090594));
#73034=CARTESIAN_POINT('Ctrl Pts',(201.456244397918,11.432470907913,30.5968750927033));
#73035=CARTESIAN_POINT('Ctrl Pts',(201.447493404416,11.5413341584674,30.5479224979836));
#73036=CARTESIAN_POINT('Ctrl Pts',(201.442793146366,11.5974276542748,30.516988579471));
#73037=CARTESIAN_POINT('Ctrl Pts',(201.437436851325,11.6607878214599,30.4749871619562));
#73038=CARTESIAN_POINT('Ctrl Pts',(201.436594469793,11.6707374998226,30.4681692749309));
#73039=CARTESIAN_POINT('Ctrl Pts',(201.435328286891,11.685694011656,30.4575792562201));
#73040=CARTESIAN_POINT('Ctrl Pts',(201.434897902763,11.6907780517263,30.4539182340482));
#73041=CARTESIAN_POINT('Ctrl Pts',(201.434117162802,11.7000053584495,30.4471611834037));
#73042=CARTESIAN_POINT('Ctrl Pts',(201.433766012383,11.7041576548165,30.4440782849928));
#73043=CARTESIAN_POINT('Ctrl Pts',(201.432955784872,11.7137419336976,30.4368639620695));
#73044=CARTESIAN_POINT('Ctrl Pts',(201.432498061956,11.7191584954838,30.4327125469762));
#73045=CARTESIAN_POINT('Ctrl Pts',(201.431009475686,11.736767603365,30.4189717954543));
#73046=CARTESIAN_POINT('Ctrl Pts',(201.429990830916,11.7488073735372,30.4091882281754));
#73047=CARTESIAN_POINT('Ctrl Pts',(201.427504514035,11.7780513681171,30.3844493067417));
#73048=CARTESIAN_POINT('Ctrl Pts',(201.426050920933,11.7950218120127,30.3692266369248));
#73049=CARTESIAN_POINT('Ctrl Pts',(201.418825676392,11.87800179582,30.2903279381873));
#73050=CARTESIAN_POINT('Ctrl Pts',(201.413286511841,11.9368549665042,30.2195896578896));
#73051=CARTESIAN_POINT('Ctrl Pts',(201.405393041502,12.0047709597261,30.1153064062986));
#73052=CARTESIAN_POINT('Ctrl Pts',(201.403288041948,12.021482877036,30.087144871367));
#73053=CARTESIAN_POINT('Ctrl Pts',(201.400276817889,12.0432584451949,30.0467002885503));
#73054=CARTESIAN_POINT('Ctrl Pts',(201.39940495484,12.049321458575,30.0349708802921));
#73055=CARTESIAN_POINT('Ctrl Pts',(201.397907086474,12.0593188706077,30.0148059549901));
#73056=CARTESIAN_POINT('Ctrl Pts',(201.397284545475,12.0633528893501,30.0064210355883));
#73057=CARTESIAN_POINT('Ctrl Pts',(201.396004583675,12.0713976682063,29.9891795274967));
#73058=CARTESIAN_POINT('Ctrl Pts',(201.395346901066,12.0753989496729,29.9803193342964));
#73059=CARTESIAN_POINT('Ctrl Pts',(201.393672237542,12.0852510767664,29.9577629967835));
#73060=CARTESIAN_POINT('Ctrl Pts',(201.392650390361,12.0909525130591,29.9440038740498));
#73061=CARTESIAN_POINT('Ctrl Pts',(201.387908649118,12.1159822610865,29.8802052438645));
#73062=CARTESIAN_POINT('Ctrl Pts',(201.38408836531,12.1321361753797,29.8289964975176));
#73063=CARTESIAN_POINT('Ctrl Pts',(201.379013107253,12.1485851880693,29.7609869860538));
#73064=CARTESIAN_POINT('Ctrl Pts',(201.377822164519,12.1520959573422,29.745024538644));
#73065=CARTESIAN_POINT('Ctrl Pts',(201.371270938611,12.1695242082937,29.6570993215936));
#73066=CARTESIAN_POINT('Ctrl Pts',(201.365846509798,12.1770332629156,29.5840282430586));
#73067=CARTESIAN_POINT('Ctrl Pts',(201.359641872036,12.1778298736185,29.4965991976671));
#73068=CARTESIAN_POINT('Ctrl Pts',(201.358648162214,12.1777042800285,29.4824658365934));
#73069=CARTESIAN_POINT('Ctrl Pts',(201.357148412728,12.1771239453652,29.4608869623649));
#73070=CARTESIAN_POINT('Ctrl Pts',(201.356633905049,12.1768528487025,29.4534382971488));
#73071=CARTESIAN_POINT('Ctrl Pts',(201.355763601846,12.1762704959815,29.4407522067386));
#73072=CARTESIAN_POINT('Ctrl Pts',(201.35540595734,12.1759949284964,29.4355134641921));
#73073=CARTESIAN_POINT('Ctrl Pts',(201.35465083073,12.1753355889074,29.4243956227917));
#73074=CARTESIAN_POINT('Ctrl Pts',(201.354253833354,12.1749426989966,29.4185173258228));
#73075=CARTESIAN_POINT('Ctrl Pts',(201.353148673834,12.1737192878163,29.4020688662455));
#73076=CARTESIAN_POINT('Ctrl Pts',(201.352445587332,12.1727900976472,29.391506316014));
#73077=CARTESIAN_POINT('Ctrl Pts',(201.350854026918,12.1703423423246,29.3674134472792));
#73078=CARTESIAN_POINT('Ctrl Pts',(201.349969715226,12.1687315426173,29.353893852848));
#73079=CARTESIAN_POINT('Ctrl Pts',(201.34699754887,12.1624734799147,29.3081378239526));
#73080=CARTESIAN_POINT('Ctrl Pts',(201.344949057344,12.1567235719836,29.276065773533));
#73081=CARTESIAN_POINT('Ctrl Pts',(201.336773311026,12.1282519611206,29.1480690286486));
#73082=CARTESIAN_POINT('Ctrl Pts',(201.330786981782,12.0948649423851,29.0549408565797));
#73083=CARTESIAN_POINT('Ctrl Pts',(201.323226871369,12.0420926889981,28.9509421419043));
#73084=CARTESIAN_POINT('Ctrl Pts',(201.322044160784,12.0335448886444,28.9350162733253));
#73085=CARTESIAN_POINT('Ctrl Pts',(201.320156042155,12.0194692232059,28.9101802775707));
#73086=CARTESIAN_POINT('Ctrl Pts',(201.319459065865,12.0141828299515,28.9011360941359));
#73087=CARTESIAN_POINT('Ctrl Pts',(201.318150026819,12.0040912363104,28.8843878896256));
#73088=CARTESIAN_POINT('Ctrl Pts',(201.317539078791,11.9993162007732,28.8766665384385));
#73089=CARTESIAN_POINT('Ctrl Pts',(201.316147596791,11.9882972248495,28.8593006567634));
#73090=CARTESIAN_POINT('Ctrl Pts',(201.315365184199,11.982000542372,28.8496908644555));
#73091=CARTESIAN_POINT('Ctrl Pts',(201.312940548797,11.9621861421804,28.8203948766583));
#73092=CARTESIAN_POINT('Ctrl Pts',(201.311281651661,11.9482102224543,28.8010275190197));
#73093=CARTESIAN_POINT('Ctrl Pts',(201.307283867745,11.9135638720506,28.755968661839));
#73094=CARTESIAN_POINT('Ctrl Pts',(201.304927897913,11.8923849995774,28.730694935336));
#73095=CARTESIAN_POINT('Ctrl Pts',(201.299172823292,11.8387511730918,28.6718900263226));
#73096=CARTESIAN_POINT('Ctrl Pts',(201.295750278093,11.805309367304,28.6393339154061));
#73097=CARTESIAN_POINT('Ctrl Pts',(201.288466081575,11.7301155866324,28.574360426116));
#73098=CARTESIAN_POINT('Ctrl Pts',(201.284613343666,11.6879281734789,28.542590367015));
#73099=CARTESIAN_POINT('Ctrl Pts',(201.280012116475,11.633282144719,28.5069214373652));
#73100=CARTESIAN_POINT('Ctrl Pts',(201.279138643055,11.6227062379737,28.5002558936441));
#73101=CARTESIAN_POINT('Ctrl Pts',(201.277841237762,11.6066637765065,28.4904983847786));
#73102=CARTESIAN_POINT('Ctrl Pts',(201.277410066887,11.6012757070054,28.487279911585));
#73103=CARTESIAN_POINT('Ctrl Pts',(201.276631973568,11.5914445068039,28.4815135318708));
#73104=CARTESIAN_POINT('Ctrl Pts',(201.276284209448,11.5870102591065,28.4789513978604));
#73105=CARTESIAN_POINT('Ctrl Pts',(201.275480276416,11.5766670445097,28.4730646831912));
#73106=CARTESIAN_POINT('Ctrl Pts',(201.275025456543,11.57074589883,28.469762090791));
#73107=CARTESIAN_POINT('Ctrl Pts',(201.273556932732,11.5514143989914,28.459197529091));
#73108=CARTESIAN_POINT('Ctrl Pts',(201.272554997358,11.5378908723992,28.4521445307378));
#73109=CARTESIAN_POINT('Ctrl Pts',(201.265967158782,11.4470592720983,28.4069947432926));
#73110=CARTESIAN_POINT('Ctrl Pts',(201.260739134868,11.365899126778,28.3772160635964));
#73111=CARTESIAN_POINT('Ctrl Pts',(201.251844010635,11.2271299694692,28.3429669841012));
#73112=CARTESIAN_POINT('Ctrl Pts',(201.248269598779,11.1711480511288,28.3333720983529));
#73113=CARTESIAN_POINT('Ctrl Pts',(201.24356923747,11.0994158996172,28.3263529986118));
#73114=CARTESIAN_POINT('Ctrl Pts',(201.242559613089,11.0841077992264,28.3251567560074));
#73115=CARTESIAN_POINT('Ctrl Pts',(201.240889581241,11.0589826527097,28.3236869251502));
#73116=CARTESIAN_POINT('Ctrl Pts',(201.240234634754,11.0491775394609,28.3232362330219));
#73117=CARTESIAN_POINT('Ctrl Pts',(201.238947983311,11.030017432227,28.3225954176414));
#73118=CARTESIAN_POINT('Ctrl Pts',(201.238316670836,11.0206635277601,28.3223941207709));
#73119=CARTESIAN_POINT('Ctrl Pts',(201.236802655575,10.9983498961897,28.3221798613185));
#73120=CARTESIAN_POINT('Ctrl Pts',(201.235916886265,10.9853906440994,28.3222693238348));
#73121=CARTESIAN_POINT('Ctrl Pts',(201.232723091143,10.9390208556698,28.3233548597041));
#73122=CARTESIAN_POINT('Ctrl Pts',(201.230379165481,10.9056573083935,28.3255591434639));
#73123=CARTESIAN_POINT('Ctrl Pts',(201.224052454285,10.8173596809428,28.3351794543637));
#73124=CARTESIAN_POINT('Ctrl Pts',(201.220010502055,10.762780938074,28.3450582422521));
#73125=CARTESIAN_POINT('Ctrl Pts',(201.211258505371,10.6471023444632,28.37454347029));
#73126=CARTESIAN_POINT('Ctrl Pts',(201.206555322366,10.5864856007286,28.3953750237505));
#73127=CARTESIAN_POINT('Ctrl Pts',(201.201196459391,10.5168103299881,28.4258639694471));
#73128=CARTESIAN_POINT('Ctrl Pts',(201.200354201222,10.5058375778034,28.4308676426956));
#73129=CARTESIAN_POINT('Ctrl Pts',(201.19908816495,10.4892839566599,28.4387255641742));
#73130=CARTESIAN_POINT('Ctrl Pts',(201.198657806269,10.4836461688041,28.4414571191947));
#73131=CARTESIAN_POINT('Ctrl Pts',(201.1978770897,10.4733941885005,28.4465256866687));
#73132=CARTESIAN_POINT('Ctrl Pts',(201.197525937561,10.4687733628306,28.448848216792));
#73133=CARTESIAN_POINT('Ctrl Pts',(201.196715677012,10.4580903152521,28.4543061961582));
#73134=CARTESIAN_POINT('Ctrl Pts',(201.196257923197,10.452039848233,28.4574639980012));
#73135=CARTESIAN_POINT('Ctrl Pts',(201.19476912224,10.432326330276,28.4679717282163));
#73136=CARTESIAN_POINT('Ctrl Pts',(201.193750298548,10.4187804081867,28.4755393663561));
#73137=CARTESIAN_POINT('Ctrl Pts',(201.191263439141,10.3857088674029,28.4948825062888));
#73138=CARTESIAN_POINT('Ctrl Pts',(201.18980949043,10.3663676710592,28.5069617510702));
#73139=CARTESIAN_POINT('Ctrl Pts',(201.182579463854,10.2709879025143,28.5704518274736));
#73140=CARTESIAN_POINT('Ctrl Pts',(201.177036154116,10.2007937373166,28.6300638566814));
#73141=CARTESIAN_POINT('Ctrl Pts',(201.169141401909,10.1159590098412,28.7211326861858));
#73142=CARTESIAN_POINT('Ctrl Pts',(201.167040102228,10.0946929720052,28.7459564573821));
#73143=CARTESIAN_POINT('Ctrl Pts',(201.164033289955,10.0663277279381,28.7819991352735));
#73144=CARTESIAN_POINT('Ctrl Pts',(201.163161999316,10.0583428892701,28.7925036986413));
#73145=CARTESIAN_POINT('Ctrl Pts',(201.161664806267,10.0450318712351,28.810639800074));
#73146=CARTESIAN_POINT('Ctrl Pts',(201.161042360163,10.0396164721958,28.8182045149888));
#73147=CARTESIAN_POINT('Ctrl Pts',(201.159762321224,10.0287250994101,28.8338058175555));
#73148=CARTESIAN_POINT('Ctrl Pts',(201.159104463604,10.0232579228957,28.8418476419992));
#73149=CARTESIAN_POINT('Ctrl Pts',(201.157428781072,10.0096644400586,28.8623851463101));
#73150=CARTESIAN_POINT('Ctrl Pts',(201.156406077854,10.0016748186599,28.8749687846016));
#73151=CARTESIAN_POINT('Ctrl Pts',(201.1516502623,9.965940543406,28.933683988276));
#73152=CARTESIAN_POINT('Ctrl Pts',(201.147815996433,9.94114400401658,28.9815259589734));
#73153=CARTESIAN_POINT('Ctrl Pts',(201.141216324113,9.90490749591627,29.0649733195644));
#73154=CARTESIAN_POINT('Ctrl Pts',(201.138492222391,9.8917287098359,29.0997371158308));
#73155=CARTESIAN_POINT('Ctrl Pts',(201.131710446974,9.86306996553872,29.1876748563525));
#73156=CARTESIAN_POINT('Ctrl Pts',(201.127658525455,9.84965186003018,29.2414326784359));
#73157=CARTESIAN_POINT('Ctrl Pts',(201.122789792463,9.83771537926866,29.3092826729482));
#73158=CARTESIAN_POINT('Ctrl Pts',(201.121841224332,9.83559814392707,29.322666996057));
#73159=CARTESIAN_POINT('Ctrl Pts',(201.120456024267,9.83281099339859,29.3424981917767));
#73160=CARTESIAN_POINT('Ctrl Pts',(201.12001070515,9.83196261412641,29.3489183439737));
#73161=CARTESIAN_POINT('Ctrl Pts',(201.119215656273,9.8305333574789,29.3604669671642));
#73162=CARTESIAN_POINT('Ctrl Pts',(201.118864938291,9.82993318506185,29.365592610796));
#73163=CARTESIAN_POINT('Ctrl Pts',(201.118176884112,9.82881593833743,29.3757094893251));
#73164=CARTESIAN_POINT('Ctrl Pts',(201.117839437719,9.82829705199674,29.3807002043782));
#73165=CARTESIAN_POINT('Ctrl Pts',(201.117064830852,9.82717379658595,29.3922190304139));
#73166=CARTESIAN_POINT('Ctrl Pts',(201.116628827027,9.82659200228432,29.3987492403682));
#73167=CARTESIAN_POINT('Ctrl Pts',(201.115395904236,9.82509240713505,29.4173356485609));
#73168=CARTESIAN_POINT('Ctrl Pts',(201.114605096929,9.82430565885677,29.4294019282801));
#73169=CARTESIAN_POINT('Ctrl Pts',(201.112573089147,9.82274800621775,29.4607111913763));
#73170=CARTESIAN_POINT('Ctrl Pts',(201.111342978938,9.8222629626427,29.4799650731109));
#73171=CARTESIAN_POINT('Ctrl Pts',(201.110124610169,9.82225025635667,29.4992229233845));
#73172=CARTESIAN_POINT('Ctrl Pts',(201.110124713057,9.82225025743081,29.4992212971066));
#73173=CARTESIAN_POINT('Ctrl Pts',(201.104151888081,9.82218783691321,29.5936292531427));
#73174=CARTESIAN_POINT('Ctrl Pts',(201.098460114152,9.83347653828057,29.6877030432394));
#73175=CARTESIAN_POINT('Ctrl Pts',(201.090358931108,9.86377767613873,29.8117737585436));
#73176=CARTESIAN_POINT('Ctrl Pts',(201.088216876693,9.87304639088254,29.8437721711053));
#73177=CARTESIAN_POINT('Ctrl Pts',(201.08518348506,9.88778237809044,29.8876010103538));
#73178=CARTESIAN_POINT('Ctrl Pts',(201.084328321107,9.89210892235285,29.8997998502548));
#73179=CARTESIAN_POINT('Ctrl Pts',(201.082843920557,9.89990683947174,29.9206870379719));
#73180=CARTESIAN_POINT('Ctrl Pts',(201.082217850589,9.90328237405759,29.929410044389));
#73181=CARTESIAN_POINT('Ctrl Pts',(201.080927360193,9.91041430718043,29.9472074703001));
#73182=CARTESIAN_POINT('Ctrl Pts',(201.080262638926,9.91418102266728,29.9562769355842));
#73183=CARTESIAN_POINT('Ctrl Pts',(201.078547179923,9.92413640189605,29.9794257922263));
#73184=CARTESIAN_POINT('Ctrl Pts',(201.077491086649,9.93048805947844,29.9934326120486));
#73185=CARTESIAN_POINT('Ctrl Pts',(201.072441890579,9.96188800024985,30.0592199816247));
#73186=CARTESIAN_POINT('Ctrl Pts',(201.068332657324,9.99042988014662,30.1092372043916));
#73187=CARTESIAN_POINT('Ctrl Pts',(201.060922689542,10.0472623805589,30.1937980300933));
#73188=CARTESIAN_POINT('Ctrl Pts',(201.05766110407,10.0740622414228,30.2291763656033));
#73189=CARTESIAN_POINT('Ctrl Pts',(201.054417864302,10.1027692940023,30.2629365128992));
#73190=CARTESIAN_POINT('',(201.01213288523,9.8222500132958,29.5001769696233));
#73191=CARTESIAN_POINT('Ctrl Pts',(200.956011803843,10.1027690874833,30.2629362700282));
#73192=CARTESIAN_POINT('Ctrl Pts',(200.959190471249,10.0722756306458,30.2270752509904));
#73193=CARTESIAN_POINT('Ctrl Pts',(200.962369138654,10.043969850099,30.1894237375346));
#73194=CARTESIAN_POINT('Ctrl Pts',(200.965547806059,10.0180504941751,30.1502847303376));
#73195=CARTESIAN_POINT('Ctrl Pts',(200.968724905787,9.99214392133812,30.1111650259864));
#73196=CARTESIAN_POINT('Ctrl Pts',(200.971902005515,9.96862164118809,30.0705598070775));
#73197=CARTESIAN_POINT('Ctrl Pts',(200.975079105243,9.94763539218599,30.028794662152));
#73198=CARTESIAN_POINT('Ctrl Pts',(200.97846066285,9.92529860202408,29.9843417788288));
#73199=CARTESIAN_POINT('Ctrl Pts',(200.981842220457,9.9057468437586,29.9384012012819));
#73200=CARTESIAN_POINT('Ctrl Pts',(200.985223778064,9.88916484957826,29.8913314849172));
#73201=CARTESIAN_POINT('Ctrl Pts',(200.988597235419,9.87262257624429,29.8443745203092));
#73202=CARTESIAN_POINT('Ctrl Pts',(200.991970692773,9.8590360828417,29.796294207783));
#73203=CARTESIAN_POINT('Ctrl Pts',(200.995344150128,9.84854292882478,29.7474705553002));
#73204=CARTESIAN_POINT('Ctrl Pts',(200.998706501391,9.83808432035578,29.6988076399821));
#73205=CARTESIAN_POINT('Ctrl Pts',(201.002068852654,9.83069888325395,29.6494066876973));
#73206=CARTESIAN_POINT('Ctrl Pts',(201.005431203917,9.82647429469484,29.5996618356646));
#73207=CARTESIAN_POINT('Ctrl Pts',(201.007665097688,9.82366754390407,29.566612131338));
#73208=CARTESIAN_POINT('Ctrl Pts',(201.009898991459,9.82225500706502,29.533410987548));
#73209=CARTESIAN_POINT('Ctrl Pts',(201.01213288523,9.8222500132958,29.5001769696233));
#73210=CARTESIAN_POINT('Ctrl Pts',(201.012132885264,9.82225001329572,29.5001769691125));
#73211=CARTESIAN_POINT('Ctrl Pts',(201.015413022268,9.82224268071789,29.4513778124986));
#73212=CARTESIAN_POINT('Ctrl Pts',(201.018693159271,9.82527259804305,29.4026201959092));
#73213=CARTESIAN_POINT('Ctrl Pts',(201.021973296275,9.83129844917431,29.3542888213018));
#73214=CARTESIAN_POINT('Ctrl Pts',(201.025261094398,9.83733837434069,29.3058445634769));
#73215=CARTESIAN_POINT('Ctrl Pts',(201.028548892521,9.84638813450003,29.2578290295261));
#73216=CARTESIAN_POINT('Ctrl Pts',(201.031836690643,9.85835498925079,29.2106183628296));
#73217=CARTESIAN_POINT('Ctrl Pts',(201.035128826312,9.87033763170422,29.1633454117663));
#73218=CARTESIAN_POINT('Ctrl Pts',(201.03842096198,9.88524487952968,29.1168799161247));
#73219=CARTESIAN_POINT('Ctrl Pts',(201.041713097649,9.90293469427636,29.0715810724565));
#73220=CARTESIAN_POINT('Ctrl Pts',(201.045013366669,9.92066821241159,29.0261703161995));
#73221=CARTESIAN_POINT('Ctrl Pts',(201.048313635689,9.94119781207875,28.9819324175217));
#73222=CARTESIAN_POINT('Ctrl Pts',(201.05161390471,9.96433457710791,28.9392039637036));
#73223=CARTESIAN_POINT('Ctrl Pts',(201.052319604466,9.9692819342293,28.9300672965846));
#73224=CARTESIAN_POINT('Ctrl Pts',(201.053025304222,9.97434834264665,28.9209995417588));
#73225=CARTESIAN_POINT('Ctrl Pts',(201.053731003978,9.97953170284227,28.9120038120906));
#73226=CARTESIAN_POINT('Ctrl Pts',(201.057008166425,10.0036024400579,28.8702290102759));
#73227=CARTESIAN_POINT('Ctrl Pts',(201.060285328873,10.0302968970173,28.8298404704134));
#73228=CARTESIAN_POINT('Ctrl Pts',(201.06356249132,10.0594276106822,28.7911850432214));
#73229=CARTESIAN_POINT('Ctrl Pts',(201.066736443651,10.0876408891035,28.7537470201642));
#73230=CARTESIAN_POINT('Ctrl Pts',(201.069910395983,10.1181388718815,28.7179350402314));
#73231=CARTESIAN_POINT('Ctrl Pts',(201.073084348314,10.1507054735937,28.6840380707923));
#73232=CARTESIAN_POINT('Ctrl Pts',(201.076255175683,10.1832400113639,28.650174475129));
#73233=CARTESIAN_POINT('Ctrl Pts',(201.079426003052,10.2178387525764,28.6182225577383));
#73234=CARTESIAN_POINT('Ctrl Pts',(201.08259683042,10.2542458351852,28.5884377211834));
#73235=CARTESIAN_POINT('Ctrl Pts',(201.085765927365,10.2906330492674,28.5586691391804));
#73236=CARTESIAN_POINT('Ctrl Pts',(201.088935024311,10.328826219401,28.5310656471142));
#73237=CARTESIAN_POINT('Ctrl Pts',(201.092104121256,10.3685351866865,28.5058434469125));
#73238=CARTESIAN_POINT('Ctrl Pts',(201.095272879319,10.4082399077559,28.4806239438071));
#73239=CARTESIAN_POINT('Ctrl Pts',(201.098441637381,10.4494596331683,28.4577855234577));
#73240=CARTESIAN_POINT('Ctrl Pts',(201.101610395444,10.4918761932964,28.437500466089));
#73241=CARTESIAN_POINT('Ctrl Pts',(201.10478233988,10.5343354057729,28.4171950109009));
#73242=CARTESIAN_POINT('Ctrl Pts',(201.107954284315,10.5779933502418,28.3994482803588));
#73243=CARTESIAN_POINT('Ctrl Pts',(201.111126228751,10.622510093867,28.3843851770133));
#73244=CARTESIAN_POINT('Ctrl Pts',(201.114300118021,10.6670541323296,28.3693128379303));
#73245=CARTESIAN_POINT('Ctrl Pts',(201.117474007291,10.7124574804751,28.3569275468502));
#73246=CARTESIAN_POINT('Ctrl Pts',(201.120647896562,10.7583666920129,28.3473038531464));
#73247=CARTESIAN_POINT('Ctrl Pts',(201.12382740104,10.8043571255972,28.3376631333148));
#73248=CARTESIAN_POINT('Ctrl Pts',(201.127006905519,10.8508546571298,28.330793834172));
#73249=CARTESIAN_POINT('Ctrl Pts',(201.130186409997,10.8974993081254,28.3267188441532));
#73250=CARTESIAN_POINT('Ctrl Pts',(201.130918574235,10.9082404615346,28.3257804708993));
#73251=CARTESIAN_POINT('Ctrl Pts',(201.131650738474,10.9189894168709,28.3249900534933));
#73252=CARTESIAN_POINT('Ctrl Pts',(201.132382902712,10.9297417918825,28.3243474804637));
#73253=CARTESIAN_POINT('Ctrl Pts',(201.135660065159,10.9778693536535,28.3214713276933));
#73254=CARTESIAN_POINT('Ctrl Pts',(201.138937227607,11.026282390912,28.3215488389594));
#73255=CARTESIAN_POINT('Ctrl Pts',(201.142214390054,11.0745881236887,28.3246142444692));
#73256=CARTESIAN_POINT('Ctrl Pts',(201.145388342385,11.1213725280764,28.3275831088823));
#73257=CARTESIAN_POINT('Ctrl Pts',(201.148562294717,11.1680556831734,28.333354407741));
#73258=CARTESIAN_POINT('Ctrl Pts',(201.151736247049,11.2142774053045,28.3419066289474));
#73259=CARTESIAN_POINT('Ctrl Pts',(201.154907074417,11.2604536191376,28.3504504299347));
#73260=CARTESIAN_POINT('Ctrl Pts',(201.158077901786,11.3061687540886,28.3617696328631));
#73261=CARTESIAN_POINT('Ctrl Pts',(201.161248729155,11.3510687782139,28.3757910445725));
#73262=CARTESIAN_POINT('Ctrl Pts',(201.1644178261,11.3959442989388,28.3898048043425));
#73263=CARTESIAN_POINT('Ctrl Pts',(201.167586923045,11.4400050594317,28.4065176857212));
#73264=CARTESIAN_POINT('Ctrl Pts',(201.17075601999,11.4829109002926,28.4258062908029));
#73265=CARTESIAN_POINT('Ctrl Pts',(201.173924778053,11.5258121530849,28.445092833288));
#73266=CARTESIAN_POINT('Ctrl Pts',(201.177093536116,11.5675582247912,28.4669543223567));
#73267=CARTESIAN_POINT('Ctrl Pts',(201.180262294179,11.6078302289611,28.491219808253));
#73268=CARTESIAN_POINT('Ctrl Pts',(201.183434238615,11.648142729002,28.5155096945239));
#73269=CARTESIAN_POINT('Ctrl Pts',(201.18660618305,11.6869777274219,28.5422081112936));
#73270=CARTESIAN_POINT('Ctrl Pts',(201.189778127486,11.724043933369,28.5710998734786));
#73271=CARTESIAN_POINT('Ctrl Pts',(201.192952016756,11.7611328659576,28.6000093502557));
#73272=CARTESIAN_POINT('Ctrl Pts',(201.196125906026,11.7964504300725,28.631114480428));
#73273=CARTESIAN_POINT('Ctrl Pts',(201.199299795297,11.8297399531936,28.6641610965178));
#73274=CARTESIAN_POINT('Ctrl Pts',(201.202479299775,11.8630883717543,28.6972661782989));
#73275=CARTESIAN_POINT('Ctrl Pts',(201.205658804254,11.89440122465,28.7323191803524));
#73276=CARTESIAN_POINT('Ctrl Pts',(201.208838308733,11.9234613899029,28.7690320637275));
#73277=CARTESIAN_POINT('Ctrl Pts',(201.20957047297,11.9301532545904,28.7774861673327));
#73278=CARTESIAN_POINT('Ctrl Pts',(201.210302637208,11.9367258483966,28.7860281700837));
#73279=CARTESIAN_POINT('Ctrl Pts',(201.211034801446,11.9431768539451,28.7946543509157));
#73280=CARTESIAN_POINT('Ctrl Pts',(201.214311963893,11.9720515135337,28.8332650811653));
#73281=CARTESIAN_POINT('Ctrl Pts',(201.217589126341,11.9986165065409,28.8737388916002));
#73282=CARTESIAN_POINT('Ctrl Pts',(201.220866288788,12.0226271965887,28.9157665883424));
#73283=CARTESIAN_POINT('Ctrl Pts',(201.224040241119,12.045881700107,28.9564706755556));
#73284=CARTESIAN_POINT('Ctrl Pts',(201.227214193451,12.0667401143642,28.9986316932728));
#73285=CARTESIAN_POINT('Ctrl Pts',(201.230388145782,12.0850222847301,29.0419370085468));
#73286=CARTESIAN_POINT('Ctrl Pts',(201.233558973151,12.1032864551077,29.0851996869154));
#73287=CARTESIAN_POINT('Ctrl Pts',(201.23672980052,12.1189791866155,29.129603922032));
#73288=CARTESIAN_POINT('Ctrl Pts',(201.239900627888,12.131966868801,29.1748137911335));
#73289=CARTESIAN_POINT('Ctrl Pts',(201.243069724834,12.1449474631867,29.2199989877421));
#73290=CARTESIAN_POINT('Ctrl Pts',(201.246238821779,12.155225779285,29.2659884130192));
#73291=CARTESIAN_POINT('Ctrl Pts',(201.249407918724,12.1627177647587,29.3124301143186));
#73292=CARTESIAN_POINT('Ctrl Pts',(201.252576676787,12.1702089490887,29.3588668494477));
#73293=CARTESIAN_POINT('Ctrl Pts',(201.25574543485,12.1749143079762,29.4057552147945));
#73294=CARTESIAN_POINT('Ctrl Pts',(201.258914192912,12.1768012023009,29.4527348673623));
#73295=CARTESIAN_POINT('Ctrl Pts',(201.262086137348,12.1786899940089,29.4997617607366));
#73296=CARTESIAN_POINT('Ctrl Pts',(201.265258081784,12.1777546460219,29.5468795671834));
#73297=CARTESIAN_POINT('Ctrl Pts',(201.268430026219,12.1740146404998,29.593726657852));
#73298=CARTESIAN_POINT('Ctrl Pts',(201.271603915489,12.1702723418441,29.6406024721788));
#73299=CARTESIAN_POINT('Ctrl Pts',(201.27477780476,12.1637220412537,29.6872066889426));
#73300=CARTESIAN_POINT('Ctrl Pts',(201.27795169403,12.1544348181607,29.7331851477225));
#73301=CARTESIAN_POINT('Ctrl Pts',(201.281131198509,12.1451311642198,29.7792449510604));
#73302=CARTESIAN_POINT('Ctrl Pts',(201.284310702987,12.133081075288,29.8246762515713));
#73303=CARTESIAN_POINT('Ctrl Pts',(201.287490207466,12.1184056727622,29.8691392875775));
#73304=CARTESIAN_POINT('Ctrl Pts',(201.288222371704,12.1150262767015,29.8793780669544));
#73305=CARTESIAN_POINT('Ctrl Pts',(201.288954535942,12.1115078681575,29.8895655888197));
#73306=CARTESIAN_POINT('Ctrl Pts',(201.28968670018,12.1078522800235,29.8996978710812));
#73307=CARTESIAN_POINT('Ctrl Pts',(201.292963862627,12.0914898909157,29.9450499016802));
#73308=CARTESIAN_POINT('Ctrl Pts',(201.296241025075,12.0723011493438,29.9894978530556));
#73309=CARTESIAN_POINT('Ctrl Pts',(201.299518187522,12.0504097094453,30.0326673491055));
#73310=CARTESIAN_POINT('Ctrl Pts',(201.302692139854,12.0292077129543,30.0744772760912));
#73311=CARTESIAN_POINT('Ctrl Pts',(201.305866092185,12.0054710147095,30.1150875459341));
#73312=CARTESIAN_POINT('Ctrl Pts',(201.309040044517,11.9793616092817,30.1541757414986));
#73313=CARTESIAN_POINT('Ctrl Pts',(201.312210871885,11.9532779102652,30.1932254521868));
#73314=CARTESIAN_POINT('Ctrl Pts',(201.315381699254,11.9248264360125,30.2307555938241));
#73315=CARTESIAN_POINT('Ctrl Pts',(201.318552526623,11.8942142328695,30.2664698090816));
#73316=CARTESIAN_POINT('Ctrl Pts',(201.321721623568,11.8636187357993,30.3021645339328));
#73317=CARTESIAN_POINT('Ctrl Pts',(201.324890720513,11.8308652076759,30.3360448735801));
#73318=CARTESIAN_POINT('Ctrl Pts',(201.328059817458,11.7962013414586,30.3678470408774));
#73319=CARTESIAN_POINT('Ctrl Pts',(201.331228575521,11.7615411819674,30.3996458074597));
#73320=CARTESIAN_POINT('Ctrl Pts',(201.334397333584,11.7249715015898,30.429366468358));
#73321=CARTESIAN_POINT('Ctrl Pts',(201.337566091647,11.6867752802996,30.4567835580054));
#73322=CARTESIAN_POINT('Ctrl Pts',(201.340738036083,11.6485406504601,30.4842282171506));
#73323=CARTESIAN_POINT('Ctrl Pts',(201.343909980518,11.6086766705483,30.5093643597709));
#73324=CARTESIAN_POINT('Ctrl Pts',(201.347081924954,11.5674960638477,30.5320093410514));
#73325=CARTESIAN_POINT('Ctrl Pts',(201.350255814224,11.5262902078167,30.5546682067951));
#73326=CARTESIAN_POINT('Ctrl Pts',(201.353429703494,11.4837666218053,30.5748326331628));
#73327=CARTESIAN_POINT('Ctrl Pts',(201.356603592765,11.44026017321,30.5923671737951));
#73328=CARTESIAN_POINT('Ctrl Pts',(201.359783097243,11.3966767535084,30.6099327363342));
#73329=CARTESIAN_POINT('Ctrl Pts',(201.362962601722,11.352107531153,30.6248589591658));
#73330=CARTESIAN_POINT('Ctrl Pts',(201.366142106201,11.3069028744401,30.6370601075407));
#73331=CARTESIAN_POINT('Ctrl Pts',(201.366874270439,11.296493317459,30.639869741735));
#73332=CARTESIAN_POINT('Ctrl Pts',(201.367606434677,11.2860501029579,30.6425350881116));
#73333=CARTESIAN_POINT('Ctrl Pts',(201.368338598915,11.2755775646891,30.6450554870136));
#73334=CARTESIAN_POINT('Ctrl Pts',(201.371615761362,11.2287025503744,30.6563367763801));
#73335=CARTESIAN_POINT('Ctrl Pts',(201.374892923809,11.1810279166683,30.6647604030086));
#73336=CARTESIAN_POINT('Ctrl Pts',(201.378170086257,11.1329343325491,30.6702237075575));
#73337=CARTESIAN_POINT('Ctrl Pts',(201.381344038588,11.0863553954637,30.6755149521908));
#73338=CARTESIAN_POINT('Ctrl Pts',(201.38451799092,11.0393841082258,30.6780295168643));
#73339=CARTESIAN_POINT('Ctrl Pts',(201.387691943251,10.9923788365881,30.6777253416515));
#73340=CARTESIAN_POINT('Ctrl Pts',(201.39086277062,10.9454198447041,30.6774214659191));
#73341=CARTESIAN_POINT('Ctrl Pts',(201.394033597989,10.8984274890609,30.674304347124));
#73342=CARTESIAN_POINT('Ctrl Pts',(201.397204425357,10.8517631529411,30.6683838836932));
#73343=CARTESIAN_POINT('Ctrl Pts',(201.400373522303,10.805124283064,30.6624666512515));
#73344=CARTESIAN_POINT('Ctrl Pts',(201.403542619248,10.758813629581,30.6537491749466));
#73345=CARTESIAN_POINT('Ctrl Pts',(201.406711716193,10.7131877332229,30.6422932137268));
#73346=CARTESIAN_POINT('Ctrl Pts',(201.409880474256,10.6675667157985,30.6308384775321));
#73347=CARTESIAN_POINT('Ctrl Pts',(201.413049232319,10.6226308493316,30.6166459755668));
#73348=CARTESIAN_POINT('Ctrl Pts',(201.416217990381,10.5787240807764,30.5998280149106));
#73349=CARTESIAN_POINT('Ctrl Pts',(201.419389934817,10.5347731613804,30.582993142805));
#73350=CARTESIAN_POINT('Ctrl Pts',(201.422561879253,10.4918539246562,30.5635277458337));
#73351=CARTESIAN_POINT('Ctrl Pts',(201.425733823688,10.4502909170569,30.5415925242771));
#73352=CARTESIAN_POINT('Ctrl Pts',(201.428907712959,10.4087024256632,30.5196438534368));
#73353=CARTESIAN_POINT('Ctrl Pts',(201.432081602229,10.368472294167,30.4952226336101));
#73354=CARTESIAN_POINT('Ctrl Pts',(201.435255491499,10.3298978326106,30.4685340199291));
#73355=CARTESIAN_POINT('Ctrl Pts',(201.438434995978,10.2912551255625,30.4417981890611));
#73356=CARTESIAN_POINT('Ctrl Pts',(201.441614500456,10.2542743665554,30.4127873088151));
#73357=CARTESIAN_POINT('Ctrl Pts',(201.444794004935,10.2192198762922,30.3817468235967));
#73358=CARTESIAN_POINT('Ctrl Pts',(201.445526169173,10.2111476611634,30.3745989383328));
#73359=CARTESIAN_POINT('Ctrl Pts',(201.446258333411,10.203177431694,30.3673435787545));
#73360=CARTESIAN_POINT('Ctrl Pts',(201.446990497649,10.1953121225757,30.3599840012619));
#73361=CARTESIAN_POINT('Ctrl Pts',(201.450023747427,10.1627272926992,30.3294943438368));
#73362=CARTESIAN_POINT('Ctrl Pts',(201.453056997205,10.1317989100048,30.2970760208492));
#73363=CARTESIAN_POINT('Ctrl Pts',(201.456090246984,10.1027690874833,30.2629362700282));
#73364=CARTESIAN_POINT('Origin',(197.762132885264,11.,29.5));
#73365=CARTESIAN_POINT('',(202.054067314992,10.1027691090856,30.2629362954329));
#73366=CARTESIAN_POINT('',(201.956062524555,10.1027690874833,30.2629362700282));
#73367=CARTESIAN_POINT('',(197.762132885264,10.1027690874833,30.2629362700282));
#73368=CARTESIAN_POINT('Ctrl Pts',(202.054067314992,10.1027691090856,30.2629362954329));
#73369=CARTESIAN_POINT('Ctrl Pts',(202.047604320826,10.1692854702585,30.3411610887122));
#73370=CARTESIAN_POINT('Ctrl Pts',(202.041419150576,10.2457670530881,30.4103772800603));
#73371=CARTESIAN_POINT('Ctrl Pts',(202.033298780019,10.3497453620161,30.482254088737));
#73372=CARTESIAN_POINT('Ctrl Pts',(202.031762106183,10.3695956478954,30.4951102566408));
#73373=CARTESIAN_POINT('Ctrl Pts',(202.029449713983,10.3996093949205,30.5132902939744));
#73374=CARTESIAN_POINT('Ctrl Pts',(202.028690518296,10.4094860381672,30.5190776929628));
#73375=CARTESIAN_POINT('Ctrl Pts',(202.027320246648,10.4273411241685,30.5291934860977));
#73376=CARTESIAN_POINT('Ctrl Pts',(202.02671111811,10.435288304298,30.5335754025877));
#73377=CARTESIAN_POINT('Ctrl Pts',(202.025389899221,10.4525419389523,30.5428303203903));
#73378=CARTESIAN_POINT('Ctrl Pts',(202.024676766715,10.461864480563,30.54767149249));
#73379=CARTESIAN_POINT('Ctrl Pts',(202.022715639286,10.487519976455,30.5605615547266));
#73380=CARTESIAN_POINT('Ctrl Pts',(202.021459201629,10.5039762207167,30.5683571186333));
#73381=CARTESIAN_POINT('Ctrl Pts',(202.014715603041,10.5923578376161,30.6077426043634));
#73382=CARTESIAN_POINT('Ctrl Pts',(202.009007262484,10.6671176615132,30.6324536954834));
#73383=CARTESIAN_POINT('Ctrl Pts',(201.999861081094,10.7888761492997,30.6595937892407));
#73384=CARTESIAN_POINT('Ctrl Pts',(201.996467881437,10.8345403619749,30.6669852233019));
#73385=CARTESIAN_POINT('Ctrl Pts',(201.991379582015,10.9049315607282,30.6741631287229));
#73386=CARTESIAN_POINT('Ctrl Pts',(201.989636245669,10.9294144669434,30.675888997398));
#73387=CARTESIAN_POINT('Ctrl Pts',(201.987365444222,10.9619979569207,30.6771643956317));
#73388=CARTESIAN_POINT('Ctrl Pts',(201.986807326943,10.9700639933086,30.6773971352645));
#73389=CARTESIAN_POINT('Ctrl Pts',(201.985886008559,10.9834855486692,30.6776463837408));
#73390=CARTESIAN_POINT('Ctrl Pts',(201.985520417177,10.9888398392272,30.6777092966193));
#73391=CARTESIAN_POINT('Ctrl Pts',(201.984820686737,10.9991460013706,30.6777600987789));
#73392=CARTESIAN_POINT('Ctrl Pts',(201.984486243844,11.0040976324191,30.6777532811409));
#73393=CARTESIAN_POINT('Ctrl Pts',(201.983565302125,11.0177988477746,30.6776480053991));
#73394=CARTESIAN_POINT('Ctrl Pts',(201.982982270267,11.0265478079249,30.6774832689451));
#73395=CARTESIAN_POINT('Ctrl Pts',(201.98048608091,11.0642849665453,30.6763518657092));
#73396=CARTESIAN_POINT('Ctrl Pts',(201.97861839672,11.0932360963969,30.6744120200369));
#73397=CARTESIAN_POINT('Ctrl Pts',(201.969774122392,11.2319389661801,30.6599558608248));
#73398=CARTESIAN_POINT('Ctrl Pts',(201.963166627069,11.3396324421168,30.6331131497155));
#73399=CARTESIAN_POINT('Ctrl Pts',(201.954551758699,11.4639302367716,30.5827847649107));
#73400=CARTESIAN_POINT('Ctrl Pts',(201.953015188154,11.4855726402678,30.5732535598469));
#73401=CARTESIAN_POINT('Ctrl Pts',(201.950702920697,11.517244745616,30.5581512013742));
#73402=CARTESIAN_POINT('Ctrl Pts',(201.949943743762,11.5275043417661,30.5530741883359));
#73403=CARTESIAN_POINT('Ctrl Pts',(201.948573492258,11.5457621469612,30.5437054653588));
#73404=CARTESIAN_POINT('Ctrl Pts',(201.947964364868,11.5537879206016,30.5394692639389));
#73405=CARTESIAN_POINT('Ctrl Pts',(201.946643132863,11.5709964290611,30.5301303257523));
#73406=CARTESIAN_POINT('Ctrl Pts',(201.94592998591,11.5801613913265,30.5249966623229));
#73407=CARTESIAN_POINT('Ctrl Pts',(201.943968777309,11.6050220390879,30.510630967775));
#73408=CARTESIAN_POINT('Ctrl Pts',(201.942712271764,11.6205736714864,30.5011567687971));
#73409=CARTESIAN_POINT('Ctrl Pts',(201.935970328372,11.7019977138409,30.4489262937548));
#73410=CARTESIAN_POINT('Ctrl Pts',(201.930263870392,11.7636800311644,30.4000282929514));
#73411=CARTESIAN_POINT('Ctrl Pts',(201.921118295787,11.8532150927828,30.3131768532952));
#73412=CARTESIAN_POINT('Ctrl Pts',(201.917723832434,11.8844776970614,30.279058508426));
#73413=CARTESIAN_POINT('Ctrl Pts',(201.912633927381,11.9291404349111,30.2241514782553));
#73414=CARTESIAN_POINT('Ctrl Pts',(201.910890218898,11.9440287093345,30.2046327397892));
#73415=CARTESIAN_POINT('Ctrl Pts',(201.908619018214,11.9629882728012,30.1780956902999));
#73416=CARTESIAN_POINT('Ctrl Pts',(201.908060860826,11.9676118556828,30.1714815593181));
#73417=CARTESIAN_POINT('Ctrl Pts',(201.907139494889,11.9751897873637,30.1604003422456));
#73418=CARTESIAN_POINT('Ctrl Pts',(201.906773895561,11.978182253726,30.1559597672137));
#73419=CARTESIAN_POINT('Ctrl Pts',(201.906074165711,11.9838833958618,30.1473739581172));
#73420=CARTESIAN_POINT('Ctrl Pts',(201.905739731192,11.9865963660816,30.1432318329929));
#73421=CARTESIAN_POINT('Ctrl Pts',(201.904818842101,11.9940307266243,30.1317234572071));
#73422=CARTESIAN_POINT('Ctrl Pts',(201.904235853831,11.9986963911128,30.1243213446484));
#73423=CARTESIAN_POINT('Ctrl Pts',(201.901740218467,12.0184663492074,30.0921673007899));
#73424=CARTESIAN_POINT('Ctrl Pts',(201.899873019277,12.0327374057809,30.0669123042258));
#73425=CARTESIAN_POINT('Ctrl Pts',(201.891028793919,12.0968130081001,29.9430527695842));
#73426=CARTESIAN_POINT('Ctrl Pts',(201.884421002874,12.1335118575356,29.8383012340464));
#73427=CARTESIAN_POINT('Ctrl Pts',(201.87580565366,12.1596976317177,29.7067743291888));
#73428=CARTESIAN_POINT('Ctrl Pts',(201.87426893821,12.1636150592538,29.6834505248178));
#73429=CARTESIAN_POINT('Ctrl Pts',(201.871956495753,12.1683830486066,29.6486847435213));
#73430=CARTESIAN_POINT('Ctrl Pts',(201.871197292512,12.1697729550378,29.637321956628));
#73431=CARTESIAN_POINT('Ctrl Pts',(201.869827012748,12.1719674099389,29.6169179631392));
#73432=CARTESIAN_POINT('Ctrl Pts',(201.869217883747,12.172833497239,29.607884197267));
#73433=CARTESIAN_POINT('Ctrl Pts',(201.867896670141,12.1744766487479,29.5883742357462));
#73434=CARTESIAN_POINT('Ctrl Pts',(201.867183543455,12.1752181151935,29.5778959141664));
#73435=CARTESIAN_POINT('Ctrl Pts',(201.865222448723,12.1768614194645,29.5492318109622));
#73436=CARTESIAN_POINT('Ctrl Pts',(201.863966038411,12.1774818183726,29.5310334640761));
#73437=CARTESIAN_POINT('Ctrl Pts',(201.857221775629,12.1785359029456,29.4342694537427));
#73438=CARTESIAN_POINT('Ctrl Pts',(201.851512679495,12.1715287851462,29.355833786498));
#73439=CARTESIAN_POINT('Ctrl Pts',(201.842366254427,12.1480874499109,29.2333061289548));
#73440=CARTESIAN_POINT('Ctrl Pts',(201.838973561777,12.1367402973589,29.1884678560925));
#73441=CARTESIAN_POINT('Ctrl Pts',(201.833885906584,12.1153800501616,29.1210220266441));
#73442=CARTESIAN_POINT('Ctrl Pts',(201.832142719576,12.107243184764,29.0978685774277));
#73443=CARTESIAN_POINT('Ctrl Pts',(201.829872078345,12.0954765738816,29.0674595486759));
#73444=CARTESIAN_POINT('Ctrl Pts',(201.829313977165,12.0924874723601,29.0599644358746));
#73445=CARTESIAN_POINT('Ctrl Pts',(201.828392677866,12.0873870222569,29.0475475764285));
#73446=CARTESIAN_POINT('Ctrl Pts',(201.828027089674,12.0853187467281,29.0426085330259));
#73447=CARTESIAN_POINT('Ctrl Pts',(201.827327358996,12.0812730920725,29.0331294821189));
#73448=CARTESIAN_POINT('Ctrl Pts',(201.826992912741,12.0793006652321,29.0285875941636));
#73449=CARTESIAN_POINT('Ctrl Pts',(201.826071949894,12.0737635588939,29.0160542923954));
#73450=CARTESIAN_POINT('Ctrl Pts',(201.825488900538,12.0701382928782,29.0080897708088));
#73451=CARTESIAN_POINT('Ctrl Pts',(201.822992488739,12.0541141059541,28.9739012429677));
#73452=CARTESIAN_POINT('Ctrl Pts',(201.82112460981,12.0408365295538,28.9480977777271));
#73453=CARTESIAN_POINT('Ctrl Pts',(201.812280315777,11.9724924757837,28.8265379249276));
#73454=CARTESIAN_POINT('Ctrl Pts',(201.805672939163,11.9050954908719,28.7383588402031));
#73455=CARTESIAN_POINT('Ctrl Pts',(201.797058263843,11.8095516587997,28.6442662914965));
#73456=CARTESIAN_POINT('Ctrl Pts',(201.795521751499,11.7922111113383,28.6281883780274));
#73457=CARTESIAN_POINT('Ctrl Pts',(201.79320955433,11.765775079931,28.6051175412255));
#73458=CARTESIAN_POINT('Ctrl Pts',(201.792450387961,11.7570417936721,28.5977174524661));
#73459=CARTESIAN_POINT('Ctrl Pts',(201.791080147807,11.7411937833177,28.5846808235318));
#73460=CARTESIAN_POINT('Ctrl Pts',(201.790471021064,11.7341190562846,28.5789969475394));
#73461=CARTESIAN_POINT('Ctrl Pts',(201.789149781667,11.7187148100524,28.5669113470457));
#73462=CARTESIAN_POINT('Ctrl Pts',(201.788436626572,11.7103639616308,28.5605382167431));
#73463=CARTESIAN_POINT('Ctrl Pts',(201.786475372225,11.687307325046,28.5434252347977));
#73464=CARTESIAN_POINT('Ctrl Pts',(201.785218828421,11.6724364646892,28.5329137690585));
#73465=CARTESIAN_POINT('Ctrl Pts',(201.778477821833,11.5921799795312,28.4789306773197));
#73466=CARTESIAN_POINT('Ctrl Pts',(201.772772429132,11.5228228254777,28.4417409571442));
#73467=CARTESIAN_POINT('Ctrl Pts',(201.763627197657,11.407565687096,28.394050779051));
#73468=CARTESIAN_POINT('Ctrl Pts',(201.760232018943,11.3638301330806,28.3789016681159));
#73469=CARTESIAN_POINT('Ctrl Pts',(201.755141205018,11.2956911053484,28.3597087112878));
#73470=CARTESIAN_POINT('Ctrl Pts',(201.753397285927,11.271862574244,28.3537939171058));
#73471=CARTESIAN_POINT('Ctrl Pts',(201.751125859302,11.2399757802255,28.3469293998935));
#73472=CARTESIAN_POINT('Ctrl Pts',(201.750567679218,11.2320692096259,28.345312130974));
#73473=CARTESIAN_POINT('Ctrl Pts',(201.749646286374,11.2188896544508,28.3427571329853));
#73474=CARTESIAN_POINT('Ctrl Pts',(201.749280682549,11.2136258672373,28.3417738876973));
#73475=CARTESIAN_POINT('Ctrl Pts',(201.748580953032,11.2034821713149,28.3399506115992));
#73476=CARTESIAN_POINT('Ctrl Pts',(201.748246523249,11.1986034110434,28.3391054031765));
#73477=CARTESIAN_POINT('Ctrl Pts',(201.747325663929,11.1850896448277,28.3368519317845));
#73478=CARTESIAN_POINT('Ctrl Pts',(201.746742700316,11.1764438534976,28.3355090455809));
#73479=CARTESIAN_POINT('Ctrl Pts',(201.744247378285,11.1390879395483,28.3301324408666));
#73480=CARTESIAN_POINT('Ctrl Pts',(201.742380453405,11.1102470027975,28.3270628949147));
#73481=CARTESIAN_POINT('Ctrl Pts',(201.73353625568,10.9711290027812,28.31743427112));
#73482=CARTESIAN_POINT('Ctrl Pts',(201.72692829733,10.8604139469235,28.3253454561834));
#73483=CARTESIAN_POINT('Ctrl Pts',(201.718312676124,10.7292979740445,28.3535381843589));
#73484=CARTESIAN_POINT('Ctrl Pts',(201.716775878743,10.7063348884977,28.3592042405397));
#73485=CARTESIAN_POINT('Ctrl Pts',(201.714463337342,10.6725325493593,28.3686330501083));
#73486=CARTESIAN_POINT('Ctrl Pts',(201.713704119228,10.6615518002158,28.3718692861725));
#73487=CARTESIAN_POINT('Ctrl Pts',(201.712333823487,10.6419536574919,28.3779571144504));
#73488=CARTESIAN_POINT('Ctrl Pts',(201.711724693574,10.6333186558883,28.3807492664827));
#73489=CARTESIAN_POINT('Ctrl Pts',(201.710403490368,10.6147603270199,28.3869879628022));
#73490=CARTESIAN_POINT('Ctrl Pts',(201.709690375138,10.6048491818316,28.3904680179411));
#73491=CARTESIAN_POINT('Ctrl Pts',(201.70772934477,10.5778899510145,28.4003411207563));
#73492=CARTESIAN_POINT('Ctrl Pts',(201.706472988289,10.5609420727921,28.4069974302987));
#73493=CARTESIAN_POINT('Ctrl Pts',(201.699727422266,10.471697163321,28.4444591092895));
#73494=CARTESIAN_POINT('Ctrl Pts',(201.694016843361,10.4024756117815,28.4820455440432));
#73495=CARTESIAN_POINT('Ctrl Pts',(201.68486993985,10.2993270241127,28.5522201876927));
#73496=CARTESIAN_POINT('Ctrl Pts',(201.681478241867,10.26269194068,28.5804314140691));
#73497=CARTESIAN_POINT('Ctrl Pts',(201.676391850609,10.2092860804806,28.6268057140235));
#73498=CARTESIAN_POINT('Ctrl Pts',(201.674648956634,10.1912701038536,28.6434645896286));
#73499=CARTESIAN_POINT('Ctrl Pts',(201.67237862979,10.1680364659596,28.6663352971444));
#73500=CARTESIAN_POINT('Ctrl Pts',(201.671820560203,10.1623447491578,28.6720544411017));
#73501=CARTESIAN_POINT('Ctrl Pts',(201.67089929836,10.1529743245136,28.6816655720861));
#73502=CARTESIAN_POINT('Ctrl Pts',(201.670533716425,10.1492626445055,28.6855249008713));
#73503=CARTESIAN_POINT('Ctrl Pts',(201.669833985278,10.1421692905466,28.6930018246362));
#73504=CARTESIAN_POINT('Ctrl Pts',(201.669499532425,10.1387839261544,28.6966156228104));
#73505=CARTESIAN_POINT('Ctrl Pts',(201.668578528106,10.1294792159885,28.7066745925052));
#73506=CARTESIAN_POINT('Ctrl Pts',(201.667995444401,10.1236086164729,28.7131646985526));
#73507=CARTESIAN_POINT('Ctrl Pts',(201.665498595918,10.0985891738631,28.7414518277028));
#73508=CARTESIAN_POINT('Ctrl Pts',(201.663630334685,10.0801755231633,28.7638885730886));
#73509=CARTESIAN_POINT('Ctrl Pts',(201.654786001899,9.99574773947515,28.8748846540172));
#73510=CARTESIAN_POINT('Ctrl Pts',(201.648178858281,9.9415828047883,28.9717508545302));
#73511=CARTESIAN_POINT('Ctrl Pts',(201.639564561913,9.89316655028268,29.0967957128793));
#73512=CARTESIAN_POINT('Ctrl Pts',(201.638028163855,9.88529655822736,29.1190930553388));
#73513=CARTESIAN_POINT('Ctrl Pts',(201.635716104707,9.87462011352128,29.1525144725769));
#73514=CARTESIAN_POINT('Ctrl Pts',(201.634956959086,9.8712962453129,29.1634678325912));
#73515=CARTESIAN_POINT('Ctrl Pts',(201.633581134087,9.86560107529085,29.1832697842408));
#73516=CARTESIAN_POINT('Ctrl Pts',(201.632966342806,9.8631723337018,29.1921009920791));
#73517=CARTESIAN_POINT('Ctrl Pts',(201.631637182221,9.85817164950415,29.2111503965525));
#73518=CARTESIAN_POINT('Ctrl Pts',(201.630921805251,9.85563335531425,29.221376516513));
#73519=CARTESIAN_POINT('Ctrl Pts',(201.628948054172,9.84904982180014,29.2495090307131));
#73520=CARTESIAN_POINT('Ctrl Pts',(201.627681055577,9.84528564528884,29.2674774580354));
#73521=CARTESIAN_POINT('Ctrl Pts',(201.621361377559,9.82877745453049,29.3566136511067));
#73522=CARTESIAN_POINT('Ctrl Pts',(201.616125382876,9.82218736478418,29.4287520479956));
#73523=CARTESIAN_POINT('Ctrl Pts',(201.605715287031,9.82231138499072,29.570843521344));
#73524=CARTESIAN_POINT('Ctrl Pts',(201.600568081262,9.82858002547111,29.6405204828484));
#73525=CARTESIAN_POINT('Ctrl Pts',(201.594829067043,9.84306271396452,29.7207440406304));
#73526=CARTESIAN_POINT('Ctrl Pts',(201.594012838175,9.84531164554728,29.7322211117353));
#73527=CARTESIAN_POINT('Ctrl Pts',(201.592777789827,9.84901148175518,29.7497174095076));
#73528=CARTESIAN_POINT('Ctrl Pts',(201.592352843163,9.85033943740846,29.7557615077516));
#73529=CARTESIAN_POINT('Ctrl Pts',(201.591577011976,9.85286650159896,29.7668457133549));
#73530=CARTESIAN_POINT('Ctrl Pts',(201.59122540484,9.85405127028369,29.7718885954875));
#73531=CARTESIAN_POINT('Ctrl Pts',(201.59040772308,9.85689882168436,29.7836596291627));
#73532=CARTESIAN_POINT('Ctrl Pts',(201.589943095713,9.85858776797011,29.7903811486136));
#73533=CARTESIAN_POINT('Ctrl Pts',(201.588405920724,9.86440889735034,29.8127117079266));
#73534=CARTESIAN_POINT('Ctrl Pts',(201.58734671775,9.86880290442364,29.8282513621288));
#73535=CARTESIAN_POINT('Ctrl Pts',(201.584736262872,9.88055530235827,29.8667704947647));
#73536=CARTESIAN_POINT('Ctrl Pts',(201.583200983467,9.88830296911926,29.8896240191425));
#73537=CARTESIAN_POINT('Ctrl Pts',(201.574624847396,9.93597219059407,30.0172029435896));
#73538=CARTESIAN_POINT('Ctrl Pts',(201.567898488929,9.98997597966212,30.1160409303099));
#73539=CARTESIAN_POINT('Ctrl Pts',(201.559462506899,10.0679552947174,30.2202179066136));
#73540=CARTESIAN_POINT('Ctrl Pts',(201.558280744897,10.0791072321931,30.234423324952));
#73541=CARTESIAN_POINT('Ctrl Pts',(201.556667637363,10.0946044914041,30.2532556885621));
#73542=CARTESIAN_POINT('Ctrl Pts',(201.55624731731,10.0986673606599,30.2581125432704));
#73543=CARTESIAN_POINT('Ctrl Pts',(201.555825452273,10.1027690875306,30.2629362700837));
#73544=CARTESIAN_POINT('',(201.512132885209,9.82225036610555,29.4990713657972));
#73545=CARTESIAN_POINT('Ctrl Pts',(201.456090246984,10.1027690874833,30.2629362700282));
#73546=CARTESIAN_POINT('Ctrl Pts',(201.459217919371,10.0728355900905,30.2277337764049));
#73547=CARTESIAN_POINT('Ctrl Pts',(201.462345591759,10.0449212876478,30.1907011699184));
#73548=CARTESIAN_POINT('Ctrl Pts',(201.465473264147,10.0192575340884,30.1521037325899));
#73549=CARTESIAN_POINT('Ctrl Pts',(201.468597790043,9.99361959870365,30.1135451249428));
#73550=CARTESIAN_POINT('Ctrl Pts',(201.471722315939,9.97022805109866,30.0734252765857));
#73551=CARTESIAN_POINT('Ctrl Pts',(201.474846841836,9.94927302065566,30.032041236539));
#73552=CARTESIAN_POINT('Ctrl Pts',(201.47797127168,9.92831863439262,29.9906584686817));
#73553=CARTESIAN_POINT('Ctrl Pts',(201.481095701525,9.90980090327951,29.9480120850801));
#73554=CARTESIAN_POINT('Ctrl Pts',(201.48422013137,9.89386448097275,29.9044246234421));
#73555=CARTESIAN_POINT('Ctrl Pts',(201.487344187057,9.87792996708856,29.8608423815012));
#73556=CARTESIAN_POINT('Ctrl Pts',(201.490468242744,9.86457633736907,29.8163198290956));
#73557=CARTESIAN_POINT('Ctrl Pts',(201.493592298432,9.85389912864669,29.7711970781243));
#73558=CARTESIAN_POINT('Ctrl Pts',(201.496720654507,9.84320722231794,29.7260122138752));
#73559=CARTESIAN_POINT('Ctrl Pts',(201.499849010582,9.83519921713805,29.6802260650162));
#73560=CARTESIAN_POINT('Ctrl Pts',(201.502977366658,9.82991956341843,29.6341895466461));
#73561=CARTESIAN_POINT('Ctrl Pts',(201.506029206175,9.82476904491298,29.5892790369074));
#73562=CARTESIAN_POINT('Ctrl Pts',(201.509081045692,9.82221483756981,29.5441307872882));
#73563=CARTESIAN_POINT('Ctrl Pts',(201.512132885209,9.82225036610555,29.4990713657972));
#73564=CARTESIAN_POINT('Ctrl Pts',(201.512132885264,9.82225036610619,29.4990713649792));
#73565=CARTESIAN_POINT('Ctrl Pts',(201.516636055637,9.82230279061592,29.4325835137179));
#73566=CARTESIAN_POINT('Ctrl Pts',(201.52113922601,9.82798776705774,29.3663156636972));
#73567=CARTESIAN_POINT('Ctrl Pts',(201.525642396383,9.83918085218961,29.3010176676768));
#73568=CARTESIAN_POINT('Ctrl Pts',(201.52891955883,9.84732657070003,29.2534973380618));
#73569=CARTESIAN_POINT('Ctrl Pts',(201.532196721278,9.8584134694595,29.2063708183464));
#73570=CARTESIAN_POINT('Ctrl Pts',(201.535473883725,9.87238554473478,29.1600283794536));
#73571=CARTESIAN_POINT('Ctrl Pts',(201.538647836056,9.88591758704595,29.1151454374751));
#73572=CARTESIAN_POINT('Ctrl Pts',(201.541821788388,9.90215558414496,29.0709984974849));
#73573=CARTESIAN_POINT('Ctrl Pts',(201.544995740719,9.92099666492068,29.0279334100069));
#73574=CARTESIAN_POINT('Ctrl Pts',(201.548166568088,9.93981919542436,28.9849107229144));
#73575=CARTESIAN_POINT('Ctrl Pts',(201.551337395457,9.96123951442141,28.9429682879285));
#73576=CARTESIAN_POINT('Ctrl Pts',(201.554508222825,9.98510582347525,28.9024342103532));
#73577=CARTESIAN_POINT('Ctrl Pts',(201.557677319771,10.0089591079097,28.8619222535396));
#73578=CARTESIAN_POINT('Ctrl Pts',(201.560846416716,10.0352554558839,28.8228176105625));
#73579=CARTESIAN_POINT('Ctrl Pts',(201.564015513661,10.0637973353376,28.7854234588381));
#73580=CARTESIAN_POINT('Ctrl Pts',(201.567184271724,10.0923361627101,28.7480333057985));
#73581=CARTESIAN_POINT('Ctrl Pts',(201.570353029787,10.1231197053437,28.7123537218591));
#73582=CARTESIAN_POINT('Ctrl Pts',(201.573521787849,10.1559089641209,28.6786563534984));
#73583=CARTESIAN_POINT('Ctrl Pts',(201.576693732285,10.1887311944281,28.6449251004499));
#73584=CARTESIAN_POINT('Ctrl Pts',(201.579865676721,10.2235627746507,28.6131804382304));
#73585=CARTESIAN_POINT('Ctrl Pts',(201.583037621156,10.2601279062822,28.5836570797798));
#73586=CARTESIAN_POINT('Ctrl Pts',(201.586211510427,10.2967154573282,28.5541156194825));
#73587=CARTESIAN_POINT('Ctrl Pts',(201.589385399697,10.335038221367,28.5267984963833));
#73588=CARTESIAN_POINT('Ctrl Pts',(201.592559288967,10.3747903130615,28.5018978459805));
#73589=CARTESIAN_POINT('Ctrl Pts',(201.595738793446,10.4146127336974,28.4769531416348));
#73590=CARTESIAN_POINT('Ctrl Pts',(201.598918297924,10.4558690362348,28.4544337009151));
#73591=CARTESIAN_POINT('Ctrl Pts',(201.602097802403,10.49822934729,28.4344854414045));
#73592=CARTESIAN_POINT('Ctrl Pts',(201.602829966641,10.5079839191355,28.4298918318265));
#73593=CARTESIAN_POINT('Ctrl Pts',(201.603562130879,10.5177969584718,28.4254343595157));
#73594=CARTESIAN_POINT('Ctrl Pts',(201.604294295117,10.5276643146806,28.4211144347643));
#73595=CARTESIAN_POINT('Ctrl Pts',(201.607571457564,10.5718305379666,28.4017784792043));
#73596=CARTESIAN_POINT('Ctrl Pts',(201.610848620012,10.617285683156,28.3851154074467));
#73597=CARTESIAN_POINT('Ctrl Pts',(201.614125782459,10.6636730183221,28.3712931186993));
#73598=CARTESIAN_POINT('Ctrl Pts',(201.61729973479,10.7085994426223,28.3579061455775));
#73599=CARTESIAN_POINT('Ctrl Pts',(201.620473687122,10.7543996275644,28.3471838361457));
#73600=CARTESIAN_POINT('Ctrl Pts',(201.623647639453,10.8007281584948,28.3392305156996));
#73601=CARTESIAN_POINT('Ctrl Pts',(201.626818466822,10.8470110759668,28.3312850258158));
#73602=CARTESIAN_POINT('Ctrl Pts',(201.629989294191,10.8938207633434,28.3261032224443));
#73603=CARTESIAN_POINT('Ctrl Pts',(201.633160121559,10.940799712924,28.3237388094007));
#73604=CARTESIAN_POINT('Ctrl Pts',(201.636329218505,10.9877530245671,28.3213756866941));
#73605=CARTESIAN_POINT('Ctrl Pts',(201.63949831545,11.0348748601952,28.3218269362728));
#73606=CARTESIAN_POINT('Ctrl Pts',(201.642667412395,11.0818033742262,28.3250943567821));
#73607=CARTESIAN_POINT('Ctrl Pts',(201.645836170458,11.1287268700302,28.328361427895));
#73608=CARTESIAN_POINT('Ctrl Pts',(201.649004928521,11.175456530261,28.3344440311103));
#73609=CARTESIAN_POINT('Ctrl Pts',(201.652173686583,11.2216340326959,28.3432919910146));
#73610=CARTESIAN_POINT('Ctrl Pts',(201.655345631019,11.2678579693282,28.3521488480635));
#73611=CARTESIAN_POINT('Ctrl Pts',(201.658517575455,11.3135280930283,28.3637765030913));
#73612=CARTESIAN_POINT('Ctrl Pts',(201.66168951989,11.3582966842705,28.3780737330195));
#73613=CARTESIAN_POINT('Ctrl Pts',(201.664863409161,11.4030927247672,28.3923797291003));
#73614=CARTESIAN_POINT('Ctrl Pts',(201.668037298431,11.4469856134574,28.409358356266));
#73615=CARTESIAN_POINT('Ctrl Pts',(201.671211187701,11.4896466391654,28.4288598451864));
#73616=CARTESIAN_POINT('Ctrl Pts',(201.67439069218,11.5323831402671,28.4483958359157));
#73617=CARTESIAN_POINT('Ctrl Pts',(201.677570196658,11.5738829418941,28.4704633272616));
#73618=CARTESIAN_POINT('Ctrl Pts',(201.680749701137,11.6138427361426,28.4948670944671));
#73619=CARTESIAN_POINT('Ctrl Pts',(201.681481865375,11.6230445260779,28.5004867014665));
#73620=CARTESIAN_POINT('Ctrl Pts',(201.682214029613,11.6321647839154,28.5062300190961));
#73621=CARTESIAN_POINT('Ctrl Pts',(201.682946193851,11.6412000488187,28.5120943567856));
#73622=CARTESIAN_POINT('Ctrl Pts',(201.686223356298,11.6816418367429,28.5383430947793));
#73623=CARTESIAN_POINT('Ctrl Pts',(201.689500518745,11.7205603945304,28.5671384771231));
#73624=CARTESIAN_POINT('Ctrl Pts',(201.692777681193,11.7576192831497,28.5982749397406));
#73625=CARTESIAN_POINT('Ctrl Pts',(201.695951633524,11.7935110486119,28.6284307985705));
#73626=CARTESIAN_POINT('Ctrl Pts',(201.699125585856,11.8276580881997,28.6607820666704));
#73627=CARTESIAN_POINT('Ctrl Pts',(201.702299538187,11.8597832804536,28.6950976623513));
#73628=CARTESIAN_POINT('Ctrl Pts',(201.705470365556,11.891876843362,28.7293794720915));
#73629=CARTESIAN_POINT('Ctrl Pts',(201.708641192925,11.9219521202615,28.7656213765379));
#73630=CARTESIAN_POINT('Ctrl Pts',(201.711812020293,11.9497676133906,28.8035543502509));
#73631=CARTESIAN_POINT('Ctrl Pts',(201.714981117239,11.9775679267023,28.8414666227091));
#73632=CARTESIAN_POINT('Ctrl Pts',(201.718150214184,12.003110570642,28.8810676878428));
#73633=CARTESIAN_POINT('Ctrl Pts',(201.721319311129,12.0261950089443,28.9220563469353));
#73634=CARTESIAN_POINT('Ctrl Pts',(201.724488069192,12.0492769787485,28.9630406229699));
#73635=CARTESIAN_POINT('Ctrl Pts',(201.727656827255,12.0699009937059,29.0054117123376));
#73636=CARTESIAN_POINT('Ctrl Pts',(201.730825585317,12.0879118606755,29.0488427703099));
#73637=CARTESIAN_POINT('Ctrl Pts',(201.733997529753,12.1059408386322,29.092317500768));
#73638=CARTESIAN_POINT('Ctrl Pts',(201.737169474189,12.121351214005,29.1368538105736));
#73639=CARTESIAN_POINT('Ctrl Pts',(201.740341418624,12.1340362571272,29.1821056307184));
#73640=CARTESIAN_POINT('Ctrl Pts',(201.743515307895,12.1467290779115,29.227385196403));
#73641=CARTESIAN_POINT('Ctrl Pts',(201.746689197165,12.1566931234071,29.273380601123));
#73642=CARTESIAN_POINT('Ctrl Pts',(201.749863086435,12.1638726619692,29.319734947312));
#73643=CARTESIAN_POINT('Ctrl Pts',(201.753042590914,12.1710649024881,29.3661713030746));
#73644=CARTESIAN_POINT('Ctrl Pts',(201.756222095392,12.1754627611754,29.4129673130365));
#73645=CARTESIAN_POINT('Ctrl Pts',(201.759401599871,12.177062440713,29.4597622917797));
#73646=CARTESIAN_POINT('Ctrl Pts',(201.760133764109,12.1774308088526,29.4705380620888));
#73647=CARTESIAN_POINT('Ctrl Pts',(201.760865928347,12.1776510155898,29.4813137898791));
#73648=CARTESIAN_POINT('Ctrl Pts',(201.761598092585,12.1777234042577,29.4920851049469));
#73649=CARTESIAN_POINT('Ctrl Pts',(201.764875255032,12.1780474154721,29.5402974423047));
#73650=CARTESIAN_POINT('Ctrl Pts',(201.76815241748,12.1754067908878,29.58863847339));
#73651=CARTESIAN_POINT('Ctrl Pts',(201.771429579927,12.1697881439925,29.6367141568183));
#73652=CARTESIAN_POINT('Ctrl Pts',(201.774603532259,12.1643464493251,29.6832757569724));
#73653=CARTESIAN_POINT('Ctrl Pts',(201.77777748459,12.1561116114345,29.729587875313));
#73654=CARTESIAN_POINT('Ctrl Pts',(201.780951436922,12.1451241821247,29.7752919723006));
#73655=CARTESIAN_POINT('Ctrl Pts',(201.78412226429,12.1341475706553,29.8209510706257));
#73656=CARTESIAN_POINT('Ctrl Pts',(201.787293091659,12.1204238616838,29.8660027934623));
#73657=CARTESIAN_POINT('Ctrl Pts',(201.790463919028,12.1040448898881,29.9100974806213));
#73658=CARTESIAN_POINT('Ctrl Pts',(201.793633015973,12.0876748566289,29.9541681038784));
#73659=CARTESIAN_POINT('Ctrl Pts',(201.796802112918,12.0686526248256,29.9972822050097));
#73660=CARTESIAN_POINT('Ctrl Pts',(201.799971209864,12.0471194290063,30.0391066349968));
#73661=CARTESIAN_POINT('Ctrl Pts',(201.803139967926,12.0255885358054,30.0809265925542));
#73662=CARTESIAN_POINT('Ctrl Pts',(201.806308725989,12.0015474684606,30.1214566590244));
#73663=CARTESIAN_POINT('Ctrl Pts',(201.809477484052,11.9751838203621,30.1603874461284));
#73664=CARTESIAN_POINT('Ctrl Pts',(201.812649428488,11.9487936620634,30.1993573804307));
#73665=CARTESIAN_POINT('Ctrl Pts',(201.815821372923,11.9200765775157,30.236724366064));
#73666=CARTESIAN_POINT('Ctrl Pts',(201.818993317359,11.8892628723486,30.2722089136771));
#73667=CARTESIAN_POINT('Ctrl Pts',(201.822167206629,11.8584302741761,30.3077152181592));
#73668=CARTESIAN_POINT('Ctrl Pts',(201.8253410959,11.8254988870274,30.3413363900374));
#73669=CARTESIAN_POINT('Ctrl Pts',(201.82851498517,11.7907361113877,30.3728295736554));
#73670=CARTESIAN_POINT('Ctrl Pts',(201.831694489648,11.7559118338471,30.4043784746499));
#73671=CARTESIAN_POINT('Ctrl Pts',(201.834873994127,11.719250140878,30.4337915326009));
#73672=CARTESIAN_POINT('Ctrl Pts',(201.838053498606,11.6810501629335,30.4608671802431));
#73673=CARTESIAN_POINT('Ctrl Pts',(201.838785662844,11.6722536168253,30.4671020577406));
#73674=CARTESIAN_POINT('Ctrl Pts',(201.839517827082,11.6633756096369,30.4732131778327));
#73675=CARTESIAN_POINT('Ctrl Pts',(201.84024999132,11.6544199799073,30.4791984234046));
#73676=CARTESIAN_POINT('Ctrl Pts',(201.843527153767,11.6143346385116,30.505988344307));
#73677=CARTESIAN_POINT('Ctrl Pts',(201.846804316214,11.5725111150186,30.5303731975406));
#73678=CARTESIAN_POINT('Ctrl Pts',(201.850081478662,11.5292711218841,30.5521250600758));
#73679=CARTESIAN_POINT('Ctrl Pts',(201.853255430993,11.4873929180307,30.5731918750174));
#73680=CARTESIAN_POINT('Ctrl Pts',(201.856429383325,11.4441866877486,30.5917888243663));
#73681=CARTESIAN_POINT('Ctrl Pts',(201.859603335656,11.3999741637609,30.6077525584822));
#73682=CARTESIAN_POINT('Ctrl Pts',(201.862774163025,11.3558051698847,30.6237005752613));
#73683=CARTESIAN_POINT('Ctrl Pts',(201.865944990394,11.3106323648664,30.6370203202011));
#73684=CARTESIAN_POINT('Ctrl Pts',(201.869115817762,11.2647982743046,30.6475961556337));
#73685=CARTESIAN_POINT('Ctrl Pts',(201.872284914708,11.2189891968934,30.6581662194897));
#73686=CARTESIAN_POINT('Ctrl Pts',(201.875454011653,11.1725200905719,30.6659952153911));
#73687=CARTESIAN_POINT('Ctrl Pts',(201.878623108598,11.1257468644904,30.6710178429771));
#73688=CARTESIAN_POINT('Ctrl Pts',(201.881791866661,11.0789786400304,30.6760399334764));
#73689=CARTESIAN_POINT('Ctrl Pts',(201.884960624724,11.0319069139624,30.6782561943257));
#73690=CARTESIAN_POINT('Ctrl Pts',(201.888129382786,10.9848932519535,30.6776531104971));
#73691=CARTESIAN_POINT('Ctrl Pts',(201.891301327222,10.9378323149396,30.6770494202321));
#73692=CARTESIAN_POINT('Ctrl Pts',(201.894473271658,10.8908301160774,30.6736207379259));
#73693=CARTESIAN_POINT('Ctrl Pts',(201.897645216093,10.8442467455301,30.6674056648064));
#73694=CARTESIAN_POINT('Ctrl Pts',(201.900819105364,10.797634813021,30.6611867809991));
#73695=CARTESIAN_POINT('Ctrl Pts',(201.903992994634,10.7514427664435,30.6521782133556));
#73696=CARTESIAN_POINT('Ctrl Pts',(201.907166883904,10.7060205061947,30.6404696925925));
#73697=CARTESIAN_POINT('Ctrl Pts',(201.910346388383,10.6605178854079,30.6287404572497));
#73698=CARTESIAN_POINT('Ctrl Pts',(201.913525892861,10.6157882955807,30.6143019149662));
#73699=CARTESIAN_POINT('Ctrl Pts',(201.91670539734,10.5721646090964,30.597293005897));
#73700=CARTESIAN_POINT('Ctrl Pts',(201.917437561578,10.5621191119466,30.5933762587959));
#73701=CARTESIAN_POINT('Ctrl Pts',(201.918169725816,10.5521321604145,30.5893234080077));
#73702=CARTESIAN_POINT('Ctrl Pts',(201.918901890054,10.542207633965,30.5851364946863));
#73703=CARTESIAN_POINT('Ctrl Pts',(201.922080584737,10.4991202529918,30.5669589896641));
#73704=CARTESIAN_POINT('Ctrl Pts',(201.925259279421,10.4570229406646,30.5461714465251));
#73705=CARTESIAN_POINT('Ctrl Pts',(201.928437974104,10.4162511379083,30.5229038706089));
#73706=CARTESIAN_POINT('Ctrl Pts',(201.931612116937,10.3755377198582,30.4996696135672));
#73707=CARTESIAN_POINT('Ctrl Pts',(201.93478625977,10.3361465356879,30.4739626231147));
#73708=CARTESIAN_POINT('Ctrl Pts',(201.937960402603,10.2983917674929,30.4459603324549));
#73709=CARTESIAN_POINT('Ctrl Pts',(201.941131583528,10.2606722296368,30.4179841717448));
#73710=CARTESIAN_POINT('Ctrl Pts',(201.944302764454,10.2245865330093,30.387717277307));
#73711=CARTESIAN_POINT('Ctrl Pts',(201.947473945379,10.1904207089845,30.3553808707581));
#73712=CARTESIAN_POINT('Ctrl Pts',(201.950336805105,10.1595766909726,30.3261884032997));
#73713=CARTESIAN_POINT('Ctrl Pts',(201.95319966483,10.1302972464099,30.2953100293104));
#73714=CARTESIAN_POINT('Ctrl Pts',(201.956062524555,10.1027690874833,30.2629362700282));
#73715=CARTESIAN_POINT('Origin',(197.762132885264,11.,29.5));
#73716=CARTESIAN_POINT('',(202.554740968482,10.1027692175106,30.2629364229433));
#73717=CARTESIAN_POINT('',(202.455993057958,10.1022055060817,30.2634229920695));
#73718=CARTESIAN_POINT('',(197.762132885264,10.1027690874833,30.2629362700282));
#73719=CARTESIAN_POINT('',(202.111797459566,9.8222500756293,29.4995779279502));
#73720=CARTESIAN_POINT('Ctrl Pts',(202.554740968482,10.1027692175106,30.2629364229433));
#73721=CARTESIAN_POINT('Ctrl Pts',(202.551960232187,10.1273404241732,30.2918327271669));
#73722=CARTESIAN_POINT('Ctrl Pts',(202.549173805468,10.153306367189,30.3195406316827));
#73723=CARTESIAN_POINT('Ctrl Pts',(202.544099121304,10.2035899648221,30.3682466365461));
#73724=CARTESIAN_POINT('Ctrl Pts',(202.541804407233,10.2275005328419,30.38958760777));
#73725=CARTESIAN_POINT('Ctrl Pts',(202.53893503173,10.2592317714701,30.4156631874325));
#73726=CARTESIAN_POINT('Ctrl Pts',(202.53830860141,10.2662759625235,30.42131736682));
#73727=CARTESIAN_POINT('Ctrl Pts',(202.537305432702,10.2777569378722,30.4303176259428));
#73728=CARTESIAN_POINT('Ctrl Pts',(202.536925418902,10.2821534200698,30.433714205095));
#73729=CARTESIAN_POINT('Ctrl Pts',(202.536178482652,10.2908921212018,30.4403672336965));
#73730=CARTESIAN_POINT('Ctrl Pts',(202.535811484359,10.2952331101845,30.4436250056164));
#73731=CARTESIAN_POINT('Ctrl Pts',(202.53487939963,10.3063745309721,30.4518665087001));
#73732=CARTESIAN_POINT('Ctrl Pts',(202.534317098837,10.3132063951316,30.4568075543328));
#73733=CARTESIAN_POINT('Ctrl Pts',(202.531901256486,10.3430070821966,30.4778767893962));
#73734=CARTESIAN_POINT('Ctrl Pts',(202.530090716421,10.3664970192476,30.4932557345955));
#73735=CARTESIAN_POINT('Ctrl Pts',(202.524534891989,10.4413265274764,30.538510954867));
#73736=CARTESIAN_POINT('Ctrl Pts',(202.520889207193,10.4943911262989,30.5653551229465));
#73737=CARTESIAN_POINT('Ctrl Pts',(202.5131142898,10.6102180391572,30.6133369245908));
#73738=CARTESIAN_POINT('Ctrl Pts',(202.50898715164,10.6731865122077,30.6334198461389));
#73739=CARTESIAN_POINT('Ctrl Pts',(202.50365987023,10.7528961863222,30.65164411892));
#73740=CARTESIAN_POINT('Ctrl Pts',(202.502622187586,10.7683602303358,30.6548538653976));
#73741=CARTESIAN_POINT('Ctrl Pts',(202.500917937525,10.7936207382878,30.6595692213524));
#73742=CARTESIAN_POINT('Ctrl Pts',(202.500257289207,10.8033801954236,30.6612638895795));
#73743=CARTESIAN_POINT('Ctrl Pts',(202.498968081178,10.8223535997132,30.6643124711324));
#73744=CARTESIAN_POINT('Ctrl Pts',(202.498340015447,10.8315645386323,30.6656805998332));
#73745=CARTESIAN_POINT('Ctrl Pts',(202.49684793314,10.8533640313455,30.6686547785236));
#73746=CARTESIAN_POINT('Ctrl Pts',(202.49598108415,10.8659640130026,30.6701668390432));
#73747=CARTESIAN_POINT('Ctrl Pts',(202.492943980129,10.9098685401097,30.674717208421));
#73748=CARTESIAN_POINT('Ctrl Pts',(202.490742375719,10.9412661100783,30.6767048129087));
#73749=CARTESIAN_POINT('Ctrl Pts',(202.48495580168,11.0226725331412,30.6785920801637));
#73750=CARTESIAN_POINT('Ctrl Pts',(202.481324238941,11.0726604337243,30.6765682955158));
#73751=CARTESIAN_POINT('Ctrl Pts',(202.472322134592,11.1949393537006,30.6637947971776));
#73752=CARTESIAN_POINT('Ctrl Pts',(202.466933679217,11.2666576728945,30.6494846240999));
#73753=CARTESIAN_POINT('Ctrl Pts',(202.460988769861,11.3476182720866,30.6253394768748));
#73754=CARTESIAN_POINT('Ctrl Pts',(202.460186126835,11.3585940687382,30.6218902439131));
#73755=CARTESIAN_POINT('Ctrl Pts',(202.458967291192,11.3753552867929,30.6163517657282));
#73756=CARTESIAN_POINT('Ctrl Pts',(202.458545202683,11.3811774940067,30.614377215505));
#73757=CARTESIAN_POINT('Ctrl Pts',(202.457775241298,11.391835545058,30.6106693265542));
#73758=CARTESIAN_POINT('Ctrl Pts',(202.457426647153,11.3966757122099,30.6089498762958));
#73759=CARTESIAN_POINT('Ctrl Pts',(202.456610106818,11.4080459226621,30.6048266836054));
#73760=CARTESIAN_POINT('Ctrl Pts',(202.456143665445,11.4145661335786,30.6023966629925));
#73761=CARTESIAN_POINT('Ctrl Pts',(202.454593513435,11.4363025805553,30.5940755660237));
#73762=CARTESIAN_POINT('Ctrl Pts',(202.453523456901,11.451418580527,30.5879258311098));
#73763=CARTESIAN_POINT('Ctrl Pts',(202.450879379118,11.4888880727225,30.5717663645126));
#73764=CARTESIAN_POINT('Ctrl Pts',(202.449321865635,11.5110668531565,30.5613696350463));
#73765=CARTESIAN_POINT('Ctrl Pts',(202.442124088541,11.6130560481044,30.5096212632605));
#73766=CARTESIAN_POINT('Ctrl Pts',(202.436687165938,11.6882865249071,30.4599141788348));
#73767=CARTESIAN_POINT('Ctrl Pts',(202.42895147597,11.781624207456,30.3815786737201));
#73768=CARTESIAN_POINT('Ctrl Pts',(202.426893926822,11.8052661872954,30.3600368931716));
#73769=CARTESIAN_POINT('Ctrl Pts',(202.423938905603,11.8373133630245,30.328355515304));
#73770=CARTESIAN_POINT('Ctrl Pts',(202.423074020923,11.8464710510474,30.318995277839));
#73771=CARTESIAN_POINT('Ctrl Pts',(202.421584374208,11.8618529485024,30.302739552475));
#73772=CARTESIAN_POINT('Ctrl Pts',(202.420962979096,11.8681552567601,30.2959194279658));
#73773=CARTESIAN_POINT('Ctrl Pts',(202.419682016383,11.8809095878748,30.2817854357582));
#73774=CARTESIAN_POINT('Ctrl Pts',(202.419022150206,11.8873527111679,30.2744645413184));
#73775=CARTESIAN_POINT('Ctrl Pts',(202.417334792171,11.9035022669995,30.2556487574543));
#73776=CARTESIAN_POINT('Ctrl Pts',(202.416302283388,11.9130804741851,30.2440466401949));
#73777=CARTESIAN_POINT('Ctrl Pts',(202.411377175681,11.9573232165224,30.1883140802555));
#73778=CARTESIAN_POINT('Ctrl Pts',(202.407373961684,11.9890223013109,30.1419324680314));
#73779=CARTESIAN_POINT('Ctrl Pts',(202.398253272719,12.0522852548754,30.0334916020876));
#73780=CARTESIAN_POINT('Ctrl Pts',(202.393111617308,12.0819038483196,29.9705330789618));
#73781=CARTESIAN_POINT('Ctrl Pts',(202.386012449755,12.1157085920347,29.8783091286168));
#73782=CARTESIAN_POINT('Ctrl Pts',(202.383957111363,12.1246210724822,29.8509290349413));
#73783=CARTESIAN_POINT('Ctrl Pts',(202.381338506928,12.1349182299877,29.8148521876278));
#73784=CARTESIAN_POINT('Ctrl Pts',(202.38073346103,12.1372211548994,29.80642999999));
#73785=CARTESIAN_POINT('Ctrl Pts',(202.379793334744,12.1406821241273,29.7931958978888));
#73786=CARTESIAN_POINT('Ctrl Pts',(202.379454893384,12.1419038102303,29.7884011672507));
#73787=CARTESIAN_POINT('Ctrl Pts',(202.37875356737,12.1443853892996,29.7783987215763));
#73788=CARTESIAN_POINT('Ctrl Pts',(202.378391016823,12.1456400219038,29.7731898774099));
#73789=CARTESIAN_POINT('Ctrl Pts',(202.377486181234,12.1486986892493,29.7600995061544));
#73790=CARTESIAN_POINT('Ctrl Pts',(202.376946358788,12.150457234793,29.7522074377083));
#73791=CARTESIAN_POINT('Ctrl Pts',(202.374774466698,12.1572542137225,29.7201521377375));
#73792=CARTESIAN_POINT('Ctrl Pts',(202.37317534365,12.1616141169352,29.6958497265245));
#73793=CARTESIAN_POINT('Ctrl Pts',(202.368618143973,12.1720047861223,29.6252230135169));
#73794=CARTESIAN_POINT('Ctrl Pts',(202.36572306985,12.1760485810298,29.5786531489674));
#73795=CARTESIAN_POINT('Ctrl Pts',(202.358010189211,12.1794285207688,29.4541597543406));
#73796=CARTESIAN_POINT('Ctrl Pts',(202.353204361497,12.1738233144532,29.3763464469293));
#73797=CARTESIAN_POINT('Ctrl Pts',(202.346979318126,12.1574835634851,29.2816897795632));
#73798=CARTESIAN_POINT('Ctrl Pts',(202.345786354447,12.1539650812882,29.2637965155006));
#73799=CARTESIAN_POINT('Ctrl Pts',(202.343885584894,12.1477660694697,29.2357301101122));
#73800=CARTESIAN_POINT('Ctrl Pts',(202.343186407096,12.1453621271405,29.225498432039));
#73801=CARTESIAN_POINT('Ctrl Pts',(202.341875473737,12.1406280520877,29.2064952212172));
#73802=CARTESIAN_POINT('Ctrl Pts',(202.341264863963,12.1383328279824,29.1977157409286));
#73803=CARTESIAN_POINT('Ctrl Pts',(202.339877172715,12.1329154633657,29.1779309598615));
#73804=CARTESIAN_POINT('Ctrl Pts',(202.339098253862,12.1297340102291,29.1669430018586));
#73805=CARTESIAN_POINT('Ctrl Pts',(202.336696535335,12.1194997990496,29.1334317791305));
#73806=CARTESIAN_POINT('Ctrl Pts',(202.335057518132,12.1119300388235,29.1110738972545));
#73807=CARTESIAN_POINT('Ctrl Pts',(202.325639836195,12.0651794541282,28.9855427454284));
#73808=CARTESIAN_POINT('Ctrl Pts',(202.317416187995,12.0123216839667,28.888059953376));
#73809=CARTESIAN_POINT('Ctrl Pts',(202.307332262731,11.9293526571941,28.7759499391536));
#73810=CARTESIAN_POINT('Ctrl Pts',(202.305249809137,11.9111457026238,28.7531675856395));
#73811=CARTESIAN_POINT('Ctrl Pts',(202.302602928235,11.8863896722701,28.7244452344738));
#73812=CARTESIAN_POINT('Ctrl Pts',(202.301995624792,11.8805947336533,28.7178716397885));
#73813=CARTESIAN_POINT('Ctrl Pts',(202.301015472042,11.8710455793582,28.7072800725767));
#73814=CARTESIAN_POINT('Ctrl Pts',(202.300639603373,11.8673357648595,28.7032227671791));
#73815=CARTESIAN_POINT('Ctrl Pts',(202.299893400544,11.8598719906001,28.6951737800827));
#73816=CARTESIAN_POINT('Ctrl Pts',(202.299523063515,11.8561183161034,28.6911820252706));
#73817=CARTESIAN_POINT('Ctrl Pts',(202.298571373718,11.8463483251833,28.6809365869243));
#73818=CARTESIAN_POINT('Ctrl Pts',(202.297993043373,11.8402903825742,28.674722806553));
#73819=CARTESIAN_POINT('Ctrl Pts',(202.295379379666,11.8123910955407,28.6467315616968));
#73820=CARTESIAN_POINT('Ctrl Pts',(202.293396270798,11.7897663499811,28.6257484455269));
#73821=CARTESIAN_POINT('Ctrl Pts',(202.286833881049,11.7110523478269,28.5582987942358));
#73822=CARTESIAN_POINT('Ctrl Pts',(202.282398957624,11.6514865005786,28.5161489115263));
#73823=CARTESIAN_POINT('Ctrl Pts',(202.274682174716,11.5444209384503,28.454400060992));
#73824=CARTESIAN_POINT('Ctrl Pts',(202.271468008235,11.498845016673,28.4319053525508));
#73825=CARTESIAN_POINT('Ctrl Pts',(202.267172728344,11.4380660658995,28.4066475079555));
#73826=CARTESIAN_POINT('Ctrl Pts',(202.266182580057,11.4240599287354,28.4011393656927));
#73827=CARTESIAN_POINT('Ctrl Pts',(202.264536251259,11.4008091643122,28.3925063411857));
#73828=CARTESIAN_POINT('Ctrl Pts',(202.263885221659,11.3916241559436,28.3892251796864));
#73829=CARTESIAN_POINT('Ctrl Pts',(202.26259994936,11.3735168342792,28.3830092030314));
#73830=CARTESIAN_POINT('Ctrl Pts',(202.261966025628,11.364598058348,28.3800662907447));
#73831=CARTESIAN_POINT('Ctrl Pts',(202.260434968091,11.3430929283237,28.3732543876834));
#73832=CARTESIAN_POINT('Ctrl Pts',(202.259534584571,11.3304752646235,28.3694892713367));
#73833=CARTESIAN_POINT('Ctrl Pts',(202.256213440429,11.2840583506269,28.3564819015173));
#73834=CARTESIAN_POINT('Ctrl Pts',(202.25375283203,11.2499172890328,28.348538446409));
#73835=CARTESIAN_POINT('Ctrl Pts',(202.244297781506,11.1196581841898,28.3242976779898));
#73836=CARTESIAN_POINT('Ctrl Pts',(202.237035502614,11.0220119630204,28.3184306998474));
#73837=CARTESIAN_POINT('Ctrl Pts',(202.228099293334,10.8983345845817,28.3263472824764));
#73838=CARTESIAN_POINT('Ctrl Pts',(202.22621225451,10.8719652531414,28.3289304495842));
#73839=CARTESIAN_POINT('Ctrl Pts',(202.223770475137,10.8372581888328,28.3335169381678));
#73840=CARTESIAN_POINT('Ctrl Pts',(202.223180472195,10.8288249651324,28.3347246039811));
#73841=CARTESIAN_POINT('Ctrl Pts',(202.22225810465,10.815555613766,28.3367719870329));
#73842=CARTESIAN_POINT('Ctrl Pts',(202.221922579919,10.8107105513479,28.3375505823512));
#73843=CARTESIAN_POINT('Ctrl Pts',(202.221221699291,10.8005485419445,28.3392488245125));
#73844=CARTESIAN_POINT('Ctrl Pts',(202.220856727616,10.7952327938774,28.34017476805));
#73845=CARTESIAN_POINT('Ctrl Pts',(202.219936861365,10.781779926252,28.3426134789471));
#73846=CARTESIAN_POINT('Ctrl Pts',(202.2193846068,10.7736518502921,28.34417558238));
#73847=CARTESIAN_POINT('Ctrl Pts',(202.217082032174,10.7395825240928,28.3510964225721));
#73848=CARTESIAN_POINT('Ctrl Pts',(202.215369865782,10.7138074880022,28.3572442206944));
#73849=CARTESIAN_POINT('Ctrl Pts',(202.210303398002,10.6370712384756,28.3783068840432));
#73850=CARTESIAN_POINT('Ctrl Pts',(202.207029744722,10.5868880170377,28.3958025914628));
#73851=CARTESIAN_POINT('Ctrl Pts',(202.199473587729,10.4746513116737,28.4436598272312));
#73852=CARTESIAN_POINT('Ctrl Pts',(202.195190834194,10.4137510780786,28.4762047962713));
#73853=CARTESIAN_POINT('Ctrl Pts',(202.189533890876,10.3406406648647,28.5239472412827));
#73854=CARTESIAN_POINT('Ctrl Pts',(202.188330212342,10.3254710142461,28.5343684401743));
#73855=CARTESIAN_POINT('Ctrl Pts',(202.186416224703,10.302002181585,28.551313894553));
#73856=CARTESIAN_POINT('Ctrl Pts',(202.185714750933,10.2935355456379,28.5576018654728));
#73857=CARTESIAN_POINT('Ctrl Pts',(202.184395967035,10.2778765181609,28.5695610664678));
#73858=CARTESIAN_POINT('Ctrl Pts',(202.183779773645,10.2706635842321,28.5752041757013));
#73859=CARTESIAN_POINT('Ctrl Pts',(202.182386878713,10.2545957512016,28.5880798968049));
#73860=CARTESIAN_POINT('Ctrl Pts',(202.181608405642,10.2457789925937,28.5953583997615));
#73861=CARTESIAN_POINT('Ctrl Pts',(202.179209599797,10.2191172016969,28.61802922611));
#73862=CARTESIAN_POINT('Ctrl Pts',(202.177573107094,10.2016279420082,28.6338289358867));
#73863=CARTESIAN_POINT('Ctrl Pts',(202.168164433066,10.1050545951264,28.7264837400066));
#73864=CARTESIAN_POINT('Ctrl Pts',(202.15994785122,10.036606398993,28.813618377259));
#73865=CARTESIAN_POINT('Ctrl Pts',(202.149860365087,9.9665980474703,28.9342861070032));
#73866=CARTESIAN_POINT('Ctrl Pts',(202.147769170218,9.9528569689626,28.9601448580042));
#73867=CARTESIAN_POINT('Ctrl Pts',(202.145113181235,9.93626771097557,28.9943858770252));
#73868=CARTESIAN_POINT('Ctrl Pts',(202.144505155025,9.93253089424146,29.002323655675));
#73869=CARTESIAN_POINT('Ctrl Pts',(202.143524132538,9.92659628328447,29.0153044567301));
#73870=CARTESIAN_POINT('Ctrl Pts',(202.14314810735,9.92434458167624,29.0203222614596));
#73871=CARTESIAN_POINT('Ctrl Pts',(202.142401887484,9.91992072897877,29.0303684108311));
#73872=CARTESIAN_POINT('Ctrl Pts',(202.142031687107,9.91774834296817,29.0353964970172));
#73873=CARTESIAN_POINT('Ctrl Pts',(202.141080789307,9.91222894697797,29.0484201886932));
#73874=CARTESIAN_POINT('Ctrl Pts',(202.140503104659,9.90893491206901,29.0564380826462));
#73875=CARTESIAN_POINT('Ctrl Pts',(202.137897873104,9.89436865289219,29.0930376925021));
#73876=CARTESIAN_POINT('Ctrl Pts',(202.135922137746,9.88412800905759,29.1220197890091));
#73877=CARTESIAN_POINT('Ctrl Pts',(202.130618443937,9.85933247914011,29.2020310365511));
#73878=CARTESIAN_POINT('Ctrl Pts',(202.127354402169,9.84707220739804,29.2536953932601));
#73879=CARTESIAN_POINT('Ctrl Pts',(202.120047762593,9.8276522411702,29.3699887905078));
#73880=CARTESIAN_POINT('Ctrl Pts',(202.116002863071,9.8222733154405,29.4347295545688));
#73881=CARTESIAN_POINT('Ctrl Pts',(202.111797459566,9.8222500756293,29.4995779279502));
#73882=CARTESIAN_POINT('Ctrl Pts',(202.111797390249,9.82225007524673,29.4995789968314));
#73883=CARTESIAN_POINT('Ctrl Pts',(202.110815059892,9.82224466046326,29.5147267707691));
#73884=CARTESIAN_POINT('Ctrl Pts',(202.109824898362,9.82253148291806,29.5298728065725));
#73885=CARTESIAN_POINT('Ctrl Pts',(202.108225926865,9.82345809938344,29.5541020106972));
#73886=CARTESIAN_POINT('Ctrl Pts',(202.107622749208,9.82391123110373,29.5631907553504));
#73887=CARTESIAN_POINT('Ctrl Pts',(202.106433228909,9.82500660924456,29.5810072000648));
#73888=CARTESIAN_POINT('Ctrl Pts',(202.105847166201,9.82564090147191,29.5897348066708));
#73889=CARTESIAN_POINT('Ctrl Pts',(202.104673854135,9.82709785043405,29.6071024061211));
#73890=CARTESIAN_POINT('Ctrl Pts',(202.104086690831,9.82791887480166,29.6157419841826));
#73891=CARTESIAN_POINT('Ctrl Pts',(202.102511124886,9.83036559446865,29.6387819218762));
#73892=CARTESIAN_POINT('Ctrl Pts',(202.101517551966,9.83216167784353,29.6531622850066));
#73893=CARTESIAN_POINT('Ctrl Pts',(202.097419651724,9.84059314690329,29.7118423120483));
#73894=CARTESIAN_POINT('Ctrl Pts',(202.094247697465,9.84948708032826,29.7557744767564));
#73895=CARTESIAN_POINT('Ctrl Pts',(202.08804442112,9.87134243596284,29.8390149254104));
#73896=CARTESIAN_POINT('Ctrl Pts',(202.085026047646,9.88391647458372,29.8783599405461));
#73897=CARTESIAN_POINT('Ctrl Pts',(202.078610468218,9.91489553506312,29.9601960921077));
#73898=CARTESIAN_POINT('Ctrl Pts',(202.075216367976,9.93379397194834,30.0024313043787));
#73899=CARTESIAN_POINT('Ctrl Pts',(202.070126924273,9.96645013082245,30.065218459771));
#73900=CARTESIAN_POINT('Ctrl Pts',(202.068383322709,9.97845184713072,30.0866317426348));
#73901=CARTESIAN_POINT('Ctrl Pts',(202.066112236727,9.99527814067069,30.1145682724623));
#73902=CARTESIAN_POINT('Ctrl Pts',(202.065554090862,9.99951254329009,30.1214378763027));
#73903=CARTESIAN_POINT('Ctrl Pts',(202.064632738586,10.0066736826792,30.1327926677804));
#73904=CARTESIAN_POINT('Ctrl Pts',(202.06426714154,10.0095609550455,30.1373023109949));
#73905=CARTESIAN_POINT('Ctrl Pts',(202.063567411522,10.0151771608702,30.145943924965));
#73906=CARTESIAN_POINT('Ctrl Pts',(202.063232974597,10.0179015365306,30.1500786021413));
#73907=CARTESIAN_POINT('Ctrl Pts',(202.062312070389,10.0255119565867,30.1614715930988));
#73908=CARTESIAN_POINT('Ctrl Pts',(202.061729069598,10.030453044844,30.1686929999087));
#73909=CARTESIAN_POINT('Ctrl Pts',(202.059233275113,10.0521150070246,30.1996070229639));
#73910=CARTESIAN_POINT('Ctrl Pts',(202.057365936619,10.0696285723152,30.222734561568));
#73911=CARTESIAN_POINT('Ctrl Pts',(202.055038058666,10.0928528699894,30.251158084902));
#73912=CARTESIAN_POINT('Ctrl Pts',(202.054551786683,10.0977829845227,30.2570724965672));
#73913=CARTESIAN_POINT('Ctrl Pts',(202.054067314992,10.1027691090856,30.2629362954329));
#73914=CARTESIAN_POINT('',(202.012132885264,9.82225039357706,29.5009628450546));
#73915=CARTESIAN_POINT('Ctrl Pts',(201.956062524555,10.1027690874833,30.2629362700282));
#73916=CARTESIAN_POINT('Ctrl Pts',(201.959231248475,10.0722998560055,30.2271037405805));
#73917=CARTESIAN_POINT('Ctrl Pts',(201.962399972395,10.0439770287748,30.1894390707115));
#73918=CARTESIAN_POINT('Ctrl Pts',(201.965568696315,10.0180161642766,30.1502328881854));
#73919=CARTESIAN_POINT('Ctrl Pts',(201.968740482662,9.99203020978663,30.1109888146717));
#73920=CARTESIAN_POINT('Ctrl Pts',(201.971912269009,9.96841108119265,30.0702007206587));
#73921=CARTESIAN_POINT('Ctrl Pts',(201.975084055356,9.94733054177144,30.0281875369722));
#73922=CARTESIAN_POINT('Ctrl Pts',(201.978257627242,9.92623813518307,29.9861507022082));
#73923=CARTESIAN_POINT('Ctrl Pts',(201.981431199127,9.90768738274832,29.9428879167524));
#73924=CARTESIAN_POINT('Ctrl Pts',(201.984604771013,9.89180212028469,29.8987386636564));
#73925=CARTESIAN_POINT('Ctrl Pts',(201.987784073839,9.87588817169199,29.8545096843881));
#73926=CARTESIAN_POINT('Ctrl Pts',(201.990963376665,9.86264947248109,29.8093915779742));
#73927=CARTESIAN_POINT('Ctrl Pts',(201.994142679492,9.85215965284453,29.7637377484207));
#73928=CARTESIAN_POINT('Ctrl Pts',(201.995279715924,9.84840810486501,29.7474102482393));
#73929=CARTESIAN_POINT('Ctrl Pts',(201.996416752356,9.84500766990641,29.7310142991353));
#73930=CARTESIAN_POINT('Ctrl Pts',(201.997553788788,9.84196010705662,29.7145662341835));
#73931=CARTESIAN_POINT('Ctrl Pts',(202.002413487614,9.82893480972929,29.6442671305995));
#73932=CARTESIAN_POINT('Ctrl Pts',(202.007273186439,9.8223090797843,29.57274766355));
#73933=CARTESIAN_POINT('Ctrl Pts',(202.012132885264,9.82225039357706,29.5009628450546));
#73934=CARTESIAN_POINT('Ctrl Pts',(202.012133243127,9.82166172758912,29.5009580375033));
#73935=CARTESIAN_POINT('Ctrl Pts',(202.033490724592,9.82444460082249,29.1853167740295));
#73936=CARTESIAN_POINT('Ctrl Pts',(202.081065505636,10.1166312015937,28.4776655224031));
#73937=CARTESIAN_POINT('Ctrl Pts',(202.154857586256,11.3065618033661,28.1464851504412));
#73938=CARTESIAN_POINT('Ctrl Pts',(202.233509484991,12.2989858935547,29.0115143445247));
#73939=CARTESIAN_POINT('Ctrl Pts',(202.312161383725,12.122459760303,30.3161290791044));
#73940=CARTESIAN_POINT('Ctrl Pts',(202.386322574714,11.003589618022,30.8537585105574));
#73941=CARTESIAN_POINT('Ctrl Pts',(202.434266466125,10.3124415083501,30.5059938962083));
#73942=CARTESIAN_POINT('Ctrl Pts',(202.455993057958,10.1022055060817,30.2634229920695));
#73943=CARTESIAN_POINT('Origin',(197.762132885264,11.,29.5));
#73944=CARTESIAN_POINT('',(203.055732095072,10.1027690874946,30.2629362700414));
#73945=CARTESIAN_POINT('',(202.956095255396,10.1027690874833,30.2629362700282));
#73946=CARTESIAN_POINT('',(197.762132885264,10.1027690874833,30.2629362700282));
#73947=CARTESIAN_POINT('Ctrl Pts',(203.055732095072,10.1027690874946,30.2629362700414));
#73948=CARTESIAN_POINT('Ctrl Pts',(203.055680843042,10.1032781498017,30.2635349392308));
#73949=CARTESIAN_POINT('Ctrl Pts',(203.055629568757,10.1037878130808,30.264133101021));
#73950=CARTESIAN_POINT('Ctrl Pts',(203.054627409232,10.1137565972493,30.2758091832254));
#73951=CARTESIAN_POINT('Ctrl Pts',(203.053669019665,10.1234194835438,30.2867107637418));
#73952=CARTESIAN_POINT('Ctrl Pts',(203.052647775855,10.1338394543902,30.2980361208704));
#73953=CARTESIAN_POINT('Ctrl Pts',(203.05259308966,10.1343978004303,30.2986417050714));
#73954=CARTESIAN_POINT('Ctrl Pts',(203.05248303782,10.1355221718152,30.2998586382674));
#73955=CARTESIAN_POINT('Ctrl Pts',(203.052427671609,10.1360882114565,30.3004699733555));
#73956=CARTESIAN_POINT('Ctrl Pts',(203.052315191132,10.1372389239659,30.3017101255663));
#73957=CARTESIAN_POINT('Ctrl Pts',(203.052258075249,10.1378236366753,30.3023389048731));
#73958=CARTESIAN_POINT('Ctrl Pts',(203.052184527674,10.1385770753782,30.3031473514772));
#73959=CARTESIAN_POINT('Ctrl Pts',(203.052168121955,10.1387451720562,30.3033276072637));
#73960=CARTESIAN_POINT('Ctrl Pts',(203.05212771863,10.1391592337816,30.3037713403921));
#73961=CARTESIAN_POINT('Ctrl Pts',(203.05210371837,10.1394052631049,30.304034757487));
#73962=CARTESIAN_POINT('Ctrl Pts',(203.052042729131,10.1400306470631,30.3047037236707));
#73963=CARTESIAN_POINT('Ctrl Pts',(203.052005733301,10.1404101673567,30.3051091171356));
#73964=CARTESIAN_POINT('Ctrl Pts',(203.051906171747,10.1414319576996,30.3061990202835));
#73965=CARTESIAN_POINT('Ctrl Pts',(203.051843584017,10.1420747585667,30.3068830297314));
#73966=CARTESIAN_POINT('Ctrl Pts',(203.051167479638,10.1490236547461,30.3142597135316));
#73967=CARTESIAN_POINT('Ctrl Pts',(203.050550754934,10.1554069532658,30.3208789183382));
#73968=CARTESIAN_POINT('Ctrl Pts',(203.049237100713,10.16909327834,30.3347424048816));
#73969=CARTESIAN_POINT('Ctrl Pts',(203.048539392156,10.1764149779946,30.341967079295));
#73970=CARTESIAN_POINT('Ctrl Pts',(203.046633966654,10.1965459228127,30.3613174168705));
#73971=CARTESIAN_POINT('Ctrl Pts',(203.04541840481,10.2095340063792,30.3732523128998));
#73972=CARTESIAN_POINT('Ctrl Pts',(203.038084981684,10.2887110509025,30.4427949462142));
#73973=CARTESIAN_POINT('Ctrl Pts',(203.031681283272,10.3608914857695,30.4931411840402));
#73974=CARTESIAN_POINT('Ctrl Pts',(203.022267843458,10.4737248643307,30.5544118795783));
#73975=CARTESIAN_POINT('Ctrl Pts',(203.01929087227,10.510457895681,30.5719602586778));
#73976=CARTESIAN_POINT('Ctrl Pts',(203.014738385877,10.5690456783002,30.5963081303578));
#73977=CARTESIAN_POINT('Ctrl Pts',(203.013124362118,10.5903147573183,30.6044325703768));
#73978=CARTESIAN_POINT('Ctrl Pts',(203.010993040844,10.6192317412858,30.6145278971009));
#73979=CARTESIAN_POINT('Ctrl Pts',(203.010449461822,10.6266820344865,30.6170454803909));
#73980=CARTESIAN_POINT('Ctrl Pts',(203.009545315264,10.6392099006661,30.6211395196765));
#73981=CARTESIAN_POINT('Ctrl Pts',(203.009182539078,10.6442738607892,30.6227565349147));
#73982=CARTESIAN_POINT('Ctrl Pts',(203.008433252243,10.6548140336075,30.6260437312999));
#73983=CARTESIAN_POINT('Ctrl Pts',(203.008047045596,10.6602917430333,30.6277083575887));
#73984=CARTESIAN_POINT('Ctrl Pts',(203.007004280114,10.6751966696347,30.6321193700147));
#73985=CARTESIAN_POINT('Ctrl Pts',(203.006351911604,10.6846466765809,30.6347879837958));
#73986=CARTESIAN_POINT('Ctrl Pts',(203.002164895242,10.7460214579951,30.6512938443267));
#73987=CARTESIAN_POINT('Ctrl Pts',(202.998791908116,10.7988145861149,30.6616834621295));
#73988=CARTESIAN_POINT('Ctrl Pts',(202.992769888853,10.894926854562,30.6738461823303));
#73989=CARTESIAN_POINT('Ctrl Pts',(202.990114214701,10.9379801782754,30.6769064415476));
#73990=CARTESIAN_POINT('Ctrl Pts',(202.98397387263,11.0365449798987,30.6784880093941));
#73991=CARTESIAN_POINT('Ctrl Pts',(202.980474848749,11.0919731100244,30.6754613590028));
#73992=CARTESIAN_POINT('Ctrl Pts',(202.975877275283,11.1618656840739,30.6666703536199));
#73993=CARTESIAN_POINT('Ctrl Pts',(202.974889972326,11.1767157005816,30.6645135215963));
#73994=CARTESIAN_POINT('Ctrl Pts',(202.973247102297,11.2011345833073,30.6604890754538));
#73995=CARTESIAN_POINT('Ctrl Pts',(202.972596641371,11.2107289459064,30.6587852763489));
#73996=CARTESIAN_POINT('Ctrl Pts',(202.971318688234,11.2294276491071,30.6552247986348));
#73997=CARTESIAN_POINT('Ctrl Pts',(202.970691580828,11.2385333564163,30.6533790404657));
#73998=CARTESIAN_POINT('Ctrl Pts',(202.969170521598,11.2604449155126,30.6486669227774));
#73999=CARTESIAN_POINT('Ctrl Pts',(202.968273291072,11.2732263043942,30.6456939452318));
#74000=CARTESIAN_POINT('Ctrl Pts',(202.965153367229,11.3171608775189,30.634697693232));
#74001=CARTESIAN_POINT('Ctrl Pts',(202.962898111862,11.3480309674229,30.6256127175271));
#74002=CARTESIAN_POINT('Ctrl Pts',(202.954032973177,11.4659757254293,30.5855861397693));
#74003=CARTESIAN_POINT('Ctrl Pts',(202.947174156403,11.5496610942254,30.5457054026598));
#74004=CARTESIAN_POINT('Ctrl Pts',(202.938813610157,11.6471416240832,30.4842889339539));
#74005=CARTESIAN_POINT('Ctrl Pts',(202.937169021679,11.666113520727,30.4715502473107));
#74006=CARTESIAN_POINT('Ctrl Pts',(202.934445477494,11.6973457816444,30.4492340790081));
#74007=CARTESIAN_POINT('Ctrl Pts',(202.933354180476,11.7098084929985,30.4399512939669));
#74008=CARTESIAN_POINT('Ctrl Pts',(202.931804333534,11.7274791297496,30.4262374467272));
#74009=CARTESIAN_POINT('Ctrl Pts',(202.931334035724,11.7328373648677,30.4220038471901));
#74010=CARTESIAN_POINT('Ctrl Pts',(202.930513096468,11.7421886970022,30.4144822302504));
#74011=CARTESIAN_POINT('Ctrl Pts',(202.930161151955,11.7461973778875,30.4112141834317));
#74012=CARTESIAN_POINT('Ctrl Pts',(202.929387288056,11.7550115095409,30.4039313513662));
#74013=CARTESIAN_POINT('Ctrl Pts',(202.928966216342,11.7598066278451,30.3999045283765));
#74014=CARTESIAN_POINT('Ctrl Pts',(202.927717016697,11.7740209647889,30.3877730600783));
#74015=CARTESIAN_POINT('Ctrl Pts',(202.926896294633,11.7833446006181,30.379557119491));
#74016=CARTESIAN_POINT('Ctrl Pts',(202.922710967772,11.8306909423731,30.3364855536004));
#74017=CARTESIAN_POINT('Ctrl Pts',(202.919481849449,11.8665279785901,30.2993034108727));
#74018=CARTESIAN_POINT('Ctrl Pts',(202.913535620728,11.9283039056173,30.2261519439091));
#74019=CARTESIAN_POINT('Ctrl Pts',(202.910816554321,11.9548732780497,30.1908413557434));
#74020=CARTESIAN_POINT('Ctrl Pts',(202.904784716255,12.0085664476718,30.1104482551197));
#74021=CARTESIAN_POINT('Ctrl Pts',(202.901462639821,12.0347786643422,30.0648765558394));
#74022=CARTESIAN_POINT('Ctrl Pts',(202.8970664188,12.0643751118692,30.0044009185384));
#74023=CARTESIAN_POINT('Ctrl Pts',(202.896091023205,12.0706371536587,29.9909691628448));
#74024=CARTESIAN_POINT('Ctrl Pts',(202.894462614784,12.080578718015,29.9685498037149));
#74025=CARTESIAN_POINT('Ctrl Pts',(202.893814522233,12.0844035991361,29.9596282292777));
#74026=CARTESIAN_POINT('Ctrl Pts',(202.892537267893,12.091681752065,29.9420551674603));
#74027=CARTESIAN_POINT('Ctrl Pts',(202.8919084453,12.0951435290475,29.9334079615581));
#74028=CARTESIAN_POINT('Ctrl Pts',(202.890376220481,12.1032835029046,29.912354649154));
#74029=CARTESIAN_POINT('Ctrl Pts',(202.889469418248,12.1078553795046,29.8999090870023));
#74030=CARTESIAN_POINT('Ctrl Pts',(202.88627442573,12.1231051703897,29.8561261108039));
#74031=CARTESIAN_POINT('Ctrl Pts',(202.883951519012,12.1326703187605,29.8244204337307));
#74032=CARTESIAN_POINT('Ctrl Pts',(202.875321200213,12.1627358145608,29.7070933788016));
#74033=CARTESIAN_POINT('Ctrl Pts',(202.868797896447,12.1749561833651,29.6196543094049));
#74034=CARTESIAN_POINT('Ctrl Pts',(202.860603847715,12.1779880007342,29.5070022994887));
#74035=CARTESIAN_POINT('Ctrl Pts',(202.858822267767,12.1778759334513,29.4823028715509));
#74036=CARTESIAN_POINT('Ctrl Pts',(202.855901017729,12.1763968956361,29.4412228894436));
#74037=CARTESIAN_POINT('Ctrl Pts',(202.854746807826,12.1754636066253,29.4248349871955));
#74038=CARTESIAN_POINT('Ctrl Pts',(202.853125269173,12.1736460752085,29.4015186213488));
#74039=CARTESIAN_POINT('Ctrl Pts',(202.852644716915,12.1730423771763,29.3945709759028));
#74040=CARTESIAN_POINT('Ctrl Pts',(202.85181264557,12.171882352138,29.3824683395311));
#74041=CARTESIAN_POINT('Ctrl Pts',(202.851459696122,12.1713536465001,29.3773110556263));
#74042=CARTESIAN_POINT('Ctrl Pts',(202.850691619274,12.1701223728775,29.366034995921));
#74043=CARTESIAN_POINT('Ctrl Pts',(202.850277242421,12.1694058481839,29.3599180373785));
#74044=CARTESIAN_POINT('Ctrl Pts',(202.849092397077,12.167207046065,29.3423412191106));
#74045=CARTESIAN_POINT('Ctrl Pts',(202.848328100148,12.1656040163684,29.3308968340791));
#74046=CARTESIAN_POINT('Ctrl Pts',(202.842847317745,12.1527817371813,29.24823135497));
#74047=CARTESIAN_POINT('Ctrl Pts',(202.838409050936,12.1352104187687,29.1781410722922));
#74048=CARTESIAN_POINT('Ctrl Pts',(202.830816480958,12.0946178772813,29.06244240569));
#74049=CARTESIAN_POINT('Ctrl Pts',(202.827685327214,12.0748540342913,29.0159201462508));
#74050=CARTESIAN_POINT('Ctrl Pts',(202.822465190349,12.0379475106917,28.9425401119848));
#74051=CARTESIAN_POINT('Ctrl Pts',(202.820426284475,12.0225954238784,28.9148548074865));
#74052=CARTESIAN_POINT('Ctrl Pts',(202.817514404407,11.9995378481877,28.8769583579396));
#74053=CARTESIAN_POINT('Ctrl Pts',(202.816673700478,11.9927521488411,28.8662019657554));
#74054=CARTESIAN_POINT('Ctrl Pts',(202.815206204755,11.9806961195293,28.8477600313134));
#74055=CARTESIAN_POINT('Ctrl Pts',(202.814582382036,11.9755062121205,28.8400231236357));
#74056=CARTESIAN_POINT('Ctrl Pts',(202.813288878381,11.964615496345,28.8241968261762));
#74057=CARTESIAN_POINT('Ctrl Pts',(202.812618811956,11.9589034392141,28.8161161139785));
#74058=CARTESIAN_POINT('Ctrl Pts',(202.810872551444,11.9438405194629,28.795366726435));
#74059=CARTESIAN_POINT('Ctrl Pts',(202.809790622335,11.9343364768442,28.7828122399104));
#74060=CARTESIAN_POINT('Ctrl Pts',(202.804141480277,11.8838563209864,28.7188367650232));
#74061=CARTESIAN_POINT('Ctrl Pts',(202.799419252803,11.8388844241077,28.6707301712796));
#74062=CARTESIAN_POINT('Ctrl Pts',(202.790264333226,11.7459129723658,28.5866182531947));
#74063=CARTESIAN_POINT('Ctrl Pts',(202.785860359933,11.6987083496574,28.550021470181));
#74064=CARTESIAN_POINT('Ctrl Pts',(202.779523365885,11.6254627175357,28.5016601115336));
#74065=CARTESIAN_POINT('Ctrl Pts',(202.777517313253,11.601441470568,28.4870071209755));
#74066=CARTESIAN_POINT('Ctrl Pts',(202.774967519875,11.5695615095073,28.4690946086997));
#74067=CARTESIAN_POINT('Ctrl Pts',(202.774383337573,11.5621619376391,28.4650409645794));
#74068=CARTESIAN_POINT('Ctrl Pts',(202.773430952061,11.5499305941691,28.4585102632211));
#74069=CARTESIAN_POINT('Ctrl Pts',(202.773060028539,11.545124234702,28.4559865409443));
#74070=CARTESIAN_POINT('Ctrl Pts',(202.772359851088,11.535966984788,28.4512587362909));
#74071=CARTESIAN_POINT('Ctrl Pts',(202.77203019341,11.5316195730708,28.4490482986031));
#74072=CARTESIAN_POINT('Ctrl Pts',(202.771139869936,11.5197845981412,28.4431230469294));
#74073=CARTESIAN_POINT('Ctrl Pts',(202.770582289674,11.5122708547884,28.4394607487037));
#74074=CARTESIAN_POINT('Ctrl Pts',(202.76837294971,11.4821223770687,28.4251611633876));
#74075=CARTESIAN_POINT('Ctrl Pts',(202.766754577643,11.4591887894553,28.4151652821945));
#74076=CARTESIAN_POINT('Ctrl Pts',(202.760508462554,11.3681958896788,28.3789082449727));
#74077=CARTESIAN_POINT('Ctrl Pts',(202.756061716407,11.2980736246609,28.3582607568604));
#74078=CARTESIAN_POINT('Ctrl Pts',(202.749151273178,11.1891143927155,28.3369087664863));
#74079=CARTESIAN_POINT('Ctrl Pts',(202.746761534561,11.1514098555323,28.3314024538564));
#74080=CARTESIAN_POINT('Ctrl Pts',(202.742636273087,11.0872377364288,28.3251888764688));
#74081=CARTESIAN_POINT('Ctrl Pts',(202.740926536077,11.0608922317289,28.3235291871946));
#74082=CARTESIAN_POINT('Ctrl Pts',(202.738405999966,11.0226011179861,28.3224065615593));
#74083=CARTESIAN_POINT('Ctrl Pts',(202.737616553207,11.0106833403763,28.3222381539321));
#74084=CARTESIAN_POINT('Ctrl Pts',(202.736207610044,10.989561162409,28.3222602955815));
#74085=CARTESIAN_POINT('Ctrl Pts',(202.735590398887,10.9803575762404,28.3223778416808));
#74086=CARTESIAN_POINT('Ctrl Pts',(202.734279188534,10.9609157152983,28.3228541218712));
#74087=CARTESIAN_POINT('Ctrl Pts',(202.733584450051,10.9506788985628,28.3232385894829));
#74088=CARTESIAN_POINT('Ctrl Pts',(202.731696215378,10.9230379234061,28.3246380079384));
#74089=CARTESIAN_POINT('Ctrl Pts',(202.7304951147,10.9056497422518,28.3259059037964));
#74090=CARTESIAN_POINT('Ctrl Pts',(202.722146413182,10.7861721740504,28.3372890096141));
#74091=CARTESIAN_POINT('Ctrl Pts',(202.714591947284,10.6857714163812,28.360319457924));
#74092=CARTESIAN_POINT('Ctrl Pts',(202.704835598859,10.5606254772465,28.4068377045368));
#74093=CARTESIAN_POINT('Ctrl Pts',(202.702586784527,10.5320375337698,28.4187668478015));
#74094=CARTESIAN_POINT('Ctrl Pts',(202.699434230431,10.4919845989892,28.4373667124116));
#74095=CARTESIAN_POINT('Ctrl Pts',(202.698499505484,10.4801114007151,28.4431248765721));
#74096=CARTESIAN_POINT('Ctrl Pts',(202.696847966787,10.4590990843684,28.4537550755485));
#74097=CARTESIAN_POINT('Ctrl Pts',(202.696127656477,10.4499228236178,28.4585503561841));
#74098=CARTESIAN_POINT('Ctrl Pts',(202.695011820326,10.4356721149258,28.4662383304664));
#74099=CARTESIAN_POINT('Ctrl Pts',(202.694611657582,10.4305541653932,28.4690486935046));
#74100=CARTESIAN_POINT('Ctrl Pts',(202.693855194093,10.4208613809318,28.4744653881438));
#74101=CARTESIAN_POINT('Ctrl Pts',(202.693498502634,10.4162828478185,28.4770644851774));
#74102=CARTESIAN_POINT('Ctrl Pts',(202.692714019237,10.4061986483785,28.4828787370349));
#74103=CARTESIAN_POINT('Ctrl Pts',(202.692287098517,10.4007012857268,28.4861081101428));
#74104=CARTESIAN_POINT('Ctrl Pts',(202.690820638438,10.3817975197126,28.4974204221378));
#74105=CARTESIAN_POINT('Ctrl Pts',(202.689793854242,10.3685256027968,28.5057262661534));
#74106=CARTESIAN_POINT('Ctrl Pts',(202.683424349168,10.2863011080919,28.5594949332292));
#74107=CARTESIAN_POINT('Ctrl Pts',(202.678402752934,10.2221184000583,28.6118450978308));
#74108=CARTESIAN_POINT('Ctrl Pts',(202.670801216305,10.1360005821777,28.6986428328698));
#74109=CARTESIAN_POINT('Ctrl Pts',(202.668316523167,10.1095060957555,28.7281913549308));
#74110=CARTESIAN_POINT('Ctrl Pts',(202.664047620732,10.0674885565508,28.7801019418046));
#74111=CARTESIAN_POINT('Ctrl Pts',(202.662291833948,10.0511576767984,28.8017673180915));
#74112=CARTESIAN_POINT('Ctrl Pts',(202.659716200441,10.0286803261493,28.8338333036164));
#74113=CARTESIAN_POINT('Ctrl Pts',(202.658919095352,10.0219223088576,28.843795772036));
#74114=CARTESIAN_POINT('Ctrl Pts',(202.657501573814,10.0102608438711,28.8615671936962));
#74115=CARTESIAN_POINT('Ctrl Pts',(202.656883543495,10.0052940965329,28.869333524916));
#74116=CARTESIAN_POINT('Ctrl Pts',(202.655575836246,9.99503453246077,28.8857987765837));
#74117=CARTESIAN_POINT('Ctrl Pts',(202.654885479561,9.98976235763914,28.8945095966244));
#74118=CARTESIAN_POINT('Ctrl Pts',(202.653022544091,9.97592383109144,28.9180579291021));
#74119=CARTESIAN_POINT('Ctrl Pts',(202.651842708975,9.96756747539825,28.9330153416418));
#74120=CARTESIAN_POINT('Ctrl Pts',(202.643424956179,9.91083221083597,29.0399839594525));
#74121=CARTESIAN_POINT('Ctrl Pts',(202.635766425098,9.87450427603867,29.1378502867752));
#74122=CARTESIAN_POINT('Ctrl Pts',(202.62595135567,9.8447502920661,29.2688722253721));
#74123=CARTESIAN_POINT('Ctrl Pts',(202.623741271508,9.83916153736228,29.2988129817721));
#74124=CARTESIAN_POINT('Ctrl Pts',(202.620636630948,9.8328427917312,29.3418558450068));
#74125=CARTESIAN_POINT('Ctrl Pts',(202.619711978533,9.83116131894318,29.3548046486921));
#74126=CARTESIAN_POINT('Ctrl Pts',(202.618076318371,9.82854248947339,29.3779842841225));
#74127=CARTESIAN_POINT('Ctrl Pts',(202.617361904896,9.82752301187368,29.3882043654187));
#74128=CARTESIAN_POINT('Ctrl Pts',(202.616253121267,9.82613533765032,29.4042362220099));
#74129=CARTESIAN_POINT('Ctrl Pts',(202.615854204919,9.82567635150799,29.4100393480641));
#74130=CARTESIAN_POINT('Ctrl Pts',(202.615098540063,9.82488372064845,29.4211039742857));
#74131=CARTESIAN_POINT('Ctrl Pts',(202.61474141895,9.82454235063374,29.4263646250114));
#74132=CARTESIAN_POINT('Ctrl Pts',(202.613954494939,9.82386441492197,29.4380227049632));
#74133=CARTESIAN_POINT('Ctrl Pts',(202.613525584593,9.82354469624644,29.4444210255535));
#74134=CARTESIAN_POINT('Ctrl Pts',(202.612019626454,9.82259988548525,29.4670282102739));
#74135=CARTESIAN_POINT('Ctrl Pts',(202.610956421556,9.82225741589799,29.4832478281828));
#74136=CARTESIAN_POINT('Ctrl Pts',(202.608292383451,9.82223891553685,29.5243782920293));
#74137=CARTESIAN_POINT('Ctrl Pts',(202.606709136802,9.82301788011519,29.5492819480859));
#74138=CARTESIAN_POINT('Ctrl Pts',(202.599236485343,9.83049718147126,29.6678529509664));
#74139=CARTESIAN_POINT('Ctrl Pts',(202.593563375472,9.84759260540199,29.7605174382398));
#74140=CARTESIAN_POINT('Ctrl Pts',(202.585762568486,9.88397375315317,29.8773468721764));
#74141=CARTESIAN_POINT('Ctrl Pts',(202.583924565957,9.89341845913494,29.9042058166407));
#74142=CARTESIAN_POINT('Ctrl Pts',(202.581310258946,9.90797830106162,29.9412624933523));
#74143=CARTESIAN_POINT('Ctrl Pts',(202.580560010367,9.91228290717186,29.9517692889339));
#74144=CARTESIAN_POINT('Ctrl Pts',(202.579182362429,9.92041068852575,29.9708179357425));
#74145=CARTESIAN_POINT('Ctrl Pts',(202.578556616415,9.9241850848633,29.9793796720359));
#74146=CARTESIAN_POINT('Ctrl Pts',(202.577278736077,9.93205712452158,29.9966750750828));
#74147=CARTESIAN_POINT('Ctrl Pts',(202.576626434617,9.93616085624116,30.0054051664011));
#74148=CARTESIAN_POINT('Ctrl Pts',(202.574983263801,9.94670784972809,30.0271446196849));
#74149=CARTESIAN_POINT('Ctrl Pts',(202.573987895985,9.95328512521703,30.0400867915711));
#74150=CARTESIAN_POINT('Ctrl Pts',(202.569638853393,9.98281966813092,30.0956353175832));
#74151=CARTESIAN_POINT('Ctrl Pts',(202.566204732469,10.0081489902168,30.1369205345175));
#74152=CARTESIAN_POINT('Ctrl Pts',(202.560074241281,10.0568819520254,30.2063655021954));
#74153=CARTESIAN_POINT('Ctrl Pts',(202.557410233282,10.0791829978597,30.2351984861022));
#74154=CARTESIAN_POINT('Ctrl Pts',(202.554740968482,10.1027692175106,30.2629364229433));
#74155=CARTESIAN_POINT('',(202.512132885264,9.82241330366484,29.4997412329417));
#74156=CARTESIAN_POINT('Ctrl Pts',(202.455993057958,10.1022055060817,30.2634229920695));
#74157=CARTESIAN_POINT('Ctrl Pts',(202.460483765703,10.0587514544313,30.2132855822843));
#74158=CARTESIAN_POINT('Ctrl Pts',(202.479197041472,9.89600478671947,29.9892296846299));
#74159=CARTESIAN_POINT('Ctrl Pts',(202.49791031724,9.82442155048356,29.7110002446274));
#74160=CARTESIAN_POINT('Ctrl Pts',(202.512132885264,9.82399939596064,29.4997415814752));
#74161=CARTESIAN_POINT('Ctrl Pts',(202.512132885264,9.82225002843514,29.499741197063));
#74162=CARTESIAN_POINT('Ctrl Pts',(202.515518432404,9.82226109535632,29.4493782983299));
#74163=CARTESIAN_POINT('Ctrl Pts',(202.518903979543,9.82550685479233,29.3990983077968));
#74164=CARTESIAN_POINT('Ctrl Pts',(202.522289526683,9.83193010758237,29.3493089620201));
#74165=CARTESIAN_POINT('Ctrl Pts',(202.525682877626,9.83836816619204,29.299404850081));
#74166=CARTESIAN_POINT('Ctrl Pts',(202.529076228569,9.84799823769769,29.2499940631929));
#74167=CARTESIAN_POINT('Ctrl Pts',(202.532469579511,9.86071226979931,29.2014727310376));
#74168=CARTESIAN_POINT('Ctrl Pts',(202.535875585276,9.87347371633343,29.1527704483065));
#74169=CARTESIAN_POINT('Ctrl Pts',(202.539281591041,9.88934198360819,29.1049646660309));
#74170=CARTESIAN_POINT('Ctrl Pts',(202.542687596805,9.90815950392749,29.0584352894126));
#74171=CARTESIAN_POINT('Ctrl Pts',(202.544497424512,9.91815845049761,29.0337112693051));
#74172=CARTESIAN_POINT('Ctrl Pts',(202.54630725222,9.92898931246574,29.0093472532393));
#74173=CARTESIAN_POINT('Ctrl Pts',(202.548117079927,9.94062323588956,28.9853973045515));
#74174=CARTESIAN_POINT('Ctrl Pts',(202.551394242374,9.96168947153411,28.9420297109759));
#74175=CARTESIAN_POINT('Ctrl Pts',(202.554671404822,9.98547061576457,28.8998599900416));
#74176=CARTESIAN_POINT('Ctrl Pts',(202.557948567269,10.0118041206999,28.8592473436386));
#74177=CARTESIAN_POINT('Ctrl Pts',(202.561122519601,10.0373082849678,28.8199137415311));
#74178=CARTESIAN_POINT('Ctrl Pts',(202.564296471932,10.0652060874267,28.7820410933764));
#74179=CARTESIAN_POINT('Ctrl Pts',(202.567470424264,10.0953023489157,28.7459328792325));
#74180=CARTESIAN_POINT('Ctrl Pts',(202.570641251632,10.1253689786737,28.7098602159789));
#74181=CARTESIAN_POINT('Ctrl Pts',(202.573812079001,10.1576294280711,28.6755489740434));
#74182=CARTESIAN_POINT('Ctrl Pts',(202.57698290637,10.1918464743423,28.6432719559469));
#74183=CARTESIAN_POINT('Ctrl Pts',(202.580152003315,10.2260448472609,28.6110125524667));
#74184=CARTESIAN_POINT('Ctrl Pts',(202.58332110026,10.262197297307,28.5807855550173));
#74185=CARTESIAN_POINT('Ctrl Pts',(202.586490197205,10.300029626991,28.5528270805129));
#74186=CARTESIAN_POINT('Ctrl Pts',(202.589658955268,10.3378579111343,28.5248715957041));
#74187=CARTESIAN_POINT('Ctrl Pts',(202.592827713331,10.3773652693388,28.4991844811355));
#74188=CARTESIAN_POINT('Ctrl Pts',(202.595996471394,10.4182464671013,28.4759600156928));
#74189=CARTESIAN_POINT('Ctrl Pts',(202.599168415829,10.4591687733149,28.4527121966829));
#74190=CARTESIAN_POINT('Ctrl Pts',(202.602340360265,10.5014671895777,28.431932241392));
#74191=CARTESIAN_POINT('Ctrl Pts',(202.6055123047,10.5448114327462,28.4137687029268));
#74192=CARTESIAN_POINT('Ctrl Pts',(202.608686193971,10.5881822518494,28.3955940277343));
#74193=CARTESIAN_POINT('Ctrl Pts',(202.611860083241,10.6325996482413,28.3800391456787));
#74194=CARTESIAN_POINT('Ctrl Pts',(202.615033972511,10.677716309635,28.3672033344749));
#74195=CARTESIAN_POINT('Ctrl Pts',(202.61821347699,10.7229127909046,28.3543448143023));
#74196=CARTESIAN_POINT('Ctrl Pts',(202.621392981468,10.7688104610883,28.3442150768383));
#74197=CARTESIAN_POINT('Ctrl Pts',(202.624572485947,10.8150518504685,28.3368623278026));
#74198=CARTESIAN_POINT('Ctrl Pts',(202.625304650185,10.8257001423181,28.3351691646282));
#74199=CARTESIAN_POINT('Ctrl Pts',(202.626036814423,10.8363666458221,28.3336230393355));
#74200=CARTESIAN_POINT('Ctrl Pts',(202.626768978661,10.8470469817718,28.3322241496268));
#74201=CARTESIAN_POINT('Ctrl Pts',(202.630046141109,10.8948520971775,28.325962728237));
#74202=CARTESIAN_POINT('Ctrl Pts',(202.633323303556,10.9431501762926,28.3226275013512));
#74203=CARTESIAN_POINT('Ctrl Pts',(202.636600466003,10.9915518289659,28.3222803003659));
#74204=CARTESIAN_POINT('Ctrl Pts',(202.639774418335,11.0384291323728,28.3219440340396));
#74205=CARTESIAN_POINT('Ctrl Pts',(202.642948370666,11.0854029767498,28.324410368306));
#74206=CARTESIAN_POINT('Ctrl Pts',(202.646122322998,11.1321125579884,28.3296832332562));
#74207=CARTESIAN_POINT('Ctrl Pts',(202.649293150366,11.1787761505999,28.3349509067272));
#74208=CARTESIAN_POINT('Ctrl Pts',(202.652463977735,11.2251754441529,28.3430195792481));
#74209=CARTESIAN_POINT('Ctrl Pts',(202.655634805104,11.2709521280664,28.3538411947744));
#74210=CARTESIAN_POINT('Ctrl Pts',(202.658803902049,11.3167038301579,28.3646569045938));
#74211=CARTESIAN_POINT('Ctrl Pts',(202.661972998994,11.3618330547225,28.3782224532127));
#74212=CARTESIAN_POINT('Ctrl Pts',(202.665142095939,11.4059917903771,28.3944387268693));
#74213=CARTESIAN_POINT('Ctrl Pts',(202.668310854002,11.4501458039867,28.4106532664641));
#74214=CARTESIAN_POINT('Ctrl Pts',(202.671479612065,11.4933290131051,28.4295177743398));
#74215=CARTESIAN_POINT('Ctrl Pts',(202.674648370128,11.5352112745426,28.4508842036732));
#74216=CARTESIAN_POINT('Ctrl Pts',(202.677820314563,11.5771356510597,28.4722721182091));
#74217=CARTESIAN_POINT('Ctrl Pts',(202.680992258999,11.6177559739234,28.4961667186593));
#74218=CARTESIAN_POINT('Ctrl Pts',(202.684164203435,11.6567665088359,28.5223738877406));
#74219=CARTESIAN_POINT('Ctrl Pts',(202.687338092705,11.6958009625288,28.5485971253921));
#74220=CARTESIAN_POINT('Ctrl Pts',(202.690511981975,11.7332232213621,28.5771354154916));
#74221=CARTESIAN_POINT('Ctrl Pts',(202.693685871246,11.7687593354638,28.6077533151436));
#74222=CARTESIAN_POINT('Ctrl Pts',(202.696865375724,11.804358319648,28.63842538363));
#74223=CARTESIAN_POINT('Ctrl Pts',(202.700044880203,11.838064106692,28.6711840104192));
#74224=CARTESIAN_POINT('Ctrl Pts',(202.703224384681,11.8696398113512,28.7057571775502));
#74225=CARTESIAN_POINT('Ctrl Pts',(202.70395654892,11.87691094492,28.7137185554139));
#74226=CARTESIAN_POINT('Ctrl Pts',(202.704688713158,11.8840693001278,28.7217760209683));
#74227=CARTESIAN_POINT('Ctrl Pts',(202.705420877396,11.8911123030715,28.7299260257516));
#74228=CARTESIAN_POINT('Ctrl Pts',(202.708698039843,11.922636739202,28.7664053950365));
#74229=CARTESIAN_POINT('Ctrl Pts',(202.71197520229,11.9519885788489,28.8049060144331));
#74230=CARTESIAN_POINT('Ctrl Pts',(202.715252364738,11.9789019996351,28.8451367031124));
#74231=CARTESIAN_POINT('Ctrl Pts',(202.718426317069,12.0049678160328,28.8841003767756));
#74232=CARTESIAN_POINT('Ctrl Pts',(202.721600269401,12.0287461994947,28.9246862528936));
#74233=CARTESIAN_POINT('Ctrl Pts',(202.724774221732,12.0500354065866,28.9665951749238));
#74234=CARTESIAN_POINT('Ctrl Pts',(202.727945049101,12.0713036530665,29.0084628348886));
#74235=CARTESIAN_POINT('Ctrl Pts',(202.73111587647,12.0900873230514,29.0516504680771));
#74236=CARTESIAN_POINT('Ctrl Pts',(202.734286703838,12.1062294598556,29.095832405248));
#74237=CARTESIAN_POINT('Ctrl Pts',(202.737455800784,12.1223627873718,29.1399902309018));
#74238=CARTESIAN_POINT('Ctrl Pts',(202.740624897729,12.1358572467915,29.1851407633922));
#74239=CARTESIAN_POINT('Ctrl Pts',(202.743793994674,12.1466041863574,29.2309388502076));
#74240=CARTESIAN_POINT('Ctrl Pts',(202.746962752737,12.1573499767163,29.2767320396764));
#74241=CARTESIAN_POINT('Ctrl Pts',(202.7501315108,12.1653487056253,29.3231721036627));
#74242=CARTESIAN_POINT('Ctrl Pts',(202.753300268863,12.1705424152397,29.3699018961518));
#74243=CARTESIAN_POINT('Ctrl Pts',(202.756472213298,12.1757413474348,29.4166786781985));
#74244=CARTESIAN_POINT('Ctrl Pts',(202.759644157734,12.1781295729463,29.4637452155598));
#74245=CARTESIAN_POINT('Ctrl Pts',(202.76281610217,12.1777010349264,29.510739405633));
#74246=CARTESIAN_POINT('Ctrl Pts',(202.76598999144,12.1772722341542,29.5577624095565));
#74247=CARTESIAN_POINT('Ctrl Pts',(202.76916388071,12.1740232716144,29.604712422341));
#74248=CARTESIAN_POINT('Ctrl Pts',(202.772337769981,12.1680000858249,29.6512311542408));
#74249=CARTESIAN_POINT('Ctrl Pts',(202.775517274459,12.1619662438848,29.6978321865436));
#74250=CARTESIAN_POINT('Ctrl Pts',(202.778696778938,12.1531484963889,29.7439998704635));
#74251=CARTESIAN_POINT('Ctrl Pts',(202.781876283416,12.1416437142876,29.7893867518176));
#74252=CARTESIAN_POINT('Ctrl Pts',(202.782608447654,12.1389944366799,29.7998382707944));
#74253=CARTESIAN_POINT('Ctrl Pts',(202.783340611892,12.1362028793193,29.8102484584892));
#74254=CARTESIAN_POINT('Ctrl Pts',(202.78407277613,12.1332705898496,29.8206132135175));
#74255=CARTESIAN_POINT('Ctrl Pts',(202.787349938577,12.1201456809315,29.8670057907543));
#74256=CARTESIAN_POINT('Ctrl Pts',(202.790627101024,12.1041377229001,29.9126957619106));
#74257=CARTESIAN_POINT('Ctrl Pts',(202.793904263472,12.0853436732396,29.9573009659499));
#74258=CARTESIAN_POINT('Ctrl Pts',(202.797078215803,12.067141518571,30.0005013851046));
#74259=CARTESIAN_POINT('Ctrl Pts',(202.800252168135,12.0463264053124,30.0426837975565));
#74260=CARTESIAN_POINT('Ctrl Pts',(202.803426120466,12.0230371985048,30.0835151694477));
#74261=CARTESIAN_POINT('Ctrl Pts',(202.806596947835,11.9997709214392,30.1243063401919));
#74262=CARTESIAN_POINT('Ctrl Pts',(202.809767775204,11.9740356470927,30.1637486217276));
#74263=CARTESIAN_POINT('Ctrl Pts',(202.812938602572,11.9460170171285,30.2015317995667));
#74264=CARTESIAN_POINT('Ctrl Pts',(202.816107699517,11.91801367784,30.2392943578993));
#74265=CARTESIAN_POINT('Ctrl Pts',(202.819276796462,11.8877297826949,30.2753991597121));
#74266=CARTESIAN_POINT('Ctrl Pts',(202.822445893408,11.8553938146777,30.3095656145806));
#74267=CARTESIAN_POINT('Ctrl Pts',(202.82561465147,11.8230613044563,30.3437284159128));
#74268=CARTESIAN_POINT('Ctrl Pts',(202.828783409533,11.7886775412368,30.3759528791974));
#74269=CARTESIAN_POINT('Ctrl Pts',(202.831952167596,11.752508908463,30.4059941529524));
#74270=CARTESIAN_POINT('Ctrl Pts',(202.835124112032,11.7163039059995,30.4360656349767));
#74271=CARTESIAN_POINT('Ctrl Pts',(202.838296056467,11.6783108832264,30.4639491925107));
#74272=CARTESIAN_POINT('Ctrl Pts',(202.841468000903,11.6388289112696,30.4894405917619));
#74273=CARTESIAN_POINT('Ctrl Pts',(202.844641890173,11.5993227314772,30.5149476207188));
#74274=CARTESIAN_POINT('Ctrl Pts',(202.847815779443,11.5583262709911,30.5380592992723));
#74275=CARTESIAN_POINT('Ctrl Pts',(202.850989668714,11.5161640169009,30.5586169137874));
#74276=CARTESIAN_POINT('Ctrl Pts',(202.854169173192,11.4739271698379,30.5792108985966));
#74277=CARTESIAN_POINT('Ctrl Pts',(202.857348677671,11.430520930021,30.597241596151));
#74278=CARTESIAN_POINT('Ctrl Pts',(202.860528182149,11.3862887509629,30.612598788144));
#74279=CARTESIAN_POINT('Ctrl Pts',(202.861260346387,11.3761031324462,30.6161351840996));
#74280=CARTESIAN_POINT('Ctrl Pts',(202.861992510626,11.3658737695475,30.6195300235928));
#74281=CARTESIAN_POINT('Ctrl Pts',(202.862724674864,11.3556049387415,30.6227823431292));
#74282=CARTESIAN_POINT('Ctrl Pts',(202.866001837311,11.309641717742,30.6373397045696));
#74283=CARTESIAN_POINT('Ctrl Pts',(202.869278999759,11.2626794349558,30.6491028750644));
#74284=CARTESIAN_POINT('Ctrl Pts',(202.872556162206,11.2150905762247,30.6579426179735));
#74285=CARTESIAN_POINT('Ctrl Pts',(202.875730114537,11.1690004688363,30.6665039642808));
#74286=CARTESIAN_POINT('Ctrl Pts',(202.878904066869,11.1223232641915,30.672323193331));
#74287=CARTESIAN_POINT('Ctrl Pts',(202.8820780192,11.075413471924,30.6753330892783));
#74288=CARTESIAN_POINT('Ctrl Pts',(202.885248846569,11.0285498654045,30.6783400217868));
#74289=CARTESIAN_POINT('Ctrl Pts',(202.888419673937,10.98145467782,30.6785430605955));
#74290=CARTESIAN_POINT('Ctrl Pts',(202.891590501306,10.9344890912761,30.6759266062719));
#74291=CARTESIAN_POINT('Ctrl Pts',(202.894759598251,10.887549135377,30.6733115798323));
#74292=CARTESIAN_POINT('Ctrl Pts',(202.897928695196,10.8407391954672,30.667880139443));
#74293=CARTESIAN_POINT('Ctrl Pts',(202.901097792141,10.7944192786983,30.659668758538));
#74294=CARTESIAN_POINT('Ctrl Pts',(202.904266550204,10.7481043150769,30.6514582557041));
#74295=CARTESIAN_POINT('Ctrl Pts',(202.907435308267,10.7022798181404,30.6404685019495));
#74296=CARTESIAN_POINT('Ctrl Pts',(202.91060406633,10.657296795633,30.6267872808195));
#74297=CARTESIAN_POINT('Ctrl Pts',(202.913776010765,10.6122685400483,30.6130923024162));
#74298=CARTESIAN_POINT('Ctrl Pts',(202.916947955201,10.5680839801183,30.5967006208692));
#74299=CARTESIAN_POINT('Ctrl Pts',(202.920119899636,10.5250781824901,30.5777496600571));
#74300=CARTESIAN_POINT('Ctrl Pts',(202.923293788907,10.4820460164404,30.5587870797203));
#74301=CARTESIAN_POINT('Ctrl Pts',(202.926467678177,10.4401945461271,30.5372623522999));
#74302=CARTESIAN_POINT('Ctrl Pts',(202.929641567447,10.3998348030737,30.5133591657939));
#74303=CARTESIAN_POINT('Ctrl Pts',(202.932821071926,10.3594036560292,30.4894136900465));
#74304=CARTESIAN_POINT('Ctrl Pts',(202.936000576404,10.3204699591061,30.4630816762004));
#74305=CARTESIAN_POINT('Ctrl Pts',(202.939180080882,10.2833146764623,30.4345893266701));
#74306=CARTESIAN_POINT('Ctrl Pts',(202.939912245121,10.2747586988218,30.4280282164279));
#74307=CARTESIAN_POINT('Ctrl Pts',(202.94064440936,10.266296877498,30.4213527104206));
#74308=CARTESIAN_POINT('Ctrl Pts',(202.941376573598,10.2579323694205,30.4145658500874));
#74309=CARTESIAN_POINT('Ctrl Pts',(202.944516392661,10.2220619450998,30.3854610231567));
#74310=CARTESIAN_POINT('Ctrl Pts',(202.947656211723,10.1878184127143,30.3541710319064));
#74311=CARTESIAN_POINT('Ctrl Pts',(202.950796030786,10.1554840821467,30.3209067711941));
#74312=CARTESIAN_POINT('Ctrl Pts',(202.952562438989,10.1372933438807,30.3021928702224));
#74313=CARTESIAN_POINT('Ctrl Pts',(202.954328847192,10.1197063743492,30.2828549158538));
#74314=CARTESIAN_POINT('Ctrl Pts',(202.956095255396,10.1027690874833,30.2629362700282));
#74315=CARTESIAN_POINT('Origin',(197.762132885264,11.,29.5));
#74316=CARTESIAN_POINT('',(203.553841401988,10.1027690875417,30.2629362700969));
#74317=CARTESIAN_POINT('',(203.45604596219,10.1027690874833,30.2629362700282));
#74318=CARTESIAN_POINT('',(197.762132885264,10.1027690874833,30.2629362700282));
#74319=CARTESIAN_POINT('',(203.111140857964,9.82225052377447,29.5010225701789));
#74320=CARTESIAN_POINT('Ctrl Pts',(203.553841401988,10.1027690875417,30.2629362700969));
#74321=CARTESIAN_POINT('Ctrl Pts',(203.553636636426,10.1048324583781,30.2653628424999));
#74322=CARTESIAN_POINT('Ctrl Pts',(203.553432306356,10.1069057386442,30.267781121179));
#74323=CARTESIAN_POINT('Ctrl Pts',(203.55059954678,10.13584324624,30.3012580633699));
#74324=CARTESIAN_POINT('Ctrl Pts',(203.548040546119,10.1643058974711,30.3309014308498));
#74325=CARTESIAN_POINT('Ctrl Pts',(203.540101214774,10.257669174366,30.4184760026797));
#74326=CARTESIAN_POINT('Ctrl Pts',(203.534766044947,10.3274611959891,30.4707435858822));
#74327=CARTESIAN_POINT('Ctrl Pts',(203.527971980805,10.4176818116929,30.5238732857151));
#74328=CARTESIAN_POINT('Ctrl Pts',(203.526807829198,10.4331989868856,30.5325442052846));
#74329=CARTESIAN_POINT('Ctrl Pts',(203.524948872563,10.4580209192621,30.5456864325651));
#74330=CARTESIAN_POINT('Ctrl Pts',(203.524262225733,10.4671987967357,30.550392453231));
#74331=CARTESIAN_POINT('Ctrl Pts',(203.522955832613,10.4846693017841,30.5590626964345));
#74332=CARTESIAN_POINT('Ctrl Pts',(203.522336990897,10.4929488755893,30.5630515851031));
#74333=CARTESIAN_POINT('Ctrl Pts',(203.520916426367,10.5119574595265,30.5719368514128));
#74334=CARTESIAN_POINT('Ctrl Pts',(203.520112631508,10.5227148846532,30.5767697228317));
#74335=CARTESIAN_POINT('Ctrl Pts',(203.517544095768,10.5570836449706,30.5915939907905));
#74336=CARTESIAN_POINT('Ctrl Pts',(203.515759663993,10.5809481313927,30.6009757928831));
#74337=CARTESIAN_POINT('Ctrl Pts',(203.511378082039,10.6394852467639,30.6218094422828));
#74338=CARTESIAN_POINT('Ctrl Pts',(203.508758939796,10.6744197841495,30.6324418009247));
#74339=CARTESIAN_POINT('Ctrl Pts',(203.502977007787,10.7516242361449,30.6520711223058));
#74340=CARTESIAN_POINT('Ctrl Pts',(203.499806159218,10.7940114884619,30.6603994551776));
#74341=CARTESIAN_POINT('Ctrl Pts',(203.492960851652,10.8865368697168,30.6733488831739));
#74342=CARTESIAN_POINT('Ctrl Pts',(203.489295674134,10.9367148356339,30.6771225000189));
#74343=CARTESIAN_POINT('Ctrl Pts',(203.484880907378,10.9993434717685,30.6778146708193));
#74344=CARTESIAN_POINT('Ctrl Pts',(203.484017430906,11.01170462077,30.6777567072013));
#74345=CARTESIAN_POINT('Ctrl Pts',(203.482731775176,11.0303103551321,30.6773764855621));
#74346=CARTESIAN_POINT('Ctrl Pts',(203.482302541188,11.0365566237423,30.6771991012756));
#74347=CARTESIAN_POINT('Ctrl Pts',(203.48152285457,11.0479712475656,30.6767840009988));
#74348=CARTESIAN_POINT('Ctrl Pts',(203.481171622502,11.0531396972671,30.6765619405509));
#74349=CARTESIAN_POINT('Ctrl Pts',(203.480359884649,11.0651442126838,30.6759669037407));
#74350=CARTESIAN_POINT('Ctrl Pts',(203.479900752068,11.0719787137758,30.6755683721173));
#74351=CARTESIAN_POINT('Ctrl Pts',(203.478402346832,11.0944138676409,30.6740637435272));
#74352=CARTESIAN_POINT('Ctrl Pts',(203.477375516184,11.1099966881769,30.6727064580783));
#74353=CARTESIAN_POINT('Ctrl Pts',(203.474864332617,11.1484745056807,30.668581198148));
#74354=CARTESIAN_POINT('Ctrl Pts',(203.473394427601,11.171324538913,30.6654504371996));
#74355=CARTESIAN_POINT('Ctrl Pts',(203.465942303451,11.2878575234329,30.6459820541884));
#74356=CARTESIAN_POINT('Ctrl Pts',(203.460206011005,11.3794025856853,30.6190136665376));
#74357=CARTESIAN_POINT('Ctrl Pts',(203.452249434493,11.4941904108065,30.5694702720876));
#74358=CARTESIAN_POINT('Ctrl Pts',(203.450319445721,11.5212054434442,30.5565677853047));
#74359=CARTESIAN_POINT('Ctrl Pts',(203.447599861438,11.5578902891465,30.5372974642034));
#74360=CARTESIAN_POINT('Ctrl Pts',(203.446839455317,11.568002993592,30.5317946443496));
#74361=CARTESIAN_POINT('Ctrl Pts',(203.445505825468,11.5854764090567,30.5219517696008));
#74362=CARTESIAN_POINT('Ctrl Pts',(203.444934948519,11.5928736848672,30.5176781575262));
#74363=CARTESIAN_POINT('Ctrl Pts',(203.443726955957,11.6083489010225,30.5085117055143));
#74364=CARTESIAN_POINT('Ctrl Pts',(203.443089249355,11.6164157580093,30.5036014397842));
#74365=CARTESIAN_POINT('Ctrl Pts',(203.441534193548,11.6358334500228,30.4914595344302));
#74366=CARTESIAN_POINT('Ctrl Pts',(203.440613334216,11.6471208353088,30.4841294545266));
#74367=CARTESIAN_POINT('Ctrl Pts',(203.437103110023,11.6893366263854,30.455674019676));
#74368=CARTESIAN_POINT('Ctrl Pts',(203.434467613505,11.7193740864881,30.4332728556166));
#74369=CARTESIAN_POINT('Ctrl Pts',(203.42688226914,11.8012436767198,30.3659132596763));
#74370=CARTESIAN_POINT('Ctrl Pts',(203.421835920595,11.8502866209029,30.3178070395446));
#74371=CARTESIAN_POINT('Ctrl Pts',(203.413178882355,11.9271919331121,30.2279306311516));
#74372=CARTESIAN_POINT('Ctrl Pts',(203.409566143736,11.9571003411006,30.1881335961857));
#74373=CARTESIAN_POINT('Ctrl Pts',(203.405397137579,11.9897842094336,30.1383715841497));
#74374=CARTESIAN_POINT('Ctrl Pts',(203.404716303748,11.9950608584083,30.1301150405122));
#74375=CARTESIAN_POINT('Ctrl Pts',(203.403647752854,12.0032541186534,30.1169351329356));
#74376=CARTESIAN_POINT('Ctrl Pts',(203.403255992826,12.0062388214089,30.1120549179457));
#74377=CARTESIAN_POINT('Ctrl Pts',(203.402504458088,12.0119295212609,30.1025960412482));
#74378=CARTESIAN_POINT('Ctrl Pts',(203.402144417686,12.0146402345381,30.0980205185362));
#74379=CARTESIAN_POINT('Ctrl Pts',(203.401255858066,12.021288573188,30.0866231765656));
#74380=CARTESIAN_POINT('Ctrl Pts',(203.400729611035,12.025189023181,30.0797797651401));
#74381=CARTESIAN_POINT('Ctrl Pts',(203.398690151874,12.0401442069583,30.0529177301412));
#74382=CARTESIAN_POINT('Ctrl Pts',(203.397205025935,12.0506843521603,30.0326166886945));
#74383=CARTESIAN_POINT('Ctrl Pts',(203.393116409464,12.0784494872939,29.9751024204265));
#74384=CARTESIAN_POINT('Ctrl Pts',(203.39056161515,12.0943331256441,29.9372768651497));
#74385=CARTESIAN_POINT('Ctrl Pts',(203.382618604363,12.1376858578538,29.8167744589788));
#74386=CARTESIAN_POINT('Ctrl Pts',(203.377276129873,12.1579817250588,29.731844394941));
#74387=CARTESIAN_POINT('Ctrl Pts',(203.37047461223,12.1709266666097,29.6278327676274));
#74388=CARTESIAN_POINT('Ctrl Pts',(203.369311362076,12.1727210608599,29.6101623133969));
#74389=CARTESIAN_POINT('Ctrl Pts',(203.367453509063,12.1749246345349,29.5821795748549));
#74390=CARTESIAN_POINT('Ctrl Pts',(203.366767047409,12.1755990500046,29.5718904847246));
#74391=CARTESIAN_POINT('Ctrl Pts',(203.365460800093,12.1766189296353,29.552415910573));
#74392=CARTESIAN_POINT('Ctrl Pts',(203.364841916287,12.1769921268865,29.5432326075625));
#74393=CARTESIAN_POINT('Ctrl Pts',(203.363420960911,12.1775988502407,29.5222531143959));
#74394=CARTESIAN_POINT('Ctrl Pts',(203.362616813096,12.1777626698849,29.5104560605453));
#74395=CARTESIAN_POINT('Ctrl Pts',(203.360045845327,12.1777200091808,29.4729916996093));
#74396=CARTESIAN_POINT('Ctrl Pts',(203.358259281262,12.1768517339911,29.4473341596087));
#74397=CARTESIAN_POINT('Ctrl Pts',(203.353871047536,12.1727162341265,29.3852460691279));
#74398=CARTESIAN_POINT('Ctrl Pts',(203.35124729432,12.1685891161939,29.3489010139919));
#74399=CARTESIAN_POINT('Ctrl Pts',(203.345465724963,12.1559294554885,29.2702625248178));
#74400=CARTESIAN_POINT('Ctrl Pts',(203.34230011101,12.1467501375995,29.2281248277924));
#74401=CARTESIAN_POINT('Ctrl Pts',(203.335462429083,12.1219155940489,29.1381662317735));
#74402=CARTESIAN_POINT('Ctrl Pts',(203.331799656383,12.1054630618378,29.0906461159768));
#74403=CARTESIAN_POINT('Ctrl Pts',(203.327387251835,12.0812429095858,29.0329223127718));
#74404=CARTESIAN_POINT('Ctrl Pts',(203.32652387479,12.0762819787965,29.0216017065007));
#74405=CARTESIAN_POINT('Ctrl Pts',(203.325238336129,12.0685458854959,29.0046780909974));
#74406=CARTESIAN_POINT('Ctrl Pts',(203.324809121602,12.0659029818614,28.9990160275945));
#74407=CARTESIAN_POINT('Ctrl Pts',(203.324029452841,12.0609896902548,28.9887048767647));
#74408=CARTESIAN_POINT('Ctrl Pts',(203.323678219427,12.0587336289821,28.9840494883115));
#74409=CARTESIAN_POINT('Ctrl Pts',(203.322866456162,12.0534206842414,28.9732678155437));
#74410=CARTESIAN_POINT('Ctrl Pts',(203.322407299839,12.0503409623433,28.9671531171396));
#74411=CARTESIAN_POINT('Ctrl Pts',(203.320908728761,12.0400504899214,28.9471576188553));
#74412=CARTESIAN_POINT('Ctrl Pts',(203.319881759805,12.0326162117128,28.9333929622172));
#74413=CARTESIAN_POINT('Ctrl Pts',(203.317370155283,12.0135481399249,28.8997108435776));
#74414=CARTESIAN_POINT('Ctrl Pts',(203.31589997391,12.0015990869346,28.8799787938515));
#74415=CARTESIAN_POINT('Ctrl Pts',(203.308443865967,11.9374227544632,28.7807040093803));
#74416=CARTESIAN_POINT('Ctrl Pts',(203.302704103762,11.8762761801676,28.7073529890055));
#74417=CARTESIAN_POINT('Ctrl Pts',(203.294746800868,11.7852095666352,28.6216871657776));
#74418=CARTESIAN_POINT('Ctrl Pts',(203.292820309845,11.7626809659901,28.6020551142903));
#74419=CARTESIAN_POINT('Ctrl Pts',(203.290104610918,11.730474164568,28.5760762995567));
#74420=CARTESIAN_POINT('Ctrl Pts',(203.28934446815,11.7214113556898,28.5689827337202));
#74421=CARTESIAN_POINT('Ctrl Pts',(203.288011163924,11.70544331556,28.5568575096024));
#74422=CARTESIAN_POINT('Ctrl Pts',(203.287440346225,11.6985844840604,28.551765988347));
#74423=CARTESIAN_POINT('Ctrl Pts',(203.286232341902,11.6840266682557,28.541202950828));
#74424=CARTESIAN_POINT('Ctrl Pts',(203.285594562917,11.6763160657195,28.5357485624812));
#74425=CARTESIAN_POINT('Ctrl Pts',(203.284039054702,11.6574566101502,28.5227451009566));
#74426=CARTESIAN_POINT('Ctrl Pts',(203.283117810409,11.6462425140864,28.5152934858205));
#74427=CARTESIAN_POINT('Ctrl Pts',(203.279603900548,11.6033185058647,28.4878201052407));
#74428=CARTESIAN_POINT('Ctrl Pts',(203.276964975755,11.570789227894,28.4691263427009));
#74429=CARTESIAN_POINT('Ctrl Pts',(203.269363205353,11.4762523855355,28.4206459399401));
#74430=CARTESIAN_POINT('Ctrl Pts',(203.264303288652,11.4124527858537,28.3946933889983));
#74431=CARTESIAN_POINT('Ctrl Pts',(203.255650874701,11.2994601710618,28.3598822669803));
#74432=CARTESIAN_POINT('Ctrl Pts',(203.252055591277,11.2512821311311,28.3483042309437));
#74433=CARTESIAN_POINT('Ctrl Pts',(203.24790306089,11.192864578211,28.338107463902));
#74434=CARTESIAN_POINT('Ctrl Pts',(203.247222407506,11.1831941114399,28.3365435358324));
#74435=CARTESIAN_POINT('Ctrl Pts',(203.246154073071,11.1678474828549,28.3342577467001));
#74436=CARTESIAN_POINT('Ctrl Pts',(203.245762351698,11.1621838764581,28.3334563135946));
#74437=CARTESIAN_POINT('Ctrl Pts',(203.24501083687,11.1512432709921,28.3319893746366));
#74438=CARTESIAN_POINT('Ctrl Pts',(203.244650778316,11.1459672783901,28.3313183055983));
#74439=CARTESIAN_POINT('Ctrl Pts',(203.243762097893,11.1328652368477,28.3297419283086));
#74440=CARTESIAN_POINT('Ctrl Pts',(203.243235749618,11.1250341290514,28.3288793399453));
#74441=CARTESIAN_POINT('Ctrl Pts',(203.2411953387,11.0944277162182,28.3258185881347));
#74442=CARTESIAN_POINT('Ctrl Pts',(203.239709395691,11.0715974789532,28.3242055706098));
#74443=CARTESIAN_POINT('Ctrl Pts',(203.235617558168,11.0077351314567,28.3215608008853));
#74444=CARTESIAN_POINT('Ctrl Pts',(203.233060451799,10.9666736567975,28.3220065475302));
#74445=CARTESIAN_POINT('Ctrl Pts',(203.225119466313,10.8388956570369,28.3300818467023));
#74446=CARTESIAN_POINT('Ctrl Pts',(203.21978100919,10.752958694087,28.3451701345876));
#74447=CARTESIAN_POINT('Ctrl Pts',(203.212983590418,10.6524160561556,28.3745684588741));
#74448=CARTESIAN_POINT('Ctrl Pts',(203.211819843834,10.6354782552229,28.379939914059));
#74449=CARTESIAN_POINT('Ctrl Pts',(203.209961383137,10.6089120299119,28.3890312281864));
#74450=CARTESIAN_POINT('Ctrl Pts',(203.209274819587,10.5991994816548,28.392498150978));
#74451=CARTESIAN_POINT('Ctrl Pts',(203.207968492222,10.5809196819271,28.3992951281812));
#74452=CARTESIAN_POINT('Ctrl Pts',(203.207349631759,10.5723434035504,28.4025988175659));
#74453=CARTESIAN_POINT('Ctrl Pts',(203.205928892179,10.5528505094967,28.4103709250597));
#74454=CARTESIAN_POINT('Ctrl Pts',(203.205124939132,10.5419607497753,28.4149035915338));
#74455=CARTESIAN_POINT('Ctrl Pts',(203.202555313135,10.5076106808615,28.4298103988605));
#74456=CARTESIAN_POINT('Ctrl Pts',(203.200769925438,10.484421693482,28.4407871505742));
#74457=CARTESIAN_POINT('Ctrl Pts',(203.196385362001,10.4291232886598,28.4692094700497));
#74458=CARTESIAN_POINT('Ctrl Pts',(203.193764153209,10.3974327053614,28.4874084791047));
#74459=CARTESIAN_POINT('Ctrl Pts',(203.18798329268,10.3302856508829,28.5302385699635));
#74460=CARTESIAN_POINT('Ctrl Pts',(203.184815721449,10.2952321636467,28.5554066429871));
#74461=CARTESIAN_POINT('Ctrl Pts',(203.177973873752,10.2224817316164,28.6139488910721));
#74462=CARTESIAN_POINT('Ctrl Pts',(203.17430888967,10.185377989793,28.6479359682478));
#74463=CARTESIAN_POINT('Ctrl Pts',(203.169894313044,10.1419954182802,28.6931072160547));
#74464=CARTESIAN_POINT('Ctrl Pts',(203.169030844627,10.1335744349118,28.7021562829259));
#74465=CARTESIAN_POINT('Ctrl Pts',(203.1677451985,10.121112863154,28.7159773557035));
#74466=CARTESIAN_POINT('Ctrl Pts',(203.167315966204,10.1169655329529,28.7206513998919));
#74467=CARTESIAN_POINT('Ctrl Pts',(203.166536281233,10.1094528436882,28.7292551732299));
#74468=CARTESIAN_POINT('Ctrl Pts',(203.166185049144,10.1060760096403,28.7331742526192));
#74469=CARTESIAN_POINT('Ctrl Pts',(203.165373309486,10.0982905533223,28.7423312060794));
#74470=CARTESIAN_POINT('Ctrl Pts',(203.164914175149,10.0939016286838,28.7475854369919));
#74471=CARTESIAN_POINT('Ctrl Pts',(203.164448903624,10.0894724894911,28.752982775601));
#74472=CARTESIAN_POINT('Ctrl Pts',(203.164439855082,10.0893863593136,28.7530877706596));
#74473=CARTESIAN_POINT('Ctrl Pts',(203.163392505071,10.0794178020576,28.7652440037462));
#74474=CARTESIAN_POINT('Ctrl Pts',(203.162369421707,10.0697749725908,28.7774908921946));
#74475=CARTESIAN_POINT('Ctrl Pts',(203.159304242824,10.0412927769419,28.8151806545838));
#74476=CARTESIAN_POINT('Ctrl Pts',(203.157300038872,10.0232324749491,28.8411961071008));
#74477=CARTESIAN_POINT('Ctrl Pts',(203.149760445824,9.95861039114315,28.9427935158048));
#74478=CARTESIAN_POINT('Ctrl Pts',(203.144377351342,9.91959760795539,29.0228185425296));
#74479=CARTESIAN_POINT('Ctrl Pts',(203.136921817303,9.88053724125063,29.1329978671223));
#74480=CARTESIAN_POINT('Ctrl Pts',(203.135103511391,9.87208632508038,29.1598559353139));
#74481=CARTESIAN_POINT('Ctrl Pts',(203.132512680251,9.86160149975831,29.1978878992864));
#74482=CARTESIAN_POINT('Ctrl Pts',(203.131765577045,9.85875411881394,29.2088287598886));
#74483=CARTESIAN_POINT('Ctrl Pts',(203.130391855611,9.85384163159301,29.2288849342393));
#74484=CARTESIAN_POINT('Ctrl Pts',(203.129766856375,9.85172666596165,29.23798716397));
#74485=CARTESIAN_POINT('Ctrl Pts',(203.128488574466,9.84764550124394,29.2565507440171));
#74486=CARTESIAN_POINT('Ctrl Pts',(203.127835103543,9.84568699177589,29.2660130333497));
#74487=CARTESIAN_POINT('Ctrl Pts',(203.126513125027,9.84198180605738,29.2850942464111));
#74488=CARTESIAN_POINT('Ctrl Pts',(203.125844583352,9.84023802567225,29.2947129487094));
#74489=CARTESIAN_POINT('Ctrl Pts',(203.124213212264,9.8362974465002,29.3181046142437));
#74490=CARTESIAN_POINT('Ctrl Pts',(203.123246670765,9.83422521864639,29.3318967718816));
#74491=CARTESIAN_POINT('Ctrl Pts',(203.118646184257,9.82559445279263,29.3972158368744));
#74492=CARTESIAN_POINT('Ctrl Pts',(203.114921238938,9.82220532788681,29.4490958683268));
#74493=CARTESIAN_POINT('Ctrl Pts',(203.111140945057,9.82225044453215,29.5010232767361));
#74494=CARTESIAN_POINT('Ctrl Pts',(203.111140995759,9.82225044392725,29.5010225802788));
#74495=CARTESIAN_POINT('Ctrl Pts',(203.105006122021,9.82232361193448,29.5852933117094));
#74496=CARTESIAN_POINT('Ctrl Pts',(203.098739959637,9.83144089566503,29.6693162629537));
#74497=CARTESIAN_POINT('Ctrl Pts',(203.092040144829,9.85165111638797,29.7617175719854));
#74498=CARTESIAN_POINT('Ctrl Pts',(203.091315249602,9.85398500002695,29.7717551871937));
#74499=CARTESIAN_POINT('Ctrl Pts',(203.089999077818,9.85849885695753,29.7900750212459));
#74500=CARTESIAN_POINT('Ctrl Pts',(203.089405973835,9.86063798134824,29.7983665172388));
#74501=CARTESIAN_POINT('Ctrl Pts',(203.088442892122,9.86428759874874,29.8119008793343));
#74502=CARTESIAN_POINT('Ctrl Pts',(203.088070079566,9.86574439045436,29.8171577408209));
#74503=CARTESIAN_POINT('Ctrl Pts',(203.087324016489,9.86874974884729,29.8277170143305));
#74504=CARTESIAN_POINT('Ctrl Pts',(203.086950823131,9.87029919496497,29.8330190181278));
#74505=CARTESIAN_POINT('Ctrl Pts',(203.085982673637,9.87443783667621,29.8468195535655));
#74506=CARTESIAN_POINT('Ctrl Pts',(203.08539094096,9.87708604300266,29.8553002153843));
#74507=CARTESIAN_POINT('Ctrl Pts',(203.082791863014,9.88923285766064,29.8927063498549));
#74508=CARTESIAN_POINT('Ctrl Pts',(203.080834768041,9.89975574636381,29.921289493624));
#74509=CARTESIAN_POINT('Ctrl Pts',(203.07444233653,9.93828889423108,30.014624729076));
#74510=CARTESIAN_POINT('Ctrl Pts',(203.070141600923,9.97100438833895,30.077267771998));
#74511=CARTESIAN_POINT('Ctrl Pts',(203.063517996035,10.0284167532611,30.1666289928229));
#74512=CARTESIAN_POINT('Ctrl Pts',(203.061273057511,10.0490566481164,30.1957547666944));
#74513=CARTESIAN_POINT('Ctrl Pts',(203.057910865136,10.0813012417469,30.2371358911483));
#74514=CARTESIAN_POINT('Ctrl Pts',(203.056826574791,10.0918981353055,30.250151775798));
#74515=CARTESIAN_POINT('Ctrl Pts',(203.055732095072,10.1027690874946,30.2629362700414));
#74516=CARTESIAN_POINT('',(203.012132885223,9.82225017240322,29.4993627435653));
#74517=CARTESIAN_POINT('Ctrl Pts',(202.956095255396,10.1027690874833,30.2629362700282));
#74518=CARTESIAN_POINT('Ctrl Pts',(202.959228378578,10.0727269907474,30.2276060610354));
#74519=CARTESIAN_POINT('Ctrl Pts',(202.96236150176,10.0447311384701,30.19044701957));
#74520=CARTESIAN_POINT('Ctrl Pts',(202.965494624942,10.0190091789132,30.1517300602576));
#74521=CARTESIAN_POINT('Ctrl Pts',(202.96862550212,9.9933056583499,30.1130408555089));
#74522=CARTESIAN_POINT('Ctrl Pts',(202.971756379298,9.96987312057105,30.0727964182464));
#74523=CARTESIAN_POINT('Ctrl Pts',(202.974887256475,9.94889727092247,30.0312985181852));
#74524=CARTESIAN_POINT('Ctrl Pts',(202.978019397072,9.92791295678256,29.9897838722652));
#74525=CARTESIAN_POINT('Ctrl Pts',(202.981151537668,9.90938758623201,29.9470152558707));
#74526=CARTESIAN_POINT('Ctrl Pts',(202.984283678265,9.89346090484598,29.9033190962448));
#74527=CARTESIAN_POINT('Ctrl Pts',(202.9874161995,9.87753228794224,29.8596176263669));
#74528=CARTESIAN_POINT('Ctrl Pts',(202.990548720735,9.86420316801225,29.8149889334246));
#74529=CARTESIAN_POINT('Ctrl Pts',(202.993681241971,9.85356378597987,29.7697759620188));
#74530=CARTESIAN_POINT('Ctrl Pts',(202.99681923689,9.84290581297378,29.7244839866672));
#74531=CARTESIAN_POINT('Ctrl Pts',(202.99995723181,9.83494707659015,29.6786062571383));
#74532=CARTESIAN_POINT('Ctrl Pts',(203.00309522673,9.82972653664071,29.632495597878));
#74533=CARTESIAN_POINT('Ctrl Pts',(203.006107779561,9.82471468900977,29.5882282231212));
#74534=CARTESIAN_POINT('Ctrl Pts',(203.009120332392,9.82222615716822,29.5437466639892));
#74535=CARTESIAN_POINT('Ctrl Pts',(203.012132885223,9.82225017240322,29.4993627435653));
#74536=CARTESIAN_POINT('Ctrl Pts',(203.012132885264,9.82225017240355,29.4993627429623));
#74537=CARTESIAN_POINT('Ctrl Pts',(203.01476474762,9.82227115289961,29.4605875327235));
#74538=CARTESIAN_POINT('Ctrl Pts',(203.017396609976,9.82420692233509,29.4218659833471));
#74539=CARTESIAN_POINT('Ctrl Pts',(203.020028472332,9.82804235792228,29.3833366052456));
#74540=CARTESIAN_POINT('Ctrl Pts',(203.02330563478,9.83281819486747,29.3353603002785));
#74541=CARTESIAN_POINT('Ctrl Pts',(203.026582797227,9.8405556551505,29.2875695073051));
#74542=CARTESIAN_POINT('Ctrl Pts',(203.029859959674,9.85122638381556,29.2403574740946));
#74543=CARTESIAN_POINT('Ctrl Pts',(203.033033912005,9.86156105128063,29.1946323245856));
#74544=CARTESIAN_POINT('Ctrl Pts',(203.036207864336,9.87464682220411,29.1494506086035));
#74545=CARTESIAN_POINT('Ctrl Pts',(203.039381816667,9.89040545971779,29.1051645676033));
#74546=CARTESIAN_POINT('Ctrl Pts',(203.042552644036,9.90614858182573,29.0609221290969));
#74547=CARTESIAN_POINT('Ctrl Pts',(203.045723471404,9.92455917570205,29.0175741423954));
#74548=CARTESIAN_POINT('Ctrl Pts',(203.048894298772,9.94550894802642,28.9754585966698));
#74549=CARTESIAN_POINT('Ctrl Pts',(203.052063395717,9.96644728738013,28.9333660347643));
#74550=CARTESIAN_POINT('Ctrl Pts',(203.055232492661,9.98992181238473,28.8925050791412));
#74551=CARTESIAN_POINT('Ctrl Pts',(203.058401589606,10.0157568527323,28.8531920767673));
#74552=CARTESIAN_POINT('Ctrl Pts',(203.061570347669,10.0415891304504,28.8138832782676));
#74553=CARTESIAN_POINT('Ctrl Pts',(203.064739105731,10.0697811148109,28.7761225682047));
#74554=CARTESIAN_POINT('Ctrl Pts',(203.067907863793,10.1001135490356,28.7401977639736));
#74555=CARTESIAN_POINT('Ctrl Pts',(203.071079808229,10.130476484309,28.7042368352366));
#74556=CARTESIAN_POINT('Ctrl Pts',(203.074251752664,10.1629838025832,28.6701159205608));
#74557=CARTESIAN_POINT('Ctrl Pts',(203.077423697099,10.197376935849,28.6380885895912));
#74558=CARTESIAN_POINT('Ctrl Pts',(203.080597586369,10.2317911567981,28.606041621498));
#74559=CARTESIAN_POINT('Ctrl Pts',(203.083771475639,10.2680930640106,28.5760911458728));
#74560=CARTESIAN_POINT('Ctrl Pts',(203.086945364909,10.3059910762788,28.5484503815905));
#74561=CARTESIAN_POINT('Ctrl Pts',(203.090124869387,10.3439561372725,28.5207607155872));
#74562=CARTESIAN_POINT('Ctrl Pts',(203.093304373865,10.3835224658961,28.4953892089696));
#74563=CARTESIAN_POINT('Ctrl Pts',(203.096483878343,10.4243712947476,28.4725046685316));
#74564=CARTESIAN_POINT('Ctrl Pts',(203.097216042584,10.4337778082397,28.4672349032912));
#74565=CARTESIAN_POINT('Ctrl Pts',(203.097948206825,10.4432522398561,28.4620968154283));
#74566=CARTESIAN_POINT('Ctrl Pts',(203.098680371066,10.4527905487114,28.4570921042967));
#74567=CARTESIAN_POINT('Ctrl Pts',(203.101957533513,10.495483957977,28.4346910493673));
#74568=CARTESIAN_POINT('Ctrl Pts',(203.105234695961,10.5396514897336,28.414865376036));
#74569=CARTESIAN_POINT('Ctrl Pts',(203.108511858408,10.5849491342878,28.3978077112538));
#74570=CARTESIAN_POINT('Ctrl Pts',(203.111685810739,10.6288201864082,28.3812872562042));
#74571=CARTESIAN_POINT('Ctrl Pts',(203.11485976307,10.6737506530024,28.3673632470349));
#74572=CARTESIAN_POINT('Ctrl Pts',(203.118033715402,10.7194033322925,28.3561640971838));
#74573=CARTESIAN_POINT('Ctrl Pts',(203.12120454277,10.7650110635441,28.3449759736256));
#74574=CARTESIAN_POINT('Ctrl Pts',(203.124375370138,10.8113390615666,28.3365075311969));
#74575=CARTESIAN_POINT('Ctrl Pts',(203.127546197506,10.8580344934006,28.330837540187));
#74576=CARTESIAN_POINT('Ctrl Pts',(203.130715294451,10.9047044420218,28.3251706434753));
#74577=CARTESIAN_POINT('Ctrl Pts',(203.133884391396,10.9517408753356,28.3222992396827));
#74578=CARTESIAN_POINT('Ctrl Pts',(203.137053488341,10.9987829745916,28.3222506288055));
#74579=CARTESIAN_POINT('Ctrl Pts',(203.140222246404,11.0458200434745,28.3222020231264));
#74580=CARTESIAN_POINT('Ctrl Pts',(203.143391004466,11.0928622205722,28.3249756093529));
#74581=CARTESIAN_POINT('Ctrl Pts',(203.146559762528,11.1395485381747,28.330546594347));
#74582=CARTESIAN_POINT('Ctrl Pts',(203.149731706964,11.186281801618,28.3361231812945));
#74583=CARTESIAN_POINT('Ctrl Pts',(203.152903651399,11.2326579380935,28.3445027114324));
#74584=CARTESIAN_POINT('Ctrl Pts',(203.156075595834,11.2783229579594,28.3556087235684));
#74585=CARTESIAN_POINT('Ctrl Pts',(203.159249485104,11.3240159767128,28.3667215452051));
#74586=CARTESIAN_POINT('Ctrl Pts',(203.162423374374,11.368996478961,28.3805640115672));
#74587=CARTESIAN_POINT('Ctrl Pts',(203.165597263644,11.412926014196,28.3970098961005));
#74588=CARTESIAN_POINT('Ctrl Pts',(203.168776768122,11.4569332690573,28.4134848765027));
#74589=CARTESIAN_POINT('Ctrl Pts',(203.1719562726,11.4998853413804,28.4325722333654));
#74590=CARTESIAN_POINT('Ctrl Pts',(203.175135777078,11.5414659166732,28.4540986071425));
#74591=CARTESIAN_POINT('Ctrl Pts',(203.175867941319,11.5510409339599,28.4590556189102));
#74592=CARTESIAN_POINT('Ctrl Pts',(203.17660010556,11.560543342083,28.46414178064));
#74593=CARTESIAN_POINT('Ctrl Pts',(203.177332269801,11.5699694991614,28.4693546524018));
#74594=CARTESIAN_POINT('Ctrl Pts',(203.180609432248,11.6121609178042,28.4926874329833));
#74595=CARTESIAN_POINT('Ctrl Pts',(203.183886594695,11.6530124034109,28.5186678931059));
#74596=CARTESIAN_POINT('Ctrl Pts',(203.187163757143,11.692173863972,28.5471146949742));
#74597=CARTESIAN_POINT('Ctrl Pts',(203.190337709477,11.730101983546,28.5746656005661));
#74598=CARTESIAN_POINT('Ctrl Pts',(203.193511661811,11.766444467378,28.6045294371039));
#74599=CARTESIAN_POINT('Ctrl Pts',(203.196685614146,11.8009085947955,28.636495231465));
#74600=CARTESIAN_POINT('Ctrl Pts',(203.199856441517,11.8353387900332,28.668429553418));
#74601=CARTESIAN_POINT('Ctrl Pts',(203.203027268888,11.8678938829555,28.7024613598172));
#74602=CARTESIAN_POINT('Ctrl Pts',(203.20619809626,11.8983140133927,28.738339317122));
#74603=CARTESIAN_POINT('Ctrl Pts',(203.209367193208,11.9287175425775,28.774197694661));
#74604=CARTESIAN_POINT('Ctrl Pts',(203.212536290156,11.9569880579436,28.8118998031371));
#74605=CARTESIAN_POINT('Ctrl Pts',(203.215705387104,11.9829042910962,28.8511593284598));
#74606=CARTESIAN_POINT('Ctrl Pts',(203.218874145169,12.008817752937,28.8904146556267));
#74607=CARTESIAN_POINT('Ctrl Pts',(203.222042903235,12.0323771277062,28.9312266032784));
#74608=CARTESIAN_POINT('Ctrl Pts',(203.2252116613,12.0534045696077,28.9732800789512));
#74609=CARTESIAN_POINT('Ctrl Pts',(203.228383605738,12.0744531558397,29.0153758418691));
#74610=CARTESIAN_POINT('Ctrl Pts',(203.231555550177,12.0929644817139,29.0587151240289));
#74611=CARTESIAN_POINT('Ctrl Pts',(203.234727494615,12.1088076892772,29.1029602404045));
#74612=CARTESIAN_POINT('Ctrl Pts',(203.237901383888,12.1246606108883,29.1472324850727));
#74613=CARTESIAN_POINT('Ctrl Pts',(203.241075273161,12.1378420028837,29.1924111345289));
#74614=CARTESIAN_POINT('Ctrl Pts',(203.244249162434,12.148271115196,29.2381441073672));
#74615=CARTESIAN_POINT('Ctrl Pts',(203.247428666915,12.1587186785731,29.2839579904519));
#74616=CARTESIAN_POINT('Ctrl Pts',(203.250608171396,12.1664041621707,29.3303276039395));
#74617=CARTESIAN_POINT('Ctrl Pts',(203.253787675877,12.1712983540684,29.3768934272404));
#74618=CARTESIAN_POINT('Ctrl Pts',(203.254519840097,12.1724253699953,29.3876164282187));
#74619=CARTESIAN_POINT('Ctrl Pts',(203.255252004316,12.1734045900643,29.3983498304063));
#74620=CARTESIAN_POINT('Ctrl Pts',(203.255984168535,12.1742360487072,29.4090892502693));
#74621=CARTESIAN_POINT('Ctrl Pts',(203.259261330982,12.1779576523707,29.4571588261297));
#74622=CARTESIAN_POINT('Ctrl Pts',(203.26253849343,12.1787310658024,29.5055657472966));
#74623=CARTESIAN_POINT('Ctrl Pts',(203.265815655877,12.1765151605395,29.5539178961072));
#74624=CARTESIAN_POINT('Ctrl Pts',(203.268989608204,12.1743690424332,29.6007472546453));
#74625=CARTESIAN_POINT('Ctrl Pts',(203.272163560531,12.169419143217,29.6475246354218));
#74626=CARTESIAN_POINT('Ctrl Pts',(203.275337512858,12.1616806410386,29.6938895323014));
#74627=CARTESIAN_POINT('Ctrl Pts',(203.278508340222,12.15394975792,29.7402087799183));
#74628=CARTESIAN_POINT('Ctrl Pts',(203.281679167586,12.1434357976166,29.7861158006402));
#74629=CARTESIAN_POINT('Ctrl Pts',(203.28484999495,12.1302057194786,29.8312553307614));
#74630=CARTESIAN_POINT('Ctrl Pts',(203.28801909189,12.1169828614235,29.8763702267764));
#74631=CARTESIAN_POINT('Ctrl Pts',(203.291188188831,12.1010469783912,29.9207179284697));
#74632=CARTESIAN_POINT('Ctrl Pts',(203.294357285772,12.0825154705478,29.9639561601323));
#74633=CARTESIAN_POINT('Ctrl Pts',(203.29752604383,12.0639859443418,30.0071897681831));
#74634=CARTESIAN_POINT('Ctrl Pts',(203.300694801888,12.0428615657284,30.0493136311309));
#74635=CARTESIAN_POINT('Ctrl Pts',(203.303863559947,12.0193076532744,30.0900059071537));
#74636=CARTESIAN_POINT('Ctrl Pts',(203.307035504378,11.9957300559739,30.130739101657));
#74637=CARTESIAN_POINT('Ctrl Pts',(203.310207448809,11.9697183315038,30.1700373553653));
#74638=CARTESIAN_POINT('Ctrl Pts',(203.31337939324,11.9414825119482,30.2076056403081));
#74639=CARTESIAN_POINT('Ctrl Pts',(203.316553282506,11.9132293799822,30.2451969597358));
#74640=CARTESIAN_POINT('Ctrl Pts',(203.319727171772,11.8827498000311,30.2810557753601));
#74641=CARTESIAN_POINT('Ctrl Pts',(203.322901061038,11.850293389007,30.3149209870356));
#74642=CARTESIAN_POINT('Ctrl Pts',(203.326080565512,11.8177795564741,30.3488461126536));
#74643=CARTESIAN_POINT('Ctrl Pts',(203.329260069987,11.7832823272527,30.3807702239048));
#74644=CARTESIAN_POINT('Ctrl Pts',(203.332439574461,11.7470858796401,30.410471169748));
#74645=CARTESIAN_POINT('Ctrl Pts',(203.33317173873,11.7387506985348,30.417310591264));
#74646=CARTESIAN_POINT('Ctrl Pts',(203.333903903,11.730325535536,30.4240323052374));
#74647=CARTESIAN_POINT('Ctrl Pts',(203.334636067269,11.7218140704041,30.4306339292475));
#74648=CARTESIAN_POINT('Ctrl Pts',(203.337913229716,11.6837168085328,30.4601827548366));
#74649=CARTESIAN_POINT('Ctrl Pts',(203.341190392164,11.6437161593219,30.4874550163208));
#74650=CARTESIAN_POINT('Ctrl Pts',(203.344467554611,11.6021169691323,30.5122006806868));
#74651=CARTESIAN_POINT('Ctrl Pts',(203.347641506941,11.5618278932114,30.536167011421));
#74652=CARTESIAN_POINT('Ctrl Pts',(203.350815459271,11.5200399979202,30.5577632301916));
#74653=CARTESIAN_POINT('Ctrl Pts',(203.353989411602,11.4770627014955,30.5768037153269));
#74654=CARTESIAN_POINT('Ctrl Pts',(203.357160238969,11.434127719021,30.5958254538633));
#74655=CARTESIAN_POINT('Ctrl Pts',(203.360331066337,11.390006160252,30.612296214871));
#74656=CARTESIAN_POINT('Ctrl Pts',(203.363501893704,11.345031547709,30.6260765043218));
#74657=CARTESIAN_POINT('Ctrl Pts',(203.366670990648,11.3000814792725,30.6398492734212));
#74658=CARTESIAN_POINT('Ctrl Pts',(203.369840087592,11.2542798108653,30.6509343168706));
#74659=CARTESIAN_POINT('Ctrl Pts',(203.373009184536,11.2079769634536,30.659241409359));
#74660=CARTESIAN_POINT('Ctrl Pts',(203.376177942597,11.161679067365,30.6675476135414));
#74661=CARTESIAN_POINT('Ctrl Pts',(203.379346700658,11.1148806468559,30.6730763605161));
#74662=CARTESIAN_POINT('Ctrl Pts',(203.38251545872,11.0679414155913,30.6757886827774));
#74663=CARTESIAN_POINT('Ctrl Pts',(203.385687403154,11.020954984167,30.6785037324384));
#74664=CARTESIAN_POINT('Ctrl Pts',(203.388859347588,10.9738280163311,30.6783966765544));
#74665=CARTESIAN_POINT('Ctrl Pts',(203.392031292022,10.9269224274933,30.6754806382483));
#74666=CARTESIAN_POINT('Ctrl Pts',(203.395205181291,10.8799880791304,30.6725628120128));
#74667=CARTESIAN_POINT('Ctrl Pts',(203.39837907056,10.8332759326326,30.666832643974));
#74668=CARTESIAN_POINT('Ctrl Pts',(203.401552959829,10.7871413430124,30.6583549778222));
#74669=CARTESIAN_POINT('Ctrl Pts',(203.404732464306,10.7409251326099,30.6498623130815));
#74670=CARTESIAN_POINT('Ctrl Pts',(203.407911968783,10.6952890563117,30.6386125909654));
#74671=CARTESIAN_POINT('Ctrl Pts',(203.41109147326,10.6505749521543,30.6247209424733));
#74672=CARTESIAN_POINT('Ctrl Pts',(203.411823637508,10.6402783576154,30.6215220262768));
#74673=CARTESIAN_POINT('Ctrl Pts',(203.412555801755,10.6300305693733,30.6181832181594));
#74674=CARTESIAN_POINT('Ctrl Pts',(203.413287966003,10.6198356011203,30.6147062807414));
#74675=CARTESIAN_POINT('Ctrl Pts',(203.416467664206,10.5755601228656,30.5996063742758));
#74676=CARTESIAN_POINT('Ctrl Pts',(203.419647362409,10.532088782024,30.581831442884));
#74677=CARTESIAN_POINT('Ctrl Pts',(203.422827060611,10.4897656725798,30.5614876323453));
#74678=CARTESIAN_POINT('Ctrl Pts',(203.426001128801,10.447517500954,30.5411798428079));
#74679=CARTESIAN_POINT('Ctrl Pts',(203.429175196991,10.4064140282021,30.5183124306163));
#74680=CARTESIAN_POINT('Ctrl Pts',(203.432349265181,10.3667811326855,30.493040245195));
#74681=CARTESIAN_POINT('Ctrl Pts',(203.435520065421,10.32718904231,30.4677940794495));
#74682=CARTESIAN_POINT('Ctrl Pts',(203.438690865662,10.2890649986719,30.4401483408109));
#74683=CARTESIAN_POINT('Ctrl Pts',(203.441861665902,10.2527098003953,30.4103034769102));
#74684=CARTESIAN_POINT('Ctrl Pts',(203.445031001829,10.2163713913887,30.3804723957283));
#74685=CARTESIAN_POINT('Ctrl Pts',(203.448200337755,10.1818006428641,30.3484445493972));
#74686=CARTESIAN_POINT('Ctrl Pts',(203.451369673682,10.1492667758389,30.3144618123697));
#74687=CARTESIAN_POINT('Ctrl Pts',(203.452928436518,10.1332657636376,30.2977482077621));
#74688=CARTESIAN_POINT('Ctrl Pts',(203.454487199354,10.1177569400978,30.2805623355414));
#74689=CARTESIAN_POINT('Ctrl Pts',(203.45604596219,10.1027690874833,30.2629362700282));
#74690=CARTESIAN_POINT('Origin',(197.762132885264,11.,29.5));
#74691=CARTESIAN_POINT('',(204.05505724195,10.1027693394584,30.2629365663567));
#74692=CARTESIAN_POINT('',(203.956022491041,10.1027690874833,30.2629362700282));
#74693=CARTESIAN_POINT('',(197.762132885264,10.1027690874833,30.2629362700282));
#74694=CARTESIAN_POINT('Ctrl Pts',(204.05505724195,10.1027693394584,30.2629365663567));
#74695=CARTESIAN_POINT('Ctrl Pts',(204.052835907548,10.1224928512846,30.2861318624328));
#74696=CARTESIAN_POINT('Ctrl Pts',(204.050599460949,10.1431218690039,30.3085694322674));
#74697=CARTESIAN_POINT('Ctrl Pts',(204.045520212742,10.1919703511427,30.3577233259098));
#74698=CARTESIAN_POINT('Ctrl Pts',(204.042683703823,10.2206723739991,30.383883470213));
#74699=CARTESIAN_POINT('Ctrl Pts',(204.03831536764,10.2676776166748,30.4226527885049));
#74700=CARTESIAN_POINT('Ctrl Pts',(204.036748192096,10.2851345060036,30.4362434041408));
#74701=CARTESIAN_POINT('Ctrl Pts',(204.034667807352,10.3092399669662,30.4539424724109));
#74702=CARTESIAN_POINT('Ctrl Pts',(204.0341298239,10.3155606200916,30.4584875624022));
#74703=CARTESIAN_POINT('Ctrl Pts',(204.033232260932,10.3262604567308,30.4660218383061));
#74704=CARTESIAN_POINT('Ctrl Pts',(204.032870542089,10.3306155304966,30.4690446845855));
#74705=CARTESIAN_POINT('Ctrl Pts',(204.032120436399,10.3397394541981,30.4752867139556));
#74706=CARTESIAN_POINT('Ctrl Pts',(204.031732385785,10.344511703729,30.4785005159385));
#74707=CARTESIAN_POINT('Ctrl Pts',(204.030679028501,10.3576023131747,30.4871774455548));
#74708=CARTESIAN_POINT('Ctrl Pts',(204.030018057272,10.3659668776202,30.4925704573194));
#74709=CARTESIAN_POINT('Ctrl Pts',(204.025683092899,10.421740904041,30.5275376711661));
#74710=CARTESIAN_POINT('Ctrl Pts',(204.022183556766,10.4711411201107,30.5538154917262));
#74711=CARTESIAN_POINT('Ctrl Pts',(204.015955961827,10.5627996408373,30.5944959511124));
#74712=CARTESIAN_POINT('Ctrl Pts',(204.013222538309,10.6043583198254,30.6101951036616));
#74713=CARTESIAN_POINT('Ctrl Pts',(204.007192911502,10.69653095015,30.6391794649589));
#74714=CARTESIAN_POINT('Ctrl Pts',(204.003888197558,10.7473399243291,30.6515143383119));
#74715=CARTESIAN_POINT('Ctrl Pts',(203.999511750217,10.8133781756465,30.6629644837922));
#74716=CARTESIAN_POINT('Ctrl Pts',(203.998537584715,10.8280061894554,30.6652176592421));
#74717=CARTESIAN_POINT('Ctrl Pts',(203.996910657824,10.8522883987296,30.6684906912002));
#74718=CARTESIAN_POINT('Ctrl Pts',(203.996262797415,10.8619199334116,30.6696679436373));
#74719=CARTESIAN_POINT('Ctrl Pts',(203.994985575199,10.880826251221,30.6717420745074));
#74720=CARTESIAN_POINT('Ctrl Pts',(203.994356547724,10.8900993188943,30.672648158375));
#74721=CARTESIAN_POINT('Ctrl Pts',(203.99296443976,10.9105318464105,30.6744001645528));
#74722=CARTESIAN_POINT('Ctrl Pts',(203.992199916843,10.9216944707229,30.6751972286528));
#74723=CARTESIAN_POINT('Ctrl Pts',(203.989514138873,10.960693826931,30.6774238723756));
#74724=CARTESIAN_POINT('Ctrl Pts',(203.987568176793,10.9885666916492,30.6780241974024));
#74725=CARTESIAN_POINT('Ctrl Pts',(203.979790269153,11.0984359735785,30.6764910801662));
#74726=CARTESIAN_POINT('Ctrl Pts',(203.973753597248,11.1800872767338,30.6667845832605));
#74727=CARTESIAN_POINT('Ctrl Pts',(203.965335421973,11.2923175536204,30.6413762400088));
#74728=CARTESIAN_POINT('Ctrl Pts',(203.96292842024,11.3242598418333,30.6327157985599));
#74729=CARTESIAN_POINT('Ctrl Pts',(203.959581246976,11.3688992429543,30.6185693214331));
#74730=CARTESIAN_POINT('Ctrl Pts',(203.958606391311,11.3819286241893,30.6141878380162));
#74731=CARTESIAN_POINT('Ctrl Pts',(203.956891795463,11.4049406915171,30.6059982645015));
#74732=CARTESIAN_POINT('Ctrl Pts',(203.956148186608,11.4149537704856,30.6022805962369));
#74733=CARTESIAN_POINT('Ctrl Pts',(203.955004517532,11.4304250027757,30.5962957077719));
#74734=CARTESIAN_POINT('Ctrl Pts',(203.954599455425,11.4359187268129,30.5941228584001));
#74735=CARTESIAN_POINT('Ctrl Pts',(203.953839642912,11.446254854153,30.5899445554007));
#74736=CARTESIAN_POINT('Ctrl Pts',(203.953484442784,11.4511003623981,30.5879480653001));
#74737=CARTESIAN_POINT('Ctrl Pts',(203.952630905518,11.4627730538088,30.5830471840331));
#74738=CARTESIAN_POINT('Ctrl Pts',(203.952134444027,11.4695863957594,30.580110515698));
#74739=CARTESIAN_POINT('Ctrl Pts',(203.950440373318,11.4928973983994,30.569800791019));
#74740=CARTESIAN_POINT('Ctrl Pts',(203.949259529218,11.5092537130237,30.5621121956177));
#74741=CARTESIAN_POINT('Ctrl Pts',(203.943522976248,11.5888194709494,30.5224498878186));
#74742=CARTESIAN_POINT('Ctrl Pts',(203.93918448111,11.6492374879105,30.4851927492431));
#74743=CARTESIAN_POINT('Ctrl Pts',(203.933802172331,11.7187221801916,30.4331603741348));
#74744=CARTESIAN_POINT('Ctrl Pts',(203.932810685901,11.7313031602659,30.4233339223295));
#74745=CARTESIAN_POINT('Ctrl Pts',(203.929616232122,11.7710091199807,30.3910006246545));
#74746=CARTESIAN_POINT('Ctrl Pts',(203.927397715491,11.7973235121348,30.3675322093738));
#74747=CARTESIAN_POINT('Ctrl Pts',(203.923534135699,11.840455371847,30.325442959711));
#74748=CARTESIAN_POINT('Ctrl Pts',(203.921910457725,11.8578031578968,30.307400095851));
#74749=CARTESIAN_POINT('Ctrl Pts',(203.919493210379,11.8823909608635,30.2801396548811));
#74750=CARTESIAN_POINT('Ctrl Pts',(203.918718514852,11.8900898117696,30.2713441513764));
#74751=CARTESIAN_POINT('Ctrl Pts',(203.917325874911,11.9035988716057,30.2554392153952));
#74752=CARTESIAN_POINT('Ctrl Pts',(203.916710022165,11.9094593350438,30.2483735957153));
#74753=CARTESIAN_POINT('Ctrl Pts',(203.915390968403,11.9217667525383,30.2331771790416));
#74754=CARTESIAN_POINT('Ctrl Pts',(203.914686904711,11.9281900105031,30.2250282853295));
#74755=CARTESIAN_POINT('Ctrl Pts',(203.91277652855,11.9452215795612,30.2028238034947));
#74756=CARTESIAN_POINT('Ctrl Pts',(203.911562487059,11.9556233451436,30.1886138962142));
#74757=CARTESIAN_POINT('Ctrl Pts',(203.904310815562,12.0152532824935,30.1031989686845));
#74758=CARTESIAN_POINT('Ctrl Pts',(203.89799623503,12.056820281184,30.0269859066105));
#74759=CARTESIAN_POINT('Ctrl Pts',(203.888624797964,12.1053225714124,29.9087311631785));
#74760=CARTESIAN_POINT('Ctrl Pts',(203.885602710583,12.1189693922557,29.8697390872537));
#74761=CARTESIAN_POINT('Ctrl Pts',(203.880991448339,12.1369773225309,29.8080664523042));
#74762=CARTESIAN_POINT('Ctrl Pts',(203.879362734056,12.1427680908482,29.7858384538874));
#74763=CARTESIAN_POINT('Ctrl Pts',(203.877215491364,12.1496700214736,29.7557657575486));
#74764=CARTESIAN_POINT('Ctrl Pts',(203.876670199822,12.1513572600192,29.7480599710953));
#74765=CARTESIAN_POINT('Ctrl Pts',(203.87576403892,12.1540526460263,29.7351294446682));
#74766=CARTESIAN_POINT('Ctrl Pts',(203.875400939565,12.1551030205704,29.729913857477));
#74767=CARTESIAN_POINT('Ctrl Pts',(203.874651891722,12.1572086176434,29.7190797888695));
#74768=CARTESIAN_POINT('Ctrl Pts',(203.87426623755,12.1582583356723,29.713460464498));
#74769=CARTESIAN_POINT('Ctrl Pts',(203.873226638282,12.1609928143643,29.6982079179623));
#74770=CARTESIAN_POINT('Ctrl Pts',(203.87257684056,12.1625986191563,29.6885607586204));
#74771=CARTESIAN_POINT('Ctrl Pts',(203.868742400214,12.1714383554727,29.6310396713103));
#74772=CARTESIAN_POINT('Ctrl Pts',(203.865688100292,12.1758355501235,29.5827711883056));
#74773=CARTESIAN_POINT('Ctrl Pts',(203.860150221329,12.1784281613573,29.493953129332));
#74774=CARTESIAN_POINT('Ctrl Pts',(203.857659456515,12.1775262443206,29.453507930113));
#74775=CARTESIAN_POINT('Ctrl Pts',(203.852547969694,12.1714579467391,29.3714044367933));
#74776=CARTESIAN_POINT('Ctrl Pts',(203.849929299999,12.1661423026335,29.3298168255078));
#74777=CARTESIAN_POINT('Ctrl Pts',(203.845459489568,12.1535738992326,29.2609320240257));
#74778=CARTESIAN_POINT('Ctrl Pts',(203.843640725555,12.1475358541894,29.2334526133792));
#74779=CARTESIAN_POINT('Ctrl Pts',(203.840989934214,12.1374778843301,29.1944056697384));
#74780=CARTESIAN_POINT('Ctrl Pts',(203.840182620614,12.1342521823018,29.1826424716073));
#74781=CARTESIAN_POINT('Ctrl Pts',(203.83875356189,12.1282629986583,29.1620606103496));
#74782=CARTESIAN_POINT('Ctrl Pts',(203.838134337998,12.1255772942379,29.1532202835904));
#74783=CARTESIAN_POINT('Ctrl Pts',(203.836830782244,12.1197369194628,29.1347789561071));
#74784=CARTESIAN_POINT('Ctrl Pts',(203.836145845869,12.1165621390541,29.1251851678169));
#74785=CARTESIAN_POINT('Ctrl Pts',(203.83431411122,12.1077942299657,29.0997901210721));
#74786=CARTESIAN_POINT('Ctrl Pts',(203.833160476738,12.1019867382816,29.0840658920285));
#74787=CARTESIAN_POINT('Ctrl Pts',(203.825417290153,12.0611464596619,28.9803539356571));
#74788=CARTESIAN_POINT('Ctrl Pts',(203.818485152985,12.0159507545616,28.896757569094));
#74789=CARTESIAN_POINT('Ctrl Pts',(203.807576859357,11.9299213255743,28.7752370866083));
#74790=CARTESIAN_POINT('Ctrl Pts',(203.803625604819,11.8955703283721,28.7331949691175));
#74791=CARTESIAN_POINT('Ctrl Pts',(203.799139462438,11.85171295339,28.6865034232678));
#74792=CARTESIAN_POINT('Ctrl Pts',(203.798456546617,11.8448952405991,28.6794247850486));
#74793=CARTESIAN_POINT('Ctrl Pts',(203.797385499418,11.8339655522644,28.6683574601672));
#74794=CARTESIAN_POINT('Ctrl Pts',(203.796993294494,11.8299118805489,28.6643121812518));
#74795=CARTESIAN_POINT('Ctrl Pts',(203.79624572188,11.8220833295916,28.6566129842009));
#74796=CARTESIAN_POINT('Ctrl Pts',(203.795890034974,11.8183132806606,28.6529545259866));
#74797=CARTESIAN_POINT('Ctrl Pts',(203.795010306112,11.8088791553193,28.6439214173039));
#74798=CARTESIAN_POINT('Ctrl Pts',(203.794488512221,11.8031857431121,28.6385775149027));
#74799=CARTESIAN_POINT('Ctrl Pts',(203.792595947004,11.7821961472855,28.6192654729975));
#74800=CARTESIAN_POINT('Ctrl Pts',(203.791247643051,11.7665844536462,28.605644078208));
#74801=CARTESIAN_POINT('Ctrl Pts',(203.784959508864,11.6911229421945,28.5432316742109));
#74802=CARTESIAN_POINT('Ctrl Pts',(203.780258051014,11.6269257956876,28.499988674596));
#74803=CARTESIAN_POINT('Ctrl Pts',(203.771837629189,11.5077780226486,28.4357459103207));
#74804=CARTESIAN_POINT('Ctrl Pts',(203.76817662595,11.4546361471705,28.4119834172088));
#74805=CARTESIAN_POINT('Ctrl Pts',(203.763395159632,11.3857055034298,28.3870956720097));
#74806=CARTESIAN_POINT('Ctrl Pts',(203.762398171474,11.3713523744983,28.3822244595857));
#74807=CARTESIAN_POINT('Ctrl Pts',(203.760743522307,11.3475943235182,28.3746694702944));
#74808=CARTESIAN_POINT('Ctrl Pts',(203.760091120343,11.3382426180778,28.3718233575652));
#74809=CARTESIAN_POINT('Ctrl Pts',(203.758812489884,11.319952583571,28.3665047877925));
#74810=CARTESIAN_POINT('Ctrl Pts',(203.758186682504,11.3110183235955,28.3640208426989));
#74811=CARTESIAN_POINT('Ctrl Pts',(203.756674219465,11.2894742010538,28.3583042465817));
#74812=CARTESIAN_POINT('Ctrl Pts',(203.755784378132,11.2768384965162,28.3551747164221));
#74813=CARTESIAN_POINT('Ctrl Pts',(203.752717227279,11.233436851311,28.3451858083869));
#74814=CARTESIAN_POINT('Ctrl Pts',(203.750508796845,11.2024510190121,28.3393528307842));
#74815=CARTESIAN_POINT('Ctrl Pts',(203.741640262798,11.0790772476091,28.3212187858246));
#74816=CARTESIAN_POINT('Ctrl Pts',(203.734722214072,10.9856059829233,28.3186586185084));
#74817=CARTESIAN_POINT('Ctrl Pts',(203.726298741185,10.8700141789542,28.3292209538258));
#74818=CARTESIAN_POINT('Ctrl Pts',(203.724649453458,10.8472644778638,28.3319709472456));
#74819=CARTESIAN_POINT('Ctrl Pts',(203.721919083114,10.8092137993591,28.3377013924152));
#74820=CARTESIAN_POINT('Ctrl Pts',(203.720825586205,10.7938658891871,28.3403249541164));
#74821=CARTESIAN_POINT('Ctrl Pts',(203.719273222351,10.7718617555778,28.3445370173452));
#74822=CARTESIAN_POINT('Ctrl Pts',(203.718802557287,10.7651609576225,28.3458802520192));
#74823=CARTESIAN_POINT('Ctrl Pts',(203.717981222747,10.7534096418494,28.3483424941947));
#74824=CARTESIAN_POINT('Ctrl Pts',(203.717629245643,10.7483542769184,28.3494365515412));
#74825=CARTESIAN_POINT('Ctrl Pts',(203.716855605197,10.7371988963229,28.3519277902144));
#74826=CARTESIAN_POINT('Ctrl Pts',(203.716434785891,10.7311026133432,28.3533403212785));
#74827=CARTESIAN_POINT('Ctrl Pts',(203.715212571445,10.7133246152663,28.3576091308158));
#74828=CARTESIAN_POINT('Ctrl Pts',(203.714417957363,10.7016746624216,28.3605959039402));
#74829=CARTESIAN_POINT('Ctrl Pts',(203.709399505872,10.6276820027327,28.3807786243057));
#74830=CARTESIAN_POINT('Ctrl Pts',(203.705395097199,10.5667917834196,28.4029084588218));
#74831=CARTESIAN_POINT('Ctrl Pts',(203.697985457178,10.4580805483938,28.4528898842018));
#74832=CARTESIAN_POINT('Ctrl Pts',(203.694589657529,10.4098106535687,28.4793176947714));
#74833=CARTESIAN_POINT('Ctrl Pts',(203.688992701592,10.3355682931643,28.5269981148427));
#74834=CARTESIAN_POINT('Ctrl Pts',(203.686852409059,10.3083483483887,28.5461552264396));
#74835=CARTESIAN_POINT('Ctrl Pts',(203.683821088964,10.2717210603782,28.5743260452145));
#74836=CARTESIAN_POINT('Ctrl Pts',(203.682966166023,10.2615956642631,28.5823827050844));
#74837=CARTESIAN_POINT('Ctrl Pts',(203.681482048412,10.2443837828455,28.5965473635551));
#74838=CARTESIAN_POINT('Ctrl Pts',(203.680856017061,10.2372334207898,28.6025760917583));
#74839=CARTESIAN_POINT('Ctrl Pts',(203.6795654824,10.2227228708218,28.6151091642517));
#74840=CARTESIAN_POINT('Ctrl Pts',(203.678900676885,10.2153707526306,28.621621686916));
#74841=CARTESIAN_POINT('Ctrl Pts',(203.677184731048,10.1967133510109,28.6385696140709));
#74842=CARTESIAN_POINT('Ctrl Pts',(203.676128229257,10.1855298413182,28.6491356909623));
#74843=CARTESIAN_POINT('Ctrl Pts',(203.671064714263,10.1333862115855,28.7003706481116));
#74844=CARTESIAN_POINT('Ctrl Pts',(203.666940687652,10.0952508996848,28.7437897819964));
#74845=CARTESIAN_POINT('Ctrl Pts',(203.658781687065,10.0276121823865,28.8332739161955));
#74846=CARTESIAN_POINT('Ctrl Pts',(203.654765239416,9.99782340616605,28.8789495952375));
#74847=CARTESIAN_POINT('Ctrl Pts',(203.648805453967,9.9580081664312,28.950369631282));
#74848=CARTESIAN_POINT('Ctrl Pts',(203.646829669774,9.94554602352513,28.97467390172));
#74849=CARTESIAN_POINT('Ctrl Pts',(203.643632441726,9.92646163779091,29.0153146031872));
#74850=CARTESIAN_POINT('Ctrl Pts',(203.642393110891,9.91934120111442,29.0314050920125));
#74851=CARTESIAN_POINT('Ctrl Pts',(203.640675382206,9.90983359434278,29.0542606892761));
#74852=CARTESIAN_POINT('Ctrl Pts',(203.640181642921,9.90714391360983,29.0608964745907));
#74853=CARTESIAN_POINT('Ctrl Pts',(203.639334940366,9.90260374745161,29.0723978282189));
#74854=CARTESIAN_POINT('Ctrl Pts',(203.638980383895,9.90072473963864,29.0772517788513));
#74855=CARTESIAN_POINT('Ctrl Pts',(203.638218330027,9.89673375227158,29.0877680675223));
#74856=CARTESIAN_POINT('Ctrl Pts',(203.637811471064,9.89463309380784,29.0934344011043));
#74857=CARTESIAN_POINT('Ctrl Pts',(203.636669573462,9.88882640578398,29.1094751463394));
#74858=CARTESIAN_POINT('Ctrl Pts',(203.635940039191,9.88522207797972,29.119886038787));
#74859=CARTESIAN_POINT('Ctrl Pts',(203.630110313355,9.85733701312374,29.2042409030244));
#74860=CARTESIAN_POINT('Ctrl Pts',(203.625340366416,9.84029112482895,29.2803849877759));
#74861=CARTESIAN_POINT('Ctrl Pts',(203.617583335211,9.82515975734209,29.4046696685909));
#74862=CARTESIAN_POINT('Ctrl Pts',(203.61463894431,9.82227727926294,29.4519766908943));
#74863=CARTESIAN_POINT('Ctrl Pts',(203.609726484388,9.82223312669742,29.5291590023504));
#74864=CARTESIAN_POINT('Ctrl Pts',(203.607802566791,9.82334956396589,29.5589795058165));
#74865=CARTESIAN_POINT('Ctrl Pts',(203.605089726457,9.82646342739179,29.6001965699306));
#74866=CARTESIAN_POINT('Ctrl Pts',(203.604329777116,9.82749822288538,29.611655754157));
#74867=CARTESIAN_POINT('Ctrl Pts',(203.602996712311,9.82959343789739,29.6315921579023));
#74868=CARTESIAN_POINT('Ctrl Pts',(203.602425938396,9.83057853046149,29.6400765390137));
#74869=CARTESIAN_POINT('Ctrl Pts',(203.601217926214,9.83284714279946,29.6579192389235));
#74870=CARTESIAN_POINT('Ctrl Pts',(203.60058009458,9.83415113342793,29.6672742942761));
#74871=CARTESIAN_POINT('Ctrl Pts',(203.599024255667,9.83758704461222,29.689927778203));
#74872=CARTESIAN_POINT('Ctrl Pts',(203.598102729704,9.83983478581976,29.7032070119741));
#74873=CARTESIAN_POINT('Ctrl Pts',(203.594586116635,9.84920781646309,29.7533403066453));
#74874=CARTESIAN_POINT('Ctrl Pts',(203.591944676557,9.85786512263747,29.7898816350214));
#74875=CARTESIAN_POINT('Ctrl Pts',(203.58433082435,9.88731369403648,29.8921334534756));
#74876=CARTESIAN_POINT('Ctrl Pts',(203.579260920003,9.91214480609692,29.9565183643017));
#74877=CARTESIAN_POINT('Ctrl Pts',(203.570611870851,9.96416475895057,30.0626485218357));
#74878=CARTESIAN_POINT('Ctrl Pts',(203.567029387455,9.9886372126498,30.1055363949191));
#74879=CARTESIAN_POINT('Ctrl Pts',(203.562888958763,10.021107804077,30.1549511729283));
#74880=CARTESIAN_POINT('Ctrl Pts',(203.562208453497,10.0265879033658,30.1630685302341));
#74881=CARTESIAN_POINT('Ctrl Pts',(203.561140296925,10.0354278933322,30.1758168572441));
#74882=CARTESIAN_POINT('Ctrl Pts',(203.560748607466,10.0387212291433,30.1804931312233));
#74883=CARTESIAN_POINT('Ctrl Pts',(203.559997109199,10.0451426591428,30.1894713983153));
#74884=CARTESIAN_POINT('Ctrl Pts',(203.559637035781,10.0482660175161,30.1937764613178));
#74885=CARTESIAN_POINT('Ctrl Pts',(203.558748256438,10.0560885847851,30.2044064067175));
#74886=CARTESIAN_POINT('Ctrl Pts',(203.55822182526,10.0608224117722,30.2107057138403));
#74887=CARTESIAN_POINT('Ctrl Pts',(203.556391910927,10.0776154301364,30.2325913604401));
#74888=CARTESIAN_POINT('Ctrl Pts',(203.555108328926,10.0900025848589,30.2479225641033));
#74889=CARTESIAN_POINT('Ctrl Pts',(203.553841401988,10.1027690875417,30.2629362700969));
#74890=CARTESIAN_POINT('',(203.512132885208,9.82225044284812,29.5010213366495));
#74891=CARTESIAN_POINT('Ctrl Pts',(203.45604596219,10.1027690874833,30.2629362700282));
#74892=CARTESIAN_POINT('Ctrl Pts',(203.45921737708,10.0722752253946,30.2270747744055));
#74893=CARTESIAN_POINT('Ctrl Pts',(203.46238879197,10.0439406535874,30.1893892494117));
#74894=CARTESIAN_POINT('Ctrl Pts',(203.46556020686,10.0179771118165,30.1501739071846));
#74895=CARTESIAN_POINT('Ctrl Pts',(203.468732893903,9.99200315525983,30.1109428344617));
#74896=CARTESIAN_POINT('Ctrl Pts',(203.471905580946,9.96840240753564,30.0701812021462));
#74897=CARTESIAN_POINT('Ctrl Pts',(203.47507826799,9.94734179825937,30.0282099703794));
#74898=CARTESIAN_POINT('Ctrl Pts',(203.478257091189,9.92624045657508,29.9861575638795));
#74899=CARTESIAN_POINT('Ctrl Pts',(203.481435914388,9.90768928947866,29.9428913969871));
#74900=CARTESIAN_POINT('Ctrl Pts',(203.484614737587,9.89180735454263,29.8987532107133));
#74901=CARTESIAN_POINT('Ctrl Pts',(203.487056446638,9.87960816577514,29.8648499068415));
#74902=CARTESIAN_POINT('Ctrl Pts',(203.489498155688,9.86898284931918,29.8304325616935));
#74903=CARTESIAN_POINT('Ctrl Pts',(203.491939864738,9.85996497249551,29.7956606138173));
#74904=CARTESIAN_POINT('Ctrl Pts',(203.495988552475,9.84501209868252,29.7380039659176));
#74905=CARTESIAN_POINT('Ctrl Pts',(203.500037240213,9.83442672707395,29.6791717338297));
#74906=CARTESIAN_POINT('Ctrl Pts',(203.50408592795,9.82835314494067,29.619744350721));
#74907=CARTESIAN_POINT('Ctrl Pts',(203.506768247036,9.82432930157885,29.5803727779349));
#74908=CARTESIAN_POINT('Ctrl Pts',(203.509450566122,9.82228488691305,29.5407403482437));
#74909=CARTESIAN_POINT('Ctrl Pts',(203.512132885208,9.82225044284812,29.5010213366495));
#74910=CARTESIAN_POINT('Ctrl Pts',(203.512132885264,9.8222504428474,29.5010213358201));
#74911=CARTESIAN_POINT('Ctrl Pts',(203.515270544845,9.82221015171904,29.4545597727904));
#74912=CARTESIAN_POINT('Ctrl Pts',(203.518408204426,9.82492346972817,29.40803242817));
#74913=CARTESIAN_POINT('Ctrl Pts',(203.521545864007,9.83038714755937,29.361794218986));
#74914=CARTESIAN_POINT('Ctrl Pts',(203.524681486004,9.83584727729981,29.315586036712));
#74915=CARTESIAN_POINT('Ctrl Pts',(203.527817108002,9.84405416548516,29.2696671832549));
#74916=CARTESIAN_POINT('Ctrl Pts',(203.530952729999,9.85495262916811,29.2243887138541));
#74917=CARTESIAN_POINT('Ctrl Pts',(203.534087766409,9.86584905752816,29.1791187003521));
#74918=CARTESIAN_POINT('Ctrl Pts',(203.537222802819,9.87943592937715,29.1344893872576));
#74919=CARTESIAN_POINT('Ctrl Pts',(203.540357839229,9.8956073301553,29.090840015039));
#74920=CARTESIAN_POINT('Ctrl Pts',(203.543495829822,9.91179396944655,29.0471495114713));
#74921=CARTESIAN_POINT('Ctrl Pts',(203.546633820416,9.93056979619447,29.0044413257409));
#74922=CARTESIAN_POINT('Ctrl Pts',(203.54977181101,9.95178028604199,28.9630358542977));
#74923=CARTESIAN_POINT('Ctrl Pts',(203.552911636061,9.97300317545919,28.9216061773774));
#74924=CARTESIAN_POINT('Ctrl Pts',(203.556051461112,9.99666326771046,28.8814812196115));
#74925=CARTESIAN_POINT('Ctrl Pts',(203.559191286163,10.0225613570507,28.8429545207755));
#74926=CARTESIAN_POINT('Ctrl Pts',(203.562336629387,10.0485049617121,28.8043601121154));
#74927=CARTESIAN_POINT('Ctrl Pts',(203.565481972611,10.0766940559281,28.7673700115092));
#74928=CARTESIAN_POINT('Ctrl Pts',(203.568627315836,10.1068889991453,28.732244959214));
#74929=CARTESIAN_POINT('Ctrl Pts',(203.569282131714,10.1131751583546,28.7249324211717));
#74930=CARTESIAN_POINT('Ctrl Pts',(203.569936947593,10.1195481297463,28.7177005859782));
#74931=CARTESIAN_POINT('Ctrl Pts',(203.570591763472,10.1260055620902,28.7105515944643));
#74932=CARTESIAN_POINT('Ctrl Pts',(203.573868925919,10.1583231271821,28.6747729774718));
#74933=CARTESIAN_POINT('Ctrl Pts',(203.577146088366,10.1929142128349,28.6409013821579));
#74934=CARTESIAN_POINT('Ctrl Pts',(203.580423250814,10.2295226065395,28.6092364799419));
#74935=CARTESIAN_POINT('Ctrl Pts',(203.583597203154,10.2649780649534,28.5785688239731));
#74936=CARTESIAN_POINT('Ctrl Pts',(203.586771155494,10.3023251845411,28.5499713149255));
#74937=CARTESIAN_POINT('Ctrl Pts',(203.589945107834,10.341291943156,28.5236810160871));
#74938=CARTESIAN_POINT('Ctrl Pts',(203.59311593521,10.3802203364505,28.4974166017659));
#74939=CARTESIAN_POINT('Ctrl Pts',(203.596286762587,10.4207647527763,28.4734552113849));
#74940=CARTESIAN_POINT('Ctrl Pts',(203.599457589964,10.4626213414356,28.4519927291189));
#74941=CARTESIAN_POINT('Ctrl Pts',(203.602626686916,10.5044550875888,28.4305419596299));
#74942=CARTESIAN_POINT('Ctrl Pts',(203.605795783869,10.547599092752,28.4115876502471));
#74943=CARTESIAN_POINT('Ctrl Pts',(203.608964880821,10.5917242201031,28.3952801486125));
#74944=CARTESIAN_POINT('Ctrl Pts',(203.612133638891,10.635844628995,28.3789743907979));
#74945=CARTESIAN_POINT('Ctrl Pts',(203.615302396961,10.6809454289694,28.3653150695729));
#74946=CARTESIAN_POINT('Ctrl Pts',(203.61847115503,10.7266793354574,28.3544037025051));
#74947=CARTESIAN_POINT('Ctrl Pts',(203.621643099472,10.7724592300683,28.3434813634184));
#74948=CARTESIAN_POINT('Ctrl Pts',(203.624815043913,10.8188729585003,28.3353126192441));
#74949=CARTESIAN_POINT('Ctrl Pts',(203.627986988355,10.865561923027,28.3299480926216));
#74950=CARTESIAN_POINT('Ctrl Pts',(203.631160877631,10.9122795142515,28.3245802768132));
#74951=CARTESIAN_POINT('Ctrl Pts',(203.634334766906,10.9592721212958,28.3220201302267));
#74952=CARTESIAN_POINT('Ctrl Pts',(203.637508656182,11.0061785242847,28.322266206506));
#74953=CARTESIAN_POINT('Ctrl Pts',(203.640688160665,11.0531679135282,28.3225127181407));
#74954=CARTESIAN_POINT('Ctrl Pts',(203.643867665148,11.1000702398532,28.3255753159026));
#74955=CARTESIAN_POINT('Ctrl Pts',(203.647047169632,11.1465287613955,28.3314006740615));
#74956=CARTESIAN_POINT('Ctrl Pts',(203.647779333823,11.1572270529188,28.3327421153675));
#74957=CARTESIAN_POINT('Ctrl Pts',(203.648511498015,11.1679018572594,28.3342298445736));
#74958=CARTESIAN_POINT('Ctrl Pts',(203.649243662206,11.178548913606,28.3358628311277));
#74959=CARTESIAN_POINT('Ctrl Pts',(203.652520824653,11.2262050727579,28.3431720689655));
#74960=CARTESIAN_POINT('Ctrl Pts',(203.6557979871,11.2735191772522,28.3534289543614));
#74961=CARTESIAN_POINT('Ctrl Pts',(203.659075149548,11.3201000321551,28.3665843516546));
#74962=CARTESIAN_POINT('Ctrl Pts',(203.66224910206,11.3652138840976,28.3793254369559));
#74963=CARTESIAN_POINT('Ctrl Pts',(203.665423054572,11.4096394077614,28.3947849953841));
#74964=CARTESIAN_POINT('Ctrl Pts',(203.668597007084,11.4530289979444,28.412866250399));
#74965=CARTESIAN_POINT('Ctrl Pts',(203.671767834634,11.4963758682539,28.4309297032424));
#74966=CARTESIAN_POINT('Ctrl Pts',(203.674938662183,11.5386883121724,28.4516095301784));
#74967=CARTESIAN_POINT('Ctrl Pts',(203.678109489733,11.5796356070272,28.4747597230082));
#74968=CARTESIAN_POINT('Ctrl Pts',(203.681278586858,11.620560555614,28.4978972820263));
#74969=CARTESIAN_POINT('Ctrl Pts',(203.684447683984,11.6601213471134,28.5235022625312));
#74970=CARTESIAN_POINT('Ctrl Pts',(203.68761678111,11.6980113790721,28.5513824916301));
#74971=CARTESIAN_POINT('Ctrl Pts',(203.690785539353,11.7358973593143,28.5792597393965));
#74972=CARTESIAN_POINT('Ctrl Pts',(203.693954297597,11.7721124878349,28.6094114210323));
#74973=CARTESIAN_POINT('Ctrl Pts',(203.69712305584,11.8063809594186,28.6416033488025));
#74974=CARTESIAN_POINT('Ctrl Pts',(203.700295000453,11.840683889944,28.6738276474287));
#74975=CARTESIAN_POINT('Ctrl Pts',(203.703466945067,11.873035852828,28.7080959022972));
#74976=CARTESIAN_POINT('Ctrl Pts',(203.706638889681,11.9031973238985,28.7441364828208));
#74977=CARTESIAN_POINT('Ctrl Pts',(203.709812779129,11.9333772880552,28.7801991611247));
#74978=CARTESIAN_POINT('Ctrl Pts',(203.712986668576,11.9613637566435,28.8180358797258));
#74979=CARTESIAN_POINT('Ctrl Pts',(203.716160558024,11.9869592475456,28.857344177507));
#74980=CARTESIAN_POINT('Ctrl Pts',(203.719340062676,12.0126000216661,28.8967220190307));
#74981=CARTESIAN_POINT('Ctrl Pts',(203.722519567329,12.0358411085791,28.9375761477844));
#74982=CARTESIAN_POINT('Ctrl Pts',(203.725699071981,12.0565308153257,28.9795793059772));
#74983=CARTESIAN_POINT('Ctrl Pts',(203.726431234967,12.0612951541561,28.9892516169495));
#74984=CARTESIAN_POINT('Ctrl Pts',(203.727163397954,12.0659244048403,28.9989847789349));
#74985=CARTESIAN_POINT('Ctrl Pts',(203.72789556094,12.0704170843594,29.0087746667653));
#74986=CARTESIAN_POINT('Ctrl Pts',(203.731172723387,12.0905263235356,29.0525942170029));
#74987=CARTESIAN_POINT('Ctrl Pts',(203.734449885835,12.1079857460662,29.0977494691135));
#74988=CARTESIAN_POINT('Ctrl Pts',(203.737727048282,12.1226212086448,29.1438866972425));
#74989=CARTESIAN_POINT('Ctrl Pts',(203.740901000165,12.1367957437058,29.1885708849965));
#74990=CARTESIAN_POINT('Ctrl Pts',(203.744074952048,12.148321384721,29.2341755326984));
#74991=CARTESIAN_POINT('Ctrl Pts',(203.747248903931,12.1570877514646,29.2803571127702));
#74992=CARTESIAN_POINT('Ctrl Pts',(203.750419730852,12.1658454871523,29.3264932240856));
#74993=CARTESIAN_POINT('Ctrl Pts',(203.753590557774,12.1718492225175,29.3732045987342));
#74994=CARTESIAN_POINT('Ctrl Pts',(203.756761384696,12.1750389784448,29.420134728227));
#74995=CARTESIAN_POINT('Ctrl Pts',(203.759930481197,12.1782269936212,29.4670392464605));
#74996=CARTESIAN_POINT('Ctrl Pts',(203.763099577698,12.1786040339559,29.5141617283881));
#74997=CARTESIAN_POINT('Ctrl Pts',(203.766268674199,12.1761619412433,29.5611404160168));
#74998=CARTESIAN_POINT('Ctrl Pts',(203.769437431821,12.1737201096694,29.608114080105));
#74999=CARTESIAN_POINT('Ctrl Pts',(203.772606189443,12.1684597747374,29.6549434247692));
#75000=CARTESIAN_POINT('Ctrl Pts',(203.775774947065,12.1604248061988,29.7012693013313));
#75001=CARTESIAN_POINT('Ctrl Pts',(203.778946891068,12.1523817580038,29.7476417614194));
#75002=CARTESIAN_POINT('Ctrl Pts',(203.782118835072,12.1415586066478,29.7935091941591));
#75003=CARTESIAN_POINT('Ctrl Pts',(203.785290779075,12.1280504480154,29.8385221547139));
#75004=CARTESIAN_POINT('Ctrl Pts',(203.788464667918,12.1145340070186,29.8835627144226));
#75005=CARTESIAN_POINT('Ctrl Pts',(203.79163855676,12.0983294745641,29.9277472365617));
#75006=CARTESIAN_POINT('Ctrl Pts',(203.794812445603,12.0795808193802,29.9707444284603));
#75007=CARTESIAN_POINT('Ctrl Pts',(203.797991949664,12.0607989942246,30.013817690649));
#75008=CARTESIAN_POINT('Ctrl Pts',(203.801171453726,12.0394643237894,30.055698938682));
#75009=CARTESIAN_POINT('Ctrl Pts',(203.804350957787,12.0157666716959,30.0960814803127));
#75010=CARTESIAN_POINT('Ctrl Pts',(203.805083125083,12.0103096427031,30.1053806589661));
#75011=CARTESIAN_POINT('Ctrl Pts',(203.805815292378,12.0047274881293,30.1146004918079));
#75012=CARTESIAN_POINT('Ctrl Pts',(203.806547459674,11.9990228373354,30.1237374712028));
#75013=CARTESIAN_POINT('Ctrl Pts',(203.809824622121,11.9734889634953,30.1646343617529));
#75014=CARTESIAN_POINT('Ctrl Pts',(203.813101784569,11.9453820663439,30.2040530175907));
#75015=CARTESIAN_POINT('Ctrl Pts',(203.816378947016,11.9149017648864,30.2416534386813));
#75016=CARTESIAN_POINT('Ctrl Pts',(203.819552899594,11.8853813999498,30.278069684561));
#75017=CARTESIAN_POINT('Ctrl Pts',(203.822726852172,11.8536352991124,30.3127800606325));
#75018=CARTESIAN_POINT('Ctrl Pts',(203.825900804751,11.8198896376673,30.3455034266907));
#75019=CARTESIAN_POINT('Ctrl Pts',(203.829071632361,11.7861772010776,30.3781945744115));
#75020=CARTESIAN_POINT('Ctrl Pts',(203.832242459971,11.750469498702,30.408902198503));
#75021=CARTESIAN_POINT('Ctrl Pts',(203.835413287581,11.7130312698498,30.4373801100495));
#75022=CARTESIAN_POINT('Ctrl Pts',(203.838582384763,11.6756134723184,30.4658424802265));
#75023=CARTESIAN_POINT('Ctrl Pts',(203.841751481944,11.6364674617191,30.4920772119245));
#75024=CARTESIAN_POINT('Ctrl Pts',(203.844920579125,11.5958908656149,30.5158785059133));
#75025=CARTESIAN_POINT('Ctrl Pts',(203.848089337418,11.5553186085821,30.5396772547032));
#75026=CARTESIAN_POINT('Ctrl Pts',(203.851258095711,11.513316550963,30.5610428028245));
#75027=CARTESIAN_POINT('Ctrl Pts',(203.854426854004,11.4702087593309,30.5798142364076));
#75028=CARTESIAN_POINT('Ctrl Pts',(203.857598798659,11.4270576204216,30.5986045457091));
#75029=CARTESIAN_POINT('Ctrl Pts',(203.860770743314,11.3827990411416,30.6147953150461));
#75030=CARTESIAN_POINT('Ctrl Pts',(203.863942687969,11.3377771611781,30.6282737486472));
#75031=CARTESIAN_POINT('Ctrl Pts',(203.867116577453,11.2927276767451,30.6417604463414));
#75032=CARTESIAN_POINT('Ctrl Pts',(203.870290466937,11.2469145024704,30.6525313715803));
#75033=CARTESIAN_POINT('Ctrl Pts',(203.873464356421,11.2006935012809,30.660524528411));
#75034=CARTESIAN_POINT('Ctrl Pts',(203.876643861103,11.1543907265893,30.6685318266149));
#75035=CARTESIAN_POINT('Ctrl Pts',(203.879823365784,11.1076792388029,30.6737514955824));
#75036=CARTESIAN_POINT('Ctrl Pts',(203.883002870466,11.0609196009251,30.6761733990884));
#75037=CARTESIAN_POINT('Ctrl Pts',(203.883735033113,11.050151992858,30.6767311045992));
#75038=CARTESIAN_POINT('Ctrl Pts',(203.884467195761,11.0393818232111,30.6771406714871));
#75039=CARTESIAN_POINT('Ctrl Pts',(203.885199358408,11.0286134675187,30.6774023662183));
#75040=CARTESIAN_POINT('Ctrl Pts',(203.888378113557,10.9818616068113,30.6785385392771));
#75041=CARTESIAN_POINT('Ctrl Pts',(203.891556868707,10.9349396859611,30.676888279367));
#75042=CARTESIAN_POINT('Ctrl Pts',(203.894735623856,10.8882069579571,30.6724322488958));
#75043=CARTESIAN_POINT('Ctrl Pts',(203.897909711837,10.8415428447053,30.6679827609364));
#75044=CARTESIAN_POINT('Ctrl Pts',(203.901083799818,10.795067924098,30.6607357068325));
#75045=CARTESIAN_POINT('Ctrl Pts',(203.904257887799,10.7491415207722,30.6507237226631));
#75046=CARTESIAN_POINT('Ctrl Pts',(203.907428708611,10.7032623906616,30.6407220440836));
#75047=CARTESIAN_POINT('Ctrl Pts',(203.910599529423,10.6579312015293,30.6279611886194));
#75048=CARTESIAN_POINT('Ctrl Pts',(203.913770350234,10.6134995096863,30.612525250719));
#75049=CARTESIAN_POINT('Ctrl Pts',(203.916939298735,10.5690940539301,30.5970984274524));
#75050=CARTESIAN_POINT('Ctrl Pts',(203.920108247236,10.5255875676862,30.5789998350351));
#75051=CARTESIAN_POINT('Ctrl Pts',(203.923277195737,10.4833161705163,30.5583633038093));
#75052=CARTESIAN_POINT('Ctrl Pts',(203.926447272807,10.4410297190819,30.5377194232214));
#75053=CARTESIAN_POINT('Ctrl Pts',(203.929617349877,10.3999797404455,30.5145360339655));
#75054=CARTESIAN_POINT('Ctrl Pts',(203.932787426947,10.3604800787254,30.4889941014955));
#75055=CARTESIAN_POINT('Ctrl Pts',(203.93595812237,10.3209727122315,30.4634471868357));
#75056=CARTESIAN_POINT('Ctrl Pts',(203.939128817793,10.2830167219262,30.4355411317108));
#75057=CARTESIAN_POINT('Ctrl Pts',(203.942299513216,10.2468962926746,30.4054997893499));
#75058=CARTESIAN_POINT('Ctrl Pts',(203.945474436867,10.2107276956168,30.3754183858495));
#75059=CARTESIAN_POINT('Ctrl Pts',(203.948649360519,10.1763999577101,30.3431963866487));
#75060=CARTESIAN_POINT('Ctrl Pts',(203.951824284171,10.1441620501808,30.3090960796773));
#75061=CARTESIAN_POINT('Ctrl Pts',(203.953223686461,10.1299526371139,30.294065781975));
#75062=CARTESIAN_POINT('Ctrl Pts',(203.954623088751,10.1161487176961,30.2786710283514));
#75063=CARTESIAN_POINT('Ctrl Pts',(203.956022491041,10.1027690874833,30.2629362700282));
#75064=CARTESIAN_POINT('Origin',(197.762132885264,11.,29.5));
#75065=CARTESIAN_POINT('',(204.55557810053,10.1027691095676,30.2629362959998));
#75066=CARTESIAN_POINT('',(204.456095751509,10.1027690874833,30.2629362700282));
#75067=CARTESIAN_POINT('',(197.762132885264,10.1027690874833,30.2629362700282));
#75068=CARTESIAN_POINT('',(204.109784405193,9.82224970774337,29.4997795333053));
#75069=CARTESIAN_POINT('Ctrl Pts',(204.55557810053,10.1027691095676,30.2629362959998));
#75070=CARTESIAN_POINT('Ctrl Pts',(204.554745776962,10.1111980219123,30.2728488936414));
#75071=CARTESIAN_POINT('Ctrl Pts',(204.553908087797,10.1197925935299,30.2826234406836));
#75072=CARTESIAN_POINT('Ctrl Pts',(204.551884317315,10.1407946177784,30.3057248486708));
#75073=CARTESIAN_POINT('Ctrl Pts',(204.550693062403,10.1533497353789,30.318907621637));
#75074=CARTESIAN_POINT('Ctrl Pts',(204.548803084603,10.1735280718412,30.3391345148177));
#75075=CARTESIAN_POINT('Ctrl Pts',(204.548113103554,10.1809477838916,30.3463781884366));
#75076=CARTESIAN_POINT('Ctrl Pts',(204.546807871193,10.1950758178344,30.3598112650973));
#75077=CARTESIAN_POINT('Ctrl Pts',(204.546193618398,10.2017623608044,30.3660225251029));
#75078=CARTESIAN_POINT('Ctrl Pts',(204.544794249705,10.2170758317143,30.3799194789959));
#75079=CARTESIAN_POINT('Ctrl Pts',(204.544007222387,10.225744917043,30.3875570927461));
#75080=CARTESIAN_POINT('Ctrl Pts',(204.541539198746,10.2530953389058,30.4109476351716));
#75081=CARTESIAN_POINT('Ctrl Pts',(204.539840473675,10.2721544739678,30.4262466764234));
#75082=CARTESIAN_POINT('Ctrl Pts',(204.532031285784,10.3607694339367,30.4929546206106));
#75083=CARTESIAN_POINT('Ctrl Pts',(204.525669634465,10.4353752218609,30.5371929714194));
#75084=CARTESIAN_POINT('Ctrl Pts',(204.516822567785,10.5454123843986,30.5870253237653));
#75085=CARTESIAN_POINT('Ctrl Pts',(204.514320324364,10.5772958717402,30.599816096644));
#75086=CARTESIAN_POINT('Ctrl Pts',(204.510858149916,10.6229478750447,30.615851282649));
#75087=CARTESIAN_POINT('Ctrl Pts',(204.509860917012,10.6362842472105,30.6202692878998));
#75088=CARTESIAN_POINT('Ctrl Pts',(204.508112092945,10.6600540619066,30.6276743766632));
#75089=CARTESIAN_POINT('Ctrl Pts',(204.507356378825,10.6704556117793,30.6307578244591));
#75090=CARTESIAN_POINT('Ctrl Pts',(204.506199788064,10.6865983859883,30.6353015241072));
#75091=CARTESIAN_POINT('Ctrl Pts',(204.505793668175,10.6923102162764,30.6368628426981));
#75092=CARTESIAN_POINT('Ctrl Pts',(204.50503434556,10.7030763376691,30.6397186575149));
#75093=CARTESIAN_POINT('Ctrl Pts',(204.504680659137,10.7081276187083,30.641022696464));
#75094=CARTESIAN_POINT('Ctrl Pts',(204.503835791482,10.7202778874684,30.6440734431089));
#75095=CARTESIAN_POINT('Ctrl Pts',(204.503346398639,10.7273847615884,30.6457876947001));
#75096=CARTESIAN_POINT('Ctrl Pts',(204.501623789972,10.7526240125976,30.6516275303393));
#75097=CARTESIAN_POINT('Ctrl Pts',(204.500408692096,10.7708386157387,30.655389976436));
#75098=CARTESIAN_POINT('Ctrl Pts',(204.497297648052,10.8182915405941,30.6640254743173));
#75099=CARTESIAN_POINT('Ctrl Pts',(204.495426641045,10.8476390295869,30.6682292694141));
#75100=CARTESIAN_POINT('Ctrl Pts',(204.487523861422,10.9733374894133,30.6814164112386));
#75101=CARTESIAN_POINT('Ctrl Pts',(204.481661909588,11.0704308629258,30.6796163736572));
#75102=CARTESIAN_POINT('Ctrl Pts',(204.474023883215,11.1878534656056,30.6628774906809));
#75103=CARTESIAN_POINT('Ctrl Pts',(204.472600695937,11.2094047910487,30.6591904593781));
#75104=CARTESIAN_POINT('Ctrl Pts',(204.470416310092,11.2418881050987,30.6526977677804));
#75105=CARTESIAN_POINT('Ctrl Pts',(204.469668656499,11.2529036117014,30.6503311471025));
#75106=CARTESIAN_POINT('Ctrl Pts',(204.468304134126,11.272810370177,30.645754542507));
#75107=CARTESIAN_POINT('Ctrl Pts',(204.467688991975,11.2817131062426,30.6435981319967));
#75108=CARTESIAN_POINT('Ctrl Pts',(204.46634805724,11.3009595690559,30.6386979002208));
#75109=CARTESIAN_POINT('Ctrl Pts',(204.465621123966,11.3112927935014,30.6359165259502));
#75110=CARTESIAN_POINT('Ctrl Pts',(204.463546764024,11.3404865582047,30.6276302411897));
#75111=CARTESIAN_POINT('Ctrl Pts',(204.462188993247,11.3592484873497,30.6217938769279));
#75112=CARTESIAN_POINT('Ctrl Pts',(204.459057046591,11.4017200237634,30.6074073265689));
#75113=CARTESIAN_POINT('Ctrl Pts',(204.457274372454,11.4253181903111,30.5985600804324));
#75114=CARTESIAN_POINT('Ctrl Pts',(204.450615775465,11.5113982158899,30.5630982546894));
#75115=CARTESIAN_POINT('Ctrl Pts',(204.445621875268,11.5718244254159,30.5318533729823));
#75116=CARTESIAN_POINT('Ctrl Pts',(204.436977362713,11.6716886138843,30.4687383079762));
#75117=CARTESIAN_POINT('Ctrl Pts',(204.433326630719,11.7124043028962,30.4392021364571));
#75118=CARTESIAN_POINT('Ctrl Pts',(204.429121042398,11.7586677153507,30.4008965438966));
#75119=CARTESIAN_POINT('Ctrl Pts',(204.428439463496,11.7661451169688,30.3945462315567));
#75120=CARTESIAN_POINT('Ctrl Pts',(204.427369443249,11.7778642775782,30.3843387780364));
#75121=CARTESIAN_POINT('Ctrl Pts',(204.426976964063,11.7821585383281,30.3805429762643));
#75122=CARTESIAN_POINT('Ctrl Pts',(204.426224165178,11.790390030381,30.3731592256754));
#75123=CARTESIAN_POINT('Ctrl Pts',(204.42586357981,11.7943308738264,30.3695756997327));
#75124=CARTESIAN_POINT('Ctrl Pts',(204.424973120861,11.8040538041751,30.3606130987966));
#75125=CARTESIAN_POINT('Ctrl Pts',(204.424445532006,11.8098064879895,30.3552022487109));
#75126=CARTESIAN_POINT('Ctrl Pts',(204.422395599075,11.8321038574246,30.3338030694266));
#75127=CARTESIAN_POINT('Ctrl Pts',(204.420901667475,11.8482341201247,30.317388173009));
#75128=CARTESIAN_POINT('Ctrl Pts',(204.416778776716,11.8920152867722,30.2701415163189));
#75129=CARTESIAN_POINT('Ctrl Pts',(204.414199423287,11.9185372869186,30.238308152145));
#75130=CARTESIAN_POINT('Ctrl Pts',(204.406279980061,11.9949899273806,30.1360309127493));
#75131=CARTESIAN_POINT('Ctrl Pts',(204.400982168585,12.0388945956149,30.0614593749804));
#75132=CARTESIAN_POINT('Ctrl Pts',(204.394240122505,12.0814877453746,29.9666800598424));
#75133=CARTESIAN_POINT('Ctrl Pts',(204.39308534383,12.088353533864,29.9504359610527));
#75134=CARTESIAN_POINT('Ctrl Pts',(204.391231512937,12.098678702535,29.9243913290238));
#75135=CARTESIAN_POINT('Ctrl Pts',(204.390540361116,12.1023776808149,29.9146882310558));
#75136=CARTESIAN_POINT('Ctrl Pts',(204.389230013585,12.1091051380097,29.8963145020388));
#75137=CARTESIAN_POINT('Ctrl Pts',(204.388611784007,12.1121614564469,29.8876548443636));
#75138=CARTESIAN_POINT('Ctrl Pts',(204.387199105754,12.1188769449826,29.8678940807945));
#75139=CARTESIAN_POINT('Ctrl Pts',(204.386402675847,12.1224726985126,29.8567726122705));
#75140=CARTESIAN_POINT('Ctrl Pts',(204.38388570204,12.1332391259366,29.8216975213308));
#75141=CARTESIAN_POINT('Ctrl Pts',(204.382146591257,12.1398125036699,29.7975693319459));
#75142=CARTESIAN_POINT('Ctrl Pts',(204.377905842197,12.1537776953688,29.7390200180092));
#75143=CARTESIAN_POINT('Ctrl Pts',(204.375384110328,12.1604035985836,29.704442315802));
#75144=CARTESIAN_POINT('Ctrl Pts',(204.371726201364,12.1676713334131,29.6545058840086));
#75145=CARTESIAN_POINT('Ctrl Pts',(204.370613920137,12.1695770324573,29.6393483319633));
#75146=CARTESIAN_POINT('Ctrl Pts',(204.364423258903,12.1785130936366,29.5550543202146));
#75147=CARTESIAN_POINT('Ctrl Pts',(204.359281618865,12.1797086750246,29.4854362752628));
#75148=CARTESIAN_POINT('Ctrl Pts',(204.352907200928,12.173357620497,29.3964909665236));
#75149=CARTESIAN_POINT('Ctrl Pts',(204.35151623384,12.1714644858877,29.3769013034547));
#75150=CARTESIAN_POINT('Ctrl Pts',(204.349614468664,12.1681522977836,29.3497531863812));
#75151=CARTESIAN_POINT('Ctrl Pts',(204.349084582911,12.1671489888399,29.3421483561042));
#75152=CARTESIAN_POINT('Ctrl Pts',(204.348200036601,12.165336838816,29.3293762641083));
#75153=CARTESIAN_POINT('Ctrl Pts',(204.34784329957,12.1645677601495,29.3242036874267));
#75154=CARTESIAN_POINT('Ctrl Pts',(204.347096619893,12.1628766886828,29.3133285397174));
#75155=CARTESIAN_POINT('Ctrl Pts',(204.346707085192,12.1619471601479,29.3076273727663));
#75156=CARTESIAN_POINT('Ctrl Pts',(204.34564465038,12.1592827137057,29.2920096295967));
#75157=CARTESIAN_POINT('Ctrl Pts',(204.344976216975,12.1574624955683,29.2821078424359));
#75158=CARTESIAN_POINT('Ctrl Pts',(204.34012046097,12.1431968627417,29.2097358231912));
#75159=CARTESIAN_POINT('Ctrl Pts',(204.336160702075,12.1258269466844,29.1483351257714));
#75160=CARTESIAN_POINT('Ctrl Pts',(204.327127904238,12.074908913771,29.0117370654091));
#75161=CARTESIAN_POINT('Ctrl Pts',(204.322075742681,12.0382896372784,28.9380544029841));
#75162=CARTESIAN_POINT('Ctrl Pts',(204.315588171637,11.9846576902123,28.8535723292387));
#75163=CARTESIAN_POINT('Ctrl Pts',(204.314409377392,11.974656844726,28.8385897791776));
#75164=CARTESIAN_POINT('Ctrl Pts',(204.312526326095,11.9583121467903,28.8152794121022));
#75165=CARTESIAN_POINT('Ctrl Pts',(204.31183043347,11.9521938712117,28.806796368924));
#75166=CARTESIAN_POINT('Ctrl Pts',(204.310522725908,11.9405576354677,28.791107379467));
#75167=CARTESIAN_POINT('Ctrl Pts',(204.309912015226,11.9350677556221,28.7838815058672));
#75168=CARTESIAN_POINT('Ctrl Pts',(204.308520137631,11.9224340268286,28.7676457634479));
#75169=CARTESIAN_POINT('Ctrl Pts',(204.307737080301,11.9152407256599,28.7586757392233));
#75170=CARTESIAN_POINT('Ctrl Pts',(204.3053067895,11.8926611795702,28.73134874348));
#75171=CARTESIAN_POINT('Ctrl Pts',(204.303642749872,11.8768462267564,28.7133556787146));
#75172=CARTESIAN_POINT('Ctrl Pts',(204.299629325177,11.837890852275,28.6716703727502));
#75173=CARTESIAN_POINT('Ctrl Pts',(204.297262655316,11.8142789620539,28.648448175744));
#75174=CARTESIAN_POINT('Ctrl Pts',(204.291506543989,11.755234017991,28.5950813708977));
#75175=CARTESIAN_POINT('Ctrl Pts',(204.288094326118,11.7189320233866,28.5659804464613));
#75176=CARTESIAN_POINT('Ctrl Pts',(204.280823855644,11.6380105098521,28.5086297599253));
#75177=CARTESIAN_POINT('Ctrl Pts',(204.276974534597,11.5930129744244,28.4810746042428));
#75178=CARTESIAN_POINT('Ctrl Pts',(204.272376929497,11.5352478572156,28.4508284592319));
#75179=CARTESIAN_POINT('Ctrl Pts',(204.271503771116,11.5240862654587,28.4452086426314));
#75180=CARTESIAN_POINT('Ctrl Pts',(204.270206900487,11.5071900733611,28.4370359187963));
#75181=CARTESIAN_POINT('Ctrl Pts',(204.269775948708,11.5015214381559,28.434349653983));
#75182=CARTESIAN_POINT('Ctrl Pts',(204.268998162646,11.4911873108329,28.4295532229692));
#75183=CARTESIAN_POINT('Ctrl Pts',(204.268650488276,11.4865292862608,28.4274280759828));
#75184=CARTESIAN_POINT('Ctrl Pts',(204.267846729463,11.4756722661313,28.4225600236078));
#75185=CARTESIAN_POINT('Ctrl Pts',(204.267391994105,11.4694632548893,28.4198401667947));
#75186=CARTESIAN_POINT('Ctrl Pts',(204.265924122469,11.4492180507266,28.411179306674));
#75187=CARTESIAN_POINT('Ctrl Pts',(204.264922739257,11.4350893387576,28.4054568630078));
#75188=CARTESIAN_POINT('Ctrl Pts',(204.258345572308,11.3405077118606,28.3692702274533));
#75189=CARTESIAN_POINT('Ctrl Pts',(204.25312642971,11.2570277139934,28.3474222297287));
#75190=CARTESIAN_POINT('Ctrl Pts',(204.244231415542,11.1156167382245,28.3265584344973));
#75191=CARTESIAN_POINT('Ctrl Pts',(204.240646943057,11.058807524477,28.322344320574));
#75192=CARTESIAN_POINT('Ctrl Pts',(204.235935295069,10.9865590564877,28.3222265188801));
#75193=CARTESIAN_POINT('Ctrl Pts',(204.234925193039,10.9711993712725,28.3225020083185));
#75194=CARTESIAN_POINT('Ctrl Pts',(204.233254494822,10.9460388005098,28.3234458589001));
#75195=CARTESIAN_POINT('Ctrl Pts',(204.232599365507,10.9362328234938,28.3239365682666));
#75196=CARTESIAN_POINT('Ctrl Pts',(204.231312439351,10.9170952848175,28.325134292428));
#75197=CARTESIAN_POINT('Ctrl Pts',(204.230681036085,10.907763735471,28.325830044027));
#75198=CARTESIAN_POINT('Ctrl Pts',(204.22916693346,10.8855308215203,28.3277543734305));
#75199=CARTESIAN_POINT('Ctrl Pts',(204.228281169237,10.8726397385016,28.3290848269138));
#75200=CARTESIAN_POINT('Ctrl Pts',(204.22508806256,10.8265967731223,28.3346061106229));
#75201=CARTESIAN_POINT('Ctrl Pts',(204.22274485365,10.7936072879412,28.3399942792959));
#75202=CARTESIAN_POINT('Ctrl Pts',(204.216420672344,10.7066693616982,28.3580197395405));
#75203=CARTESIAN_POINT('Ctrl Pts',(204.212380613469,10.65330986838,28.3730720118885));
#75204=CARTESIAN_POINT('Ctrl Pts',(204.203631289139,10.5410138016058,28.4134827070862));
#75205=CARTESIAN_POINT('Ctrl Pts',(204.198928860319,10.4826759569628,28.4400163528347));
#75206=CARTESIAN_POINT('Ctrl Pts',(204.193570689384,10.4162452711662,28.4770284121859));
#75207=CARTESIAN_POINT('Ctrl Pts',(204.192728490488,10.4058022506269,28.4830587454804));
#75208=CARTESIAN_POINT('Ctrl Pts',(204.19146244962,10.39007627934,28.4924647045212));
#75209=CARTESIAN_POINT('Ctrl Pts',(204.191032031073,10.3847249487371,28.4957236772754));
#75210=CARTESIAN_POINT('Ctrl Pts',(204.190251186479,10.3750033523339,28.5017510277007));
#75211=CARTESIAN_POINT('Ctrl Pts',(204.189899966324,10.3706250968491,28.5045056236173));
#75212=CARTESIAN_POINT('Ctrl Pts',(204.189089486471,10.3605105440549,28.5109626372211));
#75213=CARTESIAN_POINT('Ctrl Pts',(204.188631582506,10.3547881010653,28.514686202123));
#75214=CARTESIAN_POINT('Ctrl Pts',(204.18714186702,10.336158999619,28.5270399612884));
#75215=CARTESIAN_POINT('Ctrl Pts',(204.186122297674,10.3233900014001,28.5358760062349));
#75216=CARTESIAN_POINT('Ctrl Pts',(204.183633203972,10.2922933699872,28.5583168382468));
#75217=CARTESIAN_POINT('Ctrl Pts',(204.182177797436,10.2741789379744,28.5722070501096));
#75218=CARTESIAN_POINT('Ctrl Pts',(204.174928251564,10.1850764330714,28.6447390773026));
#75219=CARTESIAN_POINT('Ctrl Pts',(204.169367996765,10.1207357642974,28.7110341144688));
#75220=CARTESIAN_POINT('Ctrl Pts',(204.161468371099,10.0450624434254,28.8098979704313));
#75221=CARTESIAN_POINT('Ctrl Pts',(204.159382572204,10.0264264430857,28.8364483460071));
#75222=CARTESIAN_POINT('Ctrl Pts',(204.156394129913,10.0018017531591,28.8748052513019));
#75223=CARTESIAN_POINT('Ctrl Pts',(204.155525123391,9.99487921469159,28.8859964184365));
#75224=CARTESIAN_POINT('Ctrl Pts',(204.154030610076,9.98338809670228,28.9052885241774));
#75225=CARTESIAN_POINT('Ctrl Pts',(204.153408527385,9.97872520973934,28.9133320395185));
#75226=CARTESIAN_POINT('Ctrl Pts',(204.15212813132,9.96937612431642,28.9299085619115));
#75227=CARTESIAN_POINT('Ctrl Pts',(204.151469541064,9.96469952930371,28.9384461321075));
#75228=CARTESIAN_POINT('Ctrl Pts',(204.149789657626,9.9531079909186,28.9602446530653));
#75229=CARTESIAN_POINT('Ctrl Pts',(204.148763436784,9.94633899082173,28.9735808175985));
#75230=CARTESIAN_POINT('Ctrl Pts',(204.143949116277,9.91603758825061,29.0362072755362));
#75231=CARTESIAN_POINT('Ctrl Pts',(204.140056653699,9.89570132312146,29.0869610898323));
#75232=CARTESIAN_POINT('Ctrl Pts',(204.131732373736,9.86054078064419,29.1961283208153));
#75233=CARTESIAN_POINT('Ctrl Pts',(204.127296777677,9.8465242743122,29.2546457658897));
#75234=CARTESIAN_POINT('Ctrl Pts',(204.121446219523,9.83383472865169,29.3339760672685));
#75235=CARTESIAN_POINT('Ctrl Pts',(204.119979435993,9.83115164405392,29.354058315545));
#75236=CARTESIAN_POINT('Ctrl Pts',(204.116999983028,9.82671004016305,29.3954032695704));
#75237=CARTESIAN_POINT('Ctrl Pts',(204.115489471811,9.82500838341042,29.4166655094815));
#75238=CARTESIAN_POINT('Ctrl Pts',(204.1134667947,9.8234774545883,29.4456896073132));
#75239=CARTESIAN_POINT('Ctrl Pts',(204.112931883378,9.82314606023393,29.453419628203));
#75240=CARTESIAN_POINT('Ctrl Pts',(204.11204068262,9.82271770775898,29.4663990733415));
#75241=CARTESIAN_POINT('Ctrl Pts',(204.111682272025,9.82257963375483,29.4716468161139));
#75242=CARTESIAN_POINT('Ctrl Pts',(204.111039268964,9.82239385946823,29.4811148265866));
#75243=CARTESIAN_POINT('Ctrl Pts',(204.110753978788,9.82233374819688,29.485334641075));
#75244=CARTESIAN_POINT('Ctrl Pts',(204.110240427777,9.82226609048611,29.4929630738052));
#75245=CARTESIAN_POINT('Ctrl Pts',(204.110011756713,9.82225065704661,29.496371537964));
#75246=CARTESIAN_POINT('Ctrl Pts',(204.109783827458,9.82225002053532,29.4997800660184));
#75247=CARTESIAN_POINT('Ctrl Pts',(204.10978386549,9.82225002064167,29.4997794972763));
#75248=CARTESIAN_POINT('Ctrl Pts',(204.109493826047,9.82224920858832,29.5041168396691));
#75249=CARTESIAN_POINT('Ctrl Pts',(204.109204990594,9.82227235645611,29.5084542433456));
#75250=CARTESIAN_POINT('Ctrl Pts',(204.108379855853,9.82240746594007,29.520893416986));
#75251=CARTESIAN_POINT('Ctrl Pts',(204.107846393483,9.82257907222981,29.5289944467413));
#75252=CARTESIAN_POINT('Ctrl Pts',(204.101471028651,9.82564897302465,29.6264185570605));
#75253=CARTESIAN_POINT('Ctrl Pts',(204.09605367425,9.83862196096357,29.7151449027121));
#75254=CARTESIAN_POINT('Ctrl Pts',(204.088069294272,9.8714905643461,29.8392354012598));
#75255=CARTESIAN_POINT('Ctrl Pts',(204.085625935575,9.88333385118579,29.876391552533));
#75256=CARTESIAN_POINT('Ctrl Pts',(204.081419446639,9.90639465079352,29.9379966397552));
#75257=CARTESIAN_POINT('Ctrl Pts',(204.079683576393,9.91664662027715,29.9627731652066));
#75258=CARTESIAN_POINT('Ctrl Pts',(204.077131784329,9.93269249009064,29.9980897641917));
#75259=CARTESIAN_POINT('Ctrl Pts',(204.076337999482,9.93781677914765,30.0089258511647));
#75260=CARTESIAN_POINT('Ctrl Pts',(204.074924237649,9.9471701139909,30.0279480570959));
#75261=CARTESIAN_POINT('Ctrl Pts',(204.074306603485,9.95133156268224,30.0361664110164));
#75262=CARTESIAN_POINT('Ctrl Pts',(204.072997524398,9.96030649845121,30.053386549645));
#75263=CARTESIAN_POINT('Ctrl Pts',(204.072305374689,9.9651414476128,30.0623762226366));
#75264=CARTESIAN_POINT('Ctrl Pts',(204.070431971251,9.97846348767142,30.0863923763004));
#75265=CARTESIAN_POINT('Ctrl Pts',(204.06924331685,9.98716473063975,30.1012965391982));
#75266=CARTESIAN_POINT('Ctrl Pts',(204.063826114451,10.027910747529,30.1676943165029));
#75267=CARTESIAN_POINT('Ctrl Pts',(204.059474275311,10.0635499361904,30.2168136609253));
#75268=CARTESIAN_POINT('Ctrl Pts',(204.05505724195,10.1027693394584,30.2629365663567));
#75269=CARTESIAN_POINT('',(204.012132885318,9.82225017882538,29.4993509829379));
#75270=CARTESIAN_POINT('Ctrl Pts',(203.956022491041,10.1027690874833,30.2629362700282));
#75271=CARTESIAN_POINT('Ctrl Pts',(203.958632079741,10.0778189126353,30.2335942803683));
#75272=CARTESIAN_POINT('Ctrl Pts',(203.961241668442,10.0543454181236,30.2030692919077));
#75273=CARTESIAN_POINT('Ctrl Pts',(203.963851257142,10.0324550016372,30.1715294026647));
#75274=CARTESIAN_POINT('Ctrl Pts',(203.967065387968,10.005493410941,30.1326829245767));
#75275=CARTESIAN_POINT('Ctrl Pts',(203.970279518795,9.98081770306318,30.0921278837912));
#75276=CARTESIAN_POINT('Ctrl Pts',(203.973493649621,9.95864549626695,30.0501598495482));
#75277=CARTESIAN_POINT('Ctrl Pts',(203.976713585924,9.93643324124246,30.0081160111496));
#75278=CARTESIAN_POINT('Ctrl Pts',(203.979933522228,9.91673389153112,29.9646544914047));
#75279=CARTESIAN_POINT('Ctrl Pts',(203.983153458532,9.89972341279482,29.9201029566048));
#75280=CARTESIAN_POINT('Ctrl Pts',(203.986357215351,9.88279840803636,29.8757752836349));
#75281=CARTESIAN_POINT('Ctrl Pts',(203.989560972171,9.86853554105832,29.8303690191676));
#75282=CARTESIAN_POINT('Ctrl Pts',(203.992764728991,9.85706155550171,29.7842301437002));
#75283=CARTESIAN_POINT('Ctrl Pts',(203.995992755036,9.84550065175501,29.7377417551949));
#75284=CARTESIAN_POINT('Ctrl Pts',(203.999220781082,9.83677128654062,29.6905101206683));
#75285=CARTESIAN_POINT('Ctrl Pts',(204.002448807127,9.83095203688582,29.6429052918495));
#75286=CARTESIAN_POINT('Ctrl Pts',(204.005676833173,9.82513278723102,29.5953004630307));
#75287=CARTESIAN_POINT('Ctrl Pts',(204.008904859218,9.82222374314532,29.547322997184));
#75288=CARTESIAN_POINT('Ctrl Pts',(204.012132885264,9.82225017882494,29.499350983736));
#75289=CARTESIAN_POINT('Ctrl Pts',(204.012132885318,9.82225017882538,29.4993509829379));
#75290=CARTESIAN_POINT('Ctrl Pts',(204.015663251205,9.82227909053024,29.4468858672742));
#75291=CARTESIAN_POINT('Ctrl Pts',(204.019193617093,9.82581787908988,29.3945447125145));
#75292=CARTESIAN_POINT('Ctrl Pts',(204.022723982981,9.8327924956972,29.3427686278148));
#75293=CARTESIAN_POINT('Ctrl Pts',(204.026279617378,9.8398170329567,29.2906219570227));
#75294=CARTESIAN_POINT('Ctrl Pts',(204.029835251775,9.8503266225995,29.2390487802656));
#75295=CARTESIAN_POINT('Ctrl Pts',(204.033390886173,9.8641956238876,29.1884819721045));
#75296=CARTESIAN_POINT('Ctrl Pts',(204.036428309407,9.87604330619742,29.1452849555299));
#75297=CARTESIAN_POINT('Ctrl Pts',(204.039465732642,9.8903416381416,29.1028221357794));
#75298=CARTESIAN_POINT('Ctrl Pts',(204.042503155876,9.90698494103074,29.0613507741185));
#75299=CARTESIAN_POINT('Ctrl Pts',(204.045780318324,9.92494187459465,29.0166061407299));
#75300=CARTESIAN_POINT('Ctrl Pts',(204.049057480771,9.94569139827068,28.972865032023));
#75301=CARTESIAN_POINT('Ctrl Pts',(204.052334643218,9.96909668806319,28.9304972134065));
#75302=CARTESIAN_POINT('Ctrl Pts',(204.055508599211,9.99176488379466,28.8894636686982));
#75303=CARTESIAN_POINT('Ctrl Pts',(204.058682555204,10.0169237484024,28.8497187236338));
#75304=CARTESIAN_POINT('Ctrl Pts',(204.061856511196,10.0443999796418,28.8115788617486));
#75305=CARTESIAN_POINT('Ctrl Pts',(204.065027342179,10.071849158366,28.7734765515635));
#75306=CARTESIAN_POINT('Ctrl Pts',(204.068198173162,10.1016108634411,28.7369766463296));
#75307=CARTESIAN_POINT('Ctrl Pts',(204.071369004145,10.133467691192,28.7023679919337));
#75308=CARTESIAN_POINT('Ctrl Pts',(204.074538104651,10.1653071331192,28.6677782251675));
#75309=CARTESIAN_POINT('Ctrl Pts',(204.077707205157,10.1992390560383,28.6350780734984));
#75310=CARTESIAN_POINT('Ctrl Pts',(204.080876305663,10.2350065876053,28.6045223947564));
#75311=CARTESIAN_POINT('Ctrl Pts',(204.084045067226,10.2707702937499,28.5739699840169));
#75312=CARTESIAN_POINT('Ctrl Pts',(204.087213828789,10.308368794137,28.5455619505807));
#75313=CARTESIAN_POINT('Ctrl Pts',(204.090382590352,10.3475113074931,28.5195136060859));
#75314=CARTESIAN_POINT('Ctrl Pts',(204.093554538174,10.3866931795006,28.4934390694122));
#75315=CARTESIAN_POINT('Ctrl Pts',(204.096726485996,10.4274216967813,28.4697292630943));
#75316=CARTESIAN_POINT('Ctrl Pts',(204.099898433818,10.4693778685642,28.4485556523855));
#75317=CARTESIAN_POINT('Ctrl Pts',(204.103072326411,10.511359764341,28.4273690598004));
#75318=CARTESIAN_POINT('Ctrl Pts',(204.106246219005,10.5545703010809,28.4087219777471));
#75319=CARTESIAN_POINT('Ctrl Pts',(204.109420111598,10.5986700278209,28.3927379190405));
#75320=CARTESIAN_POINT('Ctrl Pts',(204.112599619276,10.6428477734905,28.3767255821734));
#75321=CARTESIAN_POINT('Ctrl Pts',(204.115779126955,10.6879173127942,28.3633858205434));
#75322=CARTESIAN_POINT('Ctrl Pts',(204.118958634633,10.7335254625529,28.352791918006));
#75323=CARTESIAN_POINT('Ctrl Pts',(204.119690774625,10.7440275760287,28.3503524775291));
#75324=CARTESIAN_POINT('Ctrl Pts',(204.120422914618,10.754558218417,28.3480584158965));
#75325=CARTESIAN_POINT('Ctrl Pts',(204.121155054611,10.7651130357751,28.3459102389601));
#75326=CARTESIAN_POINT('Ctrl Pts',(204.124432217058,10.812357895264,28.336294694316));
#75327=CARTESIAN_POINT('Ctrl Pts',(204.127709379505,10.8603007492285,28.3295633197699));
#75328=CARTESIAN_POINT('Ctrl Pts',(204.130986541953,10.9085575354729,28.3258052383948));
#75329=CARTESIAN_POINT('Ctrl Pts',(204.134160503933,10.9552946769115,28.3221655020087));
#75330=CARTESIAN_POINT('Ctrl Pts',(204.137334465913,11.0023256673031,28.3213146073809));
#75331=CARTESIAN_POINT('Ctrl Pts',(204.140508427893,11.0492908750336,28.3232819062586));
#75332=CARTESIAN_POINT('Ctrl Pts',(204.143679264962,11.0962098433739,28.3252472682408));
#75333=CARTESIAN_POINT('Ctrl Pts',(204.146850102032,11.1430626033167,28.3300253084613));
#75334=CARTESIAN_POINT('Ctrl Pts',(204.150020939101,11.1894883463443,28.3375933460704));
#75335=CARTESIAN_POINT('Ctrl Pts',(204.15319004578,11.2358887538872,28.3451572536455));
#75336=CARTESIAN_POINT('Ctrl Pts',(204.156359152458,11.2818620574893,28.3555080528606));
#75337=CARTESIAN_POINT('Ctrl Pts',(204.159528259136,11.3270541233728,28.3685714061927));
#75338=CARTESIAN_POINT('Ctrl Pts',(204.162697026945,11.3722413569009,28.3816333626697));
#75339=CARTESIAN_POINT('Ctrl Pts',(204.165865794753,11.4166469845708,28.3974071406536));
#75340=CARTESIAN_POINT('Ctrl Pts',(204.169034562561,11.4599312472217,28.4157683317994));
#75341=CARTESIAN_POINT('Ctrl Pts',(204.172206516686,11.5032590338526,28.4341479858244));
#75342=CARTESIAN_POINT('Ctrl Pts',(204.175378470811,11.5454626930871,28.4551200244726));
#75343=CARTESIAN_POINT('Ctrl Pts',(204.178550424936,11.5862235665511,28.4785123630116));
#75344=CARTESIAN_POINT('Ctrl Pts',(204.181724323873,11.6270094316214,28.5019190440331));
#75345=CARTESIAN_POINT('Ctrl Pts',(204.18489822281,11.6663502850955,28.5277486722163));
#75346=CARTESIAN_POINT('Ctrl Pts',(204.188072121747,11.7039562609683,28.5557856995663));
#75347=CARTESIAN_POINT('Ctrl Pts',(204.191251635763,11.741628767168,28.5838723284104));
#75348=CARTESIAN_POINT('Ctrl Pts',(204.19443114978,11.777559850823,28.6141737848394));
#75349=CARTESIAN_POINT('Ctrl Pts',(204.197610663796,11.8114940402065,28.6464354241129));
#75350=CARTESIAN_POINT('Ctrl Pts',(204.198342760312,11.8193075304778,28.653863802665));
#75351=CARTESIAN_POINT('Ctrl Pts',(204.199074856829,11.8270153154154,28.6613959601647));
#75352=CARTESIAN_POINT('Ctrl Pts',(204.199806953345,11.8346145781743,28.6690285393596));
#75353=CARTESIAN_POINT('Ctrl Pts',(204.203084115792,11.8686319761315,28.7031950752653));
#75354=CARTESIAN_POINT('Ctrl Pts',(204.206361278239,11.9006246662942,28.7395309886941));
#75355=CARTESIAN_POINT('Ctrl Pts',(204.209638440687,11.9303069551227,28.7777645593365));
#75356=CARTESIAN_POINT('Ctrl Pts',(204.212812355243,11.9590540953993,28.8147935709767));
#75357=CARTESIAN_POINT('Ctrl Pts',(204.2159862698,11.9856338928332,28.8536019554062));
#75358=CARTESIAN_POINT('Ctrl Pts',(204.219160184356,12.009824020999,28.8939055278973));
#75359=CARTESIAN_POINT('Ctrl Pts',(204.222330974031,12.0339903327477,28.9341694194622));
#75360=CARTESIAN_POINT('Ctrl Pts',(204.225501763707,12.0557713468835,28.9759251098867));
#75361=CARTESIAN_POINT('Ctrl Pts',(204.228672553382,12.0749875432816,29.0188588104419));
#75362=CARTESIAN_POINT('Ctrl Pts',(204.231841612791,12.094193253605,29.0617690825318));
#75363=CARTESIAN_POINT('Ctrl Pts',(204.2350106722,12.110836691774,29.1058555838299));
#75364=CARTESIAN_POINT('Ctrl Pts',(204.238179731609,12.1247851490231,29.1507816857078));
#75365=CARTESIAN_POINT('Ctrl Pts',(204.241348452368,12.138732115721,29.1957029867213));
#75366=CARTESIAN_POINT('Ctrl Pts',(204.244517173128,12.1499845104401,29.2414631779945));
#75367=CARTESIAN_POINT('Ctrl Pts',(204.247685893887,12.1584593468386,29.2877100939229));
#75368=CARTESIAN_POINT('Ctrl Pts',(204.250857801636,12.1669427069349,29.3340035234022));
#75369=CARTESIAN_POINT('Ctrl Pts',(204.254029709385,12.1726428363341,29.3807841053537));
#75370=CARTESIAN_POINT('Ctrl Pts',(204.257201617133,12.1755281712391,29.4276910716214));
#75371=CARTESIAN_POINT('Ctrl Pts',(204.260375470041,12.1784152755635,29.4746268033869));
#75372=CARTESIAN_POINT('Ctrl Pts',(204.263549322949,12.1784841496943,29.5216885167714));
#75373=CARTESIAN_POINT('Ctrl Pts',(204.266723175857,12.1757553646369,29.5685155823705));
#75374=CARTESIAN_POINT('Ctrl Pts',(204.269902644799,12.1730217510792,29.6154255070054));
#75375=CARTESIAN_POINT('Ctrl Pts',(204.273082113741,12.1674806730412,29.6620994038791));
#75376=CARTESIAN_POINT('Ctrl Pts',(204.276261582683,12.1592042709851,29.7081838625587));
#75377=CARTESIAN_POINT('Ctrl Pts',(204.276994005815,12.1572977172724,29.7187998881216));
#75378=CARTESIAN_POINT('Ctrl Pts',(204.277726428947,12.1552462220558,29.7293846924416));
#75379=CARTESIAN_POINT('Ctrl Pts',(204.278458852079,12.1530510414502,29.7399340707581));
#75380=CARTESIAN_POINT('Ctrl Pts',(204.281736014526,12.1432289002165,29.7871363298747));
#75381=CARTESIAN_POINT('Ctrl Pts',(204.285013176974,12.1304813671924,29.8338409394038));
#75382=CARTESIAN_POINT('Ctrl Pts',(204.288290339421,12.114878222444,29.8796598630618));
#75383=CARTESIAN_POINT('Ctrl Pts',(204.291464336444,12.0997662663612,29.9240364021023));
#75384=CARTESIAN_POINT('Ctrl Pts',(204.294638333467,12.0819760303894,29.9675816226212));
#75385=CARTESIAN_POINT('Ctrl Pts',(204.297812330489,12.0616225628927,30.0099535238206));
#75386=CARTESIAN_POINT('Ctrl Pts',(204.300983202136,12.0412891370782,30.0522837021944));
#75387=CARTESIAN_POINT('Ctrl Pts',(204.304154073783,12.0183977156809,30.0934423483772));
#75388=CARTESIAN_POINT('Ctrl Pts',(204.30732494543,11.9931116157764,30.1331069270747));
#75389=CARTESIAN_POINT('Ctrl Pts',(204.310494086156,11.9678393190922,30.1727498536028));
#75390=CARTESIAN_POINT('Ctrl Pts',(204.313663226882,11.9401752324205,30.2108998596238));
#75391=CARTESIAN_POINT('Ctrl Pts',(204.316832367608,11.9103274957914,30.2472609403054));
#75392=CARTESIAN_POINT('Ctrl Pts',(204.320001168869,11.8804829563256,30.2836181261418));
#75393=CARTESIAN_POINT('Ctrl Pts',(204.32316997013,11.8484555861549,30.318186338393));
#75394=CARTESIAN_POINT('Ctrl Pts',(204.326338771391,11.8144938508834,30.3507025504683));
#75395=CARTESIAN_POINT('Ctrl Pts',(204.329510757855,11.7804979780832,30.3832514470666));
#75396=CARTESIAN_POINT('Ctrl Pts',(204.33268274432,11.7445642648754,30.4137438438669));
#75397=CARTESIAN_POINT('Ctrl Pts',(204.335854730785,11.7069766465997,30.4419549265558));
#75398=CARTESIAN_POINT('Ctrl Pts',(204.339028661442,11.669365989896,30.4701833005503));
#75399=CARTESIAN_POINT('Ctrl Pts',(204.3422025921,11.6300998755446,30.4961272709943));
#75400=CARTESIAN_POINT('Ctrl Pts',(204.345376522757,11.5894908009597,30.5196056385112));
#75401=CARTESIAN_POINT('Ctrl Pts',(204.348556067293,11.5488098992197,30.5431255333065));
#75402=CARTESIAN_POINT('Ctrl Pts',(204.35173561183,11.5067817979646,30.5641708805389));
#75403=CARTESIAN_POINT('Ctrl Pts',(204.354915156366,11.4637413329924,30.5826075182514));
#75404=CARTESIAN_POINT('Ctrl Pts',(204.355647021181,11.45383431593,30.5868512476002));
#75405=CARTESIAN_POINT('Ctrl Pts',(204.356378885997,11.4438737289345,30.5909569686217));
#75406=CARTESIAN_POINT('Ctrl Pts',(204.357110750813,11.433863764695,30.5949234202376));
#75407=CARTESIAN_POINT('Ctrl Pts',(204.36038791326,11.3890408982376,30.6126844957851));
#75408=CARTESIAN_POINT('Ctrl Pts',(204.363665075708,11.3430245285796,30.6277287261434));
#75409=CARTESIAN_POINT('Ctrl Pts',(204.366942238155,11.2961771025132,30.6399009546653));
#75410=CARTESIAN_POINT('Ctrl Pts',(204.370116251076,11.2508042111568,30.6516900591832));
#75411=CARTESIAN_POINT('Ctrl Pts',(204.373290263998,11.2046523925093,30.6607851362038));
#75412=CARTESIAN_POINT('Ctrl Pts',(204.37646427692,11.1580705506583,30.6670941536631));
#75413=CARTESIAN_POINT('Ctrl Pts',(204.379635165468,11.111534562129,30.6733969607753));
#75414=CARTESIAN_POINT('Ctrl Pts',(204.382806054017,11.064569937647,30.6769190623471));
#75415=CARTESIAN_POINT('Ctrl Pts',(204.385976942566,11.0175358741519,30.6776194443103));
#75416=CARTESIAN_POINT('Ctrl Pts',(204.389146101151,10.9705274713647,30.6783194441611));
#75417=CARTESIAN_POINT('Ctrl Pts',(204.392315259736,10.9234502604559,30.676200765931));
#75418=CARTESIAN_POINT('Ctrl Pts',(204.39548441832,10.8766659357925,30.6712744217757));
#75419=CARTESIAN_POINT('Ctrl Pts',(204.398653238351,10.8298866089832,30.6663486038897));
#75420=CARTESIAN_POINT('Ctrl Pts',(204.401822058383,10.7834006594968,30.6586157761273));
#75421=CARTESIAN_POINT('Ctrl Pts',(204.404990878414,10.7375644207131,30.6481387674076));
#75422=CARTESIAN_POINT('Ctrl Pts',(204.40816288483,10.6916820916273,30.6376512236068));
#75423=CARTESIAN_POINT('Ctrl Pts',(204.411334891245,10.6464513199307,30.624414119431));
#75424=CARTESIAN_POINT('Ctrl Pts',(204.414506897661,10.6022160361884,30.6085409242037));
#75425=CARTESIAN_POINT('Ctrl Pts',(204.41768084898,10.5579536297547,30.5926579963887));
#75426=CARTESIAN_POINT('Ctrl Pts',(204.420854800299,10.5146884378187,30.5741359803831));
#75427=CARTESIAN_POINT('Ctrl Pts',(204.424028751618,10.4727436766404,30.5531361887132));
#75428=CARTESIAN_POINT('Ctrl Pts',(204.427208317625,10.4307247155982,30.5320992486213));
#75429=CARTESIAN_POINT('Ctrl Pts',(204.430387883632,10.3900313241586,30.5085760712266));
#75430=CARTESIAN_POINT('Ctrl Pts',(204.433567449639,10.3509597229013,30.482772497175));
#75431=CARTESIAN_POINT('Ctrl Pts',(204.434299182942,10.3419679322715,30.4768341601756));
#75432=CARTESIAN_POINT('Ctrl Pts',(204.435030916245,10.3330618999511,30.4707752177292));
#75433=CARTESIAN_POINT('Ctrl Pts',(204.435762649547,10.324244983437,30.4645984760977));
#75434=CARTESIAN_POINT('Ctrl Pts',(204.438927171542,10.2861145250704,30.4378859639348));
#75435=CARTESIAN_POINT('Ctrl Pts',(204.442091693537,10.2494829341546,30.4088476656972));
#75436=CARTESIAN_POINT('Ctrl Pts',(204.445256215531,10.2146494857929,30.3776785472681));
#75437=CARTESIAN_POINT('Ctrl Pts',(204.448415347126,10.1798753722143,30.3465625218564));
#75438=CARTESIAN_POINT('Ctrl Pts',(204.45157447872,10.1468937495134,30.3133232391173));
#75439=CARTESIAN_POINT('Ctrl Pts',(204.454733610315,10.1159730560568,30.2781975487513));
#75440=CARTESIAN_POINT('Ctrl Pts',(204.455187657379,10.111528970814,30.2731490991613));
#75441=CARTESIAN_POINT('Ctrl Pts',(204.455641704444,10.1071274017728,30.2680617496528));
#75442=CARTESIAN_POINT('Ctrl Pts',(204.456095751509,10.1027690874833,30.2629362700282));
#75443=CARTESIAN_POINT('Origin',(201.825,11.,29.5));
#75444=CARTESIAN_POINT('',(198.847155100818,9.5357120419226,29.5003329957075));
#75445=CARTESIAN_POINT('',(198.6865,11.6340070945751,30.8190402776369));
#75446=CARTESIAN_POINT('Ctrl Pts',(198.847155045843,9.5340043049682,29.5003343903779));
#75447=CARTESIAN_POINT('Ctrl Pts',(198.846037963051,9.53394303232492,29.5207934613441));
#75448=CARTESIAN_POINT('Ctrl Pts',(198.84492088026,9.53434377109394,29.541249874511));
#75449=CARTESIAN_POINT('Ctrl Pts',(198.81758649789,9.55565955034218,30.041323968822));
#75450=CARTESIAN_POINT('Ctrl Pts',(198.765151898734,10.1147327781393,30.9788657994748));
#75451=CARTESIAN_POINT('Ctrl Pts',(198.712717299578,11.1994409611895,31.0279179110948));
#75452=CARTESIAN_POINT('Ctrl Pts',(198.6865,11.6340070945751,30.8190402776369));
#75453=CARTESIAN_POINT('',(198.6865,10.3659929054241,30.8190402776365));
#75454=CARTESIAN_POINT('Origin',(198.6865,11.,29.5));
#75455=CARTESIAN_POINT('',(198.775844954157,9.53646362701638,29.5011978292248));
#75456=CARTESIAN_POINT('Ctrl Pts',(198.6865,10.3659929054241,30.8190402776365));
#75457=CARTESIAN_POINT('Ctrl Pts',(198.712748879998,9.93090330924719,30.6099110376662));
#75458=CARTESIAN_POINT('Ctrl Pts',(198.742530531383,9.56801055501681,30.1110552949604));
#75459=CARTESIAN_POINT('Ctrl Pts',(198.772312182769,9.53498328393008,29.5659452088545));
#75460=CARTESIAN_POINT('Ctrl Pts',(198.775844954157,9.53549762207678,29.5011986198501));
#75461=CARTESIAN_POINT('',(199.275844954108,9.5365000054828,29.5001266813354));
#75462=CARTESIAN_POINT('Ctrl Pts',(198.775844954157,9.53650049016837,29.5011977990542));
#75463=CARTESIAN_POINT('Ctrl Pts',(198.778791649872,9.53645632016616,29.4472298347593));
#75464=CARTESIAN_POINT('Ctrl Pts',(198.781738345587,9.53940154252127,29.3931370361555));
#75465=CARTESIAN_POINT('Ctrl Pts',(198.784685041302,9.54535112027514,29.3392863206967));
#75466=CARTESIAN_POINT('Ctrl Pts',(198.787628183599,9.55129352343638,29.2855005437868));
#75467=CARTESIAN_POINT('Ctrl Pts',(198.790571325895,9.56023305821482,29.2319568159945));
#75468=CARTESIAN_POINT('Ctrl Pts',(198.793514468191,9.57213268319622,29.1790215340501));
#75469=CARTESIAN_POINT('Ctrl Pts',(198.796455329146,9.58402308432575,29.1261272842558));
#75470=CARTESIAN_POINT('Ctrl Pts',(198.799396190101,9.59886891553508,29.0738410828827));
#75471=CARTESIAN_POINT('Ctrl Pts',(198.802337051055,9.6165817291683,29.0225210602246));
#75472=CARTESIAN_POINT('Ctrl Pts',(198.805276898398,9.63428843781035,28.9712187257945));
#75473=CARTESIAN_POINT('Ctrl Pts',(198.80821674574,9.65485999115351,28.920882430529));
#75474=CARTESIAN_POINT('Ctrl Pts',(198.811156593082,9.67815831354728,28.8718544707189));
#75475=CARTESIAN_POINT('Ctrl Pts',(198.814098759117,9.70147501160776,28.822787841968));
#75476=CARTESIAN_POINT('Ctrl Pts',(198.817040925152,9.72752254036119,28.7750321098689));
#75477=CARTESIAN_POINT('Ctrl Pts',(198.819983091187,9.75611570679522,28.7289071942247));
#75478=CARTESIAN_POINT('Ctrl Pts',(198.822926399207,9.78471997149858,28.6827643754658));
#75479=CARTESIAN_POINT('Ctrl Pts',(198.825869707226,9.81587152468746,28.6382540854398));
#75480=CARTESIAN_POINT('Ctrl Pts',(198.828813015246,9.8493424183292,28.5956663338438));
#75481=CARTESIAN_POINT('Ctrl Pts',(198.831761738694,9.88287489548651,28.5530002245113));
#75482=CARTESIAN_POINT('Ctrl Pts',(198.834710462143,9.91873486644139,28.5122641281858));
#75483=CARTESIAN_POINT('Ctrl Pts',(198.837659185592,9.95665580113758,28.4737129384523));
#75484=CARTESIAN_POINT('Ctrl Pts',(198.83977055039,9.98380820386801,28.4461092562708));
#75485=CARTESIAN_POINT('Ctrl Pts',(198.841881915188,10.0120164483374,28.4196249997495));
#75486=CARTESIAN_POINT('Ctrl Pts',(198.843993279985,10.041172772022,28.3943406506125));
#75487=CARTESIAN_POINT('Ctrl Pts',(198.847005328754,10.0827668484904,28.3582702885587));
#75488=CARTESIAN_POINT('Ctrl Pts',(198.850017377523,10.1264862950172,28.3244747310288));
#75489=CARTESIAN_POINT('Ctrl Pts',(198.853029426292,10.1720526307868,28.2932127760815));
#75490=CARTESIAN_POINT('Ctrl Pts',(198.856036078144,10.2175373218911,28.2620068355537));
#75491=CARTESIAN_POINT('Ctrl Pts',(198.859042729996,10.2648619033235,28.2333257839958));
#75492=CARTESIAN_POINT('Ctrl Pts',(198.862049381848,10.3137146782264,28.2073884159895));
#75493=CARTESIAN_POINT('Ctrl Pts',(198.865053031751,10.3625186767598,28.1814769447853));
#75494=CARTESIAN_POINT('Ctrl Pts',(198.868056681654,10.4128473825597,28.1583039762517));
#75495=CARTESIAN_POINT('Ctrl Pts',(198.871060331557,10.4643615234754,28.1380441738197));
#75496=CARTESIAN_POINT('Ctrl Pts',(198.874062164677,10.51584450563,28.1177966256995));
#75497=CARTESIAN_POINT('Ctrl Pts',(198.877063997796,10.5685110118662,28.100458943567));
#75498=CARTESIAN_POINT('Ctrl Pts',(198.880065830916,10.6220007529088,28.08615813501));
#75499=CARTESIAN_POINT('Ctrl Pts',(198.883067029728,10.6754791911956,28.0718603483136));
#75500=CARTESIAN_POINT('Ctrl Pts',(198.886068228539,10.7297800096696,28.0605982969217));
#75501=CARTESIAN_POINT('Ctrl Pts',(198.889069427351,10.7845289073962,28.052448806345));
#75502=CARTESIAN_POINT('Ctrl Pts',(198.892073285715,10.8393263215893,28.0442920939884));
#75503=CARTESIAN_POINT('Ctrl Pts',(198.895077144079,10.8945720856757,28.039253531007));
#75504=CARTESIAN_POINT('Ctrl Pts',(198.898081002443,10.9498843807075,28.0373583232032));
#75505=CARTESIAN_POINT('Ctrl Pts',(198.901086191942,11.0052211869347,28.0354622755534));
#75506=CARTESIAN_POINT('Ctrl Pts',(198.904091381442,11.0606240547654,28.0367123485731));
#75507=CARTESIAN_POINT('Ctrl Pts',(198.907096570941,11.1157120452941,28.0410815743936));
#75508=CARTESIAN_POINT('Ctrl Pts',(198.91010727564,11.1709011346923,28.0454588187275));
#75509=CARTESIAN_POINT('Ctrl Pts',(198.913117980339,11.2257736687237,28.0529665793148));
#75510=CARTESIAN_POINT('Ctrl Pts',(198.916128685038,11.2799559003873,28.0635262119209));
#75511=CARTESIAN_POINT('Ctrl Pts',(198.918332430018,11.3196156588098,28.0712555443114));
#75512=CARTESIAN_POINT('Ctrl Pts',(198.920536174999,11.3589057330949,28.0806189165104));
#75513=CARTESIAN_POINT('Ctrl Pts',(198.922739919979,11.3976850882574,28.0915686667154));
#75514=CARTESIAN_POINT('Ctrl Pts',(198.925755713335,11.4507540788644,28.1065532426153));
#75515=CARTESIAN_POINT('Ctrl Pts',(198.928771506691,11.5030816332125,28.1245715079638));
#75516=CARTESIAN_POINT('Ctrl Pts',(198.931787300047,11.5542979605813,28.1455310926804));
#75517=CARTESIAN_POINT('Ctrl Pts',(198.934797919014,11.6054264128316,28.1664547157012));
#75518=CARTESIAN_POINT('Ctrl Pts',(198.937808537981,11.6554469393322,28.1903094442393));
#75519=CARTESIAN_POINT('Ctrl Pts',(198.940819156949,11.7040051552978,28.2169532388435));
#75520=CARTESIAN_POINT('Ctrl Pts',(198.943826907058,11.7525170995114,28.2435716442313));
#75521=CARTESIAN_POINT('Ctrl Pts',(198.946834657167,11.7995690352762,28.2729735980771));
#75522=CARTESIAN_POINT('Ctrl Pts',(198.949842407277,11.8448285280044,28.3049698713966));
#75523=CARTESIAN_POINT('Ctrl Pts',(198.952848465744,11.8900625655311,28.3369481491192));
#75524=CARTESIAN_POINT('Ctrl Pts',(198.955854524211,11.9335057300886,28.3715175507233));
#75525=CARTESIAN_POINT('Ctrl Pts',(198.958860582677,11.9748540492909,28.4084452223635));
#75526=CARTESIAN_POINT('Ctrl Pts',(198.961866124186,12.0161952577378,28.445366543476));
#75527=CARTESIAN_POINT('Ctrl Pts',(198.964871665695,12.0554419447302,28.4846449787968));
#75528=CARTESIAN_POINT('Ctrl Pts',(198.967877207204,12.0923245227013,28.5260085282174));
#75529=CARTESIAN_POINT('Ctrl Pts',(198.970885554931,12.1292415372513,28.5674106980167));
#75530=CARTESIAN_POINT('Ctrl Pts',(198.973893902658,12.1637896829338,28.6109014775952));
#75531=CARTESIAN_POINT('Ctrl Pts',(198.976902250385,12.1957384829353,28.6561743483232));
#75532=CARTESIAN_POINT('Ctrl Pts',(198.979912017522,12.22770235714,28.7014685798678));
#75533=CARTESIAN_POINT('Ctrl Pts',(198.982921784659,12.257064162318,28.7485461318182));
#75534=CARTESIAN_POINT('Ctrl Pts',(198.985931551796,12.2836375865475,28.7970726947953));
#75535=CARTESIAN_POINT('Ctrl Pts',(198.988946921717,12.3102604781084,28.8456895916167));
#75536=CARTESIAN_POINT('Ctrl Pts',(198.991962291638,12.3340843938176,28.8957604118083));
#75537=CARTESIAN_POINT('Ctrl Pts',(198.994977661559,12.3549702085235,28.9469285904932));
#75538=CARTESIAN_POINT('Ctrl Pts',(198.997147294363,12.3699980657755,28.9837453532556));
#75539=CARTESIAN_POINT('Ctrl Pts',(198.999316927167,12.3835058329917,29.0211297861003));
#75540=CARTESIAN_POINT('Ctrl Pts',(199.001486559972,12.3954578171697,29.0589447534605));
#75541=CARTESIAN_POINT('Ctrl Pts',(199.004495371137,12.4120326326725,29.1113859295786));
#75542=CARTESIAN_POINT('Ctrl Pts',(199.007504182302,12.4256822793691,29.1648736097929));
#75543=CARTESIAN_POINT('Ctrl Pts',(199.010512993467,12.4362797294248,29.2190502022719));
#75544=CARTESIAN_POINT('Ctrl Pts',(199.013516438647,12.4468582797364,29.2731301749294));
#75545=CARTESIAN_POINT('Ctrl Pts',(199.016519883827,12.4543953348941,29.3278961071117));
#75546=CARTESIAN_POINT('Ctrl Pts',(199.019523329007,12.4588137565104,29.382975755435));
#75547=CARTESIAN_POINT('Ctrl Pts',(199.022523793782,12.4632277936006,29.4380007466478));
#75548=CARTESIAN_POINT('Ctrl Pts',(199.025524258558,12.4645292853747,29.4933383129887));
#75549=CARTESIAN_POINT('Ctrl Pts',(199.028524723333,12.4626925424559,29.5486083968457));
#75550=CARTESIAN_POINT('Ctrl Pts',(199.031523398684,12.4608568949383,29.6038455185937));
#75551=CARTESIAN_POINT('Ctrl Pts',(199.034522074035,12.4558867397765,29.6590147103353));
#75552=CARTESIAN_POINT('Ctrl Pts',(199.037520749386,12.4478084716962,29.7137355358491));
#75553=CARTESIAN_POINT('Ctrl Pts',(199.040518823625,12.4397318229771,29.7684453920833));
#75554=CARTESIAN_POINT('Ctrl Pts',(199.043516897864,12.4285483758565,29.822706537908));
#75555=CARTESIAN_POINT('Ctrl Pts',(199.046514972104,12.4143361450525,29.8761456085057));
#75556=CARTESIAN_POINT('Ctrl Pts',(199.049515782481,12.4001109437173,29.9296334492888));
#75557=CARTESIAN_POINT('Ctrl Pts',(199.052516592857,12.3828515726585,29.9822972040417));
#75558=CARTESIAN_POINT('Ctrl Pts',(199.055517403234,12.3626864066177,30.0337771138024));
#75559=CARTESIAN_POINT('Ctrl Pts',(199.058519582831,12.3425120395483,30.0852805129867));
#75560=CARTESIAN_POINT('Ctrl Pts',(199.061521762427,12.3194294554494,30.1355985091639));
#75561=CARTESIAN_POINT('Ctrl Pts',(199.064523942024,12.2936145477954,30.1843929074238));
#75562=CARTESIAN_POINT('Ctrl Pts',(199.067531736411,12.2677513601204,30.2332785628213));
#75563=CARTESIAN_POINT('Ctrl Pts',(199.070539530797,12.2391459153857,30.2806344749031));
#75564=CARTESIAN_POINT('Ctrl Pts',(199.073547325184,12.2080186595901,30.3261496039351));
#75565=CARTESIAN_POINT('Ctrl Pts',(199.075775950111,12.1849549227622,30.3598740338873));
#75566=CARTESIAN_POINT('Ctrl Pts',(199.078004575038,12.1605076313727,30.3925884404986));
#75567=CARTESIAN_POINT('Ctrl Pts',(199.080233199965,12.1347802346372,30.4241785915486));
#75568=CARTESIAN_POINT('Ctrl Pts',(199.083244840677,12.1000136507694,30.4668677779892));
#75569=CARTESIAN_POINT('Ctrl Pts',(199.086256481389,12.0627625870014,30.5076811369861));
#75570=CARTESIAN_POINT('Ctrl Pts',(199.089268122101,12.0232570704895,30.5463160219041));
#75571=CARTESIAN_POINT('Ctrl Pts',(199.09227444723,11.9838212817127,30.5848827157628));
#75572=CARTESIAN_POINT('Ctrl Pts',(199.095280772358,11.9421393112584,30.6212782004769));
#75573=CARTESIAN_POINT('Ctrl Pts',(199.098287097487,11.898480765214,30.6552335541095));
#75574=CARTESIAN_POINT('Ctrl Pts',(199.101290470819,11.8548650858309,30.6891555682754));
#75575=CARTESIAN_POINT('Ctrl Pts',(199.104293844151,11.8092770899249,30.7206418754746));
#75576=CARTESIAN_POINT('Ctrl Pts',(199.107297217484,11.7620211020091,30.7494623203974));
#75577=CARTESIAN_POINT('Ctrl Pts',(199.110298824626,11.7147929038641,30.7782658169165));
#75578=CARTESIAN_POINT('Ctrl Pts',(199.113300431768,11.6658991074839,30.8044062845581));
#75579=CARTESIAN_POINT('Ctrl Pts',(199.116302038911,11.6156728951277,30.8276969293499));
#75580=CARTESIAN_POINT('Ctrl Pts',(199.119303062839,11.5654564417592,30.8509830487533));
#75581=CARTESIAN_POINT('Ctrl Pts',(199.122304086767,11.5139085648906,30.8714202233517));
#75582=CARTESIAN_POINT('Ctrl Pts',(199.125305110695,11.461384832269,30.8888687074566));
#75583=CARTESIAN_POINT('Ctrl Pts',(199.128308874831,11.4088131406859,30.9063331236198));
#75584=CARTESIAN_POINT('Ctrl Pts',(199.131312638968,11.3552643148979,30.9208032309239));
#75585=CARTESIAN_POINT('Ctrl Pts',(199.134316403105,11.3011101646474,30.9321888558238));
#75586=CARTESIAN_POINT('Ctrl Pts',(199.137321543191,11.2469312077315,30.9435796961945));
#75587=CARTESIAN_POINT('Ctrl Pts',(199.140326683277,11.1921468959952,30.9518831584158));
#75588=CARTESIAN_POINT('Ctrl Pts',(199.143331823363,11.1371370863662,30.9570606265846));
#75589=CARTESIAN_POINT('Ctrl Pts',(199.146342552568,11.0820249665871,30.9622477240821));
#75590=CARTESIAN_POINT('Ctrl Pts',(199.149353281772,11.0266870394626,30.9642971944789));
#75591=CARTESIAN_POINT('Ctrl Pts',(199.152364010976,10.9715049136464,30.9632225668208));
#75592=CARTESIAN_POINT('Ctrl Pts',(199.154569287303,10.9310855243646,30.9624354316207));
#75593=CARTESIAN_POINT('Ctrl Pts',(199.15677456363,10.8907497479876,30.9599732718661));
#75594=CARTESIAN_POINT('Ctrl Pts',(199.158979839957,10.8506449528868,30.9558589629156));
#75595=CARTESIAN_POINT('Ctrl Pts',(199.161991606742,10.7958734540428,30.9502400121802));
#75596=CARTESIAN_POINT('Ctrl Pts',(199.165003373527,10.7413059434149,30.9415142471686));
#75597=CARTESIAN_POINT('Ctrl Pts',(199.168015140312,10.6873216990735,30.9297078478241));
#75598=CARTESIAN_POINT('Ctrl Pts',(199.171021608774,10.6334324242169,30.9179222183852));
#75599=CARTESIAN_POINT('Ctrl Pts',(199.174028077236,10.5801248904549,30.90306682183));
#75600=CARTESIAN_POINT('Ctrl Pts',(199.177034545698,10.5277719071787,30.885219433285));
#75601=CARTESIAN_POINT('Ctrl Pts',(199.180038072841,10.4754701424236,30.8673895053848));
#75602=CARTESIAN_POINT('Ctrl Pts',(199.183041599983,10.4241215749087,30.8465735537857));
#75603=CARTESIAN_POINT('Ctrl Pts',(199.186045127125,10.3740856613946,30.8228996525543));
#75604=CARTESIAN_POINT('Ctrl Pts',(199.189046898269,10.3240790011582,30.7992395921655));
#75605=CARTESIAN_POINT('Ctrl Pts',(199.192048669412,10.2753839495258,30.772725119322));
#75606=CARTESIAN_POINT('Ctrl Pts',(199.195050440555,10.2283395540161,30.7435322296201));
#75607=CARTESIAN_POINT('Ctrl Pts',(199.198051638403,10.1813041433144,30.7143449153434));
#75608=CARTESIAN_POINT('Ctrl Pts',(199.201052836251,10.1359192104467,30.6824804782212));
#75609=CARTESIAN_POINT('Ctrl Pts',(199.204054034099,10.0924967602004,30.6481594487497));
#75610=CARTESIAN_POINT('Ctrl Pts',(199.207057986182,10.0490344606516,30.6138069224585));
#75611=CARTESIAN_POINT('Ctrl Pts',(199.210061938265,10.007538656223,30.5769936278358));
#75612=CARTESIAN_POINT('Ctrl Pts',(199.213065890349,9.96828882932279,30.5379808814713));
#75613=CARTESIAN_POINT('Ctrl Pts',(199.216071226479,9.92902091837477,30.4989501602919));
#75614=CARTESIAN_POINT('Ctrl Pts',(199.219076562609,9.89200140066081,30.4577183604341));
#75615=CARTESIAN_POINT('Ctrl Pts',(199.22208189874,9.85747107758766,30.4145818232675));
#75616=CARTESIAN_POINT('Ctrl Pts',(199.225092834847,9.82287641261668,30.3713649078588));
#75617=CARTESIAN_POINT('Ctrl Pts',(199.228103770955,9.79078051364795,30.3262365963112));
#75618=CARTESIAN_POINT('Ctrl Pts',(199.231114707063,9.76138155605344,30.2795233160819));
#75619=CARTESIAN_POINT('Ctrl Pts',(199.233318631359,9.73986230935198,30.245330450629));
#75620=CARTESIAN_POINT('Ctrl Pts',(199.235522555654,9.71978713192138,30.2102890081123));
#75621=CARTESIAN_POINT('Ctrl Pts',(199.23772647995,9.70121767855363,30.1745344553827));
#75622=CARTESIAN_POINT('Ctrl Pts',(199.240908966812,9.67440321786568,30.1229045538666));
#75623=CARTESIAN_POINT('Ctrl Pts',(199.244091453674,9.65062931503385,30.0695931020557));
#75624=CARTESIAN_POINT('Ctrl Pts',(199.247273940537,9.63009563156702,30.0149701654933));
#75625=CARTESIAN_POINT('Ctrl Pts',(199.250449576398,9.60960615135481,29.9604648167753));
#75626=CARTESIAN_POINT('Ctrl Pts',(199.25362521226,9.59234318165365,29.9046539981085));
#75627=CARTESIAN_POINT('Ctrl Pts',(199.256800848122,9.578459727853,29.8479303158166));
#75628=CARTESIAN_POINT('Ctrl Pts',(199.259974865786,9.56458334859381,29.7912355380068));
#75629=CARTESIAN_POINT('Ctrl Pts',(199.26314888345,9.5540832325529,29.7336292250163));
#75630=CARTESIAN_POINT('Ctrl Pts',(199.266322901115,9.547063630942,29.6755225269547));
#75631=CARTESIAN_POINT('Ctrl Pts',(199.269496918779,9.5400440293311,29.617415828893));
#75632=CARTESIAN_POINT('Ctrl Pts',(199.272670936444,9.53650508507005,29.5588091690068));
#75633=CARTESIAN_POINT('Ctrl Pts',(199.275844954108,9.5365000054828,29.5001266813354));
#75634=CARTESIAN_POINT('',(199.775844954107,9.53650044565997,29.49885787631));
#75635=CARTESIAN_POINT('Ctrl Pts',(199.275844954157,9.53650000548272,29.5001266804286));
#75636=CARTESIAN_POINT('Ctrl Pts',(199.278966002871,9.5364950107009,29.4424235035644));
#75637=CARTESIAN_POINT('Ctrl Pts',(199.282087051584,9.53990702549526,29.3847749920601));
#75638=CARTESIAN_POINT('Ctrl Pts',(199.285208100298,9.5466909013332,29.3275908536872));
#75639=CARTESIAN_POINT('Ctrl Pts',(199.288336991433,9.5534918233685,29.2702630257582));
#75640=CARTESIAN_POINT('Ctrl Pts',(199.291465882567,9.56368146852732,29.2134023618349));
#75641=CARTESIAN_POINT('Ctrl Pts',(199.294594773702,9.5771632283295,29.1574101998274));
#75642=CARTESIAN_POINT('Ctrl Pts',(199.297727987064,9.59066361173449,29.1013406906634));
#75643=CARTESIAN_POINT('Ctrl Pts',(199.300861200426,9.60746503472237,29.0461425161852));
#75644=CARTESIAN_POINT('Ctrl Pts',(199.303994413788,9.62742142305117,28.9922005316061));
#75645=CARTESIAN_POINT('Ctrl Pts',(199.30713558909,9.64742852339869,28.9381214727786));
#75646=CARTESIAN_POINT('Ctrl Pts',(199.310276764392,9.67060641654856,28.8853054040128));
#75647=CARTESIAN_POINT('Ctrl Pts',(199.313417939694,9.6967616592254,28.8341155677334));
#75648=CARTESIAN_POINT('Ctrl Pts',(199.31443633311,9.70524139192979,28.8175194254534));
#75649=CARTESIAN_POINT('Ctrl Pts',(199.315454726526,9.71403372900158,28.8010940000388));
#75650=CARTESIAN_POINT('Ctrl Pts',(199.316473119942,9.72313110523733,28.7848510116154));
#75651=CARTESIAN_POINT('Ctrl Pts',(199.319484515685,9.75003210403694,28.7368203925931));
#75652=CARTESIAN_POINT('Ctrl Pts',(199.322495911428,9.77970288332518,28.6902098620291));
#75653=CARTESIAN_POINT('Ctrl Pts',(199.32550730717,9.81196895974587,28.6453570936393));
#75654=CARTESIAN_POINT('Ctrl Pts',(199.32851339067,9.84417811730354,28.6005834476239));
#75655=CARTESIAN_POINT('Ctrl Pts',(199.331519474171,9.87897318052574,28.557561834934));
#75656=CARTESIAN_POINT('Ctrl Pts',(199.334525557671,9.91613487312491,28.5166035200673));
#75657=CARTESIAN_POINT('Ctrl Pts',(199.337528691627,9.95326010298587,28.4756853931524));
#75658=CARTESIAN_POINT('Ctrl Pts',(199.340531825584,9.99274700919291,28.4368269422737));
#75659=CARTESIAN_POINT('Ctrl Pts',(199.34353495954,10.0343354438467,28.4003072179062));
#75660=CARTESIAN_POINT('Ctrl Pts',(199.34653633001,10.0758994571236,28.3638089384898));
#75661=CARTESIAN_POINT('Ctrl Pts',(199.349537700479,10.1195621570822,28.3296470108104));
#75662=CARTESIAN_POINT('Ctrl Pts',(199.352539070949,10.1650275077834,28.2980627357297));
#75663=CARTESIAN_POINT('Ctrl Pts',(199.355539861361,10.210484071654,28.2664845647628));
#75664=CARTESIAN_POINT('Ctrl Pts',(199.358540651772,10.2577421612415,28.2374833577421));
#75665=CARTESIAN_POINT('Ctrl Pts',(199.361541442184,10.3064755950602,28.2112579196159));
#75666=CARTESIAN_POINT('Ctrl Pts',(199.364544979613,10.3552536409925,28.1850084739011));
#75667=CARTESIAN_POINT('Ctrl Pts',(199.367548517043,10.4055092636874,28.1615401238871));
#75668=CARTESIAN_POINT('Ctrl Pts',(199.370552054472,10.4568917539653,28.1410056353726));
#75669=CARTESIAN_POINT('Ctrl Pts',(199.373556971309,10.5082978422191,28.1204617161675));
#75670=CARTESIAN_POINT('Ctrl Pts',(199.376561888146,10.5608313286254,28.1028545122959));
#75671=CARTESIAN_POINT('Ctrl Pts',(199.379566804983,10.6141247099964,28.0882873838615));
#75672=CARTESIAN_POINT('Ctrl Pts',(199.382577319389,10.6675173664533,28.0736931197323));
#75673=CARTESIAN_POINT('Ctrl Pts',(199.385587833795,10.7216722283061,28.0621503534102));
#75674=CARTESIAN_POINT('Ctrl Pts',(199.388598348201,10.7762110987655,28.0537113781529));
#75675=CARTESIAN_POINT('Ctrl Pts',(199.390805485446,10.8161958841069,28.0475244034077));
#75676=CARTESIAN_POINT('Ctrl Pts',(199.393012622691,10.8563868605222,28.0430046284988));
#75677=CARTESIAN_POINT('Ctrl Pts',(199.395219759936,10.8966345341256,28.0401548607936));
#75678=CARTESIAN_POINT('Ctrl Pts',(199.398231136404,10.9515477016101,28.0362666914342));
#75679=CARTESIAN_POINT('Ctrl Pts',(199.401242512873,11.0067947442693,28.0354731412825));
#75680=CARTESIAN_POINT('Ctrl Pts',(199.404253889341,11.0619976415287,28.0378137798335));
#75681=CARTESIAN_POINT('Ctrl Pts',(199.407259954687,11.1171031782137,28.0401502902331));
#75682=CARTESIAN_POINT('Ctrl Pts',(199.410266020033,11.1721642010943,28.0456099969915));
#75683=CARTESIAN_POINT('Ctrl Pts',(199.413272085379,11.2268001683379,28.0541805321404));
#75684=CARTESIAN_POINT('Ctrl Pts',(199.416275201884,11.2813825396793,28.0627426599051));
#75685=CARTESIAN_POINT('Ctrl Pts',(199.419278318388,11.3355401627154,28.0744094892951));
#75686=CARTESIAN_POINT('Ctrl Pts',(199.422281434893,11.3888969792225,28.0891168051353));
#75687=CARTESIAN_POINT('Ctrl Pts',(199.425282788647,11.4422224766638,28.103815488163));
#75688=CARTESIAN_POINT('Ctrl Pts',(199.4282841424,11.4947475916853,28.1215509801459));
#75689=CARTESIAN_POINT('Ctrl Pts',(199.431285496154,11.5461081125882,28.14220834464));
#75690=CARTESIAN_POINT('Ctrl Pts',(199.434286270619,11.5974587204478,28.1628617220766));
#75691=CARTESIAN_POINT('Ctrl Pts',(199.437287045084,11.6476446914489,28.1864356551269));
#75692=CARTESIAN_POINT('Ctrl Pts',(199.440287819549,11.6963207803285,28.2127666797031));
#75693=CARTESIAN_POINT('Ctrl Pts',(199.443291342359,11.7450414505932,28.2391218202995));
#75694=CARTESIAN_POINT('Ctrl Pts',(199.446294865169,11.7922490111345,28.2682388454497));
#75695=CARTESIAN_POINT('Ctrl Pts',(199.449298387979,11.8376232289154,28.2999085133285));
#75696=CARTESIAN_POINT('Ctrl Pts',(199.452303290915,11.8830182962553,28.3315927334937));
#75697=CARTESIAN_POINT('Ctrl Pts',(199.455308193851,11.9265779260924,28.3658316079328));
#75698=CARTESIAN_POINT('Ctrl Pts',(199.458313096787,11.968013957783,28.4023747326445));
#75699=CARTESIAN_POINT('Ctrl Pts',(199.461323598643,12.009527195645,28.4389859467613));
#75700=CARTESIAN_POINT('Ctrl Pts',(199.464334100499,12.048908555423,28.4779096156836));
#75701=CARTESIAN_POINT('Ctrl Pts',(199.467344602356,12.0859066865429,28.5188583598066));
#75702=CARTESIAN_POINT('Ctrl Pts',(199.469551868213,12.1130332971587,28.548881515123));
#75703=CARTESIAN_POINT('Ctrl Pts',(199.471759134071,12.138879554346,28.5799925085115));
#75704=CARTESIAN_POINT('Ctrl Pts',(199.473966399929,12.1633610186832,28.6120679135157));
#75705=CARTESIAN_POINT('Ctrl Pts',(199.476977703779,12.1967603156363,28.6558273864732));
#75706=CARTESIAN_POINT('Ctrl Pts',(199.47998900763,12.22775667217,28.7015649777552));
#75707=CARTESIAN_POINT('Ctrl Pts',(199.483000311481,12.2561094566838,28.7489864962403));
#75708=CARTESIAN_POINT('Ctrl Pts',(199.486006301957,12.284412213379,28.796324340576));
#75709=CARTESIAN_POINT('Ctrl Pts',(199.489012292434,12.310080386523,28.8453397662176));
#75710=CARTESIAN_POINT('Ctrl Pts',(199.49201828291,12.3329153668911,28.8957079557816));
#75711=CARTESIAN_POINT('Ctrl Pts',(199.495021323225,12.3557279363834,28.9460267126237));
#75712=CARTESIAN_POINT('Ctrl Pts',(199.49802436354,12.3757126047435,28.9976951250544));
#75713=CARTESIAN_POINT('Ctrl Pts',(199.501027403855,12.392716556171,29.0503636534184));
#75714=CARTESIAN_POINT('Ctrl Pts',(199.50402868024,12.4097105197968,29.103001245278));
#75715=CARTESIAN_POINT('Ctrl Pts',(199.507029956626,12.4237270751371,29.1566372875299));
#75716=CARTESIAN_POINT('Ctrl Pts',(199.510031233011,12.4346623019812,29.2109042904607));
#75717=CARTESIAN_POINT('Ctrl Pts',(199.513031929071,12.4455954143938,29.2651608003435));
#75718=CARTESIAN_POINT('Ctrl Pts',(199.51603262513,12.453448277553,29.3200475116519));
#75719=CARTESIAN_POINT('Ctrl Pts',(199.51903332119,12.4581679431271,29.3751861400463));
#75720=CARTESIAN_POINT('Ctrl Pts',(199.522036764616,12.4628919299148,29.4303752520582));
#75721=CARTESIAN_POINT('Ctrl Pts',(199.525040208041,12.4644769431849,29.4858162151371));
#75722=CARTESIAN_POINT('Ctrl Pts',(199.528043651467,12.4629220279571,29.5411265135622));
#75723=CARTESIAN_POINT('Ctrl Pts',(199.531048474355,12.461366398567,29.5964622156431));
#75724=CARTESIAN_POINT('Ctrl Pts',(199.534053297242,12.4566680107546,29.6516666068551));
#75725=CARTESIAN_POINT('Ctrl Pts',(199.537058120129,12.4488779219585,29.7063613754104));
#75726=CARTESIAN_POINT('Ctrl Pts',(199.540068541841,12.4410733180506,29.7611580555994));
#75727=CARTESIAN_POINT('Ctrl Pts',(199.543078963553,12.4301656101571,29.8154426979028));
#75728=CARTESIAN_POINT('Ctrl Pts',(199.546089385265,12.416256970448,29.8688474530988));
#75729=CARTESIAN_POINT('Ctrl Pts',(199.548297270151,12.4060561818776,29.9080152385761));
#75730=CARTESIAN_POINT('Ctrl Pts',(199.550505155036,12.3942422832989,29.9467099708587));
#75731=CARTESIAN_POINT('Ctrl Pts',(199.552713039922,12.3808721213668,29.9847931872787));
#75732=CARTESIAN_POINT('Ctrl Pts',(199.555724386742,12.3626364810578,30.0367351039119));
#75733=CARTESIAN_POINT('Ctrl Pts',(199.558735733561,12.3414281238509,30.08775471955));
#75734=CARTESIAN_POINT('Ctrl Pts',(199.561747080381,12.3173608222,30.137489383545));
#75735=CARTESIAN_POINT('Ctrl Pts',(199.564753114759,12.293335978676,30.1871363085526));
#75736=CARTESIAN_POINT('Ctrl Pts',(199.567759149137,12.2664624280492,30.2355023094808));
#75737=CARTESIAN_POINT('Ctrl Pts',(199.570765183515,12.2369026119477,30.2822430431503));
#75738=CARTESIAN_POINT('Ctrl Pts',(199.573768268267,12.2073718009655,30.3289379131867));
#75739=CARTESIAN_POINT('Ctrl Pts',(199.57677135302,12.1751602269147,30.3740102315267));
#75740=CARTESIAN_POINT('Ctrl Pts',(199.579774437772,12.1404761365253,30.4171403556798));
#75741=CARTESIAN_POINT('Ctrl Pts',(199.582775759048,12.1058124133867,30.4602451528876));
#75742=CARTESIAN_POINT('Ctrl Pts',(199.585777080323,12.0686793818517,30.501409606242));
#75743=CARTESIAN_POINT('Ctrl Pts',(199.588778401599,12.029327136875,30.540345084716));
#75744=CARTESIAN_POINT('Ctrl Pts',(199.59177914292,11.9899824960625,30.579273039559));
#75745=CARTESIAN_POINT('Ctrl Pts',(199.59477988424,11.9484198683968,30.6159725041514));
#75746=CARTESIAN_POINT('Ctrl Pts',(199.597780625561,11.9049263567014,30.6501915227244));
#75747=CARTESIAN_POINT('Ctrl Pts',(199.600784114457,11.8613930209423,30.6844418733358));
#75748=CARTESIAN_POINT('Ctrl Pts',(199.603787603353,11.815925684731,30.7162069138282));
#75749=CARTESIAN_POINT('Ctrl Pts',(199.60679109225,11.7688435342395,30.7452758207956));
#75750=CARTESIAN_POINT('Ctrl Pts',(199.609795960792,11.7217397566593,30.7743580805055));
#75751=CARTESIAN_POINT('Ctrl Pts',(199.612800829335,11.6730201508957,30.8007414863127));
#75752=CARTESIAN_POINT('Ctrl Pts',(199.615805697878,11.6230289469955,30.8242609943684));
#75753=CARTESIAN_POINT('Ctrl Pts',(199.618816164981,11.5729446013205,30.8478243231077));
#75754=CARTESIAN_POINT('Ctrl Pts',(199.621826632084,11.5215844154539,30.8685128978839));
#75755=CARTESIAN_POINT('Ctrl Pts',(199.624837099188,11.4693119396476,30.8862101403843));
#75756=CARTESIAN_POINT('Ctrl Pts',(199.627044626097,11.4309813773204,30.8991872425057));
#75757=CARTESIAN_POINT('Ctrl Pts',(199.629252153005,11.3921606682031,30.9105569200359));
#75758=CARTESIAN_POINT('Ctrl Pts',(199.631459679914,11.3529966746977,30.9202906736483));
#75759=CARTESIAN_POINT('Ctrl Pts',(199.634471020875,11.299572121942,30.9335687228673));
#75760=CARTESIAN_POINT('Ctrl Pts',(199.637482361835,11.2452862201099,30.9438558378596));
#75761=CARTESIAN_POINT('Ctrl Pts',(199.640493702795,11.1905045331431,30.9510479912298));
#75762=CARTESIAN_POINT('Ctrl Pts',(199.643499731343,11.1358194884645,30.9582274566709));
#75763=CARTESIAN_POINT('Ctrl Pts',(199.646505759891,11.0806409133706,30.9623227279793));
#75764=CARTESIAN_POINT('Ctrl Pts',(199.64951178844,11.025345793023,30.963280506525));
#75765=CARTESIAN_POINT('Ctrl Pts',(199.652514867386,10.9701049298448,30.9642373452707));
#75766=CARTESIAN_POINT('Ctrl Pts',(199.655517946332,10.9147482729346,30.9620627810189));
#75767=CARTESIAN_POINT('Ctrl Pts',(199.658521025279,10.8596573127426,30.9567553604272));
#75768=CARTESIAN_POINT('Ctrl Pts',(199.661522340783,10.8045987025918,30.9514510564135));
#75769=CARTESIAN_POINT('Ctrl Pts',(199.664523656287,10.7498060040383,30.9430175930706));
#75770=CARTESIAN_POINT('Ctrl Pts',(199.667524971791,10.6956577657883,30.9315055202391));
#75771=CARTESIAN_POINT('Ctrl Pts',(199.670525707385,10.6415199899855,30.9199956717543));
#75772=CARTESIAN_POINT('Ctrl Pts',(199.673526442978,10.5880269429317,30.9054085049404));
#75773=CARTESIAN_POINT('Ctrl Pts',(199.676527178573,10.5355468402103,30.8878456370798));
#75774=CARTESIAN_POINT('Ctrl Pts',(199.679530661859,10.483018682877,30.8702666873756));
#75775=CARTESIAN_POINT('Ctrl Pts',(199.682534145145,10.431505824191,30.8497067610724));
#75776=CARTESIAN_POINT('Ctrl Pts',(199.685537628432,10.3813597175766,30.8263168742661));
#75777=CARTESIAN_POINT('Ctrl Pts',(199.688542491422,10.3311905754607,30.8029162429014));
#75778=CARTESIAN_POINT('Ctrl Pts',(199.691547354411,10.2823899024228,30.776683309883));
#75779=CARTESIAN_POINT('Ctrl Pts',(199.694552217401,10.2352846405451,30.747815158192));
#75780=CARTESIAN_POINT('Ctrl Pts',(199.697562679114,10.1880916111693,30.7188932187638));
#75781=CARTESIAN_POINT('Ctrl Pts',(199.700573140826,10.1426007374354,30.6873265542632));
#75782=CARTESIAN_POINT('Ctrl Pts',(199.703583602539,10.0991090625624,30.6533550055568));
#75783=CARTESIAN_POINT('Ctrl Pts',(199.705791174995,10.0672166046345,30.6284436589363));
#75784=CARTESIAN_POINT('Ctrl Pts',(199.707998747451,10.0363985309859,30.6022400324764));
#75785=CARTESIAN_POINT('Ctrl Pts',(199.710206319907,10.0067593032422,30.5748512307776));
#75786=CARTESIAN_POINT('Ctrl Pts',(199.713172329925,9.96693716911701,30.538052683116));
#75787=CARTESIAN_POINT('Ctrl Pts',(199.716138339944,9.92906818386051,30.4989503247606));
#75788=CARTESIAN_POINT('Ctrl Pts',(199.719104349962,9.89343564648049,30.4577826379299));
#75789=CARTESIAN_POINT('Ctrl Pts',(199.722066214401,9.85785291254795,30.4166724910018));
#75790=CARTESIAN_POINT('Ctrl Pts',(199.72502807884,9.82450079510673,30.3735031346316));
#75791=CARTESIAN_POINT('Ctrl Pts',(199.727989943279,9.79362724051211,30.3285511542238));
#75792=CARTESIAN_POINT('Ctrl Pts',(199.730948918977,9.76278379725795,30.2836430160105));
#75793=CARTESIAN_POINT('Ctrl Pts',(199.733907894675,9.73441443835141,30.2369561423422));
#75794=CARTESIAN_POINT('Ctrl Pts',(199.736866870372,9.70872648068688,30.1887996430899));
#75795=CARTESIAN_POINT('Ctrl Pts',(199.739824209263,9.68305273274946,30.1406697824175));
#75796=CARTESIAN_POINT('Ctrl Pts',(199.742781548153,9.66005770248644,30.0910723869667));
#75797=CARTESIAN_POINT('Ctrl Pts',(199.745738887044,9.63990370325761,30.0403427741607));
#75798=CARTESIAN_POINT('Ctrl Pts',(199.748697257538,9.61974267373835,29.9895954654171));
#75799=CARTESIAN_POINT('Ctrl Pts',(199.751655628033,9.60242486459018,29.9377156537215));
#75800=CARTESIAN_POINT('Ctrl Pts',(199.754613998528,9.58806436995143,29.8850584716629));
#75801=CARTESIAN_POINT('Ctrl Pts',(199.75757296662,9.57370097446109,29.8323906527373));
#75802=CARTESIAN_POINT('Ctrl Pts',(199.760531934712,9.56229620567979,29.7789456819502));
#75803=CARTESIAN_POINT('Ctrl Pts',(199.763490902804,9.55391339084591,29.725090579157));
#75804=CARTESIAN_POINT('Ctrl Pts',(199.766453613072,9.54551997435425,29.6711673663815));
#75805=CARTESIAN_POINT('Ctrl Pts',(199.769416323339,9.54015619498495,29.6168335284714));
#75806=CARTESIAN_POINT('Ctrl Pts',(199.772379033607,9.53783350335657,29.5624610766275));
#75807=CARTESIAN_POINT('Ctrl Pts',(199.77353434044,9.53692777135211,29.5412585763928));
#75808=CARTESIAN_POINT('Ctrl Pts',(199.774689647274,9.5364839070462,29.5200501990782));
#75809=CARTESIAN_POINT('Ctrl Pts',(199.775844954107,9.53650044565997,29.49885787631));
#75810=CARTESIAN_POINT('',(200.275844954197,9.53650048976732,29.5011973089453));
#75811=CARTESIAN_POINT('Ctrl Pts',(199.775844954157,9.53650044566069,29.4988578753877));
#75812=CARTESIAN_POINT('Ctrl Pts',(199.780214289405,9.53656299424463,29.4187091562833));
#75813=CARTESIAN_POINT('Ctrl Pts',(199.784583624652,9.54321187874569,29.3388148236768));
#75814=CARTESIAN_POINT('Ctrl Pts',(199.788952959899,9.55630950416147,29.2600208296008));
#75815=CARTESIAN_POINT('Ctrl Pts',(199.791964298979,9.56533636729763,29.2057161310087));
#75816=CARTESIAN_POINT('Ctrl Pts',(199.79497563806,9.57745028612169,29.1518085046576));
#75817=CARTESIAN_POINT('Ctrl Pts',(199.79798697714,9.59260158197756,29.0986747666195));
#75818=CARTESIAN_POINT('Ctrl Pts',(199.800993003692,9.60772614829929,29.0456347657823));
#75819=CARTESIAN_POINT('Ctrl Pts',(199.803999030244,9.62587731386913,28.9933664471136));
#75820=CARTESIAN_POINT('Ctrl Pts',(199.807005056796,9.64695430672566,28.9422369661659));
#75821=CARTESIAN_POINT('Ctrl Pts',(199.810008133676,9.66801061772365,28.8911576561654));
#75822=CARTESIAN_POINT('Ctrl Pts',(199.813011210556,9.69198686835455,28.8412154555126));
#75823=CARTESIAN_POINT('Ctrl Pts',(199.816014287436,9.71873291471523,28.7927610685448));
#75824=CARTESIAN_POINT('Ctrl Pts',(199.819015600807,9.74546325489223,28.744335135633));
#75825=CARTESIAN_POINT('Ctrl Pts',(199.822016914179,9.77495991228419,28.6973957455857));
#75826=CARTESIAN_POINT('Ctrl Pts',(199.825018227551,9.807026183116,28.6522702540142));
#75827=CARTESIAN_POINT('Ctrl Pts',(199.82801896095,9.83908625747709,28.6071534824708));
#75828=CARTESIAN_POINT('Ctrl Pts',(199.83101969435,9.87371465356943,28.5638503430253));
#75829=CARTESIAN_POINT('Ctrl Pts',(199.834020427749,9.91067190144827,28.5226584303808));
#75830=CARTESIAN_POINT('Ctrl Pts',(199.837023908762,9.94766298912868,28.4814288004757));
#75831=CARTESIAN_POINT('Ctrl Pts',(199.840027389774,9.98698683548436,28.4423146527842));
#75832=CARTESIAN_POINT('Ctrl Pts',(199.843030870787,10.0283652886303,28.4055785831493));
#75833=CARTESIAN_POINT('Ctrl Pts',(199.846035731455,10.06976274906,28.3688256387197));
#75834=CARTESIAN_POINT('Ctrl Pts',(199.849040592124,10.1132162831236,28.3344532777201));
#75835=CARTESIAN_POINT('Ctrl Pts',(199.852045452792,10.1584151919626,28.3026833080255));
#75836=CARTESIAN_POINT('Ctrl Pts',(199.855055912134,10.203698315667,28.2708541443418));
#75837=CARTESIAN_POINT('Ctrl Pts',(199.858066371476,10.2507328609209,28.2416373365857));
#75838=CARTESIAN_POINT('Ctrl Pts',(199.861076830817,10.2991807580831,28.2152102739518));
#75839=CARTESIAN_POINT('Ctrl Pts',(199.863284420509,10.3347079206294,28.1958311346122));
#75840=CARTESIAN_POINT('Ctrl Pts',(199.865492010201,10.3709945293636,28.1779512020213));
#75841=CARTESIAN_POINT('Ctrl Pts',(199.867699599893,10.4079008028976,28.1616238231384));
#75842=CARTESIAN_POINT('Ctrl Pts',(199.87071093792,10.4582440642904,28.1393519049994));
#75843=CARTESIAN_POINT('Ctrl Pts',(199.873722275947,10.5099504315498,28.1198781125562));
#75844=CARTESIAN_POINT('Ctrl Pts',(199.876733613973,10.5626776915904,28.1033678191566));
#75845=CARTESIAN_POINT('Ctrl Pts',(199.879739639464,10.6153119313653,28.0868866528514));
#75846=CARTESIAN_POINT('Ctrl Pts',(199.882745664954,10.6689629901461,28.0733587663774));
#75847=CARTESIAN_POINT('Ctrl Pts',(199.885751690445,10.7232686757375,28.0629015259308));
#75848=CARTESIAN_POINT('Ctrl Pts',(199.88875476626,10.7775210736366,28.0524545466974));
#75849=CARTESIAN_POINT('Ctrl Pts',(199.891757842075,10.8324263102265,28.0450723437012));
#75850=CARTESIAN_POINT('Ctrl Pts',(199.894760917889,10.8876088348908,28.0408219861835));
#75851=CARTESIAN_POINT('Ctrl Pts',(199.897762230194,10.9427589544663,28.0365741246229));
#75852=CARTESIAN_POINT('Ctrl Pts',(199.900763542499,10.9981855143398,28.0354545034967));
#75853=CARTESIAN_POINT('Ctrl Pts',(199.903764854804,11.053506914299,28.0374784582365));
#75854=CARTESIAN_POINT('Ctrl Pts',(199.906765587136,11.108817623979,28.0395020218683));
#75855=CARTESIAN_POINT('Ctrl Pts',(199.909766319469,11.1640226871553,28.0446679355206));
#75856=CARTESIAN_POINT('Ctrl Pts',(199.912767051802,11.2187418961886,28.0529394508688));
#75857=CARTESIAN_POINT('Ctrl Pts',(199.915770531757,11.2735112088979,28.0612185400349));
#75858=CARTESIAN_POINT('Ctrl Pts',(199.918774011712,11.3277932559645,28.0726088326987));
#75859=CARTESIAN_POINT('Ctrl Pts',(199.921777491667,11.3812158426026,28.0870220343725));
#75860=CARTESIAN_POINT('Ctrl Pts',(199.924782351281,11.4346629690946,28.1014418568014));
#75861=CARTESIAN_POINT('Ctrl Pts',(199.927787210895,11.4872493465873,28.1188871898068));
#75862=CARTESIAN_POINT('Ctrl Pts',(199.930792070509,11.5386190000547,28.1392201416908));
#75863=CARTESIAN_POINT('Ctrl Pts',(199.933802528815,11.5900843661098,28.1595909781878));
#75864=CARTESIAN_POINT('Ctrl Pts',(199.936812987122,11.6403279998836,28.1828599585515));
#75865=CARTESIAN_POINT('Ctrl Pts',(199.939823445428,11.6890160226327,28.2088419265809));
#75866=CARTESIAN_POINT('Ctrl Pts',(199.942031043581,11.7247194199613,28.2278947546801));
#75867=CARTESIAN_POINT('Ctrl Pts',(199.944238641733,11.7595867779055,28.248405478792));
#75868=CARTESIAN_POINT('Ctrl Pts',(199.946446239885,11.7934967604058,28.2702865613382));
#75869=CARTESIAN_POINT('Ctrl Pts',(199.949457577301,11.8397526421459,28.3001340779681));
#75870=CARTESIAN_POINT('Ctrl Pts',(199.952468914716,11.8844183203329,28.332657189576));
#75871=CARTESIAN_POINT('Ctrl Pts',(199.955480252132,11.9271676837001,28.3676606796979));
#75872=CARTESIAN_POINT('Ctrl Pts',(199.958486276988,11.9698416292416,28.4026024171548));
#75873=CARTESIAN_POINT('Ctrl Pts',(199.961492301845,12.0106055643059,28.4400155173502));
#75874=CARTESIAN_POINT('Ctrl Pts',(199.964498326701,12.0491625315286,28.4796617068656));
#75875=CARTESIAN_POINT('Ctrl Pts',(199.967501401868,12.0876816643742,28.5192689931945));
#75876=CARTESIAN_POINT('Ctrl Pts',(199.970504477035,12.1239977534923,28.5611046514853));
#75877=CARTESIAN_POINT('Ctrl Pts',(199.973507552202,12.1578485443479,28.6048916275939));
#75878=CARTESIAN_POINT('Ctrl Pts',(199.976508863847,12.191679456702,28.6486528902865));
#75879=CARTESIAN_POINT('Ctrl Pts',(199.979510175491,12.223047618373,28.6943627828438));
#75880=CARTESIAN_POINT('Ctrl Pts',(199.982511487136,12.2517306915302,28.7417107900799));
#75881=CARTESIAN_POINT('Ctrl Pts',(199.985512218797,12.2804082218757,28.7890496476308));
#75882=CARTESIAN_POINT('Ctrl Pts',(199.988512950458,12.3064014211035,28.8380255401038));
#75883=CARTESIAN_POINT('Ctrl Pts',(199.991513682119,12.3295322467552,28.8883005191779));
#75884=CARTESIAN_POINT('Ctrl Pts',(199.99451716139,12.352684252072,28.9386215323728));
#75885=CARTESIAN_POINT('Ctrl Pts',(199.997520640662,12.3729684269442,28.9902435281642));
#75886=CARTESIAN_POINT('Ctrl Pts',(200.000524119933,12.3902542098966,29.0428069533941));
#75887=CARTESIAN_POINT('Ctrl Pts',(200.003528978855,12.4075479330914,29.0953945236882));
#75888=CARTESIAN_POINT('Ctrl Pts',(200.006533837778,12.421840382534,29.14892387486));
#75889=CARTESIAN_POINT('Ctrl Pts',(200.009538696701,12.4330513548999,29.2030217782064));
#75890=CARTESIAN_POINT('Ctrl Pts',(200.012549154312,12.4442832156802,29.2572204773977));
#75891=CARTESIAN_POINT('Ctrl Pts',(200.015559611922,12.4524220529524,29.3119893217723));
#75892=CARTESIAN_POINT('Ctrl Pts',(200.018570069533,12.4574392984579,29.366947599381));
#75893=CARTESIAN_POINT('Ctrl Pts',(200.020777672982,12.4611185027226,29.4072491411602));
#75894=CARTESIAN_POINT('Ctrl Pts',(200.02298527643,12.4631201782027,29.4476524048473));
#75895=CARTESIAN_POINT('Ctrl Pts',(200.025192879879,12.4634508669257,29.4880079153393));
#75896=CARTESIAN_POINT('Ctrl Pts',(200.028204217864,12.4639019513418,29.5430558822733));
#75897=CARTESIAN_POINT('Ctrl Pts',(200.031215555848,12.4612437003182,29.5982438389137));
#75898=CARTESIAN_POINT('Ctrl Pts',(200.034226893833,12.4554602187907,29.6531920413002));
#75899=CARTESIAN_POINT('Ctrl Pts',(200.037232919273,12.4496869403711,29.708043305115));
#75900=CARTESIAN_POINT('Ctrl Pts',(200.040238944713,12.4407994281139,29.7626551335608));
#75901=CARTESIAN_POINT('Ctrl Pts',(200.043244970152,12.428833780463,29.8166485082985));
#75902=CARTESIAN_POINT('Ctrl Pts',(200.046248045911,12.4168798741789,29.8705889016991));
#75903=CARTESIAN_POINT('Ctrl Pts',(200.049251121669,12.4018539297456,29.9239115309983));
#75904=CARTESIAN_POINT('Ctrl Pts',(200.052254197427,12.3838435117912,29.9762450890805));
#75905=CARTESIAN_POINT('Ctrl Pts',(200.05525550967,12.3658436702109,30.0285479149895));
#75906=CARTESIAN_POINT('Ctrl Pts',(200.058256821913,12.3448630004139,30.079862323062));
#75907=CARTESIAN_POINT('Ctrl Pts',(200.061258134156,12.3210389498237,30.1298319958915));
#75908=CARTESIAN_POINT('Ctrl Pts',(200.064258866421,12.2972195030237,30.179792012517));
#75909=CARTESIAN_POINT('Ctrl Pts',(200.067259598686,12.2705579937173,30.2284073340654));
#75910=CARTESIAN_POINT('Ctrl Pts',(200.070260330952,12.2412391182358,30.2753436021282));
#75911=CARTESIAN_POINT('Ctrl Pts',(200.073263810832,12.2118933969847,30.3223228472909));
#75912=CARTESIAN_POINT('Ctrl Pts',(200.076267290711,12.1798857287696,30.3676195192098));
#75913=CARTESIAN_POINT('Ctrl Pts',(200.079270770591,12.1454449367162,30.4109270810286));
#75914=CARTESIAN_POINT('Ctrl Pts',(200.082275630126,12.1109883242143,30.4542545362648));
#75915=CARTESIAN_POINT('Ctrl Pts',(200.08528048966,12.0740967118477,30.495590665767));
#75916=CARTESIAN_POINT('Ctrl Pts',(200.088285349195,12.0350380020923,30.5346635125609));
#75917=CARTESIAN_POINT('Ctrl Pts',(200.091295807415,11.995906517736,30.5738091602959));
#75918=CARTESIAN_POINT('Ctrl Pts',(200.094306265636,11.9546002649204,30.6106827496535));
#75919=CARTESIAN_POINT('Ctrl Pts',(200.097316723856,11.911421751148,30.6450513706967));
#75920=CARTESIAN_POINT('Ctrl Pts',(200.099524322528,11.8797585216102,30.6702542191023));
#75921=CARTESIAN_POINT('Ctrl Pts',(200.1017319212,11.8470892182861,30.6941108724835));
#75922=CARTESIAN_POINT('Ctrl Pts',(200.103939519872,11.8135423611787,30.7165447285521));
#75923=CARTESIAN_POINT('Ctrl Pts',(200.106950857697,11.7677818155575,30.7471462686843));
#75924=CARTESIAN_POINT('Ctrl Pts',(200.109962195522,11.7201970630349,30.7752259382833));
#75925=CARTESIAN_POINT('Ctrl Pts',(200.112973533348,11.6710967602429,30.800561951001));
#75926=CARTESIAN_POINT('Ctrl Pts',(200.115979558626,11.6220830793072,30.8258532663883));
#75927=CARTESIAN_POINT('Ctrl Pts',(200.118985583904,11.571559619394,30.8484102908232));
#75928=CARTESIAN_POINT('Ctrl Pts',(200.121991609183,11.5198629781336,30.8680550917145));
#75929=CARTESIAN_POINT('Ctrl Pts',(200.124994684778,11.4682170645481,30.8876806160137));
#75930=CARTESIAN_POINT('Ctrl Pts',(200.127997760374,11.4154007409956,30.9043993913857));
#75931=CARTESIAN_POINT('Ctrl Pts',(200.13100083597,11.3617724181172,30.91808073377));
#75932=CARTESIAN_POINT('Ctrl Pts',(200.13400214805,11.3081755877612,30.9317540419672));
#75933=CARTESIAN_POINT('Ctrl Pts',(200.137003460129,11.2537682134788,30.9423933226096));
#75934=CARTESIAN_POINT('Ctrl Pts',(200.140004772209,11.1989235663055,30.9499178131081));
#75935=CARTESIAN_POINT('Ctrl Pts',(200.14300550431,11.1440895173922,30.9574408495632));
#75936=CARTESIAN_POINT('Ctrl Pts',(200.146006236412,11.0888188858345,30.9618502197319));
#75937=CARTESIAN_POINT('Ctrl Pts',(200.149006968513,11.0334925320831,30.9631167076808));
#75938=CARTESIAN_POINT('Ctrl Pts',(200.15201044823,10.9781155188538,30.9643843552871));
#75939=CARTESIAN_POINT('Ctrl Pts',(200.155013927947,10.9226832100697,30.9625033595698));
#75940=CARTESIAN_POINT('Ctrl Pts',(200.158017407663,10.867577441544,30.9574966607207));
#75941=CARTESIAN_POINT('Ctrl Pts',(200.161022267035,10.8124463600681,30.9524876620339));
#75942=CARTESIAN_POINT('Ctrl Pts',(200.164027126406,10.757642640595,30.9443501757504));
#75943=CARTESIAN_POINT('Ctrl Pts',(200.167031985777,10.7035406744545,30.9331587903289));
#75944=CARTESIAN_POINT('Ctrl Pts',(200.170042443837,10.6493379049152,30.9219465529909));
#75945=CARTESIAN_POINT('Ctrl Pts',(200.173052901896,10.5958400114111,30.9076691867994));
#75946=CARTESIAN_POINT('Ctrl Pts',(200.176063359956,10.5434077505465,30.8904516416399));
#75947=CARTESIAN_POINT('Ctrl Pts',(200.178270959925,10.5049586324358,30.8778258380506));
#75948=CARTESIAN_POINT('Ctrl Pts',(200.180478559895,10.4670822504933,30.863620032738));
#75949=CARTESIAN_POINT('Ctrl Pts',(200.182686159865,10.4299131928923,30.8478995817055));
#75950=CARTESIAN_POINT('Ctrl Pts',(200.185697497642,10.3792117121727,30.8264556658149));
#75951=CARTESIAN_POINT('Ctrl Pts',(200.188708835419,10.3296163752628,30.8021024532849));
#75952=CARTESIAN_POINT('Ctrl Pts',(200.191720173197,10.2814820181045,30.7749761408328));
#75953=CARTESIAN_POINT('Ctrl Pts',(200.194726198425,10.2334325787354,30.7478976841456));
#75954=CARTESIAN_POINT('Ctrl Pts',(200.197732223653,10.1868394599955,30.7180560935339));
#75955=CARTESIAN_POINT('Ctrl Pts',(200.200738248881,10.1420361867845,30.6856349966211));
#75956=CARTESIAN_POINT('Ctrl Pts',(200.203741324425,10.097276877105,30.6532457131409));
#75957=CARTESIAN_POINT('Ctrl Pts',(200.206744399969,10.0543043590039,30.6182822455201));
#75958=CARTESIAN_POINT('Ctrl Pts',(200.209747475513,10.0134246444191,30.5809723945413));
#75959=CARTESIAN_POINT('Ctrl Pts',(200.21274878754,9.97256893592204,30.5436844532937));
#75960=CARTESIAN_POINT('Ctrl Pts',(200.215750099567,9.93380398383163,30.5040532148703));
#75961=CARTESIAN_POINT('Ctrl Pts',(200.218751411593,9.89740223573112,30.4623463099266));
#75962=CARTESIAN_POINT('Ctrl Pts',(200.221752143641,9.86100752197141,30.4206474645019));
#75963=CARTESIAN_POINT('Ctrl Pts',(200.224752875689,9.82697545188296,30.3768741465184));
#75964=CARTESIAN_POINT('Ctrl Pts',(200.227753607736,9.79553955820122,30.331328631855));
#75965=CARTESIAN_POINT('Ctrl Pts',(200.230757087398,9.76407488031213,30.2857414135406));
#75966=CARTESIAN_POINT('Ctrl Pts',(200.233760567059,9.73521142811629,30.2383791919452));
#75967=CARTESIAN_POINT('Ctrl Pts',(200.23676404672,9.70913967861635,30.189573694885));
#75968=CARTESIAN_POINT('Ctrl Pts',(200.239768906036,9.68305595301036,30.1407457789299));
#75969=CARTESIAN_POINT('Ctrl Pts',(200.242773765351,9.6597667084959,30.0904737454787));
#75970=CARTESIAN_POINT('Ctrl Pts',(200.245778624666,9.6394151678175,30.0391114582671));
#75971=CARTESIAN_POINT('Ctrl Pts',(200.248789082669,9.61902570792044,29.9876534722664));
#75972=CARTESIAN_POINT('Ctrl Pts',(200.251799540672,9.6015850520218,29.9351016766448));
#75973=CARTESIAN_POINT('Ctrl Pts',(200.254809998675,9.58718684532642,29.8818261908006));
#75974=CARTESIAN_POINT('Ctrl Pts',(200.257017599069,9.57662848950547,29.8427587188593));
#75975=CARTESIAN_POINT('Ctrl Pts',(200.259225199463,9.56770514020051,29.8033024178133));
#75976=CARTESIAN_POINT('Ctrl Pts',(200.261432799857,9.56043607063758,29.763605658662));
#75977=CARTESIAN_POINT('Ctrl Pts',(200.265901162103,9.54572288428293,29.6832561985266));
#75978=CARTESIAN_POINT('Ctrl Pts',(200.270369524349,9.53773431809565,29.6016400343671));
#75979=CARTESIAN_POINT('Ctrl Pts',(200.274837886595,9.53663226839757,29.5196756729177));
#75980=CARTESIAN_POINT('Ctrl Pts',(200.275173575782,9.53654947605727,29.5135180365446));
#75981=CARTESIAN_POINT('Ctrl Pts',(200.27550926497,9.53650553028377,29.5073584496461));
#75982=CARTESIAN_POINT('Ctrl Pts',(200.275844954157,9.53650048976792,29.5011973096727));
#75983=CARTESIAN_POINT('',(200.775844954206,9.53650002111796,29.4997513792903));
#75984=CARTESIAN_POINT('Ctrl Pts',(200.275844954197,9.53650048976732,29.5011973089453));
#75985=CARTESIAN_POINT('Ctrl Pts',(200.278807267562,9.53645600939984,29.4468278863525));
#75986=CARTESIAN_POINT('Ctrl Pts',(200.281769580928,9.53944553388517,29.3923573443137));
#75987=CARTESIAN_POINT('Ctrl Pts',(200.284731894294,9.54547632636966,29.3381570735284));
#75988=CARTESIAN_POINT('Ctrl Pts',(200.28769134432,9.55150128955749,29.2840091921195));
#75989=CARTESIAN_POINT('Ctrl Pts',(200.290650794347,9.56056164358428,29.2301316035641));
#75990=CARTESIAN_POINT('Ctrl Pts',(200.293610244374,9.5726126399746,29.176893865054));
#75991=CARTESIAN_POINT('Ctrl Pts',(200.296568082553,9.58465707285924,29.1236851221712));
#75992=CARTESIAN_POINT('Ctrl Pts',(200.299525920733,9.59968880213546,29.0711160693902));
#75993=CARTESIAN_POINT('Ctrl Pts',(200.302483758912,9.61761186279543,29.0195467888378));
#75994=CARTESIAN_POINT('Ctrl Pts',(200.305441233927,9.63553272285592,28.9679838399792));
#75995=CARTESIAN_POINT('Ctrl Pts',(200.308398708942,9.65634402898352,28.917420933234));
#75996=CARTESIAN_POINT('Ctrl Pts',(200.311356183957,9.67990054256185,28.8682012405271));
#75997=CARTESIAN_POINT('Ctrl Pts',(200.314316438232,9.7034791931595,28.8189352940617));
#75998=CARTESIAN_POINT('Ctrl Pts',(200.317276692507,9.72980796069768,28.7710155710276));
#75999=CARTESIAN_POINT('Ctrl Pts',(200.320236946782,9.75869499593452,28.7247618837531));
#76000=CARTESIAN_POINT('Ctrl Pts',(200.323198897984,9.78759859027576,28.6784816821746));
#76001=CARTESIAN_POINT('Ctrl Pts',(200.326160849185,9.81906305282296,28.6338698590219));
#76002=CARTESIAN_POINT('Ctrl Pts',(200.329122800386,9.85285438256853,28.5912155467836));
#76003=CARTESIAN_POINT('Ctrl Pts',(200.332089746762,9.8867026996197,28.5484893002845));
#76004=CARTESIAN_POINT('Ctrl Pts',(200.335056693139,9.92288534338377,28.5077275494681));
#76005=CARTESIAN_POINT('Ctrl Pts',(200.338023639515,9.96113064903218,28.4691834684971));
#76006=CARTESIAN_POINT('Ctrl Pts',(200.338742239627,9.9703937355266,28.4598480180456));
#76007=CARTESIAN_POINT('Ctrl Pts',(200.339460839739,9.97977766981178,28.4506424738096));
#76008=CARTESIAN_POINT('Ctrl Pts',(200.34017943985,9.98927831341127,28.4415700673832));
#76009=CARTESIAN_POINT('Ctrl Pts',(200.343190777668,10.0290913428017,28.4035515921175));
#76010=CARTESIAN_POINT('Ctrl Pts',(200.346202115486,10.0711352732911,28.367703518185));
#76011=CARTESIAN_POINT('Ctrl Pts',(200.349213453304,10.1151442102846,28.3342974301276));
#76012=CARTESIAN_POINT('Ctrl Pts',(200.352219478574,10.1590755075026,28.3009502764902));
#76013=CARTESIAN_POINT('Ctrl Pts',(200.355225503844,10.2049645145514,28.2700368754397));
#76014=CARTESIAN_POINT('Ctrl Pts',(200.358231529114,10.2525102672969,28.2417904190861));
#76015=CARTESIAN_POINT('Ctrl Pts',(200.361234604701,10.3000093654457,28.213571679762));
#76016=CARTESIAN_POINT('Ctrl Pts',(200.364237680288,10.3491615373096,28.1880149689842));
#76017=CARTESIAN_POINT('Ctrl Pts',(200.367240755874,10.3996362017358,28.1653106879375));
#76018=CARTESIAN_POINT('Ctrl Pts',(200.370242067944,10.4500812255747,28.1426197396833));
#76019=CARTESIAN_POINT('Ctrl Pts',(200.373243380014,10.5018467223615,28.1227781169169));
#76020=CARTESIAN_POINT('Ctrl Pts',(200.376244692084,10.5545788829705,28.1059296005925));
#76021=CARTESIAN_POINT('Ctrl Pts',(200.379245424176,10.6073008535302,28.089084340103));
#76022=CARTESIAN_POINT('Ctrl Pts',(200.382246156267,10.6609886145945,28.075231197716));
#76023=CARTESIAN_POINT('Ctrl Pts',(200.385246888359,10.7152720119965,28.0644644822062));
#76024=CARTESIAN_POINT('Ctrl Pts',(200.388250368065,10.7696051138822,28.053687908175));
#76025=CARTESIAN_POINT('Ctrl Pts',(200.391253847771,10.8245344230488,28.0460035096159));
#76026=CARTESIAN_POINT('Ctrl Pts',(200.394257327476,10.8796798508475,28.0414543847696));
#76027=CARTESIAN_POINT('Ctrl Pts',(200.397262186836,10.9348506098064,28.0369031702738));
#76028=CARTESIAN_POINT('Ctrl Pts',(200.400267046197,10.9902371569852,28.0354901138159));
#76029=CARTESIAN_POINT('Ctrl Pts',(200.403271905557,11.0454578509173,28.0372061547197));
#76030=CARTESIAN_POINT('Ctrl Pts',(200.406282363604,11.1007814326649,28.0389253929701));
#76031=CARTESIAN_POINT('Ctrl Pts',(200.409292821652,11.1559380171466,28.043785328107));
#76032=CARTESIAN_POINT('Ctrl Pts',(200.4123032797,11.2105507294148,28.0517249431331));
#76033=CARTESIAN_POINT('Ctrl Pts',(200.414510879747,11.2505987966152,28.0575471450144));
#76034=CARTESIAN_POINT('Ctrl Pts',(200.416718479795,11.2903545139687,28.065024328512));
#76035=CARTESIAN_POINT('Ctrl Pts',(200.418926079842,11.3296740555719,28.074115268655));
#76036=CARTESIAN_POINT('Ctrl Pts',(200.421937417657,11.3833089622339,28.0865160166333));
#76037=CARTESIAN_POINT('Ctrl Pts',(200.424948755472,11.4363547761409,28.101972992898));
#76038=CARTESIAN_POINT('Ctrl Pts',(200.427960093287,11.488438519647,28.1204130826494));
#76039=CARTESIAN_POINT('Ctrl Pts',(200.430966118554,11.5404303779458,28.1388206407247));
#76040=CARTESIAN_POINT('Ctrl Pts',(200.433972143821,11.5914630407979,28.1602006932887));
#76041=CARTESIAN_POINT('Ctrl Pts',(200.436978169088,11.6411763631297,28.1844297352996));
#76042=CARTESIAN_POINT('Ctrl Pts',(200.439981244671,11.6908409039203,28.2086350023956));
#76043=CARTESIAN_POINT('Ctrl Pts',(200.442984320255,11.7391881969001,28.2356834907018));
#76044=CARTESIAN_POINT('Ctrl Pts',(200.445987395839,11.7858775995091,28.2654034470363));
#76045=CARTESIAN_POINT('Ctrl Pts',(200.448988707905,11.8325395843746,28.2951059507136));
#76046=CARTESIAN_POINT('Ctrl Pts',(200.451990019972,11.8775451644612,28.3274765300474));
#76047=CARTESIAN_POINT('Ctrl Pts',(200.454991332039,11.920579908153,28.3622984210677));
#76048=CARTESIAN_POINT('Ctrl Pts',(200.457992064127,11.9636063357389,28.3971135830475));
#76049=CARTESIAN_POINT('Ctrl Pts',(200.460992796215,12.0046622734666,28.4343787841528));
#76050=CARTESIAN_POINT('Ctrl Pts',(200.463993528303,12.0434656634074,28.4738364363857));
#76051=CARTESIAN_POINT('Ctrl Pts',(200.466997008005,12.0823045835926,28.5133302179367));
#76052=CARTESIAN_POINT('Ctrl Pts',(200.470000487708,12.1188864648877,28.5550200841132));
#76053=CARTESIAN_POINT('Ctrl Pts',(200.47300396741,12.1529665957103,28.598612026275));
#76054=CARTESIAN_POINT('Ctrl Pts',(200.476008826767,12.1870623813069,28.6422239924796));
#76055=CARTESIAN_POINT('Ctrl Pts',(200.479013686123,12.2186538243424,28.6877393421784));
#76056=CARTESIAN_POINT('Ctrl Pts',(200.48201854548,12.2475389542448,28.7348341306346));
#76057=CARTESIAN_POINT('Ctrl Pts',(200.485029003524,12.2764779032441,28.7820166666269));
#76058=CARTESIAN_POINT('Ctrl Pts',(200.488039461568,12.3027002162781,28.8307840540367));
#76059=CARTESIAN_POINT('Ctrl Pts',(200.491049919612,12.3260499641419,28.8807878048688));
#76060=CARTESIAN_POINT('Ctrl Pts',(200.493257519686,12.3431725761745,28.917456073437));
#76061=CARTESIAN_POINT('Ctrl Pts',(200.495465119761,12.3587514636632,28.9547886817217));
#76062=CARTESIAN_POINT('Ctrl Pts',(200.497672719836,12.3727421130063,28.9926427873983));
#76063=CARTESIAN_POINT('Ctrl Pts',(200.500684057657,12.3918264444484,29.0442787251921));
#76064=CARTESIAN_POINT('Ctrl Pts',(200.503695395479,12.4080329824707,29.0971003555017));
#76065=CARTESIAN_POINT('Ctrl Pts',(200.506706733301,12.4212180488663,29.1507558052357));
#76066=CARTESIAN_POINT('Ctrl Pts',(200.509712758574,12.4343798544049,29.2043165969898));
#76067=CARTESIAN_POINT('Ctrl Pts',(200.512718783848,12.4445306420242,29.2587077805627));
#76068=CARTESIAN_POINT('Ctrl Pts',(200.515724809122,12.4515758947125,29.3135605409531));
#76069=CARTESIAN_POINT('Ctrl Pts',(200.518727884712,12.4586142341981,29.3683594766954));
#76070=CARTESIAN_POINT('Ctrl Pts',(200.521730960303,12.4625530087727,29.4236185712117));
#76071=CARTESIAN_POINT('Ctrl Pts',(200.524734035894,12.4633487344701,29.4789588183609));
#76072=CARTESIAN_POINT('Ctrl Pts',(200.527735347967,12.4641439928879,29.5342665676727));
#76073=CARTESIAN_POINT('Ctrl Pts',(200.530736660041,12.4617998533954,29.5896548486423));
#76074=CARTESIAN_POINT('Ctrl Pts',(200.533737972115,12.4563248426624,29.6447418482831));
#76075=CARTESIAN_POINT('Ctrl Pts',(200.53673870421,12.4508508899294,29.6998182028213));
#76076=CARTESIAN_POINT('Ctrl Pts',(200.539739436305,12.4422473198108,29.7545928669506));
#76077=CARTESIAN_POINT('Ctrl Pts',(200.5427401684,12.4305745540886,29.8086886703365));
#76078=CARTESIAN_POINT('Ctrl Pts',(200.54574364811,12.4188911002223,29.8628340064348));
#76079=CARTESIAN_POINT('Ctrl Pts',(200.548747127819,12.4041329480555,29.916298723198));
#76080=CARTESIAN_POINT('Ctrl Pts',(200.551750607529,12.386411464481,29.9687168667283));
#76081=CARTESIAN_POINT('Ctrl Pts',(200.554755466893,12.3686818405086,30.021159088635));
#76082=CARTESIAN_POINT('Ctrl Pts',(200.557760326256,12.3479863691258,30.0725532887803));
#76083=CARTESIAN_POINT('Ctrl Pts',(200.56076518562,12.3244849046397,30.1225527988705));
#76084=CARTESIAN_POINT('Ctrl Pts',(200.563775643671,12.3009396519625,30.1726454686063));
#76085=CARTESIAN_POINT('Ctrl Pts',(200.566786101723,12.2745782145316,30.221337792492));
#76086=CARTESIAN_POINT('Ctrl Pts',(200.569796559774,12.2456062389068,30.2683081072046));
#76087=CARTESIAN_POINT('Ctrl Pts',(200.572004159792,12.2243607896,30.3027519246743));
#76088=CARTESIAN_POINT('Ctrl Pts',(200.57421175981,12.2017125012651,30.3362702827466));
#76089=CARTESIAN_POINT('Ctrl Pts',(200.576419359829,12.1777563186957,30.3687475489303));
#76090=CARTESIAN_POINT('Ctrl Pts',(200.579430697647,12.1450782257582,30.4130490614784));
#76091=CARTESIAN_POINT('Ctrl Pts',(200.582442035466,12.1098290739686,30.45559637391));
#76092=CARTESIAN_POINT('Ctrl Pts',(200.585453373285,12.0722240656048,30.4960762034794));
#76093=CARTESIAN_POINT('Ctrl Pts',(200.588459398556,12.0346853993213,30.5364846192605));
#76094=CARTESIAN_POINT('Ctrl Pts',(200.591465423827,11.9947994808948,30.574832407268));
#76095=CARTESIAN_POINT('Ctrl Pts',(200.594471449097,11.9528226647358,30.6108380708122));
#76096=CARTESIAN_POINT('Ctrl Pts',(200.597474524685,11.9108870386168,30.6468084035511));
#76097=CARTESIAN_POINT('Ctrl Pts',(200.600477600273,11.8668649778316,30.6804408228867));
#76098=CARTESIAN_POINT('Ctrl Pts',(200.60348067586,11.8210493744918,30.7114908892132));
#76099=CARTESIAN_POINT('Ctrl Pts',(200.606481987931,11.7752606757671,30.7425227217936));
#76100=CARTESIAN_POINT('Ctrl Pts',(200.609483300002,11.727680958082,30.7709749118339));
#76101=CARTESIAN_POINT('Ctrl Pts',(200.612484612073,11.6786340163266,30.796644948274));
#76102=CARTESIAN_POINT('Ctrl Pts',(200.615485344165,11.6295965524833,30.8223100241938));
#76103=CARTESIAN_POINT('Ctrl Pts',(200.618486076257,11.5790928949116,30.8451937698566));
#76104=CARTESIAN_POINT('Ctrl Pts',(200.62148680835,11.5274714516784,30.8651395964019));
#76105=CARTESIAN_POINT('Ctrl Pts',(200.624490288056,11.4758027413758,30.8851036863027));
#76106=CARTESIAN_POINT('Ctrl Pts',(200.627493767763,11.4230146939145,30.9021242924499));
#76107=CARTESIAN_POINT('Ctrl Pts',(200.630497247469,11.3694743146674,30.9160935635759));
#76108=CARTESIAN_POINT('Ctrl Pts',(200.63350210683,11.315909341543,30.9300692515137));
#76109=CARTESIAN_POINT('Ctrl Pts',(200.636506966191,11.2615918658583,30.9409907062689));
#76110=CARTESIAN_POINT('Ctrl Pts',(200.639511825551,11.2068993967915,30.9488011905045));
#76111=CARTESIAN_POINT('Ctrl Pts',(200.6425222836,11.1521050241049,30.9566262273217));
#76112=CARTESIAN_POINT('Ctrl Pts',(200.645532741648,11.096934789252,30.9613286702391));
#76113=CARTESIAN_POINT('Ctrl Pts',(200.648543199696,11.0417704452592,30.9629037835425));
#76114=CARTESIAN_POINT('Ctrl Pts',(200.650750799738,11.001317860917,30.9640588304286));
#76115=CARTESIAN_POINT('Ctrl Pts',(200.65295839978,10.9608685207544,30.9635332756275));
#76116=CARTESIAN_POINT('Ctrl Pts',(200.655165999822,10.9205711987917,30.961342983539));
#76117=CARTESIAN_POINT('Ctrl Pts',(200.65817733764,10.8656025236147,30.9583552551121));
#76118=CARTESIAN_POINT('Ctrl Pts',(200.661188675459,10.8106883204334,30.9522555185764));
#76119=CARTESIAN_POINT('Ctrl Pts',(200.664200013278,10.7562085845656,30.9430516261591));
#76120=CARTESIAN_POINT('Ctrl Pts',(200.667206038549,10.7018249608698,30.9338639710836));
#76121=CARTESIAN_POINT('Ctrl Pts',(200.670212063819,10.6478747994457,30.9215831154162));
#76122=CARTESIAN_POINT('Ctrl Pts',(200.67321808909,10.5947341242407,30.9062687580776));
#76123=CARTESIAN_POINT('Ctrl Pts',(200.676221164678,10.5416455936893,30.8909694280575));
#76124=CARTESIAN_POINT('Ctrl Pts',(200.679224240265,10.4893654803024,30.8726426386432));
#76125=CARTESIAN_POINT('Ctrl Pts',(200.682227315853,10.4382588976238,30.85139897288));
#76126=CARTESIAN_POINT('Ctrl Pts',(200.685228627924,10.3871823266191,30.8301677821824));
#76127=CARTESIAN_POINT('Ctrl Pts',(200.688229939994,10.3372784065553,30.806023312521));
#76128=CARTESIAN_POINT('Ctrl Pts',(200.691231252065,10.2888941751825,30.7791249962027));
#76129=CARTESIAN_POINT('Ctrl Pts',(200.694231984157,10.2405192936589,30.7522318777597));
#76130=CARTESIAN_POINT('Ctrl Pts',(200.697232716249,10.1936639784066,30.7225862258666));
#76131=CARTESIAN_POINT('Ctrl Pts',(200.700233448342,10.1486504001919,30.6903932580902));
#76132=CARTESIAN_POINT('Ctrl Pts',(200.703236928048,10.1035956053859,30.6581708128883));
#76133=CARTESIAN_POINT('Ctrl Pts',(200.706240407754,10.0603863465903,30.6233966997778));
#76134=CARTESIAN_POINT('Ctrl Pts',(200.709243887461,10.0193142714637,30.5863184394298));
#76135=CARTESIAN_POINT('Ctrl Pts',(200.712248746821,9.97822332979961,30.5492231471109));
#76136=CARTESIAN_POINT('Ctrl Pts',(200.715253606182,9.93927190027695,30.5098219735649));
#76137=CARTESIAN_POINT('Ctrl Pts',(200.718258465543,9.90271467753942,30.4683992828955));
#76138=CARTESIAN_POINT('Ctrl Pts',(200.721268923591,9.86608934097599,30.4268994130061));
#76139=CARTESIAN_POINT('Ctrl Pts',(200.724279381639,9.83186744882186,30.383370917966));
#76140=CARTESIAN_POINT('Ctrl Pts',(200.727289839687,9.80026256370662,30.3381302607329));
#76141=CARTESIAN_POINT('Ctrl Pts',(200.72949743973,9.77708637436698,30.3049548185802));
#76142=CARTESIAN_POINT('Ctrl Pts',(200.731705039772,9.75531658657298,30.2708593398782));
#76143=CARTESIAN_POINT('Ctrl Pts',(200.733912639815,9.73502162669244,30.2359768780771));
#76144=CARTESIAN_POINT('Ctrl Pts',(200.737034469505,9.70632194962605,30.1866486017531));
#76145=CARTESIAN_POINT('Ctrl Pts',(200.740156299194,9.68046138456981,30.1355535224928));
#76146=CARTESIAN_POINT('Ctrl Pts',(200.743278128884,9.65765161603659,30.0830377912887));
#76147=CARTESIAN_POINT('Ctrl Pts',(200.746391806722,9.63490140932597,30.0306591913607));
#76148=CARTESIAN_POINT('Ctrl Pts',(200.749505484559,9.61518634070828,29.9768677493751));
#76149=CARTESIAN_POINT('Ctrl Pts',(200.752619162397,9.59867218006485,29.9220338743227));
#76150=CARTESIAN_POINT('Ctrl Pts',(200.755727965602,9.58218387324064,29.8672858446924));
#76151=CARTESIAN_POINT('Ctrl Pts',(200.758836768807,9.56888666071386,29.8114990725187));
#76152=CARTESIAN_POINT('Ctrl Pts',(200.761945572012,9.55889793952383,29.755062935942));
#76153=CARTESIAN_POINT('Ctrl Pts',(200.765049230185,9.548925749549,29.6987202005025));
#76154=CARTESIAN_POINT('Ctrl Pts',(200.768152888357,9.54225124455546,29.6417307019684));
#76155=CARTESIAN_POINT('Ctrl Pts',(200.77125654653,9.53894124389919,29.5844959242873));
#76156=CARTESIAN_POINT('Ctrl Pts',(200.772786015739,9.53731009001419,29.5562908755073));
#76157=CARTESIAN_POINT('Ctrl Pts',(200.774315484948,9.53649521774352,29.5280264340767));
#76158=CARTESIAN_POINT('Ctrl Pts',(200.775844954157,9.5365000211178,29.4997513802026));
#76159=CARTESIAN_POINT('',(201.275844954123,9.5365002812049,29.4990927587658));
#76160=CARTESIAN_POINT('Ctrl Pts',(200.775844954206,9.53650002111796,29.4997513792903));
#76161=CARTESIAN_POINT('Ctrl Pts',(200.779035926708,9.53651004256292,29.4407603784615));
#76162=CARTESIAN_POINT('Ctrl Pts',(200.782226899209,9.54009107565949,29.381855563932));
#76163=CARTESIAN_POINT('Ctrl Pts',(200.78541787171,9.54718642921113,29.3234639455191));
#76164=CARTESIAN_POINT('Ctrl Pts',(200.788615175693,9.55429586126113,29.2649564672976));
#76165=CARTESIAN_POINT('Ctrl Pts',(200.791812479676,9.56493344073772,29.20696463018));
#76166=CARTESIAN_POINT('Ctrl Pts',(200.795009783659,9.57899146312995,29.1499043157329));
#76167=CARTESIAN_POINT('Ctrl Pts',(200.798218635059,9.59310025762155,29.0926379216628));
#76168=CARTESIAN_POINT('Ctrl Pts',(200.801427486458,9.61065407727911,29.0363101839334));
#76169=CARTESIAN_POINT('Ctrl Pts',(200.804636337857,9.63149530938396,28.9813217165121));
#76170=CARTESIAN_POINT('Ctrl Pts',(200.807310651841,9.64886476390697,28.9354933470876));
#76171=CARTESIAN_POINT('Ctrl Pts',(200.809984965824,9.66851667080154,28.8905949606548));
#76172=CARTESIAN_POINT('Ctrl Pts',(200.812659279808,9.69033553689697,28.8468451607122));
#76173=CARTESIAN_POINT('Ctrl Pts',(200.815670617627,9.71490407187492,28.7975818999421));
#76174=CARTESIAN_POINT('Ctrl Pts',(200.818681955446,9.74230714183326,28.7496043191936));
#76175=CARTESIAN_POINT('Ctrl Pts',(200.821693293265,9.77238665520209,28.7032580557834));
#76176=CARTESIAN_POINT('Ctrl Pts',(200.824699318536,9.80241310283357,28.6569935556189));
#76177=CARTESIAN_POINT('Ctrl Pts',(200.827705343807,9.83510633831289,28.6123551003561));
#76178=CARTESIAN_POINT('Ctrl Pts',(200.830711369078,9.8702622627025,28.5696640956483));
#76179=CARTESIAN_POINT('Ctrl Pts',(200.833714444666,9.90538369009925,28.5270149817828));
#76180=CARTESIAN_POINT('Ctrl Pts',(200.836717520254,9.94296268536604,28.4863099380973));
#76181=CARTESIAN_POINT('Ctrl Pts',(200.839720595842,9.98275278091625,28.4478401522267));
#76182=CARTESIAN_POINT('Ctrl Pts',(200.842721907913,10.0225195102521,28.4093929572358));
#76183=CARTESIAN_POINT('Ctrl Pts',(200.845723219984,10.0644943875634,28.3731787842046));
#76184=CARTESIAN_POINT('Ctrl Pts',(200.848724532055,10.1083932893525,28.3394528344232));
#76185=CARTESIAN_POINT('Ctrl Pts',(200.851725264147,10.1522837080452,28.3057334019001));
#76186=CARTESIAN_POINT('Ctrl Pts',(200.85472599624,10.1980969945793,28.2745015588358));
#76187=CARTESIAN_POINT('Ctrl Pts',(200.857726728332,10.2455168782303,28.2459715039264));
#76188=CARTESIAN_POINT('Ctrl Pts',(200.860730208039,10.2929801818012,28.2174153255303));
#76189=CARTESIAN_POINT('Ctrl Pts',(200.863733687746,10.3420525682668,28.1915661500015));
#76190=CARTESIAN_POINT('Ctrl Pts',(200.866737167452,10.3923910614365,28.1685933649791));
#76191=CARTESIAN_POINT('Ctrl Pts',(200.869742026813,10.4427526776909,28.1456100273632));
#76192=CARTESIAN_POINT('Ctrl Pts',(200.872746886174,10.4943810675172,28.125505905814));
#76193=CARTESIAN_POINT('Ctrl Pts',(200.875751745535,10.5469141132065,28.1084018434948));
#76194=CARTESIAN_POINT('Ctrl Pts',(200.878762203584,10.5995450390537,28.0912659126956));
#76195=CARTESIAN_POINT('Ctrl Pts',(200.881772661632,10.6530834764401,28.0771413416956));
#76196=CARTESIAN_POINT('Ctrl Pts',(200.884783119681,10.707154180014,28.0660984776782));
#76197=CARTESIAN_POINT('Ctrl Pts',(200.88699071972,10.7468047864749,28.0580006312214));
#76198=CARTESIAN_POINT('Ctrl Pts',(200.88919831976,10.7867413511787,28.0515588827169));
#76199=CARTESIAN_POINT('Ctrl Pts',(200.891405919799,10.8268145891604,28.0467832014898));
#76200=CARTESIAN_POINT('Ctrl Pts',(200.894417257618,10.8814775964558,28.0402688015834));
#76201=CARTESIAN_POINT('Ctrl Pts',(200.897428595438,10.9366223771427,28.036829374209));
#76202=CARTESIAN_POINT('Ctrl Pts',(200.900439933257,10.9918732515618,28.0365225639048));
#76203=CARTESIAN_POINT('Ctrl Pts',(200.903445958528,11.0470266533804,28.0362162948698));
#76204=CARTESIAN_POINT('Ctrl Pts',(200.906451983799,11.1022852540853,28.0390316780644));
#76205=CARTESIAN_POINT('Ctrl Pts',(200.90945800907,11.1572683657401,28.0449746012054));
#76206=CARTESIAN_POINT('Ctrl Pts',(200.912461084658,11.2121975248379,28.0509116928121));
#76207=CARTESIAN_POINT('Ctrl Pts',(200.915464160246,11.2668512084008,28.0599701882586));
#76208=CARTESIAN_POINT('Ctrl Pts',(200.918467235834,11.3208507213836,28.072103972767));
#76209=CARTESIAN_POINT('Ctrl Pts',(200.921468547905,11.374818523857,28.0842306318689));
#76210=CARTESIAN_POINT('Ctrl Pts',(200.924469859976,11.4281324034541,28.099428884926));
#76211=CARTESIAN_POINT('Ctrl Pts',(200.927471172047,11.4804230666641,28.1176013863516));
#76212=CARTESIAN_POINT('Ctrl Pts',(200.93047190414,11.5327036251398,28.1357703760929));
#76213=CARTESIAN_POINT('Ctrl Pts',(200.933472636232,11.5839608618802,28.1569122995162));
#76214=CARTESIAN_POINT('Ctrl Pts',(200.936473368325,11.6338421019984,28.1808804300844));
#76215=CARTESIAN_POINT('Ctrl Pts',(200.939476848032,11.6837690157725,28.2048705070225));
#76216=CARTESIAN_POINT('Ctrl Pts',(200.942480327739,11.7323169393867,28.2316917318594));
#76217=CARTESIAN_POINT('Ctrl Pts',(200.945483807446,11.7791559874737,28.2611504541778));
#76218=CARTESIAN_POINT('Ctrl Pts',(200.948488666807,11.8260165511686,28.2906227084176));
#76219=CARTESIAN_POINT('Ctrl Pts',(200.951493526168,11.8711662439269,28.322734568893));
#76220=CARTESIAN_POINT('Ctrl Pts',(200.954498385529,11.9143052432807,28.3572497332709));
#76221=CARTESIAN_POINT('Ctrl Pts',(200.957508843577,11.9575246197001,28.3918292066887));
#76222=CARTESIAN_POINT('Ctrl Pts',(200.960519301626,11.9987254258101,28.4288205754071));
#76223=CARTESIAN_POINT('Ctrl Pts',(200.963529759675,12.0376428350449,28.467948839989));
#76224=CARTESIAN_POINT('Ctrl Pts',(200.965737359714,12.066181373956,28.4966420013082));
#76225=CARTESIAN_POINT('Ctrl Pts',(200.967944959753,12.0934927800915,28.5264834560106));
#76226=CARTESIAN_POINT('Ctrl Pts',(200.970152559793,12.1194867551266,28.5573539078232));
#76227=CARTESIAN_POINT('Ctrl Pts',(200.973163897612,12.1549445548629,28.5994636004217));
#76228=CARTESIAN_POINT('Ctrl Pts',(200.976175235431,12.1880968627921,28.643664290199));
#76229=CARTESIAN_POINT('Ctrl Pts',(200.979186573251,12.2186892305583,28.6896736402404));
#76230=CARTESIAN_POINT('Ctrl Pts',(200.982192598522,12.2492276278187,28.7356018214128));
#76231=CARTESIAN_POINT('Ctrl Pts',(200.985198623793,12.2772147578341,28.7833318946167));
#76232=CARTESIAN_POINT('Ctrl Pts',(200.988204649064,12.3024366799456,28.8325489195962));
#76233=CARTESIAN_POINT('Ctrl Pts',(200.991207724652,12.3276338528725,28.8817176500311));
#76234=CARTESIAN_POINT('Ctrl Pts',(200.99421080024,12.3500709537771,28.9323699744583));
#76235=CARTESIAN_POINT('Ctrl Pts',(200.997213875828,12.3695785990762,28.9841640658578));
#76236=CARTESIAN_POINT('Ctrl Pts',(201.000215187899,12.3890747887652,29.0359277418529));
#76237=CARTESIAN_POINT('Ctrl Pts',(201.00321649997,12.4056447471642,29.088831363019));
#76238=CARTESIAN_POINT('Ctrl Pts',(201.006217812042,12.4191670705782,29.1425128312982));
#76239=CARTESIAN_POINT('Ctrl Pts',(201.009218544134,12.4326867809161,29.1961839260818));
#76240=CARTESIAN_POINT('Ctrl Pts',(201.012219276227,12.443159897221,29.250632058091));
#76241=CARTESIAN_POINT('Ctrl Pts',(201.015220008319,12.4505154122051,29.3054819058402));
#76242=CARTESIAN_POINT('Ctrl Pts',(201.018223488026,12.4578776622515,29.3603819767408));
#76243=CARTESIAN_POINT('Ctrl Pts',(201.021226967733,12.462116537947,29.4156839741909));
#76244=CARTESIAN_POINT('Ctrl Pts',(201.02423044744,12.4632127630113,29.4710058598879));
#76245=CARTESIAN_POINT('Ctrl Pts',(201.027235306801,12.4643094916287,29.5263531578006));
#76246=CARTESIAN_POINT('Ctrl Pts',(201.030240166162,12.4622607115556,29.5817198340573));
#76247=CARTESIAN_POINT('Ctrl Pts',(201.033245025523,12.4570993005867,29.6367255580705));
#76248=CARTESIAN_POINT('Ctrl Pts',(201.036255483572,12.4519282728193,29.6918337693633));
#76249=CARTESIAN_POINT('Ctrl Pts',(201.039265941621,12.4436331087229,29.746579162197));
#76250=CARTESIAN_POINT('Ctrl Pts',(201.042276399669,12.4322982433033,29.8005894080472));
#76251=CARTESIAN_POINT('Ctrl Pts',(201.044483999708,12.4239862691997,29.8401956802187));
#76252=CARTESIAN_POINT('Ctrl Pts',(201.046691599747,12.4140408024542,29.8794068140229));
#76253=CARTESIAN_POINT('Ctrl Pts',(201.048899199786,12.4025119699772,29.918081838963));
#76254=CARTESIAN_POINT('Ctrl Pts',(201.051910537605,12.3867857475464,29.9708375751519));
#76255=CARTESIAN_POINT('Ctrl Pts',(201.054921875424,12.3680460537856,30.0228144967179));
#76256=CARTESIAN_POINT('Ctrl Pts',(201.057933213243,12.3463891544883,30.0736449203786));
#76257=CARTESIAN_POINT('Ctrl Pts',(201.060939238514,12.3247704619039,30.1243856699187));
#76258=CARTESIAN_POINT('Ctrl Pts',(201.063945263785,12.3002449825008,30.173983454088));
#76259=CARTESIAN_POINT('Ctrl Pts',(201.066951289056,12.2729584725088,30.2220865441676));
#76260=CARTESIAN_POINT('Ctrl Pts',(201.069954364644,12.2456987375927,30.270142432759));
#76261=CARTESIAN_POINT('Ctrl Pts',(201.072957440232,12.2156835983674,30.3167060761311));
#76262=CARTESIAN_POINT('Ctrl Pts',(201.07596051582,12.1831057470186,30.361448223268));
#76263=CARTESIAN_POINT('Ctrl Pts',(201.078961827892,12.1505470265878,30.4061640961629));
#76264=CARTESIAN_POINT('Ctrl Pts',(201.081963139963,12.1154288870029,30.4490601673796));
#76265=CARTESIAN_POINT('Ctrl Pts',(201.084964452034,12.0779873064085,30.4898361567563));
#76266=CARTESIAN_POINT('Ctrl Pts',(201.087965184126,12.0405529610871,30.5306042665134));
#76267=CARTESIAN_POINT('Ctrl Pts',(201.090965916219,12.0007964231907,30.5692527197662));
#76268=CARTESIAN_POINT('Ctrl Pts',(201.093966648312,11.9589923933519,30.6055160964423));
#76269=CARTESIAN_POINT('Ctrl Pts',(201.096970128018,11.9171500857384,30.6418126776055));
#76270=CARTESIAN_POINT('Ctrl Pts',(201.099973607725,11.8732569402624,30.6757194729314));
#76271=CARTESIAN_POINT('Ctrl Pts',(201.102977087432,11.8276216746949,30.7070106103822));
#76272=CARTESIAN_POINT('Ctrl Pts',(201.105981946793,11.7819654464794,30.7383161214779));
#76273=CARTESIAN_POINT('Ctrl Pts',(201.108986806154,11.7345659551008,30.7670033060115));
#76274=CARTESIAN_POINT('Ctrl Pts',(201.111991665515,11.6857591266666,30.7928908191311));
#76275=CARTESIAN_POINT('Ctrl Pts',(201.115002123564,11.6368613608043,30.8188265661544));
#76276=CARTESIAN_POINT('Ctrl Pts',(201.118012581613,11.5865515004884,30.8419520010438));
#76277=CARTESIAN_POINT('Ctrl Pts',(201.121023039661,11.5351870917338,30.8621332632461));
#76278=CARTESIAN_POINT('Ctrl Pts',(201.1232306397,11.4975210392768,30.8769323916541));
#76279=CARTESIAN_POINT('Ctrl Pts',(201.12543823974,11.4592883548363,30.8901493188304));
#76280=CARTESIAN_POINT('Ctrl Pts',(201.127645839779,11.42063438191,30.9017485390594));
#76281=CARTESIAN_POINT('Ctrl Pts',(201.130657177598,11.3679073623102,30.9175707758453));
#76282=CARTESIAN_POINT('Ctrl Pts',(201.133668515417,11.3141766927841,30.930446786486));
#76283=CARTESIAN_POINT('Ctrl Pts',(201.136679853236,11.2598025327165,30.9402551489212));
#76284=CARTESIAN_POINT('Ctrl Pts',(201.139685878507,11.2055242985658,30.9500462076196));
#76285=CARTESIAN_POINT('Ctrl Pts',(201.142691903778,11.1506053419185,30.9567802654788));
#76286=CARTESIAN_POINT('Ctrl Pts',(201.145697929049,11.0954196607132,30.9603860237449));
#76287=CARTESIAN_POINT('Ctrl Pts',(201.148701004637,11.0402881308376,30.9639882438359));
#76288=CARTESIAN_POINT('Ctrl Pts',(201.151704080226,10.9848909188312,30.9644682112614));
#76289=CARTESIAN_POINT('Ctrl Pts',(201.154707155814,10.929609006691,30.9618061971619));
#76290=CARTESIAN_POINT('Ctrl Pts',(201.157708467885,10.8743595581323,30.9591457462955));
#76291=CARTESIAN_POINT('Ctrl Pts',(201.160709779956,10.8192258011874,30.9533469965259));
#76292=CARTESIAN_POINT('Ctrl Pts',(201.163711092027,10.7645882709785,30.9444423033957));
#76293=CARTESIAN_POINT('Ctrl Pts',(201.16671182412,10.7099612990164,30.9355393310232));
#76294=CARTESIAN_POINT('Ctrl Pts',(201.169712556212,10.6558308837645,30.9235316922459));
#76295=CARTESIAN_POINT('Ctrl Pts',(201.172713288305,10.6025696857297,30.9085032464638));
#76296=CARTESIAN_POINT('Ctrl Pts',(201.175716768012,10.5492597191874,30.8934610399159));
#76297=CARTESIAN_POINT('Ctrl Pts',(201.178720247718,10.4968210686832,30.8753926442385));
#76298=CARTESIAN_POINT('Ctrl Pts',(201.181723727425,10.4456120184879,30.8544320639866));
#76299=CARTESIAN_POINT('Ctrl Pts',(201.184728586786,10.3943794453159,30.8334618554514));
#76300=CARTESIAN_POINT('Ctrl Pts',(201.187733446147,10.3443780752864,30.8095970417164));
#76301=CARTESIAN_POINT('Ctrl Pts',(201.190738305508,10.2959439165109,30.7830188156461));
#76302=CARTESIAN_POINT('Ctrl Pts',(201.193748763557,10.2474195146695,30.7563910687281));
#76303=CARTESIAN_POINT('Ctrl Pts',(201.196759221606,10.2004686053393,30.7270400909435));
#76304=CARTESIAN_POINT('Ctrl Pts',(201.199769679654,10.1553993805914,30.6951912163727));
#76305=CARTESIAN_POINT('Ctrl Pts',(201.201977279693,10.1223496517097,30.6718361070795));
#76306=CARTESIAN_POINT('Ctrl Pts',(201.204184879732,10.0903111877009,30.6471386953245));
#76307=CARTESIAN_POINT('Ctrl Pts',(201.206392479772,10.0593934657064,30.6212009622026));
#76308=CARTESIAN_POINT('Ctrl Pts',(201.209362370245,10.0177997682988,30.5863068576791));
#76309=CARTESIAN_POINT('Ctrl Pts',(201.212332260719,9.9780525919316,30.5490127380806));
#76310=CARTESIAN_POINT('Ctrl Pts',(201.215302151193,9.94044673915803,30.5095440245176));
#76311=CARTESIAN_POINT('Ctrl Pts',(201.218267924276,9.90289302231497,30.4701300295144));
#76312=CARTESIAN_POINT('Ctrl Pts',(201.221233697358,9.86747512676013,30.4285477946313));
#76313=CARTESIAN_POINT('Ctrl Pts',(201.224199470441,9.83445434527412,30.3850624705351));
#76314=CARTESIAN_POINT('Ctrl Pts',(201.227162378013,9.80146546825652,30.3416191616815));
#76315=CARTESIAN_POINT('Ctrl Pts',(201.230125285585,9.77086944765679,30.296276833923));
#76316=CARTESIAN_POINT('Ctrl Pts',(201.233088193156,9.74288854327967,30.2493350621601));
#76317=CARTESIAN_POINT('Ctrl Pts',(201.236049482399,9.71492292196651,30.2024189298151));
#76318=CARTESIAN_POINT('Ctrl Pts',(201.239010771642,9.68956986442099,30.1539055502177));
#76319=CARTESIAN_POINT('Ctrl Pts',(201.241972060885,9.6670079355758,30.1041228403083));
#76320=CARTESIAN_POINT('Ctrl Pts',(201.244934752111,9.64443532507853,30.0543165614216));
#76321=CARTESIAN_POINT('Ctrl Pts',(201.247897443338,9.62465671848826,30.0032402423141));
#76322=CARTESIAN_POINT('Ctrl Pts',(201.250860134565,9.60780351635772,29.9512440591676));
#76323=CARTESIAN_POINT('Ctrl Pts',(201.253823411797,9.59094698074699,29.8992375914327));
#76324=CARTESIAN_POINT('Ctrl Pts',(201.256786689029,9.57701714999311,29.8463114209451));
#76325=CARTESIAN_POINT('Ctrl Pts',(201.259749966262,9.56609526273123,29.7928300777553));
#76326=CARTESIAN_POINT('Ctrl Pts',(201.262717941725,9.55515605898502,29.7392639407182));
#76327=CARTESIAN_POINT('Ctrl Pts',(201.265685917188,9.54723440875636,29.6851414109736));
#76328=CARTESIAN_POINT('Ctrl Pts',(201.268653892651,9.54235996429844,29.6308349201091));
#76329=CARTESIAN_POINT('Ctrl Pts',(201.271050913141,9.53842322580702,29.5869754701213));
#76330=CARTESIAN_POINT('Ctrl Pts',(201.273447933632,9.53647306489063,29.5429962617961));
#76331=CARTESIAN_POINT('Ctrl Pts',(201.275844954123,9.5365002812049,29.4990927587658));
#76332=CARTESIAN_POINT('',(201.775844954191,9.53650056016494,29.5012804696304));
#76333=CARTESIAN_POINT('Ctrl Pts',(201.275844954157,9.53650028120529,29.4990927581348));
#76334=CARTESIAN_POINT('Ctrl Pts',(201.278943009359,9.53653545725112,29.4423491981655));
#76335=CARTESIAN_POINT('Ctrl Pts',(201.282041064562,9.53987072460519,29.3857096621656));
#76336=CARTESIAN_POINT('Ctrl Pts',(201.285139119765,9.54647033012784,29.3294604186667));
#76337=CARTESIAN_POINT('Ctrl Pts',(201.288150457585,9.55288520668872,29.2747856426593));
#76338=CARTESIAN_POINT('Ctrl Pts',(201.291161795404,9.56240261438851,29.2203595877923));
#76339=CARTESIAN_POINT('Ctrl Pts',(201.294173133223,9.57499098432945,29.1665610171896));
#76340=CARTESIAN_POINT('Ctrl Pts',(201.297179158495,9.58755714609419,29.112857357059));
#76341=CARTESIAN_POINT('Ctrl Pts',(201.300185183766,9.60318339896488,29.0597794939176));
#76342=CARTESIAN_POINT('Ctrl Pts',(201.303191209037,9.62178667658693,29.0076989892691));
#76343=CARTESIAN_POINT('Ctrl Pts',(201.306194284625,9.64037169961471,28.9556695889743));
#76344=CARTESIAN_POINT('Ctrl Pts',(201.309197360213,9.6619277836783,28.9046361028439));
#76345=CARTESIAN_POINT('Ctrl Pts',(201.312200435801,9.68632175902193,28.8549560253899));
#76346=CARTESIAN_POINT('Ctrl Pts',(201.315201747872,9.71070140932188,28.8053051219131));
#76347=CARTESIAN_POINT('Ctrl Pts',(201.318203059943,9.73791541548378,28.7570065243937));
#76348=CARTESIAN_POINT('Ctrl Pts',(201.321204372014,9.76778298274491,28.7103966360337));
#76349=CARTESIAN_POINT('Ctrl Pts',(201.324205104106,9.79764477834792,28.6637957546456));
#76350=CARTESIAN_POINT('Ctrl Pts',(201.327205836199,9.83015883205242,28.6188833782219));
#76351=CARTESIAN_POINT('Ctrl Pts',(201.330206568291,9.86510020624162,28.575968232079));
#76352=CARTESIAN_POINT('Ctrl Pts',(201.333210047998,9.90007357442893,28.53301379077));
#76353=CARTESIAN_POINT('Ctrl Pts',(201.336213527704,9.93747836937182,28.4920606430972));
#76354=CARTESIAN_POINT('Ctrl Pts',(201.339217007411,9.97704933920155,28.4533844088817));
#76355=CARTESIAN_POINT('Ctrl Pts',(201.342221866771,10.0166384860332,28.4146904086627));
#76356=CARTESIAN_POINT('Ctrl Pts',(201.345226726132,10.0583953929353,28.3782757541214));
#76357=CARTESIAN_POINT('Ctrl Pts',(201.348231585493,10.1020203443707,28.3443768832029));
#76358=CARTESIAN_POINT('Ctrl Pts',(201.351242043541,10.1457265783032,28.3104148515292));
#76359=CARTESIAN_POINT('Ctrl Pts',(201.35425250159,10.1913073739994,28.2789782669899));
#76360=CARTESIAN_POINT('Ctrl Pts',(201.357262959638,10.2384335485633,28.250260511128));
#76361=CARTESIAN_POINT('Ctrl Pts',(201.359470559677,10.2729916600327,28.229201483583));
#76362=CARTESIAN_POINT('Ctrl Pts',(201.361678159716,10.308380177473,28.2096035715251));
#76363=CARTESIAN_POINT('Ctrl Pts',(201.363885759755,10.3444620337117,28.1915267581053));
#76364=CARTESIAN_POINT('Ctrl Pts',(201.366897097574,10.3936804864861,28.1668685813825));
#76365=CARTESIAN_POINT('Ctrl Pts',(201.369908435393,10.4443945319431,28.1449400134599));
#76366=CARTESIAN_POINT('Ctrl Pts',(201.372919773213,10.496270272697,28.1259226325162));
#76367=CARTESIAN_POINT('Ctrl Pts',(201.375925798484,10.5480544952006,28.1069388016944));
#76368=CARTESIAN_POINT('Ctrl Pts',(201.378931823755,10.6009958543138,28.0908561455167));
#76369=CARTESIAN_POINT('Ctrl Pts',(201.381937849026,10.6547381965548,28.0778092472942));
#76370=CARTESIAN_POINT('Ctrl Pts',(201.384940924614,10.7084278037525,28.0647751514305));
#76371=CARTESIAN_POINT('Ctrl Pts',(201.387944000202,10.7629163267984,28.0547710361226));
#76372=CARTESIAN_POINT('Ctrl Pts',(201.39094707579,10.8178318595013,28.0478818854559));
#76373=CARTESIAN_POINT('Ctrl Pts',(201.393948387861,10.8727151437743,28.040996780353));
#76374=CARTESIAN_POINT('Ctrl Pts',(201.396949699932,10.9280244181891,28.037223079588));
#76375=CARTESIAN_POINT('Ctrl Pts',(201.399951012004,10.9833792554417,28.0365943826641));
#76376=CARTESIAN_POINT('Ctrl Pts',(201.402951744096,11.0387233958339,28.0359658072306));
#76377=CARTESIAN_POINT('Ctrl Pts',(201.405952476189,11.0941125543052,28.0384810344984));
#76378=CARTESIAN_POINT('Ctrl Pts',(201.408953208282,11.1491651992981,28.0441215733042));
#76379=CARTESIAN_POINT('Ctrl Pts',(201.411956687989,11.2042682531333,28.0497672768578));
#76380=CARTESIAN_POINT('Ctrl Pts',(201.414960167696,11.2590336519833,28.0585439549238));
#76381=CARTESIAN_POINT('Ctrl Pts',(201.417963647403,11.3130853984731,28.0703812454843));
#76382=CARTESIAN_POINT('Ctrl Pts',(201.420968506764,11.3671619737377,28.0822239735272));
#76383=CARTESIAN_POINT('Ctrl Pts',(201.423973366125,11.4205237341886,28.0971299743663));
#76384=CARTESIAN_POINT('Ctrl Pts',(201.426978225487,11.4728085074863,28.1149785686681));
#76385=CARTESIAN_POINT('Ctrl Pts',(201.429988683535,11.5251906983579,28.1328604186703));
#76386=CARTESIAN_POINT('Ctrl Pts',(201.432999141584,11.5764914038044,28.1536956149628));
#76387=CARTESIAN_POINT('Ctrl Pts',(201.436009599633,11.6263682580533,28.1773152093929));
#76388=CARTESIAN_POINT('Ctrl Pts',(201.438217199672,11.6629434713964,28.1946357024026));
#76389=CARTESIAN_POINT('Ctrl Pts',(201.440424799711,11.6987534486628,28.2134524728893));
#76390=CARTESIAN_POINT('Ctrl Pts',(201.44263239975,11.7336727990414,28.2336838965145));
#76391=CARTESIAN_POINT('Ctrl Pts',(201.44564373757,11.7813055035869,28.2612811288119));
#76392=CARTESIAN_POINT('Ctrl Pts',(201.448655075389,11.8274780115704,28.291627067655));
#76393=CARTESIAN_POINT('Ctrl Pts',(201.451666413208,11.8718552337559,28.3245423438625));
#76394=CARTESIAN_POINT('Ctrl Pts',(201.454672438479,11.916154166443,28.3573995515308));
#76395=CARTESIAN_POINT('Ctrl Pts',(201.45767846375,11.9586636784989,28.3928167891312));
#76396=CARTESIAN_POINT('Ctrl Pts',(201.460684489021,11.9990757383647,28.4305702832766));
#76397=CARTESIAN_POINT('Ctrl Pts',(201.463687564609,12.0394481436184,28.4682867315459));
#76398=CARTESIAN_POINT('Ctrl Pts',(201.466690640197,12.0777267902844,28.5083345364326));
#76399=CARTESIAN_POINT('Ctrl Pts',(201.469693715785,12.1136364518988,28.550449525827));
#76400=CARTESIAN_POINT('Ctrl Pts',(201.472695027857,12.1495250260331,28.5925397837434));
#76401=CARTESIAN_POINT('Ctrl Pts',(201.475696339928,12.183047030988,28.6366944192596));
#76402=CARTESIAN_POINT('Ctrl Pts',(201.478697651999,12.2139655081345,28.6826139253329));
#76403=CARTESIAN_POINT('Ctrl Pts',(201.481698384091,12.2448780105433,28.7285245578448));
#76404=CARTESIAN_POINT('Ctrl Pts',(201.484699116184,12.2731876899333,28.7761989461178));
#76405=CARTESIAN_POINT('Ctrl Pts',(201.487699848276,12.2987005179312,28.8253080593891));
#76406=CARTESIAN_POINT('Ctrl Pts',(201.490703327983,12.324236706698,28.8744621393199));
#76407=CARTESIAN_POINT('Ctrl Pts',(201.49370680769,12.3469706842946,28.9250530994976));
#76408=CARTESIAN_POINT('Ctrl Pts',(201.496710287397,12.3667548137752,28.9767280544285));
#76409=CARTESIAN_POINT('Ctrl Pts',(201.499715146758,12.3865480311342,29.0284267463503));
#76410=CARTESIAN_POINT('Ctrl Pts',(201.502720006119,12.4033885386845,29.0812099221252));
#76411=CARTESIAN_POINT('Ctrl Pts',(201.50572486548,12.4171783446443,29.1347086238752));
#76412=CARTESIAN_POINT('Ctrl Pts',(201.508735323528,12.4309938439247,29.1883070050041));
#76413=CARTESIAN_POINT('Ctrl Pts',(201.511745781577,12.4417471847588,29.2426230564507));
#76414=CARTESIAN_POINT('Ctrl Pts',(201.514756239625,12.4493915926365,29.297277871966));
#76415=CARTESIAN_POINT('Ctrl Pts',(201.516963839664,12.454997316037,29.3373568137478));
#76416=CARTESIAN_POINT('Ctrl Pts',(201.519171439703,12.4589323153221,29.3776177266039));
#76417=CARTESIAN_POINT('Ctrl Pts',(201.521379039742,12.4611959639813,29.417910994373));
#76418=CARTESIAN_POINT('Ctrl Pts',(201.524390377561,12.464283756469,29.4728741393917));
#76419=CARTESIAN_POINT('Ctrl Pts',(201.527401715381,12.4642724907512,29.5281260748405));
#76420=CARTESIAN_POINT('Ctrl Pts',(201.5304130532,12.4611280972899,29.583288254334));
#76421=CARTESIAN_POINT('Ctrl Pts',(201.533419078471,12.4579892511111,29.638353117701));
#76422=CARTESIAN_POINT('Ctrl Pts',(201.536425103742,12.4517282765108,29.6933280168053));
#76423=CARTESIAN_POINT('Ctrl Pts',(201.539431129013,12.4423630725208,29.7478326391505));
#76424=CARTESIAN_POINT('Ctrl Pts',(201.542434204601,12.4330070582018,29.8022837784598));
#76425=CARTESIAN_POINT('Ctrl Pts',(201.545437280189,12.4205529377773,29.8562650377195));
#76426=CARTESIAN_POINT('Ctrl Pts',(201.548440355777,12.4050703867959,29.9094013411669));
#76427=CARTESIAN_POINT('Ctrl Pts',(201.551441667848,12.3895969277405,29.9625064410135));
#76428=CARTESIAN_POINT('Ctrl Pts',(201.554442979919,12.3710987105516,30.0147670630399));
#76429=CARTESIAN_POINT('Ctrl Pts',(201.557444291991,12.3496959544205,30.0658207142028));
#76430=CARTESIAN_POINT('Ctrl Pts',(201.560445024083,12.3282973341934,30.1168644996736));
#76431=CARTESIAN_POINT('Ctrl Pts',(201.563445756176,12.3039954937234,30.166701291245));
#76432=CARTESIAN_POINT('Ctrl Pts',(201.566446488269,12.276958898865,30.2149882660642));
#76433=CARTESIAN_POINT('Ctrl Pts',(201.569449967975,12.2498975480036,30.2633194547535));
#76434=CARTESIAN_POINT('Ctrl Pts',(201.572453447682,12.2200966986014,30.3100975304298));
#76435=CARTESIAN_POINT('Ctrl Pts',(201.575456927389,12.1877702255091,30.3550053458277));
#76436=CARTESIAN_POINT('Ctrl Pts',(201.57846178675,12.1554289031886,30.399933789718));
#76437=CARTESIAN_POINT('Ctrl Pts',(201.581466646111,12.1205599771605,30.4429898501169));
#76438=CARTESIAN_POINT('Ctrl Pts',(201.584471505473,12.0834180133996,30.4838890477291));
#76439=CARTESIAN_POINT('Ctrl Pts',(201.587481963521,12.0462068463168,30.5248644491834));
#76440=CARTESIAN_POINT('Ctrl Pts',(201.59049242157,12.006714558814,30.5636745897608));
#76441=CARTESIAN_POINT('Ctrl Pts',(201.593502879618,11.9652321528155,30.6000723345176));
#76442=CARTESIAN_POINT('Ctrl Pts',(201.595710479658,11.9348126752392,30.6267631773897));
#76443=CARTESIAN_POINT('Ctrl Pts',(201.597918079697,11.9033237844964,30.652157568172));
#76444=CARTESIAN_POINT('Ctrl Pts',(201.600125679736,11.8708901834167,30.6761728352706));
#76445=CARTESIAN_POINT('Ctrl Pts',(201.603137017555,11.8266482338728,30.7089315237877));
#76446=CARTESIAN_POINT('Ctrl Pts',(201.606148355374,11.780463354822,30.7392586312133));
#76447=CARTESIAN_POINT('Ctrl Pts',(201.609159693193,11.7326332231879,30.7669178388046));
#76448=CARTESIAN_POINT('Ctrl Pts',(201.612165718464,11.6848874726131,30.7945282505186));
#76449=CARTESIAN_POINT('Ctrl Pts',(201.615171743736,11.6355026828221,30.8194798410846));
#76450=CARTESIAN_POINT('Ctrl Pts',(201.618177769007,11.5848065405911,30.8415787565707));
#76451=CARTESIAN_POINT('Ctrl Pts',(201.621180844595,11.5341601442987,30.8636559873439));
#76452=CARTESIAN_POINT('Ctrl Pts',(201.624183920183,11.4822054260415,30.8828858785978));
#76453=CARTESIAN_POINT('Ctrl Pts',(201.627186995771,11.429294124133,30.8991207256648));
#76454=CARTESIAN_POINT('Ctrl Pts',(201.630188307842,11.376413893696,30.9153460390298));
#76455=CARTESIAN_POINT('Ctrl Pts',(201.633189619913,11.3225786964833,30.9285796400069));
#76456=CARTESIAN_POINT('Ctrl Pts',(201.636190931984,11.2681575057671,30.9387229761496));
#76457=CARTESIAN_POINT('Ctrl Pts',(201.639191664077,11.2137468314919,30.9488643521772));
#76458=CARTESIAN_POINT('Ctrl Pts',(201.642192396169,11.1587509070089,30.9559165528706));
#76459=CARTESIAN_POINT('Ctrl Pts',(201.645193128262,11.1035487557779,30.9598321496586));
#76460=CARTESIAN_POINT('Ctrl Pts',(201.648196607969,11.0482960588096,30.9637513317548));
#76461=CARTESIAN_POINT('Ctrl Pts',(201.651200087676,10.9928372852408,30.9645281350195));
#76462=CARTESIAN_POINT('Ctrl Pts',(201.654203567382,10.9375549314591,30.9621671803918));
#76463=CARTESIAN_POINT('Ctrl Pts',(201.657208426743,10.8822471836207,30.959805141255));
#76464=CARTESIAN_POINT('Ctrl Pts',(201.660213286104,10.8271165429726,30.9543025235911));
#76465=CARTESIAN_POINT('Ctrl Pts',(201.663218145466,10.7725405443215,30.945715893951));
#76466=CARTESIAN_POINT('Ctrl Pts',(201.666228603514,10.7178628590599,30.9371132656065));
#76467=CARTESIAN_POINT('Ctrl Pts',(201.669239061563,10.6637423969213,30.9254152588641));
#76468=CARTESIAN_POINT('Ctrl Pts',(201.672249519611,10.6105454863477,30.9107293970836));
#76469=CARTESIAN_POINT('Ctrl Pts',(201.67445711965,10.5715356413456,30.8999601026715));
#76470=CARTESIAN_POINT('Ctrl Pts',(201.67666471969,10.5330221805194,30.8875851821225));
#76471=CARTESIAN_POINT('Ctrl Pts',(201.678872319729,10.4951426685791,30.8736634685797));
#76472=CARTESIAN_POINT('Ctrl Pts',(201.681883657548,10.4434720738802,30.8546731706288));
#76473=CARTESIAN_POINT('Ctrl Pts',(201.684894995367,10.3927669749891,30.8327239236214));
#76474=CARTESIAN_POINT('Ctrl Pts',(201.687906333186,10.3433883253009,30.8079347684991));
#76475=CARTESIAN_POINT('Ctrl Pts',(201.690912358457,10.2940967885397,30.7831893459591));
#76476=CARTESIAN_POINT('Ctrl Pts',(201.693918383728,10.2461275246584,30.7556141930645));
#76477=CARTESIAN_POINT('Ctrl Pts',(201.696924408999,10.1998224727877,30.7253767481654));
#76478=CARTESIAN_POINT('Ctrl Pts',(201.699927484587,10.153562858068,30.6951689739673));
#76479=CARTESIAN_POINT('Ctrl Pts',(201.702930560175,10.1089646598888,30.6623043701208));
#76480=CARTESIAN_POINT('Ctrl Pts',(201.705933635763,10.0663444522473,30.6269958154983));
#76481=CARTESIAN_POINT('Ctrl Pts',(201.708934947835,10.0237492727665,30.5917079953636));
#76482=CARTESIAN_POINT('Ctrl Pts',(201.711936259906,9.98313018691714,30.5539794051631));
#76483=CARTESIAN_POINT('Ctrl Pts',(201.714937571977,9.94477215104161,30.5140643159005));
#76484=CARTESIAN_POINT('Ctrl Pts',(201.717938304069,9.9064215275364,30.4741569398957));
#76485=CARTESIAN_POINT('Ctrl Pts',(201.720939036162,9.87033145153059,30.4320642842625));
#76486=CARTESIAN_POINT('Ctrl Pts',(201.723939768255,9.83674966897721,30.3880770897706));
#76487=CARTESIAN_POINT('Ctrl Pts',(201.726943247961,9.80313713733304,30.3440496184936));
#76488=CARTESIAN_POINT('Ctrl Pts',(201.729946727668,9.77203780817293,30.2981245630788));
#76489=CARTESIAN_POINT('Ctrl Pts',(201.732950207375,9.74365783213183,30.2506241451194));
#76490=CARTESIAN_POINT('Ctrl Pts',(201.735955066736,9.71526481969356,30.2031019077508));
#76491=CARTESIAN_POINT('Ctrl Pts',(201.738959926097,9.68959389524046,30.154003333666));
#76492=CARTESIAN_POINT('Ctrl Pts',(201.741964785458,9.66680506989105,30.1036750188071));
#76493=CARTESIAN_POINT('Ctrl Pts',(201.744975243507,9.6439737841476,30.0532529316696));
#76494=CARTESIAN_POINT('Ctrl Pts',(201.747985701555,9.62403551457131,30.0015970201963));
#76495=CARTESIAN_POINT('Ctrl Pts',(201.750996159604,9.60710153044035,29.9490724924758));
#76496=CARTESIAN_POINT('Ctrl Pts',(201.753203759643,9.59468366464524,29.9105557127776));
#76497=CARTESIAN_POINT('Ctrl Pts',(201.755411359682,9.5838802995295,29.8715722210717));
#76498=CARTESIAN_POINT('Ctrl Pts',(201.757618959721,9.57471779430217,29.8322692945807));
#76499=CARTESIAN_POINT('Ctrl Pts',(201.761619230085,9.55811492355215,29.7610506275853));
#76500=CARTESIAN_POINT('Ctrl Pts',(201.765619500448,9.54684447122907,29.6885456861229));
#76501=CARTESIAN_POINT('Ctrl Pts',(201.769619770812,9.54105985342675,29.6154378565152));
#76502=CARTESIAN_POINT('Ctrl Pts',(201.771694831927,9.53805919737696,29.577514616174));
#76503=CARTESIAN_POINT('Ctrl Pts',(201.773769893042,9.53653393815549,29.5394294781608));
#76504=CARTESIAN_POINT('Ctrl Pts',(201.775844954157,9.53650056016549,29.5012804702496));
#76505=CARTESIAN_POINT('',(202.275844954211,9.5365001227665,29.4994005523254));
#76506=CARTESIAN_POINT('Ctrl Pts',(201.775844954191,9.53650056016494,29.5012804696304));
#76507=CARTESIAN_POINT('Ctrl Pts',(201.778811262791,9.53645284621078,29.4467463022148));
#76508=CARTESIAN_POINT('Ctrl Pts',(201.781777571391,9.53945754436547,29.3921280057072));
#76509=CARTESIAN_POINT('Ctrl Pts',(201.78474387999,9.5455162473522,29.3377986951854));
#76510=CARTESIAN_POINT('Ctrl Pts',(201.787707949009,9.55157037598047,29.2835104036311));
#76511=CARTESIAN_POINT('Ctrl Pts',(201.790672018027,9.56067388448575,29.2295112035404));
#76512=CARTESIAN_POINT('Ctrl Pts',(201.793636087046,9.5727763727872,29.1761713911256));
#76513=CARTESIAN_POINT('Ctrl Pts',(201.796599159415,9.5848747917047,29.1228495138801));
#76514=CARTESIAN_POINT('Ctrl Pts',(201.799562231785,9.59997007127091,29.0701871133066));
#76515=CARTESIAN_POINT('Ctrl Pts',(201.802525304154,9.61796076786666,29.0185440717529));
#76516=CARTESIAN_POINT('Ctrl Pts',(201.805490722761,9.63596570996164,28.9668601379022));
#76517=CARTESIAN_POINT('Ctrl Pts',(201.808456141367,9.65687047392248,28.9161976901676));
#76518=CARTESIAN_POINT('Ctrl Pts',(201.811421559974,9.68052431889611,28.866899552223));
#76519=CARTESIAN_POINT('Ctrl Pts',(201.814388093819,9.70418705963906,28.8175828741694));
#76520=CARTESIAN_POINT('Ctrl Pts',(201.817354627664,9.7306006801876,28.7696320047885));
#76521=CARTESIAN_POINT('Ctrl Pts',(201.82032116151,9.75956859734311,28.7233648312736));
#76522=CARTESIAN_POINT('Ctrl Pts',(201.823293215422,9.78859041741771,28.6770115647304));
#76523=CARTESIAN_POINT('Ctrl Pts',(201.826265269334,9.82017571292884,28.632348695266));
#76524=CARTESIAN_POINT('Ctrl Pts',(201.829237323245,9.85408550628692,28.5896636758328));
#76525=CARTESIAN_POINT('Ctrl Pts',(201.831613415402,9.88119564506759,28.5555379355645));
#76526=CARTESIAN_POINT('Ctrl Pts',(201.833989507558,9.90979064007753,28.5226758097128));
#76527=CARTESIAN_POINT('Ctrl Pts',(201.836365599714,9.93973182930301,28.4912068318001));
#76528=CARTESIAN_POINT('Ctrl Pts',(201.839376937533,9.97767776302064,28.4513246567453));
#76529=CARTESIAN_POINT('Ctrl Pts',(201.842388275352,10.0179560153532,28.4135035133625));
#76530=CARTESIAN_POINT('Ctrl Pts',(201.845399613171,10.060314008029,28.3780274127709));
#76531=CARTESIAN_POINT('Ctrl Pts',(201.848405638443,10.1025972734949,28.3426138984789));
#76532=CARTESIAN_POINT('Ctrl Pts',(201.851411663714,10.1469525965704,28.3095375527112));
#76533=CARTESIAN_POINT('Ctrl Pts',(201.854417688985,10.1930905304169,28.2790457183428));
#76534=CARTESIAN_POINT('Ctrl Pts',(201.857420764573,10.2391831910981,28.2485838042968));
#76535=CARTESIAN_POINT('Ctrl Pts',(201.860423840161,10.2870545592629,28.2207016670607));
#76536=CARTESIAN_POINT('Ctrl Pts',(201.863426915749,10.3363835550428,28.1956053266046));
#76537=CARTESIAN_POINT('Ctrl Pts',(201.86642822782,10.3856835830137,28.1705237236468));
#76538=CARTESIAN_POINT('Ctrl Pts',(201.869429539891,10.4364390725868,28.1482249135451));
#76539=CARTESIAN_POINT('Ctrl Pts',(201.872430851962,10.4883035091198,28.1288694623702));
#76540=CARTESIAN_POINT('Ctrl Pts',(201.875431584055,10.5401579232833,28.1095177514748));
#76541=CARTESIAN_POINT('Ctrl Pts',(201.878432316147,10.5931203647429,28.0931084541402));
#76542=CARTESIAN_POINT('Ctrl Pts',(201.88143304824,10.6468256224804,28.0797535041185));
#76543=CARTESIAN_POINT('Ctrl Pts',(201.884436527947,10.7005800553277,28.0663863256641));
#76544=CARTESIAN_POINT('Ctrl Pts',(201.887440007654,10.7550781501432,28.0560792091638));
#76545=CARTESIAN_POINT('Ctrl Pts',(201.89044348736,10.8099423194507,28.0488934125764));
#76546=CARTESIAN_POINT('Ctrl Pts',(201.893448346721,10.8648316907211,28.0417043151793));
#76547=CARTESIAN_POINT('Ctrl Pts',(201.896453206083,10.9200869446324,28.0376394345377));
#76548=CARTESIAN_POINT('Ctrl Pts',(201.899458065444,10.9753264438558,28.0367080039762));
#76549=CARTESIAN_POINT('Ctrl Pts',(201.902468523492,11.0306688659314,28.0357748379629));
#76550=CARTESIAN_POINT('Ctrl Pts',(201.905478981541,11.0859949463211,28.0379867630428));
#76551=CARTESIAN_POINT('Ctrl Pts',(201.908489439589,11.1409253196295,28.0433008875244));
#76552=CARTESIAN_POINT('Ctrl Pts',(201.910697039628,11.1812063307928,28.0471977899969));
#76553=CARTESIAN_POINT('Ctrl Pts',(201.912904639668,11.2212746142991,28.0527617795955));
#76554=CARTESIAN_POINT('Ctrl Pts',(201.915112239707,11.2609845343961,28.0599585690661));
#76555=CARTESIAN_POINT('Ctrl Pts',(201.918123577526,11.3151519479069,28.0697755485578));
#76556=CARTESIAN_POINT('Ctrl Pts',(201.921134915345,11.3688773621993,28.0826734691986));
#76557=CARTESIAN_POINT('Ctrl Pts',(201.924146253164,11.421784725125,28.098597168673));
#76558=CARTESIAN_POINT('Ctrl Pts',(201.927152278435,11.4745987498313,28.1144927758429));
#76559=CARTESIAN_POINT('Ctrl Pts',(201.930158303706,11.5265970860914,28.1334034173089));
#76560=CARTESIAN_POINT('Ctrl Pts',(201.933164328977,11.57741408551,28.1552229835937));
#76561=CARTESIAN_POINT('Ctrl Pts',(201.936167404565,11.6281812203981,28.1770211392788));
#76562=CARTESIAN_POINT('Ctrl Pts',(201.939170480153,11.677768832408,28.2017223579122));
#76563=CARTESIAN_POINT('Ctrl Pts',(201.942173555742,11.7258284418033,28.2291714029542));
#76564=CARTESIAN_POINT('Ctrl Pts',(201.945174867813,11.7738598288201,28.2566043289027));
#76565=CARTESIAN_POINT('Ctrl Pts',(201.948176179884,11.8203645345873,28.286781621612));
#76566=CARTESIAN_POINT('Ctrl Pts',(201.951177491955,11.8650181038493,28.3195018297291));
#76567=CARTESIAN_POINT('Ctrl Pts',(201.954178224047,11.9096630441817,28.3522157149391));
#76568=CARTESIAN_POINT('Ctrl Pts',(201.95717895614,11.952457133182,28.3874712278554));
#76569=CARTESIAN_POINT('Ctrl Pts',(201.960179688233,11.9931062963205,28.4250245890214));
#76570=CARTESIAN_POINT('Ctrl Pts',(201.96318316794,12.0337926797825,28.4626123358461));
#76571=CARTESIAN_POINT('Ctrl Pts',(201.966186647646,12.072329825509,28.5025017754049));
#76572=CARTESIAN_POINT('Ctrl Pts',(201.969190127353,12.1084592176021,28.5444109602381));
#76573=CARTESIAN_POINT('Ctrl Pts',(201.972194986714,12.1446052058017,28.5863393961369));
#76574=CARTESIAN_POINT('Ctrl Pts',(201.975199846075,12.1783409138953,28.6302890074987));
#76575=CARTESIAN_POINT('Ctrl Pts',(201.978204705437,12.2094490837466,28.6759458975137));
#76576=CARTESIAN_POINT('Ctrl Pts',(201.981215163485,12.2406152146876,28.7216878559564));
#76577=CARTESIAN_POINT('Ctrl Pts',(201.984225621534,12.2691437557156,28.7691429940413));
#76578=CARTESIAN_POINT('Ctrl Pts',(201.987236079582,12.2948622613818,28.8179706941419));
#76579=CARTESIAN_POINT('Ctrl Pts',(201.989443679622,12.3137219077204,28.8537765518919));
#76580=CARTESIAN_POINT('Ctrl Pts',(201.991651279661,12.3310714291689,28.8903199429348));
#76581=CARTESIAN_POINT('Ctrl Pts',(201.9938588797,12.3468595199812,28.9274603215182));
#76582=CARTESIAN_POINT('Ctrl Pts',(201.996870217519,12.3683957014059,28.9781226809425));
#76583=CARTESIAN_POINT('Ctrl Pts',(201.999881555338,12.3871141977066,29.0301072401307));
#76584=CARTESIAN_POINT('Ctrl Pts',(202.002892893157,12.4028546381928,29.0830694133301));
#76585=CARTESIAN_POINT('Ctrl Pts',(202.005898918428,12.4185673096767,29.1359381516147));
#76586=CARTESIAN_POINT('Ctrl Pts',(202.008904943699,12.4313122028411,29.1897805794268));
#76587=CARTESIAN_POINT('Ctrl Pts',(202.01191096897,12.4409772400928,29.2442328333534));
#76588=CARTESIAN_POINT('Ctrl Pts',(202.014914044558,12.4506327934602,29.298631655631));
#76589=CARTESIAN_POINT('Ctrl Pts',(202.017917120147,12.4572143861445,29.3536386015974));
#76590=CARTESIAN_POINT('Ctrl Pts',(202.020920195735,12.4606604267649,29.4088771835215));
#76591=CARTESIAN_POINT('Ctrl Pts',(202.023921507806,12.4641044437429,29.4640833273092));
#76592=CARTESIAN_POINT('Ctrl Pts',(202.026922819877,12.4644165256822,29.5195203118828));
#76593=CARTESIAN_POINT('Ctrl Pts',(202.029924131948,12.4615868976476,29.5748063541742));
#76594=CARTESIAN_POINT('Ctrl Pts',(202.032924864041,12.458757816415,29.6300817128994));
#76595=CARTESIAN_POINT('Ctrl Pts',(202.035925596133,12.4527882580257,29.6852056606625));
#76596=CARTESIAN_POINT('Ctrl Pts',(202.038926328226,12.4437205054879,29.7397985655371));
#76597=CARTESIAN_POINT('Ctrl Pts',(202.041929807933,12.4346444500811,29.7944414582938));
#76598=CARTESIAN_POINT('Ctrl Pts',(202.044933287639,12.4224646198972,29.8485518152115));
#76599=CARTESIAN_POINT('Ctrl Pts',(202.047936767346,12.4072747219128,29.9017587672537));
#76600=CARTESIAN_POINT('Ctrl Pts',(202.050941626707,12.3920778464193,29.9549901600128));
#76601=CARTESIAN_POINT('Ctrl Pts',(202.053946486068,12.373868320616,30.0073168215674));
#76602=CARTESIAN_POINT('Ctrl Pts',(202.056951345429,12.3527892071491,30.0583848234157));
#76603=CARTESIAN_POINT('Ctrl Pts',(202.059961803478,12.3316708188424,30.1095479757358));
#76604=CARTESIAN_POINT('Ctrl Pts',(202.062972261527,12.3076723919677,30.1594473073083));
#76605=CARTESIAN_POINT('Ctrl Pts',(202.065982719575,12.2809839267766,30.2077516720857));
#76606=CARTESIAN_POINT('Ctrl Pts',(202.068190319614,12.2614129990811,30.2431737626279));
#76607=CARTESIAN_POINT('Ctrl Pts',(202.070397919654,12.2403965064129,30.2777386633128));
#76608=CARTESIAN_POINT('Ctrl Pts',(202.072605519693,12.2180237448525,30.3113263258243));
#76609=CARTESIAN_POINT('Ctrl Pts',(202.075616857512,12.1875055613897,30.3571425047454));
#76610=CARTESIAN_POINT('Ctrl Pts',(202.078628195331,12.1543352314198,30.4013296715185));
#76611=CARTESIAN_POINT('Ctrl Pts',(202.08163953315,12.1187127014353,30.4435645932565));
#76612=CARTESIAN_POINT('Ctrl Pts',(202.084645558421,12.0831530160784,30.4857250049041));
#76613=CARTESIAN_POINT('Ctrl Pts',(202.087651583692,12.0451500536704,30.5259396065147));
#76614=CARTESIAN_POINT('Ctrl Pts',(202.090657608963,12.0049463883838,30.5639149432518));
#76615=CARTESIAN_POINT('Ctrl Pts',(202.093660684551,11.9647821732205,30.6018530164282));
#76616=CARTESIAN_POINT('Ctrl Pts',(202.096663760139,11.9224219148628,30.6375558171404));
#76617=CARTESIAN_POINT('Ctrl Pts',(202.099666835728,11.8781464585529,30.6707651546451));
#76618=CARTESIAN_POINT('Ctrl Pts',(202.102668147799,11.8338970024269,30.7039549903997));
#76619=CARTESIAN_POINT('Ctrl Pts',(202.10566945987,11.7877349988977,30.7346539494039));
#76620=CARTESIAN_POINT('Ctrl Pts',(202.108670771941,11.7399741692062,30.7626442408325));
#76621=CARTESIAN_POINT('Ctrl Pts',(202.111671504034,11.6922225688966,30.7906291233709));
#76622=CARTESIAN_POINT('Ctrl Pts',(202.114672236126,11.642873211028,30.8159061113701));
#76623=CARTESIAN_POINT('Ctrl Pts',(202.117672968219,11.5922666017872,30.8383021043126));
#76624=CARTESIAN_POINT('Ctrl Pts',(202.120676447926,11.5416136547077,30.8607186041003));
#76625=CARTESIAN_POINT('Ctrl Pts',(202.123679927632,11.4897016399509,30.8802486249136));
#76626=CARTESIAN_POINT('Ctrl Pts',(202.126683407339,11.4368919745653,30.8967668569093));
#76627=CARTESIAN_POINT('Ctrl Pts',(202.1296882667,11.3840580509573,30.9132926765871));
#76628=CARTESIAN_POINT('Ctrl Pts',(202.132693126061,11.3303261672975,30.9268038207952));
#76629=CARTESIAN_POINT('Ctrl Pts',(202.135697985423,11.2760706811343,30.9372255317166));
#76630=CARTESIAN_POINT('Ctrl Pts',(202.138708443471,11.2217141055429,30.9476666604862));
#76631=CARTESIAN_POINT('Ctrl Pts',(202.14171890152,11.1668325028109,30.9550067875569));
#76632=CARTESIAN_POINT('Ctrl Pts',(202.144729359568,11.1118069607444,30.9592228937106));
#76633=CARTESIAN_POINT('Ctrl Pts',(202.146936959608,11.0714561613462,30.9623146079811));
#76634=CARTESIAN_POINT('Ctrl Pts',(202.149144559647,11.0310280885006,30.9637274948763));
#76635=CARTESIAN_POINT('Ctrl Pts',(202.151352159686,10.990672105428,30.9634702731463));
#76636=CARTESIAN_POINT('Ctrl Pts',(202.154363497505,10.9356234118671,30.9631194027396));
#76637=CARTESIAN_POINT('Ctrl Pts',(202.157374835324,10.8804800383442,30.9596574879137));
#76638=CARTESIAN_POINT('Ctrl Pts',(202.160386173143,10.8256219200354,30.9530741671463));
#76639=CARTESIAN_POINT('Ctrl Pts',(202.163392198414,10.7708605814337,30.9465024605551));
#76640=CARTESIAN_POINT('Ctrl Pts',(202.166398223685,10.7163840190019,30.9368203388821));
#76641=CARTESIAN_POINT('Ctrl Pts',(202.169404248956,10.6625706849657,30.9240694180255));
#76642=CARTESIAN_POINT('Ctrl Pts',(202.172407324544,10.6088101556342,30.9113310090978));
#76643=CARTESIAN_POINT('Ctrl Pts',(202.175410400133,10.5557120763433,30.8955298875416));
#76644=CARTESIAN_POINT('Ctrl Pts',(202.178413475721,10.5036464391887,30.8767590176461));
#76645=CARTESIAN_POINT('Ctrl Pts',(202.181414787792,10.4516113769001,30.8579991706991));
#76646=CARTESIAN_POINT('Ctrl Pts',(202.184416099863,10.4006080503334,30.8362732108151));
#76647=CARTESIAN_POINT('Ctrl Pts',(202.187417411934,10.3509907368055,30.8117237614253));
#76648=CARTESIAN_POINT('Ctrl Pts',(202.190418144027,10.3013830114092,30.7871790560117));
#76649=CARTESIAN_POINT('Ctrl Pts',(202.193418876119,10.2531612396853,30.7598121786561));
#76650=CARTESIAN_POINT('Ctrl Pts',(202.196419608212,10.2066570539907,30.7298126767997));
#76651=CARTESIAN_POINT('Ctrl Pts',(202.199423087919,10.1601102868333,30.6997857059606));
#76652=CARTESIAN_POINT('Ctrl Pts',(202.202426567625,10.1152846918199,30.6671215815921));
#76653=CARTESIAN_POINT('Ctrl Pts',(202.205430047332,10.0724834398953,30.6320535679602));
#76654=CARTESIAN_POINT('Ctrl Pts',(202.208434906693,10.0296625271324,30.5969694457681));
#76655=CARTESIAN_POINT('Ctrl Pts',(202.211439766054,9.98886820018554,30.559479590762));
#76656=CARTESIAN_POINT('Ctrl Pts',(202.214444625415,9.95036848450246,30.5198558386725));
#76657=CARTESIAN_POINT('Ctrl Pts',(202.217455083464,9.91179703571885,30.4801582591652));
#76658=CARTESIAN_POINT('Ctrl Pts',(202.220465541513,9.87552908468643,30.4383192401548));
#76659=CARTESIAN_POINT('Ctrl Pts',(202.223475999561,9.84179310985319,30.3946446499122));
#76660=CARTESIAN_POINT('Ctrl Pts',(202.2256835996,9.81705417041017,30.3626176209453));
#76661=CARTESIAN_POINT('Ctrl Pts',(202.227891199639,9.79367594071422,30.3296042342714));
#76662=CARTESIAN_POINT('Ctrl Pts',(202.230098799678,9.77173314285901,30.2957341124075));
#76663=CARTESIAN_POINT('Ctrl Pts',(202.233170214418,9.74120431899568,30.248610906359));
#76664=CARTESIAN_POINT('Ctrl Pts',(202.236241629157,9.71333265900746,30.199638446855));
#76665=CARTESIAN_POINT('Ctrl Pts',(202.239313043896,9.68834143141664,30.1491410089201));
#76666=CARTESIAN_POINT('Ctrl Pts',(202.242377749617,9.6634047931973,30.0987538746264));
#76667=CARTESIAN_POINT('Ctrl Pts',(202.245442455338,9.64133630392324,30.0468488253206));
#76668=CARTESIAN_POINT('Ctrl Pts',(202.248507161059,9.62231482382211,29.993777080614));
#76669=CARTESIAN_POINT('Ctrl Pts',(202.251567901762,9.60331795310428,29.9407739984353));
#76670=CARTESIAN_POINT('Ctrl Pts',(202.254628642465,9.58736043913028,29.886607682295));
#76671=CARTESIAN_POINT('Ctrl Pts',(202.257689383168,9.57457370771792,29.8316506222985));
#76672=CARTESIAN_POINT('Ctrl Pts',(202.260747068025,9.5617997425851,29.7767484314603));
#76673=CARTESIAN_POINT('Ctrl Pts',(202.263804752883,9.5521903894846,29.7210575485588));
#76674=CARTESIAN_POINT('Ctrl Pts',(202.26686243774,9.5458271156249,29.6649650640232));
#76675=CARTESIAN_POINT('Ctrl Pts',(202.269856609879,9.53959601654511,29.6100377048558));
#76676=CARTESIAN_POINT('Ctrl Pts',(202.272850782018,9.53647746167809,29.5547257397934));
#76677=CARTESIAN_POINT('Ctrl Pts',(202.275844954157,9.53650012276609,29.4994005533173));
#76678=CARTESIAN_POINT('',(202.775844954126,9.53650011397254,29.4994224209001));
#76679=CARTESIAN_POINT('Ctrl Pts',(202.275844954211,9.53650012276649,29.4994005523254));
#76680=CARTESIAN_POINT('Ctrl Pts',(202.279119309422,9.53652490443265,29.4388982484398));
#76681=CARTESIAN_POINT('Ctrl Pts',(202.282393664633,9.540305713722,29.3785134960796));
#76682=CARTESIAN_POINT('Ctrl Pts',(202.285668019843,9.5477739722089,29.3186941418319));
#76683=CARTESIAN_POINT('Ctrl Pts',(202.288952785623,9.5552659754678,29.2586845963996));
#76684=CARTESIAN_POINT('Ctrl Pts',(202.292237551403,9.566468768621,29.1992443913266));
#76685=CARTESIAN_POINT('Ctrl Pts',(202.295522317182,9.58126302198713,29.1408097478788));
#76686=CARTESIAN_POINT('Ctrl Pts',(202.298821265787,9.59612115336547,29.0821227977566));
#76687=CARTESIAN_POINT('Ctrl Pts',(202.302120214392,9.61460166204428,29.0244504401604));
#76688=CARTESIAN_POINT('Ctrl Pts',(202.305419162996,9.63653552964663,28.9682134938869));
#76689=CARTESIAN_POINT('Ctrl Pts',(202.306561255221,9.64412900946451,28.9487443275598));
#76690=CARTESIAN_POINT('Ctrl Pts',(202.307703347446,9.65213597693153,28.9294469932177));
#76691=CARTESIAN_POINT('Ctrl Pts',(202.308845439671,9.66054814145892,28.9103382591258));
#76692=CARTESIAN_POINT('Ctrl Pts',(202.31185677749,9.6827283722935,28.8599545401987));
#76693=CARTESIAN_POINT('Ctrl Pts',(202.314868115309,9.70780147747075,28.8107192287392));
#76694=CARTESIAN_POINT('Ctrl Pts',(202.317879453128,9.73562610566513,28.762985139007));
#76695=CARTESIAN_POINT('Ctrl Pts',(202.3208854784,9.76340164615013,28.7153352608988));
#76696=CARTESIAN_POINT('Ctrl Pts',(202.323891503671,9.79391881258575,28.669181800712));
#76697=CARTESIAN_POINT('Ctrl Pts',(202.326897528942,9.82698913822091,28.6248555729776));
#76698=CARTESIAN_POINT('Ctrl Pts',(202.32990060453,9.86002701337135,28.5805728406595));
#76699=CARTESIAN_POINT('Ctrl Pts',(202.332903680118,9.89561277061498,28.5381142096381));
#76700=CARTESIAN_POINT('Ctrl Pts',(202.335906755706,9.9335141755226,28.4977823409115));
#76701=CARTESIAN_POINT('Ctrl Pts',(202.338908067777,9.97139332332479,28.4574741565486));
#76702=CARTESIAN_POINT('Ctrl Pts',(202.341909379848,10.0115850627582,28.4192906426313));
#76703=CARTESIAN_POINT('Ctrl Pts',(202.344910691919,10.0538178226943,28.3835003191451));
#76704=CARTESIAN_POINT('Ctrl Pts',(202.347911424012,10.0960424215021,28.3477169118402));
#76705=CARTESIAN_POINT('Ctrl Pts',(202.350912156104,10.1403068551407,28.3143261173153));
#76706=CARTESIAN_POINT('Ctrl Pts',(202.353912888197,10.1863054778245,28.2835570401447));
#76707=CARTESIAN_POINT('Ctrl Pts',(202.356916367904,10.2323462190534,28.2527597893313));
#76708=CARTESIAN_POINT('Ctrl Pts',(202.359919847611,10.2801238820762,28.2245893455089));
#76709=CARTESIAN_POINT('Ctrl Pts',(202.362923327317,10.3293039995066,28.1992313330488));
#76710=CARTESIAN_POINT('Ctrl Pts',(202.365928186678,10.3785067079196,28.1738616723362));
#76711=CARTESIAN_POINT('Ctrl Pts',(202.368933046039,10.4291126722085,28.1513072333536));
#76712=CARTESIAN_POINT('Ctrl Pts',(202.371937905401,10.4807659797898,28.1317060687643));
#76713=CARTESIAN_POINT('Ctrl Pts',(202.374948363449,10.5325155283909,28.1120683830662));
#76714=CARTESIAN_POINT('Ctrl Pts',(202.377958821498,10.5853158140669,28.0953951225459));
#76715=CARTESIAN_POINT('Ctrl Pts',(202.380969279546,10.638795392514,28.0817745307847));
#76716=CARTESIAN_POINT('Ctrl Pts',(202.383176879585,10.6780125207929,28.0717864099011));
#76717=CARTESIAN_POINT('Ctrl Pts',(202.385384479625,10.7175946189491,28.0634387857504));
#76718=CARTESIAN_POINT('Ctrl Pts',(202.387592079664,10.7573930510406,28.0567487681223));
#76719=CARTESIAN_POINT('Ctrl Pts',(202.390603417483,10.8116812017825,28.0476230647622));
#76720=CARTESIAN_POINT('Ctrl Pts',(202.393614755302,10.8665978878447,28.0415457224413));
#76721=CARTESIAN_POINT('Ctrl Pts',(202.396626093121,10.9217706225594,28.0385923174879));
#76722=CARTESIAN_POINT('Ctrl Pts',(202.399632118392,10.9768460225262,28.0356441228786));
#76723=CARTESIAN_POINT('Ctrl Pts',(202.402638143663,11.0321760520258,28.0358089562565));
#76724=CARTESIAN_POINT('Ctrl Pts',(202.405644168934,11.0873807423092,28.0391109364933));
#76725=CARTESIAN_POINT('Ctrl Pts',(202.408647244522,11.1425312626101,28.0424096766393));
#76726=CARTESIAN_POINT('Ctrl Pts',(202.41165032011,11.1975561632272,28.0488394339358));
#76727=CARTESIAN_POINT('Ctrl Pts',(202.414653395699,11.2520749746903,28.0583722889959));
#76728=CARTESIAN_POINT('Ctrl Pts',(202.41765470777,11.3065617706927,28.0678995460113));
#76729=CARTESIAN_POINT('Ctrl Pts',(202.420656019841,11.3605425479361,28.0805261980597));
#76730=CARTESIAN_POINT('Ctrl Pts',(202.423657331912,11.4136437733348,28.0961727033636));
#76731=CARTESIAN_POINT('Ctrl Pts',(202.426658064004,11.4667347373648,28.111816185111));
#76732=CARTESIAN_POINT('Ctrl Pts',(202.429658796097,11.5189459813392,28.130478211984));
#76733=CARTESIAN_POINT('Ctrl Pts',(202.43265952819,11.5699182059822,28.1520291217945));
#76734=CARTESIAN_POINT('Ctrl Pts',(202.435663007897,11.6209371032389,28.1735997646518));
#76735=CARTESIAN_POINT('Ctrl Pts',(202.438666487603,11.6707142277645,28.1980643689411));
#76736=CARTESIAN_POINT('Ctrl Pts',(202.44166996731,11.7189107956159,28.2252453106786));
#76737=CARTESIAN_POINT('Ctrl Pts',(202.444674826671,11.7671295026545,28.2524387380345));
#76738=CARTESIAN_POINT('Ctrl Pts',(202.447679686032,11.8137657609265,28.2823507047672));
#76739=CARTESIAN_POINT('Ctrl Pts',(202.450684545394,11.8585087715102,28.3147595437043));
#76740=CARTESIAN_POINT('Ctrl Pts',(202.453695003442,11.9033351477711,28.3472287671522));
#76741=CARTESIAN_POINT('Ctrl Pts',(202.456705461491,11.9462608200782,28.3822038217028));
#76742=CARTESIAN_POINT('Ctrl Pts',(202.459715919539,11.9870080913358,28.4194227109375));
#76743=CARTESIAN_POINT('Ctrl Pts',(202.461923519578,12.0168884869997,28.4467157075525));
#76744=CARTESIAN_POINT('Ctrl Pts',(202.464131119618,12.0455981711185,28.4752144682489));
#76745=CARTESIAN_POINT('Ctrl Pts',(202.466338719657,12.0730412338316,28.5048041597267));
#76746=CARTESIAN_POINT('Ctrl Pts',(202.469350057476,12.1104757016507,28.545166795814));
#76747=CARTESIAN_POINT('Ctrl Pts',(202.472361395295,12.1457074999546,28.5877284791222));
#76748=CARTESIAN_POINT('Ctrl Pts',(202.475372733114,12.1784689464185,28.6322193869835));
#76749=CARTESIAN_POINT('Ctrl Pts',(202.478378758385,12.2111725957268,28.676631804784));
#76750=CARTESIAN_POINT('Ctrl Pts',(202.481384783656,12.2414142319036,28.7229662711761));
#76751=CARTESIAN_POINT('Ctrl Pts',(202.484390808927,12.2689650718549,28.7709184569527));
#76752=CARTESIAN_POINT('Ctrl Pts',(202.487393884516,12.2964888773549,28.8188235893169));
#76753=CARTESIAN_POINT('Ctrl Pts',(202.490396960104,12.3213268557498,28.8683428410891));
#76754=CARTESIAN_POINT('Ctrl Pts',(202.493400035692,12.343293441774,28.9191428925398));
#76755=CARTESIAN_POINT('Ctrl Pts',(202.496401347763,12.3652471282072,28.9699131123232));
#76756=CARTESIAN_POINT('Ctrl Pts',(202.499402659834,12.3843325556044,29.0219621576059));
#76757=CARTESIAN_POINT('Ctrl Pts',(202.502403971905,12.4004111123555,29.0749341622865));
#76758=CARTESIAN_POINT('Ctrl Pts',(202.505404703998,12.4164865620598,29.1278959305692));
#76759=CARTESIAN_POINT('Ctrl Pts',(202.50840543609,12.4295561420746,29.1817797994226));
#76760=CARTESIAN_POINT('Ctrl Pts',(202.511406168183,12.439530945825,29.2362142801208));
#76761=CARTESIAN_POINT('Ctrl Pts',(202.51440964789,12.4495148829841,29.2906986036403));
#76762=CARTESIAN_POINT('Ctrl Pts',(202.517413127597,12.4563982875769,29.3457340261452));
#76763=CARTESIAN_POINT('Ctrl Pts',(202.520416607303,12.4601436028484,29.4009398714872));
#76764=CARTESIAN_POINT('Ctrl Pts',(202.523421466664,12.4638906385377,29.4561710757416));
#76765=CARTESIAN_POINT('Ctrl Pts',(202.526426326026,12.4644967056998,29.5115723304389));
#76766=CARTESIAN_POINT('Ctrl Pts',(202.529431185387,12.4619764235825,29.5667621665992));
#76767=CARTESIAN_POINT('Ctrl Pts',(202.532441643435,12.4594514456473,29.622054833079));
#76768=CARTESIAN_POINT('Ctrl Pts',(202.535452101484,12.4537885368043,29.6771347681487));
#76769=CARTESIAN_POINT('Ctrl Pts',(202.538462559532,12.4450541976733,29.7316260257114));
#76770=CARTESIAN_POINT('Ctrl Pts',(202.540670159572,12.4386492164061,29.7715850287537));
#76771=CARTESIAN_POINT('Ctrl Pts',(202.542877759611,12.4305936879302,29.8112276041533));
#76772=CARTESIAN_POINT('Ctrl Pts',(202.54508535965,12.4209309280141,29.8504105418118));
#76773=CARTESIAN_POINT('Ctrl Pts',(202.548096697469,12.4077501734128,29.9038591103702));
#76774=CARTESIAN_POINT('Ctrl Pts',(202.551108035288,12.3915220963785,29.956674127302));
#76775=CARTESIAN_POINT('Ctrl Pts',(202.554119373107,12.3723252372777,30.0084837196318));
#76776=CARTESIAN_POINT('Ctrl Pts',(202.557125398378,12.3531622449311,30.0602019104091));
#76777=CARTESIAN_POINT('Ctrl Pts',(202.560131423649,12.3310410465083,30.1109177059251));
#76778=CARTESIAN_POINT('Ctrl Pts',(202.56313744892,12.3060903803334,30.1602727984708));
#76779=CARTESIAN_POINT('Ctrl Pts',(202.566140524508,12.2811641971715,30.2095794609921));
#76780=CARTESIAN_POINT('Ctrl Pts',(202.569143600096,12.2534142833967,30.2575275970591));
#76781=CARTESIAN_POINT('Ctrl Pts',(202.572146675685,12.2230173362518,30.3037791022586));
#76782=CARTESIAN_POINT('Ctrl Pts',(202.575147987756,12.1926382393175,30.3500034468651));
#76783=CARTESIAN_POINT('Ctrl Pts',(202.578149299827,12.1596154793837,30.3945326954565));
#76784=CARTESIAN_POINT('Ctrl Pts',(202.581150611898,12.1241703778796,30.4370556074738));
#76785=CARTESIAN_POINT('Ctrl Pts',(202.584151343991,12.0887321258455,30.4795703022931));
#76786=CARTESIAN_POINT('Ctrl Pts',(202.587152076083,12.0508727996188,30.520079025576));
#76787=CARTESIAN_POINT('Ctrl Pts',(202.590152808176,12.0108540687231,30.5583035017167));
#76788=CARTESIAN_POINT('Ctrl Pts',(202.593156287883,11.9707986947581,30.5965629780211));
#76789=CARTESIAN_POINT('Ctrl Pts',(202.596159767589,11.9285803484357,30.6325336636257));
#76790=CARTESIAN_POINT('Ctrl Pts',(202.599163247296,11.884496572017,30.6659751558632));
#76791=CARTESIAN_POINT('Ctrl Pts',(202.602168106657,11.84039254563,30.6994320095151));
#76792=CARTESIAN_POINT('Ctrl Pts',(202.605172966018,11.7944218195366,30.7303570589392));
#76793=CARTESIAN_POINT('Ctrl Pts',(202.608177825379,11.7469112462918,30.7585530740349));
#76794=CARTESIAN_POINT('Ctrl Pts',(202.611188283428,11.699312150816,30.7868016242611));
#76795=CARTESIAN_POINT('Ctrl Pts',(202.614198741477,11.6501679464801,30.8123107395737));
#76796=CARTESIAN_POINT('Ctrl Pts',(202.617209199525,11.5998293557888,30.834929583886));
#76797=CARTESIAN_POINT('Ctrl Pts',(202.619416799564,11.5629155463338,30.8515162164787));
#76798=CARTESIAN_POINT('Ctrl Pts',(202.621624399604,11.5253599557688,30.8665496106646));
#76799=CARTESIAN_POINT('Ctrl Pts',(202.623831999643,11.4873060597025,30.8799873384119));
#76800=CARTESIAN_POINT('Ctrl Pts',(202.626843337462,11.4353975915199,30.8983174421681));
#76801=CARTESIAN_POINT('Ctrl Pts',(202.629854675281,11.3823454786743,30.9137527853886));
#76802=CARTESIAN_POINT('Ctrl Pts',(202.6328660131,11.3285036499403,30.9261548309969));
#76803=CARTESIAN_POINT('Ctrl Pts',(202.635872038371,11.2747568079937,30.9385349971391));
#76804=CARTESIAN_POINT('Ctrl Pts',(202.638878063642,11.220223525117,30.9478923681986));
#76805=CARTESIAN_POINT('Ctrl Pts',(202.641884088913,11.1652739540451,30.9541378098771));
#76806=CARTESIAN_POINT('Ctrl Pts',(202.644887164501,11.1103783026181,30.960377123173));
#76807=CARTESIAN_POINT('Ctrl Pts',(202.647890240089,11.0550676939211,30.9635104971319));
#76808=CARTESIAN_POINT('Ctrl Pts',(202.650893315678,10.9997217273275,30.9634999735444));
#76809=CARTESIAN_POINT('Ctrl Pts',(202.653894627749,10.9444082619306,30.9634894561367));
#76810=CARTESIAN_POINT('Ctrl Pts',(202.65689593982,10.889060006361,30.9603387008083));
#76811=CARTESIAN_POINT('Ctrl Pts',(202.659897251891,10.8340586088789,30.9540617953556));
#76812=CARTESIAN_POINT('Ctrl Pts',(202.662897983983,10.7790678399578,30.9477861028625));
#76813=CARTESIAN_POINT('Ctrl Pts',(202.665898716076,10.7244243198954,30.9383855199263));
#76814=CARTESIAN_POINT('Ctrl Pts',(202.668899448169,10.6705042988143,30.9259259563176));
#76815=CARTESIAN_POINT('Ctrl Pts',(202.671902927875,10.6165349059757,30.9134549841348));
#76816=CARTESIAN_POINT('Ctrl Pts',(202.674906407582,10.5632908506835,30.8979195547848));
#76817=CARTESIAN_POINT('Ctrl Pts',(202.677909887289,10.5111364256746,30.8794363543483));
#76818=CARTESIAN_POINT('Ctrl Pts',(202.68091474665,10.4589580434292,30.8609446636178));
#76819=CARTESIAN_POINT('Ctrl Pts',(202.683919606011,10.4078707764935,30.8395027071667));
#76820=CARTESIAN_POINT('Ctrl Pts',(202.686924465372,10.3582189277104,30.8152753724034));
#76821=CARTESIAN_POINT('Ctrl Pts',(202.689934923421,10.3084745670478,30.7910028969992));
#76822=CARTESIAN_POINT('Ctrl Pts',(202.692945381469,10.2601714281986,30.7639349351043));
#76823=CARTESIAN_POINT('Ctrl Pts',(202.695955839518,10.2136281446128,30.734281797263));
#76824=CARTESIAN_POINT('Ctrl Pts',(202.698163439557,10.1794974731306,30.7125368444342));
#76825=CARTESIAN_POINT('Ctrl Pts',(202.700371039596,10.1463125986136,30.6894026829662));
#76826=CARTESIAN_POINT('Ctrl Pts',(202.702578639635,10.1141877581856,30.6649759320483));
#76827=CARTESIAN_POINT('Ctrl Pts',(202.705631402739,10.0697641643131,30.631197583333));
#76828=CARTESIAN_POINT('Ctrl Pts',(202.708684165843,10.0271717147639,30.5947955506121));
#76829=CARTESIAN_POINT('Ctrl Pts',(202.711736928947,9.98673924406939,30.5559994746641));
#76830=CARTESIAN_POINT('Ctrl Pts',(202.714713719638,9.94731299372029,30.5181688950183));
#76831=CARTESIAN_POINT('Ctrl Pts',(202.717690510329,9.90994088495104,30.4780624372868));
#76832=CARTESIAN_POINT('Ctrl Pts',(202.72066730102,9.87489692336547,30.4359355303372));
#76833=CARTESIAN_POINT('Ctrl Pts',(202.723641242856,9.83988649963546,30.3938489397803));
#76834=CARTESIAN_POINT('Ctrl Pts',(202.726615184692,9.80720015500378,30.3497461406315));
#76835=CARTESIAN_POINT('Ctrl Pts',(202.729589126528,9.77707437246157,30.3039186274181));
#76836=CARTESIAN_POINT('Ctrl Pts',(202.732561452323,9.74696496027342,30.2581160168811));
#76837=CARTESIAN_POINT('Ctrl Pts',(202.735533778119,9.7194136488174,30.2105909989348));
#76838=CARTESIAN_POINT('Ctrl Pts',(202.738506103914,9.69461451188773,30.1616653061978));
#76839=CARTESIAN_POINT('Ctrl Pts',(202.741617674765,9.66865360554443,30.1104475831567));
#76840=CARTESIAN_POINT('Ctrl Pts',(202.744729245616,9.64570947287336,30.0576952307279));
#76841=CARTESIAN_POINT('Ctrl Pts',(202.747840816467,9.62595032668182,30.0038052652109));
#76842=CARTESIAN_POINT('Ctrl Pts',(202.75081544914,9.60706076746592,29.9522869614892));
#76843=CARTESIAN_POINT('Ctrl Pts',(202.753790081812,9.59108180910761,29.8997296520723));
#76844=CARTESIAN_POINT('Ctrl Pts',(202.756764714485,9.57810963351725,29.8464968047523));
#76845=CARTESIAN_POINT('Ctrl Pts',(202.759741049455,9.5651300343211,29.7932334937933));
#76846=CARTESIAN_POINT('Ctrl Pts',(202.762717384425,9.55516073709183,29.7392944060208));
#76847=CARTESIAN_POINT('Ctrl Pts',(202.765693719395,9.54824655854444,29.6850518717061));
#76848=CARTESIAN_POINT('Ctrl Pts',(202.768674770717,9.54132142366917,29.6307233837258));
#76849=CARTESIAN_POINT('Ctrl Pts',(202.77165582204,9.53746109245465,29.5760910270364));
#76850=CARTESIAN_POINT('Ctrl Pts',(202.774636873362,9.5366583622647,29.5215290796404));
#76851=CARTESIAN_POINT('Ctrl Pts',(202.77503956695,9.53654992592277,29.5141586106361));
#76852=CARTESIAN_POINT('Ctrl Pts',(202.775442260538,9.53649720654187,29.5067894195638));
#76853=CARTESIAN_POINT('Ctrl Pts',(202.775844954126,9.53650011397254,29.4994224209001));
#76854=CARTESIAN_POINT('',(203.275844954122,9.53650053107307,29.5012467760758));
#76855=CARTESIAN_POINT('Ctrl Pts',(202.775844954157,9.53650011397276,29.499422420335));
#76856=CARTESIAN_POINT('Ctrl Pts',(202.777671729314,9.53651330322503,29.4660028414331));
#76857=CARTESIAN_POINT('Ctrl Pts',(202.779498504471,9.537671130685,29.4326074630415));
#76858=CARTESIAN_POINT('Ctrl Pts',(202.781325279628,9.53996915343813,29.3992916235468));
#76859=CARTESIAN_POINT('Ctrl Pts',(202.784336617447,9.54375731685769,29.3443723046266));
#76860=CARTESIAN_POINT('Ctrl Pts',(202.787347955266,9.55065636465342,29.2895527858654));
#76861=CARTESIAN_POINT('Ctrl Pts',(202.790359293085,9.56065290987794,29.2352129078728));
#76862=CARTESIAN_POINT('Ctrl Pts',(202.793365318356,9.57063181937689,29.1809688953172));
#76863=CARTESIAN_POINT('Ctrl Pts',(202.796371343627,9.58369728681845,29.1272033590048));
#76864=CARTESIAN_POINT('Ctrl Pts',(202.799377368898,9.59978414191605,29.0742914133234));
#76865=CARTESIAN_POINT('Ctrl Pts',(202.802380444486,9.61585521167632,29.0214313878529));
#76866=CARTESIAN_POINT('Ctrl Pts',(202.805383520074,9.63494164303026,28.9694237960519));
#76867=CARTESIAN_POINT('Ctrl Pts',(202.808386595662,9.6569275459023,28.9186321018116));
#76868=CARTESIAN_POINT('Ctrl Pts',(202.811387907734,9.6789005378398,28.8678702343309));
#76869=CARTESIAN_POINT('Ctrl Pts',(202.814389219805,9.70376941710798,28.8183233323324));
#76870=CARTESIAN_POINT('Ctrl Pts',(202.817390531876,9.73136971287122,28.7703360742235));
#76871=CARTESIAN_POINT('Ctrl Pts',(202.820391263969,9.75896467510764,28.7223580892518));
#76872=CARTESIAN_POINT('Ctrl Pts',(202.823391996061,9.789289742555,28.675939606633));
#76873=CARTESIAN_POINT('Ctrl Pts',(202.826392728154,9.8221350262239,28.6313997734565));
#76874=CARTESIAN_POINT('Ctrl Pts',(202.829396207861,9.85501038460989,28.5868191574724));
#76875=CARTESIAN_POINT('Ctrl Pts',(202.832399687568,9.89041025543968,28.544121052898));
#76876=CARTESIAN_POINT('Ctrl Pts',(202.835403167275,9.92808289575131,28.5035934707063));
#76877=CARTESIAN_POINT('Ctrl Pts',(202.838408026636,9.96577284106353,28.463047272091));
#76878=CARTESIAN_POINT('Ctrl Pts',(202.841412885997,10.0057372557433,28.4246739493435));
#76879=CARTESIAN_POINT('Ctrl Pts',(202.844417745358,10.047688095616,28.3887240276292));
#76880=CARTESIAN_POINT('Ctrl Pts',(202.847428203407,10.0897170987624,28.3527071236191));
#76881=CARTESIAN_POINT('Ctrl Pts',(202.850438661455,10.1337394998062,28.3191229608318));
#76882=CARTESIAN_POINT('Ctrl Pts',(202.853449119504,10.1794357583125,28.2881804691854));
#76883=CARTESIAN_POINT('Ctrl Pts',(202.855656719543,10.2129452975408,28.2654900198677));
#76884=CARTESIAN_POINT('Ctrl Pts',(202.857864319583,10.2473542880417,28.2442192254203));
#76885=CARTESIAN_POINT('Ctrl Pts',(202.860071919622,10.2825286936883,28.2244345667041));
#76886=CARTESIAN_POINT('Ctrl Pts',(202.863083257441,10.3305093134119,28.1974467564263));
#76887=CARTESIAN_POINT('Ctrl Pts',(202.86609459526,10.380114578031,28.1731137701796));
#76888=CARTESIAN_POINT('Ctrl Pts',(202.869105933079,10.4310196725613,28.1516329739319));
#76889=CARTESIAN_POINT('Ctrl Pts',(202.87211195835,10.481834961238,28.1301900737191));
#76890=CARTESIAN_POINT('Ctrl Pts',(202.875117983621,10.5339450467044,28.1115895810636));
#76891=CARTESIAN_POINT('Ctrl Pts',(202.878124008892,10.5870006320155,28.0959829872668));
#76892=CARTESIAN_POINT('Ctrl Pts',(202.88112708448,10.6400041561682,28.0803917075476));
#76893=CARTESIAN_POINT('Ctrl Pts',(202.884130160068,10.6939508384774,28.0677886549604));
#76894=CARTESIAN_POINT('Ctrl Pts',(202.887133235656,10.7484732711875,28.05827653321));
#76895=CARTESIAN_POINT('Ctrl Pts',(202.890134547727,10.8029636863104,28.048769997329));
#76896=CARTESIAN_POINT('Ctrl Pts',(202.893135859798,10.8580286629236,28.0423508849124));
#76897=CARTESIAN_POINT('Ctrl Pts',(202.896137171869,10.9132898202213,28.039070982312));
#76898=CARTESIAN_POINT('Ctrl Pts',(202.899137903961,10.9685402987615,28.0357917135255));
#76899=CARTESIAN_POINT('Ctrl Pts',(202.902138636054,11.0239863563091,28.0356504808928));
#76900=CARTESIAN_POINT('Ctrl Pts',(202.905139368146,11.0792460135248,28.0386470928142));
#76901=CARTESIAN_POINT('Ctrl Pts',(202.908142847853,11.1345562691331,28.0416464485772));
#76902=CARTESIAN_POINT('Ctrl Pts',(202.91114632756,11.1896792555139,28.0477893600535));
#76903=CARTESIAN_POINT('Ctrl Pts',(202.914149807266,11.244236036138,28.0570235592181));
#76904=CARTESIAN_POINT('Ctrl Pts',(202.917154666627,11.2988178775253,28.0662620001301));
#76905=CARTESIAN_POINT('Ctrl Pts',(202.920159525988,11.3528324794864,28.0785944416681));
#76906=CARTESIAN_POINT('Ctrl Pts',(202.923164385349,11.4059123040621,28.0939176939414));
#76907=CARTESIAN_POINT('Ctrl Pts',(202.926174843398,11.45909102756,28.1092694966696));
#76908=CARTESIAN_POINT('Ctrl Pts',(202.929185301446,11.5113309957098,28.1276230661159));
#76909=CARTESIAN_POINT('Ctrl Pts',(202.932195759495,11.5622821419246,28.1488260501058));
#76910=CARTESIAN_POINT('Ctrl Pts',(202.934403359534,11.5996451446931,28.1643744176769));
#76911=CARTESIAN_POINT('Ctrl Pts',(202.936610959574,11.6363154733947,28.181454005409));
#76912=CARTESIAN_POINT('Ctrl Pts',(202.938818559613,11.6721639707555,28.1999892898833));
#76913=CARTESIAN_POINT('Ctrl Pts',(202.941829897433,11.721064103903,28.2252728567117));
#76914=CARTESIAN_POINT('Ctrl Pts',(202.944841235252,11.7686374015785,28.2533719287005));
#76915=CARTESIAN_POINT('Ctrl Pts',(202.947852573072,11.814540566128,28.2841233960094));
#76916=CARTESIAN_POINT('Ctrl Pts',(202.950858598343,11.860362749139,28.3148206121318));
#76917=CARTESIAN_POINT('Ctrl Pts',(202.953864623614,11.9045202115577,28.3481606458421));
#76918=CARTESIAN_POINT('Ctrl Pts',(202.956870648886,11.9466945550314,28.383934737807));
#76919=CARTESIAN_POINT('Ctrl Pts',(202.959873724474,11.9888275146402,28.4196737261979));
#76920=CARTESIAN_POINT('Ctrl Pts',(202.962876800063,12.0289808099204,28.4578417015899));
#76921=CARTESIAN_POINT('Ctrl Pts',(202.965879875651,12.0668668745335,28.4981879806954));
#76922=CARTESIAN_POINT('Ctrl Pts',(202.968881187722,12.1047306910494,28.5385105669749));
#76923=CARTESIAN_POINT('Ctrl Pts',(202.971882499794,12.1403295555235,28.5810085375439));
#76924=CARTESIAN_POINT('Ctrl Pts',(202.974883811865,12.1734124326928,28.6253940814275));
#76925=CARTESIAN_POINT('Ctrl Pts',(202.977884543958,12.2064889168721,28.6697710481751));
#76926=CARTESIAN_POINT('Ctrl Pts',(202.980885276051,12.2370500643195,28.7160344409564));
#76927=CARTESIAN_POINT('Ctrl Pts',(202.983886008144,12.2648863063175,28.7638649022832));
#76928=CARTESIAN_POINT('Ctrl Pts',(202.986889487851,12.2927480365137,28.8117391594744));
#76929=CARTESIAN_POINT('Ctrl Pts',(202.989892967559,12.3178796108901,28.8611828947601));
#76930=CARTESIAN_POINT('Ctrl Pts',(202.992896447266,12.3401166560611,28.9118507008015));
#76931=CARTESIAN_POINT('Ctrl Pts',(202.995901306627,12.3623639158619,28.962541781198));
#76932=CARTESIAN_POINT('Ctrl Pts',(202.998906165989,12.3817138114823,29.014457557986));
#76933=CARTESIAN_POINT('Ctrl Pts',(203.00191102535,12.3980507877041,29.0672341915076));
#76934=CARTESIAN_POINT('Ctrl Pts',(203.004921483399,12.4144182031624,29.1201091590424));
#76935=CARTESIAN_POINT('Ctrl Pts',(203.007931941448,12.4277613582521,29.1738476740637));
#76936=CARTESIAN_POINT('Ctrl Pts',(203.010942399497,12.4380153796125,29.2280735062598));
#76937=CARTESIAN_POINT('Ctrl Pts',(203.013149999534,12.4455347595751,29.2678378700871));
#76938=CARTESIAN_POINT('Ctrl Pts',(203.01535759957,12.4513940516442,29.3078640367316));
#76939=CARTESIAN_POINT('Ctrl Pts',(203.017565199607,12.4555854622499,29.3480025918423));
#76940=CARTESIAN_POINT('Ctrl Pts',(203.020576537426,12.4613028716816,29.4027546968372));
#76941=CARTESIAN_POINT('Ctrl Pts',(203.023587875244,12.4639386166715,29.4579437296724));
#76942=CARTESIAN_POINT('Ctrl Pts',(203.026599213063,12.4634405314833,29.5131932108198));
#76943=CARTESIAN_POINT('Ctrl Pts',(203.029605238334,12.4629433250081,29.5683452218249));
#76944=CARTESIAN_POINT('Ctrl Pts',(203.032611263604,12.4593232650675,29.6235569461207));
#76945=CARTESIAN_POINT('Ctrl Pts',(203.035617288875,12.4525800102121,29.6784476503969));
#76946=CARTESIAN_POINT('Ctrl Pts',(203.038620364463,12.4458433722219,29.7332844927918));
#76947=CARTESIAN_POINT('Ctrl Pts',(203.04162344005,12.4359896745757,29.7878004180681));
#76948=CARTESIAN_POINT('Ctrl Pts',(203.044626515638,12.4230705437693,29.841617443138));
#76949=CARTESIAN_POINT('Ctrl Pts',(203.047627827709,12.4101589995539,29.8954028648623));
#76950=CARTESIAN_POINT('Ctrl Pts',(203.050629139779,12.3941857132844,29.9484896878859));
#76951=CARTESIAN_POINT('Ctrl Pts',(203.05363045185,12.3752533998737,30.0005100759584));
#76952=CARTESIAN_POINT('Ctrl Pts',(203.056631183942,12.3563247449745,30.052520411525));
#76953=CARTESIAN_POINT('Ctrl Pts',(203.059631916034,12.3344383790158,30.1034642259552));
#76954=CARTESIAN_POINT('Ctrl Pts',(203.062632648126,12.3097461505299,30.1529910192124));
#76955=CARTESIAN_POINT('Ctrl Pts',(203.065636127833,12.2850313126553,30.2025631615771));
#76956=CARTESIAN_POINT('Ctrl Pts',(203.068639607539,12.2575057156321,30.2507152175747));
#76957=CARTESIAN_POINT('Ctrl Pts',(203.071643087246,12.2273677949094,30.2971201578302));
#76958=CARTESIAN_POINT('Ctrl Pts',(203.074647946606,12.1972160302742,30.3435464142852));
#76959=CARTESIAN_POINT('Ctrl Pts',(203.077652805967,12.164449862477,30.3882235290813));
#76960=CARTESIAN_POINT('Ctrl Pts',(203.080657665328,12.1293099364181,30.4308551538812));
#76961=CARTESIAN_POINT('Ctrl Pts',(203.083668123376,12.0941045372562,30.473566210401));
#76962=CARTESIAN_POINT('Ctrl Pts',(203.086678581424,12.0565169040922,30.5142237757011));
#76963=CARTESIAN_POINT('Ctrl Pts',(203.089689039472,12.0168258650238,30.5525670573501));
#76964=CARTESIAN_POINT('Ctrl Pts',(203.091896639515,11.9877200153056,30.5806845826045));
#76965=CARTESIAN_POINT('Ctrl Pts',(203.094104239557,11.957483870211,30.6075583776143));
#76966=CARTESIAN_POINT('Ctrl Pts',(203.0963118396,11.926238028769,30.6330998914757));
#76967=CARTESIAN_POINT('Ctrl Pts',(203.099323177418,11.8836162756414,30.6679404989954));
#76968=CARTESIAN_POINT('Ctrl Pts',(203.102334515237,11.8389373322898,30.7004453989026));
#76969=CARTESIAN_POINT('Ctrl Pts',(203.105345853056,11.7924872123271,30.7303642827626));
#76970=CARTESIAN_POINT('Ctrl Pts',(203.108351878327,11.7461190388321,30.7602303842649));
#76971=CARTESIAN_POINT('Ctrl Pts',(203.111357903598,11.6979863298982,30.7875192403134));
#76972=CARTESIAN_POINT('Ctrl Pts',(203.114363928868,11.6484071089273,30.8120215208191));
#76973=CARTESIAN_POINT('Ctrl Pts',(203.117367004456,11.5988765379085,30.8364997582933));
#76974=CARTESIAN_POINT('Ctrl Pts',(203.120370080044,11.547902737463,30.8581966044755));
#76975=CARTESIAN_POINT('Ctrl Pts',(203.123373155632,11.4958299658219,30.8769476732952));
#76976=CARTESIAN_POINT('Ctrl Pts',(203.126374467702,11.4437877732366,30.8956877307943));
#76977=CARTESIAN_POINT('Ctrl Pts',(203.129375779773,11.3906483840938,30.9114852614432));
#76978=CARTESIAN_POINT('Ctrl Pts',(203.132377091844,11.3367756265677,30.9242241492651));
#76979=CARTESIAN_POINT('Ctrl Pts',(203.135377823936,11.2829132795026,30.9369605754033));
#76980=CARTESIAN_POINT('Ctrl Pts',(203.138378556028,11.2283183586918,30.9466394113539));
#76981=CARTESIAN_POINT('Ctrl Pts',(203.141379288121,11.1733671801888,30.9531951248313));
#76982=CARTESIAN_POINT('Ctrl Pts',(203.144382767827,11.1183656857512,30.9597568410343));
#76983=CARTESIAN_POINT('Ctrl Pts',(203.147386247534,11.0630078069323,30.9631896592757));
#76984=CARTESIAN_POINT('Ctrl Pts',(203.15038972724,11.0076758223022,30.9634798706344));
#76985=CARTESIAN_POINT('Ctrl Pts',(203.153394586601,10.9523184208174,30.9637702153022));
#76986=CARTESIAN_POINT('Ctrl Pts',(203.156399445962,10.8969874650048,30.9609151027594));
#76987=CARTESIAN_POINT('Ctrl Pts',(203.159404305322,10.8420627661499,30.9549529477491));
#76988=CARTESIAN_POINT('Ctrl Pts',(203.162414763371,10.7870357309823,30.9489796839849));
#76989=CARTESIAN_POINT('Ctrl Pts',(203.165425221419,10.7324169863944,30.939887900727));
#76990=CARTESIAN_POINT('Ctrl Pts',(203.168435679467,10.6785775914021,30.9277674478889));
#76991=CARTESIAN_POINT('Ctrl Pts',(203.170643279509,10.6390966058739,30.9188793943889));
#76992=CARTESIAN_POINT('Ctrl Pts',(203.172850879551,10.6000345125662,30.9083637777217));
#76993=CARTESIAN_POINT('Ctrl Pts',(203.175058479593,10.561531536798,30.8962727730559));
#76994=CARTESIAN_POINT('Ctrl Pts',(203.178069817415,10.5090104890604,30.8797797041287));
#76995=CARTESIAN_POINT('Ctrl Pts',(203.181081155236,10.4573120718238,30.8602848289508));
#76996=CARTESIAN_POINT('Ctrl Pts',(203.184092493058,10.4068025270114,30.8378897593001));
#76997=CARTESIAN_POINT('Ctrl Pts',(203.187098518332,10.3563820902308,30.815534198629));
#76998=CARTESIAN_POINT('Ctrl Pts',(203.190104543606,10.3071468419408,30.7902888096372));
#76999=CARTESIAN_POINT('Ctrl Pts',(203.193110568879,10.2594463502455,30.7623044568706));
#77000=CARTESIAN_POINT('Ctrl Pts',(203.19611364447,10.2117926649861,30.7343475639427));
#77001=CARTESIAN_POINT('Ctrl Pts',(203.199116720061,10.1656712057506,30.7036572972487));
#77002=CARTESIAN_POINT('Ctrl Pts',(203.202119795651,10.1214083815894,30.6704311248675));
#77003=CARTESIAN_POINT('Ctrl Pts',(203.205121107725,10.077171550194,30.6372244641224));
#77004=CARTESIAN_POINT('Ctrl Pts',(203.208122419799,10.0347916115257,30.6014851656245));
#77005=CARTESIAN_POINT('Ctrl Pts',(203.211123731873,9.99456537628992,30.563453556788));
#77006=CARTESIAN_POINT('Ctrl Pts',(203.214124463968,9.95434691443848,30.5254292972425));
#77007=CARTESIAN_POINT('Ctrl Pts',(203.217125196063,9.91628171254241,30.4851139694643));
#77008=CARTESIAN_POINT('Ctrl Pts',(203.220125928158,9.88063116082989,30.4427861114245));
#77009=CARTESIAN_POINT('Ctrl Pts',(203.223129407868,9.84494796576275,30.4004194959683));
#77010=CARTESIAN_POINT('Ctrl Pts',(203.226132887577,9.81168417838141,30.3560370732873));
#77011=CARTESIAN_POINT('Ctrl Pts',(203.229136367287,9.78106114953375,30.3099508187687));
#77012=CARTESIAN_POINT('Ctrl Pts',(203.23214122665,9.75042405393841,30.2638433944396));
#77013=CARTESIAN_POINT('Ctrl Pts',(203.235146086014,9.72243040193221,30.2160310341985));
#77014=CARTESIAN_POINT('Ctrl Pts',(203.238150945377,9.69725662554668,30.1668522702353));
#77015=CARTESIAN_POINT('Ctrl Pts',(203.241161403428,9.6720359451002,30.1175818758506));
#77016=CARTESIAN_POINT('Ctrl Pts',(203.24417186148,9.64964584916801,30.0669404758587));
#77017=CARTESIAN_POINT('Ctrl Pts',(203.247182319531,9.63021497557521,30.0152875283389));
#77018=CARTESIAN_POINT('Ctrl Pts',(203.249389919549,9.61596611504658,29.9774098878104));
#77019=CARTESIAN_POINT('Ctrl Pts',(203.251597519567,9.60330754219997,29.9389887240316));
#77020=CARTESIAN_POINT('Ctrl Pts',(203.253805119585,9.5922726417023,29.9001698823002));
#77021=CARTESIAN_POINT('Ctrl Pts',(203.257521581763,9.57369554893588,29.8348189329119));
#77022=CARTESIAN_POINT('Ctrl Pts',(203.26123804394,9.5596592711323,29.7681244782473));
#77023=CARTESIAN_POINT('Ctrl Pts',(203.264954506117,9.55032021996541,29.7006509042065));
#77024=CARTESIAN_POINT('Ctrl Pts',(203.268584655452,9.54119806325685,29.6347443677619));
#77025=CARTESIAN_POINT('Ctrl Pts',(203.272214804787,9.53655747952402,29.5680944076123));
#77026=CARTESIAN_POINT('Ctrl Pts',(203.275844954122,9.53650053107307,29.5012467760758));
#77027=CARTESIAN_POINT('',(203.77584495419,9.53650027734347,29.4990990092893));
#77028=CARTESIAN_POINT('Ctrl Pts',(203.275844954157,9.53650053107252,29.501246775435));
#77029=CARTESIAN_POINT('Ctrl Pts',(203.278822538506,9.53645381984567,29.4464158461698));
#77030=CARTESIAN_POINT('Ctrl Pts',(203.281800122854,9.53949281226948,29.3915218506111));
#77031=CARTESIAN_POINT('Ctrl Pts',(203.284777707203,9.54561214053705,29.3369411019086));
#77032=CARTESIAN_POINT('Ctrl Pts',(203.287753798455,9.55172840029411,29.2823877224849));
#77033=CARTESIAN_POINT('Ctrl Pts',(203.290729889707,9.56092187543824,29.228147811872));
#77034=CARTESIAN_POINT('Ctrl Pts',(203.293705980959,9.57313526104874,29.1745936897699));
#77035=CARTESIAN_POINT('Ctrl Pts',(203.296681802693,9.58534754060459,29.121044417575));
#77036=CARTESIAN_POINT('Ctrl Pts',(203.299657624428,9.60057906605375,29.0681813337964));
#77037=CARTESIAN_POINT('Ctrl Pts',(203.302633446162,9.61872171788103,29.0163652645369));
#77038=CARTESIAN_POINT('Ctrl Pts',(203.305612215513,9.63688234040339,28.9644978703228));
#77039=CARTESIAN_POINT('Ctrl Pts',(203.308590984865,9.65795966395401,28.9136800675947));
#77040=CARTESIAN_POINT('Ctrl Pts',(203.311569754216,9.68179665286988,28.8642546220263));
#77041=CARTESIAN_POINT('Ctrl Pts',(203.314550255797,9.70564750359939,28.8148004343077));
#77042=CARTESIAN_POINT('Ctrl Pts',(203.317530757378,9.73226095077253,28.7667406839756));
#77043=CARTESIAN_POINT('Ctrl Pts',(203.32051125896,9.76143463323604,28.7203923536465));
#77044=CARTESIAN_POINT('Ctrl Pts',(203.323496997708,9.7906595780319,28.6739625826725));
#77045=CARTESIAN_POINT('Ctrl Pts',(203.326482736457,9.82245341829168,28.629250665693));
#77046=CARTESIAN_POINT('Ctrl Pts',(203.329468475206,9.85657221526708,28.5865422007007));
#77047=CARTESIAN_POINT('Ctrl Pts',(203.330496236663,9.86831670714956,28.5718409431863));
#77048=CARTESIAN_POINT('Ctrl Pts',(203.33152399812,9.88033635510133,28.5573767590068));
#77049=CARTESIAN_POINT('Ctrl Pts',(203.332551759578,9.89262022370826,28.5431602636491));
#77050=CARTESIAN_POINT('Ctrl Pts',(203.335563097396,9.92861191986607,28.5015059772253));
#77051=CARTESIAN_POINT('Ctrl Pts',(203.338574435214,9.96703199604216,28.4617986197016));
#77052=CARTESIAN_POINT('Ctrl Pts',(203.341585773032,10.0076417703286,28.4243339765506));
#77053=CARTESIAN_POINT('Ctrl Pts',(203.344591798303,10.0481799015793,28.3869354278513));
#77054=CARTESIAN_POINT('Ctrl Pts',(203.347597823573,10.0908996797894,28.3517720963619));
#77055=CARTESIAN_POINT('Ctrl Pts',(203.350603848843,10.1355238401233,28.3191049077056));
#77056=CARTESIAN_POINT('Ctrl Pts',(203.35360692443,10.1801042126919,28.2864697739538));
#77057=CARTESIAN_POINT('Ctrl Pts',(203.356610000017,10.2265848417551,28.25632624088));
#77058=CARTESIAN_POINT('Ctrl Pts',(203.359613075604,10.2746548860809,28.2288954741196));
#77059=CARTESIAN_POINT('Ctrl Pts',(203.362614387674,10.3226967018997,28.2014808157194));
#77060=CARTESIAN_POINT('Ctrl Pts',(203.365615699744,10.3723256255439,28.1767760269267));
#77061=CARTESIAN_POINT('Ctrl Pts',(203.368617011814,10.4232032326172,28.1549580901932));
#77062=CARTESIAN_POINT('Ctrl Pts',(203.371617743906,10.4740710080167,28.1331443695943));
#77063=CARTESIAN_POINT('Ctrl Pts',(203.374618475998,10.5261865029468,28.114216600833));
#77064=CARTESIAN_POINT('Ctrl Pts',(203.377619208089,10.5791902882369,28.0983040855857));
#77065=CARTESIAN_POINT('Ctrl Pts',(203.380622687795,10.632242606334,28.0823770000764));
#77066=CARTESIAN_POINT('Ctrl Pts',(203.383626167501,10.6861843332858,28.0694708356454));
#77067=CARTESIAN_POINT('Ctrl Pts',(203.386629647206,10.7406412499097,28.059664869292));
#77068=CARTESIAN_POINT('Ctrl Pts',(203.389634506566,10.7951231814234,28.049854398549));
#77069=CARTESIAN_POINT('Ctrl Pts',(203.392639365926,10.8501202497595,28.043147028591));
#77070=CARTESIAN_POINT('Ctrl Pts',(203.395644225286,10.9052516981477,28.0395702655396));
#77071=CARTESIAN_POINT('Ctrl Pts',(203.398654683333,10.9604858680659,28.0359868382233));
#77072=CARTESIAN_POINT('Ctrl Pts',(203.401665141381,11.0158543894073,28.0355456735817));
#77073=CARTESIAN_POINT('Ctrl Pts',(203.404675599428,11.0709762775324,28.0382221037286));
#77074=CARTESIAN_POINT('Ctrl Pts',(203.406883199476,11.1113977286625,28.0401847576591));
#77075=CARTESIAN_POINT('Ctrl Pts',(203.409090799523,11.1516865628465,28.043822775828));
#77076=CARTESIAN_POINT('Ctrl Pts',(203.411298399571,11.1916956689283,28.0491088874371));
#77077=CARTESIAN_POINT('Ctrl Pts',(203.414309737412,11.2462711955327,28.0563195540329));
#77078=CARTESIAN_POINT('Ctrl Pts',(203.417321075253,11.3005528314848,28.0666287993735));
#77079=CARTESIAN_POINT('Ctrl Pts',(203.420332413093,11.3541623137251,28.079999540304));
#77080=CARTESIAN_POINT('Ctrl Pts',(203.423338438386,11.4076772190814,28.0933466928139));
#77081=CARTESIAN_POINT('Ctrl Pts',(203.426344463679,11.4605218161861,28.1097444955115));
#77082=CARTESIAN_POINT('Ctrl Pts',(203.429350488972,11.5123257930212,28.1291044781585));
#77083=CARTESIAN_POINT('Ctrl Pts',(203.432353564582,11.5640789368482,28.1484454636895));
#77084=CARTESIAN_POINT('Ctrl Pts',(203.435356640191,11.6147929914568,28.1707426871275));
#77085=CARTESIAN_POINT('Ctrl Pts',(203.438359715801,11.6641124402058,28.1958577850695));
#77086=CARTESIAN_POINT('Ctrl Pts',(203.441361027894,11.713402926752,28.2209581344979));
#77087=CARTESIAN_POINT('Ctrl Pts',(203.444362339987,11.7612999615425,28.2488728394512));
#77088=CARTESIAN_POINT('Ctrl Pts',(203.44736365208,11.807469810782,28.2794162238192));
#77089=CARTESIAN_POINT('Ctrl Pts',(203.450364384194,11.8536307380826,28.3099537059326));
#77090=CARTESIAN_POINT('Ctrl Pts',(203.453365116308,11.8980647029871,28.3431185675757));
#77091=CARTESIAN_POINT('Ctrl Pts',(203.456365848423,11.9404662896964,28.378681397664));
#77092=CARTESIAN_POINT('Ctrl Pts',(203.459369328151,11.9829067013283,28.414276790782));
#77093=CARTESIAN_POINT('Ctrl Pts',(203.462372807879,12.0233106120234,28.4522741989873));
#77094=CARTESIAN_POINT('Ctrl Pts',(203.465376287608,12.0614062952404,28.4924043834831));
#77095=CARTESIAN_POINT('Ctrl Pts',(203.46838114699,12.099519477782,28.5325530018556));
#77096=CARTESIAN_POINT('Ctrl Pts',(203.471386006372,12.1353219777912,28.5748359461026));
#77097=CARTESIAN_POINT('Ctrl Pts',(203.474390865755,12.1685817484918,28.6189500881948));
#77098=CARTESIAN_POINT('Ctrl Pts',(203.477401323824,12.2019034891633,28.6631464242423));
#77099=CARTESIAN_POINT('Ctrl Pts',(203.480411781894,12.2326727431014,28.7091803339009));
#77100=CARTESIAN_POINT('Ctrl Pts',(203.483422239963,12.2607009446265,28.7567198521298));
#77101=CARTESIAN_POINT('Ctrl Pts',(203.48562983983,12.2812543130927,28.7915810698213));
#77102=CARTESIAN_POINT('Ctrl Pts',(203.487837439697,12.3003346244636,28.8272513205496));
#77103=CARTESIAN_POINT('Ctrl Pts',(203.490045039564,12.3178838986814,28.8635926779207));
#77104=CARTESIAN_POINT('Ctrl Pts',(203.493056377337,12.3418224724883,28.9131651135022));
#77105=CARTESIAN_POINT('Ctrl Pts',(203.49606771511,12.3630099402896,28.9641932196739));
#77106=CARTESIAN_POINT('Ctrl Pts',(203.499079052884,12.3812696071989,29.0163404893641));
#77107=CARTESIAN_POINT('Ctrl Pts',(203.502085078109,12.3994970607327,29.0683957617803));
#77108=CARTESIAN_POINT('Ctrl Pts',(203.505091103335,12.4148067910545,29.1215657853658));
#77109=CARTESIAN_POINT('Ctrl Pts',(203.50809712856,12.4270694173725,29.1754924839081));
#77110=CARTESIAN_POINT('Ctrl Pts',(203.511100204103,12.4393200109045,29.2293662665085));
#77111=CARTESIAN_POINT('Ctrl Pts',(203.514103279646,12.4485293073333,29.2839947411676));
#77112=CARTESIAN_POINT('Ctrl Pts',(203.517106355189,12.4546177493063,29.3390048031673));
#77113=CARTESIAN_POINT('Ctrl Pts',(203.520107667215,12.4607026159215,29.3939825612302));
#77114=CARTESIAN_POINT('Ctrl Pts',(203.523108979241,12.4636702028574,29.4493409390914));
#77115=CARTESIAN_POINT('Ctrl Pts',(203.526110291267,12.4634924560214,29.504699060365));
#77116=CARTESIAN_POINT('Ctrl Pts',(203.529111023315,12.4633147435335,29.5600464841496));
#77117=CARTESIAN_POINT('Ctrl Pts',(203.532111755363,12.4599929062211,29.6153931241434));
#77118=CARTESIAN_POINT('Ctrl Pts',(203.53511248741,12.4535509912168,29.6703577586512));
#77119=CARTESIAN_POINT('Ctrl Pts',(203.538115967073,12.4471031776842,29.7253727214313));
#77120=CARTESIAN_POINT('Ctrl Pts',(203.541119446736,12.4375296407133,29.7800044548445));
#77121=CARTESIAN_POINT('Ctrl Pts',(203.544122926399,12.4249062121686,29.8338780264157));
#77122=CARTESIAN_POINT('Ctrl Pts',(203.547127785717,12.4122769850257,29.8877763449247));
#77123=CARTESIAN_POINT('Ctrl Pts',(203.550132645035,12.3965952232226,29.9409153005076));
#77124=CARTESIAN_POINT('Ctrl Pts',(203.553137504352,12.3779868692051,29.992934517252));
#77125=CARTESIAN_POINT('Ctrl Pts',(203.556147962359,12.3593438438863,30.0450506568047));
#77126=CARTESIAN_POINT('Ctrl Pts',(203.559158420365,12.3377635401926,30.0960424030824));
#77127=CARTESIAN_POINT('Ctrl Pts',(203.562168878371,12.3134198757357,30.1455698877909));
#77128=CARTESIAN_POINT('Ctrl Pts',(203.564376478767,12.2955684115537,30.1818889112013));
#77129=CARTESIAN_POINT('Ctrl Pts',(203.566584079162,12.2762319757039,30.2174209825774));
#77130=CARTESIAN_POINT('Ctrl Pts',(203.568791679557,12.2554940105294,30.2520419134096));
#77131=CARTESIAN_POINT('Ctrl Pts',(203.571803017387,12.2272058206967,30.2992675430859));
#77132=CARTESIAN_POINT('Ctrl Pts',(203.574814355217,12.1961904872769,30.3449930895672));
#77133=CARTESIAN_POINT('Ctrl Pts',(203.577825693047,12.162632241804,30.3888861121189));
#77134=CARTESIAN_POINT('Ctrl Pts',(203.580831718329,12.1291331991939,30.432701699377));
#77135=CARTESIAN_POINT('Ctrl Pts',(203.58383774361,12.0931004655364,30.4746907628363));
#77136=CARTESIAN_POINT('Ctrl Pts',(203.586843768891,12.0547622776991,30.5145485634226));
#77137=CARTESIAN_POINT('Ctrl Pts',(203.589846844489,12.0164617094789,30.5543672532612));
#77138=CARTESIAN_POINT('Ctrl Pts',(203.592849920087,11.975860532681,30.5920584448174));
#77139=CARTESIAN_POINT('Ctrl Pts',(203.595852995684,11.9332269007235,30.6273507891362));
#77140=CARTESIAN_POINT('Ctrl Pts',(203.598854307765,11.8906183048172,30.6626224084804));
#77141=CARTESIAN_POINT('Ctrl Pts',(203.601855619845,11.8459800251689,30.6954976370934));
#77142=CARTESIAN_POINT('Ctrl Pts',(203.604856931925,11.7996149889168,30.7257439045329));
#77143=CARTESIAN_POINT('Ctrl Pts',(203.607857664027,11.753258912329,30.7559843271284));
#77144=CARTESIAN_POINT('Ctrl Pts',(203.610858396128,11.7051771835488,30.7835965095059));
#77145=CARTESIAN_POINT('Ctrl Pts',(203.613859128229,11.6557016249187,30.8083912370079));
#77146=CARTESIAN_POINT('Ctrl Pts',(203.616862607944,11.6061807641086,30.8332086677443));
#77147=CARTESIAN_POINT('Ctrl Pts',(203.619866087658,11.5552639965075,30.8552032530011));
#77148=CARTESIAN_POINT('Ctrl Pts',(203.622869567373,11.5033063208547,30.8742325121273));
#77149=CARTESIAN_POINT('Ctrl Pts',(203.625874426741,11.4513247783509,30.8932705123777));
#77150=CARTESIAN_POINT('Ctrl Pts',(203.62887928611,11.3983018804351,30.9093403179845));
#77151=CARTESIAN_POINT('Ctrl Pts',(203.631884145478,11.3446079733236,30.9223493223262));
#77152=CARTESIAN_POINT('Ctrl Pts',(203.634894603533,11.2908140231397,30.9353825651864));
#77153=CARTESIAN_POINT('Ctrl Pts',(203.637905061588,11.2363470865423,30.9453435199054));
#77154=CARTESIAN_POINT('Ctrl Pts',(203.640915519643,11.1815867109599,30.9521909366205));
#77155=CARTESIAN_POINT('Ctrl Pts',(203.643123119612,11.1414303622548,30.9572122179835));
#77156=CARTESIAN_POINT('Ctrl Pts',(203.645330719581,11.1011163999379,30.9605603017668));
#77157=CARTESIAN_POINT('Ctrl Pts',(203.64753831955,11.0607944334066,30.9622367410467));
#77158=CARTESIAN_POINT('Ctrl Pts',(203.65054965754,11.0057921361647,30.9645235345617));
#77159=CARTESIAN_POINT('Ctrl Pts',(203.653560995531,10.9505462244997,30.9637073914156));
#77160=CARTESIAN_POINT('Ctrl Pts',(203.656572333521,10.8954357009739,30.9597597601555));
#77161=CARTESIAN_POINT('Ctrl Pts',(203.659578358965,10.8404224024234,30.9558190932341));
#77162=CARTESIAN_POINT('Ctrl Pts',(203.662584384408,10.7855445400654,30.948757939387));
#77163=CARTESIAN_POINT('Ctrl Pts',(203.665590409851,10.7311821253338,30.9385997359446));
#77164=CARTESIAN_POINT('Ctrl Pts',(203.668593485612,10.6768730540861,30.9284515003075));
#77165=CARTESIAN_POINT('Ctrl Pts',(203.671596561373,10.6230789445967,30.91521233193));
#77166=CARTESIAN_POINT('Ctrl Pts',(203.674599637133,10.5701738178678,30.8989573628791));
#77167=CARTESIAN_POINT('Ctrl Pts',(203.677600949377,10.5172997589814,30.8827119393458));
#77168=CARTESIAN_POINT('Ctrl Pts',(203.680602261621,10.4653141514163,30.8634543802098));
#77169=CARTESIAN_POINT('Ctrl Pts',(203.683603573865,10.4145776984974,30.8413101725192));
#77170=CARTESIAN_POINT('Ctrl Pts',(203.68660430613,10.3638510499784,30.8191702440135));
#77171=CARTESIAN_POINT('Ctrl Pts',(203.689605038395,10.3143735599288,30.7941449858488));
#77172=CARTESIAN_POINT('Ctrl Pts',(203.69260577066,10.2664855607394,30.7664078400721));
#77173=CARTESIAN_POINT('Ctrl Pts',(203.695609250537,10.2185537130319,30.7386452968523));
#77174=CARTESIAN_POINT('Ctrl Pts',(203.698612730415,10.1722147212041,30.7081661703928));
#77175=CARTESIAN_POINT('Ctrl Pts',(203.701616210292,10.127782583291,30.675188932891));
#77176=CARTESIAN_POINT('Ctrl Pts',(203.704621069823,10.083330035401,30.64219654724));
#77177=CARTESIAN_POINT('Ctrl Pts',(203.707625929354,10.0407864932563,30.60670410167));
#77178=CARTESIAN_POINT('Ctrl Pts',(203.710630788885,10.0004326976241,30.5689702792973));
#77179=CARTESIAN_POINT('Ctrl Pts',(203.7136412471,9.96000371439727,30.5311661508903));
#77180=CARTESIAN_POINT('Ctrl Pts',(203.716651705316,9.92177299262161,30.491112686194));
#77181=CARTESIAN_POINT('Ctrl Pts',(203.719662163531,9.88598340189775,30.449104456397));
#77182=CARTESIAN_POINT('Ctrl Pts',(203.721869762201,9.85973854239347,30.4182994075896));
#77183=CARTESIAN_POINT('Ctrl Pts',(203.724077360872,9.83480557440133,30.3864439463869));
#77184=CARTESIAN_POINT('Ctrl Pts',(203.726284959543,9.81126534399656,30.3536639664507));
#77185=CARTESIAN_POINT('Ctrl Pts',(203.729317528431,9.77892822977764,30.3086342476645));
#77186=CARTESIAN_POINT('Ctrl Pts',(203.73235009732,9.74908658968655,30.2616718031847));
#77187=CARTESIAN_POINT('Ctrl Pts',(203.735382666209,9.72197530517356,30.2130814325263));
#77188=CARTESIAN_POINT('Ctrl Pts',(203.738410312439,9.69490802942409,30.1645699368519));
#77189=CARTESIAN_POINT('Ctrl Pts',(203.741437958668,9.67056257157521,30.1144362026879));
#77190=CARTESIAN_POINT('Ctrl Pts',(203.744465604898,9.64913114704461,30.0630147352557));
#77191=CARTESIAN_POINT('Ctrl Pts',(203.747489133158,9.62772887187511,30.0116632073143));
#77192=CARTESIAN_POINT('Ctrl Pts',(203.750512661419,9.6092329601498,29.9590278983659));
#77193=CARTESIAN_POINT('Ctrl Pts',(203.753536189679,9.59378911509744,29.9054666412685));
#77194=CARTESIAN_POINT('Ctrl Pts',(203.756557313621,9.57835755103658,29.851947976242));
#77195=CARTESIAN_POINT('Ctrl Pts',(203.759578437562,9.56597338189694,29.7975053197424));
#77196=CARTESIAN_POINT('Ctrl Pts',(203.762599561504,9.55673302857216,29.7425132969252));
#77197=CARTESIAN_POINT('Ctrl Pts',(203.765619853801,9.54749521889826,29.6875364121122));
#77198=CARTESIAN_POINT('Ctrl Pts',(203.768640146099,9.54139959904263,29.6320109701614));
#77199=CARTESIAN_POINT('Ctrl Pts',(203.771660438397,9.53849143670484,29.5763214872425));
#77200=CARTESIAN_POINT('Ctrl Pts',(203.773055276983,9.5371483822433,29.5506028375224));
#77201=CARTESIAN_POINT('Ctrl Pts',(203.77445011557,9.53648442441668,29.5248492967995));
#77202=CARTESIAN_POINT('Ctrl Pts',(203.775844954157,9.53650027734309,29.4990990099061));
#77203=CARTESIAN_POINT('',(204.275844954108,9.53650001147645,29.4998167199766));
#77204=CARTESIAN_POINT('Ctrl Pts',(203.77584495419,9.53650027734347,29.4990990092893));
#77205=CARTESIAN_POINT('Ctrl Pts',(203.779226360791,9.53653870847609,29.4366744456907));
#77206=CARTESIAN_POINT('Ctrl Pts',(203.782607767392,9.54057525081011,29.3743982782863));
#77207=CARTESIAN_POINT('Ctrl Pts',(203.785989173993,9.5485288292999,29.3127469876704));
#77208=CARTESIAN_POINT('Ctrl Pts',(203.789397074907,9.55654472641247,29.2506126410907));
#77209=CARTESIAN_POINT('Ctrl Pts',(203.792804975822,9.56853915786416,29.189113258323));
#77210=CARTESIAN_POINT('Ctrl Pts',(203.796212876736,9.58437923470691,29.128718302537));
#77211=CARTESIAN_POINT('Ctrl Pts',(203.799152451003,9.59804250821099,29.0766230502625));
#77212=CARTESIAN_POINT('Ctrl Pts',(203.802092025269,9.61456622497412,29.0253493198056));
#77213=CARTESIAN_POINT('Ctrl Pts',(203.805031599536,9.63383676531657,28.9751854935319));
#77214=CARTESIAN_POINT('Ctrl Pts',(203.808042937614,9.65357775726336,28.9237970180201));
#77215=CARTESIAN_POINT('Ctrl Pts',(203.811054275693,9.67626331988589,28.8734170402998));
#77216=CARTESIAN_POINT('Ctrl Pts',(203.814065613771,9.70176916669647,28.8244047413873));
#77217=CARTESIAN_POINT('Ctrl Pts',(203.817071639294,9.72723001649326,28.7754789092016));
#77218=CARTESIAN_POINT('Ctrl Pts',(203.820077664817,9.75550103462224,28.7279164316734));
#77219=CARTESIAN_POINT('Ctrl Pts',(203.82308369034,9.78640981931206,28.682056772546));
#77220=CARTESIAN_POINT('Ctrl Pts',(203.826086766176,9.81728827449957,28.636242113591));
#77221=CARTESIAN_POINT('Ctrl Pts',(203.829089842011,9.85079907518602,28.5921273982855));
#77222=CARTESIAN_POINT('Ctrl Pts',(203.832092917846,9.88672475340363,28.5500260659809));
#77223=CARTESIAN_POINT('Ctrl Pts',(203.83509423016,9.92262933467787,28.5079494572018));
#77224=CARTESIAN_POINT('Ctrl Pts',(203.838095542473,9.96094564073565,28.4678842883773));
#77225=CARTESIAN_POINT('Ctrl Pts',(203.841096854787,10.001415276456,28.4301117815844));
#77226=CARTESIAN_POINT('Ctrl Pts',(203.844097587117,10.0418770916852,28.3923465740802));
#77227=CARTESIAN_POINT('Ctrl Pts',(203.847098319446,10.084491024585,28.3568735084142));
#77228=CARTESIAN_POINT('Ctrl Pts',(203.850099051776,10.1289627561949,28.3239360689552));
#77229=CARTESIAN_POINT('Ctrl Pts',(203.85310253171,10.1734752081031,28.2909684705096));
#77230=CARTESIAN_POINT('Ctrl Pts',(203.856106011644,10.2198484321534,28.2605414511267));
#77231=CARTESIAN_POINT('Ctrl Pts',(203.859109491577,10.267757237836,28.2328564456785));
#77232=CARTESIAN_POINT('Ctrl Pts',(203.86211435116,10.3156880504362,28.2051587231187));
#77233=CARTESIAN_POINT('Ctrl Pts',(203.865119210743,10.3651553788918,28.1802057632513));
#77234=CARTESIAN_POINT('Ctrl Pts',(203.868124070326,10.415810333059,28.1581525112594));
#77235=CARTESIAN_POINT('Ctrl Pts',(203.871134528585,10.4665596679073,28.1360581694872));
#77236=CARTESIAN_POINT('Ctrl Pts',(203.874144986844,10.5185005525536,28.1168745109617));
#77237=CARTESIAN_POINT('Ctrl Pts',(203.877155445103,10.5712661967198,28.100707473069));
#77238=CARTESIAN_POINT('Ctrl Pts',(203.879363043245,10.6099597536398,28.0888520279055));
#77239=CARTESIAN_POINT('Ctrl Pts',(203.881570641387,10.6490964531806,28.078617708136));
#77240=CARTESIAN_POINT('Ctrl Pts',(203.883778239528,10.6885286501563,28.0700287246848));
#77241=CARTESIAN_POINT('Ctrl Pts',(203.886789578636,10.7423172970144,28.0583126694518));
#77242=CARTESIAN_POINT('Ctrl Pts',(203.889800917743,10.7968797976543,28.049611366135));
#77243=CARTESIAN_POINT('Ctrl Pts',(203.892812256851,10.8518477134735,28.0440181491526));
#77244=CARTESIAN_POINT('Ctrl Pts',(203.89581828342,10.9067186560981,28.0384347996013));
#77245=CARTESIAN_POINT('Ctrl Pts',(203.898824309989,10.9619930737726,28.0359487075318));
#77246=CARTESIAN_POINT('Ctrl Pts',(203.901830336558,11.017292589224,28.0366021674343));
#77247=CARTESIAN_POINT('Ctrl Pts',(203.904833413448,11.0725378417567,28.0372549861261));
#77248=CARTESIAN_POINT('Ctrl Pts',(203.907836490339,11.1278076182619,28.0410412475636));
#77249=CARTESIAN_POINT('Ctrl Pts',(203.91083956723,11.1827205483093,28.0479512917173));
#77250=CARTESIAN_POINT('Ctrl Pts',(203.913840880606,11.2376012315127,28.0548572780449));
#77251=CARTESIAN_POINT('Ctrl Pts',(203.916842193982,11.2921249611837,28.0648833452408));
#77252=CARTESIAN_POINT('Ctrl Pts',(203.919843507358,11.345914822217,28.0779679378542));
#77253=CARTESIAN_POINT('Ctrl Pts',(203.922844240756,11.3996942888129,28.0910500019804));
#77254=CARTESIAN_POINT('Ctrl Pts',(203.925844974153,11.4527396560845,28.1071892929545));
#77255=CARTESIAN_POINT('Ctrl Pts',(203.928845707551,11.5046858252472,28.126273510558));
#77256=CARTESIAN_POINT('Ctrl Pts',(203.931849188552,11.5566795586116,28.1453752025123));
#77257=CARTESIAN_POINT('Ctrl Pts',(203.934852669554,11.6075715869345,28.1674270256495));
#77258=CARTESIAN_POINT('Ctrl Pts',(203.937856150555,11.6570150054717,28.192267790186));
#77259=CARTESIAN_POINT('Ctrl Pts',(203.940861011207,11.7064811358652,28.2171199653387));
#77260=CARTESIAN_POINT('Ctrl Pts',(203.943865871859,11.7544968720457,28.2447633719305));
#77261=CARTESIAN_POINT('Ctrl Pts',(203.94687073251,11.8007411521433,28.2749914868605));
#77262=CARTESIAN_POINT('Ctrl Pts',(203.949881191827,11.8470715947194,28.305275922903));
#77263=CARTESIAN_POINT('Ctrl Pts',(203.952891651144,11.8916235627321,28.3381543730727));
#77264=CARTESIAN_POINT('Ctrl Pts',(203.955902110461,11.934107126041,28.3733784454931));
#77265=CARTESIAN_POINT('Ctrl Pts',(203.958109700148,11.965260603412,28.3992084902822));
#77266=CARTESIAN_POINT('Ctrl Pts',(203.960317289834,11.9953024892084,28.4262989888429));
#77267=CARTESIAN_POINT('Ctrl Pts',(203.962524879521,12.0241314837119,28.4545398362108));
#77268=CARTESIAN_POINT('Ctrl Pts',(203.965536213295,12.0634566016757,28.4930626731418));
#77269=CARTESIAN_POINT('Ctrl Pts',(203.96854754707,12.1006869375865,28.5338875525938));
#77270=CARTESIAN_POINT('Ctrl Pts',(203.971558880845,12.1355421901611,28.5767577867297));
#77271=CARTESIAN_POINT('Ctrl Pts',(203.97456490208,12.170335951748,28.6195523899968));
#77272=CARTESIAN_POINT('Ctrl Pts',(203.977570923316,12.202762615318,28.6643847807526));
#77273=CARTESIAN_POINT('Ctrl Pts',(203.980576944552,12.2325790809666,28.7109619406116));
#77274=CARTESIAN_POINT('Ctrl Pts',(203.983580016113,12.2623662890507,28.757493396386));
#77275=CARTESIAN_POINT('Ctrl Pts',(203.986583087674,12.2895480901372,28.8057657873714));
#77276=CARTESIAN_POINT('Ctrl Pts',(203.989586159236,12.3139231636225,28.8554550674342));
#77277=CARTESIAN_POINT('Ctrl Pts',(203.992587467296,12.3382839232737,28.9051151683395));
#77278=CARTESIAN_POINT('Ctrl Pts',(203.995588775357,12.359840990447,28.9561900363124));
#77279=CARTESIAN_POINT('Ctrl Pts',(203.998590083417,12.3784388641185,29.0083308552618));
#77280=CARTESIAN_POINT('Ctrl Pts',(204.001590811522,12.3970331440441,29.0604615988198));
#77281=CARTESIAN_POINT('Ctrl Pts',(204.004591539627,12.4126691890835,29.1136573875744));
#77282=CARTESIAN_POINT('Ctrl Pts',(204.007592267732,12.4252403977259,29.1675514194794));
#77283=CARTESIAN_POINT('Ctrl Pts',(204.010595743518,12.4378231174659,29.2214948006141));
#77284=CARTESIAN_POINT('Ctrl Pts',(204.013599219304,12.447335274324,29.2761371872828));
#77285=CARTESIAN_POINT('Ctrl Pts',(204.01660269509,12.4537211174992,29.3311001405069));
#77286=CARTESIAN_POINT('Ctrl Pts',(204.019607550562,12.4601098940947,29.3860883416793));
#77287=CARTESIAN_POINT('Ctrl Pts',(204.022612406034,12.4633694632053,29.4413968753827));
#77288=CARTESIAN_POINT('Ctrl Pts',(204.025617261506,12.4634961521434,29.4966440111136));
#77289=CARTESIAN_POINT('Ctrl Pts',(204.028627715764,12.4636230771343,29.5519940858772));
#77290=CARTESIAN_POINT('Ctrl Pts',(204.031638170022,12.4606054905345,29.6072820061521));
#77291=CARTESIAN_POINT('Ctrl Pts',(204.034648624281,12.4544918060457,29.662129072488));
#77292=CARTESIAN_POINT('Ctrl Pts',(204.036856256025,12.4500085079138,29.7023496220594));
#77293=CARTESIAN_POINT('Ctrl Pts',(204.039063887769,12.4438613506776,29.7423331751537));
#77294=CARTESIAN_POINT('Ctrl Pts',(204.041271519514,12.436086741375,29.7819346045576));
#77295=CARTESIAN_POINT('Ctrl Pts',(204.044282861004,12.4254817101582,29.8359533183871));
#77296=CARTESIAN_POINT('Ctrl Pts',(204.047294202494,12.4118024972489,29.8894851965204));
#77297=CARTESIAN_POINT('Ctrl Pts',(204.050305543985,12.3951097375372,29.942155029632));
#77298=CARTESIAN_POINT('Ctrl Pts',(204.053311572865,12.3784464271983,29.9947319426047));
#77299=CARTESIAN_POINT('Ctrl Pts',(204.056317601746,12.3587802791638,30.0464493297879));
#77300=CARTESIAN_POINT('Ctrl Pts',(204.059323630626,12.3362227185147,30.096943126709));
#77301=CARTESIAN_POINT('Ctrl Pts',(204.062326709783,12.3136872929046,30.1473873756238));
#77302=CARTESIAN_POINT('Ctrl Pts',(204.06532978894,12.2882662895848,30.1966099334772));
#77303=CARTESIAN_POINT('Ctrl Pts',(204.068332868098,12.260120005378,30.2442646182952));
#77304=CARTESIAN_POINT('Ctrl Pts',(204.071334183691,12.2319902501247,30.2918913178182));
#77305=CARTESIAN_POINT('Ctrl Pts',(204.074335499285,12.2011386541017,30.3379515159806));
#77306=CARTESIAN_POINT('Ctrl Pts',(204.077336814879,12.1677713740695,30.3821237259613));
#77307=CARTESIAN_POINT('Ctrl Pts',(204.080337550442,12.1344105425606,30.42628739927));
#77308=CARTESIAN_POINT('Ctrl Pts',(204.083338286004,12.0985353105404,30.4685633883658));
#77309=CARTESIAN_POINT('Ctrl Pts',(204.086339021567,12.0603937158286,30.5086612005184));
#77310=CARTESIAN_POINT('Ctrl Pts',(204.089342504637,12.0222171982498,30.5487957266724));
#77311=CARTESIAN_POINT('Ctrl Pts',(204.092345987706,11.9817705368738,30.586747708615));
#77312=CARTESIAN_POINT('Ctrl Pts',(204.095349470776,11.9393394154937,30.6222627644629));
#77313=CARTESIAN_POINT('Ctrl Pts',(204.098354333445,11.896888804092,30.6577941335541));
#77314=CARTESIAN_POINT('Ctrl Pts',(204.101359196114,11.8524523395228,30.6908860295983));
#77315=CARTESIAN_POINT('Ctrl Pts',(204.104364058783,11.806347050573,30.7213257894732));
#77316=CARTESIAN_POINT('Ctrl Pts',(204.10737452001,11.7601558598094,30.7518222636783));
#77317=CARTESIAN_POINT('Ctrl Pts',(204.110384981238,11.7122900908655,30.7796564653641));
#77318=CARTESIAN_POINT('Ctrl Pts',(204.113395442465,11.6630928377565,30.8046609285619));
#77319=CARTESIAN_POINT('Ctrl Pts',(204.115603014812,11.6270164735986,30.8229967108036));
#77320=CARTESIAN_POINT('Ctrl Pts',(204.117810587159,11.5902246710188,30.839811822276));
#77321=CARTESIAN_POINT('Ctrl Pts',(204.120018159507,11.5528587026747,30.8550570116703));
#77322=CARTESIAN_POINT('Ctrl Pts',(204.12302950634,11.5018878293625,30.8758529565279));
#77323=CARTESIAN_POINT('Ctrl Pts',(204.126040853173,11.4496359401254,30.8938122338179));
#77324=CARTESIAN_POINT('Ctrl Pts',(204.129052200006,11.3964499229062,30.9087795102952));
#77325=CARTESIAN_POINT('Ctrl Pts',(204.132058234392,11.3433577334367,30.9237203823538));
#77326=CARTESIAN_POINT('Ctrl Pts',(204.135064268778,11.2893351902625,30.9356795870154));
#77327=CARTESIAN_POINT('Ctrl Pts',(204.138070303164,11.2347477532021,30.9445503599275));
#77328=CARTESIAN_POINT('Ctrl Pts',(204.141073387922,11.1802138792876,30.9534124285198));
#77329=CARTESIAN_POINT('Ctrl Pts',(204.144076472679,11.1251167278233,30.9591919846774));
#77330=CARTESIAN_POINT('Ctrl Pts',(204.147079557437,11.0698336459468,30.9618329288581));
#77331=CARTESIAN_POINT('Ctrl Pts',(204.150080878715,11.0145830275516,30.9644723222164));
#77332=CARTESIAN_POINT('Ctrl Pts',(204.153082199993,10.9591472211274,30.9639767317573));
#77333=CARTESIAN_POINT('Ctrl Pts',(204.156083521271,10.9039081135936,30.960341946041));
#77334=CARTESIAN_POINT('Ctrl Pts',(204.159084262591,10.8486796801503,30.95670786269));
#77335=CARTESIAN_POINT('Ctrl Pts',(204.162085003911,10.7936483962654,30.9499358235573));
#77336=CARTESIAN_POINT('Ctrl Pts',(204.16508574523,10.7391932394833,30.9400736382799));
#77337=CARTESIAN_POINT('Ctrl Pts',(204.168089234121,10.6846882218852,30.9302024228825));
#77338=CARTESIAN_POINT('Ctrl Pts',(204.171092723012,10.6307609054681,30.9172355031283));
#77339=CARTESIAN_POINT('Ctrl Pts',(204.174096211903,10.5777807566252,30.9012719794972));
#77340=CARTESIAN_POINT('Ctrl Pts',(204.177101080438,10.5247762715057,30.8853011230681));
#77341=CARTESIAN_POINT('Ctrl Pts',(204.180105948972,10.4727203177654,30.8663310998614));
#77342=CARTESIAN_POINT('Ctrl Pts',(204.183110817507,10.4219647040667,30.8445101140026));
#77343=CARTESIAN_POINT('Ctrl Pts',(204.186121284598,10.3711145244418,30.8226484721141));
#77344=CARTESIAN_POINT('Ctrl Pts',(204.18913175169,10.3215699975059,30.797925493185));
#77345=CARTESIAN_POINT('Ctrl Pts',(204.192142218781,10.2736594681296,30.7705359820809));
#77346=CARTESIAN_POINT('Ctrl Pts',(204.194349745687,10.2385274505778,30.750451695863));
#77347=CARTESIAN_POINT('Ctrl Pts',(204.196557272593,10.2042735336006,30.7289345812719));
#77348=CARTESIAN_POINT('Ctrl Pts',(204.1987647995,10.1710164400011,30.7060756639828));
#77349=CARTESIAN_POINT('Ctrl Pts',(204.201765499031,10.1258099490225,30.675003452723));
#77350=CARTESIAN_POINT('Ctrl Pts',(204.204766198562,10.0822554830452,30.6413190711555));
#77351=CARTESIAN_POINT('Ctrl Pts',(204.207766898093,10.0406720412411,30.6052249171746));
#77352=CARTESIAN_POINT('Ctrl Pts',(204.210762304788,9.99916194711496,30.5691944284956));
#77353=CARTESIAN_POINT('Ctrl Pts',(204.213757711483,9.95961637746621,30.5307629467643));
#77354=CARTESIAN_POINT('Ctrl Pts',(204.216753118178,9.92232407296167,30.4901751593946));
#77355=CARTESIAN_POINT('Ctrl Pts',(204.219745603105,9.88506814397559,30.4496269620107));
#77356=CARTESIAN_POINT('Ctrl Pts',(204.222738088032,9.85006148522582,30.406927014425));
#77357=CARTESIAN_POINT('Ctrl Pts',(204.225730572958,9.81755709691058,30.3623578323025));
#77358=CARTESIAN_POINT('Ctrl Pts',(204.228721341017,9.785071357228,30.317814220706));
#77359=CARTESIAN_POINT('Ctrl Pts',(204.231712109076,9.75508535565408,30.2714039288233));
#77360=CARTESIAN_POINT('Ctrl Pts',(204.234702877134,9.72781124896586,30.2234417956838));
#77361=CARTESIAN_POINT('Ctrl Pts',(204.237693130609,9.70054183498594,30.1754879147779));
#77362=CARTESIAN_POINT('Ctrl Pts',(204.240683384084,9.67598365154099,30.1259831852319));
#77363=CARTESIAN_POINT('Ctrl Pts',(204.24367363756,9.65430377762247,30.0752685695211));
#77364=CARTESIAN_POINT('Ctrl Pts',(204.246666640412,9.63260397022328,30.0245073244426));
#77365=CARTESIAN_POINT('Ctrl Pts',(204.249659643265,9.61378796625327,29.9725344618907));
#77366=CARTESIAN_POINT('Ctrl Pts',(204.252652646118,9.59797472410803,29.9197110622322));
#77367=CARTESIAN_POINT('Ctrl Pts',(204.255647123817,9.58215368975522,29.8668616330667));
#77368=CARTESIAN_POINT('Ctrl Pts',(204.258641601516,9.56933848774583,29.8131613499567));
#77369=CARTESIAN_POINT('Ctrl Pts',(204.261636079215,9.55959732571954,29.758983369979));
#77370=CARTESIAN_POINT('Ctrl Pts',(204.264635948165,9.54983862572631,29.704707848084));
#77371=CARTESIAN_POINT('Ctrl Pts',(204.267635817115,9.54316507874804,29.6499534407802));
#77372=CARTESIAN_POINT('Ctrl Pts',(204.270635686065,9.53959305818328,29.5950989710434));
#77373=CARTESIAN_POINT('Ctrl Pts',(204.272372108746,9.53752545535506,29.5633474022292));
#77374=CARTESIAN_POINT('Ctrl Pts',(204.274108531427,9.53649603584491,29.5315623331089));
#77375=CARTESIAN_POINT('Ctrl Pts',(204.275844954108,9.53650001147645,29.4998167199766));
#77376=CARTESIAN_POINT('',(204.775844954127,9.53650044545502,29.5011418610453));
#77377=CARTESIAN_POINT('Ctrl Pts',(204.275844954157,9.53650001147656,29.4998167190727));
#77378=CARTESIAN_POINT('Ctrl Pts',(204.276400449269,9.53650128331826,29.4896610506928));
#77379=CARTESIAN_POINT('Ctrl Pts',(204.276955944381,9.53660826359327,29.4795061482609));
#77380=CARTESIAN_POINT('Ctrl Pts',(204.277511439493,9.53682091319707,29.4693534676914));
#77381=CARTESIAN_POINT('Ctrl Pts',(204.280522821154,9.53797370302999,29.4143150066341));
#77382=CARTESIAN_POINT('Ctrl Pts',(204.283534202815,9.54223866752445,29.3592272091366));
#77383=CARTESIAN_POINT('Ctrl Pts',(204.286545584476,9.54962062900635,29.3044701296577));
#77384=CARTESIAN_POINT('Ctrl Pts',(204.289551653075,9.55698956629596,29.2498096595603));
#77385=CARTESIAN_POINT('Ctrl Pts',(204.292557721675,9.56746451667963,29.1954792681896));
#77386=CARTESIAN_POINT('Ctrl Pts',(204.295563790275,9.58099835221424,29.1418567694605));
#77387=CARTESIAN_POINT('Ctrl Pts',(204.298566908844,9.594518906207,29.0882868936155));
#77388=CARTESIAN_POINT('Ctrl Pts',(204.301570027414,9.61109227001882,29.0354240432555));
#77389=CARTESIAN_POINT('Ctrl Pts',(204.304573145983,9.63062009606983,28.9836368247907));
#77390=CARTESIAN_POINT('Ctrl Pts',(204.307574500615,9.65013645208959,28.9318800245104));
#77391=CARTESIAN_POINT('Ctrl Pts',(204.310575855247,9.67260364477141,28.8811980964853));
#77392=CARTESIAN_POINT('Ctrl Pts',(204.313577209879,9.6978739016151,28.831943210569));
#77393=CARTESIAN_POINT('Ctrl Pts',(204.316577984038,9.72313927110199,28.7826978507213));
#77394=CARTESIAN_POINT('Ctrl Pts',(204.319578758197,9.75120638727083,28.7348794539368));
#77395=CARTESIAN_POINT('Ctrl Pts',(204.322579532357,9.78188088839983,28.6888168641087));
#77396=CARTESIAN_POINT('Ctrl Pts',(204.325583053042,9.81258346505192,28.6427121144652));
#77397=CARTESIAN_POINT('Ctrl Pts',(204.328586573727,9.84589790113683,28.5983668222543));
#77398=CARTESIAN_POINT('Ctrl Pts',(204.331590094412,9.88158653725754,28.5560807363146));
#77399=CARTESIAN_POINT('Ctrl Pts',(204.334594994206,9.91729156032239,28.513775234118));
#77400=CARTESIAN_POINT('Ctrl Pts',(204.337599894,9.95537259328542,28.473531206814));
#77401=CARTESIAN_POINT('Ctrl Pts',(204.340604793794,9.99555392092646,28.4356127000787));
#77402=CARTESIAN_POINT('Ctrl Pts',(204.343615290898,10.0358100954369,28.397623561493));
#77403=CARTESIAN_POINT('Ctrl Pts',(204.346625788002,10.0781739749656,28.3619689368908));
#77404=CARTESIAN_POINT('Ctrl Pts',(204.349636285106,10.1223363910121,28.3288728337801));
#77405=CARTESIAN_POINT('Ctrl Pts',(204.351843549899,10.1547158096761,28.3046071192947));
#77406=CARTESIAN_POINT('Ctrl Pts',(204.354050814692,10.1880613644728,28.2817159252824));
#77407=CARTESIAN_POINT('Ctrl Pts',(204.356258079485,10.2222424211719,28.2602720465459));
#77408=CARTESIAN_POINT('Ctrl Pts',(204.359269473318,10.2688759848679,28.2310159444379));
#77409=CARTESIAN_POINT('Ctrl Pts',(204.36228086715,10.3172595531988,28.2043339143422));
#77410=CARTESIAN_POINT('Ctrl Pts',(204.365292260982,10.3670781215844,28.1804386540131));
#77411=CARTESIAN_POINT('Ctrl Pts',(204.368298343285,10.416808819438,28.1565855404037));
#77412=CARTESIAN_POINT('Ctrl Pts',(204.371304425588,10.4679690223464,28.1355096680641));
#77413=CARTESIAN_POINT('Ctrl Pts',(204.374310507892,10.5202170756615,28.1173790846681));
#77414=CARTESIAN_POINT('Ctrl Pts',(204.377313641088,10.5724138712135,28.0992662882151));
#77415=CARTESIAN_POINT('Ctrl Pts',(204.380316774285,10.6256959069131,28.0840932286431));
#77416=CARTESIAN_POINT('Ctrl Pts',(204.383319907482,10.6797011022628,28.0719800890365));
#77417=CARTESIAN_POINT('Ctrl Pts',(204.386321277629,10.7336745927592,28.0598740606959));
#77418=CARTESIAN_POINT('Ctrl Pts',(204.389322647775,10.7883698875996,28.0508245067879));
#77419=CARTESIAN_POINT('Ctrl Pts',(204.392324017921,10.8434115077447,28.0449012768567));
#77420=CARTESIAN_POINT('Ctrl Pts',(204.395324808445,10.898442498297,28.0389791908148));
#77421=CARTESIAN_POINT('Ctrl Pts',(204.398325598969,10.9538191570559,28.0361822859652));
#77422=CARTESIAN_POINT('Ctrl Pts',(204.401326389493,11.0091599213979,28.0365286658633));
#77423=CARTESIAN_POINT('Ctrl Pts',(204.404329927704,11.0645513587528,28.0368753629255));
#77424=CARTESIAN_POINT('Ctrl Pts',(204.407333465916,11.1199063073609,28.0403710912032));
#77425=CARTESIAN_POINT('Ctrl Pts',(204.410337004127,11.1748437497578,28.0469817918654));
#77426=CARTESIAN_POINT('Ctrl Pts',(204.413341922119,11.229806429616,28.0535955293873));
#77427=CARTESIAN_POINT('Ctrl Pts',(204.416346840112,11.2843507007041,28.063326998946));
#77428=CARTESIAN_POINT('Ctrl Pts',(204.419351758105,11.3381044918167,28.07609073231));
#77429=CARTESIAN_POINT('Ctrl Pts',(204.422362274259,11.3919584262298,28.0888782445064));
#77430=CARTESIAN_POINT('Ctrl Pts',(204.425372790414,11.4450184322874,28.1047091535964));
#77431=CARTESIAN_POINT('Ctrl Pts',(204.428383306568,11.4969275350303,28.1234480485907));
#77432=CARTESIAN_POINT('Ctrl Pts',(204.430590444204,11.5349843095062,28.1371863307617));
#77433=CARTESIAN_POINT('Ctrl Pts',(204.432797581841,11.5724228080511,28.1524865970125));
#77434=CARTESIAN_POINT('Ctrl Pts',(204.435004719478,11.6091104890114,28.1692796453889));
#77435=CARTESIAN_POINT('Ctrl Pts',(204.438015741664,11.6591605717578,28.19218906454));
#77436=CARTESIAN_POINT('Ctrl Pts',(204.44102676385,11.7080206170168,28.2179737904179));
#77437=CARTESIAN_POINT('Ctrl Pts',(204.444037786037,11.7553399525135,28.2464874128526));
#77438=CARTESIAN_POINT('Ctrl Pts',(204.447043495562,11.8025757975657,28.274950725726));
#77439=CARTESIAN_POINT('Ctrl Pts',(204.450049205088,11.8482758793376,28.3061331095639));
#77440=CARTESIAN_POINT('Ctrl Pts',(204.453054914614,11.8921122033382,28.3398413614272));
#77441=CARTESIAN_POINT('Ctrl Pts',(204.456057674636,11.9359055107388,28.3735165353713));
#77442=CARTESIAN_POINT('Ctrl Pts',(204.459060434657,11.9778382671686,28.4097123469522));
#77443=CARTESIAN_POINT('Ctrl Pts',(204.462063194679,12.0176112622621,28.4481922376606));
#77444=CARTESIAN_POINT('Ctrl Pts',(204.465064191928,12.0573609085787,28.4866495387104));
#77445=CARTESIAN_POINT('Ctrl Pts',(204.468065189176,12.0949529281937,28.5273878948412));
#77446=CARTESIAN_POINT('Ctrl Pts',(204.471066186425,12.1301228188404,28.5701319102495));
#77447=CARTESIAN_POINT('Ctrl Pts',(204.474066605003,12.1652859278187,28.6128676835014));
#77448=CARTESIAN_POINT('Ctrl Pts',(204.477067023581,12.198027500383,28.6576079405851));
#77449=CARTESIAN_POINT('Ctrl Pts',(204.48006744216,12.2281229409497,28.7040437876911));
#77450=CARTESIAN_POINT('Ctrl Pts',(204.483070612855,12.2582459863915,28.7505222278192));
#77451=CARTESIAN_POINT('Ctrl Pts',(204.486073783551,12.2857177634556,28.7986989211841));
#77452=CARTESIAN_POINT('Ctrl Pts',(204.489076954246,12.3103575716893,28.8482367881534));
#77453=CARTESIAN_POINT('Ctrl Pts',(204.492081506642,12.335008716218,28.8977974465288));
#77454=CARTESIAN_POINT('Ctrl Pts',(204.495086059038,12.3568250865711,28.9487200409479));
#77455=CARTESIAN_POINT('Ctrl Pts',(204.498090611434,12.3756738622899,29.0006467436649));
#77456=CARTESIAN_POINT('Ctrl Pts',(204.501100769622,12.3945578054185,29.0526703294722));
#77457=CARTESIAN_POINT('Ctrl Pts',(204.50411092781,12.4104629420159,29.1057012591851));
#77458=CARTESIAN_POINT('Ctrl Pts',(204.507121085999,12.4233064824285,29.1593669025522));
#77459=CARTESIAN_POINT('Ctrl Pts',(204.509331177156,12.4327363506682,29.19876880652));
#77460=CARTESIAN_POINT('Ctrl Pts',(204.511541268313,12.4405168791148,29.2385125619717));
#77461=CARTESIAN_POINT('Ctrl Pts',(204.513751359471,12.4466330927872,29.2784487760064));
#77462=CARTESIAN_POINT('Ctrl Pts',(204.516763175375,12.45496800221,29.3328721079075));
#77463=CARTESIAN_POINT('Ctrl Pts',(204.51977499128,12.4602447953578,29.3878794931995));
#77464=CARTESIAN_POINT('Ctrl Pts',(204.522786807184,12.4623933569935,29.4430972810729));
#77465=CARTESIAN_POINT('Ctrl Pts',(204.525793306424,12.4645381258402,29.4982175947048));
#77466=CARTESIAN_POINT('Ctrl Pts',(204.528799805663,12.463565602104,29.5535470509709));
#77467=CARTESIAN_POINT('Ctrl Pts',(204.531806304903,12.4594572324276,29.6087052745489));
#77468=CARTESIAN_POINT('Ctrl Pts',(204.534809851571,12.4553528974288,29.6638093292804));
#77469=CARTESIAN_POINT('Ctrl Pts',(204.537813398239,12.4481188563938,29.7187419610406));
#77470=CARTESIAN_POINT('Ctrl Pts',(204.540816944907,12.4377885958395,29.773123055918));
#77471=CARTESIAN_POINT('Ctrl Pts',(204.543818724355,12.42746441338,29.8274721541724));
#77472=CARTESIAN_POINT('Ctrl Pts',(204.546820503804,12.4140477207097,29.8812698416567));
#77473=CARTESIAN_POINT('Ctrl Pts',(204.549822283252,12.397623519851,29.9341436936767));
#77474=CARTESIAN_POINT('Ctrl Pts',(204.552823478201,12.3812025170739,29.9870072502252));
#77475=CARTESIAN_POINT('Ctrl Pts',(204.55582467315,12.3617753256444,30.0389468252126));
#77476=CARTESIAN_POINT('Ctrl Pts',(204.558825868099,12.3394768554888,30.0896049555507));
#77477=CARTESIAN_POINT('Ctrl Pts',(204.561829800073,12.3171580496061,30.1403092850182));
#77478=CARTESIAN_POINT('Ctrl Pts',(204.564833732047,12.2919629467405,30.1897293514413));
#77479=CARTESIAN_POINT('Ctrl Pts',(204.567837664022,12.264074115055,30.2375289022459));
#77480=CARTESIAN_POINT('Ctrl Pts',(204.570842970426,12.2361725230138,30.2853503234277));
#77481=CARTESIAN_POINT('Ctrl Pts',(204.57384827683,12.205575036934,30.3315493104731));
#77482=CARTESIAN_POINT('Ctrl Pts',(204.576853583234,12.1725078589686,30.375818229233));
#77483=CARTESIAN_POINT('Ctrl Pts',(204.579864474381,12.1393792324633,30.420169412661));
#77484=CARTESIAN_POINT('Ctrl Pts',(204.582875365528,12.1037720863909,30.4625829584856));
#77485=CARTESIAN_POINT('Ctrl Pts',(204.585886256675,12.0659524691719,30.5027849138605));
#77486=CARTESIAN_POINT('Ctrl Pts',(204.588090170938,12.0382692386172,30.5322119700085));
#77487=CARTESIAN_POINT('Ctrl Pts',(204.590294085201,12.0094014093267,30.5604547891699));
#77488=CARTESIAN_POINT('Ctrl Pts',(204.592497999464,11.9794645777,30.5874196020999));
#77489=CARTESIAN_POINT('Ctrl Pts',(204.595509605638,11.9385564768285,30.6242664969574));
#77490=CARTESIAN_POINT('Ctrl Pts',(204.598521211813,11.8954813553504,30.6588782425937));
#77491=CARTESIAN_POINT('Ctrl Pts',(204.601532817987,11.8505130146541,30.6909911258712));
#77492=CARTESIAN_POINT('Ctrl Pts',(204.604539121475,11.8056238519877,30.7230474663723));
#77493=CARTESIAN_POINT('Ctrl Pts',(204.607545424962,11.758848511541,30.7526133723107));
#77494=CARTESIAN_POINT('Ctrl Pts',(204.610551728449,11.7104947221468,30.7794645363594));
#77495=CARTESIAN_POINT('Ctrl Pts',(204.613555088052,11.6621882825954,30.8062894067421));
#77496=CARTESIAN_POINT('Ctrl Pts',(204.616558447654,11.6123069151187,30.8304045468145));
#77497=CARTESIAN_POINT('Ctrl Pts',(204.619561807256,11.5611866969351,30.8516292913307));
#77498=CARTESIAN_POINT('Ctrl Pts',(204.622563408558,11.5100964068086,30.8728416099342));
#77499=CARTESIAN_POINT('Ctrl Pts',(204.625565009859,11.4577691898301,30.8911666853219));
#77500=CARTESIAN_POINT('Ctrl Pts',(204.628566611161,11.4045629743253,30.9064711336551));
#77501=CARTESIAN_POINT('Ctrl Pts',(204.631567637126,11.3513669572101,30.9217726484828));
#77502=CARTESIAN_POINT('Ctrl Pts',(204.63456866309,11.297292782866,30.934054540551));
#77503=CARTESIAN_POINT('Ctrl Pts',(204.637569689055,11.2427132686662,30.9432333557722));
#77504=CARTESIAN_POINT('Ctrl Pts',(204.640573467329,11.1880836983501,30.9524205890939));
#77505=CARTESIAN_POINT('Ctrl Pts',(204.643577245603,11.1329483835845,30.9584989726131));
#77506=CARTESIAN_POINT('Ctrl Pts',(204.646581023877,11.0776885739645,30.9614365314564));
#77507=CARTESIAN_POINT('Ctrl Pts',(204.649586184862,11.0224033269251,30.9643754425287));
#77508=CARTESIAN_POINT('Ctrl Pts',(204.652591345848,10.9669939991435,30.9641706488739));
#77509=CARTESIAN_POINT('Ctrl Pts',(204.655596506833,10.9118418677849,30.9608423575884));
#77510=CARTESIAN_POINT('Ctrl Pts',(204.658607267649,10.8565869656935,30.9575078643497));
#77511=CARTESIAN_POINT('Ctrl Pts',(204.661618028465,10.8015907424027,30.9510383089441));
#77512=CARTESIAN_POINT('Ctrl Pts',(204.664628789281,10.7472281931458,30.9415056932457));
#77513=CARTESIAN_POINT('Ctrl Pts',(204.666834072673,10.7074094116684,30.9345233654006));
#77514=CARTESIAN_POINT('Ctrl Pts',(204.669039356065,10.6679304544797,30.9258987751431));
#77515=CARTESIAN_POINT('Ctrl Pts',(204.671244639457,10.6289334192774,30.9156771675318));
#77516=CARTESIAN_POINT('Ctrl Pts',(204.674253319779,10.5757295485697,30.9017317717611));
#77517=CARTESIAN_POINT('Ctrl Pts',(204.677262000102,10.5232010291994,30.8847536203949));
#77518=CARTESIAN_POINT('Ctrl Pts',(204.680270680425,10.4717180778835,30.8648261650353));
#77519=CARTESIAN_POINT('Ctrl Pts',(204.683274043593,10.4203261109018,30.8449339268925));
#77520=CARTESIAN_POINT('Ctrl Pts',(204.686277406762,10.369976534148,30.8221029173947));
#77521=CARTESIAN_POINT('Ctrl Pts',(204.689280769931,10.3210253251765,30.79646659847));
#77522=CARTESIAN_POINT('Ctrl Pts',(204.692281182635,10.2721222052251,30.7708554643258));
#77523=CARTESIAN_POINT('Ctrl Pts',(204.69528159534,10.2246151978537,30.7424447239705));
#77524=CARTESIAN_POINT('Ctrl Pts',(204.698282008044,10.1788394205826,30.7114155161673));
#77525=CARTESIAN_POINT('Ctrl Pts',(204.701280661182,10.1330904881283,30.6804045051801));
#77526=CARTESIAN_POINT('Ctrl Pts',(204.70427931432,10.0890712102181,30.6467783663478));
#77527=CARTESIAN_POINT('Ctrl Pts',(204.707277967458,10.0470892181024,30.6107624821461));
#77528=CARTESIAN_POINT('Ctrl Pts',(204.710276049297,10.0051152243286,30.5747534596329));
#77529=CARTESIAN_POINT('Ctrl Pts',(204.713274131136,9.96517814644921,30.5363559400557));
#77530=CARTESIAN_POINT('Ctrl Pts',(204.716272212975,9.92755207795919,30.4958351793898));
#77531=CARTESIAN_POINT('Ctrl Pts',(204.719273076784,9.88989109562312,30.4552768188456));
#77532=CARTESIAN_POINT('Ctrl Pts',(204.722273940592,9.85454576702586,30.4125916696237));
#77533=CARTESIAN_POINT('Ctrl Pts',(204.725274804401,9.8217517992952,30.3680803116854));
#77534=CARTESIAN_POINT('Ctrl Pts',(204.728277063021,9.78894258882165,30.3235482647232));
#77535=CARTESIAN_POINT('Ctrl Pts',(204.731279321641,9.75868739212584,30.2771887607261));
#77536=CARTESIAN_POINT('Ctrl Pts',(204.73428158026,9.73117831254707,30.2293310465414));
#77537=CARTESIAN_POINT('Ctrl Pts',(204.737289494286,9.70361741364187,30.1813831819572));
#77538=CARTESIAN_POINT('Ctrl Pts',(204.740297408312,9.67881320209428,30.131931943521));
#77539=CARTESIAN_POINT('Ctrl Pts',(204.743305322338,9.65691103634704,30.0813297564323));
#77540=CARTESIAN_POINT('Ctrl Pts',(204.745533974709,9.64068307464761,30.0438371009817));
#77541=CARTESIAN_POINT('Ctrl Pts',(204.747762627079,9.62604727834639,30.0057130844164));
#77542=CARTESIAN_POINT('Ctrl Pts',(204.74999127945,9.61304502324796,29.9671061361862));
#77543=CARTESIAN_POINT('Ctrl Pts',(204.753547770861,9.59229597813274,29.9054970303406));
#77544=CARTESIAN_POINT('Ctrl Pts',(204.757104262271,9.57563762197559,29.8424493021325));
#77545=CARTESIAN_POINT('Ctrl Pts',(204.760660753682,9.56323692096333,29.7784674212849));
#77546=CARTESIAN_POINT('Ctrl Pts',(204.764179434315,9.55096805779392,29.7151657627202));
#77547=CARTESIAN_POINT('Ctrl Pts',(204.767698114948,9.54286688239446,29.6509498184118));
#77548=CARTESIAN_POINT('Ctrl Pts',(204.77121679558,9.53904836750614,29.5863283123519));
#77549=CARTESIAN_POINT('Ctrl Pts',(204.772759515096,9.5373741895816,29.5579958579657));
#77550=CARTESIAN_POINT('Ctrl Pts',(204.774302234611,9.53652263808773,29.5295856968488));
#77551=CARTESIAN_POINT('Ctrl Pts',(204.775844954127,9.53650044545502,29.5011418610453));
#77552=CARTESIAN_POINT('',(204.899999975772,10.9852095428848,28.0365747397361));
#77553=CARTESIAN_POINT('Ctrl Pts',(204.775844954157,9.53650044545459,29.5011418604867));
#77554=CARTESIAN_POINT('Ctrl Pts',(204.77884502705,9.53645728823607,29.4458281239961));
#77555=CARTESIAN_POINT('Ctrl Pts',(204.781845099943,9.53955436493385,29.3904748053103));
#77556=CARTESIAN_POINT('Ctrl Pts',(204.784845172835,9.54577854890722,29.3354636174531));
#77557=CARTESIAN_POINT('Ctrl Pts',(204.787844592698,9.55200137805301,29.2804644039648));
#77558=CARTESIAN_POINT('Ctrl Pts',(204.79084401256,9.56134990379099,29.2258076973229));
#77559=CARTESIAN_POINT('Ctrl Pts',(204.793843432423,9.5737591602953,29.1718699691305));
#77560=CARTESIAN_POINT('Ctrl Pts',(204.796845619017,9.58617986337696,29.1178824875642));
#77561=CARTESIAN_POINT('Ctrl Pts',(204.799847805612,9.60166682078197,29.0646158250656));
#77562=CARTESIAN_POINT('Ctrl Pts',(204.802849992207,9.62010423858225,29.0124346837384));
#77563=CARTESIAN_POINT('Ctrl Pts',(204.805853487826,9.63854969553359,28.960230790197));
#77564=CARTESIAN_POINT('Ctrl Pts',(204.808856983445,9.65994797423536,28.9091138493192));
#77565=CARTESIAN_POINT('Ctrl Pts',(204.811860479065,9.68413500609405,28.8594287176177));
#77566=CARTESIAN_POINT('Ctrl Pts',(204.814869825617,9.70836915528207,28.8096467972434));
#77567=CARTESIAN_POINT('Ctrl Pts',(204.817879172168,9.73540265495082,28.7613027214988));
#77568=CARTESIAN_POINT('Ctrl Pts',(204.82088851872,9.76502584936004,28.7147159130282));
#77569=CARTESIAN_POINT('Ctrl Pts',(204.823504985628,9.79078164269565,28.6742111587279));
#77570=CARTESIAN_POINT('Ctrl Pts',(204.826121452535,9.81849424882487,28.6350345149928));
#77571=CARTESIAN_POINT('Ctrl Pts',(204.828737919443,9.84800131355898,28.5973753402227));
#77572=CARTESIAN_POINT('Ctrl Pts',(204.831710460538,9.88152398578609,28.5545911397764));
#77573=CARTESIAN_POINT('Ctrl Pts',(204.834683001634,9.91751103353325,28.5135781388271));
#77574=CARTESIAN_POINT('Ctrl Pts',(204.837655542729,9.95574604316337,28.4746386375375));
#77575=CARTESIAN_POINT('Ctrl Pts',(204.840624029014,9.99392889683818,28.4357522531925));
#77576=CARTESIAN_POINT('Ctrl Pts',(204.843592515299,10.0343532692239,28.3989341555116));
#77577=CARTESIAN_POINT('Ctrl Pts',(204.846561001584,10.0767619821704,28.364454398787));
#77578=CARTESIAN_POINT('Ctrl Pts',(204.849526680816,10.1191305926865,28.3300072467315));
#77579=CARTESIAN_POINT('Ctrl Pts',(204.852492360048,10.1634794107131,28.2978943990209));
#77580=CARTESIAN_POINT('Ctrl Pts',(204.85545803928,10.2095156111155,28.26834798708));
#77581=CARTESIAN_POINT('Ctrl Pts',(204.858422154716,10.2555275367431,28.2388171548891));
#77582=CARTESIAN_POINT('Ctrl Pts',(204.861386270152,10.3032246264038,28.2118503695707));
#77583=CARTESIAN_POINT('Ctrl Pts',(204.864350385589,10.3522843261273,28.1876369954088));
#77584=CARTESIAN_POINT('Ctrl Pts',(204.867321184771,10.4014546499341,28.1633690228222));
#77585=CARTESIAN_POINT('Ctrl Pts',(204.870291983953,10.451993256,28.1418671547788));
#77586=CARTESIAN_POINT('Ctrl Pts',(204.873262783135,10.5035519629505,28.1232750468922));
#77587=CARTESIAN_POINT('Ctrl Pts',(204.876229173213,10.5550341491911,28.1047105324302));
#77588=CARTESIAN_POINT('Ctrl Pts',(204.879195563292,10.607532885305,28.0890472933377));
#77589=CARTESIAN_POINT('Ctrl Pts',(204.882161953371,10.6606857674985,28.0763785258637));
#77590=CARTESIAN_POINT('Ctrl Pts',(204.885134957104,10.713957155623,28.0636815129961));
#77591=CARTESIAN_POINT('Ctrl Pts',(204.888107960838,10.7678850709837,28.0539924264728));
#77592=CARTESIAN_POINT('Ctrl Pts',(204.891080964572,10.822096819896,28.0473532058656));
#77593=CARTESIAN_POINT('Ctrl Pts',(204.894053968305,10.8763085688083,28.0407139852585));
#77594=CARTESIAN_POINT('Ctrl Pts',(204.897026972039,10.9308036068453,28.0371246063304));
#77595=CARTESIAN_POINT('Ctrl Pts',(204.899999975772,10.9852095428848,28.0365747397361));
#77596=CARTESIAN_POINT('',(204.9,9.84750728139498,28.5980062175589));
#77597=CARTESIAN_POINT('Origin',(204.9,11.,29.5));
#77598=CARTESIAN_POINT('',(204.847155045794,9.53650147895644,29.5020806016713));
#77599=CARTESIAN_POINT('Ctrl Pts',(204.9,9.84750728139498,28.5980062175589));
#77600=CARTESIAN_POINT('Ctrl Pts',(204.896944428771,9.8128730288008,28.6422589881502));
#77601=CARTESIAN_POINT('Ctrl Pts',(204.893888857542,9.78075513505351,28.6885550368351));
#77602=CARTESIAN_POINT('Ctrl Pts',(204.890833286313,9.75139134325211,28.736580932715));
#77603=CARTESIAN_POINT('Ctrl Pts',(204.887780085735,9.722050333216,28.7845695679205));
#77604=CARTESIAN_POINT('Ctrl Pts',(204.884726885158,9.69545944481763,28.8342849570117));
#77605=CARTESIAN_POINT('Ctrl Pts',(204.88167368458,9.67181316691742,28.8853846841918));
#77606=CARTESIAN_POINT('Ctrl Pts',(204.878620835613,9.64816961215427,28.9364785266587));
#77607=CARTESIAN_POINT('Ctrl Pts',(204.875567986645,9.627470219116,28.988955939797));
#77608=CARTESIAN_POINT('Ctrl Pts',(204.872515137678,9.60986278229004,29.0424513512886));
#77609=CARTESIAN_POINT('Ctrl Pts',(204.869462692086,9.59225767194476,29.095939694401));
#77610=CARTESIAN_POINT('Ctrl Pts',(204.866410246493,9.57774385730325,29.150445287817));
#77611=CARTESIAN_POINT('Ctrl Pts',(204.863357800901,9.56641955808898,29.2055864021989));
#77612=CARTESIAN_POINT('Ctrl Pts',(204.860302850763,9.55508596723761,29.2607727601066));
#77613=CARTESIAN_POINT('Ctrl Pts',(204.857247900626,9.54694721616499,29.316595185212));
#77614=CARTESIAN_POINT('Ctrl Pts',(204.854192950489,9.54205031404698,29.3726620118367));
#77615=CARTESIAN_POINT('Ctrl Pts',(204.851846982273,9.53828986749146,29.4157170494868));
#77616=CARTESIAN_POINT('Ctrl Pts',(204.849501014058,9.53644011341938,29.4589159667267));
#77617=CARTESIAN_POINT('Ctrl Pts',(204.847155045843,9.53650147895516,29.5020806007706));
#77618=CARTESIAN_POINT('',(204.347155045812,9.53650002200871,29.4997461900754));
#77619=CARTESIAN_POINT('Ctrl Pts',(204.847155045794,9.53650147895644,29.5020806016713));
#77620=CARTESIAN_POINT('Ctrl Pts',(204.843480671734,9.5365975928036,29.5696872344555));
#77621=CARTESIAN_POINT('Ctrl Pts',(204.839806297674,9.54138208774555,29.6370889378409));
#77622=CARTESIAN_POINT('Ctrl Pts',(204.836131923613,9.55074824008612,29.70371938147));
#77623=CARTESIAN_POINT('Ctrl Pts',(204.832398190929,9.5602657003511,29.7714262237911));
#77624=CARTESIAN_POINT('Ctrl Pts',(204.828664458245,9.57451398745482,29.8383367658986));
#77625=CARTESIAN_POINT('Ctrl Pts',(204.824930725562,9.59333225587688,29.9038788279219));
#77626=CARTESIAN_POINT('Ctrl Pts',(204.823736517463,9.59935114647561,29.9248419947811));
#77627=CARTESIAN_POINT('Ctrl Pts',(204.822542309365,9.60583717740501,29.945665328066));
#77628=CARTESIAN_POINT('Ctrl Pts',(204.821348101266,9.61278405850875,29.9663305497955));
#77629=CARTESIAN_POINT('Ctrl Pts',(204.818357740167,9.63017942120929,30.0180773728522));
#77630=CARTESIAN_POINT('Ctrl Pts',(204.815367379068,9.65051610637708,30.0689738372223));
#77631=CARTESIAN_POINT('Ctrl Pts',(204.812377017968,9.67369195589128,30.1186592132447));
#77632=CARTESIAN_POINT('Ctrl Pts',(204.809392486883,9.69682262172008,30.1682477225524));
#77633=CARTESIAN_POINT('Ctrl Pts',(204.806407955799,9.72278124746231,30.216629345757));
#77634=CARTESIAN_POINT('Ctrl Pts',(204.803423424714,9.75141651626197,30.26346023743));
#77635=CARTESIAN_POINT('Ctrl Pts',(204.80044214556,9.78002058420834,30.310240102385));
#77636=CARTESIAN_POINT('Ctrl Pts',(204.797460866406,9.81129524343232,30.3554721258835));
#77637=CARTESIAN_POINT('Ctrl Pts',(204.794479587252,9.84504271709853,30.3988358719326));
#77638=CARTESIAN_POINT('Ctrl Pts',(204.791500335576,9.8787672401208,30.4421701275996));
#77639=CARTESIAN_POINT('Ctrl Pts',(204.788521083901,9.91496091787146,30.4836382002108));
#77640=CARTESIAN_POINT('Ctrl Pts',(204.785541832225,9.95338335630434,30.5229495838697));
#77641=CARTESIAN_POINT('Ctrl Pts',(204.782563386677,9.99179539837381,30.562250330634));
#77642=CARTESIAN_POINT('Ctrl Pts',(204.779584941129,10.0324346299407,30.5993951627963));
#77643=CARTESIAN_POINT('Ctrl Pts',(204.776606495581,10.0750228133266,30.6341293815671));
#77644=CARTESIAN_POINT('Ctrl Pts',(204.773625487682,10.1176476352518,30.6688934821253));
#77645=CARTESIAN_POINT('Ctrl Pts',(204.770644479783,10.1622243431096,30.7012424849852));
#77646=CARTESIAN_POINT('Ctrl Pts',(204.767663471883,10.2084417691068,30.7309621509637));
#77647=CARTESIAN_POINT('Ctrl Pts',(204.76468121849,10.2546785051806,30.760694234099));
#77648=CARTESIAN_POINT('Ctrl Pts',(204.761698965098,10.3025568579594,30.7877945260522));
#77649=CARTESIAN_POINT('Ctrl Pts',(204.758716711705,10.3517397670182,30.8120940973628));
#77650=CARTESIAN_POINT('Ctrl Pts',(204.755728826154,10.4010155608455,30.8364395598194));
#77651=CARTESIAN_POINT('Ctrl Pts',(204.752740940603,10.4516003371407,30.8579735262758));
#77652=CARTESIAN_POINT('Ctrl Pts',(204.749753055053,10.5031368856387,30.8765752052057));
#77653=CARTESIAN_POINT('Ctrl Pts',(204.747400770879,10.5437102628091,30.8912198206723));
#77654=CARTESIAN_POINT('Ctrl Pts',(204.745048486706,10.5848730993982,30.9040479657026));
#77655=CARTESIAN_POINT('Ctrl Pts',(204.742696202532,10.6264463316923,30.9150229351123));
#77656=CARTESIAN_POINT('Ctrl Pts',(204.739683723208,10.6796875617006,30.9290781537814));
#77657=CARTESIAN_POINT('Ctrl Pts',(204.736671243883,10.7338342815209,30.9401536806686));
#77658=CARTESIAN_POINT('Ctrl Pts',(204.733658764559,10.7885223279762,30.9481399946951));
#77659=CARTESIAN_POINT('Ctrl Pts',(204.730651668706,10.8431126438015,30.9561120367269));
#77660=CARTESIAN_POINT('Ctrl Pts',(204.727644572852,10.8982418488908,30.9610057468302));
#77661=CARTESIAN_POINT('Ctrl Pts',(204.724637476999,10.9535336079107,30.9627621557882));
#77662=CARTESIAN_POINT('Ctrl Pts',(204.721633374798,11.0087703223461,30.9645168161891));
#77663=CARTESIAN_POINT('Ctrl Pts',(204.718629272598,11.0641687458025,30.9631403463521));
#77664=CARTESIAN_POINT('Ctrl Pts',(204.715625170398,11.1193472528364,30.9586255459303));
#77665=CARTESIAN_POINT('Ctrl Pts',(204.712622877549,11.1744925261935,30.954113464745));
#77666=CARTESIAN_POINT('Ctrl Pts',(204.709620584701,11.2294176213348,30.9464668426916));
#77667=CARTESIAN_POINT('Ctrl Pts',(204.706618291853,11.2837430606454,30.9357305198176));
#77668=CARTESIAN_POINT('Ctrl Pts',(204.703616626739,11.3380571413316,30.9249964417456));
#77669=CARTESIAN_POINT('Ctrl Pts',(204.700614961625,11.3917712983336,30.9111740479915));
#77670=CARTESIAN_POINT('Ctrl Pts',(204.697613296511,11.4445156010062,30.8943593978821));
#77671=CARTESIAN_POINT('Ctrl Pts',(204.694608975607,11.4973065703731,30.8775298706372));
#77672=CARTESIAN_POINT('Ctrl Pts',(204.691604654702,11.5491254677475,30.8577029581842));
#77673=CARTESIAN_POINT('Ctrl Pts',(204.688600333798,11.599618372578,30.8350243657952));
#77674=CARTESIAN_POINT('Ctrl Pts',(204.685594677007,11.6501337293446,30.8123356892507));
#77675=CARTESIAN_POINT('Ctrl Pts',(204.682589020216,11.6993214493171,30.7867930478673));
#77676=CARTESIAN_POINT('Ctrl Pts',(204.679583363424,11.7468513984568,30.7585885898986));
#77677=CARTESIAN_POINT('Ctrl Pts',(204.67657221711,11.7944681561573,30.7303326193901));
#77678=CARTESIAN_POINT('Ctrl Pts',(204.673561070796,11.840420656537,30.6994054160022));
#77679=CARTESIAN_POINT('Ctrl Pts',(204.670549924482,11.8844080048257,30.6660423367101));
#77680=CARTESIAN_POINT('Ctrl Pts',(204.668381384254,11.9160864170777,30.6420152148005));
#77681=CARTESIAN_POINT('Ctrl Pts',(204.666212844026,11.9467462494712,30.6167256379604));
#77682=CARTESIAN_POINT('Ctrl Pts',(204.664044303798,11.9762868220711,30.5902734936934));
#77683=CARTESIAN_POINT('Ctrl Pts',(204.661028090037,12.017374684051,30.5534813140888));
#77684=CARTESIAN_POINT('Ctrl Pts',(204.658011876276,12.0564621266647,30.5142895979169));
#77685=CARTESIAN_POINT('Ctrl Pts',(204.654995662514,12.0932576001057,30.472944021931));
#77686=CARTESIAN_POINT('Ctrl Pts',(204.651984609947,12.1299901109792,30.4316691944195));
#77687=CARTESIAN_POINT('Ctrl Pts',(204.648973557379,12.1644380899798,30.3882482117569));
#77688=CARTESIAN_POINT('Ctrl Pts',(204.645962504812,12.1963456719334,30.3429645800663));
#77689=CARTESIAN_POINT('Ctrl Pts',(204.642954312931,12.2282229397049,30.2977239706346));
#77690=CARTESIAN_POINT('Ctrl Pts',(204.63994612105,12.2575642911831,30.2506246461356));
#77691=CARTESIAN_POINT('Ctrl Pts',(204.636937929169,12.2841543313563,30.2019828368691));
#77692=CARTESIAN_POINT('Ctrl Pts',(204.633931421654,12.3107294830621,30.1533682634392));
#77693=CARTESIAN_POINT('Ctrl Pts',(204.63092491414,12.3345561259627,30.1032133778017));
#77694=CARTESIAN_POINT('Ctrl Pts',(204.627918406625,12.3554636139356,30.0518610706478));
#77695=CARTESIAN_POINT('Ctrl Pts',(204.624912409678,12.3763675513833,30.0005174841813));
#77696=CARTESIAN_POINT('Ctrl Pts',(204.621906412731,12.3943531208892,29.9479773667534));
#77697=CARTESIAN_POINT('Ctrl Pts',(204.618900415784,12.4092977732584,29.8946036445458));
#77698=CARTESIAN_POINT('Ctrl Pts',(204.615891616779,12.4242563563722,29.8411801697128));
#77699=CARTESIAN_POINT('Ctrl Pts',(204.612882817774,12.4361682182349,29.7869220450714));
#77700=CARTESIAN_POINT('Ctrl Pts',(204.609874018769,12.4449611154638,29.7322059964722));
#77701=CARTESIAN_POINT('Ctrl Pts',(204.606863795824,12.4537581740084,29.6774640530233));
#77702=CARTESIAN_POINT('Ctrl Pts',(204.603853572879,12.4594332718064,29.6222642772503));
#77703=CARTESIAN_POINT('Ctrl Pts',(204.600843349933,12.4619660503887,29.5669889357338));
#77704=CARTESIAN_POINT('Ctrl Pts',(204.597827550221,12.4645035212199,29.5116111906123));
#77705=CARTESIAN_POINT('Ctrl Pts',(204.59481175051,12.4638870503377,29.4561581267354));
#77706=CARTESIAN_POINT('Ctrl Pts',(204.591795950798,12.460148443117,29.4010112427443));
#77707=CARTESIAN_POINT('Ctrl Pts',(204.589661435553,12.4575023409651,29.3619795178844));
#77708=CARTESIAN_POINT('Ctrl Pts',(204.587526920308,12.4532933123618,29.3231011244392));
#77709=CARTESIAN_POINT('Ctrl Pts',(204.585392405063,12.4475481247927,29.2845082915538));
#77710=CARTESIAN_POINT('Ctrl Pts',(204.582383124728,12.4394484496964,29.2300993791108));
#77711=CARTESIAN_POINT('Ctrl Pts',(204.579373844393,12.4282598493919,29.1760331613628));
#77712=CARTESIAN_POINT('Ctrl Pts',(204.576364564058,12.4140251108699,29.1226868199632));
#77713=CARTESIAN_POINT('Ctrl Pts',(204.573360635559,12.3998156880296,29.069435352031));
#77714=CARTESIAN_POINT('Ctrl Pts',(204.57035670706,12.3825710128448,29.016901726235));
#77715=CARTESIAN_POINT('Ctrl Pts',(204.567352778561,12.362385131464,28.9654543952422));
#77716=CARTESIAN_POINT('Ctrl Pts',(204.564351821726,12.3422192191539,28.9140579589998));
#77717=CARTESIAN_POINT('Ctrl Pts',(204.561350864892,12.3191180564608,28.863746178314));
#77718=CARTESIAN_POINT('Ctrl Pts',(204.558349908057,12.2932253495535,28.8148719497261));
#77719=CARTESIAN_POINT('Ctrl Pts',(204.555350732824,12.2673480145746,28.7660267366885));
#77720=CARTESIAN_POINT('Ctrl Pts',(204.552351557591,12.2386826671073,28.7186178501997));
#77721=CARTESIAN_POINT('Ctrl Pts',(204.549352382358,12.2074199818975,28.6729756730817));
#77722=CARTESIAN_POINT('Ctrl Pts',(204.54635380132,12.1761634904385,28.6273425385738));
#77723=CARTESIAN_POINT('Ctrl Pts',(204.543355220283,12.1423109816929,28.5834758540026));
#77724=CARTESIAN_POINT('Ctrl Pts',(204.540356639245,12.1060964142555,28.541676999978));
#77725=CARTESIAN_POINT('Ctrl Pts',(204.537355325727,12.069848846013,28.499840056424));
#77726=CARTESIAN_POINT('Ctrl Pts',(204.534354012209,12.0312352658389,28.4600751080151));
#77727=CARTESIAN_POINT('Ctrl Pts',(204.531352698691,11.9905289159791,28.4226492137612));
#77728=CARTESIAN_POINT('Ctrl Pts',(204.52835001098,11.9498039281474,28.385206183538));
#77729=CARTESIAN_POINT('Ctrl Pts',(204.525347323269,11.9069846700171,28.3501046777673));
#77730=CARTESIAN_POINT('Ctrl Pts',(204.522344635558,11.8623776271863,28.3175715336104));
#77731=CARTESIAN_POINT('Ctrl Pts',(204.519336359239,11.8176875616475,28.2849778387073));
#77732=CARTESIAN_POINT('Ctrl Pts',(204.51632808292,11.7712035099089,28.2549623410386));
#77733=CARTESIAN_POINT('Ctrl Pts',(204.513319806601,11.7232600749857,28.2277079289991));
#77734=CARTESIAN_POINT('Ctrl Pts',(204.51112670651,11.6883082486477,28.2078388587484));
#77735=CARTESIAN_POINT('Ctrl Pts',(204.50893360642,11.6525813804009,28.1894362919722));
#77736=CARTESIAN_POINT('Ctrl Pts',(204.506740506329,11.616215732215,28.1725549271737));
#77737=CARTESIAN_POINT('Ctrl Pts',(204.503728413225,11.5662696679212,28.1493693722983));
#77738=CARTESIAN_POINT('Ctrl Pts',(204.500716320121,11.5149098201128,28.1289586131801));
#77739=CARTESIAN_POINT('Ctrl Pts',(204.497704227016,11.4624755881642,28.1114941194391));
#77740=CARTESIAN_POINT('Ctrl Pts',(204.494697435409,11.4101336441761,28.0940603644436));
#77741=CARTESIAN_POINT('Ctrl Pts',(204.491690643802,11.3567215652475,28.0795627486606));
#77742=CARTESIAN_POINT('Ctrl Pts',(204.488683852195,11.3025995721126,28.0681250931184));
#77743=CARTESIAN_POINT('Ctrl Pts',(204.485680003688,11.2485305545185,28.0566986329507));
#77744=CARTESIAN_POINT('Ctrl Pts',(204.48267615518,11.1937535127567,28.0483263078363));
#77745=CARTESIAN_POINT('Ctrl Pts',(204.479672306672,11.1386429125202,28.0430818853457));
#77746=CARTESIAN_POINT('Ctrl Pts',(204.476670216574,11.0835645732319,28.0378405328641));
#77747=CARTESIAN_POINT('Ctrl Pts',(204.473668126476,11.0281535864119,28.0357235033241));
#77748=CARTESIAN_POINT('Ctrl Pts',(204.470666036378,10.9727913845649,28.0367529459295));
#77749=CARTESIAN_POINT('Ctrl Pts',(204.467664522619,10.9174398111179,28.0377821909031));
#77750=CARTESIAN_POINT('Ctrl Pts',(204.46466300886,10.8621375309362,28.0419566983604));
#77751=CARTESIAN_POINT('Ctrl Pts',(204.461661495101,10.8072655128246,28.0492465173389));
#77752=CARTESIAN_POINT('Ctrl Pts',(204.458657244735,10.7523434655693,28.0565429827542));
#77753=CARTESIAN_POINT('Ctrl Pts',(204.455652994369,10.6978529878251,28.066960364255));
#77754=CARTESIAN_POINT('Ctrl Pts',(204.452648744003,10.6441679554212,28.080417030938));
#77755=CARTESIAN_POINT('Ctrl Pts',(204.449643112758,10.5904582471296,28.0938798828682));
#77756=CARTESIAN_POINT('Ctrl Pts',(204.446637481513,10.5375552263495,28.1103846474473));
#77757=CARTESIAN_POINT('Ctrl Pts',(204.443631850267,10.4858174448169,28.1297998139157));
#77758=CARTESIAN_POINT('Ctrl Pts',(204.4406206558,10.4339839001211,28.149250916555));
#77759=CARTESIAN_POINT('Ctrl Pts',(204.437609461333,10.3833203862242,28.1716229680429));
#77760=CARTESIAN_POINT('Ctrl Pts',(204.434598266866,10.3341642058072,28.1967368089401));
#77761=CARTESIAN_POINT('Ctrl Pts',(204.432428380442,10.2987419407575,28.2148340069146));
#77762=CARTESIAN_POINT('Ctrl Pts',(204.430258494019,10.2641019226929,28.2343539436618));
#77763=CARTESIAN_POINT('Ctrl Pts',(204.428088607595,10.2303609019492,28.255215717985));
#77764=CARTESIAN_POINT('Ctrl Pts',(204.425076395235,10.1835219897325,28.2841758026142));
#77765=CARTESIAN_POINT('Ctrl Pts',(204.422064182875,10.1382231831636,28.3158430596894));
#77766=CARTESIAN_POINT('Ctrl Pts',(204.419051970515,10.0947943556126,28.3500282649694));
#77767=CARTESIAN_POINT('Ctrl Pts',(204.416045042677,10.0514417180964,28.3841534969063));
#77768=CARTESIAN_POINT('Ctrl Pts',(204.413038114838,10.0099529598516,28.4207875866823));
#77769=CARTESIAN_POINT('Ctrl Pts',(204.410031186999,9.9706296031815,28.4596977188558));
#77770=CARTESIAN_POINT('Ctrl Pts',(204.407027191949,9.93134460030811,28.4985699002687));
#77771=CARTESIAN_POINT('Ctrl Pts',(204.404023196899,9.89422118786101,28.5397133570908));
#77772=CARTESIAN_POINT('Ctrl Pts',(204.40101920185,9.8595269111191,28.5828558545471));
#77773=CARTESIAN_POINT('Ctrl Pts',(204.398016955171,9.82485282698333,28.6259732424021));
#77774=CARTESIAN_POINT('Ctrl Pts',(204.395014708493,9.79260540582357,28.6710869545319));
#77775=CARTESIAN_POINT('Ctrl Pts',(204.392012461815,9.76301290768435,28.7178905553284));
#77776=CARTESIAN_POINT('Ctrl Pts',(204.389010781698,9.73342599402148,28.7646853236972));
#77777=CARTESIAN_POINT('Ctrl Pts',(204.386009101582,9.70649328975003,28.8131689018786));
#77778=CARTESIAN_POINT('Ctrl Pts',(204.383007421465,9.68239928225008,28.8630065945515));
#77779=CARTESIAN_POINT('Ctrl Pts',(204.380002990889,9.65828319725208,28.912889953831));
#77780=CARTESIAN_POINT('Ctrl Pts',(204.376998560313,9.63701123510605,28.9641294306037));
#77781=CARTESIAN_POINT('Ctrl Pts',(204.373994129738,9.61872081752739,29.0163678359871));
#77782=CARTESIAN_POINT('Ctrl Pts',(204.370988310287,9.60042194473881,29.0686303898997));
#77783=CARTESIAN_POINT('Ctrl Pts',(204.367982490837,9.58510750986192,29.1218922853876));
#77784=CARTESIAN_POINT('Ctrl Pts',(204.364976671387,9.57286484592985,29.1757817062269));
#77785=CARTESIAN_POINT('Ctrl Pts',(204.36196527795,9.56059947922074,29.2297710595247));
#77786=CARTESIAN_POINT('Ctrl Pts',(204.358953884513,9.55141734928508,29.2843897415511));
#77787=CARTESIAN_POINT('Ctrl Pts',(204.355942491076,9.54535430667095,29.3392574826648));
#77788=CARTESIAN_POINT('Ctrl Pts',(204.353773897004,9.54098812917084,29.3787693766064));
#77789=CARTESIAN_POINT('Ctrl Pts',(204.351605302932,9.53823837420049,29.4184102735999));
#77790=CARTESIAN_POINT('Ctrl Pts',(204.349436708861,9.53710168569658,29.45803844607));
#77791=CARTESIAN_POINT('Ctrl Pts',(204.348676154521,9.53670303415301,29.4719365650972));
#77792=CARTESIAN_POINT('Ctrl Pts',(204.347915600182,9.53650243364758,29.4858404079313));
#77793=CARTESIAN_POINT('Ctrl Pts',(204.347155045843,9.5365000220088,29.4997461895053));
#77794=CARTESIAN_POINT('',(203.847155045875,9.53650022221242,29.4991935164512));
#77795=CARTESIAN_POINT('Ctrl Pts',(204.347155045812,9.5365000220087,29.4997461900754));
#77796=CARTESIAN_POINT('Ctrl Pts',(204.344157838136,9.53649051819596,29.5545463708471));
#77797=CARTESIAN_POINT('Ctrl Pts',(204.341160630459,9.53956326457731,29.6094653416477));
#77798=CARTESIAN_POINT('Ctrl Pts',(204.338163422783,9.54573220191339,29.6641262363192));
#77799=CARTESIAN_POINT('Ctrl Pts',(204.335171425959,9.55189041412612,29.7186920992526));
#77800=CARTESIAN_POINT('Ctrl Pts',(204.332179429135,9.5611340783862,29.7730002507101));
#77801=CARTESIAN_POINT('Ctrl Pts',(204.329187432311,9.5734251417044,29.8266747980468));
#77802=CARTESIAN_POINT('Ctrl Pts',(204.326198301077,9.58570443323677,29.8802979384987));
#77803=CARTESIAN_POINT('Ctrl Pts',(204.323209169843,9.60102522520536,29.9332881593667));
#77804=CARTESIAN_POINT('Ctrl Pts',(204.320220038609,9.61929804605378,29.9852776157717));
#77805=CARTESIAN_POINT('Ctrl Pts',(204.317232562801,9.63756074713743,30.0372382796289));
#77806=CARTESIAN_POINT('Ctrl Pts',(204.314245086993,9.65877206070803,30.0881987752968));
#77807=CARTESIAN_POINT('Ctrl Pts',(204.311257611186,9.68279275238454,30.1378066453317));
#77808=CARTESIAN_POINT('Ctrl Pts',(204.308270583197,9.70680984338501,30.1874070791999));
#77809=CARTESIAN_POINT('Ctrl Pts',(204.305283555209,9.73363524307626,30.2356548108838));
#77810=CARTESIAN_POINT('Ctrl Pts',(204.30229652722,9.76308267958039,30.282219785256));
#77811=CARTESIAN_POINT('Ctrl Pts',(204.299306701674,9.79255769563509,30.3288283709309));
#77812=CARTESIAN_POINT('Ctrl Pts',(204.296316876129,9.8246593653189,30.3737506016701));
#77813=CARTESIAN_POINT('Ctrl Pts',(204.293327050583,9.85915762894708,30.4166847519242));
#77814=CARTESIAN_POINT('Ctrl Pts',(204.290335680551,9.89367371370784,30.459641081126));
#77815=CARTESIAN_POINT('Ctrl Pts',(204.28734431052,9.93058849989877,30.5006068889149));
#77816=CARTESIAN_POINT('Ctrl Pts',(204.284352940488,9.96963329689886,30.5393154993266));
#77817=CARTESIAN_POINT('Ctrl Pts',(204.281356237518,10.0087477019789,30.5780931184732));
#77818=CARTESIAN_POINT('Ctrl Pts',(204.278359534547,10.0499992970677,30.614605155808));
#77819=CARTESIAN_POINT('Ctrl Pts',(204.275362831577,10.0930854954961,30.6486245389685));
#77820=CARTESIAN_POINT('Ctrl Pts',(204.273836824426,10.1150262241966,30.6659481851407));
#77821=CARTESIAN_POINT('Ctrl Pts',(204.272310817276,10.1374422109402,30.6826261395129));
#77822=CARTESIAN_POINT('Ctrl Pts',(204.270784810126,10.1602908369858,30.6986328760509));
#77823=CARTESIAN_POINT('Ctrl Pts',(204.267772962681,10.2053866781029,30.7302250272062));
#77824=CARTESIAN_POINT('Ctrl Pts',(204.264761115235,10.2523612927625,30.7593341490075));
#77825=CARTESIAN_POINT('Ctrl Pts',(204.26174926779,10.3009107130304,30.7857318611765));
#77826=CARTESIAN_POINT('Ctrl Pts',(204.258742718615,10.3493747279248,30.8120831359946));
#77827=CARTESIAN_POINT('Ctrl Pts',(204.25573616944,10.3994075908154,30.8357322173006));
#77828=CARTESIAN_POINT('Ctrl Pts',(204.252729620265,10.4506764672343,30.8564939757882));
#77829=CARTESIAN_POINT('Ctrl Pts',(204.249726012003,10.5018951940337,30.8772354257699));
#77830=CARTESIAN_POINT('Ctrl Pts',(204.246722403741,10.5543470526839,30.8950949511008));
#77831=CARTESIAN_POINT('Ctrl Pts',(204.243718795479,10.6076763956723,30.9099341968643));
#77832=CARTESIAN_POINT('Ctrl Pts',(204.240716942985,10.6609745648372,30.9247647683033));
#77833=CARTESIAN_POINT('Ctrl Pts',(204.237715090491,10.7151486944926,30.9365784187188));
#77834=CARTESIAN_POINT('Ctrl Pts',(204.234713237996,10.7698272156219,30.945286386614));
#77835=CARTESIAN_POINT('Ctrl Pts',(204.231711958743,10.8244952952208,30.9539926916165));
#77836=CARTESIAN_POINT('Ctrl Pts',(204.228710679489,10.8796670544413,30.9595944092412));
#77837=CARTESIAN_POINT('Ctrl Pts',(204.225709400235,10.934962234592,30.9620541505261));
#77838=CARTESIAN_POINT('Ctrl Pts',(204.222705377653,10.9903079574679,30.964516140145));
#77839=CARTESIAN_POINT('Ctrl Pts',(204.219701355071,11.0457767986833,30.9638303927569));
#77840=CARTESIAN_POINT('Ctrl Pts',(204.216697332489,11.1009864101636,30.960011642064));
#77841=CARTESIAN_POINT('Ctrl Pts',(204.213691925611,11.1562214630015,30.9561911316375));
#77842=CARTESIAN_POINT('Ctrl Pts',(204.210686518734,11.2111965239212,30.9492348063404));
#77843=CARTESIAN_POINT('Ctrl Pts',(204.207681111856,11.2655355774917,30.9392091950395));
#77844=CARTESIAN_POINT('Ctrl Pts',(204.20467013339,11.3199753678007,30.9291649977066));
#77845=CARTESIAN_POINT('Ctrl Pts',(204.201659154923,11.373776282128,30.9160402739218));
#77846=CARTESIAN_POINT('Ctrl Pts',(204.198648176456,11.4265748620129,30.8999521910046));
#77847=CARTESIAN_POINT('Ctrl Pts',(204.196476421435,11.4646573598624,30.8883481974043));
#77848=CARTESIAN_POINT('Ctrl Pts',(204.194304666413,11.50221868849,30.8752036044538));
#77849=CARTESIAN_POINT('Ctrl Pts',(204.192132911392,11.5391293734927,30.8605777334049));
#77850=CARTESIAN_POINT('Ctrl Pts',(204.189121084306,11.5903177440722,30.8402943247595));
#77851=CARTESIAN_POINT('Ctrl Pts',(204.186109257221,11.640465895444,30.8170761320679));
#77852=CARTESIAN_POINT('Ctrl Pts',(204.183097430135,11.6892159062062,30.7910513872935));
#77853=CARTESIAN_POINT('Ctrl Pts',(204.180090900248,11.7378801754961,30.7650724148152));
#77854=CARTESIAN_POINT('Ctrl Pts',(204.177084370361,11.7851507228236,30.7362969329501));
#77855=CARTESIAN_POINT('Ctrl Pts',(204.174077840474,11.8306898690518,30.7049010712314));
#77856=CARTESIAN_POINT('Ctrl Pts',(204.171074250825,11.876184480235,30.6735359131212));
#77857=CARTESIAN_POINT('Ctrl Pts',(204.168070661177,11.9199506126271,30.6395557498172));
#77858=CARTESIAN_POINT('Ctrl Pts',(204.165067071528,11.9616771018297,30.6031814908783));
#77859=CARTESIAN_POINT('Ctrl Pts',(204.162065236937,12.0033792094018,30.5668284861535));
#77860=CARTESIAN_POINT('Ctrl Pts',(204.159063402347,12.0430436394359,30.5280845046444));
#77861=CARTESIAN_POINT('Ctrl Pts',(204.156061567756,12.0803918872799,30.4872110310869));
#77862=CARTESIAN_POINT('Ctrl Pts',(204.15306030566,12.117733012261,30.446345352705));
#77863=CARTESIAN_POINT('Ctrl Pts',(204.150059043563,12.1527584769296,30.4033513780991));
#77864=CARTESIAN_POINT('Ctrl Pts',(204.147057781467,12.1852279000695,30.3585261061242));
#77865=CARTESIAN_POINT('Ctrl Pts',(204.144053774743,12.2177270162089,30.3136598418356));
#77866=CARTESIAN_POINT('Ctrl Pts',(204.141049768019,12.2476651112891,30.266959362668));
#77867=CARTESIAN_POINT('Ctrl Pts',(204.138045761295,12.2748441843811,30.2187520821185));
#77868=CARTESIAN_POINT('Ctrl Pts',(204.135040369574,12.3020357883833,30.1705225756048));
#77869=CARTESIAN_POINT('Ctrl Pts',(204.132034977853,12.3264656018709,30.1207853570473));
#77870=CARTESIAN_POINT('Ctrl Pts',(204.129029586132,12.3479823633306,30.0698910405942));
#77871=CARTESIAN_POINT('Ctrl Pts',(204.126018621485,12.369539023521,30.0189023503374));
#77872=CARTESIAN_POINT('Ctrl Pts',(204.123007656838,12.3881716640522,29.9667527740701));
#77873=CARTESIAN_POINT('Ctrl Pts',(204.119996692191,12.4037782203796,29.9138102922692));
#77874=CARTESIAN_POINT('Ctrl Pts',(204.117824799013,12.4150356668097,29.8756213965095));
#77875=CARTESIAN_POINT('Ctrl Pts',(204.115652905836,12.4247196494047,29.8370202873807));
#77876=CARTESIAN_POINT('Ctrl Pts',(204.113481012658,12.4328084900551,29.7981477499932));
#77877=CARTESIAN_POINT('Ctrl Pts',(204.110469256761,12.4440252542029,29.7442433522497));
#77878=CARTESIAN_POINT('Ctrl Pts',(204.107457500864,12.4522190964014,29.6895933604676));
#77879=CARTESIAN_POINT('Ctrl Pts',(204.104445744967,12.457300215849,29.6345671984045));
#77880=CARTESIAN_POINT('Ctrl Pts',(204.101439288488,12.462372394673,29.5796378591404));
#77881=CARTESIAN_POINT('Ctrl Pts',(204.098432832009,12.4643426724083,29.5243341842346));
#77882=CARTESIAN_POINT('Ctrl Pts',(204.09542637553,12.4631723826498,29.4690350415631));
#77883=CARTESIAN_POINT('Ctrl Pts',(204.092422860591,12.4620032379115,29.4137900039894));
#77884=CARTESIAN_POINT('Ctrl Pts',(204.089419345651,12.4576996241724,29.3585500146394));
#77885=CARTESIAN_POINT('Ctrl Pts',(204.086415830712,12.4502748564698,29.3036964323008));
#77886=CARTESIAN_POINT('Ctrl Pts',(204.083414071992,12.4428544301871,29.2488749240199));
#77887=CARTESIAN_POINT('Ctrl Pts',(204.080412313272,12.43231653811,29.1944398965253));
#77888=CARTESIAN_POINT('Ctrl Pts',(204.077410554552,12.4187263455936,29.1407677543447));
#77889=CARTESIAN_POINT('Ctrl Pts',(204.074409369348,12.405138749622,29.0871058667736));
#77890=CARTESIAN_POINT('Ctrl Pts',(204.071408184144,12.3885001409816,29.0342070859916));
#77891=CARTESIAN_POINT('Ctrl Pts',(204.068406998941,12.3689263142868,28.9824355150775));
#77892=CARTESIAN_POINT('Ctrl Pts',(204.065403070076,12.3493345933454,28.9306166149786));
#77893=CARTESIAN_POINT('Ctrl Pts',(204.062399141211,12.3268024807935,28.8799274776847));
#77894=CARTESIAN_POINT('Ctrl Pts',(204.059395212347,12.3014944833725,28.8307135443244));
#77895=CARTESIAN_POINT('Ctrl Pts',(204.056389899139,12.2761748229078,28.7814769310083));
#77896=CARTESIAN_POINT('Ctrl Pts',(204.053384585931,12.248076995451,28.7337173321117));
#77897=CARTESIAN_POINT('Ctrl Pts',(204.050379272723,12.2174105930739,28.6877539179095));
#77898=CARTESIAN_POINT('Ctrl Pts',(204.04736838669,12.1866873252437,28.6417052726342));
#77899=CARTESIAN_POINT('Ctrl Pts',(204.044357500657,12.1533862863945,28.5974598874003));
#77900=CARTESIAN_POINT('Ctrl Pts',(204.041346614624,12.1177586332827,28.5553053997603));
#77901=CARTESIAN_POINT('Ctrl Pts',(204.03917411439,12.0920515544219,28.5248888933827));
#77902=CARTESIAN_POINT('Ctrl Pts',(204.037001614157,12.0651340326139,28.4955602891252));
#77903=CARTESIAN_POINT('Ctrl Pts',(204.034829113924,12.0371118107902,28.4674152132055));
#77904=CARTESIAN_POINT('Ctrl Pts',(204.031817315547,11.9982638139436,28.4283969002588));
#77905=CARTESIAN_POINT('Ctrl Pts',(204.02880551717,11.9571303355798,28.3914930956449));
#77906=CARTESIAN_POINT('Ctrl Pts',(204.025793718793,11.9139705116544,28.3569819975931));
#77907=CARTESIAN_POINT('Ctrl Pts',(204.022787218906,11.8708866164197,28.3225316130071));
#77908=CARTESIAN_POINT('Ctrl Pts',(204.01978071902,11.8257838590416,28.2904659078781));
#77909=CARTESIAN_POINT('Ctrl Pts',(204.016774219133,11.7789573881038,28.2610255702726));
#77910=CARTESIAN_POINT('Ctrl Pts',(204.013770660253,11.7321767235706,28.2316140316772));
#77911=CARTESIAN_POINT('Ctrl Pts',(204.010767101372,11.6836761302667,28.2048230521918));
#77912=CARTESIAN_POINT('Ctrl Pts',(204.007763542492,11.6337814284563,28.1808512779281));
#77913=CARTESIAN_POINT('Ctrl Pts',(204.00476173938,11.583915893227,28.1568935166692));
#77914=CARTESIAN_POINT('Ctrl Pts',(204.001759936269,11.5326583393508,28.135751921877));
#77915=CARTESIAN_POINT('Ctrl Pts',(203.998758133157,11.4803589690574,28.117579112265));
#77916=CARTESIAN_POINT('Ctrl Pts',(203.995756903193,11.4280695845194,28.0994097724697));
#77917=CARTESIAN_POINT('Ctrl Pts',(203.992755673229,11.3747392765915,28.0842082649166));
#77918=CARTESIAN_POINT('Ctrl Pts',(203.989754443265,11.3207358221199,28.0720781595588));
#77919=CARTESIAN_POINT('Ctrl Pts',(203.986750469429,11.2666829950394,28.0599369642632));
#77920=CARTESIAN_POINT('Ctrl Pts',(203.983746495593,11.2119563076499,28.0508728965026));
#77921=CARTESIAN_POINT('Ctrl Pts',(203.980742521758,11.1569347452221,28.0449385800792));
#77922=CARTESIAN_POINT('Ctrl Pts',(203.977737163395,11.1018878234405,28.0390015285384));
#77923=CARTESIAN_POINT('Ctrl Pts',(203.974731805032,11.0465462832934,28.0361971304803));
#77924=CARTESIAN_POINT('Ctrl Pts',(203.971726446669,10.9912919693594,28.0365259072323));
#77925=CARTESIAN_POINT('Ctrl Pts',(203.968715515739,10.9359352022784,28.0368552936056));
#77926=CARTESIAN_POINT('Ctrl Pts',(203.965704584808,10.8806665119796,28.0403294261408));
#77927=CARTESIAN_POINT('Ctrl Pts',(203.962693653877,10.8258642715793,28.0468967696384));
#77928=CARTESIAN_POINT('Ctrl Pts',(203.960521507648,10.786328831353,28.0516345835379));
#77929=CARTESIAN_POINT('Ctrl Pts',(203.958349361419,10.7470360572612,28.057981147903));
#77930=CARTESIAN_POINT('Ctrl Pts',(203.95617721519,10.7081239039327,28.0659007724204));
#77931=CARTESIAN_POINT('Ctrl Pts',(203.953165422799,10.65417020333,28.0768817388678));
#77932=CARTESIAN_POINT('Ctrl Pts',(203.950153630408,10.6007252515191,28.0909344586892));
#77933=CARTESIAN_POINT('Ctrl Pts',(203.947141838017,10.548163917446,28.107995544367));
#77934=CARTESIAN_POINT('Ctrl Pts',(203.944135344093,10.4956950513916,28.1250266154947));
#77935=CARTESIAN_POINT('Ctrl Pts',(203.941128850168,10.4441072157058,28.145055387586));
#77936=CARTESIAN_POINT('Ctrl Pts',(203.938122356244,10.3937637624352,28.1679677653062));
#77937=CARTESIAN_POINT('Ctrl Pts',(203.935118803306,10.3434695557084,28.1908577298756));
#77938=CARTESIAN_POINT('Ctrl Pts',(203.932115250369,10.2944177976082,28.2166254944475));
#77939=CARTESIAN_POINT('Ctrl Pts',(203.929111697431,10.2469536008031,28.2451082235282));
#77940=CARTESIAN_POINT('Ctrl Pts',(203.926109900231,10.1995171493656,28.2735743029268));
#77941=CARTESIAN_POINT('Ctrl Pts',(203.923108103031,10.1536668710415,28.3047519301131));
#77942=CARTESIAN_POINT('Ctrl Pts',(203.920106305832,10.1097228510496,28.3384325899644));
#77943=CARTESIAN_POINT('Ctrl Pts',(203.917105081738,10.06578722089,28.3721068194735));
#77944=CARTESIAN_POINT('Ctrl Pts',(203.914103857644,10.0237575445048,28.4082828117572));
#77945=CARTESIAN_POINT('Ctrl Pts',(203.91110263355,9.9839226120019,28.4467103951909));
#77946=CARTESIAN_POINT('Ctrl Pts',(203.908098665471,9.94405125887923,28.4851731125213));
#77947=CARTESIAN_POINT('Ctrl Pts',(203.905094697393,9.90637903858919,28.5258911664901));
#77948=CARTESIAN_POINT('Ctrl Pts',(203.902090729314,9.87115835981009,28.5685770019087));
#77949=CARTESIAN_POINT('Ctrl Pts',(203.899085376654,9.83592144720398,28.6112825119756));
#77950=CARTESIAN_POINT('Ctrl Pts',(203.896080023994,9.80313864104508,28.6559571855371));
#77951=CARTESIAN_POINT('Ctrl Pts',(203.893074671334,9.77302041041059,28.702282420445));
#77952=CARTESIAN_POINT('Ctrl Pts',(203.890063745946,9.74284633252009,28.7486935547302));
#77953=CARTESIAN_POINT('Ctrl Pts',(203.887052820559,9.715346961854,28.7967609050465));
#77954=CARTESIAN_POINT('Ctrl Pts',(203.884041895171,9.69068738400953,28.8461401345791));
#77955=CARTESIAN_POINT('Ctrl Pts',(203.881869702266,9.67289705275423,28.8817641365818));
#77956=CARTESIAN_POINT('Ctrl Pts',(203.879697509361,9.65658377891154,28.9180704083684));
#77957=CARTESIAN_POINT('Ctrl Pts',(203.877525316456,9.64179364143364,28.9549240992762));
#77958=CARTESIAN_POINT('Ctrl Pts',(203.874154072383,9.61883934340668,29.0121210391798));
#77959=CARTESIAN_POINT('Ctrl Pts',(203.87078282831,9.59947538062231,29.070836036723));
#77960=CARTESIAN_POINT('Ctrl Pts',(203.867411584237,9.58387900170179,29.1306308510732));
#77961=CARTESIAN_POINT('Ctrl Pts',(203.86403549451,9.56826020534381,29.1905116114317));
#77962=CARTESIAN_POINT('Ctrl Pts',(203.860659404783,9.55642003399269,29.2514750466615));
#77963=CARTESIAN_POINT('Ctrl Pts',(203.857283315056,9.54848858019345,29.3130592388718));
#77964=CARTESIAN_POINT('Ctrl Pts',(203.853907225329,9.54055712639421,29.3746434310822));
#77965=CARTESIAN_POINT('Ctrl Pts',(203.850531135602,9.53653457858967,29.4368481027865));
#77966=CARTESIAN_POINT('Ctrl Pts',(203.847155045875,9.53650022221242,29.4991935164512));
#77967=CARTESIAN_POINT('',(203.34715504581,9.53650055029319,29.501269136656));
#77968=CARTESIAN_POINT('Ctrl Pts',(203.847155045843,9.5365002222121,29.4991935170432));
#77969=CARTESIAN_POINT('Ctrl Pts',(203.844124084037,9.53646937801091,29.5551655387819));
#77970=CARTESIAN_POINT('Ctrl Pts',(203.841093122232,9.539653874786,29.6111435828041));
#77971=CARTESIAN_POINT('Ctrl Pts',(203.838062160426,9.54602940369895,29.6667385830934));
#77972=CARTESIAN_POINT('Ctrl Pts',(203.835030400788,9.55240661082483,29.7223482175014));
#77973=CARTESIAN_POINT('Ctrl Pts',(203.831998641151,9.56197645602609,29.7775740993723));
#77974=CARTESIAN_POINT('Ctrl Pts',(203.828966881513,9.57466299303777,29.8320341346668));
#77975=CARTESIAN_POINT('Ctrl Pts',(203.825930949368,9.58736699009728,29.8865691214489));
#77976=CARTESIAN_POINT('Ctrl Pts',(203.822895017224,9.60319611861329,29.9403356592167));
#77977=CARTESIAN_POINT('Ctrl Pts',(203.819859085079,9.62202399893718,29.9929648978324));
#77978=CARTESIAN_POINT('Ctrl Pts',(203.816820713817,9.64086700588681,30.0456364196357));
#77979=CARTESIAN_POINT('Ctrl Pts',(203.813782342554,9.66271335885688,30.0971683524208));
#77980=CARTESIAN_POINT('Ctrl Pts',(203.810743971292,9.68738900762656,30.147212973217));
#77981=CARTESIAN_POINT('Ctrl Pts',(203.80769969221,9.71211263581529,30.1973549009515));
#77982=CARTESIAN_POINT('Ctrl Pts',(203.804655413128,9.7396762840394,30.2460033012221));
#77983=CARTESIAN_POINT('Ctrl Pts',(203.801611134046,9.76986121827386,30.2928372012547));
#77984=CARTESIAN_POINT('Ctrl Pts',(203.800698561938,9.77890964265523,30.3068764235911));
#77985=CARTESIAN_POINT('Ctrl Pts',(203.799785989829,9.7881933350171,30.3207528145843));
#77986=CARTESIAN_POINT('Ctrl Pts',(203.798873417721,9.79770570570672,30.334458315262));
#77987=CARTESIAN_POINT('Ctrl Pts',(203.795861627085,9.82909968402081,30.3796910133031));
#77988=CARTESIAN_POINT('Ctrl Pts',(203.792849836448,9.86311487818565,30.4232433266164));
#77989=CARTESIAN_POINT('Ctrl Pts',(203.789838045812,9.89954502329002,30.4647958821607));
#77990=CARTESIAN_POINT('Ctrl Pts',(203.786831553754,9.93591107761387,30.5062753351766));
#77991=CARTESIAN_POINT('Ctrl Pts',(203.783825061697,9.97468330624121,30.5457616190503));
#77992=CARTESIAN_POINT('Ctrl Pts',(203.78081856964,10.0156134051945,30.5829659652857));
#77993=CARTESIAN_POINT('Ctrl Pts',(203.777815018637,10.0565034649099,30.6201339169434));
#77994=CARTESIAN_POINT('Ctrl Pts',(203.774811467634,10.0995468246674,30.6550240002376));
#77995=CARTESIAN_POINT('Ctrl Pts',(203.771807916632,10.1444576037548,30.6873834503761));
#77996=CARTESIAN_POINT('Ctrl Pts',(203.768806121431,10.1893421291104,30.7197239839795));
#77997=CARTESIAN_POINT('Ctrl Pts',(203.76580432623,10.2360914828389,30.749536509104));
#77998=CARTESIAN_POINT('Ctrl Pts',(203.762802531029,10.2843876997944,30.7766092925381));
#77999=CARTESIAN_POINT('Ctrl Pts',(203.759801308994,10.3326746950134,30.803676906663));
#78000=CARTESIAN_POINT('Ctrl Pts',(203.756800086959,10.382507506974,30.8280055604714));
#78001=CARTESIAN_POINT('Ctrl Pts',(203.753798864924,10.4335422572665,30.8494287219773));
#78002=CARTESIAN_POINT('Ctrl Pts',(203.750794898982,10.4846236667601,30.8708714698944));
#78003=CARTESIAN_POINT('Ctrl Pts',(203.74779093304,10.5369087224968,30.8894032143634));
#78004=CARTESIAN_POINT('Ctrl Pts',(203.744786967098,10.5900335670003,30.9049056102862));
#78005=CARTESIAN_POINT('Ctrl Pts',(203.741781616621,10.6431828968728,30.9204151513006));
#78006=CARTESIAN_POINT('Ctrl Pts',(203.738776266144,10.6971722723627,30.9328924416287));
#78007=CARTESIAN_POINT('Ctrl Pts',(203.735770915667,10.7516258733907,30.9422699273129));
#78008=CARTESIAN_POINT('Ctrl Pts',(203.732759992511,10.8061804451494,30.9516648012241));
#78009=CARTESIAN_POINT('Ctrl Pts',(203.729749069355,10.8612004367267,30.9579483293454));
#78010=CARTESIAN_POINT('Ctrl Pts',(203.726738146199,10.916304305951,30.9611048151305));
#78011=CARTESIAN_POINT('Ctrl Pts',(203.724565937128,10.9560586000169,30.9633820393234));
#78012=CARTESIAN_POINT('Ctrl Pts',(203.722393728058,10.9958564520451,30.9640328028313));
#78013=CARTESIAN_POINT('Ctrl Pts',(203.720221518987,11.0355557713552,30.9630680220425));
#78014=CARTESIAN_POINT('Ctrl Pts',(203.717209729415,11.0905992740848,30.9617303438429));
#78015=CARTESIAN_POINT('Ctrl Pts',(203.714197939843,11.1456812449634,30.9572793119509));
#78016=CARTESIAN_POINT('Ctrl Pts',(203.711186150272,11.2004215096717,30.9497115121502));
#78017=CARTESIAN_POINT('Ctrl Pts',(203.708179659287,11.2550654708113,30.9421570262444));
#78018=CARTESIAN_POINT('Ctrl Pts',(203.705173168303,11.3093684005256,30.9314967261666));
#78019=CARTESIAN_POINT('Ctrl Pts',(203.702166677319,11.3629525595331,30.9177791398975));
#78020=CARTESIAN_POINT('Ctrl Pts',(203.699163127393,11.416484300571,30.9040749726691));
#78021=CARTESIAN_POINT('Ctrl Pts',(203.696159577467,11.4692981553777,30.8873195743526));
#78022=CARTESIAN_POINT('Ctrl Pts',(203.693156027541,11.5210257832318,30.8676126583239));
#78023=CARTESIAN_POINT('Ctrl Pts',(203.69015423342,11.5727231723453,30.8479172624894));
#78024=CARTESIAN_POINT('Ctrl Pts',(203.687152439298,11.6233351012891,30.8252739564425));
#78025=CARTESIAN_POINT('Ctrl Pts',(203.684150645176,11.6725098478943,30.7998318177692));
#78026=CARTESIAN_POINT('Ctrl Pts',(203.68114942422,11.7216752050103,30.7743945370505));
#78027=CARTESIAN_POINT('Ctrl Pts',(203.678148203265,11.7694034567133,30.7461597274536));
#78028=CARTESIAN_POINT('Ctrl Pts',(203.67514698231,11.8153663760569,30.7153229705703));
#78029=CARTESIAN_POINT('Ctrl Pts',(203.672143017438,11.8613713177592,30.6844580206723));
#78030=CARTESIAN_POINT('Ctrl Pts',(203.669139052567,11.9056072640122,30.6509866657256));
#78031=CARTESIAN_POINT('Ctrl Pts',(203.666135087696,11.947775240633,30.6151476777732));
#78032=CARTESIAN_POINT('Ctrl Pts',(203.663129738286,11.989962652628,30.5792921715007));
#78033=CARTESIAN_POINT('Ctrl Pts',(203.660124388876,12.0300798126047,30.5410672213843));
#78034=CARTESIAN_POINT('Ctrl Pts',(203.657119039466,12.0678635835183,30.5007495276019));
#78035=CARTESIAN_POINT('Ctrl Pts',(203.654108117359,12.105717415344,30.4603570743573));
#78036=CARTESIAN_POINT('Ctrl Pts',(203.651097195252,12.1412288766431,30.4178645318039));
#78037=CARTESIAN_POINT('Ctrl Pts',(203.648086273145,12.1741749905951,30.3735819031213));
#78038=CARTESIAN_POINT('Ctrl Pts',(203.645914055515,12.1979438318497,30.3416343789602));
#78039=CARTESIAN_POINT('Ctrl Pts',(203.643741837884,12.2203783159573,30.3087558315153));
#78040=CARTESIAN_POINT('Ctrl Pts',(203.641569620253,12.2414094013503,30.2750709311018));
#78041=CARTESIAN_POINT('Ctrl Pts',(203.638557831265,12.2705690907379,30.2283666733448));
#78042=CARTESIAN_POINT('Ctrl Pts',(203.635546042277,12.2971498863831,30.1799177811609));
#78043=CARTESIAN_POINT('Ctrl Pts',(203.632534253288,12.3209398209639,30.1300398712716));
#78044=CARTESIAN_POINT('Ctrl Pts',(203.62952776291,12.3446879021526,30.0802497110863));
#78045=CARTESIAN_POINT('Ctrl Pts',(203.626521272532,12.3656546412535,30.0290359948511));
#78046=CARTESIAN_POINT('Ctrl Pts',(203.623514782154,12.3836727888111,29.9767408766863));
#78047=CARTESIAN_POINT('Ctrl Pts',(203.620511232848,12.4016733102795,29.924496915746));
#78048=CARTESIAN_POINT('Ctrl Pts',(203.617507683542,12.4167307835348,29.8711741448606));
#78049=CARTESIAN_POINT('Ctrl Pts',(203.614504134235,12.4287258752695,29.8171350238235));
#78050=CARTESIAN_POINT('Ctrl Pts',(203.611502340745,12.4407139549089,29.7631274929957));
#78051=CARTESIAN_POINT('Ctrl Pts',(203.608500547255,12.4496430875533,29.7084049559746));
#78052=CARTESIAN_POINT('Ctrl Pts',(203.605498753764,12.4554443064973,29.6533431468458));
#78053=CARTESIAN_POINT('Ctrl Pts',(203.602497533452,12.4612444177277,29.598291851493));
#78054=CARTESIAN_POINT('Ctrl Pts',(203.599496313139,12.4639177463926,29.5429019369228));
#78055=CARTESIAN_POINT('Ctrl Pts',(203.596495092826,12.4634470862822,29.4875550953341));
#78056=CARTESIAN_POINT('Ctrl Pts',(203.593491128609,12.4629759958648,29.4321576521885));
#78057=CARTESIAN_POINT('Ctrl Pts',(203.590487164392,12.4593551789945,29.3768038891747));
#78058=CARTESIAN_POINT('Ctrl Pts',(203.587483200175,12.4526195896628,29.3218748256762));
#78059=CARTESIAN_POINT('Ctrl Pts',(203.584477851427,12.4458808958898,29.2669204453052));
#78060=CARTESIAN_POINT('Ctrl Pts',(203.58147250268,12.4360246619534,29.2123916744794));
#78061=CARTESIAN_POINT('Ctrl Pts',(203.578467153932,12.4231372290841,29.1586604664052));
#78062=CARTESIAN_POINT('Ctrl Pts',(203.575456232491,12.4102258995844,29.1048296267877));
#78063=CARTESIAN_POINT('Ctrl Pts',(203.57244531105,12.3942722963167,29.0517998101152));
#78064=CARTESIAN_POINT('Ctrl Pts',(203.56943438961,12.3754126630898,28.999927749008));
#78065=CARTESIAN_POINT('Ctrl Pts',(203.567262166913,12.3618064218923,28.9625047638233));
#78066=CARTESIAN_POINT('Ctrl Pts',(203.565089944216,12.3466886812148,28.9256840308773));
#78067=CARTESIAN_POINT('Ctrl Pts',(203.562917721519,12.3301255809467,28.8895917850231));
#78068=CARTESIAN_POINT('Ctrl Pts',(203.559905931974,12.3071608212593,28.8395498400247));
#78069=CARTESIAN_POINT('Ctrl Pts',(203.556894142429,12.2813205365589,28.7907019662624));
#78070=CARTESIAN_POINT('Ctrl Pts',(203.553882352884,12.2527517147781,28.7433987899029));
#78071=CARTESIAN_POINT('Ctrl Pts',(203.550875861935,12.2242331536969,28.6961788333118));
#78072=CARTESIAN_POINT('Ctrl Pts',(203.547869370986,12.1929958526426,28.6504986287517));
#78073=CARTESIAN_POINT('Ctrl Pts',(203.544862880037,12.1592335589007,28.6066860541118));
#78074=CARTESIAN_POINT('Ctrl Pts',(203.541859330152,12.1255042927199,28.5629163386004));
#78075=CARTESIAN_POINT('Ctrl Pts',(203.538855780267,12.0892552476063,28.5210110493451));
#78076=CARTESIAN_POINT('Ctrl Pts',(203.535852230382,12.0507234851196,28.481269217203));
#78077=CARTESIAN_POINT('Ctrl Pts',(203.532850436306,12.0122142474516,28.4415506172598));
#78078=CARTESIAN_POINT('Ctrl Pts',(203.52984864223,11.9714253039502,28.4039933454117));
#78079=CARTESIAN_POINT('Ctrl Pts',(203.526846848154,11.9286325062115,28.3688616714091));
#78080=CARTESIAN_POINT('Ctrl Pts',(203.52384562725,11.8858478794577,28.3337367055535));
#78081=CARTESIAN_POINT('Ctrl Pts',(203.520844406346,11.8410605658907,28.301036752032));
#78082=CARTESIAN_POINT('Ctrl Pts',(203.517843185441,11.7945798638993,28.2709861311256));
#78083=CARTESIAN_POINT('Ctrl Pts',(203.514839220628,11.7480566662743,28.2409080360176));
#78084=CARTESIAN_POINT('Ctrl Pts',(203.511835255816,11.6998374312439,28.2134843992042));
#78085=CARTESIAN_POINT('Ctrl Pts',(203.508831291003,11.6502595861629,28.1888956103333));
#78086=CARTESIAN_POINT('Ctrl Pts',(203.505825941656,11.6006588905431,28.1642954884351));
#78087=CARTESIAN_POINT('Ctrl Pts',(203.502820592309,11.5496988224808,28.1425330264411));
#78088=CARTESIAN_POINT('Ctrl Pts',(203.499815242963,11.4977375035818,28.123740712101));
#78089=CARTESIAN_POINT('Ctrl Pts',(203.496804320925,11.4456798350258,28.1049135519742));
#78090=CARTESIAN_POINT('Ctrl Pts',(203.493793398887,11.3926177136023,28.0890676917142));
#78091=CARTESIAN_POINT('Ctrl Pts',(203.490782476849,11.3389239987965,28.0762855718088));
#78092=CARTESIAN_POINT('Ctrl Pts',(203.488610258828,11.3001868765889,28.0670639609994));
#78093=CARTESIAN_POINT('Ctrl Pts',(203.486438040806,11.2611213103833,28.0594359122335));
#78094=CARTESIAN_POINT('Ctrl Pts',(203.484265822785,11.2218691021544,28.0534156258589));
#78095=CARTESIAN_POINT('Ctrl Pts',(203.4812540334,11.1674457510307,28.0450684735836));
#78096=CARTESIAN_POINT('Ctrl Pts',(203.478242244014,11.1124379139738,28.0397795600519));
#78097=CARTESIAN_POINT('Ctrl Pts',(203.475230454629,11.0572192604575,28.037618994163));
#78098=CARTESIAN_POINT('Ctrl Pts',(203.472223963842,11.0020977523338,28.0354622293271));
#78099=CARTESIAN_POINT('Ctrl Pts',(203.469217473055,10.9467666866493,28.0364229100576));
#78100=CARTESIAN_POINT('Ctrl Pts',(203.466210982268,10.891606455227,28.0405195823679));
#78101=CARTESIAN_POINT('Ctrl Pts',(203.463207432546,10.8365001836672,28.0446122471556));
#78102=CARTESIAN_POINT('Ctrl Pts',(203.460203882824,10.7815649387342,28.0518347871742));
#78103=CARTESIAN_POINT('Ctrl Pts',(203.457200333102,10.727180846372,28.0621537080015));
#78104=CARTESIAN_POINT('Ctrl Pts',(203.454198539189,10.6728285457684,28.072466596612));
#78105=CARTESIAN_POINT('Ctrl Pts',(203.451196745277,10.6190272762346,28.0858721799307));
#78106=CARTESIAN_POINT('Ctrl Pts',(203.448194951365,10.566149470245,28.1022854483725));
#78107=CARTESIAN_POINT('Ctrl Pts',(203.445193730625,10.5132817609122,28.1186955828125));
#78108=CARTESIAN_POINT('Ctrl Pts',(203.442192509885,10.4613376682902,28.1381121053616));
#78109=CARTESIAN_POINT('Ctrl Pts',(203.439191289145,10.4106746593596,28.1604000997017));
#78110=CARTESIAN_POINT('Ctrl Pts',(203.436187324496,10.3599653310518,28.182708471158));
#78111=CARTESIAN_POINT('Ctrl Pts',(203.433183359847,10.3105399099647,28.2078933460434));
#78112=CARTESIAN_POINT('Ctrl Pts',(203.430179395199,10.2627346477106,28.235772152532));
#78113=CARTESIAN_POINT('Ctrl Pts',(203.427174046016,10.2149073519034,28.2636638084253));
#78114=CARTESIAN_POINT('Ctrl Pts',(203.424168696833,10.1687021439269,28.2942515793454));
#78115=CARTESIAN_POINT('Ctrl Pts',(203.42116334765,10.1244266540162,28.3273092625066));
#78116=CARTESIAN_POINT('Ctrl Pts',(203.418152425774,10.0800690659184,28.3604282431456));
#78117=CARTESIAN_POINT('Ctrl Pts',(203.415141503898,10.0376487481492,28.3960259444461));
#78118=CARTESIAN_POINT('Ctrl Pts',(203.412130582022,9.99743964159003,28.4338363269437));
#78119=CARTESIAN_POINT('Ctrl Pts',(203.409958362698,9.9684309187308,28.4611144985057));
#78120=CARTESIAN_POINT('Ctrl Pts',(203.407786143375,9.94057236701064,28.4895435080927));
#78121=CARTESIAN_POINT('Ctrl Pts',(203.405613924051,9.91395384429548,28.5190127433654));
#78122=CARTESIAN_POINT('Ctrl Pts',(203.402635280967,9.87745335019704,28.55942226044));
#78123=CARTESIAN_POINT('Ctrl Pts',(203.399656637882,9.84312724817234,28.6019649688394));
#78124=CARTESIAN_POINT('Ctrl Pts',(203.396677994798,9.81123727986223,28.6463751144615));
#78125=CARTESIAN_POINT('Ctrl Pts',(203.393703653128,9.77939336338157,28.6907211280521));
#78126=CARTESIAN_POINT('Ctrl Pts',(203.390729311457,9.74997892838024,28.7369288058932));
#78127=CARTESIAN_POINT('Ctrl Pts',(203.387754969787,9.72321694902763,28.7846977626557));
#78128=CARTESIAN_POINT('Ctrl Pts',(203.384783688017,9.696482501479,28.8324175763585));
#78129=CARTESIAN_POINT('Ctrl Pts',(203.381812406248,9.67239536693559,28.8816950185289));
#78130=CARTESIAN_POINT('Ctrl Pts',(203.378841124478,9.65113506054209,28.9322010698309));
#78131=CARTESIAN_POINT('Ctrl Pts',(203.375870863786,9.62988206023233,28.9826897647771));
#78132=CARTESIAN_POINT('Ctrl Pts',(203.372900603095,9.61145418500448,29.0344057406854));
#78133=CARTESIAN_POINT('Ctrl Pts',(203.369930342403,9.59598385182221,29.0869976929168));
#78134=CARTESIAN_POINT('Ctrl Pts',(203.366960732882,9.58051691020423,29.1395781154039));
#78135=CARTESIAN_POINT('Ctrl Pts',(203.363991123361,9.56800636994545,29.1930336130972));
#78136=CARTESIAN_POINT('Ctrl Pts',(203.361021513841,9.55853468839566,29.2469980129695));
#78137=CARTESIAN_POINT('Ctrl Pts',(203.358049734099,9.54905608484591,29.3010018505669));
#78138=CARTESIAN_POINT('Ctrl Pts',(203.355077954358,9.54262085849238,29.3555147988211));
#78139=CARTESIAN_POINT('Ctrl Pts',(203.352106174617,9.53925994647032,29.4101626691508));
#78140=CARTESIAN_POINT('Ctrl Pts',(203.350455798359,9.53739346581252,29.4405113341236));
#78141=CARTESIAN_POINT('Ctrl Pts',(203.348805422101,9.53647421572529,29.4709015287949));
#78142=CARTESIAN_POINT('Ctrl Pts',(203.347155045843,9.53650055029265,29.5012691360414));
#78143=CARTESIAN_POINT('',(202.847155045809,9.53650021423239,29.4992081299609));
#78144=CARTESIAN_POINT('Ctrl Pts',(203.34715504581,9.53650055029319,29.501269136656));
#78145=CARTESIAN_POINT('Ctrl Pts',(203.343320363599,9.53656173921627,29.5718288788583));
#78146=CARTESIAN_POINT('Ctrl Pts',(203.339485681388,9.54172964003464,29.6421676990623));
#78147=CARTESIAN_POINT('Ctrl Pts',(203.335650999177,9.5518861311701,29.7116564974257));
#78148=CARTESIAN_POINT('Ctrl Pts',(203.332754674557,9.55955730017702,29.7641411901432));
#78149=CARTESIAN_POINT('Ctrl Pts',(203.329858349937,9.5700733053784,29.816141555552));
#78150=CARTESIAN_POINT('Ctrl Pts',(203.326962025317,9.58336551666075,29.8673948701522));
#78151=CARTESIAN_POINT('Ctrl Pts',(203.323950235916,9.59718763479828,29.9206914476964));
#78152=CARTESIAN_POINT('Ctrl Pts',(203.320938446514,9.61405025587103,29.9733173613119));
#78153=CARTESIAN_POINT('Ctrl Pts',(203.317926657113,9.63387023503536,30.0249016243809));
#78154=CARTESIAN_POINT('Ctrl Pts',(203.31492016631,9.65365534518888,30.0763951359807));
#78155=CARTESIAN_POINT('Ctrl Pts',(203.311913675507,9.67638730023825,30.1268501454996));
#78156=CARTESIAN_POINT('Ctrl Pts',(203.308907184704,9.70193292836923,30.1759098516429));
#78157=CARTESIAN_POINT('Ctrl Pts',(203.305903634967,9.72745356678049,30.2249215656875));
#78158=CARTESIAN_POINT('Ctrl Pts',(203.30290008523,9.75578218303147,30.2725402148732));
#78159=CARTESIAN_POINT('Ctrl Pts',(203.299896535492,9.7867378991367,30.3184297921073));
#78160=CARTESIAN_POINT('Ctrl Pts',(203.296894741565,9.81767551919959,30.3642925432867));
#78161=CARTESIAN_POINT('Ctrl Pts',(203.293892947638,9.85123690055986,30.4084277897234));
#78162=CARTESIAN_POINT('Ctrl Pts',(203.290891153711,9.88719687468086,30.4505269350628));
#78163=CARTESIAN_POINT('Ctrl Pts',(203.287889932956,9.92314998248528,30.492618041852));
#78164=CARTESIAN_POINT('Ctrl Pts',(203.284888712202,9.96150043095983,30.5326734189955));
#78165=CARTESIAN_POINT('Ctrl Pts',(203.281887491447,10.0019831103363,30.5704179267678));
#78166=CARTESIAN_POINT('Ctrl Pts',(203.278883526784,10.042502801569,30.6081969429847));
#78167=CARTESIAN_POINT('Ctrl Pts',(203.275879562121,10.0851582314585,30.6436605088547));
#78168=CARTESIAN_POINT('Ctrl Pts',(203.272875597459,10.1296488852503,30.6765717942625));
#78169=CARTESIAN_POINT('Ctrl Pts',(203.269870248262,10.1741600448792,30.7094982485517));
#78170=CARTESIAN_POINT('Ctrl Pts',(203.266864899066,10.2205076726589,30.7398697879506));
#78171=CARTESIAN_POINT('Ctrl Pts',(203.263859549869,10.26836247084,30.7674931068549));
#78172=CARTESIAN_POINT('Ctrl Pts',(203.26084862798,10.3163060041569,30.7951676465155));
#78173=CARTESIAN_POINT('Ctrl Pts',(203.257837706092,10.3657618181764,30.8200835488812));
#78174=CARTESIAN_POINT('Ctrl Pts',(203.254826784203,10.4163773193395,30.8420941906657));
#78175=CARTESIAN_POINT('Ctrl Pts',(203.252654564996,10.452893697996,30.8579736922296));
#78176=CARTESIAN_POINT('Ctrl Pts',(203.250482345789,10.4900132031085,30.8723420486208));
#78177=CARTESIAN_POINT('Ctrl Pts',(203.248310126582,10.5275987282865,30.8851603836681));
#78178=CARTESIAN_POINT('Ctrl Pts',(203.245298337202,10.5797111878374,30.9029330491689));
#78179=CARTESIAN_POINT('Ctrl Pts',(203.242286547822,10.6329359929293,30.9177975992496));
#78180=CARTESIAN_POINT('Ctrl Pts',(203.239274758443,10.686917587499,30.929619408438));
#78181=CARTESIAN_POINT('Ctrl Pts',(203.236268267662,10.7408042130008,30.941420419682));
#78182=CARTESIAN_POINT('Ctrl Pts',(203.233261776882,10.7954444745455,30.9501892017407));
#78183=CARTESIAN_POINT('Ctrl Pts',(203.230255286101,10.8504671451835,30.955840710837));
#78184=CARTESIAN_POINT('Ctrl Pts',(203.227251736387,10.9054359905166,30.9614866914085));
#78185=CARTESIAN_POINT('Ctrl Pts',(203.224248186672,10.9607859817116,30.9640213865873));
#78186=CARTESIAN_POINT('Ctrl Pts',(203.221244636957,11.0161370167667,30.9634110313544));
#78187=CARTESIAN_POINT('Ctrl Pts',(203.218242843052,11.0714556948001,30.9628010329221));
#78188=CARTESIAN_POINT('Ctrl Pts',(203.215241049148,11.1267748891342,30.959049634255));
#78189=CARTESIAN_POINT('Ctrl Pts',(203.212239255243,11.1817130271537,30.9521751360503));
#78190=CARTESIAN_POINT('Ctrl Pts',(203.209238034512,11.2366406751008,30.9453019504853));
#78191=CARTESIAN_POINT('Ctrl Pts',(203.20623681378,11.2911868882277,30.9353069153594));
#78192=CARTESIAN_POINT('Ctrl Pts',(203.203235593048,11.3449760647653,30.9222600903981));
#78193=CARTESIAN_POINT('Ctrl Pts',(203.200231628408,11.3988144188107,30.9092013371943));
#78194=CARTESIAN_POINT('Ctrl Pts',(203.197227663768,11.4518938400073,30.8930853449459));
#78195=CARTESIAN_POINT('Ctrl Pts',(203.194223699128,11.503851245476,30.8740328134482));
#78196=CARTESIAN_POINT('Ctrl Pts',(203.191218349954,11.5558325982232,30.8549715005982));
#78197=CARTESIAN_POINT('Ctrl Pts',(203.188213000781,11.6066904195552,30.8329711603155));
#78198=CARTESIAN_POINT('Ctrl Pts',(203.185207651607,11.6560821430479,30.808200470713));
#78199=CARTESIAN_POINT('Ctrl Pts',(203.182196729741,11.7055654515367,30.7833838498623));
#78200=CARTESIAN_POINT('Ctrl Pts',(203.179185807875,11.7535767737399,30.7557868821362));
#78201=CARTESIAN_POINT('Ctrl Pts',(203.176174886008,11.7997997151085,30.725623378413));
#78202=CARTESIAN_POINT('Ctrl Pts',(203.174002666622,11.8331470996684,30.7038620207721));
#78203=CARTESIAN_POINT('Ctrl Pts',(203.171830447235,11.8655642329307,30.6807657643867));
#78204=CARTESIAN_POINT('Ctrl Pts',(203.169658227848,11.8969432324656,30.6564277269826));
#78205=CARTESIAN_POINT('Ctrl Pts',(203.166646438471,11.9404503192905,30.6226829574814));
#78206=CARTESIAN_POINT('Ctrl Pts',(203.163634649094,11.9821406007112,30.5864096180324));
#78207=CARTESIAN_POINT('Ctrl Pts',(203.160622859717,12.0217060723746,30.5478305930221));
#78208=CARTESIAN_POINT('Ctrl Pts',(203.157616368939,12.0612019370519,30.5093194395558));
#78209=CARTESIAN_POINT('Ctrl Pts',(203.154609878161,12.0985800360574,30.4685110160496));
#78210=CARTESIAN_POINT('Ctrl Pts',(203.151603387384,12.1335651523796,30.4256685666644));
#78211=CARTESIAN_POINT('Ctrl Pts',(203.148599837672,12.1685160449063,30.3828680274221));
#78212=CARTESIAN_POINT('Ctrl Pts',(203.14559628796,12.2010782603043,30.3380378107425));
#78213=CARTESIAN_POINT('Ctrl Pts',(203.142592738248,12.2310145242394,30.2914767786307));
#78214=CARTESIAN_POINT('Ctrl Pts',(203.139590944346,12.2609332880791,30.2449429650959));
#78215=CARTESIAN_POINT('Ctrl Pts',(203.136589150444,12.2882288586422,30.1966807844995));
#78216=CARTESIAN_POINT('Ctrl Pts',(203.133587356543,12.312706634316,30.1470189658912));
#78217=CARTESIAN_POINT('Ctrl Pts',(203.130586135814,12.3371797361203,30.0973666298786));
#78218=CARTESIAN_POINT('Ctrl Pts',(203.127584915085,12.3588358787303,30.0463156595086));
#78219=CARTESIAN_POINT('Ctrl Pts',(203.124583694356,12.3775269703258,29.9942182675954));
#78220=CARTESIAN_POINT('Ctrl Pts',(203.121579729719,12.3962351505128,29.9420732449142));
#78221=CARTESIAN_POINT('Ctrl Pts',(203.118575765082,12.411972685845,29.8888803869602));
#78222=CARTESIAN_POINT('Ctrl Pts',(203.115571800446,12.4246406615891,29.8350093063586));
#78223=CARTESIAN_POINT('Ctrl Pts',(203.112566451275,12.4373144760299,29.7811133964629));
#78224=CARTESIAN_POINT('Ctrl Pts',(203.109561102105,12.4469158192182,29.7265391610833));
#78225=CARTESIAN_POINT('Ctrl Pts',(203.106555752934,12.4533971296812,29.6716654695462));
#78226=CARTESIAN_POINT('Ctrl Pts',(203.103544831071,12.4598904581654,29.6166900280316));
#78227=CARTESIAN_POINT('Ctrl Pts',(203.100533909208,12.4632521657108,29.5614145487942));
#78228=CARTESIAN_POINT('Ctrl Pts',(203.097522987345,12.4634867784783,29.5062208696472));
#78229=CARTESIAN_POINT('Ctrl Pts',(203.095350767935,12.4636560390672,29.4664015762093));
#78230=CARTESIAN_POINT('Ctrl Pts',(203.093178548524,12.4621987984612,29.4266248987027));
#78231=CARTESIAN_POINT('Ctrl Pts',(203.091006329114,12.4591334810299,29.3870321526377));
#78232=CARTESIAN_POINT('Ctrl Pts',(203.08799453973,12.4548834082921,29.3321366795165));
#78233=CARTESIAN_POINT('Ctrl Pts',(203.084982750347,12.4475223123273,29.277367628034));
#78234=CARTESIAN_POINT('Ctrl Pts',(203.081970960963,12.4370669119073,29.2231048200106));
#78235=CARTESIAN_POINT('Ctrl Pts',(203.078964470179,12.4266299055276,29.16893747579));
#78236=CARTESIAN_POINT('Ctrl Pts',(203.075957979395,12.4131094973649,29.1152751212828));
#78237=CARTESIAN_POINT('Ctrl Pts',(203.07295148861,12.3965741466135,29.0624923966251));
#78238=CARTESIAN_POINT('Ctrl Pts',(203.069947938892,12.3800549713818,29.0097613060705));
#78239=CARTESIAN_POINT('Ctrl Pts',(203.066944389173,12.3605268533572,28.9579086415404));
#78240=CARTESIAN_POINT('Ctrl Pts',(203.063940839454,12.3381088677356,28.9072969477998));
#78241=CARTESIAN_POINT('Ctrl Pts',(203.060939045546,12.315703987185,28.8567148405642));
#78242=CARTESIAN_POINT('Ctrl Pts',(203.057937251637,12.2904128008927,28.8073727474071));
#78243=CARTESIAN_POINT('Ctrl Pts',(203.054935457729,12.2624027991648,28.7596140042783));
#78244=CARTESIAN_POINT('Ctrl Pts',(203.051934236993,12.2343981457608,28.7118643803643));
#78245=CARTESIAN_POINT('Ctrl Pts',(203.048933016258,12.2036759747793,28.6656979606276));
#78246=CARTESIAN_POINT('Ctrl Pts',(203.045931795522,12.1704489713604,28.6214321566086));
#78247=CARTESIAN_POINT('Ctrl Pts',(203.042927830878,12.137191589689,28.5771258819592));
#78248=CARTESIAN_POINT('Ctrl Pts',(203.039923866234,12.1014251180251,28.5347241169849));
#78249=CARTESIAN_POINT('Ctrl Pts',(203.03691990159,12.0634038226036,28.4945127747843));
#78250=CARTESIAN_POINT('Ctrl Pts',(203.033914552413,12.0253650030869,28.4542828990912));
#78251=CARTESIAN_POINT('Ctrl Pts',(203.030909203236,11.9850696723617,28.4162458212242));
#78252=CARTESIAN_POINT('Ctrl Pts',(203.027903854058,11.9428080742143,28.3806496593129));
#78253=CARTESIAN_POINT('Ctrl Pts',(203.024892932188,11.9004681121639,28.3449874929365));
#78254=CARTESIAN_POINT('Ctrl Pts',(203.021882010318,11.8561550228794,28.3117756002876));
#78255=CARTESIAN_POINT('Ctrl Pts',(203.018871088448,11.8101901801663,28.2812202323791));
#78256=CARTESIAN_POINT('Ctrl Pts',(203.016698869092,11.7770290005155,28.2591761659861));
#78257=CARTESIAN_POINT('Ctrl Pts',(203.014526649736,11.74300874927,28.2385138803217));
#78258=CARTESIAN_POINT('Ctrl Pts',(203.01235443038,11.7082575776036,28.2192957196265));
#78259=CARTESIAN_POINT('Ctrl Pts',(203.009342640999,11.6600749622084,28.1926496757384));
#78260=CARTESIAN_POINT('Ctrl Pts',(203.006330851619,11.610286698379,28.1686712789441));
#78261=CARTESIAN_POINT('Ctrl Pts',(203.003319062238,11.5592191828815,28.1475554889396));
#78262=CARTESIAN_POINT('Ctrl Pts',(203.000312571457,11.508241509754,28.1264768476509));
#78263=CARTESIAN_POINT('Ctrl Pts',(202.997306080675,11.4559895349629,28.1082510183782));
#78264=CARTESIAN_POINT('Ctrl Pts',(202.994299589894,11.4028137878574,28.0930269006438));
#78265=CARTESIAN_POINT('Ctrl Pts',(202.991296040178,11.3496900593253,28.0778176757305));
#78266=CARTESIAN_POINT('Ctrl Pts',(202.988292490462,11.2956448533326,28.0656044895793));
#78267=CARTESIAN_POINT('Ctrl Pts',(202.985288940746,11.2410464394942,28.056487317684));
#78268=CARTESIAN_POINT('Ctrl Pts',(202.98228714684,11.1864799427118,28.0473754754908));
#78269=CARTESIAN_POINT('Ctrl Pts',(202.979285352935,11.131361398314,28.0413561467001));
#78270=CARTESIAN_POINT('Ctrl Pts',(202.97628355903,11.0760696649248,28.0384783080371));
#78271=CARTESIAN_POINT('Ctrl Pts',(202.973282338297,11.0207884891253,28.0356010188782));
#78272=CARTESIAN_POINT('Ctrl Pts',(202.970281117564,10.9653347164202,28.0358640557412));
#78273=CARTESIAN_POINT('Ctrl Pts',(202.967279896831,10.9100904147275,28.039264392001));
#78274=CARTESIAN_POINT('Ctrl Pts',(202.96427593219,10.8547956051594,28.0426678370658));
#78275=CARTESIAN_POINT('Ctrl Pts',(202.961271967549,10.7997111766841,28.0492142790211));
#78276=CARTESIAN_POINT('Ctrl Pts',(202.958268002909,10.7452157637248,28.058848639821));
#78277=CARTESIAN_POINT('Ctrl Pts',(202.955262653734,10.6906952337147,28.0684874411182));
#78278=CARTESIAN_POINT('Ctrl Pts',(202.95225730456,10.6367647745112,28.081216876905));
#78279=CARTESIAN_POINT('Ctrl Pts',(202.949251955385,10.5837912463799,28.0969310339794));
#78280=CARTESIAN_POINT('Ctrl Pts',(202.946241033518,10.5307194916642,28.1126743291542));
#78281=CARTESIAN_POINT('Ctrl Pts',(202.943230111651,10.4786087097176,28.131413221719));
#78282=CARTESIAN_POINT('Ctrl Pts',(202.940219189784,10.4278079194782,28.1529927717387));
#78283=CARTESIAN_POINT('Ctrl Pts',(202.938046970405,10.3911578614815,28.1685612649854));
#78284=CARTESIAN_POINT('Ctrl Pts',(202.935874751025,10.3551892352,28.1856072469522));
#78285=CARTESIAN_POINT('Ctrl Pts',(202.933702531646,10.320024596085,28.2040579873811));
#78286=CARTESIAN_POINT('Ctrl Pts',(202.930690742265,10.2712687072164,28.2296400002365));
#78287=CARTESIAN_POINT('Ctrl Pts',(202.927678952884,10.2238574588484,28.2580302847729));
#78288=CARTESIAN_POINT('Ctrl Pts',(202.924667163504,10.1781332030965,28.2890634954104));
#78289=CARTESIAN_POINT('Ctrl Pts',(202.921660672722,10.1324893893924,28.3200421097517));
#78290=CARTESIAN_POINT('Ctrl Pts',(202.918654181941,10.0885271111596,28.3536541286549));
#78291=CARTESIAN_POINT('Ctrl Pts',(202.915647691159,10.0465635284795,28.3896887171723));
#78292=CARTESIAN_POINT('Ctrl Pts',(202.912644141443,10.0046409961999,28.4256880552607));
#78293=CARTESIAN_POINT('Ctrl Pts',(202.909640591727,9.96471368425869,28.464104926136));
#78294=CARTESIAN_POINT('Ctrl Pts',(202.906637042011,9.92706765290005,28.5046867686268));
#78295=CARTESIAN_POINT('Ctrl Pts',(202.903635248106,9.88944362860013,28.545244887847));
#78296=CARTESIAN_POINT('Ctrl Pts',(202.900633454201,9.85409859940335,28.5879650840855));
#78297=CARTESIAN_POINT('Ctrl Pts',(202.897631660295,9.82128185947103,28.6325579009594));
#78298=CARTESIAN_POINT('Ctrl Pts',(202.894630439562,9.78847138567757,28.6771422031307));
#78299=CARTESIAN_POINT('Ctrl Pts',(202.891629218829,9.75818855464752,28.7235979911491));
#78300=CARTESIAN_POINT('Ctrl Pts',(202.888627998097,9.73064099627023,28.7716045238676));
#78301=CARTESIAN_POINT('Ctrl Pts',(202.885624033456,9.70306825215266,28.8196549472296));
#78302=CARTESIAN_POINT('Ctrl Pts',(202.882620068815,9.67823603942744,28.8692584891787));
#78303=CARTESIAN_POINT('Ctrl Pts',(202.879616104174,9.65630662968284,28.9200686449538));
#78304=CARTESIAN_POINT('Ctrl Pts',(202.876610755,9.6343671126271,28.9709022192368));
#78305=CARTESIAN_POINT('Ctrl Pts',(202.873605405825,9.61533324693363,29.0229430197891));
#78306=CARTESIAN_POINT('Ctrl Pts',(202.870600056651,9.59931837382386,29.075826412783));
#78307=CARTESIAN_POINT('Ctrl Pts',(202.867589134784,9.5832738050087,29.1288078652274));
#78308=CARTESIAN_POINT('Ctrl Pts',(202.864578212917,9.57025953488192,29.1826345172014));
#78309=CARTESIAN_POINT('Ctrl Pts',(202.86156729105,9.56033814730236,29.2369296674134));
#78310=CARTESIAN_POINT('Ctrl Pts',(202.859395071671,9.5531803958474,29.2761007195784));
#78311=CARTESIAN_POINT('Ctrl Pts',(202.857222852291,9.54763136280445,29.3155153844959));
#78312=CARTESIAN_POINT('Ctrl Pts',(202.855050632911,9.54369772092486,29.3550313069641));
#78313=CARTESIAN_POINT('Ctrl Pts',(202.852418770555,9.53893171796851,29.4029088232889));
#78314=CARTESIAN_POINT('Ctrl Pts',(202.849786908199,9.53652628509325,29.4510251361842));
#78315=CARTESIAN_POINT('Ctrl Pts',(202.847155045843,9.53650021423273,29.4992081293359));
#78316=CARTESIAN_POINT('',(202.347155045874,9.5365000353343,29.4996784047698));
#78317=CARTESIAN_POINT('Ctrl Pts',(202.847155045809,9.53650021423239,29.4992081299609));
#78318=CARTESIAN_POINT('Ctrl Pts',(202.844182904519,9.53647077263956,29.5536208020761));
#78319=CARTESIAN_POINT('Ctrl Pts',(202.841210763228,9.5394801612605,29.608151560332));
#78320=CARTESIAN_POINT('Ctrl Pts',(202.838238621938,9.54554158352536,29.6624283372632));
#78321=CARTESIAN_POINT('Ctrl Pts',(202.835270150082,9.55159552230065,29.7166381035694));
#78322=CARTESIAN_POINT('Ctrl Pts',(202.832301678225,9.56069397931198,29.7705939747778));
#78323=CARTESIAN_POINT('Ctrl Pts',(202.829333206369,9.57279816347795,29.8239246329443));
#78324=CARTESIAN_POINT('Ctrl Pts',(202.826367158666,9.58489246296194,29.8772117395101));
#78325=CARTESIAN_POINT('Ctrl Pts',(202.823401110963,9.5999875107837,29.9298741172893));
#78326=CARTESIAN_POINT('Ctrl Pts',(202.82043506326,9.6179931298954,29.9815488147464));
#78327=CARTESIAN_POINT('Ctrl Pts',(202.817470198313,9.63599156899636,30.0332029061427));
#78328=CARTESIAN_POINT('Ctrl Pts',(202.814505333366,9.65689810096678,30.0838695866816));
#78329=CARTESIAN_POINT('Ctrl Pts',(202.81154046842,9.68057291225944,30.1332017136241));
#78330=CARTESIAN_POINT('Ctrl Pts',(202.808573410788,9.70426523240693,30.1825703244497));
#78331=CARTESIAN_POINT('Ctrl Pts',(202.805606353157,9.730729693571,30.2306019171568));
#78332=CARTESIAN_POINT('Ctrl Pts',(202.802639295526,9.75977927637045,30.2769715610496));
#78333=CARTESIAN_POINT('Ctrl Pts',(202.799671292272,9.78883811748051,30.3233559832808));
#78334=CARTESIAN_POINT('Ctrl Pts',(202.796703289018,9.82048341153653,30.3680769557165));
#78335=CARTESIAN_POINT('Ctrl Pts',(202.793735285764,9.85448520143498,30.4108392263559));
#78336=CARTESIAN_POINT('Ctrl Pts',(202.790761646491,9.88855155822017,30.4536826993876));
#78337=CARTESIAN_POINT('Ctrl Pts',(202.787788007219,9.92498299101151,30.494559632155));
#78338=CARTESIAN_POINT('Ctrl Pts',(202.784814367946,9.96351052718381,30.5332094766993));
#78339=CARTESIAN_POINT('Ctrl Pts',(202.78200915669,9.99985584960956,30.5696701799061));
#78340=CARTESIAN_POINT('Ctrl Pts',(202.779203945433,10.0380659299903,30.6041490219623));
#78341=CARTESIAN_POINT('Ctrl Pts',(202.776398734177,10.0778892147288,30.6364611518598));
#78342=CARTESIAN_POINT('Ctrl Pts',(202.773386944796,10.1206451197699,30.6711527742773));
#78343=CARTESIAN_POINT('Ctrl Pts',(202.770375155415,10.1654500942286,30.7035000924404));
#78344=CARTESIAN_POINT('Ctrl Pts',(202.767363366034,10.2120170406476,30.7332538691487));
#78345=CARTESIAN_POINT('Ctrl Pts',(202.764356875252,10.2585020624853,30.7629553004513));
#78346=CARTESIAN_POINT('Ctrl Pts',(202.761350384471,10.3067424634887,30.79007196385));
#78347=CARTESIAN_POINT('Ctrl Pts',(202.758343893689,10.3564193016363,30.8143957298674));
#78348=CARTESIAN_POINT('Ctrl Pts',(202.755340343973,10.4060475439786,30.8386957014357));
#78349=CARTESIAN_POINT('Ctrl Pts',(202.752336794256,10.4571089682818,30.8602079573718));
#78350=CARTESIAN_POINT('Ctrl Pts',(202.74933324454,10.5092585781739,30.8787694175982));
#78351=CARTESIAN_POINT('Ctrl Pts',(202.746331450634,10.5613777025278,30.8973200271949));
#78352=CARTESIAN_POINT('Ctrl Pts',(202.743329656729,10.6145832556133,30.9129230838526));
#78353=CARTESIAN_POINT('Ctrl Pts',(202.740327862823,10.6685108626173,30.9254638549599));
#78354=CARTESIAN_POINT('Ctrl Pts',(202.73732664209,10.7224281725025,30.9380022314903));
#78355=CARTESIAN_POINT('Ctrl Pts',(202.734325421357,10.7770667490338,30.9474793645404));
#78356=CARTESIAN_POINT('Ctrl Pts',(202.731324200624,10.8320499276654,30.9538311536086));
#78357=CARTESIAN_POINT('Ctrl Pts',(202.728320235982,10.8870833754366,30.9601887498886));
#78358=CARTESIAN_POINT('Ctrl Pts',(202.725316271341,10.94246152968,30.9634152334097));
#78359=CARTESIAN_POINT('Ctrl Pts',(202.7223123067,10.9978019672819,30.9634983493848));
#78360=CARTESIAN_POINT('Ctrl Pts',(202.719306957526,11.0531679114081,30.9635815036684));
#78361=CARTESIAN_POINT('Ctrl Pts',(202.716301608351,11.1084955767833,30.9605184316654));
#78362=CARTESIAN_POINT('Ctrl Pts',(202.713296259176,11.1634052063721,30.9543489913121));
#78363=CARTESIAN_POINT('Ctrl Pts',(202.710285337309,11.2184166525767,30.9481681112251));
#78364=CARTESIAN_POINT('Ctrl Pts',(202.707274415441,11.2730079936089,30.9388694460215));
#78365=CARTESIAN_POINT('Ctrl Pts',(202.704263493574,11.3268084289459,30.9265442512484));
#78366=CARTESIAN_POINT('Ctrl Pts',(202.702091274197,11.3656225706884,30.9176522812498));
#78367=CARTESIAN_POINT('Ctrl Pts',(202.69991905482,11.404025270005,30.9071861329833));
#78368=CARTESIAN_POINT('Ctrl Pts',(202.697746835443,11.4418831057935,30.895195889764));
#78369=CARTESIAN_POINT('Ctrl Pts',(202.694735046062,11.4943731208542,30.8785713777163));
#78370=CARTESIAN_POINT('Ctrl Pts',(202.691723256681,11.5460324336264,30.8589461354871));
#78371=CARTESIAN_POINT('Ctrl Pts',(202.6887114673,11.5964949799208,30.8364228331368));
#78372=CARTESIAN_POINT('Ctrl Pts',(202.685704976518,11.646868748159,30.8139391557192));
#78373=CARTESIAN_POINT('Ctrl Pts',(202.682698485736,11.6960494505891,30.7885677499365));
#78374=CARTESIAN_POINT('Ctrl Pts',(202.679691994954,11.74368783712,30.760460491614));
#78375=CARTESIAN_POINT('Ctrl Pts',(202.676688445238,11.7912796219378,30.7323807288992));
#78376=CARTESIAN_POINT('Ctrl Pts',(202.673684895522,11.8373316277677,30.701570682381));
#78377=CARTESIAN_POINT('Ctrl Pts',(202.670681345806,11.8815178953516,30.668228766199));
#78378=CARTESIAN_POINT('Ctrl Pts',(202.6676795519,11.9256783325958,30.6349063409826));
#78379=CARTESIAN_POINT('Ctrl Pts',(202.664677757994,11.9679747733647,30.5990552970014));
#78380=CARTESIAN_POINT('Ctrl Pts',(202.661675964089,12.0081109756505,30.5609168255679));
#78381=CARTESIAN_POINT('Ctrl Pts',(202.658674743355,12.0482395141946,30.5227856364226));
#78382=CARTESIAN_POINT('Ctrl Pts',(202.655673522622,12.0862082514783,30.4823682504933));
#78383=CARTESIAN_POINT('Ctrl Pts',(202.652672301889,12.1217564698807,30.4399439729477));
#78384=CARTESIAN_POINT('Ctrl Pts',(202.649668337248,12.1573371887388,30.3974809084133));
#78385=CARTESIAN_POINT('Ctrl Pts',(202.646664372607,12.1904926284475,30.3530076919667));
#78386=CARTESIAN_POINT('Ctrl Pts',(202.643660407966,12.2210022017771,30.3068369558068));
#78387=CARTESIAN_POINT('Ctrl Pts',(202.640655058791,12.2515258370332,30.2606449394573));
#78388=CARTESIAN_POINT('Ctrl Pts',(202.637649709616,12.2794009093005,30.2127543003707));
#78389=CARTESIAN_POINT('Ctrl Pts',(202.634644360441,12.3044518187262,30.1635041089714));
#78390=CARTESIAN_POINT('Ctrl Pts',(202.631633438574,12.3295491789992,30.1141625950144));
#78391=CARTESIAN_POINT('Ctrl Pts',(202.628622516707,12.3518117036761,30.063456977127));
#78392=CARTESIAN_POINT('Ctrl Pts',(202.625611594839,12.3711116431405,30.0117471172801));
#78393=CARTESIAN_POINT('Ctrl Pts',(202.623439375463,12.3850355190573,29.9744412141446));
#78394=CARTESIAN_POINT('Ctrl Pts',(202.621267156086,12.3974184365851,29.9366130377746));
#78395=CARTESIAN_POINT('Ctrl Pts',(202.619094936709,12.408228833152,29.8984015605883));
#78396=CARTESIAN_POINT('Ctrl Pts',(202.616083147328,12.4232174838996,29.8454212205477));
#78397=CARTESIAN_POINT('Ctrl Pts',(202.613071357947,12.4352432050487,29.7914840648974));
#78398=CARTESIAN_POINT('Ctrl Pts',(202.610059568566,12.4441903848178,29.7369522787393));
#78399=CARTESIAN_POINT('Ctrl Pts',(202.607053077784,12.453121823938,29.6825164295945));
#78400=CARTESIAN_POINT('Ctrl Pts',(202.604046587002,12.4589853856003,29.6274885424128));
#78401=CARTESIAN_POINT('Ctrl Pts',(202.60104009622,12.4617157998699,29.5722438261069));
#78402=CARTESIAN_POINT('Ctrl Pts',(202.598036546504,12.4644435431427,29.5170531523201));
#78403=CARTESIAN_POINT('Ctrl Pts',(202.595032996788,12.4640441850761,29.4616465938575));
#78404=CARTESIAN_POINT('Ctrl Pts',(202.592029447071,12.4605041324605,29.4064055072888));
#78405=CARTESIAN_POINT('Ctrl Pts',(202.589027653165,12.4569661492833,29.3511967134687));
#78406=CARTESIAN_POINT('Ctrl Pts',(202.58602585926,12.4502911445459,29.2961537251037));
#78407=CARTESIAN_POINT('Ctrl Pts',(202.583024065354,12.4405175955905,29.2416566107017));
#78408=CARTESIAN_POINT('Ctrl Pts',(202.580022844621,12.4307459128295,29.1871699021622));
#78409=CARTESIAN_POINT('Ctrl Pts',(202.577021623887,12.4178769541139,29.1332293793805));
#78410=CARTESIAN_POINT('Ctrl Pts',(202.574020403154,12.4020005670935,29.0802064080176));
#78411=CARTESIAN_POINT('Ctrl Pts',(202.571016438513,12.3861096648643,29.0271349596619));
#78412=CARTESIAN_POINT('Ctrl Pts',(202.568012473872,12.3672059931612,28.9749832448325));
#78413=CARTESIAN_POINT('Ctrl Pts',(202.56500850923,12.3454293058665,28.9241074467268));
#78414=CARTESIAN_POINT('Ctrl Pts',(202.562003160056,12.3236425816508,28.8732081998585));
#78415=CARTESIAN_POINT('Ctrl Pts',(202.558997810881,12.2989804373979,28.823586515012));
#78416=CARTESIAN_POINT('Ctrl Pts',(202.555992461706,12.2716294517743,28.7755755474998));
#78417=CARTESIAN_POINT('Ctrl Pts',(202.552981539839,12.2442277503688,28.7274755552706));
#78418=CARTESIAN_POINT('Ctrl Pts',(202.549970617971,12.2141275358225,28.6809926898822));
#78419=CARTESIAN_POINT('Ctrl Pts',(202.546959696104,12.1815590705988,28.6364315819313));
#78420=CARTESIAN_POINT('Ctrl Pts',(202.544787476728,12.158062661748,28.6042831216318));
#78421=CARTESIAN_POINT('Ctrl Pts',(202.542615257351,12.1332824784799,28.5731342839266));
#78422=CARTESIAN_POINT('Ctrl Pts',(202.540443037975,12.1073172197368,28.5430878698259));
#78423=CARTESIAN_POINT('Ctrl Pts',(202.537431248594,12.0713163022358,28.5014284168645));
#78424=CARTESIAN_POINT('Ctrl Pts',(202.534419459213,12.0328865517901,28.4617170959423));
#78425=CARTESIAN_POINT('Ctrl Pts',(202.531407669832,11.9922668474289,28.4242496788318));
#78426=CARTESIAN_POINT('Ctrl Pts',(202.52840117905,11.9517186047489,28.3868481776273));
#78427=CARTESIAN_POINT('Ctrl Pts',(202.525394688268,11.9089884389232,28.3516831004702));
#78428=CARTESIAN_POINT('Ctrl Pts',(202.522388197486,11.8643537962268,28.3190153409344));
#78429=CARTESIAN_POINT('Ctrl Pts',(202.51938464777,11.819762816865,28.286379538265));
#78430=CARTESIAN_POINT('Ctrl Pts',(202.516381098054,11.773271475018,28.2562365234736));
#78431=CARTESIAN_POINT('Ctrl Pts',(202.513377548338,11.7251907759786,28.2288074148912));
#78432=CARTESIAN_POINT('Ctrl Pts',(202.510375754432,11.6771381838797,28.2013943407747));
#78433=CARTESIAN_POINT('Ctrl Pts',(202.507373960526,11.6274985334929,28.1766922889209));
#78434=CARTESIAN_POINT('Ctrl Pts',(202.50437216662,11.5766103959632,28.154878183484));
#78435=CARTESIAN_POINT('Ctrl Pts',(202.501370945887,11.5257319751857,28.1330682433059));
#78436=CARTESIAN_POINT('Ctrl Pts',(202.498369725154,11.4736060252663,28.1141453618837));
#78437=CARTESIAN_POINT('Ctrl Pts',(202.495368504421,11.4205921057218,28.0982387754669));
#78438=CARTESIAN_POINT('Ctrl Pts',(202.49236453978,11.3675297174603,28.0823176462311));
#78439=CARTESIAN_POINT('Ctrl Pts',(202.489360575138,11.3135782439922,28.069418472845));
#78440=CARTESIAN_POINT('Ctrl Pts',(202.486356610497,11.2591120165662,28.0596204622146));
#78441=CARTESIAN_POINT('Ctrl Pts',(202.483351261322,11.2046206855411,28.0498179356604));
#78442=CARTESIAN_POINT('Ctrl Pts',(202.480345912147,11.1496146520238,28.0431194848871));
#78443=CARTESIAN_POINT('Ctrl Pts',(202.477340562973,11.0944747720894,28.0395525454715));
#78444=CARTESIAN_POINT('Ctrl Pts',(202.474329641105,11.0392326485958,28.0359789920304));
#78445=CARTESIAN_POINT('Ctrl Pts',(202.471318719238,10.9838567114718,28.0355485526982));
#78446=CARTESIAN_POINT('Ctrl Pts',(202.468307797371,10.9287280233432,28.038236491308));
#78447=CARTESIAN_POINT('Ctrl Pts',(202.466135577994,10.8889556181346,28.0401756955081));
#78448=CARTESIAN_POINT('Ctrl Pts',(202.463963358617,10.8493118839798,28.0437368632858));
#78449=CARTESIAN_POINT('Ctrl Pts',(202.461791139241,10.8099369627027,28.0488941141828));
#78450=CARTESIAN_POINT('Ctrl Pts',(202.45877934986,10.7553435035612,28.0560446596822));
#78451=CARTESIAN_POINT('Ctrl Pts',(202.455767560479,10.7010410014664,28.066295171619));
#78452=CARTESIAN_POINT('Ctrl Pts',(202.452755771098,10.6474078603407,28.0796088450534));
#78453=CARTESIAN_POINT('Ctrl Pts',(202.449749280316,10.5938690752545,28.0928990959273));
#78454=CARTESIAN_POINT('Ctrl Pts',(202.446742789534,10.5409978219095,28.1092416872979));
#78455=CARTESIAN_POINT('Ctrl Pts',(202.443736298752,10.4891645904217,28.1285484207159));
#78456=CARTESIAN_POINT('Ctrl Pts',(202.440732749036,10.4373820642065,28.1478362675401));
#78457=CARTESIAN_POINT('Ctrl Pts',(202.437729199319,10.3866360400535,28.1700823287675));
#78458=CARTESIAN_POINT('Ctrl Pts',(202.434725649603,10.3372822498144,28.1951485013271));
#78459=CARTESIAN_POINT('Ctrl Pts',(202.431723855697,10.2879573107374,28.2202000207424));
#78460=CARTESIAN_POINT('Ctrl Pts',(202.428722061791,10.2400234616233,28.2480681452834));
#78461=CARTESIAN_POINT('Ctrl Pts',(202.425720267885,10.1938146891182,28.2785674416824));
#78462=CARTESIAN_POINT('Ctrl Pts',(202.422719047152,10.1476147398716,28.309060914443));
#78463=CARTESIAN_POINT('Ctrl Pts',(202.419717826419,10.1031396528728,28.3421842707461));
#78464=CARTESIAN_POINT('Ctrl Pts',(202.416716605686,10.0606951338846,28.377708318443));
#78465=CARTESIAN_POINT('Ctrl Pts',(202.413712641045,10.0182118094015,28.4132648444973));
#78466=CARTESIAN_POINT('Ctrl Pts',(202.410708676403,9.97776316684075,28.451226107364));
#78467=CARTESIAN_POINT('Ctrl Pts',(202.407704711762,9.93962125619621,28.4913230598011));
#78468=CARTESIAN_POINT('Ctrl Pts',(202.404699362587,9.90146176586465,28.531438493008));
#78469=CARTESIAN_POINT('Ctrl Pts',(202.401694013412,9.86561146851262,28.5736911751225));
#78470=CARTESIAN_POINT('Ctrl Pts',(202.398688664238,9.83230276734794,28.6177781328618));
#78471=CARTESIAN_POINT('Ctrl Pts',(202.39567774237,9.79893230326019,28.6619468391919));
#78472=CARTESIAN_POINT('Ctrl Pts',(202.392666820503,9.76811314319873,28.7079561758911));
#78473=CARTESIAN_POINT('Ctrl Pts',(202.389655898636,9.74003423380136,28.7554742999685));
#78474=CARTESIAN_POINT('Ctrl Pts',(202.387483679259,9.71977679978217,28.7897560895348));
#78475=CARTESIAN_POINT('Ctrl Pts',(202.385311459882,9.70094469191825,28.8248225876061));
#78476=CARTESIAN_POINT('Ctrl Pts',(202.383139240506,9.68359338206267,28.8605425219369));
#78477=CARTESIAN_POINT('Ctrl Pts',(202.379914219016,9.65783247238003,28.9135747143088));
#78478=CARTESIAN_POINT('Ctrl Pts',(202.376689197525,9.6352427898551,28.9682422387701));
#78479=CARTESIAN_POINT('Ctrl Pts',(202.373464176035,9.61601745292213,29.0241591028675));
#78480=CARTESIAN_POINT('Ctrl Pts',(202.370246978428,9.59683875654359,29.0799403129811));
#78481=CARTESIAN_POINT('Ctrl Pts',(202.367029780821,9.58100830934031,29.1369644532309));
#78482=CARTESIAN_POINT('Ctrl Pts',(202.363812583214,9.56867188081793,29.194824533688));
#78483=CARTESIAN_POINT('Ctrl Pts',(202.360606820318,9.55637929899555,29.2524789651938));
#78484=CARTESIAN_POINT('Ctrl Pts',(202.357401057422,9.54755609808255,29.3109630249618));
#78485=CARTESIAN_POINT('Ctrl Pts',(202.354195294526,9.54229812331524,29.3698558925278));
#78486=CARTESIAN_POINT('Ctrl Pts',(202.351848544976,9.53844907074235,29.4129678802155));
#78487=CARTESIAN_POINT('Ctrl Pts',(202.349501795425,9.53650956779653,29.4562985383023));
#78488=CARTESIAN_POINT('Ctrl Pts',(202.347155045874,9.5365000353343,29.4996784047699));
#78489=CARTESIAN_POINT('',(201.847155045881,9.53650048906759,29.5011964533363));
#78490=CARTESIAN_POINT('Ctrl Pts',(202.347155045843,9.53650003533417,29.4996784053507));
#78491=CARTESIAN_POINT('Ctrl Pts',(202.344062800078,9.53648747469995,29.5568388331947));
#78492=CARTESIAN_POINT('Ctrl Pts',(202.340970554314,9.53982804448367,29.613961635679));
#78493=CARTESIAN_POINT('Ctrl Pts',(202.337878308549,9.54648255526969,29.6706437454601));
#78494=CARTESIAN_POINT('Ctrl Pts',(202.334779716217,9.55315072386491,29.7274421903807));
#78495=CARTESIAN_POINT('Ctrl Pts',(202.331681123884,9.56314635575235,29.783797658737));
#78496=CARTESIAN_POINT('Ctrl Pts',(202.328582531552,9.57637867983794,29.8393148785126));
#78497=CARTESIAN_POINT('Ctrl Pts',(202.325480570849,9.58962538832023,29.8948924491162));
#78498=CARTESIAN_POINT('Ctrl Pts',(202.322378610145,9.60611565823238,29.9496294963648));
#78499=CARTESIAN_POINT('Ctrl Pts',(202.319276649441,9.62570903982726,30.0031467050349));
#78500=CARTESIAN_POINT('Ctrl Pts',(202.316167117876,9.64535024239885,30.0567945315454));
#78501=CARTESIAN_POINT('Ctrl Pts',(202.31305758631,9.66810949601393,30.1092161302731));
#78502=CARTESIAN_POINT('Ctrl Pts',(202.309948054744,9.69379870287798,30.160053347387));
#78503=CARTESIAN_POINT('Ctrl Pts',(202.308127817087,9.70883648613593,30.1898121116977));
#78504=CARTESIAN_POINT('Ctrl Pts',(202.30630757943,9.72487739373735,30.2190284520927));
#78505=CARTESIAN_POINT('Ctrl Pts',(202.304487341773,9.7418768384148,30.2476351786017));
#78506=CARTESIAN_POINT('Ctrl Pts',(202.301475552392,9.77000434514925,30.2949682478755));
#78507=CARTESIAN_POINT('Ctrl Pts',(202.298463763011,9.80086499296815,30.3408098790084));
#78508=CARTESIAN_POINT('Ctrl Pts',(202.29545197363,9.83427554241027,30.3848269542555));
#78509=CARTESIAN_POINT('Ctrl Pts',(202.292445482848,9.86762731313721,30.4287665908741));
#78510=CARTESIAN_POINT('Ctrl Pts',(202.289438992066,9.90351976623064,30.4708876252146));
#78511=CARTESIAN_POINT('Ctrl Pts',(202.286432501284,9.94172557045227,30.5108845046618));
#78512=CARTESIAN_POINT('Ctrl Pts',(202.283428951568,9.97989400027782,30.5508422576139));
#78513=CARTESIAN_POINT('Ctrl Pts',(202.280425401851,10.0203709354635,30.588679592687));
#78514=CARTESIAN_POINT('Ctrl Pts',(202.277421852135,10.0628890236482,30.6241242226734));
#78515=CARTESIAN_POINT('Ctrl Pts',(202.274420058229,10.1053822566748,30.6595481324929));
#78516=CARTESIAN_POINT('Ctrl Pts',(202.271418264324,10.1499138731675,30.6925817727536));
#78517=CARTESIAN_POINT('Ctrl Pts',(202.268416470418,10.1961816238766,30.722991524176));
#78518=CARTESIAN_POINT('Ctrl Pts',(202.265415249684,10.2424405400657,30.7533954690581));
#78519=CARTESIAN_POINT('Ctrl Pts',(202.262414028951,10.2904344915036,30.7811762307775));
#78520=CARTESIAN_POINT('Ctrl Pts',(202.259412808218,10.3398321939651,30.8061434522575));
#78521=CARTESIAN_POINT('Ctrl Pts',(202.256408843577,10.3892750589667,30.8311335003688));
#78522=CARTESIAN_POINT('Ctrl Pts',(202.253404878935,10.4401237671261,30.8533046311918));
#78523=CARTESIAN_POINT('Ctrl Pts',(202.250400914294,10.4920237082286,30.8725131463845));
#78524=CARTESIAN_POINT('Ctrl Pts',(202.247395565119,10.5439475701233,30.8917305148222));
#78525=CARTESIAN_POINT('Ctrl Pts',(202.244390215944,10.5969231257384,30.9079823908173));
#78526=CARTESIAN_POINT('Ctrl Pts',(202.24138486677,10.6505802518315,30.9211748976076));
#78527=CARTESIAN_POINT('Ctrl Pts',(202.238373944902,10.7043368720758,30.9343918667081));
#78528=CARTESIAN_POINT('Ctrl Pts',(202.235363023035,10.7587770676294,30.9445380383248));
#78529=CARTESIAN_POINT('Ctrl Pts',(202.232352101167,10.8135213520535,30.9515708607781));
#78530=CARTESIAN_POINT('Ctrl Pts',(202.230179881791,10.8530164305113,30.9566446667013));
#78531=CARTESIAN_POINT('Ctrl Pts',(202.228007662414,10.8926696066492,30.9600991125008));
#78532=CARTESIAN_POINT('Ctrl Pts',(202.225835443038,10.9323383716403,30.961935071762));
#78533=CARTESIAN_POINT('Ctrl Pts',(202.222823653657,10.9873392460684,30.9644806353762));
#78534=CARTESIAN_POINT('Ctrl Pts',(202.219811864276,11.0425979477148,30.9639233014669));
#78535=CARTESIAN_POINT('Ctrl Pts',(202.216800074895,11.097735488617,30.9602328664514));
#78536=CARTESIAN_POINT('Ctrl Pts',(202.213793584113,11.15277602681,30.9565489239668));
#78537=CARTESIAN_POINT('Ctrl Pts',(202.210787093331,11.2076953052168,30.9497428544513));
#78538=CARTESIAN_POINT('Ctrl Pts',(202.207780602549,11.2621131035355,30.9398364389593));
#78539=CARTESIAN_POINT('Ctrl Pts',(202.204777052833,11.3164776682581,30.9299397143063));
#78540=CARTESIAN_POINT('Ctrl Pts',(202.201773503116,11.3703412083566,30.9169487460775));
#78541=CARTESIAN_POINT('Ctrl Pts',(202.1987699534,11.4233292707362,30.9009370358935));
#78542=CARTESIAN_POINT('Ctrl Pts',(202.195768159494,11.4762863574364,30.8849346858101));
#78543=CARTESIAN_POINT('Ctrl Pts',(202.192766365589,11.5283684770106,30.86591524636));
#78544=CARTESIAN_POINT('Ctrl Pts',(202.189764571683,11.579214273977,30.8440026319994));
#78545=CARTESIAN_POINT('Ctrl Pts',(202.18676335095,11.6300503622757,30.8220942017071));
#78546=CARTESIAN_POINT('Ctrl Pts',(202.183762130217,11.6796501128072,30.7972939024439));
#78547=CARTESIAN_POINT('Ctrl Pts',(202.180760909483,11.7276723288805,30.7697736931365));
#78548=CARTESIAN_POINT('Ctrl Pts',(202.177756944842,11.7757384499363,30.7422283230931));
#78549=CARTESIAN_POINT('Ctrl Pts',(202.174752980201,11.8222236967836,30.7119583381411));
#78550=CARTESIAN_POINT('Ctrl Pts',(202.17174901556,11.8668130083111,30.6791808422047));
#78551=CARTESIAN_POINT('Ctrl Pts',(202.168743666385,11.9114228711462,30.6463882390514));
#78552=CARTESIAN_POINT('Ctrl Pts',(202.16573831721,11.9541346496012,30.6110861577062));
#78553=CARTESIAN_POINT('Ctrl Pts',(202.162732968036,11.9946663570722,30.5735320619845));
#78554=CARTESIAN_POINT('Ctrl Pts',(202.159722046168,12.0352732207829,30.5359083312833));
#78555=CARTESIAN_POINT('Ctrl Pts',(202.156711124301,12.073691572175,30.4960246257544));
#78556=CARTESIAN_POINT('Ctrl Pts',(202.153700202434,12.1096771375035,30.4541744602021));
#78557=CARTESIAN_POINT('Ctrl Pts',(202.151527983057,12.1356388016468,30.4239818001038));
#78558=CARTESIAN_POINT('Ctrl Pts',(202.149355763681,12.1603350517917,30.3927663743924));
#78559=CARTESIAN_POINT('Ctrl Pts',(202.147183544304,12.1836882301215,30.3606476769688));
#78560=CARTESIAN_POINT('Ctrl Pts',(202.144171754923,12.2160674894485,30.3161149963016));
#78561=CARTESIAN_POINT('Ctrl Pts',(202.141159965542,12.2459972448394,30.2696602390536));
#78562=CARTESIAN_POINT('Ctrl Pts',(202.138148176161,12.2732438090024,30.2215832958411));
#78563=CARTESIAN_POINT('Ctrl Pts',(202.135141685379,12.3004424386639,30.1735909337265));
#78564=CARTESIAN_POINT('Ctrl Pts',(202.132135194597,12.3249669873978,30.1239825046809));
#78565=CARTESIAN_POINT('Ctrl Pts',(202.129128703815,12.3466265039856,30.0730875227777));
#78566=CARTESIAN_POINT('Ctrl Pts',(202.126125154099,12.3682648323962,30.0222423283152));
#78567=CARTESIAN_POINT('Ctrl Pts',(202.123121604383,12.3870434754876,29.9701135572659));
#78568=CARTESIAN_POINT('Ctrl Pts',(202.120118054667,12.4028178477007,29.9170543563763));
#78569=CARTESIAN_POINT('Ctrl Pts',(202.117116260761,12.4185829985557,29.8640261727521));
#78570=CARTESIAN_POINT('Ctrl Pts',(202.114114466855,12.4313472097717,29.8100691419928));
#78571=CARTESIAN_POINT('Ctrl Pts',(202.111112672949,12.4410152014346,29.7555532023561));
#78572=CARTESIAN_POINT('Ctrl Pts',(202.108111452216,12.4506813470586,29.7010476721765));
#78573=CARTESIAN_POINT('Ctrl Pts',(202.105110231483,12.4572523554203,29.6459839641154));
#78574=CARTESIAN_POINT('Ctrl Pts',(202.10210901075,12.4606841583787,29.5907416082155));
#78575=CARTESIAN_POINT('Ctrl Pts',(202.099105046108,12.4641190989109,29.5354487462195));
#78576=CARTESIAN_POINT('Ctrl Pts',(202.096101081467,12.464409067828,29.4799774375864));
#78577=CARTESIAN_POINT('Ctrl Pts',(202.093097116826,12.4615620748737,29.4247102178855));
#78578=CARTESIAN_POINT('Ctrl Pts',(202.090091767651,12.4587137697344,29.3694175254064));
#78579=CARTESIAN_POINT('Ctrl Pts',(202.087086418476,12.4527256777536,29.3143296345363));
#78580=CARTESIAN_POINT('Ctrl Pts',(202.084081069302,12.4436577071515,29.2598236594038));
#78581=CARTESIAN_POINT('Ctrl Pts',(202.081070147434,12.434572922193,29.205216616135));
#78582=CARTESIAN_POINT('Ctrl Pts',(202.078059225567,12.4223969674231,29.1511941595467));
#78583=CARTESIAN_POINT('Ctrl Pts',(202.0750483037,12.4072406023832,29.0981217385773));
#78584=CARTESIAN_POINT('Ctrl Pts',(202.072876084323,12.3963060941934,29.059832820343));
#78585=CARTESIAN_POINT('Ctrl Pts',(202.070703864946,12.3838213993874,29.0220381121263));
#78586=CARTESIAN_POINT('Ctrl Pts',(202.06853164557,12.3698435949984,28.9848681962431));
#78587=CARTESIAN_POINT('Ctrl Pts',(202.065519856189,12.3504633227827,28.933331984403));
#78588=CARTESIAN_POINT('Ctrl Pts',(202.062508066808,12.3281305105252,28.8827841830126));
#78589=CARTESIAN_POINT('Ctrl Pts',(202.059496277427,12.3029670655067,28.8335849069799));
#78590=CARTESIAN_POINT('Ctrl Pts',(202.056489786645,12.2778478901871,28.7844721865496));
#78591=CARTESIAN_POINT('Ctrl Pts',(202.053483295863,12.24990820344,28.736703748984));
#78592=CARTESIAN_POINT('Ctrl Pts',(202.050476805081,12.2193181590764,28.690620313483));
#78593=CARTESIAN_POINT('Ctrl Pts',(202.047473255365,12.1887580390779,28.6445819585817));
#78594=CARTESIAN_POINT('Ctrl Pts',(202.044469705649,12.1555529880724,28.6002257775559));
#78595=CARTESIAN_POINT('Ctrl Pts',(202.041466155932,12.1199183997819,28.5578667674739));
#78596=CARTESIAN_POINT('Ctrl Pts',(202.038464362027,12.0843046427038,28.5155325195564));
#78597=CARTESIAN_POINT('Ctrl Pts',(202.035462568121,12.0462645024623,28.4751935311365));
#78598=CARTESIAN_POINT('Ctrl Pts',(202.032460774215,12.0060545165792,28.437132858881));
#78599=CARTESIAN_POINT('Ctrl Pts',(202.029459553482,11.9658522085262,28.3990794540584));
#78600=CARTESIAN_POINT('Ctrl Pts',(202.026458332749,11.923481260625,28.3633038636331));
#78601=CARTESIAN_POINT('Ctrl Pts',(202.023457112016,11.8792343899608,28.3300516517768));
#78602=CARTESIAN_POINT('Ctrl Pts',(202.020453147374,11.8349470659765,28.2967690386209));
#78603=CARTESIAN_POINT('Ctrl Pts',(202.017449182733,11.7887808155381,28.2660147302413));
#78604=CARTESIAN_POINT('Ctrl Pts',(202.014445218092,11.7410595113205,28.237992452209));
#78605=CARTESIAN_POINT('Ctrl Pts',(202.011439868917,11.6933162122531,28.2099572586497));
#78606=CARTESIAN_POINT('Ctrl Pts',(202.008434519742,11.6440169007015,28.1846568466644));
#78607=CARTESIAN_POINT('Ctrl Pts',(202.005429170567,11.5935094686339,28.1622486177761));
#78608=CARTESIAN_POINT('Ctrl Pts',(202.0024182487,11.54290838276,28.1397988382518));
#78609=CARTESIAN_POINT('Ctrl Pts',(201.999407326833,11.491095196204,28.1202521405945));
#78610=CARTESIAN_POINT('Ctrl Pts',(201.996396404965,11.4384360298945,28.1037170423978));
#78611=CARTESIAN_POINT('Ctrl Pts',(201.994224185589,11.4004452528341,28.0917878518449));
#78612=CARTESIAN_POINT('Ctrl Pts',(201.992051966212,11.3620145209045,28.0814251100782));
#78613=CARTESIAN_POINT('Ctrl Pts',(201.989879746836,11.3232842826823,28.0726529775242));
#78614=CARTESIAN_POINT('Ctrl Pts',(201.986867957455,11.2695846787362,28.0604903865994));
#78615=CARTESIAN_POINT('Ctrl Pts',(201.983856168074,11.2150864731016,28.0513372280561));
#78616=CARTESIAN_POINT('Ctrl Pts',(201.980844378693,11.1601574639435,28.0452897756793));
#78617=CARTESIAN_POINT('Ctrl Pts',(201.977837887911,11.1053250906276,28.0392529625013));
#78618=CARTESIAN_POINT('Ctrl Pts',(201.974831397129,11.0500639380232,28.0363110692666));
#78619=CARTESIAN_POINT('Ctrl Pts',(201.971824906347,10.9947521444968,28.0365094089771));
#78620=CARTESIAN_POINT('Ctrl Pts',(201.968821356631,10.9394944591071,28.0367075546639));
#78621=CARTESIAN_POINT('Ctrl Pts',(201.965817806914,10.8841867558119,28.0400398457189));
#78622=CARTESIAN_POINT('Ctrl Pts',(201.962814257198,10.8292105759947,28.0464996654118));
#78623=CARTESIAN_POINT('Ctrl Pts',(201.959812463292,10.7742665340674,28.0529557088333));
#78624=CARTESIAN_POINT('Ctrl Pts',(201.956810669386,10.7196541542458,28.0625355953953));
#78625=CARTESIAN_POINT('Ctrl Pts',(201.95380887548,10.6657509347894,28.0751807790439));
#78626=CARTESIAN_POINT('Ctrl Pts',(201.950807654747,10.6118580077953,28.0878235481787));
#78627=CARTESIAN_POINT('Ctrl Pts',(201.947806434014,10.5586744853758,28.1035303314076));
#78628=CARTESIAN_POINT('Ctrl Pts',(201.944805213281,10.5065664553562,28.1221917451909));
#78629=CARTESIAN_POINT('Ctrl Pts',(201.94180124864,10.4544107848416,28.1408702204326));
#78630=CARTESIAN_POINT('Ctrl Pts',(201.938797283998,10.4033330685613,28.162508544375));
#78631=CARTESIAN_POINT('Ctrl Pts',(201.935793319357,10.3536815908919,28.1869483010757));
#78632=CARTESIAN_POINT('Ctrl Pts',(201.932787970182,10.3040072287516,28.2113993221119));
#78633=CARTESIAN_POINT('Ctrl Pts',(201.929782621007,10.2557608755156,28.2386540898696));
#78634=CARTESIAN_POINT('Ctrl Pts',(201.926777271833,10.2092653408415,28.2685086485056));
#78635=CARTESIAN_POINT('Ctrl Pts',(201.923766349965,10.1626835914537,28.2984185651936));
#78636=CARTESIAN_POINT('Ctrl Pts',(201.920755428098,10.1178595732152,28.3309375916142));
#78637=CARTESIAN_POINT('Ctrl Pts',(201.917744506231,10.0750852982425,28.365819659634));
#78638=CARTESIAN_POINT('Ctrl Pts',(201.915572286854,10.0442259425348,28.3909852093838));
#78639=CARTESIAN_POINT('Ctrl Pts',(201.913400067478,10.0144327766592,28.4173798080866));
#78640=CARTESIAN_POINT('Ctrl Pts',(201.911227848101,9.98580323183818,28.4448994524454));
#78641=CARTESIAN_POINT('Ctrl Pts',(201.908260856627,9.94669870293719,28.4824879902618));
#78642=CARTESIAN_POINT('Ctrl Pts',(201.905293865153,9.90959419544,28.5223426406126));
#78643=CARTESIAN_POINT('Ctrl Pts',(201.902326873679,9.87476830483212,28.5642191056718));
#78644=CARTESIAN_POINT('Ctrl Pts',(201.89936403944,9.83999121092743,28.6060368950332));
#78645=CARTESIAN_POINT('Ctrl Pts',(201.896401205201,9.80748676148437,28.6498704794296));
#78646=CARTESIAN_POINT('Ctrl Pts',(201.893438370961,9.77749742944438,28.6954381844849));
#78647=CARTESIAN_POINT('Ctrl Pts',(201.890478438173,9.74753746542456,28.7409612658961));
#78648=CARTESIAN_POINT('Ctrl Pts',(201.887518505385,9.72008804040117,28.788214653367));
#78649=CARTESIAN_POINT('Ctrl Pts',(201.884558572597,9.69535034671186,28.8368849781711));
#78650=CARTESIAN_POINT('Ctrl Pts',(201.881600290387,9.67062644776295,28.88552816243));
#78651=CARTESIAN_POINT('Ctrl Pts',(201.878642008177,9.64861152914048,28.9355862335433));
#78652=CARTESIAN_POINT('Ctrl Pts',(201.875683725967,9.62946126115605,28.9867205290214));
#78653=CARTESIAN_POINT('Ctrl Pts',(201.872724575187,9.61030537053443,29.0378698378452));
#78654=CARTESIAN_POINT('Ctrl Pts',(201.869765424407,9.59401600912527,29.0900954949097));
#78655=CARTESIAN_POINT('Ctrl Pts',(201.866806273628,9.58070022768504,29.1430400494359));
#78656=CARTESIAN_POINT('Ctrl Pts',(201.863846530107,9.56738177899201,29.1959952091611));
#78657=CARTESIAN_POINT('Ctrl Pts',(201.860886786587,9.55703820822609,29.249669020086));
#78658=CARTESIAN_POINT('Ctrl Pts',(201.857927043067,9.54972558659084,29.3036931590323));
#78659=CARTESIAN_POINT('Ctrl Pts',(201.854963934922,9.54240465199745,29.3577787123971));
#78660=CARTESIAN_POINT('Ctrl Pts',(201.852000826778,9.53812158435973,29.4122148459862));
#78661=CARTESIAN_POINT('Ctrl Pts',(201.849037718633,9.53688050593125,29.4666294130105));
#78662=CARTESIAN_POINT('Ctrl Pts',(201.848410161049,9.53661765754973,29.4781538908724));
#78663=CARTESIAN_POINT('Ctrl Pts',(201.847782603465,9.53649107191448,29.4896774090577));
#78664=CARTESIAN_POINT('Ctrl Pts',(201.847155045881,9.53650048906759,29.5011964533363));
#78665=CARTESIAN_POINT('',(201.347155045797,9.53650045493154,29.498846057016));
#78666=CARTESIAN_POINT('Ctrl Pts',(201.847155045843,9.53650048906816,29.5011964540331));
#78667=CARTESIAN_POINT('Ctrl Pts',(201.842722901861,9.53656699802896,29.5825500446616));
#78668=CARTESIAN_POINT('Ctrl Pts',(201.838290757878,9.54342041677501,29.6636298191095));
#78669=CARTESIAN_POINT('Ctrl Pts',(201.833858613895,9.5569049506719,29.7435342452402));
#78670=CARTESIAN_POINT('Ctrl Pts',(201.833431059052,9.55820576079773,29.7512423712611));
#78671=CARTESIAN_POINT('Ctrl Pts',(201.833003504209,9.55956824594497,29.7589395808399));
#78672=CARTESIAN_POINT('Ctrl Pts',(201.832575949366,9.56099224510919,29.7666250763977));
#78673=CARTESIAN_POINT('Ctrl Pts',(201.829564159985,9.57102320519047,29.8207633800449));
#78674=CARTESIAN_POINT('Ctrl Pts',(201.826552370604,9.58413437912649,29.8744470074067));
#78675=CARTESIAN_POINT('Ctrl Pts',(201.823540581222,9.60026897905191,29.9273000339289));
#78676=CARTESIAN_POINT('Ctrl Pts',(201.82053409044,9.61637519359999,29.9800600768564));
#78677=CARTESIAN_POINT('Ctrl Pts',(201.817527599659,9.63549412516181,30.031991918523));
#78678=CARTESIAN_POINT('Ctrl Pts',(201.814521108877,9.65751808344034,30.0827302581043));
#78679=CARTESIAN_POINT('Ctrl Pts',(201.81151755916,9.67952049703066,30.1334189634785));
#78680=CARTESIAN_POINT('Ctrl Pts',(201.808514009444,9.70442209847273,30.1829159982691));
#78681=CARTESIAN_POINT('Ctrl Pts',(201.805510459728,9.73206614421684,30.2308734414102));
#78682=CARTESIAN_POINT('Ctrl Pts',(201.802508665822,9.75969402984755,30.2788028496636));
#78683=CARTESIAN_POINT('Ctrl Pts',(201.799506871917,9.7900609190577,30.3251939942497));
#78684=CARTESIAN_POINT('Ctrl Pts',(201.796505078011,9.82296395578155,30.3697231747002));
#78685=CARTESIAN_POINT('Ctrl Pts',(201.793503857278,9.8558607098888,30.4142438525991));
#78686=CARTESIAN_POINT('Ctrl Pts',(201.790502636545,9.89129233635037,30.4569028486328));
#78687=CARTESIAN_POINT('Ctrl Pts',(201.787501415812,9.92901377892201,30.4974070203588));
#78688=CARTESIAN_POINT('Ctrl Pts',(201.784497451171,9.96676970884983,30.5379482235901));
#78689=CARTESIAN_POINT('Ctrl Pts',(201.78149348653,10.0068192768218,30.576330280188));
#78690=CARTESIAN_POINT('Ctrl Pts',(201.778489521889,10.0488794092996,30.6122957663975));
#78691=CARTESIAN_POINT('Ctrl Pts',(201.775484172714,10.0909589273811,30.6482778291753));
#78692=CARTESIAN_POINT('Ctrl Pts',(201.77247882354,10.1350504368179,30.6818407813944));
#78693=CARTESIAN_POINT('Ctrl Pts',(201.769473474365,10.1808390847084,30.7127685866886));
#78694=CARTESIAN_POINT('Ctrl Pts',(201.766462552498,10.2267126365622,30.7437537401108));
#78695=CARTESIAN_POINT('Ctrl Pts',(201.763451630631,10.2742891587209,30.772093715934));
#78696=CARTESIAN_POINT('Ctrl Pts',(201.760440708763,10.3232272698689,30.7976174019143));
#78697=CARTESIAN_POINT('Ctrl Pts',(201.758268489387,10.3585335042961,30.8160313786603));
#78698=CARTESIAN_POINT('Ctrl Pts',(201.75609627001,10.3945478829151,30.8329804820701));
#78699=CARTESIAN_POINT('Ctrl Pts',(201.753924050634,10.4311363806478,30.8484162682857));
#78700=CARTESIAN_POINT('Ctrl Pts',(201.750912261253,10.4818664542887,30.8698180371461));
#78701=CARTESIAN_POINT('Ctrl Pts',(201.747900471872,10.5339110943134,30.8883973313584));
#78702=CARTESIAN_POINT('Ctrl Pts',(201.744888682491,10.5869251185626,30.9039947978271));
#78703=CARTESIAN_POINT('Ctrl Pts',(201.741882191709,10.6398458759761,30.9195648238898));
#78704=CARTESIAN_POINT('Ctrl Pts',(201.738875700927,10.6937321310723,30.9321632854896));
#78705=CARTESIAN_POINT('Ctrl Pts',(201.735869210145,10.7482195748634,30.9416791832853));
#78706=CARTESIAN_POINT('Ctrl Pts',(201.732865660429,10.8026537169286,30.9511857722615));
#78707=CARTESIAN_POINT('Ctrl Pts',(201.729862110713,10.8576873655468,30.9576156810671));
#78708=CARTESIAN_POINT('Ctrl Pts',(201.726858560997,10.9129437442086,30.9609084359834));
#78709=CARTESIAN_POINT('Ctrl Pts',(201.723856767091,10.9681678211823,30.9641992660262));
#78710=CARTESIAN_POINT('Ctrl Pts',(201.720854973185,11.0236138446584,30.9643565460904));
#78711=CARTESIAN_POINT('Ctrl Pts',(201.717853179279,11.0788999011562,30.9613716350051));
#78712=CARTESIAN_POINT('Ctrl Pts',(201.714851958546,11.1341754011483,30.9583872938688));
#78713=CARTESIAN_POINT('Ctrl Pts',(201.711850737812,11.1892904684896,30.9522619817705));
#78714=CARTESIAN_POINT('Ctrl Pts',(201.708849517079,11.2438654972957,30.9430391086969));
#78715=CARTESIAN_POINT('Ctrl Pts',(201.705845552438,11.2984904220849,30.9338078034827));
#78716=CARTESIAN_POINT('Ctrl Pts',(201.702841587797,11.3525738009007,30.9214733679745));
#78717=CARTESIAN_POINT('Ctrl Pts',(201.699837623155,11.4057449460853,30.9061306087011));
#78718=CARTESIAN_POINT('Ctrl Pts',(201.69683227398,11.4589405979627,30.8907807779177));
#78719=CARTESIAN_POINT('Ctrl Pts',(201.693826924805,11.511222679679,30.8724200345367));
#78720=CARTESIAN_POINT('Ctrl Pts',(201.690821575631,11.5622375870957,30.851192490231));
#78721=CARTESIAN_POINT('Ctrl Pts',(201.687810653763,11.6133470893088,30.8299255845831));
#78722=CARTESIAN_POINT('Ctrl Pts',(201.684799731896,11.6631842481321,30.8057814902572));
#78723=CARTESIAN_POINT('Ctrl Pts',(201.681788810028,11.7114183848775,30.7789511842358));
#78724=CARTESIAN_POINT('Ctrl Pts',(201.679616590652,11.7462167393563,30.7595945508906));
#78725=CARTESIAN_POINT('Ctrl Pts',(201.677444371275,11.7801812509772,30.7388407675266));
#78726=CARTESIAN_POINT('Ctrl Pts',(201.675272151899,11.8131977419609,30.7167751158163));
#78727=CARTESIAN_POINT('Ctrl Pts',(201.672260362518,11.8589752163816,30.6861810164238));
#78728=CARTESIAN_POINT('Ctrl Pts',(201.669248573136,11.9031186386945,30.6529365733508));
#78729=CARTESIAN_POINT('Ctrl Pts',(201.666236783755,11.9453050599633,30.6172424059298));
#78730=CARTESIAN_POINT('Ctrl Pts',(201.663230292973,11.9874172632476,30.5816110347613));
#78731=CARTESIAN_POINT('Ctrl Pts',(201.660223802192,12.0275788988573,30.543538830358));
#78732=CARTESIAN_POINT('Ctrl Pts',(201.65721731141,12.0654968787575,30.5032689825555));
#78733=CARTESIAN_POINT('Ctrl Pts',(201.654213761694,12.1033777658226,30.4630385282764));
#78734=CARTESIAN_POINT('Ctrl Pts',(201.651210211977,12.1390189855094,30.4206150717139));
#78735=CARTESIAN_POINT('Ctrl Pts',(201.648206662261,12.1721627874468,30.3762800064619));
#78736=CARTESIAN_POINT('Ctrl Pts',(201.645204868355,12.2052872142318,30.3319708585337));
#78737=CARTESIAN_POINT('Ctrl Pts',(201.642203074449,12.2359168020119,30.2857527386157));
#78738=CARTESIAN_POINT('Ctrl Pts',(201.639201280544,12.2638342617209,30.2379398409764));
#78739=CARTESIAN_POINT('Ctrl Pts',(201.636200059811,12.2917463907762,30.1901360728928));
#78740=CARTESIAN_POINT('Ctrl Pts',(201.633198839077,12.316947154631,30.1407385871525));
#78741=CARTESIAN_POINT('Ctrl Pts',(201.630197618344,12.3392640029974,30.0900882817643));
#78742=CARTESIAN_POINT('Ctrl Pts',(201.627193653703,12.3616012548543,30.0393916686263));
#78743=CARTESIAN_POINT('Ctrl Pts',(201.624189689062,12.3810491109476,29.987440431328));
#78744=CARTESIAN_POINT('Ctrl Pts',(201.621185724421,12.3974828492734,29.9345962908109));
#78745=CARTESIAN_POINT('Ctrl Pts',(201.618180375246,12.4139241619439,29.881727794318));
#78746=CARTESIAN_POINT('Ctrl Pts',(201.615175026071,12.4273484596738,29.8279660867879));
#78747=CARTESIAN_POINT('Ctrl Pts',(201.612169676896,12.4376815934965,29.7736857426347));
#78748=CARTESIAN_POINT('Ctrl Pts',(201.609158755029,12.4480338876144,29.7193047487232));
#78749=CARTESIAN_POINT('Ctrl Pts',(201.606147833162,12.4552834994295,29.664403721238));
#78750=CARTESIAN_POINT('Ctrl Pts',(201.603136911295,12.4594080288043,29.6093638672573));
#78751=CARTESIAN_POINT('Ctrl Pts',(201.600964691918,12.4623836565428,29.5696555511454));
#78752=CARTESIAN_POINT('Ctrl Pts',(201.598792472542,12.4637338249514,29.5298750959088));
#78753=CARTESIAN_POINT('Ctrl Pts',(201.596620253165,12.4634669515017,29.4901647642452));
#78754=CARTESIAN_POINT('Ctrl Pts',(201.593608463784,12.4630969305772,29.4351062574866));
#78755=CARTESIAN_POINT('Ctrl Pts',(201.590596674403,12.4596147135106,29.3799545676392));
#78756=CARTESIAN_POINT('Ctrl Pts',(201.587584885022,12.4530102045503,29.3250897502356));
#78757=CARTESIAN_POINT('Ctrl Pts',(201.58457839424,12.4464173148108,29.2703214557425));
#78758=CARTESIAN_POINT('Ctrl Pts',(201.581571903458,12.4367130971049,29.2158395515752));
#78759=CARTESIAN_POINT('Ctrl Pts',(201.578565412676,12.4239394326528,29.1620225715577));
#78760=CARTESIAN_POINT('Ctrl Pts',(201.57556186296,12.4111782638935,29.1082582373925));
#78761=CARTESIAN_POINT('Ctrl Pts',(201.572558313244,12.3953537181153,29.0551580494608));
#78762=CARTESIAN_POINT('Ctrl Pts',(201.569554763527,12.3765590192188,29.0030920441296));
#78763=CARTESIAN_POINT('Ctrl Pts',(201.566552969621,12.3577753072983,28.9510564754631));
#78764=CARTESIAN_POINT('Ctrl Pts',(201.563551175716,12.3360250626919,28.9000543861345));
#78765=CARTESIAN_POINT('Ctrl Pts',(201.56054938181,12.3114511579773,28.8504400641665));
#78766=CARTESIAN_POINT('Ctrl Pts',(201.557548161076,12.2868819454868,28.8008352157242));
#78767=CARTESIAN_POINT('Ctrl Pts',(201.554546940343,12.2594903777988,28.752618080638));
#78768=CARTESIAN_POINT('Ctrl Pts',(201.55154571961,12.2294662372717,28.7061202727056));
#78769=CARTESIAN_POINT('Ctrl Pts',(201.548541754969,12.1994146467543,28.6595799535022));
#78770=CARTESIAN_POINT('Ctrl Pts',(201.545537790328,12.1667259619551,28.6147625456171));
#78771=CARTESIAN_POINT('Ctrl Pts',(201.542533825686,12.131633663166,28.5719711737292));
#78772=CARTESIAN_POINT('Ctrl Pts',(201.539528476511,12.0965251902624,28.5291600792078));
#78773=CARTESIAN_POINT('Ctrl Pts',(201.536523127336,12.0590112527024,28.4883772708833));
#78774=CARTESIAN_POINT('Ctrl Pts',(201.533517778162,12.0193638829366,28.4498907084668));
#78775=CARTESIAN_POINT('Ctrl Pts',(201.530506856294,11.9796429967213,28.411332782037));
#78776=CARTESIAN_POINT('Ctrl Pts',(201.527495934427,11.9377811759394,28.3750799524755));
#78777=CARTESIAN_POINT('Ctrl Pts',(201.524485012559,11.894084456764,28.3413606108141));
#78778=CARTESIAN_POINT('Ctrl Pts',(201.522312793183,11.8625596068125,28.3170339060546));
#78779=CARTESIAN_POINT('Ctrl Pts',(201.520140573806,11.8300804229227,28.2940249906641));
#78780=CARTESIAN_POINT('Ctrl Pts',(201.51796835443,11.7967703429812,28.2724050869502));
#78781=CARTESIAN_POINT('Ctrl Pts',(201.514956565049,11.7505858064956,28.2424290186358));
#78782=CARTESIAN_POINT('Ctrl Pts',(201.511944775668,11.7026115779343,28.2150007827707));
#78783=CARTESIAN_POINT('Ctrl Pts',(201.508932986287,11.6531594998416,28.1903378612151));
#78784=CARTESIAN_POINT('Ctrl Pts',(201.505926495505,11.6037944221024,28.1657183287946));
#78785=CARTESIAN_POINT('Ctrl Pts',(201.502920004723,11.5529571229392,28.1438546891898));
#78786=CARTESIAN_POINT('Ctrl Pts',(201.499913513941,11.5009867641489,28.1249201797177));
#78787=CARTESIAN_POINT('Ctrl Pts',(201.496909964225,11.4490672447745,28.1060041927154));
#78788=CARTESIAN_POINT('Ctrl Pts',(201.493906414509,11.3960173547821,28.0900118389401));
#78789=CARTESIAN_POINT('Ctrl Pts',(201.490902864792,11.3421974006717,28.0770688038512));
#78790=CARTESIAN_POINT('Ctrl Pts',(201.487901070887,11.2884089085467,28.0641333349817));
#78791=CARTESIAN_POINT('Ctrl Pts',(201.484899276981,11.2338517564166,28.0542437744356));
#78792=CARTESIAN_POINT('Ctrl Pts',(201.481897483075,11.1789004082605,28.0474756821574));
#78793=CARTESIAN_POINT('Ctrl Pts',(201.478896262342,11.1239595526997,28.0407088822014));
#78794=CARTESIAN_POINT('Ctrl Pts',(201.475895041609,11.0686251737817,28.037062431038));
#78795=CARTESIAN_POINT('Ctrl Pts',(201.472893820875,11.0132786024162,28.0365602408306));
#78796=CARTESIAN_POINT('Ctrl Pts',(201.469889856234,10.9578814296741,28.0360575914887));
#78797=CARTESIAN_POINT('Ctrl Pts',(201.466885891593,10.9024725706955,28.0387049505745));
#78798=CARTESIAN_POINT('Ctrl Pts',(201.463881926952,10.8474336004443,28.0444740662817));
#78799=CARTESIAN_POINT('Ctrl Pts',(201.460876577777,10.7923692626156,28.0502458409865));
#78800=CARTESIAN_POINT('Ctrl Pts',(201.457871228602,10.7376756747593,28.0591421555882));
#78801=CARTESIAN_POINT('Ctrl Pts',(201.454865879428,10.6837262502445,28.0710832196326));
#78802=CARTESIAN_POINT('Ctrl Pts',(201.45185495756,10.6296767895818,28.0830464254896));
#78803=CARTESIAN_POINT('Ctrl Pts',(201.448844035693,10.576374757268,28.0980655147301));
#78804=CARTESIAN_POINT('Ctrl Pts',(201.445833113826,10.5241792255266,28.1160105345128));
#78805=CARTESIAN_POINT('Ctrl Pts',(201.443660894449,10.4865229360539,28.1289569082154));
#78806=CARTESIAN_POINT('Ctrl Pts',(201.441488675073,10.4494422378693,28.1434251284135));
#78807=CARTESIAN_POINT('Ctrl Pts',(201.439316455696,10.4130645082021,28.1593512844641));
#78808=CARTESIAN_POINT('Ctrl Pts',(201.436304666315,10.3626266651817,28.1814329527306));
#78809=CARTESIAN_POINT('Ctrl Pts',(201.433292876934,10.3133321681557,28.2064106886505));
#78810=CARTESIAN_POINT('Ctrl Pts',(201.430281087553,10.2655341725827,28.2341436896882));
#78811=CARTESIAN_POINT('Ctrl Pts',(201.427274596771,10.2178202673589,28.2618279004426));
#78812=CARTESIAN_POINT('Ctrl Pts',(201.424268105989,10.171598091173,28.2922574937954));
#78813=CARTESIAN_POINT('Ctrl Pts',(201.421261615207,10.1271988765727,28.3252445152526));
#78814=CARTESIAN_POINT('Ctrl Pts',(201.418258065491,10.0828430950021,28.3581992675291));
#78815=CARTESIAN_POINT('Ctrl Pts',(201.415254515775,10.0403071634838,28.3937061786499));
#78816=CARTESIAN_POINT('Ctrl Pts',(201.412250966059,9.99989423328979,28.431533479517));
#78817=CARTESIAN_POINT('Ctrl Pts',(201.409249172153,9.95950492762379,28.4693386673593));
#78818=CARTESIAN_POINT('Ctrl Pts',(201.406247378247,9.92123654752231,28.5094611964513));
#78819=CARTESIAN_POINT('Ctrl Pts',(201.403245584341,9.88535817030107,28.5516299026828));
#78820=CARTESIAN_POINT('Ctrl Pts',(201.400244363608,9.84948664381794,28.5937905570796));
#78821=CARTESIAN_POINT('Ctrl Pts',(201.397243142875,9.81600455531122,28.6379962110796));
#78822=CARTESIAN_POINT('Ctrl Pts',(201.394241922142,9.78514162666474,28.6839415567882));
#78823=CARTESIAN_POINT('Ctrl Pts',(201.3912379575,9.75425048115431,28.7299289086715));
#78824=CARTESIAN_POINT('Ctrl Pts',(201.388233992859,9.72598357383232,28.7776586909242));
#78825=CARTESIAN_POINT('Ctrl Pts',(201.385230028218,9.70052719713442,28.8267966988995));
#78826=CARTESIAN_POINT('Ctrl Pts',(201.382224679043,9.67505908753884,28.8759573546861));
#78827=CARTESIAN_POINT('Ctrl Pts',(201.379219329868,9.65240430669399,28.9265270478923));
#78828=CARTESIAN_POINT('Ctrl Pts',(201.376213980694,9.63270161626161,28.9781500408869));
#78829=CARTESIAN_POINT('Ctrl Pts',(201.373203058826,9.61296239195937,29.0298687562252));
#78830=CARTESIAN_POINT('Ctrl Pts',(201.370192136959,9.59618635228284,29.0826441689016));
#78831=CARTESIAN_POINT('Ctrl Pts',(201.367181215092,9.58246247839736,29.1361049260451));
#78832=CARTESIAN_POINT('Ctrl Pts',(201.365008995715,9.57256143609598,29.1746740080957));
#78833=CARTESIAN_POINT('Ctrl Pts',(201.362836776339,9.56424793889115,29.2135994925215));
#78834=CARTESIAN_POINT('Ctrl Pts',(201.360664556962,9.55753867729102,29.2527398485629));
#78835=CARTESIAN_POINT('Ctrl Pts',(201.356161386589,9.54362988502569,29.3338806825054));
#78836=CARTESIAN_POINT('Ctrl Pts',(201.351658216216,9.53656559886766,29.4162266799627));
#78837=CARTESIAN_POINT('Ctrl Pts',(201.347155045843,9.53650045493221,29.498846056164));
#78838=CARTESIAN_POINT('',(200.847155045799,9.5365000165217,29.5002199068106));
#78839=CARTESIAN_POINT('Ctrl Pts',(201.347155045797,9.53650045493154,29.498846057016));
#78840=CARTESIAN_POINT('Ctrl Pts',(201.344192093687,9.53645759219208,29.553207148138));
#78841=CARTESIAN_POINT('Ctrl Pts',(201.341229141578,9.53944780435113,29.6076722695148));
#78842=CARTESIAN_POINT('Ctrl Pts',(201.338266189469,9.54547934964435,29.661870095104));
#78843=CARTESIAN_POINT('Ctrl Pts',(201.335306223428,9.55150481633468,29.7160133000208));
#78844=CARTESIAN_POINT('Ctrl Pts',(201.332346257388,9.56056549112173,29.7698892039572));
#78845=CARTESIAN_POINT('Ctrl Pts',(201.329386291347,9.57261762047123,29.8231281365198));
#78846=CARTESIAN_POINT('Ctrl Pts',(201.326428059793,9.58466268749527,29.8763358720502));
#78847=CARTESIAN_POINT('Ctrl Pts',(201.323469828238,9.59969561773625,29.9289068453346));
#78848=CARTESIAN_POINT('Ctrl Pts',(201.320511596683,9.6176214115198,29.9804806844312));
#78849=CARTESIAN_POINT('Ctrl Pts',(201.31755385102,9.63554426097183,30.0320460524675));
#78850=CARTESIAN_POINT('Ctrl Pts',(201.314596105358,9.65635885098129,30.0826140977086));
#78851=CARTESIAN_POINT('Ctrl Pts',(201.311638359696,9.67992084960482,30.1318411878724));
#78852=CARTESIAN_POINT('Ctrl Pts',(201.308677930102,9.70350422897435,30.1811129479271));
#78853=CARTESIAN_POINT('Ctrl Pts',(201.305717500507,9.72983975539072,30.2290408332694));
#78854=CARTESIAN_POINT('Ctrl Pts',(201.302757070913,9.75873639576856,30.2753044013872));
#78855=CARTESIAN_POINT('Ctrl Pts',(201.299795054642,9.78764852363554,30.3215927650002));
#78856=CARTESIAN_POINT('Ctrl Pts',(201.296833038371,9.81912418044058,30.3662145931671));
#78857=CARTESIAN_POINT('Ctrl Pts',(201.2938710221,9.85293006357957,30.4088799761027));
#78858=CARTESIAN_POINT('Ctrl Pts',(201.290903953149,9.88679361362549,30.4516181386978));
#78859=CARTESIAN_POINT('Ctrl Pts',(201.287936884198,9.9229949535335,30.4923927964874));
#78860=CARTESIAN_POINT('Ctrl Pts',(201.284969815247,9.96126292918511,30.5309498279329));
#78861=CARTESIAN_POINT('Ctrl Pts',(201.28398409624,9.97397630779195,30.5437592365932));
#78862=CARTESIAN_POINT('Ctrl Pts',(201.282998377234,9.98691750783958,30.5563242146305));
#78863=CARTESIAN_POINT('Ctrl Pts',(201.282012658228,10.000075815232,30.568636455824));
#78864=CARTESIAN_POINT('Ctrl Pts',(201.279000868847,10.040280021733,30.6062555714649));
#78865=CARTESIAN_POINT('Ctrl Pts',(201.275989079466,10.0826934464971,30.6416806491432));
#78866=CARTESIAN_POINT('Ctrl Pts',(201.272977290085,10.1270472744573,30.6746428346385));
#78867=CARTESIAN_POINT('Ctrl Pts',(201.269970799303,10.1713230713445,30.7075470302191));
#78868=CARTESIAN_POINT('Ctrl Pts',(201.266964308521,10.2175320766006,30.7379966206306));
#78869=CARTESIAN_POINT('Ctrl Pts',(201.263957817739,10.2653708121964,30.7657615124608));
#78870=CARTESIAN_POINT('Ctrl Pts',(201.260954268023,10.31316275009,30.7934992435995));
#78871=CARTESIAN_POINT('Ctrl Pts',(201.257950718307,10.362580805985,30.8185572155652));
#78872=CARTESIAN_POINT('Ctrl Pts',(201.254947168591,10.4132923368601,30.8407484357675));
#78873=CARTESIAN_POINT('Ctrl Pts',(201.251945374685,10.4639742228671,30.8629266834606));
#78874=CARTESIAN_POINT('Ctrl Pts',(201.248943580779,10.5159476027901,30.8822412902575));
#78875=CARTESIAN_POINT('Ctrl Pts',(201.245941786873,10.5688570954449,30.8985521248247));
#78876=CARTESIAN_POINT('Ctrl Pts',(201.24294056614,10.621756485383,30.9148598449463));
#78877=CARTESIAN_POINT('Ctrl Pts',(201.239939345407,10.6755911292852,30.9281647768232));
#78878=CARTESIAN_POINT('Ctrl Pts',(201.236938124674,10.7299898178405,30.9383764290095));
#78879=CARTESIAN_POINT('Ctrl Pts',(201.233934160032,10.7844382411575,30.9485974173417));
#78880=CARTESIAN_POINT('Ctrl Pts',(201.230930195391,10.8394512198701,30.9557193789124));
#78881=CARTESIAN_POINT('Ctrl Pts',(201.22792623075,10.8946481459147,30.9597031331202));
#78882=CARTESIAN_POINT('Ctrl Pts',(201.224920881575,10.9498705123389,30.9636887234486));
#78883=CARTESIAN_POINT('Ctrl Pts',(201.2219155324,11.0052764668911,30.9645332151621));
#78884=CARTESIAN_POINT('Ctrl Pts',(201.218910183226,11.0604843876251,30.9622495986847));
#78885=CARTESIAN_POINT('Ctrl Pts',(201.215899261358,11.1157946780836,30.9599617477934));
#78886=CARTESIAN_POINT('Ctrl Pts',(201.212888339491,11.170905675232,30.9545342544754));
#78887=CARTESIAN_POINT('Ctrl Pts',(201.209877417624,11.2254410684357,30.9460320102482));
#78888=CARTESIAN_POINT('Ctrl Pts',(201.207705198247,11.2647854430297,30.9398980949666));
#78889=CARTESIAN_POINT('Ctrl Pts',(201.205532978871,11.303830359524,30.9321649151874));
#78890=CARTESIAN_POINT('Ctrl Pts',(201.203360759494,11.3424391984059,30.922873025043));
#78891=CARTESIAN_POINT('Ctrl Pts',(201.200348970113,11.3959704817639,30.9099897884927));
#78892=CARTESIAN_POINT('Ctrl Pts',(201.197337180732,11.4488846450223,30.8940547310599));
#78893=CARTESIAN_POINT('Ctrl Pts',(201.194325391351,11.5008092975111,30.8751444642387));
#78894=CARTESIAN_POINT('Ctrl Pts',(201.191318900569,11.5526425996807,30.8562674659871));
#78895=CARTESIAN_POINT('Ctrl Pts',(201.188312409787,11.6034893542792,30.8344258252572));
#78896=CARTESIAN_POINT('Ctrl Pts',(201.185305919005,11.6529904744886,30.8097464221089));
#78897=CARTESIAN_POINT('Ctrl Pts',(201.182302369289,11.7024431707867,30.7850911613078));
#78898=CARTESIAN_POINT('Ctrl Pts',(201.179298819573,11.7505523707667,30.7576038717952));
#78899=CARTESIAN_POINT('Ctrl Pts',(201.176295269857,11.7969789401109,30.7274594979142));
#78900=CARTESIAN_POINT('Ctrl Pts',(201.173293475951,11.8433783694832,30.6973327457845));
#78901=CARTESIAN_POINT('Ctrl Pts',(201.170291682045,11.888096676508,30.6645522748734));
#78902=CARTESIAN_POINT('Ctrl Pts',(201.167289888139,11.9308213549158,30.6293377950077));
#78903=CARTESIAN_POINT('Ctrl Pts',(201.164288667406,11.9735378753296,30.5941300391133));
#78904=CARTESIAN_POINT('Ctrl Pts',(201.161287446673,12.0142611165139,30.5564895326906));
#78905=CARTESIAN_POINT('Ctrl Pts',(201.15828622594,12.0527113216486,30.5166765086658));
#78906=CARTESIAN_POINT('Ctrl Pts',(201.155282261299,12.091196680421,30.4768270850271));
#78907=CARTESIAN_POINT('Ctrl Pts',(201.152278296657,12.1274044845283,30.4348015560576));
#78908=CARTESIAN_POINT('Ctrl Pts',(201.149274332016,12.161092658561,30.3908962275348));
#78909=CARTESIAN_POINT('Ctrl Pts',(201.146268982841,12.1947963595441,30.3469706629535));
#78910=CARTESIAN_POINT('Ctrl Pts',(201.143263633666,12.2259778183005,30.3011640084597));
#78911=CARTESIAN_POINT('Ctrl Pts',(201.140258284492,12.2544379713151,30.2538021133712));
#78912=CARTESIAN_POINT('Ctrl Pts',(201.137247362624,12.2829508967939,30.2063523971135));
#78913=CARTESIAN_POINT('Ctrl Pts',(201.134236440757,12.3087321911588,30.1573421476625));
#78914=CARTESIAN_POINT('Ctrl Pts',(201.131225518889,12.3316290565517,30.1071213270404));
#78915=CARTESIAN_POINT('Ctrl Pts',(201.129053299513,12.3481479224871,30.0708896862116));
#78916=CARTESIAN_POINT('Ctrl Pts',(201.126881080136,12.3631664770608,30.0340284519386));
#78917=CARTESIAN_POINT('Ctrl Pts',(201.12470886076,12.3766434403009,29.9966740261746));
#78918=CARTESIAN_POINT('Ctrl Pts',(201.121697071379,12.3953292945997,29.9448819907726));
#78919=CARTESIAN_POINT('Ctrl Pts',(201.118685281998,12.4111270334017,29.8919266683069));
#78920=CARTESIAN_POINT('Ctrl Pts',(201.115673492617,12.4238958027391,29.8381611937258));
#78921=CARTESIAN_POINT('Ctrl Pts',(201.112667001835,12.436642108158,29.7844903079966));
#78922=CARTESIAN_POINT('Ctrl Pts',(201.109660511053,12.4463698987706,29.7300126078546));
#78923=CARTESIAN_POINT('Ctrl Pts',(201.106654020271,12.4529876192118,29.6750977681673));
#78924=CARTESIAN_POINT('Ctrl Pts',(201.103650470555,12.4595988659429,29.620236648301));
#78925=CARTESIAN_POINT('Ctrl Pts',(201.100646920838,12.4631060069446,29.5649397571637));
#78926=CARTESIAN_POINT('Ctrl Pts',(201.097643371122,12.4634686017004,29.509586544585));
#78927=CARTESIAN_POINT('Ctrl Pts',(201.094641577216,12.4638309844912,29.4542656903015));
#78928=CARTESIAN_POINT('Ctrl Pts',(201.09163978331,12.4610524613765,29.3988891062102));
#78929=CARTESIAN_POINT('Ctrl Pts',(201.088637989405,12.4551446236655,29.3438386276398));
#78930=CARTESIAN_POINT('Ctrl Pts',(201.085636768671,12.4492379140169,29.2887986605932));
#78931=CARTESIAN_POINT('Ctrl Pts',(201.082635547938,12.440203132903,29.2340851994841));
#78932=CARTESIAN_POINT('Ctrl Pts',(201.079634327205,12.4281037276099,29.1800750194395));
#78933=CARTESIAN_POINT('Ctrl Pts',(201.076630362564,12.4159932602664,29.1260154598326));
#78934=CARTESIAN_POINT('Ctrl Pts',(201.073626397923,12.4008126870476,29.072660981481));
#78935=CARTESIAN_POINT('Ctrl Pts',(201.070622433281,12.3826763075204,29.0203767326102));
#78936=CARTESIAN_POINT('Ctrl Pts',(201.067617084106,12.3645315688977,28.9680683858188));
#78937=CARTESIAN_POINT('Ctrl Pts',(201.064611734932,12.3434285095276,28.916831740229));
#78938=CARTESIAN_POINT('Ctrl Pts',(201.061606385757,12.319529760483,28.8670122740529));
#78939=CARTESIAN_POINT('Ctrl Pts',(201.058595463889,12.2955866969936,28.8171004297369));
#78940=CARTESIAN_POINT('Ctrl Pts',(201.055584542022,12.2688378443226,28.7686114766531));
#78941=CARTESIAN_POINT('Ctrl Pts',(201.052573620155,12.2394914193359,28.72186551844));
#78942=CARTESIAN_POINT('Ctrl Pts',(201.050401400778,12.21831954049,28.6881408053184));
#78943=CARTESIAN_POINT('Ctrl Pts',(201.048229181402,12.1957966189195,28.6553227374654));
#78944=CARTESIAN_POINT('Ctrl Pts',(201.046056962025,12.1720138618117,28.6235208172916));
#78945=CARTESIAN_POINT('Ctrl Pts',(201.043045172644,12.1390389900826,28.5794273493344));
#78946=CARTESIAN_POINT('Ctrl Pts',(201.040033383263,12.1035040066266,28.5371059637289));
#78947=CARTESIAN_POINT('Ctrl Pts',(201.037021593882,12.0656263478846,28.4968685346904));
#78948=CARTESIAN_POINT('Ctrl Pts',(201.0340151031,12.027815326781,28.4567018948014));
#78949=CARTESIAN_POINT('Ctrl Pts',(201.031008612318,11.9876701684204,28.4186123163942));
#78950=CARTESIAN_POINT('Ctrl Pts',(201.028002121536,11.9454492390576,28.3828796007747));
#78951=CARTESIAN_POINT('Ctrl Pts',(201.02499857182,11.9032696118417,28.3471818402802));
#78952=CARTESIAN_POINT('Ctrl Pts',(201.021995022103,11.8590186370682,28.3138367141126));
#78953=CARTESIAN_POINT('Ctrl Pts',(201.018991472387,11.8129909602191,28.2830867127843));
#78954=CARTESIAN_POINT('Ctrl Pts',(201.015989678481,11.7669901901578,28.2523546872441));
#78955=CARTESIAN_POINT('Ctrl Pts',(201.012987884575,11.7192152144912,28.2242150718159));
#78956=CARTESIAN_POINT('Ctrl Pts',(201.00998609067,11.669991291152,28.1988682158288));
#78957=CARTESIAN_POINT('Ctrl Pts',(201.006984869936,11.6207767667944,28.1735261996557));
#78958=CARTESIAN_POINT('Ctrl Pts',(201.003983649203,11.5701143129518,28.1509761249983));
#78959=CARTESIAN_POINT('Ctrl Pts',(201.00098242847,11.5183534851549,28.1313722513306));
#78960=CARTESIAN_POINT('Ctrl Pts',(200.997978463829,11.4665453342977,28.1117504545474));
#78961=CARTESIAN_POINT('Ctrl Pts',(200.994974499188,11.4136372976572,28.0950804268823));
#78962=CARTESIAN_POINT('Ctrl Pts',(200.991970534546,11.3599971922288,28.0814675641398));
#78963=CARTESIAN_POINT('Ctrl Pts',(200.988965185372,11.3063323639627,28.0678484272002));
#78964=CARTESIAN_POINT('Ctrl Pts',(200.985959836197,11.2519353129124,28.0572893645905));
#78965=CARTESIAN_POINT('Ctrl Pts',(200.982954487022,11.1971840139354,28.0498445894842));
#78966=CARTESIAN_POINT('Ctrl Pts',(200.979943565154,11.1423311919285,28.0423860098447));
#78967=CARTESIAN_POINT('Ctrl Pts',(200.976932643287,11.0871233368434,28.0380532939104));
#78968=CARTESIAN_POINT('Ctrl Pts',(200.97392172142,11.0319423070637,28.0368486274416));
#78969=CARTESIAN_POINT('Ctrl Pts',(200.971749502044,10.9921321401553,28.0359795249007));
#78970=CARTESIAN_POINT('Ctrl Pts',(200.969577282667,10.9523359950373,28.0367374212764));
#78971=CARTESIAN_POINT('Ctrl Pts',(200.967405063291,10.9126954892126,28.0391063788228));
#78972=CARTESIAN_POINT('Ctrl Pts',(200.96439327391,10.8577337962055,28.0423909463303));
#78973=CARTESIAN_POINT('Ctrl Pts',(200.961381484529,10.8028438256294,28.0487882784945));
#78974=CARTESIAN_POINT('Ctrl Pts',(200.958369695148,10.7484056344831,28.0582883349157));
#78975=CARTESIAN_POINT('Ctrl Pts',(200.955363204366,10.6940632156898,28.0677716780196));
#78976=CARTESIAN_POINT('Ctrl Pts',(200.952356713584,10.6401715144009,28.0803468223565));
#78977=CARTESIAN_POINT('Ctrl Pts',(200.949350222803,10.5871063161268,28.0959519040227));
#78978=CARTESIAN_POINT('Ctrl Pts',(200.946346673086,10.534093028283,28.111541720194));
#78979=CARTESIAN_POINT('Ctrl Pts',(200.94334312337,10.4819051452679,28.1301554536672));
#78980=CARTESIAN_POINT('Ctrl Pts',(200.940339573654,10.4309072487217,28.1516804197659));
#78981=CARTESIAN_POINT('Ctrl Pts',(200.937337779748,10.3799391644468,28.1731928028335));
#78982=CARTESIAN_POINT('Ctrl Pts',(200.934335985842,10.330160172681,28.1976128404063));
#78983=CARTESIAN_POINT('Ctrl Pts',(200.931334191937,10.2819165001657,28.2247791025607));
#78984=CARTESIAN_POINT('Ctrl Pts',(200.928332971203,10.2336820394597,28.2519401774976));
#78985=CARTESIAN_POINT('Ctrl Pts',(200.92533175047,10.1869827749869,28.281846176795));
#78986=CARTESIAN_POINT('Ctrl Pts',(200.922330529737,10.1421398074332,28.3142900270263));
#78987=CARTESIAN_POINT('Ctrl Pts',(200.919326565096,10.0972558415695,28.3467635395012));
#78988=CARTESIAN_POINT('Ctrl Pts',(200.916322600455,10.0542319911496,28.3817792282481));
#78989=CARTESIAN_POINT('Ctrl Pts',(200.913318635814,10.0133585941167,28.4190878915487));
#78990=CARTESIAN_POINT('Ctrl Pts',(200.910313286639,9.97246635844887,28.456413750491));
#78991=CARTESIAN_POINT('Ctrl Pts',(200.907307937464,9.93372692119503,28.4960343129212));
#78992=CARTESIAN_POINT('Ctrl Pts',(200.904302588289,9.89739346351284,28.5376637408391));
#78993=CARTESIAN_POINT('Ctrl Pts',(200.901291666422,9.86099263422881,28.5793703604537));
#78994=CARTESIAN_POINT('Ctrl Pts',(200.898280744555,9.8270070202741,28.6230928687812));
#78995=CARTESIAN_POINT('Ctrl Pts',(200.895269822687,9.79564848930181,28.6685135667499));
#78996=CARTESIAN_POINT('Ctrl Pts',(200.89309760331,9.77302498340972,28.7012821753632));
#78997=CARTESIAN_POINT('Ctrl Pts',(200.890925383934,9.75176794569159,28.7349340092125));
#78998=CARTESIAN_POINT('Ctrl Pts',(200.888753164557,9.73194196315828,28.7693420326848));
#78999=CARTESIAN_POINT('Ctrl Pts',(200.885626860487,9.70340798977802,28.8188627877939));
#79000=CARTESIAN_POINT('Ctrl Pts',(200.882500556418,9.67772949073588,28.8701424352536));
#79001=CARTESIAN_POINT('Ctrl Pts',(200.879374252349,9.65511699549504,28.9228328195456));
#79002=CARTESIAN_POINT('Ctrl Pts',(200.876256197382,9.63256416585403,28.9753841743607));
#79003=CARTESIAN_POINT('Ctrl Pts',(200.873138142416,9.61306143181151,29.0293384316797));
#79004=CARTESIAN_POINT('Ctrl Pts',(200.87002008745,9.59677327652103,29.0843234279942));
#79005=CARTESIAN_POINT('Ctrl Pts',(200.86690698055,9.58051096903304,29.1392211681831));
#79006=CARTESIAN_POINT('Ctrl Pts',(200.86379387365,9.56745324435004,29.1951459509428));
#79007=CARTESIAN_POINT('Ctrl Pts',(200.86068076675,9.55771612755834,29.2517068641813));
#79008=CARTESIAN_POINT('Ctrl Pts',(200.857572952157,9.54799556394529,29.3081716234019));
#79009=CARTESIAN_POINT('Ctrl Pts',(200.854465137565,9.54158446134469,29.3652699002605));
#79010=CARTESIAN_POINT('Ctrl Pts',(200.851357322972,9.53854821497931,29.42259890143));
#79011=CARTESIAN_POINT('Ctrl Pts',(200.849956563929,9.53717971327944,29.4484383182992));
#79012=CARTESIAN_POINT('Ctrl Pts',(200.848555804886,9.5364961254632,29.4743244608338));
#79013=CARTESIAN_POINT('Ctrl Pts',(200.847155045843,9.53650001652158,29.5002199060039));
#79014=CARTESIAN_POINT('',(200.347155045877,9.53650026306434,29.5008774903221));
#79015=CARTESIAN_POINT('Ctrl Pts',(200.847155045799,9.5365000165217,29.5002199068106));
#79016=CARTESIAN_POINT('Ctrl Pts',(200.84396942673,9.53650886563482,29.55911156583));
#79017=CARTESIAN_POINT('Ctrl Pts',(200.840783807662,9.54007672876269,29.6179197105645));
#79018=CARTESIAN_POINT('Ctrl Pts',(200.837598188593,9.54714789381235,29.6762186356379));
#79019=CARTESIAN_POINT('Ctrl Pts',(200.834406499263,9.55423253310804,29.7346286504759));
#79020=CARTESIAN_POINT('Ctrl Pts',(200.831214809934,9.56483370669795,29.7925270926805));
#79021=CARTESIAN_POINT('Ctrl Pts',(200.828023120604,9.5788446640183,29.8494993004439));
#79022=CARTESIAN_POINT('Ctrl Pts',(200.824820092136,9.59290539816992,29.9066739137893));
#79023=CARTESIAN_POINT('Ctrl Pts',(200.821617063669,9.61040001838629,29.9629153027575));
#79024=CARTESIAN_POINT('Ctrl Pts',(200.818414035201,9.63117184102155,30.0178240253094));
#79025=CARTESIAN_POINT('Ctrl Pts',(200.815643112075,9.64914143582681,30.065325273171));
#79026=CARTESIAN_POINT('Ctrl Pts',(200.812872188948,9.66956278947609,30.1118293448901));
#79027=CARTESIAN_POINT('Ctrl Pts',(200.810101265822,9.69230685329164,30.1570927514834));
#79028=CARTESIAN_POINT('Ctrl Pts',(200.807089476441,9.71702797573658,30.2062907411541));
#79029=CARTESIAN_POINT('Ctrl Pts',(200.80407768706,9.74458056961052,30.2541936565157));
#79030=CARTESIAN_POINT('Ctrl Pts',(200.801065897678,9.77480533209191,30.3004562922044));
#79031=CARTESIAN_POINT('Ctrl Pts',(200.798059406896,9.80497692056885,30.3466375386813));
#79032=CARTESIAN_POINT('Ctrl Pts',(200.795052916114,9.83781106166955,30.3911837944356));
#79033=CARTESIAN_POINT('Ctrl Pts',(200.792046425332,9.8731025274536,30.4337742427207));
#79034=CARTESIAN_POINT('Ctrl Pts',(200.789042875615,9.90835946976022,30.4763230273812));
#79035=CARTESIAN_POINT('Ctrl Pts',(200.786039325899,9.94606863962023,30.516919390722));
#79036=CARTESIAN_POINT('Ctrl Pts',(200.783035776182,9.98598254270118,30.555272877645));
#79037=CARTESIAN_POINT('Ctrl Pts',(200.780033982276,10.0258731129746,30.5936039439462));
#79038=CARTESIAN_POINT('Ctrl Pts',(200.77703218837,10.067965482149,30.6296943680802));
#79039=CARTESIAN_POINT('Ctrl Pts',(200.774030394464,10.111974620175,30.6632898068782));
#79040=CARTESIAN_POINT('Ctrl Pts',(200.771029173731,10.155975354948,30.69687883085));
#79041=CARTESIAN_POINT('Ctrl Pts',(200.768027952997,10.2018917125966,30.7279734959418));
#79042=CARTESIAN_POINT('Ctrl Pts',(200.765026732264,10.2494066508443,30.7563605669565));
#79043=CARTESIAN_POINT('Ctrl Pts',(200.762022767622,10.2969650302885,30.7847735912477));
#79044=CARTESIAN_POINT('Ctrl Pts',(200.759018802981,10.3461244562801,30.8104738052582));
#79045=CARTESIAN_POINT('Ctrl Pts',(200.756014838339,10.396541329686,30.8332928722613));
#79046=CARTESIAN_POINT('Ctrl Pts',(200.753009489164,10.4469814403351,30.8561224566205));
#79047=CARTESIAN_POINT('Ctrl Pts',(200.750004139989,10.4986796608108,30.8760680567951));
#79048=CARTESIAN_POINT('Ctrl Pts',(200.746998790814,10.5512734057079,30.8930099402283));
#79049=CARTESIAN_POINT('Ctrl Pts',(200.743987868947,10.6039646729731,30.9099832382832));
#79050=CARTESIAN_POINT('Ctrl Pts',(200.740976947079,10.6575542700626,30.9239415610611));
#79051=CARTESIAN_POINT('Ctrl Pts',(200.737966025212,10.7116666538547,30.9348157134283));
#79052=CARTESIAN_POINT('Ctrl Pts',(200.735793805837,10.7507058496962,30.9426608337893));
#79053=CARTESIAN_POINT('Ctrl Pts',(200.733621586463,10.7900168956643,30.9489017660119));
#79054=CARTESIAN_POINT('Ctrl Pts',(200.731449367089,10.8294575758292,30.9535293363252));
#79055=CARTESIAN_POINT('Ctrl Pts',(200.728437577709,10.8841422099411,30.9599454779422));
#79056=CARTESIAN_POINT('Ctrl Pts',(200.725425788328,10.9393027474571,30.9632846138945));
#79057=CARTESIAN_POINT('Ctrl Pts',(200.722413998947,10.9945632720978,30.9634899015674));
#79058=CARTESIAN_POINT('Ctrl Pts',(200.719407508166,11.0497265776658,30.9636948280805));
#79059=CARTESIAN_POINT('Ctrl Pts',(200.716401017385,11.1049889980205,30.9607768461116));
#79060=CARTESIAN_POINT('Ctrl Pts',(200.713394526603,11.1599697233074,30.9547308815121));
#79061=CARTESIAN_POINT('Ctrl Pts',(200.710390976887,11.2148966643214,30.9486908313091));
#79062=CARTESIAN_POINT('Ctrl Pts',(200.707387427171,11.2695419344519,30.9395289178023));
#79063=CARTESIAN_POINT('Ctrl Pts',(200.704383877456,11.3235268310191,30.9272920652798));
#79064=CARTESIAN_POINT('Ctrl Pts',(200.70138208355,11.3774801691792,30.9150623661576));
#79065=CARTESIAN_POINT('Ctrl Pts',(200.698380289645,11.4307733856348,30.8997614075139));
#79066=CARTESIAN_POINT('Ctrl Pts',(200.695378495739,11.4830372892332,30.8814873243031));
#79067=CARTESIAN_POINT('Ctrl Pts',(200.692377275006,11.5352912133859,30.8632167304073));
#79068=CARTESIAN_POINT('Ctrl Pts',(200.689376054274,11.5865157175064,30.8419743135672));
#79069=CARTESIAN_POINT('Ctrl Pts',(200.686374833541,11.6363583325243,30.8179075546588));
#79070=CARTESIAN_POINT('Ctrl Pts',(200.6833708689,11.68624651685,30.7938187923797));
#79071=CARTESIAN_POINT('Ctrl Pts',(200.680366904259,11.7347498122671,30.7669007594579));
#79072=CARTESIAN_POINT('Ctrl Pts',(200.677362939618,11.7815386380886,30.7373478117226));
#79073=CARTESIAN_POINT('Ctrl Pts',(200.674357590444,11.8283490289786,30.7077812429713));
#79074=CARTESIAN_POINT('Ctrl Pts',(200.671352241269,11.8734429452229,30.675577645609));
#79075=CARTESIAN_POINT('Ctrl Pts',(200.668346892095,11.9165209534788,30.6409739663263));
#79076=CARTESIAN_POINT('Ctrl Pts',(200.665335970228,11.9596788394731,30.6063061228969));
#79077=CARTESIAN_POINT('Ctrl Pts',(200.662325048361,12.0008129582586,30.5692296618826));
#79078=CARTESIAN_POINT('Ctrl Pts',(200.659314126494,12.039658954378,30.5300201495998));
#79079=CARTESIAN_POINT('Ctrl Pts',(200.657141907114,12.0676842666655,30.5017325798079));
#79080=CARTESIAN_POINT('Ctrl Pts',(200.654969687734,12.0945194053748,30.4723355917197));
#79081=CARTESIAN_POINT('Ctrl Pts',(200.652797468355,12.1200784829496,30.4419429080541));
#79082=CARTESIAN_POINT('Ctrl Pts',(200.649785678974,12.1555162288508,30.3998033512626));
#79083=CARTESIAN_POINT('Ctrl Pts',(200.646773889593,12.1886460472905,30.3555738378347));
#79084=CARTESIAN_POINT('Ctrl Pts',(200.643762100212,12.2192136935125,30.3095370402592));
#79085=CARTESIAN_POINT('Ctrl Pts',(200.640755609431,12.2497275624994,30.2635812345818));
#79086=CARTESIAN_POINT('Ctrl Pts',(200.637749118649,12.2776879155885,30.215824890738));
#79087=CARTESIAN_POINT('Ctrl Pts',(200.634742627868,12.3028810496936,30.1665832433757));
#79088=CARTESIAN_POINT('Ctrl Pts',(200.631739078152,12.3280495389001,30.1173897660983));
#79089=CARTESIAN_POINT('Ctrl Pts',(200.628735528436,12.3504559328577,30.0667143310579));
#79090=CARTESIAN_POINT('Ctrl Pts',(200.62573197872,12.3699311129871,30.0148990150214));
#79091=CARTESIAN_POINT('Ctrl Pts',(200.622730184815,12.3893949083458,29.9631139891021));
#79092=CARTESIAN_POINT('Ctrl Pts',(200.619728390909,12.4059307012672,29.9101908957679));
#79093=CARTESIAN_POINT('Ctrl Pts',(200.616726597004,12.4194173725723,29.8564920369937));
#79094=CARTESIAN_POINT('Ctrl Pts',(200.613725376271,12.432901468687,29.8028034316604));
#79095=CARTESIAN_POINT('Ctrl Pts',(200.610724155538,12.4433374712575,29.7483398663532));
#79096=CARTESIAN_POINT('Ctrl Pts',(200.607722934805,12.450654669387,29.6934768207966));
#79097=CARTESIAN_POINT('Ctrl Pts',(200.604718970164,12.4579785573673,29.6385636159337));
#79098=CARTESIAN_POINT('Ctrl Pts',(200.601715005523,12.4621778748553,29.583250725073));
#79099=CARTESIAN_POINT('Ctrl Pts',(200.598711040883,12.4632336474477,29.5279202968632));
#79100=CARTESIAN_POINT('Ctrl Pts',(200.595705691708,12.4642899066479,29.4725643667424));
#79101=CARTESIAN_POINT('Ctrl Pts',(200.592700342534,12.4621997527736,29.4171914110496));
#79102=CARTESIAN_POINT('Ctrl Pts',(200.589694993359,12.456996362954,29.3621818287057));
#79103=CARTESIAN_POINT('Ctrl Pts',(200.586684071492,12.4517833247075,29.3070702444078));
#79104=CARTESIAN_POINT('Ctrl Pts',(200.583673149625,12.443445599141,29.2523239018628));
#79105=CARTESIAN_POINT('Ctrl Pts',(200.580662227758,12.4320679104757,29.1983151482327));
#79106=CARTESIAN_POINT('Ctrl Pts',(200.578490008379,12.4238595155374,29.1593507159164));
#79107=CARTESIAN_POINT('Ctrl Pts',(200.576317788999,12.4140699539376,29.1207699945449));
#79108=CARTESIAN_POINT('Ctrl Pts',(200.57414556962,12.4027469562315,29.0827072648808));
#79109=CARTESIAN_POINT('Ctrl Pts',(200.571133780236,12.3870475823078,29.0299331637935));
#79110=CARTESIAN_POINT('Ctrl Pts',(200.568121990853,12.3683333412133,28.9779368955227));
#79111=CARTESIAN_POINT('Ctrl Pts',(200.565110201469,12.346700453166,28.9270862722516));
#79112=CARTESIAN_POINT('Ctrl Pts',(200.562103710685,12.3251056235578,28.8763251097748));
#79113=CARTESIAN_POINT('Ctrl Pts',(200.5590972199,12.3006025422001,28.8267060737916));
#79114=CARTESIAN_POINT('Ctrl Pts',(200.556090729116,12.2733369230014,28.7785810298299));
#79115=CARTESIAN_POINT('Ctrl Pts',(200.553087179397,12.2460979760864,28.7305030636483));
#79116=CARTESIAN_POINT('Ctrl Pts',(200.550083629678,12.2161021037954,28.6839166508456));
#79117=CARTESIAN_POINT('Ctrl Pts',(200.547080079959,12.1835419605243,28.6391511876768));
#79118=CARTESIAN_POINT('Ctrl Pts',(200.544078286051,12.1510008512114,28.5944118934331));
#79119=CARTESIAN_POINT('Ctrl Pts',(200.541076492142,12.1158987519287,28.5514918644598));
#79120=CARTESIAN_POINT('Ctrl Pts',(200.538074698234,12.078471609951,28.5106915362084));
#79121=CARTESIAN_POINT('Ctrl Pts',(200.535073477498,12.0410516144378,28.4698989985091));
#79122=CARTESIAN_POINT('Ctrl Pts',(200.532072256763,12.0013078143925,28.4312257460071));
#79123=CARTESIAN_POINT('Ctrl Pts',(200.529071036027,11.9595148894375,28.3949373651472));
#79124=CARTESIAN_POINT('Ctrl Pts',(200.526067071383,11.917683754717,28.3586158071283));
#79125=CARTESIAN_POINT('Ctrl Pts',(200.523063106739,11.8738001516277,28.324683822981));
#79126=CARTESIAN_POINT('Ctrl Pts',(200.520059142096,11.8281727870113,28.2933674607181));
#79127=CARTESIAN_POINT('Ctrl Pts',(200.517053792918,11.7825243926466,28.262036664678));
#79128=CARTESIAN_POINT('Ctrl Pts',(200.514048443741,11.7351310865055,28.2333241673284));
#79129=CARTESIAN_POINT('Ctrl Pts',(200.511043094564,11.6863288002742,28.2074115009354));
#79130=CARTESIAN_POINT('Ctrl Pts',(200.508032172694,11.6374360220179,28.1814507857758));
#79131=CARTESIAN_POINT('Ctrl Pts',(200.505021250824,11.5871295251715,28.1583004926788));
#79132=CARTESIAN_POINT('Ctrl Pts',(200.502010328954,11.5357668707768,28.1380946764998));
#79133=CARTESIAN_POINT('Ctrl Pts',(200.499838109598,11.4987114582219,28.1235172590485));
#79134=CARTESIAN_POINT('Ctrl Pts',(200.497665890242,11.4611067690704,28.1104713823924));
#79135=CARTESIAN_POINT('Ctrl Pts',(200.495493670886,11.4230911995218,28.0989910468212));
#79136=CARTESIAN_POINT('Ctrl Pts',(200.492481881509,11.3703824856468,28.0830735232907));
#79137=CARTESIAN_POINT('Ctrl Pts',(200.489470092133,11.3166650271965,28.0701016545677));
#79138=CARTESIAN_POINT('Ctrl Pts',(200.486458302756,11.2622989213193,28.0601974003792));
#79139=CARTESIAN_POINT('Ctrl Pts',(200.483451811979,11.2080284609759,28.0503105706073));
#79140=CARTESIAN_POINT('Ctrl Pts',(200.480445321201,11.1531121327064,28.0434807386608));
#79141=CARTESIAN_POINT('Ctrl Pts',(200.477438830424,11.0979239402719,28.0397797591043));
#79142=CARTESIAN_POINT('Ctrl Pts',(200.474435280712,11.0427897350623,28.0360823999891));
#79143=CARTESIAN_POINT('Ctrl Pts',(200.471431731,10.9873847162564,28.0355078647442));
#79144=CARTESIAN_POINT('Ctrl Pts',(200.468428181288,10.9320899425985,28.0380764472437));
#79145=CARTESIAN_POINT('Ctrl Pts',(200.465426387386,10.876827493073,28.0406435282051));
#79146=CARTESIAN_POINT('Ctrl Pts',(200.462424593485,10.821675686762,28.0463500603523));
#79147=CARTESIAN_POINT('Ctrl Pts',(200.459422799583,10.7670152097446,28.0551642524115));
#79148=CARTESIAN_POINT('Ctrl Pts',(200.456421578855,10.712365169782,28.0639767614592));
#79149=CARTESIAN_POINT('Ctrl Pts',(200.453420358126,10.6582067931507,28.0758956678317));
#79150=CARTESIAN_POINT('Ctrl Pts',(200.450419137397,10.6049129673173,28.0908376649207));
#79151=CARTESIAN_POINT('Ctrl Pts',(200.44741517276,10.551570416857,28.10579332294));
#79152=CARTESIAN_POINT('Ctrl Pts',(200.444411208123,10.4990945050881,28.1237774503732));
#79153=CARTESIAN_POINT('Ctrl Pts',(200.441407243486,10.4478438165162,28.1446565752398));
#79154=CARTESIAN_POINT('Ctrl Pts',(200.438401894315,10.3965695063931,28.1655453233395));
#79155=CARTESIAN_POINT('Ctrl Pts',(200.435396545144,10.3465220222501,28.189331501865));
#79156=CARTESIAN_POINT('Ctrl Pts',(200.432391195974,10.2980377472623,28.2158344165446));
#79157=CARTESIAN_POINT('Ctrl Pts',(200.42938027411,10.2494635699212,28.2423864744649));
#79158=CARTESIAN_POINT('Ctrl Pts',(200.426369352247,10.2024588402598,28.2716650514699));
#79159=CARTESIAN_POINT('Ctrl Pts',(200.423358430384,10.1573321889348,28.3034452748852));
#79160=CARTESIAN_POINT('Ctrl Pts',(200.421186210973,10.1247757187265,28.3263730097481));
#79161=CARTESIAN_POINT('Ctrl Pts',(200.419013991563,10.093196152973,28.3506018902364));
#79162=CARTESIAN_POINT('Ctrl Pts',(200.416841772152,10.0626980115527,28.3760350394907));
#79163=CARTESIAN_POINT('Ctrl Pts',(200.413870697636,10.0209838779215,28.4108214801473));
#79164=CARTESIAN_POINT('Ctrl Pts',(200.410899623119,9.98111135542615,28.4480149358457));
#79165=CARTESIAN_POINT('Ctrl Pts',(200.407928548603,9.94337598668605,28.4873905271585));
#79166=CARTESIAN_POINT('Ctrl Pts',(200.404961581688,9.90569278824966,28.5267116805096));
#79167=CARTESIAN_POINT('Ctrl Pts',(200.401994614774,9.87014126963611,28.568208612504));
#79168=CARTESIAN_POINT('Ctrl Pts',(200.399027647859,9.83698355660046,28.6116166354651));
#79169=CARTESIAN_POINT('Ctrl Pts',(200.396063538184,9.80385777500556,28.654982855763));
#79170=CARTESIAN_POINT('Ctrl Pts',(200.393099428508,9.77312156356463,28.7002560946092));
#79171=CARTESIAN_POINT('Ctrl Pts',(200.390135318833,9.74499809966876,28.7471371438536));
#79172=CARTESIAN_POINT('Ctrl Pts',(200.387172820682,9.71688992590959,28.7939927048559));
#79173=CARTESIAN_POINT('Ctrl Pts',(200.384210322531,9.69139196386493,28.8424538795948));
#79174=CARTESIAN_POINT('Ctrl Pts',(200.38124782438,9.66868376907831,28.8921930049066));
#79175=CARTESIAN_POINT('Ctrl Pts',(200.378283897527,9.64596462297552,28.9419561175451));
#79176=CARTESIAN_POINT('Ctrl Pts',(200.375319970673,9.62603816850224,28.9929979224341));
#79177=CARTESIAN_POINT('Ctrl Pts',(200.372356043819,9.60903685951709,29.0449683617396));
#79178=CARTESIAN_POINT('Ctrl Pts',(200.369391528461,9.592032174825,29.0969491200725));
#79179=CARTESIAN_POINT('Ctrl Pts',(200.366427013103,9.57795394172056,29.1498583572275));
#79180=CARTESIAN_POINT('Ctrl Pts',(200.363462497745,9.56688449072814,29.2033315199007));
#79181=CARTESIAN_POINT('Ctrl Pts',(200.36049322523,9.55579727659043,29.2568904909449));
#79182=CARTESIAN_POINT('Ctrl Pts',(200.357523952715,9.54772857477361,29.3110146575876));
#79183=CARTESIAN_POINT('Ctrl Pts',(200.354554680199,9.54270915193531,29.3653313913828));
#79184=CARTESIAN_POINT('Ctrl Pts',(200.352088135425,9.53853956793558,29.410451755107));
#79185=CARTESIAN_POINT('Ctrl Pts',(200.349621590651,9.53647317822599,29.4557047370735));
#79186=CARTESIAN_POINT('Ctrl Pts',(200.347155045877,9.53650026306434,29.5008774903221));
#79187=CARTESIAN_POINT('',(199.847155045885,9.53650055522948,29.4987251837867));
#79188=CARTESIAN_POINT('Ctrl Pts',(200.347155045843,9.53650026306472,29.5008774909522));
#79189=CARTESIAN_POINT('Ctrl Pts',(200.344166655035,9.53653307825662,29.5556074281586));
#79190=CARTESIAN_POINT('Ctrl Pts',(200.341178264226,9.53963588953091,29.6102432280142));
#79191=CARTESIAN_POINT('Ctrl Pts',(200.338189873417,9.54577770069793,29.6645288856481));
#79192=CARTESIAN_POINT('Ctrl Pts',(200.335178084014,9.55196760120643,29.7192395907894));
#79193=CARTESIAN_POINT('Ctrl Pts',(200.332166294612,9.56126210323049,29.7737138691559));
#79194=CARTESIAN_POINT('Ctrl Pts',(200.329154505209,9.57363105838014,29.827572728386));
#79195=CARTESIAN_POINT('Ctrl Pts',(200.326148014405,9.58597825299936,29.8813368344755));
#79196=CARTESIAN_POINT('Ctrl Pts',(200.323141523602,9.60138904926402,29.9344871601829));
#79197=CARTESIAN_POINT('Ctrl Pts',(200.320135032799,9.61978177411941,29.986651722433));
#79198=CARTESIAN_POINT('Ctrl Pts',(200.317131483061,9.63815650649988,30.0387652552906));
#79199=CARTESIAN_POINT('Ctrl Pts',(200.314127933323,9.65950721403042,30.0898944400664));
#79200=CARTESIAN_POINT('Ctrl Pts',(200.311124383585,9.68370206735094,30.1396811725413));
#79201=CARTESIAN_POINT('Ctrl Pts',(200.308122589658,9.70788277688154,30.1894388007652));
#79202=CARTESIAN_POINT('Ctrl Pts',(200.305120795731,9.73490410643084,30.2378550588371));
#79203=CARTESIAN_POINT('Ctrl Pts',(200.302119001804,9.76458652155721,30.2845927525041));
#79204=CARTESIAN_POINT('Ctrl Pts',(200.29911778105,9.79426326902277,30.3313215219176));
#79205=CARTESIAN_POINT('Ctrl Pts',(200.296116560295,9.826599810181,30.3763719186109));
#79206=CARTESIAN_POINT('Ctrl Pts',(200.293115339541,9.86137236140119,30.419434255735));
#79207=CARTESIAN_POINT('Ctrl Pts',(200.290111374879,9.89617670390919,30.4625359631987));
#79208=CARTESIAN_POINT('Ctrl Pts',(200.287107410217,9.93342117357896,30.5036455689202));
#79209=CARTESIAN_POINT('Ctrl Pts',(200.284103445555,9.97284154630521,30.5424863361231));
#79210=CARTESIAN_POINT('Ctrl Pts',(200.281098096359,10.0122800879627,30.5813450051158));
#79211=CARTESIAN_POINT('Ctrl Pts',(200.278092747164,10.0538961350287,30.6179324023142));
#79212=CARTESIAN_POINT('Ctrl Pts',(200.275087397968,10.0973908457618,30.6520108353159));
#79213=CARTESIAN_POINT('Ctrl Pts',(200.272076476081,10.1409662068999,30.6861524585167));
#79214=CARTESIAN_POINT('Ctrl Pts',(200.269065554193,10.1864267560934,30.7177755228739));
#79215=CARTESIAN_POINT('Ctrl Pts',(200.266054632305,10.2334440225545,30.7466852784254));
#79216=CARTESIAN_POINT('Ctrl Pts',(200.263882413099,10.2673644672104,30.7675421218153));
#79217=CARTESIAN_POINT('Ctrl Pts',(200.261710193892,10.3020945507117,30.7869876515616));
#79218=CARTESIAN_POINT('Ctrl Pts',(200.259537974685,10.3375039961018,30.8049640971379));
#79219=CARTESIAN_POINT('Ctrl Pts',(200.256526185348,10.3865993128694,30.829888500223));
#79220=CARTESIAN_POINT('Ctrl Pts',(200.253514396011,10.4372048771768,30.8520901106701));
#79221=CARTESIAN_POINT('Ctrl Pts',(200.250502606675,10.4889875979802,30.8713856405045));
#79222=CARTESIAN_POINT('Ctrl Pts',(200.247496115937,10.5406792181654,30.8906472239825));
#79223=CARTESIAN_POINT('Ctrl Pts',(200.244489625199,10.5935433945327,30.9070126906442));
#79224=CARTESIAN_POINT('Ctrl Pts',(200.241483134461,10.6472245484176,30.9203456377801));
#79225=CARTESIAN_POINT('Ctrl Pts',(200.238479584788,10.7008531893231,30.9336655421118));
#79226=CARTESIAN_POINT('Ctrl Pts',(200.235476035116,10.755296715062,30.9439586773447));
#79227=CARTESIAN_POINT('Ctrl Pts',(200.232472485443,10.8101835490024,30.9511381619028));
#79228=CARTESIAN_POINT('Ctrl Pts',(200.229470691581,10.8650382972867,30.9583134494895));
#79229=CARTESIAN_POINT('Ctrl Pts',(200.226468897718,10.9203353181472,30.9623786261168));
#79230=CARTESIAN_POINT('Ctrl Pts',(200.223467103856,10.9756942571773,30.9632981517332));
#79231=CARTESIAN_POINT('Ctrl Pts',(200.220465883166,11.0310426257912,30.9642175017724));
#79232=CARTESIAN_POINT('Ctrl Pts',(200.217464662476,11.0864523620517,30.961992385128));
#79233=CARTESIAN_POINT('Ctrl Pts',(200.214463441785,11.1415417444191,30.9566393460932));
#79234=CARTESIAN_POINT('Ctrl Pts',(200.211459477186,11.1966814930408,30.951281412966));
#79235=CARTESIAN_POINT('Ctrl Pts',(200.208455512587,11.2514997766515,30.9427898957246));
#79236=CARTESIAN_POINT('Ctrl Pts',(200.205451547988,11.3056201469078,30.9312332359906));
#79237=CARTESIAN_POINT('Ctrl Pts',(200.202446198855,11.3597654613646,30.919671249766));
#79238=CARTESIAN_POINT('Ctrl Pts',(200.199440849722,11.4132117117433,30.9050414444456));
#79239=CARTESIAN_POINT('Ctrl Pts',(200.196435500589,11.4655960152989,30.8874626483397));
#79240=CARTESIAN_POINT('Ctrl Pts',(200.193424578762,11.5180774528864,30.8698512566045));
#79241=CARTESIAN_POINT('Ctrl Pts',(200.190413656936,11.5694925196308,30.8492801478071));
#79242=CARTESIAN_POINT('Ctrl Pts',(200.187402735109,11.6194978977645,30.8259165149682));
#79243=CARTESIAN_POINT('Ctrl Pts',(200.185230515389,11.6555741145356,30.8090608983462));
#79244=CARTESIAN_POINT('Ctrl Pts',(200.183058295669,11.6909170448264,30.7907528304533));
#79245=CARTESIAN_POINT('Ctrl Pts',(200.180886075948,11.7254067834574,30.7710693326935));
#79246=CARTESIAN_POINT('Ctrl Pts',(200.177874286558,11.7732269132098,30.7437781019039));
#79247=CARTESIAN_POINT('Ctrl Pts',(200.174862497168,11.819603873189,30.7137279385383));
#79248=CARTESIAN_POINT('Ctrl Pts',(200.171850707778,11.8642013764692,30.6810961988377));
#79249=CARTESIAN_POINT('Ctrl Pts',(200.168844216988,11.9087204199704,30.6485218677115));
#79250=CARTESIAN_POINT('Ctrl Pts',(200.165837726198,11.9514657974227,30.6133752827255));
#79251=CARTESIAN_POINT('Ctrl Pts',(200.162831235409,11.9921280078101,30.5758783695747));
#79252=CARTESIAN_POINT('Ctrl Pts',(200.159827685685,12.0327504408434,30.5384181373613));
#79253=CARTESIAN_POINT('Ctrl Pts',(200.156824135961,12.0712933580795,30.4986124876854));
#79254=CARTESIAN_POINT('Ctrl Pts',(200.153820586237,12.1074798153552,30.4567239458594));
#79255=CARTESIAN_POINT('Ctrl Pts',(200.150818792324,12.1436451188019,30.4148598911791));
#79256=CARTESIAN_POINT('Ctrl Pts',(200.147816998411,12.177456348763,30.3709157562617));
#79257=CARTESIAN_POINT('Ctrl Pts',(200.144815204499,12.2086746096786,30.325189637549));
#79258=CARTESIAN_POINT('Ctrl Pts',(200.141813983759,12.2398869096691,30.2794722499431));
#79259=CARTESIAN_POINT('Ctrl Pts',(200.138812763019,12.2685069268659,30.2319739897437));
#79260=CARTESIAN_POINT('Ctrl Pts',(200.13581154228,12.294338510907,30.1830227442648));
#79261=CARTESIAN_POINT('Ctrl Pts',(200.132807577633,12.3201937118279,30.1340267444388));
#79262=CARTESIAN_POINT('Ctrl Pts',(200.129803612986,12.3432551401478,30.0835755730157));
#79263=CARTESIAN_POINT('Ctrl Pts',(200.126799648339,12.3633728870516,30.0320212597751));
#79264=CARTESIAN_POINT('Ctrl Pts',(200.123794299159,12.3834999062642,29.9804431850506));
#79265=CARTESIAN_POINT('Ctrl Pts',(200.120788949979,12.4006803757923,29.9277614572397));
#79266=CARTESIAN_POINT('Ctrl Pts',(200.117783600799,12.4148139280457,29.8743444924237));
#79267=CARTESIAN_POINT('Ctrl Pts',(200.114772678927,12.4289736875466,29.8208284787914));
#79268=CARTESIAN_POINT('Ctrl Pts',(200.111761757055,12.4400751384979,29.766575022768));
#79269=CARTESIAN_POINT('Ctrl Pts',(200.108750835183,12.4480690658949,29.7119628042802));
#79270=CARTESIAN_POINT('Ctrl Pts',(200.106578615861,12.4538362575707,29.6725630053804));
#79271=CARTESIAN_POINT('Ctrl Pts',(200.104406396538,12.4579871180878,29.6329766711804));
#79272=CARTESIAN_POINT('Ctrl Pts',(200.102234177215,12.4605200161449,29.5933463038373));
#79273=CARTESIAN_POINT('Ctrl Pts',(200.099222387664,12.4640318879998,29.5383986634128));
#79274=CARTESIAN_POINT('Ctrl Pts',(200.096210598113,12.4644458728765,29.483138698796));
#79275=CARTESIAN_POINT('Ctrl Pts',(200.093198808562,12.4617251107476,29.4279448085845));
#79276=CARTESIAN_POINT('Ctrl Pts',(200.09019231761,12.4590091352167,29.3728480201968));
#79277=CARTESIAN_POINT('Ctrl Pts',(200.087185826657,12.4531693833186,29.3178175981223));
#79278=CARTESIAN_POINT('Ctrl Pts',(200.084179335705,12.4442209499736,29.2632340867916));
#79279=CARTESIAN_POINT('Ctrl Pts',(200.081175785817,12.4352812703308,29.2087039711545));
#79280=CARTESIAN_POINT('Ctrl Pts',(200.07817223593,12.4232390187041,29.1546204181236));
#79281=CARTESIAN_POINT('Ctrl Pts',(200.075168686042,12.4081611039551,29.1013591148564));
#79282=CARTESIAN_POINT('Ctrl Pts',(200.072166891965,12.3930920034294,29.0481289469969));
#79283=CARTESIAN_POINT('Ctrl Pts',(200.069165097888,12.3749909007801,28.9957205825852));
#79284=CARTESIAN_POINT('Ctrl Pts',(200.066163303811,12.3539753401218,28.9444974992477));
#79285=CARTESIAN_POINT('Ctrl Pts',(200.063162082907,12.3329637922471,28.8932841966224));
#79286=CARTESIAN_POINT('Ctrl Pts',(200.060160862003,12.3090390918353,28.8432562131816));
#79287=CARTESIAN_POINT('Ctrl Pts',(200.057159641099,12.2823671743628,28.7947577153085));
#79288=CARTESIAN_POINT('Ctrl Pts',(200.054155676289,12.2556708717342,28.7462148770373));
#79289=CARTESIAN_POINT('Ctrl Pts',(200.051151711479,12.2262225892105,28.6992047808735));
#79290=CARTESIAN_POINT('Ctrl Pts',(200.048147746668,12.1942338596529,28.6540462551306));
#79291=CARTESIAN_POINT('Ctrl Pts',(200.045142397325,12.1622303864312,28.6088669157405));
#79292=CARTESIAN_POINT('Ctrl Pts',(200.042137047982,12.1276844615012,28.5655412609229));
#79293=CARTESIAN_POINT('Ctrl Pts',(200.039131698639,12.0908485527022,28.5243557589636));
#79294=CARTESIAN_POINT('Ctrl Pts',(200.036120776606,12.0539443406716,28.4830938885102));
#79295=CARTESIAN_POINT('Ctrl Pts',(200.033109854574,12.0147420371894,28.4439804710278));
#79296=CARTESIAN_POINT('Ctrl Pts',(200.030098932542,11.9735308183608,28.4072649014048));
#79297=CARTESIAN_POINT('Ctrl Pts',(200.027926714521,11.9437991444042,28.3807765961281));
#79298=CARTESIAN_POINT('Ctrl Pts',(200.025754496501,11.9130226230988,28.3555355316041));
#79299=CARTESIAN_POINT('Ctrl Pts',(200.023582278481,11.8813193647311,28.3316214537446));
#79300=CARTESIAN_POINT('Ctrl Pts',(200.020570489526,11.8373626704676,28.2984644893445));
#79301=CARTESIAN_POINT('Ctrl Pts',(200.017558700571,11.7914411441689,28.2677228671092));
#79302=CARTESIAN_POINT('Ctrl Pts',(200.014546911616,11.7438505227137,28.239635509125));
#79303=CARTESIAN_POINT('Ctrl Pts',(200.011540421258,11.6963436267639,28.2115975648314));
#79304=CARTESIAN_POINT('Ctrl Pts',(200.008533930901,11.6471739138674,28.1862048834493));
#79305=CARTESIAN_POINT('Ctrl Pts',(200.005527440544,11.5966674909243,28.163654178263));
#79306=CARTESIAN_POINT('Ctrl Pts',(200.002523891251,11.5462104753034,28.1411255330423));
#79307=CARTESIAN_POINT('Ctrl Pts',(199.999520341958,11.4944198194221,28.1214335703311));
#79308=CARTESIAN_POINT('Ctrl Pts',(199.996516792664,11.4416460741353,28.1047290602894));
#79309=CARTESIAN_POINT('Ctrl Pts',(199.99351499918,11.3889031792108,28.0880343153342));
#79310=CARTESIAN_POINT('Ctrl Pts',(199.990513205695,11.3351788358903,28.0743237201462));
#79311=CARTESIAN_POINT('Ctrl Pts',(199.98751141221,11.2808412505503,28.0636990419869));
#79312=CARTESIAN_POINT('Ctrl Pts',(199.984510191896,11.2265140405622,28.0530763925297));
#79313=CARTESIAN_POINT('Ctrl Pts',(199.981508971581,11.1715743384589,28.0455385908318));
#79314=CARTESIAN_POINT('Ctrl Pts',(199.978507751266,11.1164008410242,28.0411363688786));
#79315=CARTESIAN_POINT('Ctrl Pts',(199.975503787035,11.061176900301,28.0367301221206));
#79316=CARTESIAN_POINT('Ctrl Pts',(199.972499822805,11.0057192640682,28.0354652239802));
#79317=CARTESIAN_POINT('Ctrl Pts',(199.969495858574,10.9504105494985,28.0373403894279));
#79318=CARTESIAN_POINT('Ctrl Pts',(199.966490509807,10.8950763429549,28.0392164191457));
#79319=CARTESIAN_POINT('Ctrl Pts',(199.963485161039,10.8398917209894,28.0442353495187));
#79320=CARTESIAN_POINT('Ctrl Pts',(199.960479812271,10.7852347923406,28.0523439097703));
#79321=CARTESIAN_POINT('Ctrl Pts',(199.9574688908,10.7304765154372,28.0604675054155));
#79322=CARTESIAN_POINT('Ctrl Pts',(199.954457969329,10.6762484039289,28.0716920673509));
#79323=CARTESIAN_POINT('Ctrl Pts',(199.951447047857,10.6229177969303,28.0859132763058));
#79324=CARTESIAN_POINT('Ctrl Pts',(199.949274825154,10.5844425472703,28.0961731363712));
#79325=CARTESIAN_POINT('Ctrl Pts',(199.947102602451,10.5464341864154,28.1079916346583));
#79326=CARTESIAN_POINT('Ctrl Pts',(199.944930379747,10.5090242803149,28.1213139977936));
#79327=CARTESIAN_POINT('Ctrl Pts',(199.941918590125,10.4571553965352,28.1397854717205));
#79328=CARTESIAN_POINT('Ctrl Pts',(199.938906800503,10.4062228765033,28.1612264023683));
#79329=CARTESIAN_POINT('Ctrl Pts',(199.935895010881,10.3565889221947,28.1855212306935));
#79330=CARTESIAN_POINT('Ctrl Pts',(199.932888519866,10.3070422883209,28.2097733174117));
#79331=CARTESIAN_POINT('Ctrl Pts',(199.92988202885,10.2587901562201,28.2368691074569));
#79332=CARTESIAN_POINT('Ctrl Pts',(199.926875537834,10.2121761831416,28.2666444618073));
#79333=CARTESIAN_POINT('Ctrl Pts',(199.923871987889,10.1656078097211,28.2963906887118));
#79334=CARTESIAN_POINT('Ctrl Pts',(199.920868437943,10.1206748629444,28.3288110044335));
#79335=CARTESIAN_POINT('Ctrl Pts',(199.917864887998,10.0776960770454,28.3636955849322));
#79336=CARTESIAN_POINT('Ctrl Pts',(199.914863093868,10.0347424156859,28.3985597726021));
#79337=CARTESIAN_POINT('Ctrl Pts',(199.911861299737,9.99374105948417,28.4358850378109));
#79338=CARTESIAN_POINT('Ctrl Pts',(199.908859505607,9.95497953035692,28.4754198576846));
#79339=CARTESIAN_POINT('Ctrl Pts',(199.905858284654,9.91622540255326,28.5149471285787));
#79340=CARTESIAN_POINT('Ctrl Pts',(199.902857063702,9.87971062131992,28.5566827397039));
#79341=CARTESIAN_POINT('Ctrl Pts',(199.89985584275,9.84568585776882,28.6003383352365));
#79342=CARTESIAN_POINT('Ctrl Pts',(199.896851877899,9.81162998671388,28.644033843364));
#79343=CARTESIAN_POINT('Ctrl Pts',(199.893847913048,9.7800690059787,28.6896524256977));
#79344=CARTESIAN_POINT('Ctrl Pts',(199.890843948197,9.75121230213354,28.7368738402745));
#79345=CARTESIAN_POINT('Ctrl Pts',(199.887838598818,9.72234229822248,28.7841170192194));
#79346=CARTESIAN_POINT('Ctrl Pts',(199.884833249439,9.69617930514412,28.8329640373152));
#79347=CARTESIAN_POINT('Ctrl Pts',(199.881827900059,9.67288681474544,28.8830698228134));
#79348=CARTESIAN_POINT('Ctrl Pts',(199.878816977998,9.64955113414744,28.9332685171773));
#79349=CARTESIAN_POINT('Ctrl Pts',(199.875806055937,9.62909678334026,28.9847301500446));
#79350=CARTESIAN_POINT('Ctrl Pts',(199.872795133876,9.61163869818922,29.0370905643279));
#79351=CARTESIAN_POINT('Ctrl Pts',(199.870622916255,9.5990436328168,29.0748657747888));
#79352=CARTESIAN_POINT('Ctrl Pts',(199.868450698634,9.58800703906827,29.1131084034907));
#79353=CARTESIAN_POINT('Ctrl Pts',(199.866278481013,9.57855554213467,29.1516784485509));
#79354=CARTESIAN_POINT('Ctrl Pts',(199.862361330468,9.56151169900859,29.2212316422924));
#79355=CARTESIAN_POINT('Ctrl Pts',(199.858444179922,9.54956641122312,29.2920793217693));
#79356=CARTESIAN_POINT('Ctrl Pts',(199.854527029377,9.54287258404038,29.3635744024794));
#79357=CARTESIAN_POINT('Ctrl Pts',(199.852069701546,9.53867337657027,29.408425078901));
#79358=CARTESIAN_POINT('Ctrl Pts',(199.849612373716,9.53653992342768,29.4535301700919));
#79359=CARTESIAN_POINT('Ctrl Pts',(199.847155045885,9.53650055522948,29.4987251837867));
#79360=CARTESIAN_POINT('',(199.347155045813,9.53650017837068,29.5007225586097));
#79361=CARTESIAN_POINT('Ctrl Pts',(199.847155045843,9.53650055522881,29.4987251845542));
#79362=CARTESIAN_POINT('Ctrl Pts',(199.844186143803,9.53645299126435,29.5533290378456));
#79363=CARTESIAN_POINT('Ctrl Pts',(199.841217241763,9.53946564116368,29.6080119926478));
#79364=CARTESIAN_POINT('Ctrl Pts',(199.838248339723,9.54553843940391,29.6624001808755));
#79365=CARTESIAN_POINT('Ctrl Pts',(199.835281504372,9.5516070102936,29.7167505088075));
#79366=CARTESIAN_POINT('Ctrl Pts',(199.832314669022,9.56073145143656,29.7708059399479));
#79367=CARTESIAN_POINT('Ctrl Pts',(199.829347833672,9.57285971481966,29.8241957069663));
#79368=CARTESIAN_POINT('Ctrl Pts',(199.82638182629,9.58498459351303,29.8775705742591));
#79369=CARTESIAN_POINT('Ctrl Pts',(199.823415818908,9.60011151178393,29.9302796184272));
#79370=CARTESIAN_POINT('Ctrl Pts',(199.820449811525,9.61813743050191,29.9819627465066));
#79371=CARTESIAN_POINT('Ctrl Pts',(199.817481326748,9.63617840559801,30.0336890435767));
#79372=CARTESIAN_POINT('Ctrl Pts',(199.81451284197,9.65712304052316,30.0843872002799));
#79373=CARTESIAN_POINT('Ctrl Pts',(199.811544357193,9.68081908982352,30.1337144279768));
#79374=CARTESIAN_POINT('Ctrl Pts',(199.808574612818,9.70452519390792,30.183062586362));
#79375=CARTESIAN_POINT('Ctrl Pts',(199.805604868444,9.73098477598868,30.231038182389));
#79376=CARTESIAN_POINT('Ctrl Pts',(199.802635124069,9.75999987188039,30.2773235698622));
#79377=CARTESIAN_POINT('Ctrl Pts',(199.799659959631,9.78906792305384,30.3236934325253));
#79378=CARTESIAN_POINT('Ctrl Pts',(199.796684795194,9.82070048633078,30.3683664856554));
#79379=CARTESIAN_POINT('Ctrl Pts',(199.793709630756,9.85465740638949,30.4110557574932));
#79380=CARTESIAN_POINT('Ctrl Pts',(199.79168194793,9.87780028304774,30.4401500496453));
#79381=CARTESIAN_POINT('Ctrl Pts',(199.789654265105,9.90202194565885,30.468323574742));
#79382=CARTESIAN_POINT('Ctrl Pts',(199.787626582279,9.92723678838578,30.4954955257595));
#79383=CARTESIAN_POINT('Ctrl Pts',(199.784614796865,9.9646892412928,30.5358549373527));
#79384=CARTESIAN_POINT('Ctrl Pts',(199.781603011451,10.0045000661863,30.5741814986321));
#79385=CARTESIAN_POINT('Ctrl Pts',(199.778591226037,10.0464200685972,30.6101880761501));
#79386=CARTESIAN_POINT('Ctrl Pts',(199.775584739212,10.0882663217627,30.6461313078243));
#79387=CARTESIAN_POINT('Ctrl Pts',(199.772578252388,10.1322139913949,30.6797623149588));
#79388=CARTESIAN_POINT('Ctrl Pts',(199.769571765564,10.1779765740526,30.7108301851183));
#79389=CARTESIAN_POINT('Ctrl Pts',(199.766568219797,10.2236943900567,30.7418676635364));
#79390=CARTESIAN_POINT('Ctrl Pts',(199.763564674029,10.2712231675746,30.770346677451));
#79391=CARTESIAN_POINT('Ctrl Pts',(199.760561128262,10.3202442725791,30.7960572522225));
#79392=CARTESIAN_POINT('Ctrl Pts',(199.757559338289,10.3692367211233,30.821752797262));
#79393=CARTESIAN_POINT('Ctrl Pts',(199.754557548316,10.4197193017533,30.8446828666115));
#79394=CARTESIAN_POINT('Ctrl Pts',(199.751555758343,10.4713473956468,30.8646826275404));
#79395=CARTESIAN_POINT('Ctrl Pts',(199.74855454152,10.5229656318795,30.8846785697953));
#79396=CARTESIAN_POINT('Ctrl Pts',(199.745553324697,10.5757284554008,30.9017451245872));
#79397=CARTESIAN_POINT('Ctrl Pts',(199.742552107874,10.6292719595987,30.9157658599007));
#79398=CARTESIAN_POINT('Ctrl Pts',(199.739548147077,10.682864417938,30.9297994141932));
#79399=CARTESIAN_POINT('Ctrl Pts',(199.73654418628,10.7372384715601,30.9407814521049));
#79400=CARTESIAN_POINT('Ctrl Pts',(199.733540225482,10.7920172216692,30.9486460623347));
#79401=CARTESIAN_POINT('Ctrl Pts',(199.73053488012,10.8468212200212,30.9565142974663));
#79402=CARTESIAN_POINT('Ctrl Pts',(199.727529534758,10.9020297603562,30.961262195475));
#79403=CARTESIAN_POINT('Ctrl Pts',(199.724524189396,10.9572612551116,30.9628758148542));
#79404=CARTESIAN_POINT('Ctrl Pts',(199.721513271244,11.0125951652202,30.9644924263559));
#79405=CARTESIAN_POINT('Ctrl Pts',(199.718502353092,11.0679515864211,30.9629631647149));
#79406=CARTESIAN_POINT('Ctrl Pts',(199.71549143494,11.1229505708737,30.9583262348054));
#79407=CARTESIAN_POINT('Ctrl Pts',(199.713319184475,11.1626300186545,30.9549808854315));
#79408=CARTESIAN_POINT('Ctrl Pts',(199.711146934009,11.2021234776193,30.950019095071));
#79409=CARTESIAN_POINT('Ctrl Pts',(199.708974683544,11.2412918033836,30.9434716885412));
#79410=CARTESIAN_POINT('Ctrl Pts',(199.705962890636,11.2955981035294,30.9343938069303));
#79411=CARTESIAN_POINT('Ctrl Pts',(199.702951097727,11.3495039340656,30.9222281897881));
#79412=CARTESIAN_POINT('Ctrl Pts',(199.699939304819,11.4026324297627,30.9070250091961));
#79413=CARTESIAN_POINT('Ctrl Pts',(199.69693281057,11.4556674562733,30.8918485756239));
#79414=CARTESIAN_POINT('Ctrl Pts',(199.693926316322,11.5079273589684,30.8736453282288));
#79415=CARTESIAN_POINT('Ctrl Pts',(199.690919822074,11.5590450000732,30.8525165203771));
#79416=CARTESIAN_POINT('Ctrl Pts',(199.687916268931,11.6101126353031,30.8314083817994));
#79417=CARTESIAN_POINT('Ctrl Pts',(199.684912715788,11.6600397375717,30.8073805529998));
#79418=CARTESIAN_POINT('Ctrl Pts',(199.681909162645,11.7084756840184,30.7805836384847));
#79419=CARTESIAN_POINT('Ctrl Pts',(199.678907365358,11.7568833151515,30.7538023892573));
#79420=CARTESIAN_POINT('Ctrl Pts',(199.675905568071,11.8038010578136,30.7242555179317));
#79421=CARTESIAN_POINT('Ctrl Pts',(199.672903770784,11.8489016955114,30.6921401601145));
#79422=CARTESIAN_POINT('Ctrl Pts',(199.669902546721,11.8939937207795,30.6600309350546));
#79423=CARTESIAN_POINT('Ctrl Pts',(199.666901322659,11.9372689009615,30.625354503514));
#79424=CARTESIAN_POINT('Ctrl Pts',(199.663900098596,11.9784298311313,30.5883507318656));
#79425=CARTESIAN_POINT('Ctrl Pts',(199.66089613073,12.0196283917791,30.5513131303303));
#79426=CARTESIAN_POINT('Ctrl Pts',(199.657892162864,12.0587084480754,30.5119442915319));
#79427=CARTESIAN_POINT('Ctrl Pts',(199.654888194997,12.0954076400463,30.4705227210778));
#79428=CARTESIAN_POINT('Ctrl Pts',(199.651882842651,12.1321237460789,30.4290820600944));
#79429=CARTESIAN_POINT('Ctrl Pts',(199.648877490305,12.1664564731692,30.3855871962501));
#79430=CARTESIAN_POINT('Ctrl Pts',(199.645872137959,12.1981842837386,30.3403491370864));
#79431=CARTESIAN_POINT('Ctrl Pts',(199.642861213045,12.2299709244697,30.2950271968642));
#79432=CARTESIAN_POINT('Ctrl Pts',(199.639850288132,12.2591427222622,30.24795605421));
#79433=CARTESIAN_POINT('Ctrl Pts',(199.636839363218,12.2855225904214,30.1994740306232));
#79434=CARTESIAN_POINT('Ctrl Pts',(199.634667170415,12.3045540048185,30.1644973023045));
#79435=CARTESIAN_POINT('Ctrl Pts',(199.632494977613,12.322133253818,30.1287868103729));
#79436=CARTESIAN_POINT('Ctrl Pts',(199.63032278481,12.3382095470459,30.0924757026201));
#79437=CARTESIAN_POINT('Ctrl Pts',(199.627310986406,12.3604997204729,30.0421294643636));
#79438=CARTESIAN_POINT('Ctrl Pts',(199.624299188002,12.3799909399452,29.9904192511729));
#79439=CARTESIAN_POINT('Ctrl Pts',(199.621287389598,12.396517810639,29.937687393659));
#79440=CARTESIAN_POINT('Ctrl Pts',(199.618280889694,12.4130156064681,29.8850483045616));
#79441=CARTESIAN_POINT('Ctrl Pts',(199.615274389791,12.4265592467518,29.8313916373946));
#79442=CARTESIAN_POINT('Ctrl Pts',(199.612267889887,12.4370313468767,29.7770796962855));
#79443=CARTESIAN_POINT('Ctrl Pts',(199.609264330996,12.4474932030038,29.7228208841));
#79444=CARTESIAN_POINT('Ctrl Pts',(199.606260772105,12.4548893720455,29.6679085832335));
#79445=CARTESIAN_POINT('Ctrl Pts',(199.603257213214,12.4591527681321,29.612718451251));
#79446=CARTESIAN_POINT('Ctrl Pts',(199.600255410097,12.4634136719876,29.5575605814743));
#79447=CARTESIAN_POINT('Ctrl Pts',(199.597253606981,12.4645453924085,29.5021257273295));
#79448=CARTESIAN_POINT('Ctrl Pts',(199.594251803864,12.4625325777978,29.4467955934154));
#79449=CARTESIAN_POINT('Ctrl Pts',(199.591250573902,12.4605201475071,29.3914760240481));
#79450=CARTESIAN_POINT('Ctrl Pts',(199.58824934394,12.4553643939643,29.3362616619538));
#79451=CARTESIAN_POINT('Ctrl Pts',(199.585248113977,12.4471020492454,29.2815328192389));
#79452=CARTESIAN_POINT('Ctrl Pts',(199.582244140153,12.4388321507116,29.226753940903));
#79453=CARTESIAN_POINT('Ctrl Pts',(199.579240166328,12.42745006613,29.1724619912569));
#79454=CARTESIAN_POINT('Ctrl Pts',(199.576236192504,12.4130440729133,29.1190292688346));
#79455=CARTESIAN_POINT('Ctrl Pts',(199.573230834157,12.3986314400218,29.065571919447));
#79456=CARTESIAN_POINT('Ctrl Pts',(199.570225475811,12.3811922865884,29.0129750881006));
#79457=CARTESIAN_POINT('Ctrl Pts',(199.567220117465,12.3608644878099,28.9615948590347));
#79458=CARTESIAN_POINT('Ctrl Pts',(199.564209186559,12.3404989970635,28.9101193603352));
#79459=CARTESIAN_POINT('Ctrl Pts',(199.561198255653,12.3172343842009,28.8598654495474));
#79460=CARTESIAN_POINT('Ctrl Pts',(199.558187324747,12.2912557854271,28.8111671127182));
#79461=CARTESIAN_POINT('Ctrl Pts',(199.556015178524,12.2725143008195,28.7760351512892));
#79462=CARTESIAN_POINT('Ctrl Pts',(199.5538430323,12.2523613224879,28.7417122946265));
#79463=CARTESIAN_POINT('Ctrl Pts',(199.551670886076,12.2308801030755,28.7083141899384));
#79464=CARTESIAN_POINT('Ctrl Pts',(199.548659132467,12.2010956717236,28.6620065973725));
#79465=CARTESIAN_POINT('Ctrl Pts',(199.545647378858,12.1686326388749,28.6172861704565));
#79466=CARTESIAN_POINT('Ctrl Pts',(199.542635625249,12.1336859088169,28.5744793302416));
#79467=CARTESIAN_POINT('Ctrl Pts',(199.539629170203,12.0988006603654,28.5317477998855));
#79468=CARTESIAN_POINT('Ctrl Pts',(199.536622715157,12.0614407174041,28.4909235803021));
#79469=CARTESIAN_POINT('Ctrl Pts',(199.533616260111,12.0218440733813,28.4523039850723));
#79470=CARTESIAN_POINT('Ctrl Pts',(199.53061274608,11.9822861641207,28.4137221688227));
#79471=CARTESIAN_POINT('Ctrl Pts',(199.527609232049,11.9404962642052,28.3773410709358));
#79472=CARTESIAN_POINT('Ctrl Pts',(199.524605718018,11.8967511863767,28.3434233446364));
#79473=CARTESIAN_POINT('Ctrl Pts',(199.521603959683,11.8530316796125,28.3095254448502));
#79474=CARTESIAN_POINT('Ctrl Pts',(199.518602201348,11.8073596764035,28.2780883848852));
#79475=CARTESIAN_POINT('Ctrl Pts',(199.515600443013,11.7600454964975,28.2493349396206));
#79476=CARTESIAN_POINT('Ctrl Pts',(199.512599257672,11.7127403482125,28.22058698299));
#79477=CARTESIAN_POINT('Ctrl Pts',(199.509598072331,11.6637940963546,28.1945218972784));
#79478=CARTESIAN_POINT('Ctrl Pts',(199.50659688699,11.6135445467326,28.1713181949109));
#79479=CARTESIAN_POINT('Ctrl Pts',(199.503592957185,11.5632490459227,28.1480932736929));
#79480=CARTESIAN_POINT('Ctrl Pts',(199.500589027381,11.5116483463261,28.1277351845344));
#79481=CARTESIAN_POINT('Ctrl Pts',(199.497585097577,11.4591019141554,28.1103749849622));
#79482=CARTESIAN_POINT('Ctrl Pts',(199.494579782981,11.4065312584276,28.093006782453));
#79483=CARTESIAN_POINT('Ctrl Pts',(199.491574468385,11.3530145112847,28.0786393613286));
#79484=CARTESIAN_POINT('Ctrl Pts',(199.48856915379,11.2989248790498,28.067353439719));
#79485=CARTESIAN_POINT('Ctrl Pts',(199.48555826566,11.2447349343855,28.0560465876987));
#79486=CARTESIAN_POINT('Ctrl Pts',(199.48254737753,11.1899705051224,28.0478327288488));
#79487=CARTESIAN_POINT('Ctrl Pts',(199.4795364894,11.1350123385002,28.0427409569837));
#79488=CARTESIAN_POINT('Ctrl Pts',(199.477363988714,11.0953573763999,28.0390669985396));
#79489=CARTESIAN_POINT('Ctrl Pts',(199.475191488028,11.0556016858806,28.0370173999341));
#79490=CARTESIAN_POINT('Ctrl Pts',(199.473018987342,11.0158877126441,28.0365862408099));
#79491=CARTESIAN_POINT('Ctrl Pts',(199.47000715515,10.9608305042163,28.0359885061631));
#79492=CARTESIAN_POINT('Ctrl Pts',(199.466995322958,10.9056254374112,28.0385009286239));
#79493=CARTESIAN_POINT('Ctrl Pts',(199.463983490766,10.8506523401595,28.0441402792507));
#79494=CARTESIAN_POINT('Ctrl Pts',(199.46097695768,10.7957759642054,28.0497697078368));
#79495=CARTESIAN_POINT('Ctrl Pts',(199.457970424595,10.7411312683149,28.0585150927121));
#79496=CARTESIAN_POINT('Ctrl Pts',(199.45496389151,10.6870974719425,28.0703412092617));
#79497=CARTESIAN_POINT('Ctrl Pts',(199.451960299834,10.6331165389569,28.0821557558567));
#79498=CARTESIAN_POINT('Ctrl Pts',(199.448956708158,10.5797458341841,28.0970449509043));
#79499=CARTESIAN_POINT('Ctrl Pts',(199.445953116483,10.5273569830918,28.114922085741));
#79500=CARTESIAN_POINT('Ctrl Pts',(199.442951281033,10.4749987642145,28.1327887676622));
#79501=CARTESIAN_POINT('Ctrl Pts',(199.439949445583,10.423621759186,28.1536397562874));
#79502=CARTESIAN_POINT('Ctrl Pts',(199.436947610133,10.3735827201601,28.1773384251752));
#79503=CARTESIAN_POINT('Ctrl Pts',(199.433946348344,10.3235532437556,28.2010325651711));
#79504=CARTESIAN_POINT('Ctrl Pts',(199.430945086555,10.2748617018364,28.2275730788476));
#79505=CARTESIAN_POINT('Ctrl Pts',(199.427943824765,10.2278430004879,28.2567760386381));
#79506=CARTESIAN_POINT('Ctrl Pts',(199.424939820138,10.1807813289851,28.2860056868664));
#79507=CARTESIAN_POINT('Ctrl Pts',(199.421935815511,10.1353960010385,28.3179023631074));
#79508=CARTESIAN_POINT('Ctrl Pts',(199.418931810884,10.0919942062385,28.352237947789));
#79509=CARTESIAN_POINT('Ctrl Pts',(199.41592642226,10.0485724154928,28.386589351459));
#79510=CARTESIAN_POINT('Ctrl Pts',(199.412921033637,10.0071363745303,28.4233815526671));
#79511=CARTESIAN_POINT('Ctrl Pts',(199.409915645013,9.96795879150149,28.4623472671645));
#79512=CARTESIAN_POINT('Ctrl Pts',(199.406904685046,9.92870858166622,28.5013852157097));
#79513=CARTESIAN_POINT('Ctrl Pts',(199.403893725079,9.89172554559009,28.5426043324622));
#79514=CARTESIAN_POINT('Ctrl Pts',(199.400882765112,9.85724342692036,28.5857026388077));
#79515=CARTESIAN_POINT('Ctrl Pts',(199.398710872944,9.83237048131507,28.6167906888106));
#79516=CARTESIAN_POINT('Ctrl Pts',(199.396538980776,9.80879796000743,28.6488557914288));
#79517=CARTESIAN_POINT('Ctrl Pts',(199.394367088608,9.78659921254147,28.6817758381745));
#79518=CARTESIAN_POINT('Ctrl Pts',(199.391312151604,9.75537492983388,28.7280804708081));
#79519=CARTESIAN_POINT('Ctrl Pts',(199.3882572146,9.72674340609812,28.7762658439025));
#79520=CARTESIAN_POINT('Ctrl Pts',(199.385202277597,9.70093225921005,28.8260153897611));
#79521=CARTESIAN_POINT('Ctrl Pts',(199.382031674951,9.67414385390876,28.8776485466989));
#79522=CARTESIAN_POINT('Ctrl Pts',(199.378861072304,9.65039409250268,28.9309663124073));
#79523=CARTESIAN_POINT('Ctrl Pts',(199.375690469658,9.62988870897934,28.9855806183495));
#79524=CARTESIAN_POINT('Ctrl Pts',(199.372645582071,9.61019636820771,29.0380294556217));
#79525=CARTESIAN_POINT('Ctrl Pts',(199.369600694484,9.59349615832397,29.0916734209036));
#79526=CARTESIAN_POINT('Ctrl Pts',(199.366555806897,9.57992289330038,29.1461451412971));
#79527=CARTESIAN_POINT('Ctrl Pts',(199.36351361467,9.56636164344493,29.2005686428665));
#79528=CARTESIAN_POINT('Ctrl Pts',(199.360471422443,9.55592196783507,29.2558179546714));
#79529=CARTESIAN_POINT('Ctrl Pts',(199.357429230216,9.54868887481389,29.3115105628662));
#79530=CARTESIAN_POINT('Ctrl Pts',(199.354388673487,9.54145967034044,29.3671732304305));
#79531=CARTESIAN_POINT('Ctrl Pts',(199.351348116758,9.53743369000977,29.4232782185999));
#79532=CARTESIAN_POINT('Ctrl Pts',(199.348307560029,9.53664449786614,29.4794348747984));
#79533=CARTESIAN_POINT('Ctrl Pts',(199.347923388634,9.53654478420382,29.4865302138721));
#79534=CARTESIAN_POINT('Ctrl Pts',(199.347539217238,9.53649667484675,29.4936263721534));
#79535=CARTESIAN_POINT('Ctrl Pts',(199.347155045843,9.5365001783704,29.5007225580503));
#79536=CARTESIAN_POINT('Ctrl Pts',(199.347155045813,9.53650017837068,29.5007225586097));
#79537=CARTESIAN_POINT('Ctrl Pts',(199.343841136659,9.53653040021501,29.5619351207308));
#79538=CARTESIAN_POINT('Ctrl Pts',(199.340527227506,9.54040521676902,29.6230182051036));
#79539=CARTESIAN_POINT('Ctrl Pts',(199.337213318352,9.54805131113806,29.6835136368559));
#79540=CARTESIAN_POINT('Ctrl Pts',(199.333886785213,9.55572653249469,29.7442395195555));
#79541=CARTESIAN_POINT('Ctrl Pts',(199.330560252073,9.56720167272118,29.8043729560867));
#79542=CARTESIAN_POINT('Ctrl Pts',(199.327233718933,9.58235272736732,29.8634672755519));
#79543=CARTESIAN_POINT('Ctrl Pts',(199.323891681091,9.59757439985442,29.9228370288632));
#79544=CARTESIAN_POINT('Ctrl Pts',(199.320549643249,9.61650617573339,29.9811576601772));
#79545=CARTESIAN_POINT('Ctrl Pts',(199.317207605408,9.63897437045939,30.0379976633161));
#79546=CARTESIAN_POINT('Ctrl Pts',(199.316710133563,9.6423188251934,30.0464584595615));
#79547=CARTESIAN_POINT('Ctrl Pts',(199.316212661718,9.64574155335958,30.0548864924784));
#79548=CARTESIAN_POINT('Ctrl Pts',(199.315715189873,9.64924189529193,30.0632803853903));
#79549=CARTESIAN_POINT('Ctrl Pts',(199.312703713051,9.67043143337053,30.1140933393597));
#79550=CARTESIAN_POINT('Ctrl Pts',(199.309692236228,9.69453614823446,30.1638143929741));
#79551=CARTESIAN_POINT('Ctrl Pts',(199.306680759406,9.72142152962381,30.2120880177973));
#79552=CARTESIAN_POINT('Ctrl Pts',(199.303674581285,9.74825960611454,30.2602767050519));
#79553=CARTESIAN_POINT('Ctrl Pts',(199.300668403164,9.77786838474692,30.3070225605282));
#79554=CARTESIAN_POINT('Ctrl Pts',(199.297662225042,9.81006582268166,30.3519911405934));
#79555=CARTESIAN_POINT('Ctrl Pts',(199.2946589878,9.84223176256306,30.3969157288747));
#79556=CARTESIAN_POINT('Ctrl Pts',(199.291655750558,9.87698103919725,30.4400660593064));
#79557=CARTESIAN_POINT('Ctrl Pts',(199.288652513315,9.91408730586176,30.4811349910738));
#79558=CARTESIAN_POINT('Ctrl Pts',(199.285651031134,9.95117188799834,30.5221799225718));
#79559=CARTESIAN_POINT('Ctrl Pts',(199.282649548953,9.99061037690318,30.5611454757929));
#79560=CARTESIAN_POINT('Ctrl Pts',(199.279648066772,10.0321364360397,30.5977578838515));
#79561=CARTESIAN_POINT('Ctrl Pts',(199.276647156453,10.073654583366,30.63436331628));
#79562=CARTESIAN_POINT('Ctrl Pts',(199.273646246134,10.117259115408,30.6686161454159));
#79563=CARTESIAN_POINT('Ctrl Pts',(199.270645335815,10.1626488643213,30.7002813526743));
#79564=CARTESIAN_POINT('Ctrl Pts',(199.267641677108,10.2080801834855,30.7319755605471));
#79565=CARTESIAN_POINT('Ctrl Pts',(199.264638018402,10.2552995521394,30.7610771098658));
#79566=CARTESIAN_POINT('Ctrl Pts',(199.261634359696,10.3039761461935,30.7873938965726));
#79567=CARTESIAN_POINT('Ctrl Pts',(199.25862931441,10.3526752108257,30.8137228318987));
#79568=CARTESIAN_POINT('Ctrl Pts',(199.255624269125,10.4028323634365,30.8372642176464));
#79569=CARTESIAN_POINT('Ctrl Pts',(199.25261922384,10.4540944166606,30.8578730957195));
#79570=CARTESIAN_POINT('Ctrl Pts',(199.249608598822,10.5054516526525,30.8785202401111));
#79571=CARTESIAN_POINT('Ctrl Pts',(199.246597973805,10.5579173862867,30.8962238314625));
#79572=CARTESIAN_POINT('Ctrl Pts',(199.243587348787,10.6111219443893,30.9108884108477));
#79573=CARTESIAN_POINT('Ctrl Pts',(199.241412662904,10.6495535659721,30.9214811793191));
#79574=CARTESIAN_POINT('Ctrl Pts',(199.239237977022,10.6883703561137,30.930489336424));
#79575=CARTESIAN_POINT('Ctrl Pts',(199.237063291139,10.7274305992426,30.9378936580188));
#79576=CARTESIAN_POINT('Ctrl Pts',(199.234051030188,10.7815348016252,30.9481497363732));
#79577=CARTESIAN_POINT('Ctrl Pts',(199.231038769237,10.8363306405577,30.9553690988392));
#79578=CARTESIAN_POINT('Ctrl Pts',(199.228026508286,10.8914470393717,30.9594685692878));
#79579=CARTESIAN_POINT('Ctrl Pts',(199.225019550016,10.9464664131636,30.9635608231689));
#79580=CARTESIAN_POINT('Ctrl Pts',(199.222012591746,11.0018047052847,30.9645440460637));
#79581=CARTESIAN_POINT('Ctrl Pts',(199.219005633476,11.0570823156062,30.9623863577198));
#79582=CARTESIAN_POINT('Ctrl Pts',(199.21600161914,11.1123058068991,30.9602307818406));
#79583=CARTESIAN_POINT('Ctrl Pts',(199.212997604805,11.1674682097885,30.9549404072662));
#79584=CARTESIAN_POINT('Ctrl Pts',(199.209993590469,11.2221883647312,30.9465353713539));
#79585=CARTESIAN_POINT('Ctrl Pts',(199.20699133562,11.2768764694288,30.9381352583711));
#79586=CARTESIAN_POINT('Ctrl Pts',(199.203989080772,11.3311223195393,30.9266241801385));
#79587=CARTESIAN_POINT('Ctrl Pts',(199.200986825923,11.3845506351572,30.9120740274505));
#79588=CARTESIAN_POINT('Ctrl Pts',(199.197985148735,11.4379686706961,30.8975266743401));
#79589=CARTESIAN_POINT('Ctrl Pts',(199.194983471546,11.4905689757804,30.8799415467321));
#79590=CARTESIAN_POINT('Ctrl Pts',(199.191981794358,11.5419894718377,30.8594409374508));
#79591=CARTESIAN_POINT('Ctrl Pts',(199.188977383739,11.5934567931637,30.838921659611));
#79592=CARTESIAN_POINT('Ctrl Pts',(199.185972973121,11.6437416684417,30.8154817920101));
#79593=CARTESIAN_POINT('Ctrl Pts',(199.182968562502,11.6925015450675,30.7892919995405));
#79594=CARTESIAN_POINT('Ctrl Pts',(199.179962772536,11.7412838077147,30.7630901831427));
#79595=CARTESIAN_POINT('Ctrl Pts',(199.17695698257,11.7885392257408,30.7341362010396));
#79596=CARTESIAN_POINT('Ctrl Pts',(199.173951192604,11.8339523114518,30.70264533102));
#79597=CARTESIAN_POINT('Ctrl Pts',(199.170939843705,11.8794493845107,30.6710962215169));
#79598=CARTESIAN_POINT('Ctrl Pts',(199.167928494806,11.9230969029341,30.6370011776122));
#79599=CARTESIAN_POINT('Ctrl Pts',(199.164917145906,11.9646116428316,30.6006164765775));
#79600=CARTESIAN_POINT('Ctrl Pts',(199.162748561406,11.9945079532505,30.5744144982121));
#79601=CARTESIAN_POINT('Ctrl Pts',(199.160579976905,12.0232989123031,30.5470259635572));
#79602=CARTESIAN_POINT('Ctrl Pts',(199.158411392405,12.0508912880956,30.5185576815305));
#79603=CARTESIAN_POINT('Ctrl Pts',(199.155399333181,12.0892157665761,30.4790166115585));
#79604=CARTESIAN_POINT('Ctrl Pts',(199.152387273957,12.1253847074543,30.4372277818558));
#79605=CARTESIAN_POINT('Ctrl Pts',(199.149375214733,12.1591245791634,30.3934553486208));
#79606=CARTESIAN_POINT('Ctrl Pts',(199.146368444345,12.1928052074713,30.3497597748313));
#79607=CARTESIAN_POINT('Ctrl Pts',(199.143361673956,12.2240649119281,30.3040879241949));
#79608=CARTESIAN_POINT('Ctrl Pts',(199.140354903568,12.2526683148564,30.2567392833432));
#79609=CARTESIAN_POINT('Ctrl Pts',(199.137351068508,12.2812437940074,30.2094368661141));
#79610=CARTESIAN_POINT('Ctrl Pts',(199.134347233448,12.3071678376621,30.1604613508079));
#79611=CARTESIAN_POINT('Ctrl Pts',(199.131343398389,12.3302476565136,30.1101421329003));
#79612=CARTESIAN_POINT('Ctrl Pts',(199.128341313988,12.3533140242571,30.0598522414463));
#79613=CARTESIAN_POINT('Ctrl Pts',(199.125339229588,12.3735392336328,30.0082206780741));
#79614=CARTESIAN_POINT('Ctrl Pts',(199.122337145188,12.3907769542751,29.955600387903));
#79615=CARTESIAN_POINT('Ctrl Pts',(199.11933562939,12.4080114100561,29.9029900641277));
#79616=CARTESIAN_POINT('Ctrl Pts',(199.116334113591,12.4222593370221,29.8493918863434));
#79617=CARTESIAN_POINT('Ctrl Pts',(199.113332597792,12.4334237614922,29.7951754901572));
#79618=CARTESIAN_POINT('Ctrl Pts',(199.110328333512,12.4445984091983,29.7409094481506));
#79619=CARTESIAN_POINT('Ctrl Pts',(199.107324069233,12.4526838073393,29.6860245743851));
#79620=CARTESIAN_POINT('Ctrl Pts',(199.104319804954,12.4576341211716,29.6309007975384));
#79621=CARTESIAN_POINT('Ctrl Pts',(199.101314153152,12.46258672131,29.5757515617357));
#79622=CARTESIAN_POINT('Ctrl Pts',(199.098308501351,12.4644013335964,29.5203637307685));
#79623=CARTESIAN_POINT('Ctrl Pts',(199.09530284955,12.4630842685681,29.4651191590033));
#79624=CARTESIAN_POINT('Ctrl Pts',(199.092291624031,12.4617647611579,29.4097721410137));
#79625=CARTESIAN_POINT('Ctrl Pts',(199.089280398512,12.4573020187898,29.3545694395871));
#79626=CARTESIAN_POINT('Ctrl Pts',(199.086269172992,12.4497543379427,29.2998885070358));
#79627=CARTESIAN_POINT('Ctrl Pts',(199.084099279885,12.4443154691035,29.2604853544417));
#79628=CARTESIAN_POINT('Ctrl Pts',(199.081929386778,12.4372757958333,29.2213530221574));
#79629=CARTESIAN_POINT('Ctrl Pts',(199.079759493671,12.4286733336564,29.1826283634301));
#79630=CARTESIAN_POINT('Ctrl Pts',(199.07675034364,12.4167436679778,29.1289260369756));
#79631=CARTESIAN_POINT('Ctrl Pts',(199.073741193609,12.4017568779544,29.0757847809708));
#79632=CARTESIAN_POINT('Ctrl Pts',(199.070732043578,12.383782542528,29.0235777870472));
#79633=CARTESIAN_POINT('Ctrl Pts',(199.067728196713,12.3658398841116,28.9714627999454));
#79634=CARTESIAN_POINT('Ctrl Pts',(199.064724349847,12.3449202993446,28.9202793031738));
#79635=CARTESIAN_POINT('Ctrl Pts',(199.061720502982,12.3211438748843,28.8703881260208));
#79636=CARTESIAN_POINT('Ctrl Pts',(199.058719597923,12.2973907357786,28.82054580961));
#79637=CARTESIAN_POINT('Ctrl Pts',(199.055718692864,12.270786525552,28.7719937804295));
#79638=CARTESIAN_POINT('Ctrl Pts',(199.052717787805,12.2414997540638,28.7250738030886));
#79639=CARTESIAN_POINT('Ctrl Pts',(199.049718634572,12.2122300791931,28.6781812160289));
#79640=CARTESIAN_POINT('Ctrl Pts',(199.046719481339,12.1802812262359,28.632919239829));
#79641=CARTESIAN_POINT('Ctrl Pts',(199.043720328106,12.1458669461172,28.5896038270094));
#79642=CARTESIAN_POINT('Ctrl Pts',(199.040721739337,12.111459143039,28.546296566494));
#79643=CARTESIAN_POINT('Ctrl Pts',(199.037723150568,12.0745871630082,28.5049355551979));
#79644=CARTESIAN_POINT('Ctrl Pts',(199.0347245618,12.0355058586884,28.4658047251017));
#79645=CARTESIAN_POINT('Ctrl Pts',(199.031723194895,11.9963883462823,28.4266376410345));
#79646=CARTESIAN_POINT('Ctrl Pts',(199.028721827991,11.955057794877,28.3897052403928));
#79647=CARTESIAN_POINT('Ctrl Pts',(199.025720461087,11.9118057930955,28.3552544187998));
#79648=CARTESIAN_POINT('Ctrl Pts',(199.022717694468,11.8685336203466,28.3207875307504));
#79649=CARTESIAN_POINT('Ctrl Pts',(199.019714927849,11.8233386433526,28.2888048340456));
#79650=CARTESIAN_POINT('Ctrl Pts',(199.01671216123,11.7765427345572,28.259510729024));
#79651=CARTESIAN_POINT('Ctrl Pts',(199.0137037656,11.7296591017816,28.2301617090419));
#79652=CARTESIAN_POINT('Ctrl Pts',(199.010695369971,11.6811690068258,28.2035116029031));
#79653=CARTESIAN_POINT('Ctrl Pts',(199.007686974342,11.6314192312139,28.1797189676234));
#79654=CARTESIAN_POINT('Ctrl Pts',(199.005493847874,11.5951515446659,28.1623740886193));
#79655=CARTESIAN_POINT('Ctrl Pts',(199.003300721405,11.5582149209316,28.1465468160399));
#79656=CARTESIAN_POINT('Ctrl Pts',(199.001107594937,11.5207491537022,28.1322819848673));
#79657=CARTESIAN_POINT('Ctrl Pts',(198.998090930476,11.4692146662257,28.1126605859803));
#79658=CARTESIAN_POINT('Ctrl Pts',(198.995074266014,11.4164644752731,28.0959158357281));
#79659=CARTESIAN_POINT('Ctrl Pts',(198.992057601553,11.3628503020118,28.082194686027));
#79660=CARTESIAN_POINT('Ctrl Pts',(198.989046266859,11.3093308529307,28.0684977785101));
#79661=CARTESIAN_POINT('Ctrl Pts',(198.986034932165,11.2549509564839,28.0578139977815));
#79662=CARTESIAN_POINT('Ctrl Pts',(198.983023597471,11.2000796617887,28.0502412687145));
#79663=CARTESIAN_POINT('Ctrl Pts',(198.980015226992,11.1452623797891,28.0426759938822));
#79664=CARTESIAN_POINT('Ctrl Pts',(198.977006856512,11.0899551760505,28.0382157745756));
#79665=CARTESIAN_POINT('Ctrl Pts',(198.973998486033,11.0345377234283,28.0369075915512));
#79666=CARTESIAN_POINT('Ctrl Pts',(198.970991903168,10.9791532006022,28.0356001858669));
#79667=CARTESIAN_POINT('Ctrl Pts',(198.967985320303,10.9236590831148,28.0374411157049));
#79668=CARTESIAN_POINT('Ctrl Pts',(198.964978737438,10.8684383194882,28.042425379536));
#79669=CARTESIAN_POINT('Ctrl Pts',(198.961972768234,10.8132288267504,28.0474086260489));
#79670=CARTESIAN_POINT('Ctrl Pts',(198.958966799031,10.7582931001436,28.0555338849726));
#79671=CARTESIAN_POINT('Ctrl Pts',(198.955960829828,10.7040099414027,28.0667442184971));
#79672=CARTESIAN_POINT('Ctrl Pts',(198.952952216565,10.6496790350379,28.0779644126635));
#79673=CARTESIAN_POINT('Ctrl Pts',(198.949943603302,10.5960023590066,28.0922749963719));
#79674=CARTESIAN_POINT('Ctrl Pts',(198.94693499004,10.5433479918902,28.1095679831472));
#79675=CARTESIAN_POINT('Ctrl Pts',(198.943925041331,10.4906702528656,28.126868645831));
#79676=CARTESIAN_POINT('Ctrl Pts',(198.940915092623,10.4390162176512,28.1471541590495));
#79677=CARTESIAN_POINT('Ctrl Pts',(198.937905143915,10.3887351995767,28.1702678488645));
#79678=CARTESIAN_POINT('Ctrl Pts',(198.9348897579,10.3383633516001,28.1934232922928));
#79679=CARTESIAN_POINT('Ctrl Pts',(198.931874371884,10.2893699407518,28.2194168713064));
#79680=CARTESIAN_POINT('Ctrl Pts',(198.928858985869,10.2420797583762,28.2480458645234));
#79681=CARTESIAN_POINT('Ctrl Pts',(198.92672455598,10.2086055768981,28.2683107919637));
#79682=CARTESIAN_POINT('Ctrl Pts',(198.924590126091,10.1759842445242,28.2898952236279));
#79683=CARTESIAN_POINT('Ctrl Pts',(198.922455696203,10.1443211833688,28.3127148561662));
#79684=CARTESIAN_POINT('Ctrl Pts',(198.919318172452,10.0977777916554,28.3462587731857));
#79685=CARTESIAN_POINT('Ctrl Pts',(198.916180648701,10.0531030287581,28.3826208168073));
#79686=CARTESIAN_POINT('Ctrl Pts',(198.91304312495,10.0106574334974,28.4215596742953));
#79687=CARTESIAN_POINT('Ctrl Pts',(198.910057117073,9.9702616016631,28.4586181141462));
#79688=CARTESIAN_POINT('Ctrl Pts',(198.907071109196,9.93188506305593,28.4980098223084));
#79689=CARTESIAN_POINT('Ctrl Pts',(198.904085101318,9.89580812800508,28.5394831808759));
#79690=CARTESIAN_POINT('Ctrl Pts',(198.901101865289,9.8597646824164,28.5809180405944));
#79691=CARTESIAN_POINT('Ctrl Pts',(198.89811862926,9.82601696303526,28.6244303220827));
#79692=CARTESIAN_POINT('Ctrl Pts',(198.895135393231,9.79480843547741,28.6697316441032));
#79693=CARTESIAN_POINT('Ctrl Pts',(198.892153710288,9.76361615522021,28.7150093820505));
#79694=CARTESIAN_POINT('Ctrl Pts',(198.889172027346,9.73496075035578,28.7620738746278));
#79695=CARTESIAN_POINT('Ctrl Pts',(198.886190344403,9.70904387744193,28.8106056718903));
#79696=CARTESIAN_POINT('Ctrl Pts',(198.883208998249,9.68312993190989,28.8591319873532));
#79697=CARTESIAN_POINT('Ctrl Pts',(198.880227652096,9.65995415457463,28.9091248054983));
#79698=CARTESIAN_POINT('Ctrl Pts',(198.877246305942,9.63967233018285,28.960239978574));
#79699=CARTESIAN_POINT('Ctrl Pts',(198.874262118805,9.61937117883709,29.011403860315));
#79700=CARTESIAN_POINT('Ctrl Pts',(198.871277931667,9.6019696806173,29.0636917325209));
#79701=CARTESIAN_POINT('Ctrl Pts',(198.86829374453,9.58757487353748,29.1167409333919));
#79702=CARTESIAN_POINT('Ctrl Pts',(198.865307895739,9.57317205115243,29.1698196730774));
#79703=CARTESIAN_POINT('Ctrl Pts',(198.862322046949,9.56177936146926,29.2236600609534));
#79704=CARTESIAN_POINT('Ctrl Pts',(198.859336198159,9.55345273827624,29.2778890601535));
#79705=CARTESIAN_POINT('Ctrl Pts',(198.856345198788,9.54511175168336,29.3322116042134));
#79706=CARTESIAN_POINT('Ctrl Pts',(198.853354199418,9.53984743173593,29.3869235644018));
#79707=CARTESIAN_POINT('Ctrl Pts',(198.850363200047,9.53766374727779,29.4416481879084));
#79708=CARTESIAN_POINT('Ctrl Pts',(198.849293842093,9.53688302483176,29.461213625471));
#79709=CARTESIAN_POINT('Ctrl Pts',(198.848224484139,9.5364955976742,29.4807807041731));
#79710=CARTESIAN_POINT('Ctrl Pts',(198.847155126185,9.5365000377376,29.500332352169));
#79711=CARTESIAN_POINT('Origin',(197.762132885264,11.,29.5));
#79712=CARTESIAN_POINT('',(204.512132885225,9.82225001771146,29.4997957468552));
#79713=CARTESIAN_POINT('Ctrl Pts',(204.456095751509,10.1027690874833,30.2629362700282));
#79714=CARTESIAN_POINT('Ctrl Pts',(204.459251171507,10.0724807910944,30.2273165244804));
#79715=CARTESIAN_POINT('Ctrl Pts',(204.462406591505,10.0442847328763,30.18985243697));
#79716=CARTESIAN_POINT('Ctrl Pts',(204.465562011503,10.0184068810581,30.1508225651788));
#79717=CARTESIAN_POINT('Ctrl Pts',(204.468715935768,9.99254129587267,30.1118111943477));
#79718=CARTESIAN_POINT('Ctrl Pts',(204.471869860032,9.96899205078237,30.0712359781232));
#79719=CARTESIAN_POINT('Ctrl Pts',(204.475023784296,9.94794254402139,30.0294054890345));
#79720=CARTESIAN_POINT('Ctrl Pts',(204.47817997384,9.92687791862971,29.9875449555498));
#79721=CARTESIAN_POINT('Ctrl Pts',(204.481336163384,9.90831687996344,29.9444278478773));
#79722=CARTESIAN_POINT('Ctrl Pts',(204.484492352928,9.89239647383176,29.9003866772505));
#79723=CARTESIAN_POINT('Ctrl Pts',(204.487649506968,9.87647120260323,29.8563320481379));
#79724=CARTESIAN_POINT('Ctrl Pts',(204.490806661008,9.86318833913874,29.8113533321652));
#79725=CARTESIAN_POINT('Ctrl Pts',(204.493963815047,9.85263516109169,29.7657987752735));
#79726=CARTESIAN_POINT('Ctrl Pts',(204.497127144096,9.84206134231471,29.7201551192213));
#79727=CARTESIAN_POINT('Ctrl Pts',(204.500290473144,9.83422797565444,29.6739339282284));
#79728=CARTESIAN_POINT('Ctrl Pts',(204.503453802192,9.82917094541982,29.6274926956766));
#79729=CARTESIAN_POINT('Ctrl Pts',(204.50634682987,9.82454603027125,29.5850197916237));
#79730=CARTESIAN_POINT('Ctrl Pts',(204.509239857548,9.82224263537602,29.5423632453761));
#79731=CARTESIAN_POINT('Ctrl Pts',(204.512132885225,9.82225001771146,29.4997957468552));
#79732=CARTESIAN_POINT('',(204.899997647687,10.8098243290602,30.6622944018977));
#79733=CARTESIAN_POINT('Ctrl Pts',(204.512132885264,9.82225001771156,29.4997957462862));
#79734=CARTESIAN_POINT('Ctrl Pts',(204.512893439603,9.82225195847519,29.4886050840047));
#79735=CARTESIAN_POINT('Ctrl Pts',(204.513653993942,9.8224133915092,29.4774159819222));
#79736=CARTESIAN_POINT('Ctrl Pts',(204.514414548282,9.82273420589625,29.4662314860668));
#79737=CARTESIAN_POINT('Ctrl Pts',(204.517691710729,9.82411656716551,29.418038466954));
#79738=CARTESIAN_POINT('Ctrl Pts',(204.520968873176,9.82846618208739,29.3698219095396));
#79739=CARTESIAN_POINT('Ctrl Pts',(204.524246035624,9.83578244468732,29.3219759948721));
#79740=CARTESIAN_POINT('Ctrl Pts',(204.527420481918,9.84286939355581,29.2756297154456));
#79741=CARTESIAN_POINT('Ctrl Pts',(204.530594928212,9.85273966328401,29.2296317836103));
#79742=CARTESIAN_POINT('Ctrl Pts',(204.533769374506,9.86534000748018,29.1843391632227));
#79743=CARTESIAN_POINT('Ctrl Pts',(204.53694069231,9.87792793374334,29.1390911797687));
#79744=CARTESIAN_POINT('Ctrl Pts',(204.540112010113,9.89324046023478,29.0945476658318));
#79745=CARTESIAN_POINT('Ctrl Pts',(204.543283327916,9.91117340460796,29.0510548945951));
#79746=CARTESIAN_POINT('Ctrl Pts',(204.546452910818,9.92909653858145,29.0075859165215));
#79747=CARTESIAN_POINT('Ctrl Pts',(204.549622493719,9.94963703863887,28.965167056149));
#79748=CARTESIAN_POINT('Ctrl Pts',(204.552792076621,9.97264193779918,28.9241263380472));
#79749=CARTESIAN_POINT('Ctrl Pts',(204.555961315207,9.99564433790623,28.883090078254));
#79750=CARTESIAN_POINT('Ctrl Pts',(204.559130553792,10.0211103315968,28.8434321476796));
#79751=CARTESIAN_POINT('Ctrl Pts',(204.562299792378,10.048841461537,28.8054551870406));
#79752=CARTESIAN_POINT('Ctrl Pts',(204.565472205846,10.0766003719902,28.7674401818121));
#79753=CARTESIAN_POINT('Ctrl Pts',(204.568644619314,10.1066286158871,28.7311099554934));
#79754=CARTESIAN_POINT('Ctrl Pts',(204.571817032781,10.1386861062732,28.6967357601803));
#79755=CARTESIAN_POINT('Ctrl Pts',(204.57499138483,10.1707631861689,28.6623405596787));
#79756=CARTESIAN_POINT('Ctrl Pts',(204.578165736878,10.2048715767345,28.6299041524169));
#79757=CARTESIAN_POINT('Ctrl Pts',(204.581340088926,10.2407354097751,28.5996598728643));
#79758=CARTESIAN_POINT('Ctrl Pts',(204.584520042633,10.2766625303599,28.5693622223802));
#79759=CARTESIAN_POINT('Ctrl Pts',(204.58769999634,10.314350824734,28.541264745237));
#79760=CARTESIAN_POINT('Ctrl Pts',(204.590879950047,10.3534941684928,28.5155583956744));
#79761=CARTESIAN_POINT('Ctrl Pts',(204.59160878237,10.3624656620405,28.5096666059832));
#79762=CARTESIAN_POINT('Ctrl Pts',(204.592337614693,10.3715134882872,28.5039002332347));
#79763=CARTESIAN_POINT('Ctrl Pts',(204.593066447016,10.3806337904139,28.498261231197));
#79764=CARTESIAN_POINT('Ctrl Pts',(204.596343609463,10.4216428273245,28.4729057068416));
#79765=CARTESIAN_POINT('Ctrl Pts',(204.599620771911,10.4643037186516,28.4500154946675));
#79766=CARTESIAN_POINT('Ctrl Pts',(204.602897934358,10.5082868708975,28.4298069047278));
#79767=CARTESIAN_POINT('Ctrl Pts',(204.606072182813,10.5508888033101,28.4102329329044));
#79768=CARTESIAN_POINT('Ctrl Pts',(204.609246431269,10.5947306225305,28.3931748907485));
#79769=CARTESIAN_POINT('Ctrl Pts',(204.612420679724,10.6394849311947,28.3787846113862));
#79770=CARTESIAN_POINT('Ctrl Pts',(204.615591809407,10.6841952677083,28.3644084708086));
#79771=CARTESIAN_POINT('Ctrl Pts',(204.618762939089,10.7298157913554,28.3526950744201));
#79772=CARTESIAN_POINT('Ctrl Pts',(204.621934068771,10.7760000228538,28.3437478334124));
#79773=CARTESIAN_POINT('Ctrl Pts',(204.625103473532,10.8221591326404,28.3348054592175));
#79774=CARTESIAN_POINT('Ctrl Pts',(204.628272878292,10.8688807971651,28.3286263652757));
#79775=CARTESIAN_POINT('Ctrl Pts',(204.631442283052,10.9158069516336,28.3252631813437));
#79776=CARTESIAN_POINT('Ctrl Pts',(204.634611353751,10.9627281599921,28.321900351898));
#79777=CARTESIAN_POINT('Ctrl Pts',(204.637780424449,11.0098532603664,28.3213528806569));
#79778=CARTESIAN_POINT('Ctrl Pts',(204.640949495148,11.0568203743606,28.3236214437701));
#79779=CARTESIAN_POINT('Ctrl Pts',(204.644121756859,11.10383478065,28.325892291153));
#79780=CARTESIAN_POINT('Ctrl Pts',(204.647294018569,11.1506903263654,28.3309848015154));
#79781=CARTESIAN_POINT('Ctrl Pts',(204.65046628028,11.1970284568235,28.3388476199474));
#79782=CARTESIAN_POINT('Ctrl Pts',(204.653640489855,11.2433950402878,28.3467152663865));
#79783=CARTESIAN_POINT('Ctrl Pts',(204.65681469943,11.2892430339211,28.357356479953));
#79784=CARTESIAN_POINT('Ctrl Pts',(204.659988909005,11.3342258791852,28.3706691697368));
#79785=CARTESIAN_POINT('Ctrl Pts',(204.663168734926,11.3792883156843,28.3840054145763));
#79786=CARTESIAN_POINT('Ctrl Pts',(204.666348560848,11.4234820289682,28.400022371368));
#79787=CARTESIAN_POINT('Ctrl Pts',(204.66952838677,11.4664792212056,28.4185693740774));
#79788=CARTESIAN_POINT('Ctrl Pts',(204.670258373096,11.4763500013037,28.4228271726846));
#79789=CARTESIAN_POINT('Ctrl Pts',(204.670988359423,11.4861578265088,28.4272181176327));
#79790=CARTESIAN_POINT('Ctrl Pts',(204.67171834575,11.4958989262837,28.4317400515742));
#79791=CARTESIAN_POINT('Ctrl Pts',(204.674995508197,11.5396301102882,28.4520405853768));
#79792=CARTESIAN_POINT('Ctrl Pts',(204.678272670645,11.5822124998671,28.4750772168618));
#79793=CARTESIAN_POINT('Ctrl Pts',(204.681549833092,11.6232835343469,28.5006938915867));
#79794=CARTESIAN_POINT('Ctrl Pts',(204.684720990222,11.6630260573188,28.5254819519951));
#79795=CARTESIAN_POINT('Ctrl Pts',(204.687892147353,11.701352999871,28.5526853558338));
#79796=CARTESIAN_POINT('Ctrl Pts',(204.691063304483,11.7379578236565,28.5821147604389));
#79797=CARTESIAN_POINT('Ctrl Pts',(204.694231337706,11.774526588025,28.6115151741334));
#79798=CARTESIAN_POINT('Ctrl Pts',(204.697399370929,11.8093761583506,28.6431369004431));
#79799=CARTESIAN_POINT('Ctrl Pts',(204.700567404152,11.8422299025174,28.6767480010315));
#79800=CARTESIAN_POINT('Ctrl Pts',(204.703733713565,11.8750657700944,28.7103408129325));
#79801=CARTESIAN_POINT('Ctrl Pts',(204.706900022977,11.905907573397,28.7459204564798));
#79802=CARTESIAN_POINT('Ctrl Pts',(204.71006633239,11.9345146968104,28.7832173663199));
#79803=CARTESIAN_POINT('Ctrl Pts',(204.713232315092,11.9631188684441,28.8205104277387));
#79804=CARTESIAN_POINT('Ctrl Pts',(204.716398297794,11.9894884804504,28.8595199597774));
#79805=CARTESIAN_POINT('Ctrl Pts',(204.719564280496,12.0134242008582,28.8999446262095));
#79806=CARTESIAN_POINT('Ctrl Pts',(204.722733487946,12.0373843012709,28.9404104676531));
#79807=CARTESIAN_POINT('Ctrl Pts',(204.725902695396,12.0589052809648,28.9822938374839));
#79808=CARTESIAN_POINT('Ctrl Pts',(204.729071902847,12.0778330889414,29.0252675544236));
#79809=CARTESIAN_POINT('Ctrl Pts',(204.732243074755,12.0967726294682,29.0682679089586));
#79810=CARTESIAN_POINT('Ctrl Pts',(204.735414246663,12.1131156063047,29.1123594320846));
#79811=CARTESIAN_POINT('Ctrl Pts',(204.738585418572,12.1267569467799,29.1571970750076));
#79812=CARTESIAN_POINT('Ctrl Pts',(204.741762260819,12.1404226791918,29.2021148916462));
#79813=CARTESIAN_POINT('Ctrl Pts',(204.744939103066,12.1513770134583,29.247780946518));
#79814=CARTESIAN_POINT('Ctrl Pts',(204.748115945314,12.1595657696491,29.2938391687104));
#79815=CARTESIAN_POINT('Ctrl Pts',(204.748867378371,12.1615026936814,29.3047335310979));
#79816=CARTESIAN_POINT('Ctrl Pts',(204.749618811427,12.1632851163349,29.3156498153152));
#79817=CARTESIAN_POINT('Ctrl Pts',(204.750370244484,12.1649127461391,29.3265832868996));
#79818=CARTESIAN_POINT('Ctrl Pts',(204.753647406931,12.1720111925336,29.3742665265072));
#79819=CARTESIAN_POINT('Ctrl Pts',(204.756924569379,12.1761928797529,29.4224921053704));
#79820=CARTESIAN_POINT('Ctrl Pts',(204.760201731826,12.1773897634831,29.4708725671355));
#79821=CARTESIAN_POINT('Ctrl Pts',(204.763380803022,12.1785508223725,29.5178049163603));
#79822=CARTESIAN_POINT('Ctrl Pts',(204.766559874218,12.1769032410329,29.564882406677));
#79823=CARTESIAN_POINT('Ctrl Pts',(204.769738945413,12.1724369784728,29.6117434293802));
#79824=CARTESIAN_POINT('Ctrl Pts',(204.772914862409,12.1679751472337,29.6585579576738));
#79825=CARTESIAN_POINT('Ctrl Pts',(204.776090779405,12.1607002235794,29.7051558935741));
#79826=CARTESIAN_POINT('Ctrl Pts',(204.779266696401,12.1506541863793,29.7511772399477));
#79827=CARTESIAN_POINT('Ctrl Pts',(204.782440843553,12.1406137475358,29.7971729399991));
#79828=CARTESIAN_POINT('Ctrl Pts',(204.785614990705,12.1278053729575,29.8425921459696));
#79829=CARTESIAN_POINT('Ctrl Pts',(204.788789137858,12.1123222703681,29.8870842664629));
#79830=CARTESIAN_POINT('Ctrl Pts',(204.79196289648,12.0968410629802,29.9315709409205));
#79831=CARTESIAN_POINT('Ctrl Pts',(204.795136655102,12.0786859618688,29.9751302321802));
#79832=CARTESIAN_POINT('Ctrl Pts',(204.798310413724,12.0579994206949,30.0174285344946));
#79833=CARTESIAN_POINT('Ctrl Pts',(204.801487248844,12.0372928269251,30.0597678388671));
#79834=CARTESIAN_POINT('Ctrl Pts',(204.804664083965,12.0140501425046,30.1008432169051));
#79835=CARTESIAN_POINT('Ctrl Pts',(204.807840919085,11.9884603266246,30.1403446300152));
#79836=CARTESIAN_POINT('Ctrl Pts',(204.811019639365,11.9628553255382,30.1798694835873));
#79837=CARTESIAN_POINT('Ctrl Pts',(204.814198359645,11.9349007495811,30.217818066111));
#79838=CARTESIAN_POINT('Ctrl Pts',(204.817377079925,11.9048274810867,30.253911328984));
#79839=CARTESIAN_POINT('Ctrl Pts',(204.820561282099,11.874702349435,30.2900668368558));
#79840=CARTESIAN_POINT('Ctrl Pts',(204.823745484273,11.8424516184588,30.324360240831));
#79841=CARTESIAN_POINT('Ctrl Pts',(204.826929686447,11.8083434499435,30.3565488482471));
#79842=CARTESIAN_POINT('Ctrl Pts',(204.827627172037,11.8008722044781,30.3635996222307));
#79843=CARTESIAN_POINT('Ctrl Pts',(204.828324657628,11.793311960662,30.3705495616509));
#79844=CARTESIAN_POINT('Ctrl Pts',(204.829022143218,11.7856657360398,30.3773963834625));
#79845=CARTESIAN_POINT('Ctrl Pts',(204.832160484023,11.7512615002151,30.4082037013083));
#79846=CARTESIAN_POINT('Ctrl Pts',(204.835298824828,11.7149584985154,30.4370593463094));
#79847=CARTESIAN_POINT('Ctrl Pts',(204.838437165633,11.6770096964571,30.4637182852904));
#79848=CARTESIAN_POINT('Ctrl Pts',(204.8415710348,11.6391149654251,30.49033923951));
#79849=CARTESIAN_POINT('Ctrl Pts',(204.844704903967,11.599579532835,30.5147693478104));
#79850=CARTESIAN_POINT('Ctrl Pts',(204.847838773134,11.5586905173501,30.5368027624978));
#79851=CARTESIAN_POINT('Ctrl Pts',(204.850969639116,11.5178406857839,30.5588150625773));
#79852=CARTESIAN_POINT('Ctrl Pts',(204.854100505098,11.4756403384177,30.5784349409332));
#79853=CARTESIAN_POINT('Ctrl Pts',(204.85723137108,11.4324043118212,30.5955006041159));
#79854=CARTESIAN_POINT('Ctrl Pts',(204.860360696891,11.3891895543849,30.6125578721627));
#79855=CARTESIAN_POINT('Ctrl Pts',(204.863490022701,11.3449406583823,30.6270632035716));
#79856=CARTESIAN_POINT('Ctrl Pts',(204.866619348512,11.2999930468601,30.6389026448014));
#79857=CARTESIAN_POINT('Ctrl Pts',(204.869750597747,11.2550178085163,30.6507493630838));
#79858=CARTESIAN_POINT('Ctrl Pts',(204.872881846982,11.2093435496543,30.6599267660785));
#79859=CARTESIAN_POINT('Ctrl Pts',(204.876013096216,11.1633193090463,30.6663712384111));
#79860=CARTESIAN_POINT('Ctrl Pts',(204.879145355631,11.1172802204449,30.6728177898108));
#79861=CARTESIAN_POINT('Ctrl Pts',(204.882277615046,11.0708914961412,30.6765296033856));
#79862=CARTESIAN_POINT('Ctrl Pts',(204.885409874461,11.0245070441812,30.6774949967136));
#79863=CARTESIAN_POINT('Ctrl Pts',(204.888547402122,10.9780445767542,30.6784620137669));
#79864=CARTESIAN_POINT('Ctrl Pts',(204.891684929782,10.9315869687223,30.676673411482));
#79865=CARTESIAN_POINT('Ctrl Pts',(204.894822457443,10.8854858481198,30.6721696001514));
#79866=CARTESIAN_POINT('Ctrl Pts',(204.896547520857,10.8601387069477,30.6696933318934));
#79867=CARTESIAN_POINT('Ctrl Pts',(204.898272584272,10.8348992087756,30.6663971766041));
#79868=CARTESIAN_POINT('Ctrl Pts',(204.899997647687,10.8098243290602,30.6622944018976));
#79869=CARTESIAN_POINT('',(204.9,12.0381913065552,30.0561059912401));
#79870=CARTESIAN_POINT('Origin',(204.9,11.,29.5));
#79871=CARTESIAN_POINT('Ctrl Pts',(204.9,12.0381913065552,30.0561059912401));
#79872=CARTESIAN_POINT('Ctrl Pts',(204.8997621394,12.0398535320846,30.0530027912723));
#79873=CARTESIAN_POINT('Ctrl Pts',(204.89952497894,12.0415018578031,30.0498921132293));
#79874=CARTESIAN_POINT('Ctrl Pts',(204.899013325775,12.0450378088497,30.0431462212962));
#79875=CARTESIAN_POINT('Ctrl Pts',(204.898739072365,12.0469204737467,30.0395084450192));
#79876=CARTESIAN_POINT('Ctrl Pts',(204.897680308448,12.0541376476317,30.0253830292433));
#79877=CARTESIAN_POINT('Ctrl Pts',(204.89690203245,12.0593340221635,30.0148251714119));
#79878=CARTESIAN_POINT('Ctrl Pts',(204.892716259105,12.0866302329651,29.9572015369054));
#79879=CARTESIAN_POINT('Ctrl Pts',(204.889419901625,12.1057547581559,29.9087857804606));
#79880=CARTESIAN_POINT('Ctrl Pts',(204.88277133655,12.1378588951479,29.8085562301249));
#79881=CARTESIAN_POINT('Ctrl Pts',(204.879426409703,12.1506424663593,29.7568101653783));
#79882=CARTESIAN_POINT('Ctrl Pts',(204.873957668299,12.1654413373207,29.6728239710727));
#79883=CARTESIAN_POINT('Ctrl Pts',(204.871880972903,12.1697110786283,29.6410581390914));
#79884=CARTESIAN_POINT('Ctrl Pts',(204.86888439387,12.1739260763192,29.5957771724359));
#79885=CARTESIAN_POINT('Ctrl Pts',(204.867993052736,12.1749425694157,29.5823749751506));
#79886=CARTESIAN_POINT('Ctrl Pts',(204.866414377093,12.1763264255328,29.5587805592554));
#79887=CARTESIAN_POINT('Ctrl Pts',(204.865729800394,12.1767911863115,29.5485953429596));
#79888=CARTESIAN_POINT('Ctrl Pts',(204.864283413661,12.1774897790295,29.5271836312266));
#79889=CARTESIAN_POINT('Ctrl Pts',(204.863520879776,12.1776954105801,29.5159573038996));
#79890=CARTESIAN_POINT('Ctrl Pts',(204.861460576082,12.1778165078225,29.4858051968804));
#79891=CARTESIAN_POINT('Ctrl Pts',(204.860154549293,12.1774363518464,29.4668822054782));
#79892=CARTESIAN_POINT('Ctrl Pts',(204.851760518394,12.1721170338875,29.3465745301024));
#79893=CARTESIAN_POINT('Ctrl Pts',(204.84429566794,12.1545442070436,29.2461938481589));
#79894=CARTESIAN_POINT('Ctrl Pts',(204.832481771872,12.1068316636469,29.0932147548902));
#79895=CARTESIAN_POINT('Ctrl Pts',(204.828171512584,12.0851503279611,29.0384798070805));
#79896=CARTESIAN_POINT('Ctrl Pts',(204.823333120496,12.0550535108067,28.9764932034397));
#79897=CARTESIAN_POINT('Ctrl Pts',(204.822628894145,12.0505205545771,28.9674552991932));
#79898=CARTESIAN_POINT('Ctrl Pts',(204.821530312826,12.0431997640778,28.9533162876739));
#79899=CARTESIAN_POINT('Ctrl Pts',(204.821131560455,12.0404897145043,28.9481757646331));
#79900=CARTESIAN_POINT('Ctrl Pts',(204.820380238465,12.0352809514194,28.9384704004453));
#79901=CARTESIAN_POINT('Ctrl Pts',(204.820027264506,12.0327899591039,28.9339019150734));
#79902=CARTESIAN_POINT('Ctrl Pts',(204.819251361133,12.0272177924107,28.9238417617422));
#79903=CARTESIAN_POINT('Ctrl Pts',(204.818829303563,12.0241227628582,28.9183581173867));
#79904=CARTESIAN_POINT('Ctrl Pts',(204.817372035183,12.0132196290819,28.8993972727712));
#79905=CARTESIAN_POINT('Ctrl Pts',(204.816349865883,12.005187907466,28.8860496927542));
#79906=CARTESIAN_POINT('Ctrl Pts',(204.810677945495,11.9586168467305,28.8120204159697));
#79907=CARTESIAN_POINT('Ctrl Pts',(204.806276193001,11.9148462150769,28.7548014717858));
#79908=CARTESIAN_POINT('Ctrl Pts',(204.800859524225,11.8555976668415,28.6905007113916));
#79909=CARTESIAN_POINT('Ctrl Pts',(204.799895492085,11.8448443379115,28.6792841537973));
#79910=CARTESIAN_POINT('Ctrl Pts',(204.796717948592,11.8088265218339,28.643172966142));
#79911=CARTESIAN_POINT('Ctrl Pts',(204.794488948545,11.7826606131208,28.6192077368393));
#79912=CARTESIAN_POINT('Ctrl Pts',(204.790623897005,11.7363554295078,28.5804916860132));
#79913=CARTESIAN_POINT('Ctrl Pts',(204.789010268092,11.7167557547728,28.5651332147385));
#79914=CARTESIAN_POINT('Ctrl Pts',(204.786622134294,11.6874922607355,28.5436635249152));
#79915=CARTESIAN_POINT('Ctrl Pts',(204.785866986079,11.6782021358176,28.5370530077902));
#79916=CARTESIAN_POINT('Ctrl Pts',(204.784516542602,11.6615351404257,28.5255542079479));
#79917=CARTESIAN_POINT('Ctrl Pts',(204.783923370422,11.6541963053092,28.5206121655161));
#79918=CARTESIAN_POINT('Ctrl Pts',(204.782661341268,11.6385496556531,28.510329890232));
#79919=CARTESIAN_POINT('Ctrl Pts',(204.781991751255,11.630228998063,28.5050105586854));
#79920=CARTESIAN_POINT('Ctrl Pts',(204.780170726628,11.6075561671157,28.4909144920433));
#79921=CARTESIAN_POINT('Ctrl Pts',(204.779011906754,11.5930817216433,28.4823399007452));
#79922=CARTESIAN_POINT('Ctrl Pts',(204.770989069588,11.4926125388997,28.4256939284209));
#79923=CARTESIAN_POINT('Ctrl Pts',(204.763732780374,11.401079393115,28.3882769545885));
#79924=CARTESIAN_POINT('Ctrl Pts',(204.753631994265,11.2688033510141,28.3526891134676));
#79925=CARTESIAN_POINT('Ctrl Pts',(204.750804328036,11.2311523543663,28.3445146195401));
#79926=CARTESIAN_POINT('Ctrl Pts',(204.746960200983,11.1784255428744,28.3357480122263));
#79927=CARTESIAN_POINT('Ctrl Pts',(204.745894692865,11.1636384986637,28.3335777553877));
#79928=CARTESIAN_POINT('Ctrl Pts',(204.744046256935,11.1376194936769,28.3302635875255));
#79929=CARTESIAN_POINT('Ctrl Pts',(204.743258128614,11.1264050946354,28.3289986437637));
#79930=CARTESIAN_POINT('Ctrl Pts',(204.742075044553,11.1093614911839,28.3273239002478));
#79931=CARTESIAN_POINT('Ctrl Pts',(204.741673878754,11.1035449080758,28.3267959993782));
#79932=CARTESIAN_POINT('Ctrl Pts',(204.740926438267,11.0926327594941,28.3258874247159));
#79933=CARTESIAN_POINT('Ctrl Pts',(204.740579582805,11.0875382366932,28.3254966039862));
#79934=CARTESIAN_POINT('Ctrl Pts',(204.73977870613,11.0757085508936,28.3246665027824));
#79935=CARTESIAN_POINT('Ctrl Pts',(204.739326029258,11.0689717577804,28.3242519332794));
#79936=CARTESIAN_POINT('Ctrl Pts',(204.737878475276,11.0472819280288,28.3231042529416));
#79937=CARTESIAN_POINT('Ctrl Pts',(204.736894886709,11.0323177233119,28.3225982866763));
#79938=CARTESIAN_POINT('Ctrl Pts',(204.731117051202,10.9433771928577,28.3212881356391));
#79939=CARTESIAN_POINT('Ctrl Pts',(204.726587413168,10.8694606630325,28.3271701914354));
#79940=CARTESIAN_POINT('Ctrl Pts',(204.718423111919,10.7396533226863,28.3499327253727));
#79941=CARTESIAN_POINT('Ctrl Pts',(204.714821888093,10.6835456352904,28.3640902866266));
#79942=CARTESIAN_POINT('Ctrl Pts',(204.709666519717,10.6075550195903,28.3893340893997));
#79943=CARTESIAN_POINT('Ctrl Pts',(204.708215569518,10.5866082330783,28.396959214733));
#79944=CARTESIAN_POINT('Ctrl Pts',(204.70600285836,10.5554215912255,28.4093250019287));
#79945=CARTESIAN_POINT('Ctrl Pts',(204.705255329852,10.5450121928987,28.413626218097));
#79946=CARTESIAN_POINT('Ctrl Pts',(204.703946108039,10.5270108615761,28.4213685589823));
#79947=CARTESIAN_POINT('Ctrl Pts',(204.703386678647,10.5193906882608,28.4247422661992));
#79948=CARTESIAN_POINT('Ctrl Pts',(204.702114415478,10.5022269844102,28.4325601151705));
#79949=CARTESIAN_POINT('Ctrl Pts',(204.701400026632,10.4927060586697,28.4370518697298));
#79950=CARTESIAN_POINT('Ctrl Pts',(204.699449334287,10.467031355635,28.4495881197688));
#79951=CARTESIAN_POINT('Ctrl Pts',(204.698204932061,10.4510007458687,28.4578769495896));
#79952=CARTESIAN_POINT('Ctrl Pts',(204.691579123177,10.367502300047,28.503512184149));
#79953=CARTESIAN_POINT('Ctrl Pts',(204.685988565283,10.3036426338576,28.5470444743933));
#79954=CARTESIAN_POINT('Ctrl Pts',(204.677061702671,10.2099690235038,28.625372822217));
#79955=CARTESIAN_POINT('Ctrl Pts',(204.673766637479,10.1771167262118,28.6562079076123));
#79956=CARTESIAN_POINT('Ctrl Pts',(204.668803075765,10.1294807006603,28.7063538972275));
#79957=CARTESIAN_POINT('Ctrl Pts',(204.66709033462,10.1133930330931,28.7243671937004));
#79958=CARTESIAN_POINT('Ctrl Pts',(204.664846260019,10.0926593639401,28.74907143223));
#79959=CARTESIAN_POINT('Ctrl Pts',(204.664286092104,10.0875133527247,28.7553330467909));
#79960=CARTESIAN_POINT('Ctrl Pts',(204.663357978279,10.0790305112331,28.7658748706159));
#79961=CARTESIAN_POINT('Ctrl Pts',(204.662987703017,10.0756579503402,28.7701258437393));
#79962=CARTESIAN_POINT('Ctrl Pts',(204.662228769661,10.0687673346919,28.7789355507026));
#79963=CARTESIAN_POINT('Ctrl Pts',(204.661840366852,10.0652531093118,28.7834970545875));
#79964=CARTESIAN_POINT('Ctrl Pts',(204.660794245967,10.0558262370379,28.7959206483484));
#79965=CARTESIAN_POINT('Ctrl Pts',(204.660140676092,10.0499782613084,28.8038315294323));
#79966=CARTESIAN_POINT('Ctrl Pts',(204.656251258742,10.0154831567366,28.8517392778778));
#79967=CARTESIAN_POINT('Ctrl Pts',(204.653148647334,9.98926276363873,28.8934303479486));
#79968=CARTESIAN_POINT('Ctrl Pts',(204.645799026573,9.93286816337074,28.9969661573862));
#79969=CARTESIAN_POINT('Ctrl Pts',(204.641593877423,9.90535244248988,29.060045484077));
#79970=CARTESIAN_POINT('Ctrl Pts',(204.634885854393,9.87156267080785,29.1606934057659));
#79971=CARTESIAN_POINT('Ctrl Pts',(204.632483470342,9.86133807472025,29.1967700871807));
#79972=CARTESIAN_POINT('Ctrl Pts',(204.629143052692,9.84979343198479,29.2464212002093));
#79973=CARTESIAN_POINT('Ctrl Pts',(204.628251747704,9.8469621351811,29.2596231813895));
#79974=CARTESIAN_POINT('Ctrl Pts',(204.626721994398,9.84252851621573,29.2821815627156));
#79975=CARTESIAN_POINT('Ctrl Pts',(204.626087168365,9.8408111635584,29.2915141729892));
#79976=CARTESIAN_POINT('Ctrl Pts',(204.62479374824,9.83756041306616,29.3104634964701));
#79977=CARTESIAN_POINT('Ctrl Pts',(204.624135018228,9.83603314421863,29.320080494722));
#79978=CARTESIAN_POINT('Ctrl Pts',(204.622466227357,9.83248665838815,29.3443514920207));
#79979=CARTESIAN_POINT('Ctrl Pts',(204.621451449481,9.83062399535249,29.3590262912858));
#79980=CARTESIAN_POINT('Ctrl Pts',(204.617293943785,9.82418039852081,29.4187816436883));
#79981=CARTESIAN_POINT('Ctrl Pts',(204.614082568928,9.82192689548017,29.4640689578767));
#79982=CARTESIAN_POINT('Ctrl Pts',(204.605180762538,9.82290861423555,29.5874750785639));
#79983=CARTESIAN_POINT('Ctrl Pts',(204.599389406086,9.83129804255859,29.6653197939489));
#79984=CARTESIAN_POINT('Ctrl Pts',(204.591428354726,9.85385487288358,29.7728677207805));
#79985=CARTESIAN_POINT('Ctrl Pts',(204.589153131017,9.86163712014357,29.8037034215908));
#79986=CARTESIAN_POINT('Ctrl Pts',(204.586321260908,9.8731481269769,29.8426031463734));
#79987=CARTESIAN_POINT('Ctrl Pts',(204.585713078908,9.87573204446398,29.8509895086234));
#79988=CARTESIAN_POINT('Ctrl Pts',(204.584730963057,9.88009160156128,29.8645965354617));
#79989=CARTESIAN_POINT('Ctrl Pts',(204.584354015249,9.88181054208747,29.8698348197347));
#79990=CARTESIAN_POINT('Ctrl Pts',(204.583651927284,9.88509935238766,29.8796245315236));
#79991=CARTESIAN_POINT('Ctrl Pts',(204.583326298668,9.88666044773974,29.8841787106893));
#79992=CARTESIAN_POINT('Ctrl Pts',(204.582459780755,9.89090916277573,29.896330057781));
#79993=CARTESIAN_POINT('Ctrl Pts',(204.581921709043,9.89364696839344,29.9039096164536));
#79994=CARTESIAN_POINT('Ctrl Pts',(204.579883315049,9.90439061225302,29.9327240656868));
#79995=CARTESIAN_POINT('Ctrl Pts',(204.57841037789,9.91293228610771,29.9537554258736));
#79996=CARTESIAN_POINT('Ctrl Pts',(204.572669531453,9.9490803079368,30.0358680904623));
#79997=CARTESIAN_POINT('Ctrl Pts',(204.568566189962,9.98127216169274,30.0947955784569));
#79998=CARTESIAN_POINT('Ctrl Pts',(204.561501206555,10.0442084259457,30.1897506761016));
#79999=CARTESIAN_POINT('Ctrl Pts',(204.558575493033,10.0724146180511,30.2272387055263));
#80000=CARTESIAN_POINT('Ctrl Pts',(204.55557810053,10.1027691095676,30.2629362959998));
#80001=CARTESIAN_POINT('Ctrl Pts',(198.520303559452,10.4906978680325,30.5595938614862));
#80002=CARTESIAN_POINT('Ctrl Pts',(198.54655243945,10.1411874905847,30.3915989467844));
#80003=CARTESIAN_POINT('Ctrl Pts',(198.599050199445,9.6273193758111,29.6852027538047));
#80004=CARTESIAN_POINT('Ctrl Pts',(198.677796839438,10.0915926961985,28.4524239122179));
#80005=CARTESIAN_POINT('Ctrl Pts',(198.756543479431,11.3767175053669,28.166546434716));
#80006=CARTESIAN_POINT('Ctrl Pts',(198.835290119423,12.3213447234544,29.0822494362045));
#80007=CARTESIAN_POINT('Ctrl Pts',(198.914036759416,12.0746318004869,30.3752124421159));
#80008=CARTESIAN_POINT('Ctrl Pts',(198.992783399409,10.8585526214878,30.8785952513234));
#80009=CARTESIAN_POINT('Ctrl Pts',(199.071530039402,9.77012615756758,30.1387612927136));
#80010=CARTESIAN_POINT('Ctrl Pts',(199.150276679395,9.79086261747825,28.822782934047));
#80011=CARTESIAN_POINT('Ctrl Pts',(199.229023319388,10.9021199481224,28.1176026645591));
#80012=CARTESIAN_POINT('Ctrl Pts',(199.307769959381,12.1016443134302,28.6591711062653));
#80013=CARTESIAN_POINT('Ctrl Pts',(199.386516599373,12.3076180711695,29.9590757800039));
#80014=CARTESIAN_POINT('Ctrl Pts',(199.465263239366,11.3342701062169,30.8449444178606));
#80015=CARTESIAN_POINT('Ctrl Pts',(199.544009879359,10.0594504089439,30.5178309587577));
#80016=CARTESIAN_POINT('Ctrl Pts',(199.622756519352,9.63289662650049,29.2727515562712));
#80017=CARTESIAN_POINT('Ctrl Pts',(199.701503159345,10.4393114539152,28.232624181157));
#80018=CARTESIAN_POINT('Ctrl Pts',(199.780249799338,11.7514020703729,28.3355223410407));
#80019=CARTESIAN_POINT('Ctrl Pts',(199.858996439331,12.3858154013911,29.4886440980506));
#80020=CARTESIAN_POINT('Ctrl Pts',(199.937743079323,11.7703842663141,30.6520075205645));
#80021=CARTESIAN_POINT('Ctrl Pts',(200.016489719316,10.4601560671557,30.7763940594563));
#80022=CARTESIAN_POINT('Ctrl Pts',(200.095236359309,9.63680435061106,29.7496214849068));
#80023=CARTESIAN_POINT('Ctrl Pts',(200.173982999302,10.0428966880961,28.4977193452295));
#80024=CARTESIAN_POINT('Ctrl Pts',(200.252729639295,11.3121849809262,28.1497578732641));
#80025=CARTESIAN_POINT('Ctrl Pts',(200.331476279288,12.2999187025004,29.0195578811959));
#80026=CARTESIAN_POINT('Ctrl Pts',(200.41022291928,12.1152768251165,30.3226608448567));
#80027=CARTESIAN_POINT('Ctrl Pts',(200.488969559273,10.9247848643951,30.8838193328497));
#80028=CARTESIAN_POINT('Ctrl Pts',(200.567716199266,9.80212821472357,30.1969336041217));
#80029=CARTESIAN_POINT('Ctrl Pts',(200.646462839259,9.75981270382478,28.8814947592023));
#80030=CARTESIAN_POINT('Ctrl Pts',(200.725209479252,10.8360020047419,28.1238757613965));
#80031=CARTESIAN_POINT('Ctrl Pts',(200.803956119245,12.0600984382385,28.6073608994928));
#80032=CARTESIAN_POINT('Ctrl Pts',(200.882702759238,12.3281092805904,29.8959027675046));
#80033=CARTESIAN_POINT('Ctrl Pts',(200.96144939923,11.3983198990878,30.8273863493732));
#80034=CARTESIAN_POINT('Ctrl Pts',(201.040196039223,10.1092922596587,30.5617217073256));
#80035=CARTESIAN_POINT('Ctrl Pts',(201.118942679216,9.62357948773663,29.3385074740712));
#80036=CARTESIAN_POINT('Ctrl Pts',(201.197689319209,10.3792380561133,28.2609407312269));
#80037=CARTESIAN_POINT('Ctrl Pts',(201.276435959202,11.6947517555518,28.3008614505954));
#80038=CARTESIAN_POINT('Ctrl Pts',(201.355182599195,12.3836801125892,29.4222657827231));
#80039=CARTESIAN_POINT('Ctrl Pts',(201.433929239188,11.8246898135138,30.613777344893));
#80040=CARTESIAN_POINT('Ctrl Pts',(201.51267587918,10.5219251446065,30.8007911804555));
#80041=CARTESIAN_POINT('Ctrl Pts',(201.591422519173,9.65032843542909,29.814642543689));
#80042=CARTESIAN_POINT('Ctrl Pts',(201.670169159166,9.99597862438151,28.544722898939));
#80043=CARTESIAN_POINT('Ctrl Pts',(201.748915799159,11.2471394110297,28.136352181087));
#80044=CARTESIAN_POINT('Ctrl Pts',(201.827662439152,12.2754091704247,28.9578333185203));
#80045=CARTESIAN_POINT('Ctrl Pts',(201.906409079145,12.153408080749,30.2682857943327));
#80046=CARTESIAN_POINT('Ctrl Pts',(201.985155719137,10.9911669464399,30.8858337705782));
#80047=CARTESIAN_POINT('Ctrl Pts',(202.06390235913,9.83689219990197,30.2535207414938));
#80048=CARTESIAN_POINT('Ctrl Pts',(202.142648999123,9.73160551758984,28.9416195745714));
#80049=CARTESIAN_POINT('Ctrl Pts',(202.221395639116,10.7702632509767,28.1333126587772));
#80050=CARTESIAN_POINT('Ctrl Pts',(202.300142279109,12.0161168329507,28.5575988941514));
#80051=CARTESIAN_POINT('Ctrl Pts',(202.378888919102,12.345551120398,29.8318214051353));
#80052=CARTESIAN_POINT('Ctrl Pts',(202.457635559095,11.461454671499,30.8067795715665));
#80053=CARTESIAN_POINT('Ctrl Pts',(202.536382199087,10.1611797372155,30.6031744328302));
#80054=CARTESIAN_POINT('Ctrl Pts',(202.61512883908,9.61742319582523,29.4046341619453));
#80055=CARTESIAN_POINT('Ctrl Pts',(202.693875479073,10.3205902545797,28.2921027939644));
#80056=CARTESIAN_POINT('Ctrl Pts',(202.772622119066,11.6365059455802,28.2689543291454));
#80057=CARTESIAN_POINT('Ctrl Pts',(202.851368759059,12.3783672456924,29.3560659924908));
#80058=CARTESIAN_POINT('Ctrl Pts',(202.930115399052,11.8771014781942,30.5729894032756));
#80059=CARTESIAN_POINT('Ctrl Pts',(203.008862039045,10.5847921103831,30.8222010704512));
#80060=CARTESIAN_POINT('Ctrl Pts',(203.087608679037,9.66695200530575,29.8789410329763));
#80061=CARTESIAN_POINT('Ctrl Pts',(203.16635531903,9.9513662702466,28.5939202220822));
#80062=CARTESIAN_POINT('Ctrl Pts',(203.245101959023,11.1815262916617,28.1260780713519));
#80063=CARTESIAN_POINT('Ctrl Pts',(203.323848599016,12.2479706941989,28.8973538263122));
#80064=CARTESIAN_POINT('Ctrl Pts',(203.402595239009,12.1888905644702,30.2121463982623));
#80065=CARTESIAN_POINT('Ctrl Pts',(203.481341879002,11.057569313348,30.8846656706159));
#80066=CARTESIAN_POINT('Ctrl Pts',(203.560088518995,9.87432723218788,30.3083774508533));
#80067=CARTESIAN_POINT('Ctrl Pts',(203.638835158987,9.70631116638201,29.0030266693794));
#80068=CARTESIAN_POINT('Ctrl Pts',(203.71758179898,10.7050520820644,28.1458881738925));
#80069=CARTESIAN_POINT('Ctrl Pts',(203.796328438973,11.9698017408791,28.5100009735364));
#80070=CARTESIAN_POINT('Ctrl Pts',(203.875075078966,12.3599029382575,29.7669782619617));
#80071=CARTESIAN_POINT('Ctrl Pts',(203.953821718959,11.5235297221299,30.7831713140073));
#80072=CARTESIAN_POINT('Ctrl Pts',(204.032568358952,10.2149935501509,30.6420947708184));
#80073=CARTESIAN_POINT('Ctrl Pts',(204.111314998944,9.61444194280345,29.4709777328597));
#80074=CARTESIAN_POINT('Ctrl Pts',(204.190061638937,10.2635027270343,28.3260431590116));
#80075=CARTESIAN_POINT('Ctrl Pts',(204.26880827893,11.5767983600888,28.2398651595848));
#80076=CARTESIAN_POINT('Ctrl Pts',(204.347554918923,12.3698891101204,29.2902156265541));
#80077=CARTESIAN_POINT('Ctrl Pts',(204.426301558916,11.9274986610999,30.5296982380858));
#80078=CARTESIAN_POINT('Ctrl Pts',(204.505048198909,10.648613086735,30.8406556465544));
#80079=CARTESIAN_POINT('Ctrl Pts',(204.583794838902,9.68663581581289,29.9422012341082));
#80080=CARTESIAN_POINT('Ctrl Pts',(204.662541478895,9.90916386048687,28.6455463696896));
#80081=CARTESIAN_POINT('Ctrl Pts',(204.741288118887,11.1154852624214,28.1182320587536));
#80082=CARTESIAN_POINT('Ctrl Pts',(204.82004122376,12.2177166671994,28.8398027453881));
#80083=CARTESIAN_POINT('Ctrl Pts',(204.872545448635,12.2194357483118,29.7134875651393));
#80084=CARTESIAN_POINT('Ctrl Pts',(204.898800793512,12.0361954097,30.0553619354564));
#80085=CARTESIAN_POINT('Ctrl Pts',(198.576061721773,10.448859910947,30.6466369734669));
#80086=CARTESIAN_POINT('Ctrl Pts',(198.602310601771,10.0706380884556,30.4648416766526));
#80087=CARTESIAN_POINT('Ctrl Pts',(198.654808361766,9.51455693198427,29.7004167189139));
#80088=CARTESIAN_POINT('Ctrl Pts',(198.733555001759,10.0169691998355,28.3663680317231));
#80089=CARTESIAN_POINT('Ctrl Pts',(198.812301641752,11.4076639511671,28.0570064003472));
#80090=CARTESIAN_POINT('Ctrl Pts',(198.891048281745,12.4298900453077,29.0479322223869));
#80091=CARTESIAN_POINT('Ctrl Pts',(198.969794921737,12.1629102433391,30.4471090596551));
#80092=CARTESIAN_POINT('Ctrl Pts',(199.048541561731,10.8469330562424,30.9918435676819));
#80093=CARTESIAN_POINT('Ctrl Pts',(199.127288201723,9.6690949507249,30.1912340115086));
#80094=CARTESIAN_POINT('Ctrl Pts',(199.206034841716,9.69153486142714,28.7671511650745));
#80095=CARTESIAN_POINT('Ctrl Pts',(199.284781481709,10.8940793349912,28.0040420160462));
#80096=CARTESIAN_POINT('Ctrl Pts',(199.363528121702,12.1921417698824,28.5900990153309));
#80097=CARTESIAN_POINT('Ctrl Pts',(199.442274761695,12.4150357812317,29.9967877619047));
#80098=CARTESIAN_POINT('Ctrl Pts',(199.521021401688,11.3617295992783,30.9554283983997));
#80099=CARTESIAN_POINT('Ctrl Pts',(199.59976804168,9.98218650023936,30.6014433477502));
#80100=CARTESIAN_POINT('Ctrl Pts',(199.678514681673,9.52059234053389,29.2540836378792));
#80101=CARTESIAN_POINT('Ctrl Pts',(199.757261321666,10.3932522253021,28.1285122762744));
#80102=CARTESIAN_POINT('Ctrl Pts',(199.836007961659,11.8131279607647,28.2398632749097));
#80103=CARTESIAN_POINT('Ctrl Pts',(199.914754601652,12.4996568358807,29.4877112377529));
#80104=CARTESIAN_POINT('Ctrl Pts',(199.993501241645,11.8336694988909,30.7466421945276));
#80105=CARTESIAN_POINT('Ctrl Pts',(200.072247881638,10.4158091738726,30.8812467913257));
#80106=CARTESIAN_POINT('Ctrl Pts',(200.15099452163,9.52482107487274,29.7701272953434));
#80107=CARTESIAN_POINT('Ctrl Pts',(200.229741161623,9.96427293065161,28.4153843766718));
#80108=CARTESIAN_POINT('Ctrl Pts',(200.308487801616,11.3378302335473,28.038838698559));
#80109=CARTESIAN_POINT('Ctrl Pts',(200.387234441609,12.406703927765,28.9800907054531));
#80110=CARTESIAN_POINT('Ctrl Pts',(200.465981081602,12.2068941599339,30.3902404738483));
#80111=CARTESIAN_POINT('Ctrl Pts',(200.544727721595,10.9186061201527,30.9974967950628));
#80112=CARTESIAN_POINT('Ctrl Pts',(200.623474361587,9.70372590065377,30.254185039744));
#80113=CARTESIAN_POINT('Ctrl Pts',(200.70222100158,9.65793427132171,28.8306860268263));
#80114=CARTESIAN_POINT('Ctrl Pts',(200.780967641573,10.8225299600418,28.0108304328474));
#80115=CARTESIAN_POINT('Ctrl Pts',(200.859714281566,12.1471829999977,28.5340327234736));
#80116=CARTESIAN_POINT('Ctrl Pts',(200.938460921559,12.4372102947006,29.9284252368941));
#80117=CARTESIAN_POINT('Ctrl Pts',(201.017207561552,11.4310409300796,30.9364279764058));
#80118=CARTESIAN_POINT('Ctrl Pts',(201.095954201545,10.036122740277,30.648939616774));
#80119=CARTESIAN_POINT('Ctrl Pts',(201.174700841537,9.51050982101215,29.3252412477091));
#80120=CARTESIAN_POINT('Ctrl Pts',(201.25344748153,10.3282439409536,28.1591549634882));
#80121=CARTESIAN_POINT('Ctrl Pts',(201.332194121523,11.7518239575108,28.2023550748697));
#80122=CARTESIAN_POINT('Ctrl Pts',(201.410940761516,12.4973461381895,29.4158801019212));
#80123=CARTESIAN_POINT('Ctrl Pts',(201.489687401509,11.892436117448,30.7052715009815));
#80124=CARTESIAN_POINT('Ctrl Pts',(201.568434041502,10.4826524339143,30.9076480777059));
#80125=CARTESIAN_POINT('Ctrl Pts',(201.647180681494,9.5394561310469,29.8404896792376));
#80126=CARTESIAN_POINT('Ctrl Pts',(201.725927321488,9.91350065975225,28.4662491603656));
#80127=CARTESIAN_POINT('Ctrl Pts',(201.80467396148,11.2674413250092,28.0243317606992));
#80128=CARTESIAN_POINT('Ctrl Pts',(201.883420601473,12.380180996006,28.9132956169691));
#80129=CARTESIAN_POINT('Ctrl Pts',(201.962167241466,12.2481578073955,30.3313986424342));
#80130=CARTESIAN_POINT('Ctrl Pts',(202.040913881459,10.9904413321285,30.9996767140528));
#80131=CARTESIAN_POINT('Ctrl Pts',(202.119660521452,9.74134566441371,30.3154206756722));
#80132=CARTESIAN_POINT('Ctrl Pts',(202.198407161445,9.62740993192143,28.8957499525728));
#80133=CARTESIAN_POINT('Ctrl Pts',(202.277153801437,10.7513909242313,28.0210425488711));
#80134=CARTESIAN_POINT('Ctrl Pts',(202.35590044143,12.0995884105907,28.4801828879167));
#80135=CARTESIAN_POINT('Ctrl Pts',(202.434647081423,12.4560849401055,29.8590797432351));
#80136=CARTESIAN_POINT('Ctrl Pts',(202.513393721416,11.49936207367,30.9141284008834));
#80137=CARTESIAN_POINT('Ctrl Pts',(202.592140361409,10.0922726505296,30.6937975849468));
#80138=CARTESIAN_POINT('Ctrl Pts',(202.670887001402,9.50384780438328,29.3968000854914));
#80139=CARTESIAN_POINT('Ctrl Pts',(202.749633641394,10.2647783622114,28.1928769154577));
#80140=CARTESIAN_POINT('Ctrl Pts',(202.828380281387,11.68879339298,28.1678268593889));
#80141=CARTESIAN_POINT('Ctrl Pts',(202.90712692138,12.4915968319313,29.3442421565958));
#80142=CARTESIAN_POINT('Ctrl Pts',(202.985873561373,11.9491532755479,30.661132927109));
#80143=CARTESIAN_POINT('Ctrl Pts',(203.064620201366,10.5506837711931,30.9308167391706));
#80144=CARTESIAN_POINT('Ctrl Pts',(203.143366841359,9.55744528759493,29.9100701362738));
#80145=CARTESIAN_POINT('Ctrl Pts',(203.222113481352,9.86522350698284,28.5194879264268));
#80146=CARTESIAN_POINT('Ctrl Pts',(203.300860121344,11.1964382441623,28.0132136573202));
#80147=CARTESIAN_POINT('Ctrl Pts',(203.379606761337,12.3504885143112,28.8478478785262));
#80148=CARTESIAN_POINT('Ctrl Pts',(203.45835340133,12.2865550926423,30.2706475286895));
#80149=CARTESIAN_POINT('Ctrl Pts',(203.537100041323,11.0622984953209,30.9984126574607));
#80150=CARTESIAN_POINT('Ctrl Pts',(203.615846681316,9.78185589543917,30.3747837330477));
#80151=CARTESIAN_POINT('Ctrl Pts',(203.694593321309,9.60003771000796,28.9622014939599));
#80152=CARTESIAN_POINT('Ctrl Pts',(203.773339961301,10.6808228131128,28.0346511126009));
#80153=CARTESIAN_POINT('Ctrl Pts',(203.852086601294,12.0494686440188,28.4286749114918));
#80154=CARTESIAN_POINT('Ctrl Pts',(203.930833241287,12.4716157256189,29.788909890293));
#80155=CARTESIAN_POINT('Ctrl Pts',(204.00957988128,11.5665364418599,30.888580781196));
#80156=CARTESIAN_POINT('Ctrl Pts',(204.088326521273,10.150507140024,30.7359151360001));
#80157=CARTESIAN_POINT('Ctrl Pts',(204.167073161266,9.50062164852651,29.4685936227394));
#80158=CARTESIAN_POINT('Ctrl Pts',(204.245819801259,10.2030012302491,28.2296054006543));
#80159=CARTESIAN_POINT('Ctrl Pts',(204.324566441252,11.6241809715519,28.1363480838334));
#80160=CARTESIAN_POINT('Ctrl Pts',(204.403313081244,12.4824222377153,29.2729823399399));
#80161=CARTESIAN_POINT('Ctrl Pts',(204.482059721237,12.0036904669934,30.6142854958097));
#80162=CARTESIAN_POINT('Ctrl Pts',(204.56080636123,10.6197474887435,30.9507873147457));
#80163=CARTESIAN_POINT('Ctrl Pts',(204.639553001223,9.57874607625232,29.9785270122555));
#80164=CARTESIAN_POINT('Ctrl Pts',(204.718299641216,9.81955426977905,28.5753550390969));
#80165=CARTESIAN_POINT('Ctrl Pts',(204.797046281209,11.1249721016664,28.0047231134747));
#80166=CARTESIAN_POINT('Ctrl Pts',(204.875799386081,12.3177491910527,28.7855691133793));
#80167=CARTESIAN_POINT('Ctrl Pts',(204.928303610957,12.319609490584,29.7310250601308));
#80168=CARTESIAN_POINT('Ctrl Pts',(204.954558955833,12.121316394597,30.1009835956933));
#80169=CARTESIAN_POINT('Ctrl Pts',(198.631819884095,10.4070219538616,30.7336800854477));
#80170=CARTESIAN_POINT('Ctrl Pts',(198.658068764092,10.0000886863265,30.5380844065209));
#80171=CARTESIAN_POINT('Ctrl Pts',(198.710566524088,9.40179448815744,29.7156306840231));
#80172=CARTESIAN_POINT('Ctrl Pts',(198.78931316408,9.94234570347243,28.2803121512281));
#80173=CARTESIAN_POINT('Ctrl Pts',(198.868059804073,11.4386103969674,27.9474663659784));
#80174=CARTESIAN_POINT('Ctrl Pts',(198.946806444066,12.5384353671611,29.0136150085693));
#80175=CARTESIAN_POINT('Ctrl Pts',(199.025553084059,12.2511886861915,30.5190056771942));
#80176=CARTESIAN_POINT('Ctrl Pts',(199.104299724052,10.8353134909969,31.1050918840403));
#80177=CARTESIAN_POINT('Ctrl Pts',(199.183046364045,9.56806374388221,30.2437067303035));
#80178=CARTESIAN_POINT('Ctrl Pts',(199.261793004038,9.59220710537601,28.7115193961018));
#80179=CARTESIAN_POINT('Ctrl Pts',(199.34053964403,10.8860387218602,27.8904813675333));
#80180=CARTESIAN_POINT('Ctrl Pts',(199.419286284023,12.2826392263346,28.5210269243967));
#80181=CARTESIAN_POINT('Ctrl Pts',(199.498032924016,12.522453491294,30.0344997438053));
#80182=CARTESIAN_POINT('Ctrl Pts',(199.576779564009,11.3891890923396,31.0659123789388));
#80183=CARTESIAN_POINT('Ctrl Pts',(199.655526204002,9.90492259153486,30.6850557367427));
#80184=CARTESIAN_POINT('Ctrl Pts',(199.734272843994,9.40828805456728,29.2354157194871));
#80185=CARTESIAN_POINT('Ctrl Pts',(199.813019483988,10.3471929966891,28.0244003713917));
#80186=CARTESIAN_POINT('Ctrl Pts',(199.89176612398,11.8748538511566,28.1442042087787));
#80187=CARTESIAN_POINT('Ctrl Pts',(199.970512763973,12.6134982703702,29.4867783774552));
#80188=CARTESIAN_POINT('Ctrl Pts',(200.049259403966,11.8969547314676,30.8412768684909));
#80189=CARTESIAN_POINT('Ctrl Pts',(200.128006043959,10.3714622805895,30.986099523195));
#80190=CARTESIAN_POINT('Ctrl Pts',(200.206752683952,9.41283779913442,29.7906331057803));
#80191=CARTESIAN_POINT('Ctrl Pts',(200.285499323945,9.88564917320709,28.3330494081142));
#80192=CARTESIAN_POINT('Ctrl Pts',(200.364245963937,11.3634754861682,27.9279195238539));
#80193=CARTESIAN_POINT('Ctrl Pts',(200.44299260393,12.5134891530294,28.9406235297101));
#80194=CARTESIAN_POINT('Ctrl Pts',(200.521739243923,12.2985114947512,30.4578201028399));
#80195=CARTESIAN_POINT('Ctrl Pts',(200.600485883916,10.9124273759101,31.1111742572759));
#80196=CARTESIAN_POINT('Ctrl Pts',(200.679232523909,9.60532358658397,30.3114364753665));
#80197=CARTESIAN_POINT('Ctrl Pts',(200.757979163902,9.55605583881862,28.7798772944504));
#80198=CARTESIAN_POINT('Ctrl Pts',(200.836725803895,10.8090579153417,27.8977851042985));
#80199=CARTESIAN_POINT('Ctrl Pts',(200.915472443887,12.2342675617569,28.4607045474545));
#80200=CARTESIAN_POINT('Ctrl Pts',(200.99421908388,12.5463113088109,29.9609477062835));
#80201=CARTESIAN_POINT('Ctrl Pts',(201.072965723873,11.4637619610715,31.0454696034384));
#80202=CARTESIAN_POINT('Ctrl Pts',(201.151712363866,9.96295322089544,30.7361575262224));
#80203=CARTESIAN_POINT('Ctrl Pts',(201.230459003859,9.39744015428766,29.3119750213469));
#80204=CARTESIAN_POINT('Ctrl Pts',(201.309205643852,10.2772498257939,28.0573691957494));
#80205=CARTESIAN_POINT('Ctrl Pts',(201.387952283845,11.8088961594698,28.1038486991439));
#80206=CARTESIAN_POINT('Ctrl Pts',(201.466698923837,12.6110121637899,29.4094944211192));
#80207=CARTESIAN_POINT('Ctrl Pts',(201.54544556383,11.9601824213823,30.7967656570699));
#80208=CARTESIAN_POINT('Ctrl Pts',(201.624192203823,10.4433797232223,31.0145049749563));
#80209=CARTESIAN_POINT('Ctrl Pts',(201.702938843816,9.42858382666472,29.8663368147861));
#80210=CARTESIAN_POINT('Ctrl Pts',(201.781685483809,9.83102269512299,28.3877754217921));
#80211=CARTESIAN_POINT('Ctrl Pts',(201.860432123801,11.2877432389887,27.9123113403115));
#80212=CARTESIAN_POINT('Ctrl Pts',(201.939178763795,12.4849528215873,28.868757915418));
#80213=CARTESIAN_POINT('Ctrl Pts',(202.017925403787,12.342907534042,30.3945114905358));
#80214=CARTESIAN_POINT('Ctrl Pts',(202.09667204378,10.9897157178171,31.1135196575275));
#80215=CARTESIAN_POINT('Ctrl Pts',(202.175418683773,9.64579912892547,30.3773206098504));
#80216=CARTESIAN_POINT('Ctrl Pts',(202.254165323766,9.52321434625301,28.8498803305741));
#80217=CARTESIAN_POINT('Ctrl Pts',(202.332911963759,10.732518597486,27.9087724389652));
#80218=CARTESIAN_POINT('Ctrl Pts',(202.411658603752,12.1830599882308,28.4027668816818));
#80219=CARTESIAN_POINT('Ctrl Pts',(202.490405243744,12.5666187598128,29.8863380813349));
#80220=CARTESIAN_POINT('Ctrl Pts',(202.569151883737,11.5372694758411,31.0214772302005));
#80221=CARTESIAN_POINT('Ctrl Pts',(202.64789852373,10.0233655638437,30.7844207370633));
#80222=CARTESIAN_POINT('Ctrl Pts',(202.726645163723,9.39027241294133,29.3889660090376));
#80223=CARTESIAN_POINT('Ctrl Pts',(202.805391803716,10.208966469843,28.093651036951));
#80224=CARTESIAN_POINT('Ctrl Pts',(202.884138443709,11.7410808403797,28.0666993896324));
#80225=CARTESIAN_POINT('Ctrl Pts',(202.962885083701,12.6048264181704,29.3324183207009));
#80226=CARTESIAN_POINT('Ctrl Pts',(203.041631723694,12.0212050729015,30.7492764509423));
#80227=CARTESIAN_POINT('Ctrl Pts',(203.120378363687,10.5165754320031,31.0394324078902));
#80228=CARTESIAN_POINT('Ctrl Pts',(203.19912500368,9.4479385698841,29.9411992395711));
#80229=CARTESIAN_POINT('Ctrl Pts',(203.277871643673,9.7790807437191,28.4450556307714));
#80230=CARTESIAN_POINT('Ctrl Pts',(203.356618283666,11.2113501966631,27.9003492432886));
#80231=CARTESIAN_POINT('Ctrl Pts',(203.435364923658,12.4530063344234,28.7983419307402));
#80232=CARTESIAN_POINT('Ctrl Pts',(203.514111563651,12.3842196208143,30.3291486591167));
#80233=CARTESIAN_POINT('Ctrl Pts',(203.592858203644,11.0670276772939,31.1121596443056));
#80234=CARTESIAN_POINT('Ctrl Pts',(203.671604843637,9.68938455869046,30.4411900152422));
#80235=CARTESIAN_POINT('Ctrl Pts',(203.75035148363,9.49376425363389,28.9213763185404));
#80236=CARTESIAN_POINT('Ctrl Pts',(203.829098123623,10.6565935441613,27.9234140513093));
#80237=CARTESIAN_POINT('Ctrl Pts',(203.907844763616,12.1291355471585,28.3473488494473));
#80238=CARTESIAN_POINT('Ctrl Pts',(203.986591403609,12.5833285129804,29.8108415186245));
#80239=CARTESIAN_POINT('Ctrl Pts',(204.065338043601,11.60954316159,30.9939902483847));
#80240=CARTESIAN_POINT('Ctrl Pts',(204.144084683594,10.086020729897,30.8297355011819));
#80241=CARTESIAN_POINT('Ctrl Pts',(204.222831323587,9.38680135424956,29.466209512619));
#80242=CARTESIAN_POINT('Ctrl Pts',(204.30157796358,10.1424997334639,28.1331676422972));
#80243=CARTESIAN_POINT('Ctrl Pts',(204.380324603573,11.6715635830151,28.0328310080821));
#80244=CARTESIAN_POINT('Ctrl Pts',(204.459071243566,12.5949553653103,29.2557490533256));
#80245=CARTESIAN_POINT('Ctrl Pts',(204.537817883559,12.0798822728867,30.6988727535335));
#80246=CARTESIAN_POINT('Ctrl Pts',(204.616564523551,10.590881890752,31.0609189829369));
#80247=CARTESIAN_POINT('Ctrl Pts',(204.695311163544,9.47085633669177,30.0148527904026));
#80248=CARTESIAN_POINT('Ctrl Pts',(204.774057803537,9.72994467907122,28.5051637085043));
#80249=CARTESIAN_POINT('Ctrl Pts',(204.85280444353,11.1344589409116,27.8912141681958));
#80250=CARTESIAN_POINT('Ctrl Pts',(204.931557548403,12.417781714906,28.7313354813706));
#80251=CARTESIAN_POINT('Ctrl Pts',(204.984061773278,12.4197832328561,29.7485625551224));
#80252=CARTESIAN_POINT('Ctrl Pts',(205.010317118156,12.2064373794939,30.1466052559301));
#80253=CARTESIAN_POINT('Ctrl Pts',(198.687578046416,10.3651839967761,30.8207231974284));
#80254=CARTESIAN_POINT('Ctrl Pts',(198.713826926414,9.92953928419742,30.6113271363891));
#80255=CARTESIAN_POINT('Ctrl Pts',(198.766324686409,9.2890320443306,29.7308446491323));
#80256=CARTESIAN_POINT('Ctrl Pts',(198.845071326402,9.86772220710937,28.1942562707332));
#80257=CARTESIAN_POINT('Ctrl Pts',(198.923817966395,11.4695568427676,27.8379263316095));
#80258=CARTESIAN_POINT('Ctrl Pts',(199.002564606388,12.6469806890144,28.9792977947516));
#80259=CARTESIAN_POINT('Ctrl Pts',(199.08131124638,12.3394671290437,30.5909022947333));
#80260=CARTESIAN_POINT('Ctrl Pts',(199.160057886373,10.8236939257515,31.2183402003988));
#80261=CARTESIAN_POINT('Ctrl Pts',(199.238804526366,9.46703253703953,30.2961794490986));
#80262=CARTESIAN_POINT('Ctrl Pts',(199.317551166359,9.49287934932489,28.6558876271292));
#80263=CARTESIAN_POINT('Ctrl Pts',(199.396297806352,10.8779981087292,27.7769207190204));
#80264=CARTESIAN_POINT('Ctrl Pts',(199.475044446344,12.3731366827867,28.4519548334623));
#80265=CARTESIAN_POINT('Ctrl Pts',(199.553791086337,12.6298712013562,30.0722117257062));
#80266=CARTESIAN_POINT('Ctrl Pts',(199.63253772633,11.4166485854008,31.1763963594777));
#80267=CARTESIAN_POINT('Ctrl Pts',(199.711284366323,9.82765868283031,30.7686681257351));
#80268=CARTESIAN_POINT('Ctrl Pts',(199.790031006316,9.29598376860071,29.2167478010951));
#80269=CARTESIAN_POINT('Ctrl Pts',(199.868777646309,10.301133768076,27.9202884665091));
#80270=CARTESIAN_POINT('Ctrl Pts',(199.947524286302,11.9365797415486,28.0485451426477));
#80271=CARTESIAN_POINT('Ctrl Pts',(200.026270926294,12.7273397048599,29.4858455171576));
#80272=CARTESIAN_POINT('Ctrl Pts',(200.105017566287,11.9602399640443,30.9359115424541));
#80273=CARTESIAN_POINT('Ctrl Pts',(200.18376420628,10.3271153873065,31.0909522550645));
#80274=CARTESIAN_POINT('Ctrl Pts',(200.262510846273,9.30085452339609,29.811138916217));
#80275=CARTESIAN_POINT('Ctrl Pts',(200.341257486266,9.80702541576257,28.2507144395565));
#80276=CARTESIAN_POINT('Ctrl Pts',(200.420004126259,11.3891207387892,27.8170003491488));
#80277=CARTESIAN_POINT('Ctrl Pts',(200.498750766252,12.6202743782939,28.9011563539673));
#80278=CARTESIAN_POINT('Ctrl Pts',(200.577497406244,12.3901288295685,30.5253997318316));
#80279=CARTESIAN_POINT('Ctrl Pts',(200.656244046237,10.9062486316675,31.2248517194891));
#80280=CARTESIAN_POINT('Ctrl Pts',(200.73499068623,9.50692127251416,30.3686879109888));
#80281=CARTESIAN_POINT('Ctrl Pts',(200.813737326223,9.45417740631555,28.7290685620745));
#80282=CARTESIAN_POINT('Ctrl Pts',(200.892483966216,10.7955858706416,27.7847397757495));
#80283=CARTESIAN_POINT('Ctrl Pts',(200.971230606209,12.3213521235159,28.3873763714354));
#80284=CARTESIAN_POINT('Ctrl Pts',(201.049977246202,12.6554123229211,29.993470175673));
#80285=CARTESIAN_POINT('Ctrl Pts',(201.128723886194,11.4964829920634,31.1545112304711));
#80286=CARTESIAN_POINT('Ctrl Pts',(201.207470526187,9.88978370151384,30.8233754356706));
#80287=CARTESIAN_POINT('Ctrl Pts',(201.28621716618,9.28437048756318,29.2987087949847));
#80288=CARTESIAN_POINT('Ctrl Pts',(201.364963806173,10.2262557106342,27.9555834280108));
#80289=CARTESIAN_POINT('Ctrl Pts',(201.443710446166,11.8659683614289,28.0053423234181));
#80290=CARTESIAN_POINT('Ctrl Pts',(201.522457086159,12.7246781893901,29.4031087403172));
#80291=CARTESIAN_POINT('Ctrl Pts',(201.601203726151,12.0279287253164,30.8882598131583));
#80292=CARTESIAN_POINT('Ctrl Pts',(201.679950366144,10.4041070125303,31.1213618722067));
#80293=CARTESIAN_POINT('Ctrl Pts',(201.758697006137,9.31771152228255,29.8921839503347));
#80294=CARTESIAN_POINT('Ctrl Pts',(201.83744364613,9.74854473049371,28.3093016832186));
#80295=CARTESIAN_POINT('Ctrl Pts',(201.916190286123,11.3080451529682,27.8002909199237));
#80296=CARTESIAN_POINT('Ctrl Pts',(201.994936926116,12.5897246471684,28.8242202138668));
#80297=CARTESIAN_POINT('Ctrl Pts',(202.073683566109,12.4376572606885,30.4576243386374));
#80298=CARTESIAN_POINT('Ctrl Pts',(202.152430206102,10.9889901035058,31.227362601002));
#80299=CARTESIAN_POINT('Ctrl Pts',(202.231176846094,9.55025259343721,30.4392205440286));
#80300=CARTESIAN_POINT('Ctrl Pts',(202.309923486087,9.4190187605846,28.8040107085755));
#80301=CARTESIAN_POINT('Ctrl Pts',(202.38867012608,10.7136462707406,27.7965023290593));
#80302=CARTESIAN_POINT('Ctrl Pts',(202.467416766073,12.266531565871,28.325350875447));
#80303=CARTESIAN_POINT('Ctrl Pts',(202.546163406066,12.6771525795203,29.9135964194346));
#80304=CARTESIAN_POINT('Ctrl Pts',(202.624910046059,11.5751768780122,31.1288260595174));
#80305=CARTESIAN_POINT('Ctrl Pts',(202.703656686051,9.95445847715783,30.8750438891797));
#80306=CARTESIAN_POINT('Ctrl Pts',(202.782403326044,9.27669702149938,29.3811319325837));
#80307=CARTESIAN_POINT('Ctrl Pts',(202.861149966037,10.1531545774746,27.9944251584444));
#80308=CARTESIAN_POINT('Ctrl Pts',(202.93989660603,11.7933682877795,27.9655719198759));
#80309=CARTESIAN_POINT('Ctrl Pts',(203.018643246023,12.7180560044093,29.320594484806));
#80310=CARTESIAN_POINT('Ctrl Pts',(203.097389886016,12.0932568702551,30.8374199747755));
#80311=CARTESIAN_POINT('Ctrl Pts',(203.176136526008,10.4824670928131,31.1480480766096));
#80312=CARTESIAN_POINT('Ctrl Pts',(203.254883166001,9.33843185217328,29.9723283428685));
#80313=CARTESIAN_POINT('Ctrl Pts',(203.333629805994,9.69293798045533,28.3706233351159));
#80314=CARTESIAN_POINT('Ctrl Pts',(203.412376445987,11.2262621491638,27.787484829257));
#80315=CARTESIAN_POINT('Ctrl Pts',(203.49112308598,12.5555241545356,28.7488359829542));
#80316=CARTESIAN_POINT('Ctrl Pts',(203.569869725973,12.4818841489864,30.3876497895438));
#80317=CARTESIAN_POINT('Ctrl Pts',(203.648616365966,11.0717568592669,31.2259066311503));
#80318=CARTESIAN_POINT('Ctrl Pts',(203.727363005958,9.59691322194175,30.5075962974366));
#80319=CARTESIAN_POINT('Ctrl Pts',(203.806109645951,9.38749079725985,28.8805511431208));
#80320=CARTESIAN_POINT('Ctrl Pts',(203.884856285944,10.6323642752097,27.8121769900177));
#80321=CARTESIAN_POINT('Ctrl Pts',(203.963602925937,12.2088024502983,28.2660227874026));
#80322=CARTESIAN_POINT('Ctrl Pts',(204.04234956593,12.6950413003419,29.8327731469559));
#80323=CARTESIAN_POINT('Ctrl Pts',(204.121096205923,11.65254988132,31.0993997155733));
#80324=CARTESIAN_POINT('Ctrl Pts',(204.199842845915,10.0215343197701,30.9235558663637));
#80325=CARTESIAN_POINT('Ctrl Pts',(204.278589485908,9.27298105997262,29.4638254024987));
#80326=CARTESIAN_POINT('Ctrl Pts',(204.357336125901,10.0819982366787,28.0367298839401));
#80327=CARTESIAN_POINT('Ctrl Pts',(204.436082765894,11.7189461944783,27.9293139323307));
#80328=CARTESIAN_POINT('Ctrl Pts',(204.514829405887,12.7074884929052,29.2385157667114));
#80329=CARTESIAN_POINT('Ctrl Pts',(204.59357604588,12.1560740787801,30.7834600112573));
#80330=CARTESIAN_POINT('Ctrl Pts',(204.672322685873,10.5620162927605,31.1710506511282));
#80331=CARTESIAN_POINT('Ctrl Pts',(204.751069325865,9.36296659713122,30.0511785685499));
#80332=CARTESIAN_POINT('Ctrl Pts',(204.829815965859,9.6403350883634,28.4349723779117));
#80333=CARTESIAN_POINT('Ctrl Pts',(204.908562605851,11.1439457801568,27.7777052229169));
#80334=CARTESIAN_POINT('Ctrl Pts',(204.987315710724,12.5178142387592,28.6771018493619));
#80335=CARTESIAN_POINT('Ctrl Pts',(205.039819935599,12.5199569751282,29.7661000501139));
#80336=CARTESIAN_POINT('Ctrl Pts',(205.066075280477,12.2915583643908,30.1922269161671));
#80337=CARTESIAN_POINT('',(198.742834887867,9.59283488786683,29.4999999776455));
#80338=CARTESIAN_POINT('Ctrl Pts',(198.972408128224,11.1995478642895,30.6605616167741));
#80339=CARTESIAN_POINT('Ctrl Pts',(198.966501983882,11.348264713408,30.6409839384106));
#80340=CARTESIAN_POINT('Ctrl Pts',(198.960346934242,11.492521083178,30.5932335246781));
#80341=CARTESIAN_POINT('Ctrl Pts',(198.947518383083,11.7438279441065,30.4546727204742));
#80342=CARTESIAN_POINT('Ctrl Pts',(198.939902859204,11.8722401983294,30.3575442180324));
#80343=CARTESIAN_POINT('Ctrl Pts',(198.926658933748,12.0778877277915,30.098241261682));
#80344=CARTESIAN_POINT('Ctrl Pts',(198.921294598489,12.1489157369381,29.9614237661834));
#80345=CARTESIAN_POINT('Ctrl Pts',(198.909498712764,12.2370951872888,29.6741489463717));
#80346=CARTESIAN_POINT('Ctrl Pts',(198.903140038498,12.2553418433651,29.5254782198062));
#80347=CARTESIAN_POINT('Ctrl Pts',(198.889569860502,12.2386848362927,29.2166280406198));
#80348=CARTESIAN_POINT('Ctrl Pts',(198.883054686962,12.1992248449925,29.0604998586629));
#80349=CARTESIAN_POINT('Ctrl Pts',(198.871725362742,12.0655442778753,28.7779974846995));
#80350=CARTESIAN_POINT('Ctrl Pts',(198.866407482465,11.977007093434,28.6539718304304));
#80351=CARTESIAN_POINT('Ctrl Pts',(198.853705589642,11.7478211253242,28.4273791893381));
#80352=CARTESIAN_POINT('Ctrl Pts',(198.846169447702,11.6028745119117,28.3312951172536));
#80353=CARTESIAN_POINT('Ctrl Pts',(198.830658409164,11.2500215328413,28.1877695053229));
#80354=CARTESIAN_POINT('Ctrl Pts',(198.82510348869,11.0734739644163,28.1710043522631));
#80355=CARTESIAN_POINT('Ctrl Pts',(198.814498133308,10.7702425966382,28.1727599220091));
#80356=CARTESIAN_POINT('Ctrl Pts',(198.807850967611,10.5957549738643,28.2082078386801));
#80357=CARTESIAN_POINT('Ctrl Pts',(198.79593624953,10.325286655316,28.3201894396842));
#80358=CARTESIAN_POINT('Ctrl Pts',(198.788786367281,10.175500812056,28.3975680811577));
#80359=CARTESIAN_POINT('Ctrl Pts',(198.775759760057,9.90188201278484,28.6562922654616));
#80360=CARTESIAN_POINT('Ctrl Pts',(198.770524087712,9.80098972541154,28.7967707471683));
#80361=CARTESIAN_POINT('Ctrl Pts',(198.758042229528,9.64857140583055,29.1186526630969));
#80362=CARTESIAN_POINT('Ctrl Pts',(198.750674473101,9.6026374392904,29.3007603239914));
#80363=CARTESIAN_POINT('Ctrl Pts',(198.743211014123,9.59323546930708,29.4904190941088));
#80364=CARTESIAN_POINT('Ctrl Pts',(198.743022763441,9.59302276351726,29.4952102169629));
#80365=CARTESIAN_POINT('Ctrl Pts',(198.742834886993,9.59283488699264,29.4999999775771));
#80366=CARTESIAN_POINT('',(204.9,11.0092027577153,28.0365289346043));
#80367=CARTESIAN_POINT('Ctrl Pts',(204.9,11.0092027577153,28.0365289346043));
#80368=CARTESIAN_POINT('Ctrl Pts',(204.9,11.0467246940174,28.0401107183363));
#80369=CARTESIAN_POINT('Ctrl Pts',(204.9,11.0840390001416,28.0452338732584));
#80370=CARTESIAN_POINT('Ctrl Pts',(204.9,11.1210654556941,28.0519424056269));
#80371=CARTESIAN_POINT('Ctrl Pts',(204.9,11.1772434868872,28.0621208614103));
#80372=CARTESIAN_POINT('Ctrl Pts',(204.9,11.2327603402564,28.0759472193249));
#80373=CARTESIAN_POINT('Ctrl Pts',(204.9,11.2873508399968,28.0932167979845));
#80374=CARTESIAN_POINT('Ctrl Pts',(204.9,11.3055295981515,28.0989676061907));
#80375=CARTESIAN_POINT('Ctrl Pts',(204.9,11.3236054164889,28.1051005740255));
#80376=CARTESIAN_POINT('Ctrl Pts',(204.9,11.3415677738497,28.1116090823259));
#80377=CARTESIAN_POINT('Ctrl Pts',(204.9,11.3560653465849,28.1168621552154));
#80378=CARTESIAN_POINT('Ctrl Pts',(204.9,11.3704917883079,28.1223611732078));
#80379=CARTESIAN_POINT('Ctrl Pts',(204.9,11.3848184296621,28.1280931162888));
#80380=CARTESIAN_POINT('Ctrl Pts',(204.9,11.4382112265666,28.1494550297496));
#80381=CARTESIAN_POINT('Ctrl Pts',(204.9,11.4902868729584,28.1740712692501));
#80382=CARTESIAN_POINT('Ctrl Pts',(204.9,11.540775841265,28.2017251394184));
#80383=CARTESIAN_POINT('Ctrl Pts',(204.9,11.5747780701796,28.2203488755607));
#80384=CARTESIAN_POINT('Ctrl Pts',(204.9,11.6080601401866,28.2403513100541));
#80385=CARTESIAN_POINT('Ctrl Pts',(204.9,11.6405303154535,28.2616756760846));
#80386=CARTESIAN_POINT('Ctrl Pts',(204.9,11.6552489720069,28.2713419626765));
#80387=CARTESIAN_POINT('Ctrl Pts',(204.9,11.6698006835649,28.2812799668365));
#80388=CARTESIAN_POINT('Ctrl Pts',(204.9,11.6841762722072,28.2914847959323));
#80389=CARTESIAN_POINT('Ctrl Pts',(204.9,11.6930458914565,28.2977810910501));
#80390=CARTESIAN_POINT('Ctrl Pts',(204.9,11.7018484634984,28.3041791027851));
#80391=CARTESIAN_POINT('Ctrl Pts',(204.9,11.7105703291338,28.3106688265015));
#80392=CARTESIAN_POINT('Ctrl Pts',(204.9,11.7554995199851,28.3440995221365));
#80393=CARTESIAN_POINT('Ctrl Pts',(204.9,11.7983690353811,28.3800162233986));
#80394=CARTESIAN_POINT('Ctrl Pts',(204.9,11.8389289333709,28.4182226735728));
#80395=CARTESIAN_POINT('Ctrl Pts',(204.9,11.878830470216,28.4558089633541));
#80396=CARTESIAN_POINT('Ctrl Pts',(204.9,11.916497391643,28.495612127975));
#80397=CARTESIAN_POINT('Ctrl Pts',(204.9,11.9516504462208,28.5374721453969));
#80398=CARTESIAN_POINT('Ctrl Pts',(204.9,11.9727877167464,28.562642262847));
#80399=CARTESIAN_POINT('Ctrl Pts',(204.9,11.9930152525099,28.5885564984141));
#80400=CARTESIAN_POINT('Ctrl Pts',(204.9,12.0122635537669,28.6151829584833));
#80401=CARTESIAN_POINT('Ctrl Pts',(204.9,12.0215425059034,28.6280186703339));
#80402=CARTESIAN_POINT('Ctrl Pts',(204.9,12.0305937901605,28.6410199186625));
#80403=CARTESIAN_POINT('Ctrl Pts',(204.9,12.0394090002104,28.6541832358476));
#80404=CARTESIAN_POINT('Ctrl Pts',(204.9,12.0452465725742,28.6629001939441));
#80405=CARTESIAN_POINT('Ctrl Pts',(204.9,12.0509813985653,28.6716894675584));
#80406=CARTESIAN_POINT('Ctrl Pts',(204.9,12.0566084820447,28.6805461942609));
#80407=CARTESIAN_POINT('Ctrl Pts',(204.9,12.0849733998086,28.7251910490057));
#80408=CARTESIAN_POINT('Ctrl Pts',(204.9,12.1104810950123,28.7713524632294));
#80409=CARTESIAN_POINT('Ctrl Pts',(204.9,12.1328881532658,28.8188760625729));
#80410=CARTESIAN_POINT('Ctrl Pts',(204.9,12.1410969885954,28.8362863534227));
#80411=CARTESIAN_POINT('Ctrl Pts',(204.9,12.1488892176525,28.8538796496196));
#80412=CARTESIAN_POINT('Ctrl Pts',(204.9,12.1562511770789,28.8716488877078));
#80413=CARTESIAN_POINT('Ctrl Pts',(204.9,12.176836651322,28.9213351426566));
#80414=CARTESIAN_POINT('Ctrl Pts',(204.9,12.1940617705563,28.9723971863));
#80415=CARTESIAN_POINT('Ctrl Pts',(204.9,12.2079432696189,29.0245060000646));
#80416=CARTESIAN_POINT('Ctrl Pts',(204.9,12.2140838020104,29.0475565263344));
#80417=CARTESIAN_POINT('Ctrl Pts',(204.9,12.2195693705896,29.0708118633043));
#80418=CARTESIAN_POINT('Ctrl Pts',(204.9,12.2243982001874,29.0942430113211));
#80419=CARTESIAN_POINT('Ctrl Pts',(204.9,12.2278988728214,29.1112294832984));
#80420=CARTESIAN_POINT('Ctrl Pts',(204.9,12.2310543513456,29.1283083458108));
#80421=CARTESIAN_POINT('Ctrl Pts',(204.9,12.2338633353961,29.1454683109099));
#80422=CARTESIAN_POINT('Ctrl Pts',(204.9,12.2354876524558,29.1553911953245));
#80423=CARTESIAN_POINT('Ctrl Pts',(204.9,12.2369946081418,29.1653322684556));
#80424=CARTESIAN_POINT('Ctrl Pts',(204.9,12.2383840776953,29.1752855278806));
#80425=CARTESIAN_POINT('Ctrl Pts',(204.9,12.2456448442699,29.227296954227));
#80426=CARTESIAN_POINT('Ctrl Pts',(204.9,12.2497072803007,29.2796751085222));
#80427=CARTESIAN_POINT('Ctrl Pts',(204.9,12.2506115813095,29.332111511891));
#80428=CARTESIAN_POINT('Ctrl Pts',(204.9,12.2515113959996,29.384287773545));
#80429=CARTESIAN_POINT('Ctrl Pts',(204.9,12.2492840172522,29.4365228621948));
#80430=CARTESIAN_POINT('Ctrl Pts',(204.9,12.2439194548097,29.4885008047487));
#80431=CARTESIAN_POINT('Ctrl Pts',(204.9,12.2412354063128,29.5145068993889));
#80432=CARTESIAN_POINT('Ctrl Pts',(204.9,12.2377652801437,29.540448325675));
#80433=CARTESIAN_POINT('Ctrl Pts',(204.9,12.2335034987925,29.5662830099219));
#80434=CARTESIAN_POINT('Ctrl Pts',(204.9,12.2303627085674,29.5853223075921));
#80435=CARTESIAN_POINT('Ctrl Pts',(204.9,12.226791895369,29.6043035962146));
#80436=CARTESIAN_POINT('Ctrl Pts',(204.9,12.2227878760177,29.6232092328652));
#80437=CARTESIAN_POINT('Ctrl Pts',(204.9,12.2208506527614,29.6323561514443));
#80438=CARTESIAN_POINT('Ctrl Pts',(204.9,12.2188121268174,29.6414843522619));
#80439=CARTESIAN_POINT('Ctrl Pts',(204.9,12.2166751428225,29.6505793804909));
#80440=CARTESIAN_POINT('Ctrl Pts',(204.9,12.2051403348265,29.6996716547401));
#80441=CARTESIAN_POINT('Ctrl Pts',(204.9,12.1907203877244,29.7478975714839));
#80442=CARTESIAN_POINT('Ctrl Pts',(204.9,12.1734205317272,29.7949731113051));
#80443=CARTESIAN_POINT('Ctrl Pts',(204.9,12.1564678597905,29.8411039104843));
#80444=CARTESIAN_POINT('Ctrl Pts',(204.9,12.1367492989439,29.8861308946856));
#80445=CARTESIAN_POINT('Ctrl Pts',(204.9,12.1142291617453,29.9297582081839));
#80446=CARTESIAN_POINT('Ctrl Pts',(204.9,12.0917090245467,29.9733855216821));
#80447=CARTESIAN_POINT('Ctrl Pts',(204.9,12.0663870507824,30.0156140542582));
#80448=CARTESIAN_POINT('Ctrl Pts',(204.9,12.0381913065553,30.05610599124));
#80449=CARTESIAN_POINT('Ctrl Pts',(204.9,10.9852095428848,28.0365747397361));
#80450=CARTESIAN_POINT('Ctrl Pts',(204.9,10.9932072811616,28.0365594713589));
#80451=CARTESIAN_POINT('Ctrl Pts',(204.9,11.0012050194384,28.0365442029816));
#80452=CARTESIAN_POINT('Ctrl Pts',(204.9,11.0092027577153,28.0365289346043));
#80453=CARTESIAN_POINT('Ctrl Pts',(198.742834886993,9.59283488699264,29.4999999775771));
#80454=CARTESIAN_POINT('Ctrl Pts',(198.737090843768,9.58709084143462,29.6464397908325));
#80455=CARTESIAN_POINT('Ctrl Pts',(198.732013616724,9.60462181747414,29.7916213325757));
#80456=CARTESIAN_POINT('Ctrl Pts',(198.721768578781,9.69219000241292,30.0997116657855));
#80457=CARTESIAN_POINT('Ctrl Pts',(198.716403767351,9.77035013284231,30.2572004764847));
#80458=CARTESIAN_POINT('Ctrl Pts',(198.706589374933,9.9379839780765,30.4834339409197));
#80459=CARTESIAN_POINT('Ctrl Pts',(198.702622193431,10.0115439287722,30.562750641684));
#80460=CARTESIAN_POINT('Ctrl Pts',(198.694468921762,10.1766052708443,30.7053066795134));
#80461=CARTESIAN_POINT('Ctrl Pts',(198.690304067705,10.2681818274306,30.7678059282328));
#80462=CARTESIAN_POINT('Ctrl Pts',(198.6865,10.3659929054241,30.8190402776365));
#80463=CARTESIAN_POINT('Origin',(204.9,11.,29.5));
#80464=CARTESIAN_POINT('',(204.9,11.,30.9635));
#80465=CARTESIAN_POINT('Origin',(204.9,11.,29.5));
#80466=CARTESIAN_POINT('Ctrl Pts',(204.9,10.8095183674143,30.6639494701171));
#80467=CARTESIAN_POINT('Ctrl Pts',(204.9,10.7712696975013,30.6624764558929));
#80468=CARTESIAN_POINT('Ctrl Pts',(204.9,10.7332004594639,30.6590457335319));
#80469=CARTESIAN_POINT('Ctrl Pts',(204.9,10.6954537511157,30.6536225274562));
#80470=CARTESIAN_POINT('Ctrl Pts',(204.9,10.6475314468811,30.6467373567259));
#80471=CARTESIAN_POINT('Ctrl Pts',(204.9,10.6001284968355,30.6366429213737));
#80472=CARTESIAN_POINT('Ctrl Pts',(204.9,10.5534379360125,30.6235714344056));
#80473=CARTESIAN_POINT('Ctrl Pts',(204.9,10.5362710773309,30.6187654015461));
#80474=CARTESIAN_POINT('Ctrl Pts',(204.9,10.5192004912383,30.613556412169));
#80475=CARTESIAN_POINT('Ctrl Pts',(204.9,10.5022357871601,30.6079542951409));
#80476=CARTESIAN_POINT('Ctrl Pts',(204.9,10.4916312146694,30.6044524329303));
#80477=CARTESIAN_POINT('Ctrl Pts',(204.9,10.4810727536708,30.6007984267483));
#80478=CARTESIAN_POINT('Ctrl Pts',(204.9,10.4705700758602,30.5969978312444));
#80479=CARTESIAN_POINT('Ctrl Pts',(204.9,10.4230152151206,30.5797891923453));
#80480=CARTESIAN_POINT('Ctrl Pts',(204.9,10.3765580062203,30.5595645005949));
#80481=CARTESIAN_POINT('Ctrl Pts',(204.9,10.3314093737795,30.5365807286222));
#80482=CARTESIAN_POINT('Ctrl Pts',(204.9,10.2991899201142,30.5201788015628));
#80483=CARTESIAN_POINT('Ctrl Pts',(204.9,10.2676367064342,30.5023705311667));
#80484=CARTESIAN_POINT('Ctrl Pts',(204.9,10.2368280860054,30.4832333089675));
#80485=CARTESIAN_POINT('Ctrl Pts',(204.9,10.2257215662505,30.4763343328546));
#80486=CARTESIAN_POINT('Ctrl Pts',(204.9,10.214711842786,30.4692625282535));
#80487=CARTESIAN_POINT('Ctrl Pts',(204.9,10.2038027069567,30.4620211376777));
#80488=CARTESIAN_POINT('Ctrl Pts',(204.9,10.1950670831385,30.4562225056889));
#80489=CARTESIAN_POINT('Ctrl Pts',(204.9,10.1864036448346,30.4503202091041));
#80490=CARTESIAN_POINT('Ctrl Pts',(204.9,10.1778157661554,30.4443176664685));
#80491=CARTESIAN_POINT('Ctrl Pts',(204.9,10.1342875508468,30.4138933931408));
#80492=CARTESIAN_POINT('Ctrl Pts',(204.9,10.0926859169683,30.3808888745858));
#80493=CARTESIAN_POINT('Ctrl Pts',(204.9,10.0532360341447,30.3455716202146));
#80494=CARTESIAN_POINT('Ctrl Pts',(204.9,10.0139891823114,30.3104361280342));
#80495=CARTESIAN_POINT('Ctrl Pts',(204.9,9.97687099749904,30.2730109976963));
#80496=CARTESIAN_POINT('Ctrl Pts',(204.9,9.9421187286471,30.2335108505032));
#80497=CARTESIAN_POINT('Ctrl Pts',(204.9,9.92163451139171,30.2102280657109));
#80498=CARTESIAN_POINT('Ctrl Pts',(204.9,9.90197265915035,30.1862234739019));
#80499=CARTESIAN_POINT('Ctrl Pts',(204.9,9.88318645150572,30.161534408886));
#80500=CARTESIAN_POINT('Ctrl Pts',(204.9,9.87352309519722,30.1488347072387));
#80501=CARTESIAN_POINT('Ctrl Pts',(204.9,9.86409149497076,30.1359538257004));
#80502=CARTESIAN_POINT('Ctrl Pts',(204.9,9.85489938332372,30.1228964121846));
#80503=CARTESIAN_POINT('Ctrl Pts',(204.9,9.84937935931052,30.1150552067114));
#80504=CARTESIAN_POINT('Ctrl Pts',(204.9,9.84394660300455,30.1071514450078));
#80505=CARTESIAN_POINT('Ctrl Pts',(204.9,9.83860949535559,30.099196663335));
#80506=CARTESIAN_POINT('Ctrl Pts',(204.9,9.80807359169367,30.0536839132112));
#80507=CARTESIAN_POINT('Ctrl Pts',(204.9,9.78060307134752,30.0064153274634));
#80508=CARTESIAN_POINT('Ctrl Pts',(204.9,9.7564418151761,29.9576382608005));
#80509=CARTESIAN_POINT('Ctrl Pts',(204.9,9.75084518682776,29.9463397127408));
#80510=CARTESIAN_POINT('Ctrl Pts',(204.9,9.74542623557677,29.9349600394241));
#80511=CARTESIAN_POINT('Ctrl Pts',(204.9,9.74018822887327,29.9235019929462));
#80512=CARTESIAN_POINT('Ctrl Pts',(204.9,9.71832767946602,29.8756824300249));
#80513=CARTESIAN_POINT('Ctrl Pts',(204.9,9.6996152796779,29.8265001396101));
#80514=CARTESIAN_POINT('Ctrl Pts',(204.9,9.68396802411589,29.7762398165101));
#80515=CARTESIAN_POINT('Ctrl Pts',(204.9,9.67642580370168,29.7520135594897));
#80516=CARTESIAN_POINT('Ctrl Pts',(204.9,9.66959638476633,29.7275363893671));
#80517=CARTESIAN_POINT('Ctrl Pts',(204.9,9.66347414088689,29.7028381764364));
#80518=CARTESIAN_POINT('Ctrl Pts',(204.9,9.65957072765371,29.6870911181538));
#80519=CARTESIAN_POINT('Ctrl Pts',(204.9,9.65595483418736,29.6712541813871));
#80520=CARTESIAN_POINT('Ctrl Pts',(204.9,9.65262551776375,29.655334919862));
#80521=CARTESIAN_POINT('Ctrl Pts',(204.9,9.65064506445563,29.6458653020369));
#80522=CARTESIAN_POINT('Ctrl Pts',(204.9,9.64876639256952,29.6363678821321));
#80523=CARTESIAN_POINT('Ctrl Pts',(204.9,9.64699127757553,29.6268563749219));
#80524=CARTESIAN_POINT('Ctrl Pts',(204.9,9.63682229938692,29.5723684630463));
#80525=CARTESIAN_POINT('Ctrl Pts',(204.9,9.63002532774624,29.5173152919441));
#80526=CARTESIAN_POINT('Ctrl Pts',(204.9,9.62648601813751,29.4620248108003));
#80527=CARTESIAN_POINT('Ctrl Pts',(204.9,9.62294670852878,29.4067343296565));
#80528=CARTESIAN_POINT('Ctrl Pts',(204.9,9.6226650108644,29.3512055186983));
#80529=CARTESIAN_POINT('Ctrl Pts',(204.9,9.62557417374219,29.2957426309545));
#80530=CARTESIAN_POINT('Ctrl Pts',(204.9,9.62722255400633,29.2643164326324));
#80531=CARTESIAN_POINT('Ctrl Pts',(204.9,9.62989624266107,29.2329110520043));
#80532=CARTESIAN_POINT('Ctrl Pts',(204.9,9.63358997720682,29.2015803757213));
#80533=CARTESIAN_POINT('Ctrl Pts',(204.9,9.63609588323508,29.1803249959438));
#80534=CARTESIAN_POINT('Ctrl Pts',(204.9,9.639071373389,29.1591039819646));
#80535=CARTESIAN_POINT('Ctrl Pts',(204.9,9.6425161244344,29.1379341571094));
#80536=CARTESIAN_POINT('Ctrl Pts',(204.9,9.64495055563062,29.1229732843592));
#80537=CARTESIAN_POINT('Ctrl Pts',(204.9,9.64762080578892,29.1080315224471));
#80538=CARTESIAN_POINT('Ctrl Pts',(204.9,9.65051964564107,29.093150364109));
#80539=CARTESIAN_POINT('Ctrl Pts',(204.9,9.66165233100661,29.0360008622038));
#80540=CARTESIAN_POINT('Ctrl Pts',(204.9,9.67616209913347,28.9796679258513));
#80541=CARTESIAN_POINT('Ctrl Pts',(204.9,9.69396309947139,28.9244837740775));
#80542=CARTESIAN_POINT('Ctrl Pts',(204.9,9.71191078973324,28.868844874881));
#80543=CARTESIAN_POINT('Ctrl Pts',(204.9,9.73320408854728,28.8143725695034));
#80544=CARTESIAN_POINT('Ctrl Pts',(204.9,9.75780799601074,28.7614030799068));
#80545=CARTESIAN_POINT('Ctrl Pts',(204.9,9.78241190347419,28.7084335903102));
#80546=CARTESIAN_POINT('Ctrl Pts',(204.9,9.81032638815783,28.6569656545721));
#80547=CARTESIAN_POINT('Ctrl Pts',(204.9,9.84157002494772,28.6073497615898));
#80548=CARTESIAN_POINT('Ctrl Pts',(204.9,9.84353590847449,28.6042278757691));
#80549=CARTESIAN_POINT('Ctrl Pts',(204.9,9.8455149900329,28.6011133307502));
#80550=CARTESIAN_POINT('Ctrl Pts',(204.9,9.84750728139497,28.5980062175589));
#80551=CARTESIAN_POINT('Origin',(204.9,11.,29.5));
#80552=CARTESIAN_POINT('Ctrl Pts',(198.685427081353,11.6348121556185,30.820715192556));
#80553=CARTESIAN_POINT('Ctrl Pts',(198.711644380931,11.1996942109557,31.0298580584491));
#80554=CARTESIAN_POINT('Ctrl Pts',(198.764078980087,10.1136086674488,30.9807436605481));
#80555=CARTESIAN_POINT('Ctrl Pts',(198.842730878821,9.27393396051783,29.5726451812295));
#80556=CARTESIAN_POINT('Ctrl Pts',(198.921382777556,9.99078494028664,28.0992649491572));
#80557=CARTESIAN_POINT('Ctrl Pts',(199.00003467629,11.614247459966,27.8863179216116));
#80558=CARTESIAN_POINT('Ctrl Pts',(199.078686575024,12.6857081782859,29.1255487079913));
#80559=CARTESIAN_POINT('Ctrl Pts',(199.157338473758,12.2398448395701,30.7017293637303));
#80560=CARTESIAN_POINT('Ctrl Pts',(199.235990372492,10.6784277100622,31.1964884698741));
#80561=CARTESIAN_POINT('Ctrl Pts',(199.314642271227,9.40630700003317,30.1645830946929));
#80562=CARTESIAN_POINT('Ctrl Pts',(199.393294169961,9.56838264010626,28.5346249407398));
#80563=CARTESIAN_POINT('Ctrl Pts',(199.471946068695,11.0187431449501,27.7734015618396));
#80564=CARTESIAN_POINT('Ctrl Pts',(199.550597967429,12.4522462845997,28.5659350063268));
#80565=CARTESIAN_POINT('Ctrl Pts',(199.629249866163,12.5788764490999,30.1990281642664));
#80566=CARTESIAN_POINT('Ctrl Pts',(199.707901764897,11.2846866311837,31.203069843307));
#80567=CARTESIAN_POINT('Ctrl Pts',(199.786553663632,9.73430782530876,30.6745283379686));
#80568=CARTESIAN_POINT('Ctrl Pts',(199.865205562366,9.3229189215623,29.0890352988328));
#80569=CARTESIAN_POINT('Ctrl Pts',(199.9438574611,10.4207257607197,27.8733671106996));
#80570=CARTESIAN_POINT('Ctrl Pts',(200.022509359834,12.0398184039788,28.12149687136));
#80571=CARTESIAN_POINT('Ctrl Pts',(200.101161258568,12.7231841573457,29.6101339730259));
#80572=CARTESIAN_POINT('Ctrl Pts',(200.179813157302,11.8558660427577,30.999662122572));
#80573=CARTESIAN_POINT('Ctrl Pts',(200.258465056036,10.2183587950959,31.0396526191242));
#80574=CARTESIAN_POINT('Ctrl Pts',(200.337116954771,9.28424615241247,29.6941182368515));
#80575=CARTESIAN_POINT('Ctrl Pts',(200.415768853505,9.89413090757163,28.1738979263852));
#80576=CARTESIAN_POINT('Ctrl Pts',(200.494420752239,11.4991811460846,27.8470295399369));
#80577=CARTESIAN_POINT('Ctrl Pts',(200.573072650973,12.6550210305185,29.0076601310952));
#80578=CARTESIAN_POINT('Ctrl Pts',(200.651724549707,12.3215166406444,30.6113446481208));
#80579=CARTESIAN_POINT('Ctrl Pts',(200.730376448442,10.7987867324307,31.2149362609849));
#80580=CARTESIAN_POINT('Ctrl Pts',(200.809028347176,9.45712753126317,30.2752662145761));
#80581=CARTESIAN_POINT('Ctrl Pts',(200.88768024591,9.50389073404023,28.6379383881611));
#80582=CARTESIAN_POINT('Ctrl Pts',(200.966332144644,10.8969943931969,27.7763750398514));
#80583=CARTESIAN_POINT('Ctrl Pts',(201.044984043378,12.3827922283826,28.4658922631549));
#80584=CARTESIAN_POINT('Ctrl Pts',(201.123635942113,12.6242229827909,30.0859973212029));
#80585=CARTESIAN_POINT('Ctrl Pts',(201.202287840846,11.4040244554083,31.1787666299141));
#80586=CARTESIAN_POINT('Ctrl Pts',(201.280939739581,9.82024655447976,30.7608231303653));
#80587=CARTESIAN_POINT('Ctrl Pts',(201.359591638315,9.29812225624811,29.2082718669661));
#80588=CARTESIAN_POINT('Ctrl Pts',(201.438243537049,10.3075083298367,27.9182451375021));
#80589=CARTESIAN_POINT('Ctrl Pts',(201.516895435783,11.9400638285778,28.0516308631841));
#80590=CARTESIAN_POINT('Ctrl Pts',(201.595547334518,12.7266610856501,29.4883959669684));
#80591=CARTESIAN_POINT('Ctrl Pts',(201.674199233252,11.9594455785568,30.9356034759184));
#80592=CARTESIAN_POINT('Ctrl Pts',(201.752851131986,10.3288303001514,31.0909193544258));
#80593=CARTESIAN_POINT('Ctrl Pts',(201.83150303072,9.30219692370285,29.8145757021723));
#80594=CARTESIAN_POINT('Ctrl Pts',(201.910154929454,9.80340714836079,28.2551471148416));
#80595=CARTESIAN_POINT('Ctrl Pts',(201.988806828188,11.3814246641764,27.8159547559999));
#80596=CARTESIAN_POINT('Ctrl Pts',(202.067458726923,12.6162002336191,28.8922254010485));
#80597=CARTESIAN_POINT('Ctrl Pts',(202.146110625657,12.3965661488944,30.5154290472719));
#80598=CARTESIAN_POINT('Ctrl Pts',(202.224762524391,10.9201699084762,31.2248537082224));
#80599=CARTESIAN_POINT('Ctrl Pts',(202.303414423125,9.51561232603495,30.3820920539613));
#80600=CARTESIAN_POINT('Ctrl Pts',(202.382066321859,9.4468470041279,28.7455406374798));
#80601=CARTESIAN_POINT('Ctrl Pts',(202.460718220593,10.7757554757318,27.7879230298789));
#80602=CARTESIAN_POINT('Ctrl Pts',(202.539370119328,12.3064603548631,28.3709940215176));
#80603=CARTESIAN_POINT('Ctrl Pts',(202.618022018062,12.6614887841502,29.9700512508477));
#80604=CARTESIAN_POINT('Ctrl Pts',(202.696673916796,11.5213526430484,31.1461119584899));
#80605=CARTESIAN_POINT('Ctrl Pts',(202.77532581553,9.91205414106004,30.8408456161187));
#80606=CARTESIAN_POINT('Ctrl Pts',(202.853977714264,9.28179210220836,29.3289597174551));
#80607=CARTESIAN_POINT('Ctrl Pts',(202.932629612999,10.1977358505203,27.9709920232824));
#80608=CARTESIAN_POINT('Ctrl Pts',(203.011281511733,11.8356326711549,27.9889701535476));
#80609=CARTESIAN_POINT('Ctrl Pts',(203.089933410467,12.7215482713383,29.36671568772));
#80610=CARTESIAN_POINT('Ctrl Pts',(203.168585309201,12.0582521005643,30.8644030382864));
#80611=CARTESIAN_POINT('Ctrl Pts',(203.247237207935,10.4426407158838,31.1342716370908));
#80612=CARTESIAN_POINT('Ctrl Pts',(203.32588910667,9.3285938687821,29.9334682287171));
#80613=CARTESIAN_POINT('Ctrl Pts',(203.404541005403,9.71863615894957,28.342589151653));
#80614=CARTESIAN_POINT('Ctrl Pts',(203.483192904138,11.2617706826824,27.7932577107749));
#80615=CARTESIAN_POINT('Ctrl Pts',(203.561844802872,12.5693392211027,28.7798141920086));
#80616=CARTESIAN_POINT('Ctrl Pts',(203.640496701606,12.4646680616967,30.4144619565041));
#80617=CARTESIAN_POINT('Ctrl Pts',(203.71914860034,11.041950231981,31.2261903450361));
#80618=CARTESIAN_POINT('Ctrl Pts',(203.797800499075,9.5814815785967,30.4845298298707));
#80619=CARTESIAN_POINT('Ctrl Pts',(203.876452397809,9.39752989638986,28.8568958589839));
#80620=CARTESIAN_POINT('Ctrl Pts',(203.955104296543,10.65563202014,27.8079887971982));
#80621=CARTESIAN_POINT('Ctrl Pts',(204.033756195277,12.2236293586242,28.2817110867069));
#80622=CARTESIAN_POINT('Ctrl Pts',(204.112408094011,12.6904886275653,29.8517693451864));
#80623=CARTESIAN_POINT('Ctrl Pts',(204.191059992745,11.6360881356371,31.10526295475));
#80624=CARTESIAN_POINT('Ctrl Pts',(204.26971189148,10.0092721109943,30.9142087249912));
#80625=CARTESIAN_POINT('Ctrl Pts',(204.348363790214,9.27401355747157,29.4504755991501));
#80626=CARTESIAN_POINT('Ctrl Pts',(204.427015688948,10.0919463015996,28.0313927786227));
#80627=CARTESIAN_POINT('Ctrl Pts',(204.505667587682,11.7270613398761,27.9337281077398));
#80628=CARTESIAN_POINT('Ctrl Pts',(204.584319486416,12.7078361411144,29.2459025633933));
#80629=CARTESIAN_POINT('Ctrl Pts',(204.662971385151,12.1518672632886,30.7859920400904));
#80630=CARTESIAN_POINT('Ctrl Pts',(204.741623283884,10.5590803622657,31.1703805458846));
#80631=CARTESIAN_POINT('Ctrl Pts',(204.820275182619,9.36368173991768,30.048410370431));
#80632=CARTESIAN_POINT('Ctrl Pts',(204.872709781775,9.54849896857087,28.9770389950952));
#80633=CARTESIAN_POINT('Ctrl Pts',(204.898927081353,9.8460438482599,28.5968608675124));
#80634=CARTESIAN_POINT('Ctrl Pts',(198.741050723552,11.5930751352726,30.7338820776337));
#80635=CARTESIAN_POINT('Ctrl Pts',(198.76726802313,11.1865649076305,30.9292744191052));
#80636=CARTESIAN_POINT('Ctrl Pts',(198.819702622287,10.1718862740663,30.8833891474997));
#80637=CARTESIAN_POINT('Ctrl Pts',(198.898354521021,9.38741769388793,29.5678689755753));
#80638=CARTESIAN_POINT('Ctrl Pts',(198.977006419755,10.0571378434374,28.1913591329231));
#80639=CARTESIAN_POINT('Ctrl Pts',(199.055658318489,11.5738625074928,27.9924127421684));
#80640=CARTESIAN_POINT('Ctrl Pts',(199.134310217223,12.5748778548401,29.1501677721583));
#80641=CARTESIAN_POINT('Ctrl Pts',(199.212962115957,12.1583287110005,30.6227192148848));
#80642=CARTESIAN_POINT('Ctrl Pts',(199.291614014691,10.6995701363518,31.0849493741634));
#80643=CARTESIAN_POINT('Ctrl Pts',(199.370265913426,9.5110875978464,30.1208887232174));
#80644=CARTESIAN_POINT('Ctrl Pts',(199.44891781216,9.66250724428823,28.5980954936162));
#80645=CARTESIAN_POINT('Ctrl Pts',(199.527569710894,11.0175108386447,27.8869202988471));
#80646=CARTESIAN_POINT('Ctrl Pts',(199.606221609628,12.3567653896749,28.6273470150609));
#80647=CARTESIAN_POINT('Ctrl Pts',(199.684873508362,12.4750699956528,30.1530691314153));
#80648=CARTESIAN_POINT('Ctrl Pts',(199.763525407097,11.2659693277849,31.0910980417724));
#80649=CARTESIAN_POINT('Ctrl Pts',(199.842177305831,9.81752333966091,30.5973065760587));
#80650=CARTESIAN_POINT('Ctrl Pts',(199.920829204565,9.43318203872702,29.1160550115813));
#80651=CARTESIAN_POINT('Ctrl Pts',(199.999481103299,10.4588113274449,27.9803134087427));
#80652=CARTESIAN_POINT('Ctrl Pts',(200.078133002033,11.9714534215208,28.2121293720419));
#80653=CARTESIAN_POINT('Ctrl Pts',(200.156784900767,12.6098898991963,29.6028929902686));
#80654=CARTESIAN_POINT('Ctrl Pts',(200.235436799502,11.7995953835968,30.9010637766396));
#80655=CARTESIAN_POINT('Ctrl Pts',(200.314088698236,10.2697493908549,30.9384250164052));
#80656=CARTESIAN_POINT('Ctrl Pts',(200.39274059697,9.39705188968703,29.6813555373201));
#80657=CARTESIAN_POINT('Ctrl Pts',(200.471392495704,9.96683852730155,28.2610852127933));
#80658=CARTESIAN_POINT('Ctrl Pts',(200.550044394438,11.4663614631815,27.9557074553049));
#80659=CARTESIAN_POINT('Ctrl Pts',(200.628696293173,12.5462082962121,29.0400300202722));
#80660=CARTESIAN_POINT('Ctrl Pts',(200.707348191907,12.2346308328824,30.5382770268103));
#80661=CARTESIAN_POINT('Ctrl Pts',(200.786000090641,10.8120159092322,31.1021842776096));
#80662=CARTESIAN_POINT('Ctrl Pts',(200.864651989375,9.55856682956415,30.2242947555627));
#80663=CARTESIAN_POINT('Ctrl Pts',(200.943303888109,9.60225549016605,28.6946163876517));
#80664=CARTESIAN_POINT('Ctrl Pts',(201.021955786844,10.9037667069733,27.8896982794803));
#80665=CARTESIAN_POINT('Ctrl Pts',(201.100607685578,12.2918777320872,28.533881786151));
#80666=CARTESIAN_POINT('Ctrl Pts',(201.179259584312,12.5174351289682,30.04746973174));
#80667=CARTESIAN_POINT('Ctrl Pts',(201.257911483046,11.377461043277,31.0683926927285));
#80668=CARTESIAN_POINT('Ctrl Pts',(201.33656338178,9.89781185174615,30.6779277412664));
#80669=CARTESIAN_POINT('Ctrl Pts',(201.415215280514,9.4100156807653,29.2274521282705));
#80670=CARTESIAN_POINT('Ctrl Pts',(201.493867179248,10.3530376075469,28.0222408381107));
#80671=CARTESIAN_POINT('Ctrl Pts',(201.572519077983,11.8782574142038,28.1468568471176));
#80672=CARTESIAN_POINT('Ctrl Pts',(201.651170976717,12.6131382297557,29.4891588977951));
#80673=CARTESIAN_POINT('Ctrl Pts',(201.729822875451,11.8963648714868,30.8412167964057));
#80674=CARTESIAN_POINT('Ctrl Pts',(201.808474774185,10.3729577214212,30.9863211155975));
#80675=CARTESIAN_POINT('Ctrl Pts',(201.887126672919,9.41382245089489,29.7938932808203));
#80676=CARTESIAN_POINT('Ctrl Pts',(201.965778571654,9.88207958673907,28.3369925075861));
#80677=CARTESIAN_POINT('Ctrl Pts',(202.044430470388,11.3563471214289,27.9266757464382));
#80678=CARTESIAN_POINT('Ctrl Pts',(202.123082369122,12.5099398518091,28.9321847820681));
#80679=CARTESIAN_POINT('Ctrl Pts',(202.201734267856,12.3047460580928,30.448667592831));
#80680=CARTESIAN_POINT('Ctrl Pts',(202.28038616659,10.9254185007166,31.1114496820445));
#80681=CARTESIAN_POINT('Ctrl Pts',(202.359038065324,9.61320642218011,30.3240971121862));
#80682=CARTESIAN_POINT('Ctrl Pts',(202.437689964059,9.54896221666022,28.7951441075536));
#80683=CARTESIAN_POINT('Ctrl Pts',(202.516341862793,10.7904988894945,27.9004870233427));
#80684=CARTESIAN_POINT('Ctrl Pts',(202.594993761527,12.2205644533283,28.4452228230262));
#80685=CARTESIAN_POINT('Ctrl Pts',(202.673645660261,12.5522508141855,29.9391467723392));
#80686=CARTESIAN_POINT('Ctrl Pts',(202.752297558995,11.487075249842,31.0378849693009));
#80687=CARTESIAN_POINT('Ctrl Pts',(202.83094945773,9.98358336123639,30.7526889854281));
#80688=CARTESIAN_POINT('Ctrl Pts',(202.909601356464,9.39475918602047,29.3402051097958));
#80689=CARTESIAN_POINT('Ctrl Pts',(202.988253255198,10.2504823438464,28.0715197722685));
#80690=CARTESIAN_POINT('Ctrl Pts',(203.066905153932,11.7806922962912,28.0883158936796));
#80691=CARTESIAN_POINT('Ctrl Pts',(203.145557052666,12.6083615678522,29.375478736764));
#80692=CARTESIAN_POINT('Ctrl Pts',(203.224208951401,11.988675157115,30.7746975768125));
#80693=CARTESIAN_POINT('Ctrl Pts',(203.302860850135,10.4792854391697,31.0268231139892));
#80694=CARTESIAN_POINT('Ctrl Pts',(203.381512748869,9.43848387496357,29.904968975637));
#80695=CARTESIAN_POINT('Ctrl Pts',(203.460164647603,9.80288203898061,28.4186854892838));
#80696=CARTESIAN_POINT('Ctrl Pts',(203.538816546337,11.2445600350721,27.905470964759));
#80697=CARTESIAN_POINT('Ctrl Pts',(203.617468445071,12.4661598121687,28.8271642773134));
#80698=CARTESIAN_POINT('Ctrl Pts',(203.696120343806,12.368370471693,30.3543387894437));
#80699=CARTESIAN_POINT('Ctrl Pts',(203.77477224254,11.0391921283905,31.1126984389437));
#80700=CARTESIAN_POINT('Ctrl Pts',(203.853424141274,9.67474496634252,30.41979990752));
#80701=CARTESIAN_POINT('Ctrl Pts',(203.932076040008,9.5028875627896,28.8991780528276));
#80702=CARTESIAN_POINT('Ctrl Pts',(204.010727938742,10.6782731955722,27.9192335258504));
#80703=CARTESIAN_POINT('Ctrl Pts',(204.089379837476,12.1431793499329,28.361809976924));
#80704=CARTESIAN_POINT('Ctrl Pts',(204.16803173621,12.5793440037285,29.8286415518901));
#80705=CARTESIAN_POINT('Ctrl Pts',(204.246683634945,11.5942672233815,30.999721666654));
#80706=CARTESIAN_POINT('Ctrl Pts',(204.325335533679,10.0744095373885,30.8212286870288));
#80707=CARTESIAN_POINT('Ctrl Pts',(204.403987432413,9.38749205757757,29.4537316819261));
#80708=CARTESIAN_POINT('Ctrl Pts',(204.482639331147,10.1516481446564,28.1279493567164));
#80709=CARTESIAN_POINT('Ctrl Pts',(204.561291229882,11.6792592086998,28.0367058488809));
#80710=CARTESIAN_POINT('Ctrl Pts',(204.639943128615,12.595550969606,29.262608717785));
#80711=CARTESIAN_POINT('Ctrl Pts',(204.71859502735,12.0761353999678,30.7014418696708));
#80712=CARTESIAN_POINT('Ctrl Pts',(204.797246926084,10.5880695234343,31.0605579689034));
#80713=CARTESIAN_POINT('Ctrl Pts',(204.875898824818,9.47126482242333,30.0123540117334));
#80714=CARTESIAN_POINT('Ctrl Pts',(204.928333423974,9.64393086530558,29.0114221333333));
#80715=CARTESIAN_POINT('Ctrl Pts',(204.954550723552,9.92191304981385,28.6562395924064));
#80716=CARTESIAN_POINT('Ctrl Pts',(198.796674365751,11.5513381149266,30.6470489627113));
#80717=CARTESIAN_POINT('Ctrl Pts',(198.82289166533,11.1734356043053,30.8286907797611));
#80718=CARTESIAN_POINT('Ctrl Pts',(198.875326264485,10.2301638806838,30.7860346344513));
#80719=CARTESIAN_POINT('Ctrl Pts',(198.953978163219,9.50090142725805,29.5630927699211));
#80720=CARTESIAN_POINT('Ctrl Pts',(199.032630061953,10.1234907465883,28.2834533166888));
#80721=CARTESIAN_POINT('Ctrl Pts',(199.111281960687,11.5334775550196,28.0985075627251));
#80722=CARTESIAN_POINT('Ctrl Pts',(199.189933859421,12.4640475313945,29.1747868363253));
#80723=CARTESIAN_POINT('Ctrl Pts',(199.268585758156,12.0768125824308,30.5437090660394));
#80724=CARTESIAN_POINT('Ctrl Pts',(199.34723765689,10.7207125626412,30.9734102784528));
#80725=CARTESIAN_POINT('Ctrl Pts',(199.425889555624,9.61586819565963,30.0771943517418));
#80726=CARTESIAN_POINT('Ctrl Pts',(199.504541454358,9.7566318484702,28.6615660464927));
#80727=CARTESIAN_POINT('Ctrl Pts',(199.583193353092,11.0162785323393,28.0004390358545));
#80728=CARTESIAN_POINT('Ctrl Pts',(199.661845251827,12.26128449475,28.688759023795));
#80729=CARTESIAN_POINT('Ctrl Pts',(199.740497150561,12.3712635422058,30.1071100985642));
#80730=CARTESIAN_POINT('Ctrl Pts',(199.819149049295,11.2472520243861,30.9791262402378));
#80731=CARTESIAN_POINT('Ctrl Pts',(199.897800948029,9.90073885401307,30.5200848141488));
#80732=CARTESIAN_POINT('Ctrl Pts',(199.976452846763,9.54344515589176,29.1430747243298));
#80733=CARTESIAN_POINT('Ctrl Pts',(200.055104745497,10.4968968941699,28.0872597067857));
#80734=CARTESIAN_POINT('Ctrl Pts',(200.133756644232,11.903088439063,28.3027618727239));
#80735=CARTESIAN_POINT('Ctrl Pts',(200.212408542966,12.4965956410471,29.5956520075113));
#80736=CARTESIAN_POINT('Ctrl Pts',(200.2910604417,11.7433247244359,30.8024654307069));
#80737=CARTESIAN_POINT('Ctrl Pts',(200.369712340434,10.3211399866139,30.8371974136864));
#80738=CARTESIAN_POINT('Ctrl Pts',(200.448364239168,9.50985762696159,29.6685928377888));
#80739=CARTESIAN_POINT('Ctrl Pts',(200.527016137902,10.0395461470315,28.3482724992014));
#80740=CARTESIAN_POINT('Ctrl Pts',(200.605668036637,11.4335417802784,28.0643853706729));
#80741=CARTESIAN_POINT('Ctrl Pts',(200.684319935371,12.4373955619059,29.0723999094493));
#80742=CARTESIAN_POINT('Ctrl Pts',(200.762971834105,12.1477450251203,30.4652094055));
#80743=CARTESIAN_POINT('Ctrl Pts',(200.841623732839,10.8252450860336,30.9894322942343));
#80744=CARTESIAN_POINT('Ctrl Pts',(200.920275631573,9.66000612786511,30.1733232965494));
#80745=CARTESIAN_POINT('Ctrl Pts',(200.998927530308,9.7006202462919,28.7512943871423));
#80746=CARTESIAN_POINT('Ctrl Pts',(201.077579429042,10.9105390207496,28.0030215191092));
#80747=CARTESIAN_POINT('Ctrl Pts',(201.156231327776,12.2009632357919,28.601871309147));
#80748=CARTESIAN_POINT('Ctrl Pts',(201.23488322651,12.4106472751453,30.0089421422772));
#80749=CARTESIAN_POINT('Ctrl Pts',(201.313535125244,11.3508976311457,30.958018755543));
#80750=CARTESIAN_POINT('Ctrl Pts',(201.392187023979,9.97537714901258,30.5950323521675));
#80751=CARTESIAN_POINT('Ctrl Pts',(201.470838922713,9.52190910528247,29.2466323895747));
#80752=CARTESIAN_POINT('Ctrl Pts',(201.549490821447,10.3985668852571,28.1262365387192));
#80753=CARTESIAN_POINT('Ctrl Pts',(201.628142720181,11.8164509998297,28.2420828310512));
#80754=CARTESIAN_POINT('Ctrl Pts',(201.706794618915,12.4996153738612,29.4899218286219));
#80755=CARTESIAN_POINT('Ctrl Pts',(201.785446517649,11.8332841644169,30.746830116893));
#80756=CARTESIAN_POINT('Ctrl Pts',(201.864098416384,10.417085142691,30.8817228767694));
#80757=CARTESIAN_POINT('Ctrl Pts',(201.942750315118,9.52544797808693,29.7732108594681));
#80758=CARTESIAN_POINT('Ctrl Pts',(202.021402213852,9.96075202511736,28.4188379003305));
#80759=CARTESIAN_POINT('Ctrl Pts',(202.100054112586,11.3312695786813,28.0373967368765));
#80760=CARTESIAN_POINT('Ctrl Pts',(202.17870601132,12.4036794699991,28.9721441630876));
#80761=CARTESIAN_POINT('Ctrl Pts',(202.257357910054,12.2129259672911,30.3819061383901));
#80762=CARTESIAN_POINT('Ctrl Pts',(202.336009808789,10.9306670929571,30.9980456558665));
#80763=CARTESIAN_POINT('Ctrl Pts',(202.414661707523,9.71080051832528,30.2661021704112));
#80764=CARTESIAN_POINT('Ctrl Pts',(202.493313606257,9.65107742919254,28.8447475776273));
#80765=CARTESIAN_POINT('Ctrl Pts',(202.571965504991,10.8052423032571,28.0130510168065));
#80766=CARTESIAN_POINT('Ctrl Pts',(202.650617403725,12.1346685517936,28.5194516245347));
#80767=CARTESIAN_POINT('Ctrl Pts',(202.729269302459,12.4430128442209,29.9082422938307));
#80768=CARTESIAN_POINT('Ctrl Pts',(202.807921201195,11.4527978566356,30.9296579801117));
#80769=CARTESIAN_POINT('Ctrl Pts',(202.886573099928,10.0551125814128,30.6645323547376));
#80770=CARTESIAN_POINT('Ctrl Pts',(202.965224998662,9.50772626983257,29.3514505021364));
#80771=CARTESIAN_POINT('Ctrl Pts',(203.043876897396,10.3032288371725,28.1720475212547));
#80772=CARTESIAN_POINT('Ctrl Pts',(203.12252879613,11.7257519214275,28.1876616338116));
#80773=CARTESIAN_POINT('Ctrl Pts',(203.201180694865,12.495174864366,29.384241785808));
#80774=CARTESIAN_POINT('Ctrl Pts',(203.279832593599,11.9190982136657,30.6849921153385));
#80775=CARTESIAN_POINT('Ctrl Pts',(203.358484492333,10.5159301624556,30.9193745908879));
#80776=CARTESIAN_POINT('Ctrl Pts',(203.437136391067,9.54837388114503,29.876469722557));
#80777=CARTESIAN_POINT('Ctrl Pts',(203.515788289801,9.88712791901166,28.4947818269146));
#80778=CARTESIAN_POINT('Ctrl Pts',(203.594440188536,11.2273493874618,28.0176842187432));
#80779=CARTESIAN_POINT('Ctrl Pts',(203.67309208727,12.3629804032347,28.8745143626181));
#80780=CARTESIAN_POINT('Ctrl Pts',(203.751743986004,12.2720728816894,30.2942156223834));
#80781=CARTESIAN_POINT('Ctrl Pts',(203.830395884738,11.0364340248,30.9992065328513));
#80782=CARTESIAN_POINT('Ctrl Pts',(203.909047783472,9.76800835408834,30.3550699851692));
#80783=CARTESIAN_POINT('Ctrl Pts',(203.987699682206,9.60824522918933,28.9414602466712));
#80784=CARTESIAN_POINT('Ctrl Pts',(204.06635158094,10.7009143710046,28.0304782545025));
#80785=CARTESIAN_POINT('Ctrl Pts',(204.145003479675,12.0627293412418,28.4419088671411));
#80786=CARTESIAN_POINT('Ctrl Pts',(204.223655378409,12.4681993798916,29.8055137585938));
#80787=CARTESIAN_POINT('Ctrl Pts',(204.302307277143,11.5524463111259,30.894180378558));
#80788=CARTESIAN_POINT('Ctrl Pts',(204.380959175877,10.1395469637827,30.7282486490664));
#80789=CARTESIAN_POINT('Ctrl Pts',(204.459611074611,9.50097055768355,29.456987764702));
#80790=CARTESIAN_POINT('Ctrl Pts',(204.538262973346,10.2113499877134,28.2245059348102));
#80791=CARTESIAN_POINT('Ctrl Pts',(204.61691487208,11.6314570775236,28.1396835900221));
#80792=CARTESIAN_POINT('Ctrl Pts',(204.695566770814,12.4832657980976,29.2793148721768));
#80793=CARTESIAN_POINT('Ctrl Pts',(204.774218669548,12.0004035366468,30.6168916992512));
#80794=CARTESIAN_POINT('Ctrl Pts',(204.852870568282,10.6170586846029,30.950735391922));
#80795=CARTESIAN_POINT('Ctrl Pts',(204.931522467016,9.57884790492899,29.9762976530357));
#80796=CARTESIAN_POINT('Ctrl Pts',(204.983957066173,9.73936276204029,29.0458052715714));
#80797=CARTESIAN_POINT('Ctrl Pts',(205.010174365751,9.99778225136778,28.7156183173004));
#80798=CARTESIAN_POINT('Ctrl Pts',(198.85229800795,11.5096010945807,30.5602158477891));
#80799=CARTESIAN_POINT('Ctrl Pts',(198.878515307528,11.1603063009802,30.7281071404171));
#80800=CARTESIAN_POINT('Ctrl Pts',(198.930949906684,10.2884414873013,30.6886801214029));
#80801=CARTESIAN_POINT('Ctrl Pts',(199.009601805418,9.61438516062817,29.5583165642669));
#80802=CARTESIAN_POINT('Ctrl Pts',(199.088253704153,10.189843649739,28.3755475004547));
#80803=CARTESIAN_POINT('Ctrl Pts',(199.166905602887,11.4930926025464,28.2046023832819));
#80804=CARTESIAN_POINT('Ctrl Pts',(199.245557501621,12.3532172079488,29.1994059004922));
#80805=CARTESIAN_POINT('Ctrl Pts',(199.324209400355,11.9952964538612,30.4646989171939));
#80806=CARTESIAN_POINT('Ctrl Pts',(199.402861299089,10.7418549889306,30.8618711827422));
#80807=CARTESIAN_POINT('Ctrl Pts',(199.481513197823,9.72064879347285,30.0334999802663));
#80808=CARTESIAN_POINT('Ctrl Pts',(199.560165096557,9.85075645265219,28.7250365993692));
#80809=CARTESIAN_POINT('Ctrl Pts',(199.638816995292,11.0150462260339,28.113957772862));
#80810=CARTESIAN_POINT('Ctrl Pts',(199.717468894026,12.165803599825,28.7501710325291));
#80811=CARTESIAN_POINT('Ctrl Pts',(199.79612079276,12.2674570887587,30.061151065713));
#80812=CARTESIAN_POINT('Ctrl Pts',(199.874772691494,11.2285347209873,30.8671544387032));
#80813=CARTESIAN_POINT('Ctrl Pts',(199.953424590228,9.98395436836523,30.4428630522389));
#80814=CARTESIAN_POINT('Ctrl Pts',(200.032076488963,9.65370827305649,29.1700944370783));
#80815=CARTESIAN_POINT('Ctrl Pts',(200.110728387697,10.5349824608951,28.1942060048287));
#80816=CARTESIAN_POINT('Ctrl Pts',(200.189380286431,11.834723456605,28.3933943734058));
#80817=CARTESIAN_POINT('Ctrl Pts',(200.268032185165,12.3833013828978,29.588411024754));
#80818=CARTESIAN_POINT('Ctrl Pts',(200.346684083899,11.687054065275,30.7038670847745));
#80819=CARTESIAN_POINT('Ctrl Pts',(200.425335982633,10.3725305823729,30.7359698109675));
#80820=CARTESIAN_POINT('Ctrl Pts',(200.503987881368,9.62266336423614,29.6558301382575));
#80821=CARTESIAN_POINT('Ctrl Pts',(200.582639780102,10.1122537667614,28.4354597856095));
#80822=CARTESIAN_POINT('Ctrl Pts',(200.661291678836,11.4007220973753,28.173063286041));
#80823=CARTESIAN_POINT('Ctrl Pts',(200.73994357757,12.3285828275996,29.1047697986263));
#80824=CARTESIAN_POINT('Ctrl Pts',(200.818595476304,12.0608592173582,30.3921417841895));
#80825=CARTESIAN_POINT('Ctrl Pts',(200.897247375038,10.8384742628351,30.8766803108589));
#80826=CARTESIAN_POINT('Ctrl Pts',(200.975899273773,9.7614454261661,30.122351837536));
#80827=CARTESIAN_POINT('Ctrl Pts',(201.054551172507,9.79898500241771,28.8079723866329));
#80828=CARTESIAN_POINT('Ctrl Pts',(201.133203071241,10.9173113345259,28.1163447587381));
#80829=CARTESIAN_POINT('Ctrl Pts',(201.211854969975,12.1100487394965,28.6698608321431));
#80830=CARTESIAN_POINT('Ctrl Pts',(201.290506868709,12.3038594213226,29.9704145528143));
#80831=CARTESIAN_POINT('Ctrl Pts',(201.369158767444,11.3243342190144,30.8476448183576));
#80832=CARTESIAN_POINT('Ctrl Pts',(201.447810666178,10.052942446279,30.5121369630686));
#80833=CARTESIAN_POINT('Ctrl Pts',(201.526462564912,9.63380252979966,29.2658126508791));
#80834=CARTESIAN_POINT('Ctrl Pts',(201.605114463646,10.4440961629675,28.2302322393278));
#80835=CARTESIAN_POINT('Ctrl Pts',(201.68376636238,11.7546445854556,28.3373088149847));
#80836=CARTESIAN_POINT('Ctrl Pts',(201.762418261114,12.3860925179668,29.4906847594487));
#80837=CARTESIAN_POINT('Ctrl Pts',(201.841070159849,11.7702034573468,30.6524434373803));
#80838=CARTESIAN_POINT('Ctrl Pts',(201.919722058583,10.4612125639608,30.7771246379412));
#80839=CARTESIAN_POINT('Ctrl Pts',(201.998373957317,9.63707350527895,29.7525284381161));
#80840=CARTESIAN_POINT('Ctrl Pts',(202.077025856051,10.0394244634956,28.5006832930751));
#80841=CARTESIAN_POINT('Ctrl Pts',(202.155677754785,11.3061920359338,28.1481177273148));
#80842=CARTESIAN_POINT('Ctrl Pts',(202.23432965352,12.2974190881889,29.0121035441072));
#80843=CARTESIAN_POINT('Ctrl Pts',(202.312981552254,12.1211058764895,30.3151446839492));
#80844=CARTESIAN_POINT('Ctrl Pts',(202.391633450988,10.9359156851976,30.8846416296885));
#80845=CARTESIAN_POINT('Ctrl Pts',(202.470285349722,9.80839461447045,30.2081072286361));
#80846=CARTESIAN_POINT('Ctrl Pts',(202.548937248456,9.75319264172485,28.8943510477011));
#80847=CARTESIAN_POINT('Ctrl Pts',(202.62758914719,10.8199857170198,28.1256150102703));
#80848=CARTESIAN_POINT('Ctrl Pts',(202.706241045925,12.0487726502588,28.5936804260432));
#80849=CARTESIAN_POINT('Ctrl Pts',(202.784892944659,12.3337748742563,29.8773378153221));
#80850=CARTESIAN_POINT('Ctrl Pts',(202.863544843393,11.4185204634293,30.8214309909227));
#80851=CARTESIAN_POINT('Ctrl Pts',(202.942196742127,10.1266418015891,30.576375724047));
#80852=CARTESIAN_POINT('Ctrl Pts',(203.020848640861,9.62069335364468,29.362695894477));
#80853=CARTESIAN_POINT('Ctrl Pts',(203.099500539595,10.3559753304986,28.2725752702408));
#80854=CARTESIAN_POINT('Ctrl Pts',(203.17815243833,11.6708115465637,28.2870073739437));
#80855=CARTESIAN_POINT('Ctrl Pts',(203.256804337064,12.3819881608799,29.393004834852));
#80856=CARTESIAN_POINT('Ctrl Pts',(203.335456235798,11.8495212702164,30.5952866538646));
#80857=CARTESIAN_POINT('Ctrl Pts',(203.414108134532,10.5525748857415,30.8119260677863));
#80858=CARTESIAN_POINT('Ctrl Pts',(203.492760033266,9.65826388732648,29.8479704694768));
#80859=CARTESIAN_POINT('Ctrl Pts',(203.571411932001,9.97137379904272,28.5708781645454));
#80860=CARTESIAN_POINT('Ctrl Pts',(203.650063830735,11.2101387398515,28.1298974727275));
#80861=CARTESIAN_POINT('Ctrl Pts',(203.728715729469,12.2598009943006,28.9218644479227));
#80862=CARTESIAN_POINT('Ctrl Pts',(203.807367628203,12.1757752916857,30.234092455323));
#80863=CARTESIAN_POINT('Ctrl Pts',(203.886019526937,11.0336759212094,30.885714626759));
#80864=CARTESIAN_POINT('Ctrl Pts',(203.964671425671,9.86127174183416,30.2903400628184));
#80865=CARTESIAN_POINT('Ctrl Pts',(204.043323324406,9.71360289558907,28.9837424405148));
#80866=CARTESIAN_POINT('Ctrl Pts',(204.12197522314,10.7235555464368,28.1417229831548));
#80867=CARTESIAN_POINT('Ctrl Pts',(204.200627121874,11.9822793325505,28.5220077573582));
#80868=CARTESIAN_POINT('Ctrl Pts',(204.279279020608,12.3570547560548,29.7823859652975));
#80869=CARTESIAN_POINT('Ctrl Pts',(204.357930919342,11.5106253988703,30.7886390904618));
#80870=CARTESIAN_POINT('Ctrl Pts',(204.436582818076,10.2046843901768,30.635268611104));
#80871=CARTESIAN_POINT('Ctrl Pts',(204.515234716811,9.61444905778955,29.4602438474781));
#80872=CARTESIAN_POINT('Ctrl Pts',(204.593886615545,10.2710518307703,28.321062512904));
#80873=CARTESIAN_POINT('Ctrl Pts',(204.672538514279,11.5836549463473,28.2426613311632));
#80874=CARTESIAN_POINT('Ctrl Pts',(204.751190413013,12.3709806265892,29.2960210265685));
#80875=CARTESIAN_POINT('Ctrl Pts',(204.829842311747,11.924671673326,30.5323415288316));
#80876=CARTESIAN_POINT('Ctrl Pts',(204.908494210482,10.6460478457716,30.8409128149407));
#80877=CARTESIAN_POINT('Ctrl Pts',(204.987146109216,9.68643098743465,29.9402412943381));
#80878=CARTESIAN_POINT('Ctrl Pts',(205.039580708372,9.834794658775,29.0801884098095));
#80879=CARTESIAN_POINT('Ctrl Pts',(205.06579800795,10.0736514529217,28.7749970421944));
#80880=CARTESIAN_POINT('Ctrl Pts',(198.6865,11.6340070945751,30.8190402776367));
#80881=CARTESIAN_POINT('Ctrl Pts',(198.710737126766,11.4537103993182,30.8788097556703));
#80882=CARTESIAN_POINT('Ctrl Pts',(198.731653684349,11.2655768472979,30.9058979865679));
#80883=CARTESIAN_POINT('Ctrl Pts',(198.776140325335,10.9248764665845,30.8800560222072));
#80884=CARTESIAN_POINT('Ctrl Pts',(198.797718346184,10.7784026223058,30.8423706540008));
#80885=CARTESIAN_POINT('Ctrl Pts',(198.832593474394,10.5724822918099,30.7483060524685));
#80886=CARTESIAN_POINT('Ctrl Pts',(198.844351974729,10.5073488774618,30.71140036245));
#80887=CARTESIAN_POINT('Ctrl Pts',(198.865327041601,10.3947405990162,30.6347745027527));
#80888=CARTESIAN_POINT('Ctrl Pts',(198.874645877699,10.3456915364658,30.5963661489365));
#80889=CARTESIAN_POINT('Ctrl Pts',(198.898468331836,10.220730616038,30.4849982515005));
#80890=CARTESIAN_POINT('Ctrl Pts',(198.912523247939,10.1497701747385,30.405322048357));
#80891=CARTESIAN_POINT('Ctrl Pts',(198.940905585237,10.0375577642678,30.2378655455178));
#80892=CARTESIAN_POINT('Ctrl Pts',(198.954811357476,9.99489876194716,30.1534283775981));
#80893=CARTESIAN_POINT('Ctrl Pts',(198.970000790184,9.96359235009872,30.0641429946324));
#80894=CARTESIAN_POINT('Origin',(204.9,11.,29.5));
#80895=CARTESIAN_POINT('',(205.,11.,31.0635));
#80896=CARTESIAN_POINT('Origin',(205.,11.,29.5));
#80897=CARTESIAN_POINT('Origin',(204.9,11.,31.0635));
#80898=CARTESIAN_POINT('Origin',(205.,13.75,29.5));
#80899=CARTESIAN_POINT('',(205.,8.25,29.5));
#80900=CARTESIAN_POINT('Origin',(205.,11.,29.5));
#80901=CARTESIAN_POINT('Origin',(206.15,11.,29.5));
#80902=CARTESIAN_POINT('',(206.15,8.27924642791744,29.1));
#80903=CARTESIAN_POINT('',(206.15,8.25,29.5));
#80904=CARTESIAN_POINT('Origin',(206.15,11.,29.5));
#80905=CARTESIAN_POINT('',(206.15,13.7207535720826,29.1));
#80906=CARTESIAN_POINT('',(206.15,7.75,29.1));
#80907=CARTESIAN_POINT('',(206.15,13.7207535720826,29.9));
#80908=CARTESIAN_POINT('Origin',(206.15,11.,29.5));
#80909=CARTESIAN_POINT('',(206.15,8.27924642791744,29.9));
#80910=CARTESIAN_POINT('',(206.15,14.25,29.9));
#80911=CARTESIAN_POINT('Origin',(206.15,11.,29.5));
#80912=CARTESIAN_POINT('Origin',(207.,7.75,29.9));
#80913=CARTESIAN_POINT('',(206.6,8.27924642791744,29.9));
#80914=CARTESIAN_POINT('',(205.8,8.27924642791744,29.9));
#80915=CARTESIAN_POINT('',(206.6,13.7207535720826,29.9));
#80916=CARTESIAN_POINT('',(205.8,13.7207535720826,29.9));
#80917=CARTESIAN_POINT('',(207.,13.3157072353818,29.9));
#80918=CARTESIAN_POINT('Ctrl Pts',(207.,13.3157072353819,29.9));
#80919=CARTESIAN_POINT('Ctrl Pts',(206.816084562245,13.5023462336636,29.9));
#80920=CARTESIAN_POINT('Ctrl Pts',(206.6,13.7207535720826,29.9));
#80921=CARTESIAN_POINT('',(207.,8.68429276461816,29.9));
#80922=CARTESIAN_POINT('',(207.,9.375,29.9));
#80923=CARTESIAN_POINT('Ctrl Pts',(206.6,8.27924642791744,29.9));
#80924=CARTESIAN_POINT('Ctrl Pts',(206.816084562245,8.4976537663367,29.9));
#80925=CARTESIAN_POINT('Ctrl Pts',(207.,8.68429276461812,29.9));
#80926=CARTESIAN_POINT('Origin',(207.,14.25,29.1));
#80927=CARTESIAN_POINT('',(206.6,8.27924642791744,29.1));
#80928=CARTESIAN_POINT('',(205.8,8.27924642791744,29.1));
#80929=CARTESIAN_POINT('',(207.,8.68429276461816,29.1));
#80930=CARTESIAN_POINT('Ctrl Pts',(207.,8.68429276461812,29.1));
#80931=CARTESIAN_POINT('Ctrl Pts',(206.816084562245,8.4976537663364,29.1));
#80932=CARTESIAN_POINT('Ctrl Pts',(206.6,8.27924642791744,29.1));
#80933=CARTESIAN_POINT('',(207.,13.3157072353818,29.1));
#80934=CARTESIAN_POINT('',(207.,12.625,29.1));
#80935=CARTESIAN_POINT('',(206.6,13.7207535720826,29.1));
#80936=CARTESIAN_POINT('Ctrl Pts',(206.6,13.7207535720826,29.1));
#80937=CARTESIAN_POINT('Ctrl Pts',(206.816084562245,13.5023462336636,29.1));
#80938=CARTESIAN_POINT('Ctrl Pts',(207.,13.3157072353819,29.1));
#80939=CARTESIAN_POINT('',(205.8,13.7207535720826,29.1));
#80940=CARTESIAN_POINT('Origin',(205.8,11.,29.5));
#80941=CARTESIAN_POINT('',(205.8,8.25,29.5));
#80942=CARTESIAN_POINT('Origin',(206.6,11.,29.5));
#80943=CARTESIAN_POINT('Origin',(206.6,11.,29.5));
#80944=CARTESIAN_POINT('Origin',(207.,11.,29.5));
#80945=CARTESIAN_POINT('Origin',(207.,11.,29.5));
#80946=CARTESIAN_POINT('Origin',(207.,11.,29.5));
#80947=CARTESIAN_POINT('Origin',(207.,11.,29.5));
#80948=CARTESIAN_POINT('Origin',(206.8,11.,29.5));
#80949=CARTESIAN_POINT('Origin',(199.,12.15,29.5));
#80950=CARTESIAN_POINT('',(199.,9.85,29.5));
#80951=CARTESIAN_POINT('Origin',(199.,11.,29.5));
#80952=CARTESIAN_POINT('Origin',(198.825,11.,29.5));
#80953=CARTESIAN_POINT('',(198.825,9.675,29.5));
#80954=CARTESIAN_POINT('Origin',(206.8,11.,29.5));
#80955=CARTESIAN_POINT('',(0.,0.,0.));
#80956=CARTESIAN_POINT('',(0.,0.,0.));
#80957=CARTESIAN_POINT('',(0.,0.,0.));
#80958=CARTESIAN_POINT('',(0.,0.,0.));
#80959=CARTESIAN_POINT('',(0.,0.,0.));
#80960=CARTESIAN_POINT('',(0.,0.,0.));
#80961=CARTESIAN_POINT('',(0.,0.,0.));
#80962=CARTESIAN_POINT('',(0.,0.,0.));
#80963=CARTESIAN_POINT('',(0.,0.,0.));
#80964=CARTESIAN_POINT('',(0.,28.778174593052,-5.47665940288702));
#80965=CARTESIAN_POINT('',(210.,0.,100.));
#80966=CARTESIAN_POINT('',(210.,0.,100.));
#80967=CARTESIAN_POINT('',(210.,0.,100.));
#80968=CARTESIAN_POINT('',(10.,-16.476659402887,24.221825406948));
#80969=CARTESIAN_POINT('',(20.,28.778174593052,-5.47665940288702));
#80970=CARTESIAN_POINT('',(30.,-16.476659402887,24.221825406948));
#80971=CARTESIAN_POINT('',(40.,28.778174593052,-5.47665940288702));
#80972=CARTESIAN_POINT('',(50.,-16.476659402887,24.221825406948));
#80973=CARTESIAN_POINT('',(60.,28.778174593052,-5.47665940288702));
#80974=CARTESIAN_POINT('',(70.,-16.476659402887,24.221825406948));
#80975=CARTESIAN_POINT('',(80.,28.778174593052,-5.47665940288702));
#80976=CARTESIAN_POINT('',(90.,-16.476659402887,24.221825406948));
#80977=CARTESIAN_POINT('',(100.,28.778174593052,-5.47665940288702));
#80978=CARTESIAN_POINT('',(110.,-16.476659402887,24.221825406948));
#80979=CARTESIAN_POINT('',(120.,28.778174593052,-5.47665940288702));
#80980=CARTESIAN_POINT('',(210.,28.778174593052,105.476659402887));
#80981=CARTESIAN_POINT('',(200.,-16.476659402887,75.778174593052));
#80982=CARTESIAN_POINT('',(190.,28.778174593052,105.476659402887));
#80983=CARTESIAN_POINT('',(180.,-16.476659402887,75.778174593052));
#80984=CARTESIAN_POINT('',(170.,28.778174593052,105.476659402887));
#80985=CARTESIAN_POINT('',(160.,-16.476659402887,75.778174593052));
#80986=CARTESIAN_POINT('',(150.,28.778174593052,105.476659402887));
#80987=CARTESIAN_POINT('',(140.,-16.476659402887,75.778174593052));
#80988=CARTESIAN_POINT('',(130.,28.778174593052,105.476659402887));
#80989=CARTESIAN_POINT('',(120.,-16.476659402887,75.778174593052));
#80990=CARTESIAN_POINT('',(110.,28.778174593052,105.476659402887));
#80991=CARTESIAN_POINT('',(100.,-16.476659402887,75.778174593052));
#80992=CARTESIAN_POINT('',(90.,28.778174593052,105.476659402887));
#80993=CARTESIAN_POINT('',(210.,0.,100.));
#80994=CARTESIAN_POINT('',(50.,0.,0.));
#80995=CARTESIAN_POINT('',(160.,0.,100.));
#80996=CARTESIAN_POINT('',(100.,0.,0.));
#80997=CARTESIAN_POINT('',(110.,0.,100.));
#80998=CARTESIAN_POINT('',(210.,0.,100.));
#80999=CARTESIAN_POINT('',(50.,0.,0.));
#81000=CARTESIAN_POINT('',(160.,0.,100.));
#81001=CARTESIAN_POINT('',(100.,0.,0.));
#81002=CARTESIAN_POINT('',(110.,0.,100.));
#81003=CARTESIAN_POINT('',(210.,0.,100.));
#81004=CARTESIAN_POINT('',(50.,0.,0.));
#81005=CARTESIAN_POINT('',(160.,0.,100.));
#81006=CARTESIAN_POINT('',(100.,0.,0.));
#81007=CARTESIAN_POINT('',(110.,0.,100.));
#81008=CARTESIAN_POINT('',(150.,0.,0.));
#81009=CARTESIAN_POINT('',(60.,0.,100.));
#81010=CARTESIAN_POINT('',(210.,0.,100.));
#81011=CARTESIAN_POINT('',(210.,22.,0.));
#81012=CARTESIAN_POINT('',(0.,22.,100.));
#81013=CARTESIAN_POINT('',(0.,20.,5.));
#81014=CARTESIAN_POINT('',(210.,20.,95.));
#81015=CARTESIAN_POINT('',(210.,42.,5.));
#81016=CARTESIAN_POINT('',(0.,42.,95.));
#81017=UNCERTAINTY_MEASURE_WITH_UNIT(LENGTH_MEASURE(0.01),#81041,
'DISTANCE_ACCURACY_VALUE',
'Maximum model space distance between geometric entities at asserted c
onnectivities');
#81018=UNCERTAINTY_MEASURE_WITH_UNIT(LENGTH_MEASURE(0.01),#81041,
'DISTANCE_ACCURACY_VALUE',
'Maximum model space distance between geometric entities at asserted c
onnectivities');
#81019=UNCERTAINTY_MEASURE_WITH_UNIT(LENGTH_MEASURE(0.01),#81041,
'DISTANCE_ACCURACY_VALUE',
'Maximum model space distance between geometric entities at asserted c
onnectivities');
#81020=UNCERTAINTY_MEASURE_WITH_UNIT(LENGTH_MEASURE(0.01),#81041,
'DISTANCE_ACCURACY_VALUE',
'Maximum model space distance between geometric entities at asserted c
onnectivities');
#81021=UNCERTAINTY_MEASURE_WITH_UNIT(LENGTH_MEASURE(0.01),#81041,
'DISTANCE_ACCURACY_VALUE',
'Maximum model space distance between geometric entities at asserted c
onnectivities');
#81022=UNCERTAINTY_MEASURE_WITH_UNIT(LENGTH_MEASURE(0.01),#81041,
'DISTANCE_ACCURACY_VALUE',
'Maximum model space distance between geometric entities at asserted c
onnectivities');
#81023=UNCERTAINTY_MEASURE_WITH_UNIT(LENGTH_MEASURE(0.01),#81041,
'DISTANCE_ACCURACY_VALUE',
'Maximum model space distance between geometric entities at asserted c
onnectivities');
#81024=UNCERTAINTY_MEASURE_WITH_UNIT(LENGTH_MEASURE(0.01),#81041,
'DISTANCE_ACCURACY_VALUE',
'Maximum model space distance between geometric entities at asserted c
onnectivities');
#81025=UNCERTAINTY_MEASURE_WITH_UNIT(LENGTH_MEASURE(0.01),#81041,
'DISTANCE_ACCURACY_VALUE',
'Maximum model space distance between geometric entities at asserted c
onnectivities');
#81026=UNCERTAINTY_MEASURE_WITH_UNIT(LENGTH_MEASURE(0.01),#81041,
'DISTANCE_ACCURACY_VALUE',
'Maximum model space distance between geometric entities at asserted c
onnectivities');
#81027=UNCERTAINTY_MEASURE_WITH_UNIT(LENGTH_MEASURE(0.01),#81041,
'DISTANCE_ACCURACY_VALUE',
'Maximum model space distance between geometric entities at asserted c
onnectivities');
#81028=UNCERTAINTY_MEASURE_WITH_UNIT(LENGTH_MEASURE(0.01),#81041,
'DISTANCE_ACCURACY_VALUE',
'Maximum model space distance between geometric entities at asserted c
onnectivities');
#81029=(
GEOMETRIC_REPRESENTATION_CONTEXT(3)
GLOBAL_UNCERTAINTY_ASSIGNED_CONTEXT((#81017))
GLOBAL_UNIT_ASSIGNED_CONTEXT((#81041,#81043,#81044))
REPRESENTATION_CONTEXT('','3D')
);
#81030=(
GEOMETRIC_REPRESENTATION_CONTEXT(3)
GLOBAL_UNCERTAINTY_ASSIGNED_CONTEXT((#81018))
GLOBAL_UNIT_ASSIGNED_CONTEXT((#81041,#81043,#81044))
REPRESENTATION_CONTEXT('','3D')
);
#81031=(
GEOMETRIC_REPRESENTATION_CONTEXT(3)
GLOBAL_UNCERTAINTY_ASSIGNED_CONTEXT((#81019))
GLOBAL_UNIT_ASSIGNED_CONTEXT((#81041,#81043,#81044))
REPRESENTATION_CONTEXT('','3D')
);
#81032=(
GEOMETRIC_REPRESENTATION_CONTEXT(3)
GLOBAL_UNCERTAINTY_ASSIGNED_CONTEXT((#81020))
GLOBAL_UNIT_ASSIGNED_CONTEXT((#81041,#81043,#81044))
REPRESENTATION_CONTEXT('','3D')
);
#81033=(
GEOMETRIC_REPRESENTATION_CONTEXT(3)
GLOBAL_UNCERTAINTY_ASSIGNED_CONTEXT((#81021))
GLOBAL_UNIT_ASSIGNED_CONTEXT((#81041,#81043,#81044))
REPRESENTATION_CONTEXT('','3D')
);
#81034=(
GEOMETRIC_REPRESENTATION_CONTEXT(3)
GLOBAL_UNCERTAINTY_ASSIGNED_CONTEXT((#81022))
GLOBAL_UNIT_ASSIGNED_CONTEXT((#81041,#81043,#81044))
REPRESENTATION_CONTEXT('','3D')
);
#81035=(
GEOMETRIC_REPRESENTATION_CONTEXT(3)
GLOBAL_UNCERTAINTY_ASSIGNED_CONTEXT((#81023))
GLOBAL_UNIT_ASSIGNED_CONTEXT((#81041,#81043,#81044))
REPRESENTATION_CONTEXT('','3D')
);
#81036=(
GEOMETRIC_REPRESENTATION_CONTEXT(3)
GLOBAL_UNCERTAINTY_ASSIGNED_CONTEXT((#81024))
GLOBAL_UNIT_ASSIGNED_CONTEXT((#81041,#81043,#81044))
REPRESENTATION_CONTEXT('','3D')
);
#81037=(
GEOMETRIC_REPRESENTATION_CONTEXT(3)
GLOBAL_UNCERTAINTY_ASSIGNED_CONTEXT((#81025))
GLOBAL_UNIT_ASSIGNED_CONTEXT((#81041,#81043,#81044))
REPRESENTATION_CONTEXT('','3D')
);
#81038=(
GEOMETRIC_REPRESENTATION_CONTEXT(3)
GLOBAL_UNCERTAINTY_ASSIGNED_CONTEXT((#81026))
GLOBAL_UNIT_ASSIGNED_CONTEXT((#81041,#81043,#81044))
REPRESENTATION_CONTEXT('','3D')
);
#81039=(
GEOMETRIC_REPRESENTATION_CONTEXT(3)
GLOBAL_UNCERTAINTY_ASSIGNED_CONTEXT((#81027))
GLOBAL_UNIT_ASSIGNED_CONTEXT((#81041,#81043,#81044))
REPRESENTATION_CONTEXT('','3D')
);
#81040=(
GEOMETRIC_REPRESENTATION_CONTEXT(3)
GLOBAL_UNCERTAINTY_ASSIGNED_CONTEXT((#81028))
GLOBAL_UNIT_ASSIGNED_CONTEXT((#81041,#81043,#81044))
REPRESENTATION_CONTEXT('','3D')
);
#81041=(
LENGTH_UNIT()
NAMED_UNIT(*)
SI_UNIT(.MILLI.,.METRE.)
);
#81042=(
LENGTH_UNIT()
NAMED_UNIT(*)
SI_UNIT($,.METRE.)
);
#81043=(
NAMED_UNIT(*)
PLANE_ANGLE_UNIT()
SI_UNIT($,.RADIAN.)
);
#81044=(
NAMED_UNIT(*)
SI_UNIT($,.STERADIAN.)
SOLID_ANGLE_UNIT()
);
#81045=SHAPE_DEFINITION_REPRESENTATION(#81056,#81129);
#81046=SHAPE_DEFINITION_REPRESENTATION(#81057,#81130);
#81047=SHAPE_DEFINITION_REPRESENTATION(#81058,#81131);
#81048=SHAPE_DEFINITION_REPRESENTATION(#81059,#81132);
#81049=SHAPE_DEFINITION_REPRESENTATION(#81060,#81133);
#81050=SHAPE_DEFINITION_REPRESENTATION(#81061,#81134);
#81051=SHAPE_DEFINITION_REPRESENTATION(#81062,#81135);
#81052=SHAPE_DEFINITION_REPRESENTATION(#81063,#81136);
#81053=SHAPE_DEFINITION_REPRESENTATION(#81064,#81137);
#81054=SHAPE_DEFINITION_REPRESENTATION(#81065,#81138);
#81055=SHAPE_DEFINITION_REPRESENTATION(#81066,#81139);
#81056=PRODUCT_DEFINITION_SHAPE('',$,#81141);
#81057=PRODUCT_DEFINITION_SHAPE('',$,#81142);
#81058=PRODUCT_DEFINITION_SHAPE('',$,#81143);
#81059=PRODUCT_DEFINITION_SHAPE('',$,#81144);
#81060=PRODUCT_DEFINITION_SHAPE('',$,#81145);
#81061=PRODUCT_DEFINITION_SHAPE('',$,#81146);
#81062=PRODUCT_DEFINITION_SHAPE('',$,#81147);
#81063=PRODUCT_DEFINITION_SHAPE('',$,#81148);
#81064=PRODUCT_DEFINITION_SHAPE('',$,#81149);
#81065=PRODUCT_DEFINITION_SHAPE('',$,#81150);
#81066=PRODUCT_DEFINITION_SHAPE('',$,#81151);
#81067=PRODUCT_DEFINITION_SHAPE($,$,#197);
#81068=PRODUCT_DEFINITION_SHAPE($,$,#198);
#81069=PRODUCT_DEFINITION_SHAPE($,$,#199);
#81070=PRODUCT_DEFINITION_SHAPE($,$,#200);
#81071=PRODUCT_DEFINITION_SHAPE($,$,#201);
#81072=PRODUCT_DEFINITION_SHAPE($,$,#202);
#81073=PRODUCT_DEFINITION_SHAPE($,$,#203);
#81074=PRODUCT_DEFINITION_SHAPE($,$,#204);
#81075=PRODUCT_DEFINITION_SHAPE($,$,#205);
#81076=PRODUCT_DEFINITION_SHAPE($,$,#206);
#81077=PRODUCT_DEFINITION_SHAPE($,$,#207);
#81078=PRODUCT_DEFINITION_SHAPE($,$,#208);
#81079=PRODUCT_DEFINITION_SHAPE($,$,#209);
#81080=PRODUCT_DEFINITION_SHAPE($,$,#210);
#81081=PRODUCT_DEFINITION_SHAPE($,$,#211);
#81082=PRODUCT_DEFINITION_SHAPE($,$,#212);
#81083=PRODUCT_DEFINITION_SHAPE($,$,#213);
#81084=PRODUCT_DEFINITION_SHAPE($,$,#214);
#81085=PRODUCT_DEFINITION_SHAPE($,$,#215);
#81086=PRODUCT_DEFINITION_SHAPE($,$,#216);
#81087=PRODUCT_DEFINITION_SHAPE($,$,#217);
#81088=PRODUCT_DEFINITION_SHAPE($,$,#218);
#81089=PRODUCT_DEFINITION_SHAPE($,$,#219);
#81090=PRODUCT_DEFINITION_SHAPE($,$,#220);
#81091=PRODUCT_DEFINITION_SHAPE($,$,#221);
#81092=PRODUCT_DEFINITION_SHAPE($,$,#222);
#81093=PRODUCT_DEFINITION_SHAPE($,$,#223);
#81094=PRODUCT_DEFINITION_SHAPE($,$,#224);
#81095=PRODUCT_DEFINITION_SHAPE($,$,#225);
#81096=PRODUCT_DEFINITION_SHAPE($,$,#226);
#81097=PRODUCT_DEFINITION_SHAPE($,$,#227);
#81098=PRODUCT_DEFINITION_SHAPE($,$,#228);
#81099=PRODUCT_DEFINITION_SHAPE($,$,#229);
#81100=PRODUCT_DEFINITION_SHAPE($,$,#230);
#81101=PRODUCT_DEFINITION_SHAPE($,$,#231);
#81102=PRODUCT_DEFINITION_SHAPE($,$,#232);
#81103=PRODUCT_DEFINITION_SHAPE($,$,#233);
#81104=PRODUCT_DEFINITION_SHAPE($,$,#234);
#81105=PRODUCT_DEFINITION_SHAPE($,$,#235);
#81106=PRODUCT_DEFINITION_SHAPE($,$,#236);
#81107=PRODUCT_DEFINITION_SHAPE($,$,#237);
#81108=PRODUCT_DEFINITION_SHAPE($,$,#238);
#81109=PRODUCT_DEFINITION_SHAPE($,$,#239);
#81110=PRODUCT_DEFINITION_SHAPE($,$,#240);
#81111=PRODUCT_DEFINITION_SHAPE($,$,#241);
#81112=PRODUCT_DEFINITION_SHAPE($,$,#242);
#81113=PRODUCT_DEFINITION_SHAPE($,$,#243);
#81114=PRODUCT_DEFINITION_SHAPE($,$,#244);
#81115=PRODUCT_DEFINITION_SHAPE($,$,#245);
#81116=PRODUCT_DEFINITION_SHAPE($,$,#246);
#81117=PRODUCT_DEFINITION_SHAPE($,$,#247);
#81118=PRODUCT_DEFINITION_SHAPE($,$,#248);
#81119=PRODUCT_DEFINITION_SHAPE($,$,#249);
#81120=PRODUCT_DEFINITION_SHAPE($,$,#250);
#81121=PRODUCT_DEFINITION_SHAPE($,$,#251);
#81122=PRODUCT_DEFINITION_SHAPE($,$,#252);
#81123=PRODUCT_DEFINITION_SHAPE($,$,#253);
#81124=PRODUCT_DEFINITION_SHAPE($,$,#254);
#81125=PRODUCT_DEFINITION_SHAPE($,$,#255);
#81126=PRODUCT_DEFINITION_SHAPE($,$,#256);
#81127=PRODUCT_DEFINITION_SHAPE($,$,#257);
#81128=PRODUCT_DEFINITION_SHAPE($,$,#258);
#81129=SHAPE_REPRESENTATION('',(#15205,#16558,#16559,#16560,#16561,#16562,
#16563,#16564,#16565,#16566,#16567,#16568,#16569,#16570,#16571,#16572,#16573,
#16574,#16575,#16576,#16577,#16578,#16579,#16580,#16581,#16582,#16583,#16584,
#16585,#16586,#16587,#16588,#16589,#16590,#16591,#16592,#16593,#16594,#16595,
#16596,#16597,#16598,#16599,#16600,#16601,#16602,#16603,#16604,#16605,#16606,
#16607,#16608,#16609,#16610,#16611,#16612,#16613,#16614,#16615,#16616,#16617,
#16618,#16619),#81029);
#81130=SHAPE_REPRESENTATION('',(#15206),#81030);
#81131=SHAPE_REPRESENTATION('',(#15327),#81031);
#81132=SHAPE_REPRESENTATION('',(#15614),#81032);
#81133=SHAPE_REPRESENTATION('',(#15705),#81033);
#81134=SHAPE_REPRESENTATION('',(#15816),#81034);
#81135=SHAPE_REPRESENTATION('',(#16075),#81035);
#81136=SHAPE_REPRESENTATION('',(#16085),#81036);
#81137=SHAPE_REPRESENTATION('',(#16363),#81037);
#81138=SHAPE_REPRESENTATION('',(#16450),#81038);
#81139=SHAPE_REPRESENTATION('',(#16512),#81039);
#81140=PRODUCT_DEFINITION_CONTEXT('part definition',#81175,'design');
#81141=PRODUCT_DEFINITION('MAS-256',
'MAS-256',#81152,#81140);
#81142=PRODUCT_DEFINITION('Base - Stationary Rail Block',
'Base - Stationary Rail Block',#81153,#81140);
#81143=PRODUCT_DEFINITION('Table - Top Sliding Stage Platform',
'Table - Top Sliding Stage Platform',#81154,#81140);
#81144=PRODUCT_DEFINITION('V-Way Roller Rail Table Side',
'V-Way Roller Rail Table Side',#81155,#81140);
#81145=PRODUCT_DEFINITION('V-Way Roller Rail Base Side',
'V-Way Roller Rail Base Side',#81156,#81140);
#81146=PRODUCT_DEFINITION('Cross-Roller Cage Strip',
'Cross-Roller Cage Strip',#81157,#81140);
#81147=PRODUCT_DEFINITION('Cylindrical Roller','Cylindrical Roller',#81158,
#81140);
#81148=PRODUCT_DEFINITION('ISO 4762 - M5 x 20 - 12.9',
'ISO 4762 - M5 x 20 - 12.9',#81159,#81140);
#81149=PRODUCT_DEFINITION('ISO 4026 - M5 x 20 - 45H',
'ISO 4026 - M5 x 20 - 45H',#81160,#81140);
#81150=PRODUCT_DEFINITION('ISO 7380-1 - M5 x 8 - 10.9',
'ISO 7380-1 - M5 x 8 - 10.9',#81161,#81140);
#81151=PRODUCT_DEFINITION('ISO 1207 - M3 x 6 - 4.8',
'ISO 1207 - M3 x 6 - 4.8',#81162,#81140);
#81152=PRODUCT_DEFINITION_FORMATION('',$,#81177);
#81153=PRODUCT_DEFINITION_FORMATION('',$,#81178);
#81154=PRODUCT_DEFINITION_FORMATION('',$,#81179);
#81155=PRODUCT_DEFINITION_FORMATION('',$,#81180);
#81156=PRODUCT_DEFINITION_FORMATION('',$,#81181);
#81157=PRODUCT_DEFINITION_FORMATION('',$,#81182);
#81158=PRODUCT_DEFINITION_FORMATION('',$,#81183);
#81159=PRODUCT_DEFINITION_FORMATION('',$,#81184);
#81160=PRODUCT_DEFINITION_FORMATION('',$,#81185);
#81161=PRODUCT_DEFINITION_FORMATION('',$,#81186);
#81162=PRODUCT_DEFINITION_FORMATION('',$,#81187);
#81163=PRODUCT_RELATED_PRODUCT_CATEGORY(
'MAS-256','MAS-256',
(#81177));
#81164=PRODUCT_RELATED_PRODUCT_CATEGORY('Base - Stationary Rail Block',
'Base - Stationary Rail Block',(#81178));
#81165=PRODUCT_RELATED_PRODUCT_CATEGORY(
'Table - Top Sliding Stage Platform',
'Table - Top Sliding Stage Platform',(#81179));
#81166=PRODUCT_RELATED_PRODUCT_CATEGORY('V-Way Roller Rail Table Side',
'V-Way Roller Rail Table Side',(#81180));
#81167=PRODUCT_RELATED_PRODUCT_CATEGORY('V-Way Roller Rail Base Side',
'V-Way Roller Rail Base Side',(#81181));
#81168=PRODUCT_RELATED_PRODUCT_CATEGORY('Cross-Roller Cage Strip',
'Cross-Roller Cage Strip',(#81182));
#81169=PRODUCT_RELATED_PRODUCT_CATEGORY('Cylindrical Roller',
'Cylindrical Roller',(#81183));
#81170=PRODUCT_RELATED_PRODUCT_CATEGORY('ISO 4762 - M5 x 20 - 12.9',
'ISO 4762 - M5 x 20 - 12.9',(#81184));
#81171=PRODUCT_RELATED_PRODUCT_CATEGORY('ISO 4026 - M5 x 20 - 45H',
'ISO 4026 - M5 x 20 - 45H',(#81185));
#81172=PRODUCT_RELATED_PRODUCT_CATEGORY('ISO 7380-1 - M5 x 8 - 10.9',
'ISO 7380-1 - M5 x 8 - 10.9',(#81186));
#81173=PRODUCT_RELATED_PRODUCT_CATEGORY('ISO 1207 - M3 x 6 - 4.8',
'ISO 1207 - M3 x 6 - 4.8',(#81187));
#81174=APPLICATION_PROTOCOL_DEFINITION('international standard',
'automotive_design',2009,#81175);
#81175=APPLICATION_CONTEXT(
'Core Data for Automotive Mechanical Design Process');
#81176=PRODUCT_CONTEXT('part definition',#81175,'mechanical');
#81177=PRODUCT('MAS-256',
'MAS-256',$,(#81176));
#81178=PRODUCT('Base - Stationary Rail Block',
'Base - Stationary Rail Block',$,(#81176));
#81179=PRODUCT('Table - Top Sliding Stage Platform',
'Table - Top Sliding Stage Platform',$,(#81176));
#81180=PRODUCT('V-Way Roller Rail Table Side',
'V-Way Roller Rail Table Side',$,(#81176));
#81181=PRODUCT('V-Way Roller Rail Base Side',
'V-Way Roller Rail Base Side',$,(#81176));
#81182=PRODUCT('Cross-Roller Cage Strip','Cross-Roller Cage Strip',$,(#81176));
#81183=PRODUCT('Cylindrical Roller','Cylindrical Roller',$,(#81176));
#81184=PRODUCT('ISO 4762 - M5 x 20 - 12.9','ISO 4762 - M5 x 20 - 12.9',
$,(#81176));
#81185=PRODUCT('ISO 4026 - M5 x 20 - 45H','ISO 4026 - M5 x 20 - 45H',$,
(#81176));
#81186=PRODUCT('ISO 7380-1 - M5 x 8 - 10.9',
'ISO 7380-1 - M5 x 8 - 10.9',$,(#81176));
#81187=PRODUCT('ISO 1207 - M3 x 6 - 4.8','ISO 1207 - M3 x 6 - 4.8',$,(#81176));
#81188=PRESENTATION_STYLE_ASSIGNMENT((#81199));
#81189=PRESENTATION_STYLE_ASSIGNMENT((#81200));
#81190=PRESENTATION_STYLE_ASSIGNMENT((#81201));
#81191=PRESENTATION_STYLE_ASSIGNMENT((#81202));
#81192=PRESENTATION_STYLE_ASSIGNMENT((#81203));
#81193=PRESENTATION_STYLE_ASSIGNMENT((#81204));
#81194=PRESENTATION_STYLE_ASSIGNMENT((#81205));
#81195=PRESENTATION_STYLE_ASSIGNMENT((#81206));
#81196=PRESENTATION_STYLE_ASSIGNMENT((#81207));
#81197=PRESENTATION_STYLE_ASSIGNMENT((#81208));
#81198=PRESENTATION_STYLE_ASSIGNMENT((#81209));
#81199=SURFACE_STYLE_USAGE(.BOTH.,#81210);
#81200=SURFACE_STYLE_USAGE(.BOTH.,#81211);
#81201=SURFACE_STYLE_USAGE(.BOTH.,#81212);
#81202=SURFACE_STYLE_USAGE(.BOTH.,#81213);
#81203=SURFACE_STYLE_USAGE(.BOTH.,#81214);
#81204=SURFACE_STYLE_USAGE(.BOTH.,#81215);
#81205=SURFACE_STYLE_USAGE(.BOTH.,#81216);
#81206=SURFACE_STYLE_USAGE(.BOTH.,#81217);
#81207=SURFACE_STYLE_USAGE(.BOTH.,#81218);
#81208=SURFACE_STYLE_USAGE(.BOTH.,#81219);
#81209=SURFACE_STYLE_USAGE(.BOTH.,#81220);
#81210=SURFACE_SIDE_STYLE('',(#81221));
#81211=SURFACE_SIDE_STYLE('',(#81222));
#81212=SURFACE_SIDE_STYLE('',(#81223));
#81213=SURFACE_SIDE_STYLE('',(#81224));
#81214=SURFACE_SIDE_STYLE('',(#81225));
#81215=SURFACE_SIDE_STYLE('',(#81226));
#81216=SURFACE_SIDE_STYLE('',(#81227));
#81217=SURFACE_SIDE_STYLE('',(#81228));
#81218=SURFACE_SIDE_STYLE('',(#81229));
#81219=SURFACE_SIDE_STYLE('',(#81230));
#81220=SURFACE_SIDE_STYLE('',(#81231));
#81221=SURFACE_STYLE_FILL_AREA(#81232);
#81222=SURFACE_STYLE_FILL_AREA(#81233);
#81223=SURFACE_STYLE_FILL_AREA(#81234);
#81224=SURFACE_STYLE_FILL_AREA(#81235);
#81225=SURFACE_STYLE_FILL_AREA(#81236);
#81226=SURFACE_STYLE_FILL_AREA(#81237);
#81227=SURFACE_STYLE_FILL_AREA(#81238);
#81228=SURFACE_STYLE_FILL_AREA(#81239);
#81229=SURFACE_STYLE_FILL_AREA(#81240);
#81230=SURFACE_STYLE_FILL_AREA(#81241);
#81231=SURFACE_STYLE_FILL_AREA(#81242);
#81232=FILL_AREA_STYLE('Steel - Satin',(#81243));
#81233=FILL_AREA_STYLE('Opaque(204,208,214)',(#81244));
#81234=FILL_AREA_STYLE('Opaque(222,225,230)',(#81245));
#81235=FILL_AREA_STYLE('Opaque(232,234,237)',(#81246));
#81236=FILL_AREA_STYLE('Opaque(228,231,235)',(#81247));
#81237=FILL_AREA_STYLE('Opaque(194,198,204)',(#81248));
#81238=FILL_AREA_STYLE('Opaque(238,239,241)',(#81249));
#81239=FILL_AREA_STYLE('Opaque(199,204,210)',(#81250));
#81240=FILL_AREA_STYLE('Opaque(196,201,207)',(#81251));
#81241=FILL_AREA_STYLE('Opaque(202,206,212)',(#81252));
#81242=FILL_AREA_STYLE('Opaque(205,209,215)',(#81253));
#81243=FILL_AREA_STYLE_COLOUR('Steel - Satin',#81254);
#81244=FILL_AREA_STYLE_COLOUR('Opaque(204,208,214)',#81255);
#81245=FILL_AREA_STYLE_COLOUR('Opaque(222,225,230)',#81256);
#81246=FILL_AREA_STYLE_COLOUR('Opaque(232,234,237)',#81257);
#81247=FILL_AREA_STYLE_COLOUR('Opaque(228,231,235)',#81258);
#81248=FILL_AREA_STYLE_COLOUR('Opaque(194,198,204)',#81259);
#81249=FILL_AREA_STYLE_COLOUR('Opaque(238,239,241)',#81260);
#81250=FILL_AREA_STYLE_COLOUR('Opaque(199,204,210)',#81261);
#81251=FILL_AREA_STYLE_COLOUR('Opaque(196,201,207)',#81262);
#81252=FILL_AREA_STYLE_COLOUR('Opaque(202,206,212)',#81263);
#81253=FILL_AREA_STYLE_COLOUR('Opaque(205,209,215)',#81264);
#81254=COLOUR_RGB('Steel - Satin', 0.09019608, 0.27058824, 0.51372549);
#81255=COLOUR_RGB('Opaque(204,208,214)', 0.09019608, 0.27058824, 0.51372549);
#81256=COLOUR_RGB('Opaque(222,225,230)', 0.66274510, 0.83137255, 0.94901961);
#81257=COLOUR_RGB('Opaque(232,234,237)', 0.31764706, 0.68627451, 0.89019608);
#81258=COLOUR_RGB('Opaque(228,231,235)', 0.40784314, 0.44705882, 0.49803922);
#81259=COLOUR_RGB('Opaque(194,198,204)', 0.72549020, 0.75294118, 0.79215686);
#81260=COLOUR_RGB('Opaque(238,239,241)', 0.08235294, 0.09019608, 0.10196078);
#81261=COLOUR_RGB('Opaque(199,204,210)', 0.09019608, 0.27058824, 0.51372549);
#81262=COLOUR_RGB('Opaque(196,201,207)', 0.66274510, 0.83137255, 0.94901961);
#81263=COLOUR_RGB('Opaque(202,206,212)', 0.31764706, 0.68627451, 0.89019608);
#81264=COLOUR_RGB('Opaque(205,209,215)', 0.40784314, 0.44705882, 0.49803922);
ENDSEC;
END-ISO-10303-21;
